#173963=CARTESIAN_POINT('Ctrl Pts',(7.30440169836636,15.2,-7.85949861731061));
#173964=CARTESIAN_POINT('Ctrl Pts',(7.30794205593796,15.2,-7.8616645545333));
#173965=CARTESIAN_POINT('Ctrl Pts',(7.3107743417637,15.2,-7.86339730416981));
#173966=CARTESIAN_POINT('Ctrl Pts',(7.31362365465114,15.2,-7.86513376828637));
#173967=CARTESIAN_POINT('Ctrl Pts',(7.31648993774905,15.2,-7.86687379586612));
#173968=CARTESIAN_POINT('Ctrl Pts',(7.31935622123749,15.2,-7.86861382368294));
#173969=CARTESIAN_POINT('Ctrl Pts',(7.32223947388583,15.2,-7.87035741397629));
#173970=CARTESIAN_POINT('Ctrl Pts',(7.32513963891247,15.2,-7.87210441927019));
#173971=CARTESIAN_POINT('Ctrl Pts',(7.32803980354397,15.2,-7.87385142432605));
#173972=CARTESIAN_POINT('Ctrl Pts',(7.33095688067336,15.2,-7.87560184292247));
#173973=CARTESIAN_POINT('Ctrl Pts',(7.33389081321019,15.2,-7.87735552789));
#173974=CARTESIAN_POINT('Ctrl Pts',(7.33682474614678,15.2,-7.87910921309649));
#173975=CARTESIAN_POINT('Ctrl Pts',(7.33977553461869,15.2,-7.88086616522557));
#173976=CARTESIAN_POINT('Ctrl Pts',(7.34274312222597,15.2,-7.88262623787725));
#173977=CARTESIAN_POINT('Ctrl Pts',(7.34571070942892,15.2,-7.88438631028913));
#173978=CARTESIAN_POINT('Ctrl Pts',(7.34869509506136,15.2,-7.88614950430848));
#173979=CARTESIAN_POINT('Ctrl Pts',(7.35169622363116,15.2,-7.88791567475207));
#173980=CARTESIAN_POINT('Ctrl Pts',(7.35469735260987,15.2,-7.88968184543631));
#173981=CARTESIAN_POINT('Ctrl Pts',(7.35771522422608,15.2,-7.89145099240646));
#173982=CARTESIAN_POINT('Ctrl Pts',(7.36074978128144,15.2,-7.89322297366989));
#173983=CARTESIAN_POINT('Ctrl Pts',(7.36378433792335,15.2,-7.89499495469188));
#173984=CARTESIAN_POINT('Ctrl Pts',(7.36683558060356,15.2,-7.89676977047163));
#173985=CARTESIAN_POINT('Ctrl Pts',(7.36990345373996,15.2,-7.89854727899272));
#173986=CARTESIAN_POINT('Ctrl Pts',(7.37450526407154,15.2,-7.90121354213762));
#173987=CARTESIAN_POINT('Ctrl Pts',(7.37914449107004,15.2,-7.90388586714569));
#173988=CARTESIAN_POINT('Ctrl Pts',(7.38382094847736,15.2,-7.90656378325908));
#173989=CARTESIAN_POINT('Ctrl Pts',(7.3877179961044,15.2,-7.9087953798986));
#173990=CARTESIAN_POINT('Ctrl Pts',(7.39164089426428,15.2,-7.91103086062592));
#173991=CARTESIAN_POINT('Ctrl Pts',(7.39558953926637,15.2,-7.91326995729288));
#173992=CARTESIAN_POINT('Ctrl Pts',(7.3987484550098,15.2,-7.91506123448001));
#173993=CARTESIAN_POINT('Ctrl Pts',(7.40192384672332,15.2,-7.91685482577517));
#173994=CARTESIAN_POINT('Ctrl Pts',(7.40511565923911,15.2,-7.91865059812822));
#173995=CARTESIAN_POINT('Ctrl Pts',(7.40830747218978,15.2,-7.92044637072596));
#173996=CARTESIAN_POINT('Ctrl Pts',(7.41151570710461,15.2,-7.92224432322578));
#173997=CARTESIAN_POINT('Ctrl Pts',(7.41474030694288,15.2,-7.92404432146954));
#173998=CARTESIAN_POINT('Ctrl Pts',(7.4179649063418,15.2,-7.92584431946806));
#173999=CARTESIAN_POINT('Ctrl Pts',(7.42120587123443,15.2,-7.92764636550015));
#174000=CARTESIAN_POINT('Ctrl Pts',(7.42446314696709,15.2,-7.92945032535255));
#174001=CARTESIAN_POINT('Ctrl Pts',(7.42772042314354,15.2,-7.93125428545074));
#174002=CARTESIAN_POINT('Ctrl Pts',(7.43099400907197,15.2,-7.93306016080194));
#174003=CARTESIAN_POINT('Ctrl Pts',(7.43428385125231,15.2,-7.9348678196228));
#174004=CARTESIAN_POINT('Ctrl Pts',(7.43839615375362,15.2,-7.93712739302571));
#174005=CARTESIAN_POINT('Ctrl Pts',(7.4425338536735,15.2,-7.93938975434406));
#174006=CARTESIAN_POINT('Ctrl Pts',(7.44669684721657,15.2,-7.94165465272127));
#174007=CARTESIAN_POINT('Ctrl Pts',(7.45002724177875,15.2,-7.94346657127492));
#174008=CARTESIAN_POINT('Ctrl Pts',(7.45337382243719,15.2,-7.94528011225012));
#174009=CARTESIAN_POINT('Ctrl Pts',(7.4567365362168,15.2,-7.94709515010164));
#174010=CARTESIAN_POINT('Ctrl Pts',(7.46009925045458,15.2,-7.94891018820047));
#174011=CARTESIAN_POINT('Ctrl Pts',(7.46347809617761,15.2,-7.95072672205225));
#174012=CARTESIAN_POINT('Ctrl Pts',(7.46687301975257,15.2,-7.95254462620697));
#174013=CARTESIAN_POINT('Ctrl Pts',(7.47026794286497,15.2,-7.954362530114));
#174014=CARTESIAN_POINT('Ctrl Pts',(7.47367894241303,15.2,-7.95618180382438));
#174015=CARTESIAN_POINT('Ctrl Pts',(7.47710596630269,15.2,-7.95800232371085));
#174016=CARTESIAN_POINT('Ctrl Pts',(7.48053299065928,15.2,-7.95982284384536));
#174017=CARTESIAN_POINT('Ctrl Pts',(7.48397603776546,15.2,-7.96164460979129));
#174018=CARTESIAN_POINT('Ctrl Pts',(7.48743505406614,15.2,-7.96346749739071));
#174019=CARTESIAN_POINT('Ctrl Pts',(7.49089406989552,15.2,-7.96529038474176));
#174020=CARTESIAN_POINT('Ctrl Pts',(7.49436905406058,15.2,-7.96711439526759));
#174021=CARTESIAN_POINT('Ctrl Pts',(7.49785995266246,15.2,-7.96893940645163));
#174022=CARTESIAN_POINT('Ctrl Pts',(7.50135085173997,15.2,-7.97076441788432));
#174023=CARTESIAN_POINT('Ctrl Pts',(7.50485766650815,15.2,-7.9725904296684));
#174024=CARTESIAN_POINT('Ctrl Pts',(7.50838034199395,15.2,-7.97441732127625));
#174025=CARTESIAN_POINT('Ctrl Pts',(7.51190301699978,15.2,-7.9762442126352));
#174026=CARTESIAN_POINT('Ctrl Pts',(7.51544155081094,15.2,-7.97807198345061));
#174027=CARTESIAN_POINT('Ctrl Pts',(7.51899589318542,15.2,-7.97990051596771));
#174028=CARTESIAN_POINT('Ctrl Pts',(7.52255023604418,15.2,-7.98172904873396));
#174029=CARTESIAN_POINT('Ctrl Pts',(7.52612038429057,15.2,-7.98355834170584));
#174030=CARTESIAN_POINT('Ctrl Pts',(7.52970628654155,15.2,-7.98538827725001));
#174031=CARTESIAN_POINT('Ctrl Pts',(7.53418866411098,15.2,-7.98767569655557));
#174032=CARTESIAN_POINT('Ctrl Pts',(7.53869565397767,15.2,-7.98996411995003));
#174033=CARTESIAN_POINT('Ctrl Pts',(7.54322715494988,15.2,-7.99225331849168));
#174034=CARTESIAN_POINT('Ctrl Pts',(7.54685235592522,15.2,-7.99408467742482));
#174035=CARTESIAN_POINT('Ctrl Pts',(7.5504932419663,15.2,-7.99591653310803));
#174036=CARTESIAN_POINT('Ctrl Pts',(7.5541497608894,15.2,-7.99774877004125));
#174037=CARTESIAN_POINT('Ctrl Pts',(7.5578062793143,15.2,-7.99958100672483));
#174038=CARTESIAN_POINT('Ctrl Pts',(7.56147842973493,15.2,-8.00141362508195));
#174039=CARTESIAN_POINT('Ctrl Pts',(7.56516615950571,15.2,-8.00324650977377));
#174040=CARTESIAN_POINT('Ctrl Pts',(7.56885388977894,15.2,-8.00507939471531));
#174041=CARTESIAN_POINT('Ctrl Pts',(7.57255719835921,15.2,-8.00691254635538));
#174042=CARTESIAN_POINT('Ctrl Pts',(7.57627603334126,15.2,-8.00874585256643));
#174043=CARTESIAN_POINT('Ctrl Pts',(7.58092457681545,15.2,-8.01103748520534));
#174044=CARTESIAN_POINT('Ctrl Pts',(7.58559737906784,15.2,-8.01332935810536));
#174045=CARTESIAN_POINT('Ctrl Pts',(7.59029433663925,15.2,-8.01562125254979));
#174046=CARTESIAN_POINT('Ctrl Pts',(7.5940519023892,15.2,-8.01745476795546));
#174047=CARTESIAN_POINT('Ctrl Pts',(7.59782492616485,15.2,-8.01928829830977));
#174048=CARTESIAN_POINT('Ctrl Pts',(7.60161335670564,15.2,-8.02112173122377));
#174049=CARTESIAN_POINT('Ctrl Pts',(7.6054017877626,15.2,-8.02295516438757));
#174050=CARTESIAN_POINT('Ctrl Pts',(7.60920562595072,15.2,-8.0247885025054));
#174051=CARTESIAN_POINT('Ctrl Pts',(7.61302481688267,15.2,-8.02662163404973));
#174052=CARTESIAN_POINT('Ctrl Pts',(7.61684400729424,15.2,-8.0284547653443));
#174053=CARTESIAN_POINT('Ctrl Pts',(7.62067855032046,15.2,-8.03028769017776));
#174054=CARTESIAN_POINT('Ctrl Pts',(7.62452839472697,15.2,-8.03212030158353));
#174055=CARTESIAN_POINT('Ctrl Pts',(7.62837823965803,15.2,-8.033952913239));
#174056=CARTESIAN_POINT('Ctrl Pts',(7.63224338392581,15.2,-8.0357852113995));
#174057=CARTESIAN_POINT('Ctrl Pts',(7.63612377705471,15.2,-8.0376170877575));
#174058=CARTESIAN_POINT('Ctrl Pts',(7.64000416965489,15.2,-8.03944896386589));
#174059=CARTESIAN_POINT('Ctrl Pts',(7.64389980889269,15.2,-8.04128041761109));
#174060=CARTESIAN_POINT('Ctrl Pts',(7.64781064340532,15.2,-8.04311134435034));
#174061=CARTESIAN_POINT('Ctrl Pts',(7.65172147845082,15.2,-8.04494227133905));
#174062=CARTESIAN_POINT('Ctrl Pts',(7.65564750900921,15.2,-8.04677267072491));
#174063=CARTESIAN_POINT('Ctrl Pts',(7.65958868261389,15.2,-8.04860243765793));
#174064=CARTESIAN_POINT('Ctrl Pts',(7.66352985568157,15.2,-8.05043220434163));
#174065=CARTESIAN_POINT('Ctrl Pts',(7.66748616990403,15.2,-8.05226133700944));
#174066=CARTESIAN_POINT('Ctrl Pts',(7.67145757516536,15.2,-8.0540897332847));
#174067=CARTESIAN_POINT('Ctrl Pts',(7.67542898096779,15.2,-8.05591812980909));
#174068=CARTESIAN_POINT('Ctrl Pts',(7.67941547718586,15.2,-8.05774578974429));
#174069=CARTESIAN_POINT('Ctrl Pts',(7.68341701029382,15.2,-8.05957260939935));
#174070=CARTESIAN_POINT('Ctrl Pts',(7.68741854285656,15.2,-8.06139942880551));
#174071=CARTESIAN_POINT('Ctrl Pts',(7.69143511387739,15.2,-8.06322540671183));
#174072=CARTESIAN_POINT('Ctrl Pts',(7.69546667032407,15.2,-8.06505044345163));
#174073=CARTESIAN_POINT('Ctrl Pts',(7.69949822732004,15.2,-8.06687548044008));
#174074=CARTESIAN_POINT('Ctrl Pts',(7.70354477009058,15.2,-8.06869957497418));
#174075=CARTESIAN_POINT('Ctrl Pts',(7.70760624521932,15.2,-8.07052262602626));
#174076=CARTESIAN_POINT('Ctrl Pts',(7.71166771979469,15.2,-8.07234567682996));
#174077=CARTESIAN_POINT('Ctrl Pts',(7.71574412950861,15.2,-8.07416768306215));
#174078=CARTESIAN_POINT('Ctrl Pts',(7.7198354193393,15.2,-8.07598854646898));
#174079=CARTESIAN_POINT('Ctrl Pts',(7.72290388740911,15.2,-8.07735419433421));
#174080=CARTESIAN_POINT('Ctrl Pts',(7.72598072637295,15.2,-8.07871919913259));
#174081=CARTESIAN_POINT('Ctrl Pts',(7.72906591394746,15.2,-8.08008351803911));
#174082=CARTESIAN_POINT('Ctrl Pts',(7.7321511009615,15.2,-8.08144783669778));
#174083=CARTESIAN_POINT('Ctrl Pts',(7.73524463656677,15.2,-8.08281146929815));
#174084=CARTESIAN_POINT('Ctrl Pts',(7.73834649953813,15.2,-8.08417437591523));
#174085=CARTESIAN_POINT('Ctrl Pts',(7.74144836250949,15.2,-8.08553728253232));
#174086=CARTESIAN_POINT('Ctrl Pts',(7.74455855253516,15.2,-8.08689946147788));
#174087=CARTESIAN_POINT('Ctrl Pts',(7.74767704701939,15.2,-8.08826087222626));
#174088=CARTESIAN_POINT('Ctrl Pts',(7.75183503947618,15.2,-8.09007608647499));
#174089=CARTESIAN_POINT('Ctrl Pts',(7.75600779751741,15.2,-8.09188993544337));
#174090=CARTESIAN_POINT('Ctrl Pts',(7.76019526734024,15.2,-8.09370232146203));
#174091=CARTESIAN_POINT('Ctrl Pts',(7.76333587042055,15.2,-8.09506161128469));
#174092=CARTESIAN_POINT('Ctrl Pts',(7.76648474912819,15.2,-8.09642007686546));
#174093=CARTESIAN_POINT('Ctrl Pts',(7.76964188221315,15.2,-8.09777767931265));
#174094=CARTESIAN_POINT('Ctrl Pts',(7.77279901472456,15.2,-8.0991352815132));
#174095=CARTESIAN_POINT('Ctrl Pts',(7.77596440179388,15.2,-8.10049202014713));
#174096=CARTESIAN_POINT('Ctrl Pts',(7.77913802034595,15.2,-8.10184785484779));
#174097=CARTESIAN_POINT('Ctrl Pts',(7.78231163889802,15.2,-8.10320368954846));
#174098=CARTESIAN_POINT('Ctrl Pts',(7.7854934897375,15.2,-8.10455862031097));
#174099=CARTESIAN_POINT('Ctrl Pts',(7.78868355171945,15.2,-8.10591260651792));
#174100=CARTESIAN_POINT('Ctrl Pts',(7.79187361370141,15.2,-8.10726659272487));
#174101=CARTESIAN_POINT('Ctrl Pts',(7.79507188673229,15.2,-8.1086196342751));
#174102=CARTESIAN_POINT('Ctrl Pts',(7.79827834775531,15.2,-8.10997169244046));
#174103=CARTESIAN_POINT('Ctrl Pts',(7.80148480877833,15.2,-8.11132375060581));
#174104=CARTESIAN_POINT('Ctrl Pts',(7.80469945859988,15.2,-8.11267482453515));
#174105=CARTESIAN_POINT('Ctrl Pts',(7.80792227510707,15.2,-8.11402487511118));
#174106=CARTESIAN_POINT('Ctrl Pts',(7.81114509161427,15.2,-8.11537492568722));
#174107=CARTESIAN_POINT('Ctrl Pts',(7.8143760758959,15.2,-8.11672395137166));
#174108=CARTESIAN_POINT('Ctrl Pts',(7.81761520536043,15.2,-8.11807191503117));
#174109=CARTESIAN_POINT('Ctrl Pts',(7.82085433541341,15.2,-8.11941987893555));
#174110=CARTESIAN_POINT('Ctrl Pts',(7.82410161060201,15.2,-8.12076677956464));
#174111=CARTESIAN_POINT('Ctrl Pts',(7.82735700970124,15.2,-8.12211257855174));
#174112=CARTESIAN_POINT('Ctrl Pts',(7.83061240820906,15.2,-8.12345837729435));
#174113=CARTESIAN_POINT('Ctrl Pts',(7.83387593048743,15.2,-8.12480307394178));
#174114=CARTESIAN_POINT('Ctrl Pts',(7.83714755511628,15.2,-8.12614663025162));
#174115=CARTESIAN_POINT('Ctrl Pts',(7.84041917974513,15.2,-8.12749018656146));
#174116=CARTESIAN_POINT('Ctrl Pts',(7.84369890559382,15.2,-8.12883260207837));
#174117=CARTESIAN_POINT('Ctrl Pts',(7.84698671255839,15.2,-8.13017383786286));
#174118=CARTESIAN_POINT('Ctrl Pts',(7.85027451952297,15.2,-8.13151507364736));
#174119=CARTESIAN_POINT('Ctrl Pts',(7.8535704072366,15.2,-8.132855130532));
#174120=CARTESIAN_POINT('Ctrl Pts',(7.85687435324155,15.2,-8.13419397023335));
#174121=CARTESIAN_POINT('Ctrl Pts',(7.86127961498163,15.2,-8.13597908999731));
#174122=CARTESIAN_POINT('Ctrl Pts',(7.86569920325117,15.2,-8.13776204476379));
#174123=CARTESIAN_POINT('Ctrl Pts',(7.8701330682165,15.2,-8.1395427452495));
#174124=CARTESIAN_POINT('Ctrl Pts',(7.87345846663844,15.2,-8.14087827049248));
#174125=CARTESIAN_POINT('Ctrl Pts',(7.87679189515162,15.2,-8.14221252771051));
#174126=CARTESIAN_POINT('Ctrl Pts',(7.88013333211424,15.2,-8.14354547941196));
#174127=CARTESIAN_POINT('Ctrl Pts',(7.88347476907685,15.2,-8.1448784311134));
#174128=CARTESIAN_POINT('Ctrl Pts',(7.88682421419297,15.2,-8.14621007677687));
#174129=CARTESIAN_POINT('Ctrl Pts',(7.89018164625294,15.2,-8.14754038002623));
#174130=CARTESIAN_POINT('Ctrl Pts',(7.89353907831292,15.2,-8.1488706832756));
#174131=CARTESIAN_POINT('Ctrl Pts',(7.89690449902077,15.2,-8.15019964365768));
#174132=CARTESIAN_POINT('Ctrl Pts',(7.90027788449683,15.2,-8.15152722299049));
#174133=CARTESIAN_POINT('Ctrl Pts',(7.90365126997288,15.2,-8.15285480232329));
#174134=CARTESIAN_POINT('Ctrl Pts',(7.90703261990442,15.2,-8.15418100155361));
#174135=CARTESIAN_POINT('Ctrl Pts',(7.91042191486392,15.2,-8.15550578383893));
#174136=CARTESIAN_POINT('Ctrl Pts',(7.91381120982342,15.2,-8.15683056612426));
#174137=CARTESIAN_POINT('Ctrl Pts',(7.9172084492157,15.2,-8.15815393170967));
#174138=CARTESIAN_POINT('Ctrl Pts',(7.92061361075757,15.2,-8.15947584345351));
#174139=CARTESIAN_POINT('Ctrl Pts',(7.92401877291804,15.2,-8.1607977554375));
#174140=CARTESIAN_POINT('Ctrl Pts',(7.92743185824741,15.2,-8.16211821359607));
#174141=CARTESIAN_POINT('Ctrl Pts',(7.93085284395401,15.2,-8.16343718157922));
#174142=CARTESIAN_POINT('Ctrl Pts',(7.93427382903912,15.2,-8.16475614932277));
#174143=CARTESIAN_POINT('Ctrl Pts',(7.93770271698383,15.2,-8.16607362622019));
#174144=CARTESIAN_POINT('Ctrl Pts',(7.94113948369823,15.2,-8.16738957798795));
#174145=CARTESIAN_POINT('Ctrl Pts',(7.94457625041264,15.2,-8.1687055297557));
#174146=CARTESIAN_POINT('Ctrl Pts',(7.94802089680109,15.2,-8.17001995414094));
#174147=CARTESIAN_POINT('Ctrl Pts',(7.95147340134301,15.2,-8.17133281688477));
#174148=CARTESIAN_POINT('Ctrl Pts',(7.95492590588493,15.2,-8.1726456796286));
#174149=CARTESIAN_POINT('Ctrl Pts',(7.95838626900923,15.2,-8.17395698016428));
#174150=CARTESIAN_POINT('Ctrl Pts',(7.96185446946655,15.2,-8.17526668253336));
#174151=CARTESIAN_POINT('Ctrl Pts',(7.96532266992388,15.2,-8.17657638490244));
#174152=CARTESIAN_POINT('Ctrl Pts',(7.96879870768088,15.2,-8.17788449018826));
#174153=CARTESIAN_POINT('Ctrl Pts',(7.97228256113695,15.2,-8.17919096205759));
#174154=CARTESIAN_POINT('Ctrl Pts',(7.97576641459302,15.2,-8.18049743392693));
#174155=CARTESIAN_POINT('Ctrl Pts',(7.97925808400946,15.2,-8.18180227364659));
#174156=CARTESIAN_POINT('Ctrl Pts',(7.98275754809791,15.2,-8.18310544349788));
#174157=CARTESIAN_POINT('Ctrl Pts',(7.98742350063965,15.2,-8.18484300345741));
#174158=CARTESIAN_POINT('Ctrl Pts',(7.99210330678536,15.2,-8.18657759313905));
#174159=CARTESIAN_POINT('Ctrl Pts',(7.99679691987539,15.2,-8.18830913439989));
#174160=CARTESIAN_POINT('Ctrl Pts',(8.00031712937317,15.2,-8.18960779022755));
#174161=CARTESIAN_POINT('Ctrl Pts',(8.00384510547836,15.2,-8.19090473193042));
#174162=CARTESIAN_POINT('Ctrl Pts',(8.00738082801655,15.2,-8.19219992675836));
#174163=CARTESIAN_POINT('Ctrl Pts',(8.01091655055476,15.2,-8.19349512158631));
#174164=CARTESIAN_POINT('Ctrl Pts',(8.0144600206093,15.2,-8.19478857045598));
#174165=CARTESIAN_POINT('Ctrl Pts',(8.01801121306294,15.2,-8.19608023411754));
#174166=CARTESIAN_POINT('Ctrl Pts',(8.02156240551658,15.2,-8.1973718977791));
#174167=CARTESIAN_POINT('Ctrl Pts',(8.02512132091221,15.2,-8.19866177459971));
#174168=CARTESIAN_POINT('Ctrl Pts',(8.02868793308492,15.2,-8.19994982449247));
#174169=CARTESIAN_POINT('Ctrl Pts',(8.03225454525763,15.2,-8.20123787438524));
#174170=CARTESIAN_POINT('Ctrl Pts',(8.03582885370021,15.2,-8.20252409623311));
#174171=CARTESIAN_POINT('Ctrl Pts',(8.03941084394403,15.2,-8.20380846647837));
#174172=CARTESIAN_POINT('Ctrl Pts',(8.04418683136959,15.2,-8.20552096029426));
#174173=CARTESIAN_POINT('Ctrl Pts',(8.04897647635771,15.2,-8.20723016286848));
#174174=CARTESIAN_POINT('Ctrl Pts',(8.05377977099995,15.2,-8.20893607000002));
#174175=CARTESIAN_POINT('Ctrl Pts',(7.01216898599994,12.2,-7.64657512400002));
#174176=CARTESIAN_POINT('Ctrl Pts',(7.01348522039998,12.2,-7.64778327244868));
#174177=CARTESIAN_POINT('Ctrl Pts',(7.0148472207803,12.2,-7.64902613336841));
#174178=CARTESIAN_POINT('Ctrl Pts',(7.01625467904572,12.2,-7.65030255165183));
#174179=CARTESIAN_POINT('Ctrl Pts',(7.01766892478633,12.2,-7.65158512546942));
#174180=CARTESIAN_POINT('Ctrl Pts',(7.01912907680239,12.2,-7.6529015883544));
#174181=CARTESIAN_POINT('Ctrl Pts',(7.02063486162897,12.2,-7.65425083033056));
#174182=CARTESIAN_POINT('Ctrl Pts',(7.0221406463188,12.2,-7.65560007218416));
#174183=CARTESIAN_POINT('Ctrl Pts',(7.0236920633662,12.2,-7.65698209165132));
#174184=CARTESIAN_POINT('Ctrl Pts',(7.02528884122486,12.2,-7.65839580976662));
#174185=CARTESIAN_POINT('Ctrl Pts',(7.02688561908352,12.2,-7.65980952788194));
#174186=CARTESIAN_POINT('Ctrl Pts',(7.02852775929138,12.2,-7.66125494592225));
#174187=CARTESIAN_POINT('Ctrl Pts',(7.03021499706176,12.2,-7.66273101410724));
#174188=CARTESIAN_POINT('Ctrl Pts',(7.03190223498538,12.2,-7.66420708242633));
#174189=CARTESIAN_POINT('Ctrl Pts',(7.03363456925201,12.2,-7.66571380189834));
#174190=CARTESIAN_POINT('Ctrl Pts',(7.03541173743525,12.2,-7.66725015515077));
#174191=CARTESIAN_POINT('Ctrl Pts',(7.03718890545706,12.2,-7.66878650826362));
#174192=CARTESIAN_POINT('Ctrl Pts',(7.03901091135163,12.2,-7.67035249414299));
#174193=CARTESIAN_POINT('Ctrl Pts',(7.04087749604239,12.2,-7.67194712350903));
#174194=CARTESIAN_POINT('Ctrl Pts',(7.04274408073314,12.2,-7.67354175287507));
#174195=CARTESIAN_POINT('Ctrl Pts',(7.04465524144143,12.2,-7.67516502671293));
#174196=CARTESIAN_POINT('Ctrl Pts',(7.04661073111848,12.2,-7.67681598040177));
#174197=CARTESIAN_POINT('Ctrl Pts',(7.04856622097314,12.2,-7.67846693424055));
#174198=CARTESIAN_POINT('Ctrl Pts',(7.0505660383916,12.2,-7.68014557138276));
#174199=CARTESIAN_POINT('Ctrl Pts',(7.052609930506,12.2,-7.68185095122753));
#174200=CARTESIAN_POINT('Ctrl Pts',(7.05465382243473,12.2,-7.68355633091739));
#174201=CARTESIAN_POINT('Ctrl Pts',(7.0567417943918,12.2,-7.68528845520865));
#174202=CARTESIAN_POINT('Ctrl Pts',(7.05887359714957,12.2,-7.68704641381255));
#174203=CARTESIAN_POINT('Ctrl Pts',(7.06100539990735,12.2,-7.68880437241647));
#174204=CARTESIAN_POINT('Ctrl Pts',(7.06318103490329,12.2,-7.69058816246829));
#174205=CARTESIAN_POINT('Ctrl Pts',(7.06540025990411,12.2,-7.6923968984015));
#174206=CARTESIAN_POINT('Ctrl Pts',(7.06761948490493,12.2,-7.69420563433471));
#174207=CARTESIAN_POINT('Ctrl Pts',(7.0698823003436,12.2,-7.69603931773329));
#174208=CARTESIAN_POINT('Ctrl Pts',(7.07218846800684,12.2,-7.69789707783082));
#174209=CARTESIAN_POINT('Ctrl Pts',(7.07449463587956,12.2,-7.69975483809708));
#174210=CARTESIAN_POINT('Ctrl Pts',(7.07684415358985,12.2,-7.7016366785324));
#174211=CARTESIAN_POINT('Ctrl Pts',(7.07923678863878,12.2,-7.70354175580389));
#174212=CARTESIAN_POINT('Ctrl Pts',(7.08162942347036,12.2,-7.70544683290233));
#174213=CARTESIAN_POINT('Ctrl Pts',(7.08406517439434,12.2,-7.70737514680284));
#174214=CARTESIAN_POINT('Ctrl Pts',(7.08654380831542,12.2,-7.70932587299076));
#174215=CARTESIAN_POINT('Ctrl Pts',(7.0890224422365,12.2,-7.71127659917867));
#174216=CARTESIAN_POINT('Ctrl Pts',(7.09154395894146,12.2,-7.71324973923985));
#174217=CARTESIAN_POINT('Ctrl Pts',(7.09410812976205,12.2,-7.71524449049922));
#174218=CARTESIAN_POINT('Ctrl Pts',(7.09667230081556,12.2,-7.7172392419398));
#174219=CARTESIAN_POINT('Ctrl Pts',(7.09927912588989,12.2,-7.71925560495751));
#174220=CARTESIAN_POINT('Ctrl Pts',(7.10192837511943,12.2,-7.72129279365276));
#174221=CARTESIAN_POINT('Ctrl Pts',(7.10457762410833,12.2,-7.72332998216297));
#174222=CARTESIAN_POINT('Ctrl Pts',(7.10726930113565,12.2,-7.72538800047348));
#174223=CARTESIAN_POINT('Ctrl Pts',(7.11000317804864,12.2,-7.72746607899071));
#174224=CARTESIAN_POINT('Ctrl Pts',(7.11273705496165,12.2,-7.72954415750795));
#174225=CARTESIAN_POINT('Ctrl Pts',(7.11551313393964,12.2,-7.73164229980578));
#174226=CARTESIAN_POINT('Ctrl Pts',(7.11833118991771,12.2,-7.73375975631085));
#174227=CARTESIAN_POINT('Ctrl Pts',(7.12114924615177,12.2,-7.73587721300827));
#174228=CARTESIAN_POINT('Ctrl Pts',(7.12400928121682,12.2,-7.73801398467397));
#174229=CARTESIAN_POINT('Ctrl Pts',(7.12691107627235,12.2,-7.74016934248353));
#174230=CARTESIAN_POINT('Ctrl Pts',(7.1298128710643,12.2,-7.7423247000973));
#174231=CARTESIAN_POINT('Ctrl Pts',(7.13275642209165,12.2,-7.74449864123795));
#174232=CARTESIAN_POINT('Ctrl Pts',(7.13574151498319,12.2,-7.74669045474164));
#174233=CARTESIAN_POINT('Ctrl Pts',(7.13872660787473,12.2,-7.74888226824533));
#174234=CARTESIAN_POINT('Ctrl Pts',(7.14175324050544,12.2,-7.75109195327193));
#174235=CARTESIAN_POINT('Ctrl Pts',(7.14482119846152,12.2,-7.75331881030127));
#174236=CARTESIAN_POINT('Ctrl Pts',(7.14788915669627,12.2,-7.7555456675329));
#174237=CARTESIAN_POINT('Ctrl Pts',(7.15099843786044,12.2,-7.75778969883038));
#174238=CARTESIAN_POINT('Ctrl Pts',(7.15414883011829,12.2,-7.76005022170473));
#174239=CARTESIAN_POINT('Ctrl Pts',(7.15729922208998,12.2,-7.76231074437373));
#174240=CARTESIAN_POINT('Ctrl Pts',(7.16049072419569,12.2,-7.76458775550723));
#174241=CARTESIAN_POINT('Ctrl Pts',(7.16372312500968,12.2,-7.7668805912677));
#174242=CARTESIAN_POINT('Ctrl Pts',(7.16695552582367,12.2,-7.76917342702817));
#174243=CARTESIAN_POINT('Ctrl Pts',(7.17022882447495,12.2,-7.77148208502517));
#174244=CARTESIAN_POINT('Ctrl Pts',(7.17354281051944,12.2,-7.77380591110674));
#174245=CARTESIAN_POINT('Ctrl Pts',(7.17630446565685,12.2,-7.77574243291175));
#174246=CARTESIAN_POINT('Ctrl Pts',(7.17909437698944,12.2,-7.77768948970035));
#174247=CARTESIAN_POINT('Ctrl Pts',(7.18191242205741,12.2,-7.77964670963038));
#174248=CARTESIAN_POINT('Ctrl Pts',(7.18473046712538,12.2,-7.7816039295604));
#174249=CARTESIAN_POINT('Ctrl Pts',(7.18757664829088,12.2,-7.78357131208995));
#174250=CARTESIAN_POINT('Ctrl Pts',(7.19045084253998,12.2,-7.78554849376558));
#174251=CARTESIAN_POINT('Ctrl Pts',(7.19332503678907,12.2,-7.78752567544121));
#174252=CARTESIAN_POINT('Ctrl Pts',(7.19622724572209,12.2,-7.78951265435554));
#174253=CARTESIAN_POINT('Ctrl Pts',(7.1991573499582,12.2,-7.79150907504999));
#174254=CARTESIAN_POINT('Ctrl Pts',(7.20208745419431,12.2,-7.79350549574444));
#174255=CARTESIAN_POINT('Ctrl Pts',(7.20504545320452,12.2,-7.79551135381969));
#174256=CARTESIAN_POINT('Ctrl Pts',(7.20803123050984,12.2,-7.79752630146776));
#174257=CARTESIAN_POINT('Ctrl Pts',(7.21101700781514,12.2,-7.79954124911583));
#174258=CARTESIAN_POINT('Ctrl Pts',(7.21403055872526,12.2,-7.80156528312142));
#174259=CARTESIAN_POINT('Ctrl Pts',(7.21707177115726,12.2,-7.80359805985798));
#174260=CARTESIAN_POINT('Ctrl Pts',(7.22011298358926,12.2,-7.80563083659454));
#174261=CARTESIAN_POINT('Ctrl Pts',(7.22318185372333,12.2,-7.80767235337257));
#174262=CARTESIAN_POINT('Ctrl Pts',(7.22627826691921,12.2,-7.80972227115077));
#174263=CARTESIAN_POINT('Ctrl Pts',(7.22937468011509,12.2,-7.81177218892898));
#174264=CARTESIAN_POINT('Ctrl Pts',(7.232498633412,12.2,-7.81383050583054));
#174265=CARTESIAN_POINT('Ctrl Pts',(7.2356500136408,12.2,-7.8158968902399));
#174266=CARTESIAN_POINT('Ctrl Pts',(7.2388013938696,12.2,-7.81796327464925));
#174267=CARTESIAN_POINT('Ctrl Pts',(7.24198019768924,12.2,-7.82003772281617));
#174268=CARTESIAN_POINT('Ctrl Pts',(7.24518631192758,12.2,-7.82211990649735));
#174269=CARTESIAN_POINT('Ctrl Pts',(7.24839242616592,12.2,-7.82420209017854));
#174270=CARTESIAN_POINT('Ctrl Pts',(7.25162585030193,12.2,-7.8262920095904));
#174271=CARTESIAN_POINT('Ctrl Pts',(7.25488646794304,12.2,-7.82838934000766));
#174272=CARTESIAN_POINT('Ctrl Pts',(7.25814708522875,12.2,-7.83048667019634));
#174273=CARTESIAN_POINT('Ctrl Pts',(7.26143489795204,12.2,-7.83259141059899));
#174274=CARTESIAN_POINT('Ctrl Pts',(7.26474978932463,12.2,-7.83470324321544));
#174275=CARTESIAN_POINT('Ctrl Pts',(7.26806468105854,12.2,-7.83681507606209));
#174276=CARTESIAN_POINT('Ctrl Pts',(7.27140665252256,12.2,-7.83893400037807));
#174277=CARTESIAN_POINT('Ctrl Pts',(7.27477558932589,12.2,-7.84105970169696));
#174278=CARTESIAN_POINT('Ctrl Pts',(7.27881831371023,12.2,-7.84361054341865));
#174279=CARTESIAN_POINT('Ctrl Pts',(7.28289986889003,12.2,-7.84617114590798));
#174280=CARTESIAN_POINT('Ctrl Pts',(7.28702005819959,12.2,-7.84874097163176));
#174281=CARTESIAN_POINT('Ctrl Pts',(7.29045354910377,12.2,-7.85088249295154));
#174282=CARTESIAN_POINT('Ctrl Pts',(7.29391387020648,12.2,-7.85303042183648));
#174283=CARTESIAN_POINT('Ctrl Pts',(7.2974009071881,12.2,-7.85518445250007));
#174284=CARTESIAN_POINT('Ctrl Pts',(7.30088794416971,12.2,-7.85733848316366));
#174285=CARTESIAN_POINT('Ctrl Pts',(7.30440169836636,12.2,-7.85949861731061));
#174286=CARTESIAN_POINT('Ctrl Pts',(7.30794205593796,12.2,-7.8616645545333));
#174287=CARTESIAN_POINT('Ctrl Pts',(7.3107743417637,12.2,-7.86339730416981));
#174288=CARTESIAN_POINT('Ctrl Pts',(7.31362365465114,12.2,-7.86513376828637));
#174289=CARTESIAN_POINT('Ctrl Pts',(7.31648993774905,12.2,-7.86687379586612));
#174290=CARTESIAN_POINT('Ctrl Pts',(7.31935622123749,12.2,-7.86861382368294));
#174291=CARTESIAN_POINT('Ctrl Pts',(7.32223947388583,12.2,-7.87035741397629));
#174292=CARTESIAN_POINT('Ctrl Pts',(7.32513963891247,12.2,-7.87210441927019));
#174293=CARTESIAN_POINT('Ctrl Pts',(7.32803980354397,12.2,-7.87385142432605));
#174294=CARTESIAN_POINT('Ctrl Pts',(7.33095688067336,12.2,-7.87560184292247));
#174295=CARTESIAN_POINT('Ctrl Pts',(7.33389081321019,12.2,-7.87735552789));
#174296=CARTESIAN_POINT('Ctrl Pts',(7.33755822918106,12.2,-7.87954763427864));
#174297=CARTESIAN_POINT('Ctrl Pts',(7.34125198209144,12.2,-7.88174484455071));
#174298=CARTESIAN_POINT('Ctrl Pts',(7.34497196125675,12.2,-7.88394687510602));
#174299=CARTESIAN_POINT('Ctrl Pts',(7.34794794475119,12.2,-7.88570849964627));
#174300=CARTESIAN_POINT('Ctrl Pts',(7.35094071298473,12.2,-7.88747320897994));
#174301=CARTESIAN_POINT('Ctrl Pts',(7.35395020891167,12.2,-7.88924085899819));
#174302=CARTESIAN_POINT('Ctrl Pts',(7.35695970442857,12.2,-7.89100850877559));
#174303=CARTESIAN_POINT('Ctrl Pts',(7.35998592972057,12.2,-7.8927790992141));
#174304=CARTESIAN_POINT('Ctrl Pts',(7.36302882619295,12.2,-7.89455248834672));
#174305=CARTESIAN_POINT('Ctrl Pts',(7.36607172307993,12.2,-7.89632587772097));
#174306=CARTESIAN_POINT('Ctrl Pts',(7.36913129149947,12.2,-7.89810206652612));
#174307=CARTESIAN_POINT('Ctrl Pts',(7.37220747700153,12.2,-7.89988091384546));
#174308=CARTESIAN_POINT('Ctrl Pts',(7.37528366208447,12.2,-7.90165976092243));
#174309=CARTESIAN_POINT('Ctrl Pts',(7.37837646182128,12.2,-7.90344126715918));
#174310=CARTESIAN_POINT('Ctrl Pts',(7.38148582249879,12.2,-7.90522529299115));
#174311=CARTESIAN_POINT('Ctrl Pts',(7.38459518359994,12.2,-7.90700931906619));
#174312=CARTESIAN_POINT('Ctrl Pts',(7.38772110534015,12.2,-7.90879586437362));
#174313=CARTESIAN_POINT('Ctrl Pts',(7.39086353029026,12.2,-7.91058479363794));
#174314=CARTESIAN_POINT('Ctrl Pts',(7.39400595481222,12.2,-7.91237372265852));
#174315=CARTESIAN_POINT('Ctrl Pts',(7.39716488463087,12.2,-7.91416503415361));
#174316=CARTESIAN_POINT('Ctrl Pts',(7.40034026248071,12.2,-7.91595859200676));
#174317=CARTESIAN_POINT('Ctrl Pts',(7.40351564076321,12.2,-7.91775215010429));
#174318=CARTESIAN_POINT('Ctrl Pts',(7.40670746712928,12.2,-7.91954795595341));
#174319=CARTESIAN_POINT('Ctrl Pts',(7.4099156879854,12.2,-7.92134587522623));
#174320=CARTESIAN_POINT('Ctrl Pts',(7.4131239084044,12.2,-7.92314379425408));
#174321=CARTESIAN_POINT('Ctrl Pts',(7.41634852180882,12.2,-7.92494382498344));
#174322=CARTESIAN_POINT('Ctrl Pts',(7.41958947298666,12.2,-7.92674583744705));
#174323=CARTESIAN_POINT('Ctrl Pts',(7.42283042460608,12.2,-7.92854785015617));
#174324=CARTESIAN_POINT('Ctrl Pts',(7.4260877143798,12.2,-7.93035184282937));
#174325=CARTESIAN_POINT('Ctrl Pts',(7.42936128672487,12.2,-7.93215768548334));
#174326=CARTESIAN_POINT('Ctrl Pts',(7.43263485906994,12.2,-7.93396352813731));
#174327=CARTESIAN_POINT('Ctrl Pts',(7.4359247148947,12.2,-7.93577121949983));
#174328=CARTESIAN_POINT('Ctrl Pts',(7.43923079846543,12.2,-7.93758063032085));
#174329=CARTESIAN_POINT('Ctrl Pts',(7.44253688158571,12.2,-7.93939004089532));
#174330=CARTESIAN_POINT('Ctrl Pts',(7.4458591925582,12.2,-7.94120117193874));
#174331=CARTESIAN_POINT('Ctrl Pts',(7.44919767702261,12.2,-7.94301389379877));
#174332=CARTESIAN_POINT('Ctrl Pts',(7.45253616194188,12.2,-7.94482661590579));
#174333=CARTESIAN_POINT('Ctrl Pts',(7.45589081965178,12.2,-7.94664092944779));
#174334=CARTESIAN_POINT('Ctrl Pts',(7.45926159655934,12.2,-7.94845670754689));
#174335=CARTESIAN_POINT('Ctrl Pts',(7.46263237300765,12.2,-7.95027248539859));
#174336=CARTESIAN_POINT('Ctrl Pts',(7.46601926710107,12.2,-7.95208972755287));
#174337=CARTESIAN_POINT('Ctrl Pts',(7.46942222548851,12.2,-7.95390830879302));
#174338=CARTESIAN_POINT('Ctrl Pts',(7.47282518433961,12.2,-7.95572689028095));
#174339=CARTESIAN_POINT('Ctrl Pts',(7.47624420656598,12.2,-7.95754681084617));
#174340=CARTESIAN_POINT('Ctrl Pts',(7.47967923848175,12.2,-7.95936794581428));
#174341=CARTESIAN_POINT('Ctrl Pts',(7.48311426992949,12.2,-7.96118908053426));
#174342=CARTESIAN_POINT('Ctrl Pts',(7.48656531214274,12.2,-7.96301143010287));
#174343=CARTESIAN_POINT('Ctrl Pts',(7.49003230869161,12.2,-7.96483487134262));
#174344=CARTESIAN_POINT('Ctrl Pts',(7.49349930571284,12.2,-7.96665831283081));
#174345=CARTESIAN_POINT('Ctrl Pts',(7.49698225712489,12.2,-7.96848284732471));
#174346=CARTESIAN_POINT('Ctrl Pts',(7.50048111126106,12.2,-7.97030835092426));
#174347=CARTESIAN_POINT('Ctrl Pts',(7.50397996492053,12.2,-7.97213385427508));
#174348=CARTESIAN_POINT('Ctrl Pts',(7.50749471944015,12.2,-7.97396032869579));
#174349=CARTESIAN_POINT('Ctrl Pts',(7.51102532077099,12.2,-7.9757876526932));
#174350=CARTESIAN_POINT('Ctrl Pts',(7.51455592258288,12.2,-7.97761497693956));
#174351=CARTESIAN_POINT('Ctrl Pts',(7.51810237148497,12.2,-7.97944315110537));
#174352=CARTESIAN_POINT('Ctrl Pts',(7.52166461379125,12.2,-7.98127205664953));
#174353=CARTESIAN_POINT('Ctrl Pts',(7.52522685561217,12.2,-7.98310096194451));
#174354=CARTESIAN_POINT('Ctrl Pts',(7.52880489064658,12.2,-7.98493059795321));
#174355=CARTESIAN_POINT('Ctrl Pts',(7.53239866512897,12.2,-7.98676084719243));
#174356=CARTESIAN_POINT('Ctrl Pts',(7.535992440101,12.2,-7.98859109668101));
#174357=CARTESIAN_POINT('Ctrl Pts',(7.53960195397454,12.2,-7.99042195955855));
#174358=CARTESIAN_POINT('Ctrl Pts',(7.54322715494989,12.2,-7.99225331849168));
#174359=CARTESIAN_POINT('Ctrl Pts',(7.54685235592523,12.2,-7.99408467742483));
#174360=CARTESIAN_POINT('Ctrl Pts',(7.55049324196629,12.2,-7.99591653310802));
#174361=CARTESIAN_POINT('Ctrl Pts',(7.55414976088939,12.2,-7.99774877004125));
#174362=CARTESIAN_POINT('Ctrl Pts',(7.55780627931429,12.2,-7.99958100672483));
#174363=CARTESIAN_POINT('Ctrl Pts',(7.56147842973493,12.2,-8.00141362508195));
#174364=CARTESIAN_POINT('Ctrl Pts',(7.56516615950571,12.2,-8.00324650977377));
#174365=CARTESIAN_POINT('Ctrl Pts',(7.56885388977894,12.2,-8.00507939471531));
#174366=CARTESIAN_POINT('Ctrl Pts',(7.57255719835921,12.2,-8.00691254635538));
#174367=CARTESIAN_POINT('Ctrl Pts',(7.57627603334126,12.2,-8.00874585256643));
#174368=CARTESIAN_POINT('Ctrl Pts',(7.5799948678166,12.2,-8.01057915852768));
#174369=CARTESIAN_POINT('Ctrl Pts',(7.58372922740104,12.2,-8.01241261765558));
#174370=CARTESIAN_POINT('Ctrl Pts',(7.58747906042681,12.2,-8.01424611961679));
#174371=CARTESIAN_POINT('Ctrl Pts',(7.59216635209222,12.2,-8.01653799725567));
#174372=CARTESIAN_POINT('Ctrl Pts',(7.59687781814253,12.2,-8.01882993989391));
#174373=CARTESIAN_POINT('Ctrl Pts',(7.60161335670564,12.2,-8.02112173122377));
#174374=CARTESIAN_POINT('Ctrl Pts',(7.6054017877626,12.2,-8.02295516438757));
#174375=CARTESIAN_POINT('Ctrl Pts',(7.60920562595072,12.2,-8.0247885025054));
#174376=CARTESIAN_POINT('Ctrl Pts',(7.61302481688267,12.2,-8.02662163404973));
#174377=CARTESIAN_POINT('Ctrl Pts',(7.61684400729424,12.2,-8.0284547653443));
#174378=CARTESIAN_POINT('Ctrl Pts',(7.62067855032046,12.2,-8.03028769017776));
#174379=CARTESIAN_POINT('Ctrl Pts',(7.62452839472697,12.2,-8.03212030158353));
#174380=CARTESIAN_POINT('Ctrl Pts',(7.62837823965803,12.2,-8.033952913239));
#174381=CARTESIAN_POINT('Ctrl Pts',(7.63224338392581,12.2,-8.0357852113995));
#174382=CARTESIAN_POINT('Ctrl Pts',(7.63612377705471,12.2,-8.0376170877575));
#174383=CARTESIAN_POINT('Ctrl Pts',(7.64000416965489,12.2,-8.03944896386589));
#174384=CARTESIAN_POINT('Ctrl Pts',(7.64389980889268,12.2,-8.04128041761109));
#174385=CARTESIAN_POINT('Ctrl Pts',(7.64781064340532,12.2,-8.04311134435034));
#174386=CARTESIAN_POINT('Ctrl Pts',(7.65172147845082,12.2,-8.04494227133905));
#174387=CARTESIAN_POINT('Ctrl Pts',(7.65564750900921,12.2,-8.04677267072491));
#174388=CARTESIAN_POINT('Ctrl Pts',(7.65958868261389,12.2,-8.04860243765793));
#174389=CARTESIAN_POINT('Ctrl Pts',(7.66352985568157,12.2,-8.05043220434163));
#174390=CARTESIAN_POINT('Ctrl Pts',(7.66748616990403,12.2,-8.05226133700944));
#174391=CARTESIAN_POINT('Ctrl Pts',(7.67145757516536,12.2,-8.0540897332847));
#174392=CARTESIAN_POINT('Ctrl Pts',(7.67542898096779,12.2,-8.05591812980909));
#174393=CARTESIAN_POINT('Ctrl Pts',(7.67941547718586,12.2,-8.05774578974429));
#174394=CARTESIAN_POINT('Ctrl Pts',(7.68341701029382,12.2,-8.05957260939935));
#174395=CARTESIAN_POINT('Ctrl Pts',(7.68741854285656,12.2,-8.06139942880551));
#174396=CARTESIAN_POINT('Ctrl Pts',(7.6914351138774,12.2,-8.06322540671183));
#174397=CARTESIAN_POINT('Ctrl Pts',(7.69546667032408,12.2,-8.06505044345163));
#174398=CARTESIAN_POINT('Ctrl Pts',(7.69949822732005,12.2,-8.06687548044008));
#174399=CARTESIAN_POINT('Ctrl Pts',(7.70354477009057,12.2,-8.06869957497417));
#174400=CARTESIAN_POINT('Ctrl Pts',(7.70760624521931,12.2,-8.07052262602626));
#174401=CARTESIAN_POINT('Ctrl Pts',(7.71065235128918,12.2,-8.07188991419113));
#174402=CARTESIAN_POINT('Ctrl Pts',(7.71370685831119,12.2,-8.07325661520887));
#174403=CARTESIAN_POINT('Ctrl Pts',(7.71676974325544,12.2,-8.07462268645711));
#174404=CARTESIAN_POINT('Ctrl Pts',(7.71983262819969,12.2,-8.07598875770535));
#174405=CARTESIAN_POINT('Ctrl Pts',(7.72290389047696,12.2,-8.07735420070077));
#174406=CARTESIAN_POINT('Ctrl Pts',(7.72598350940601,12.2,-8.07871897185958));
#174407=CARTESIAN_POINT('Ctrl Pts',(7.72906312833507,12.2,-8.08008374301838));
#174408=CARTESIAN_POINT('Ctrl Pts',(7.7321511031052,12.2,-8.08144784196891));
#174409=CARTESIAN_POINT('Ctrl Pts',(7.73524741211657,12.2,-8.08281122816947));
#174410=CARTESIAN_POINT('Ctrl Pts',(7.73834372169042,12.2,-8.08417461461772));
#174411=CARTESIAN_POINT('Ctrl Pts',(7.74144836607497,12.2,-8.08553728883243));
#174412=CARTESIAN_POINT('Ctrl Pts',(7.74456132215352,12.2,-8.08689920732192));
#174413=CARTESIAN_POINT('Ctrl Pts',(7.74871192931572,12.2,-8.08871509822889));
#174414=CARTESIAN_POINT('Ctrl Pts',(7.7528773134865,12.2,-8.09052964854155));
#174415=CARTESIAN_POINT('Ctrl Pts',(7.75705742449704,12.2,-8.09234275945712));
#174416=CARTESIAN_POINT('Ctrl Pts',(7.76019250789733,12.2,-8.09370259270556));
#174417=CARTESIAN_POINT('Ctrl Pts',(7.76333587322172,12.2,-8.09506161708457));
#174418=CARTESIAN_POINT('Ctrl Pts',(7.76648750064817,12.2,-8.09641979032697));
#174419=CARTESIAN_POINT('Ctrl Pts',(7.76963912807461,12.2,-8.09777796356937));
#174420=CARTESIAN_POINT('Ctrl Pts',(7.77279901690881,12.2,-8.09913528725348));
#174421=CARTESIAN_POINT('Ctrl Pts',(7.77596714533424,12.2,-8.10049171999599));
#174422=CARTESIAN_POINT('Ctrl Pts',(7.77913527433522,12.2,-8.1018481529849));
#174423=CARTESIAN_POINT('Ctrl Pts',(7.7823116421302,12.2,-8.10320369578193));
#174424=CARTESIAN_POINT('Ctrl Pts',(7.78549622821913,12.2,-8.10455830727033));
#174425=CARTESIAN_POINT('Ctrl Pts',(7.78868081372953,12.2,-8.10591291851264));
#174426=CARTESIAN_POINT('Ctrl Pts',(7.79187361794138,12.2,-8.10726659894341));
#174427=CARTESIAN_POINT('Ctrl Pts',(7.79507461761095,12.2,-8.10861930829506));
#174428=CARTESIAN_POINT('Ctrl Pts',(7.79934261697653,12.2,-8.11042292068202));
#174429=CARTESIAN_POINT('Ctrl Pts',(7.80362518662598,12.2,-8.11222480775822));
#174430=CARTESIAN_POINT('Ctrl Pts',(7.80792227510707,12.2,-8.11402487511118));
#174431=CARTESIAN_POINT('Ctrl Pts',(7.81114509161427,12.2,-8.11537492568722));
#174432=CARTESIAN_POINT('Ctrl Pts',(7.8143760758959,12.2,-8.11672395137166));
#174433=CARTESIAN_POINT('Ctrl Pts',(7.81761520536043,12.2,-8.11807191503117));
#174434=CARTESIAN_POINT('Ctrl Pts',(7.82085433541341,12.2,-8.11941987893555));
#174435=CARTESIAN_POINT('Ctrl Pts',(7.82410161060201,12.2,-8.12076677956464));
#174436=CARTESIAN_POINT('Ctrl Pts',(7.82735700970124,12.2,-8.12211257855174));
#174437=CARTESIAN_POINT('Ctrl Pts',(7.83061240820906,12.2,-8.12345837729435));
#174438=CARTESIAN_POINT('Ctrl Pts',(7.83387593048743,12.2,-8.12480307394178));
#174439=CARTESIAN_POINT('Ctrl Pts',(7.83714755511628,12.2,-8.12614663025162));
#174440=CARTESIAN_POINT('Ctrl Pts',(7.84041917974513,12.2,-8.12749018656146));
#174441=CARTESIAN_POINT('Ctrl Pts',(7.84369890559382,12.2,-8.12883260207837));
#174442=CARTESIAN_POINT('Ctrl Pts',(7.84698671255839,12.2,-8.13017383786286));
#174443=CARTESIAN_POINT('Ctrl Pts',(7.85027451952297,12.2,-8.13151507364736));
#174444=CARTESIAN_POINT('Ctrl Pts',(7.8535704072366,12.2,-8.132855130532));
#174445=CARTESIAN_POINT('Ctrl Pts',(7.85687435324155,12.2,-8.13419397023335));
#174446=CARTESIAN_POINT('Ctrl Pts',(7.8601782992465,12.2,-8.13553280993471));
#174447=CARTESIAN_POINT('Ctrl Pts',(7.86349030432613,12.2,-8.13687043210278));
#174448=CARTESIAN_POINT('Ctrl Pts',(7.86681034637147,12.2,-8.13820679838767));
#174449=CARTESIAN_POINT('Ctrl Pts',(7.87013038841681,12.2,-8.13954316467256));
#174450=CARTESIAN_POINT('Ctrl Pts',(7.8734584687616,12.2,-8.14087827564088));
#174451=CARTESIAN_POINT('Ctrl Pts',(7.8767945642643,12.2,-8.14221209342592));
#174452=CARTESIAN_POINT('Ctrl Pts',(7.88013066037304,12.2,-8.14354591145326));
#174453=CARTESIAN_POINT('Ctrl Pts',(7.88347477237572,12.2,-8.14487843628027));
#174454=CARTESIAN_POINT('Ctrl Pts',(7.88682687798899,12.2,-8.14620963076522));
#174455=CARTESIAN_POINT('Ctrl Pts',(7.89017898299329,12.2,-8.14754082500835));
#174456=CARTESIAN_POINT('Ctrl Pts',(7.89353908232146,12.2,-8.14887068922244));
#174457=CARTESIAN_POINT('Ctrl Pts',(7.89690715540994,12.2,-8.15019918503204));
#174458=CARTESIAN_POINT('Ctrl Pts',(7.90027522849842,12.2,-8.15152768084165));
#174459=CARTESIAN_POINT('Ctrl Pts',(7.90365127357448,12.2,-8.15285480812613));
#174460=CARTESIAN_POINT('Ctrl Pts',(7.90703526961888,12.2,-8.15418053091117));
#174461=CARTESIAN_POINT('Ctrl Pts',(7.91154726413984,12.2,-8.15594816121095));
#174462=CARTESIAN_POINT('Ctrl Pts',(7.91607339557461,12.2,-8.15771329454178));
#174463=CARTESIAN_POINT('Ctrl Pts',(7.92061361075757,12.2,-8.15947584345351));
#174464=CARTESIAN_POINT('Ctrl Pts',(7.92515382655913,12.2,-8.16123839260539));
#174465=CARTESIAN_POINT('Ctrl Pts',(7.92970812676935,12.2,-8.16299835740859));
#174466=CARTESIAN_POINT('Ctrl Pts',(7.93427646176133,12.2,-8.16475565073456));
#174467=CARTESIAN_POINT('Ctrl Pts',(7.9377027126941,12.2,-8.16607362060932));
#174468=CARTESIAN_POINT('Ctrl Pts',(7.94113685797289,12.2,-8.16739008949063));
#174469=CARTESIAN_POINT('Ctrl Pts',(7.94457887544676,12.2,-8.16870501928216));
#174470=CARTESIAN_POINT('Ctrl Pts',(7.94802089292064,12.2,-8.1700199490737));
#174471=CARTESIAN_POINT('Ctrl Pts',(7.95147078271611,12.2,-8.17133334008787));
#174472=CARTESIAN_POINT('Ctrl Pts',(7.95492852413146,12.2,-8.17264515737368));
#174473=CARTESIAN_POINT('Ctrl Pts',(7.95838626554681,12.2,-8.17395697465949));
#174474=CARTESIAN_POINT('Ctrl Pts',(7.96185185806996,12.2,-8.17526721716206));
#174475=CARTESIAN_POINT('Ctrl Pts',(7.96532528102603,12.2,-8.17657585090641));
#174476=CARTESIAN_POINT('Ctrl Pts',(7.96995651205477,12.2,-8.17832069605736));
#174477=CARTESIAN_POINT('Ctrl Pts',(7.97460166248075,12.2,-8.18006268020411));
#174478=CARTESIAN_POINT('Ctrl Pts',(7.97926068347808,12.2,-8.18180171875121));
#174479=CARTESIAN_POINT('Ctrl Pts',(7.98275494890868,12.2,-8.18310599754308));
#174480=CARTESIAN_POINT('Ctrl Pts',(7.98625701599166,12.2,-8.18440861915686));
#174481=CARTESIAN_POINT('Ctrl Pts',(7.98976686150504,12.2,-8.18570954653218));
#174482=CARTESIAN_POINT('Ctrl Pts',(7.99444665594795,12.2,-8.18744411652349));
#174483=CARTESIAN_POINT('Ctrl Pts',(7.99914028058659,12.2,-8.18917567643041));
#174484=CARTESIAN_POINT('Ctrl Pts',(8.00384768901123,12.2,-8.1909041510243));
#174485=CARTESIAN_POINT('Ctrl Pts',(8.007378245009,12.2,-8.19220050685196));
#174486=CARTESIAN_POINT('Ctrl Pts',(8.01091655503138,12.2,-8.19349512722138));
#174487=CARTESIAN_POINT('Ctrl Pts',(8.01446259644487,12.2,-8.19478797688259));
#174488=CARTESIAN_POINT('Ctrl Pts',(8.01800863785837,12.2,-8.19608082654379));
#174489=CARTESIAN_POINT('Ctrl Pts',(8.02156241031632,12.2,-8.19737190427552));
#174490=CARTESIAN_POINT('Ctrl Pts',(8.0251238882448,12.2,-8.1986611675262));
#174491=CARTESIAN_POINT('Ctrl Pts',(8.03105968500793,12.2,-8.20080993968872));
#174492=CARTESIAN_POINT('Ctrl Pts',(8.03701687660465,12.2,-8.20295365973189));
#174493=CARTESIAN_POINT('Ctrl Pts',(8.04299539641855,12.2,-8.20509222040386));
#174494=CARTESIAN_POINT('Ctrl Pts',(8.04658250817656,12.2,-8.20637535676042));
#174495=CARTESIAN_POINT('Ctrl Pts',(8.05017730034549,12.2,-8.20765663976758));
#174496=CARTESIAN_POINT('Ctrl Pts',(8.05377977099995,12.2,-8.20893607000002));
#174497=CARTESIAN_POINT('Origin',(-5.66257110645729E-14,15.2,-1.77635683940025E-14));
#174498=CARTESIAN_POINT('',(8.02901631833639,15.2,-6.57080831866923));
#174499=CARTESIAN_POINT('',(8.02901631833639,12.2,-6.57080831866923));
#174500=CARTESIAN_POINT('',(8.02901631799994,15.2,-6.57080831900001));
#174501=CARTESIAN_POINT('Origin',(-5.66257110645729E-14,12.2,-1.77635683940025E-14));
#174502=CARTESIAN_POINT('Origin',(-5.66257110645729E-14,15.2,-1.77635683940025E-14));
#174503=CARTESIAN_POINT('Origin',(-5.66257110645729E-14,15.2,-1.77635683940025E-14));
#174504=CARTESIAN_POINT('',(9.14005731399994,15.2,-6.97920857100002));
#174505=CARTESIAN_POINT('',(9.36775917399994,15.2,-6.67046385500001));
#174506=CARTESIAN_POINT('Origin',(-5.66257110645729E-14,15.2,-1.77635683940025E-14));
#174507=CARTESIAN_POINT('',(9.36775917399994,12.2,-6.67046385500001));
#174508=CARTESIAN_POINT('',(9.36775917399994,15.2,-6.67046385500001));
#174509=CARTESIAN_POINT('',(9.14005731399994,12.2,-6.97920857100002));
#174510=CARTESIAN_POINT('Origin',(-5.66257110645729E-14,12.2,-1.77635683940025E-14));
#174511=CARTESIAN_POINT('',(9.14005731399994,15.2,-6.97920857100002));
#174512=CARTESIAN_POINT('Ctrl Pts',(8.02901631899994,15.2,-6.57080831800001));
#174513=CARTESIAN_POINT('Ctrl Pts',(8.02901631899994,11.6,-6.57080831800001));
#174514=CARTESIAN_POINT('Ctrl Pts',(8.02916024099994,15.2,-6.57090674100001));
#174515=CARTESIAN_POINT('Ctrl Pts',(8.02916024099994,11.6,-6.57090674100001));
#174516=CARTESIAN_POINT('Ctrl Pts',(8.02945316199994,15.2,-6.57110695200001));
#174517=CARTESIAN_POINT('Ctrl Pts',(8.02945316199994,11.6,-6.57110695200001));
#174518=CARTESIAN_POINT('Ctrl Pts',(8.02989715799994,15.2,-6.57141009900001));
#174519=CARTESIAN_POINT('Ctrl Pts',(8.02989715799994,11.6,-6.57141009900001));
#174520=CARTESIAN_POINT('Ctrl Pts',(8.03049556399994,15.2,-6.57181801900002));
#174521=CARTESIAN_POINT('Ctrl Pts',(8.03049556399994,11.6,-6.57181801900002));
#174522=CARTESIAN_POINT('Ctrl Pts',(8.03125297399994,15.2,-6.57233322300002));
#174523=CARTESIAN_POINT('Ctrl Pts',(8.03125297399994,11.6,-6.57233322300002));
#174524=CARTESIAN_POINT('Ctrl Pts',(8.03202318499994,15.2,-6.57285600500002));
#174525=CARTESIAN_POINT('Ctrl Pts',(8.03202318499994,11.6,-6.57285600500002));
#174526=CARTESIAN_POINT('Ctrl Pts',(8.03280179799994,15.2,-6.57338335000002));
#174527=CARTESIAN_POINT('Ctrl Pts',(8.03280179799994,11.6,-6.57338335000002));
#174528=CARTESIAN_POINT('Ctrl Pts',(8.03358879899994,15.2,-6.57391522700002));
#174529=CARTESIAN_POINT('Ctrl Pts',(8.03358879899994,11.6,-6.57391522700002));
#174530=CARTESIAN_POINT('Ctrl Pts',(8.03438417899994,15.2,-6.57445160500002));
#174531=CARTESIAN_POINT('Ctrl Pts',(8.03438417899994,11.6,-6.57445160500002));
#174532=CARTESIAN_POINT('Ctrl Pts',(8.03518792399995,15.2,-6.57499245800001));
#174533=CARTESIAN_POINT('Ctrl Pts',(8.03518792399995,11.6,-6.57499245800001));
#174534=CARTESIAN_POINT('Ctrl Pts',(8.03600002099994,15.2,-6.57553775100002));
#174535=CARTESIAN_POINT('Ctrl Pts',(8.03600002099994,11.6,-6.57553775100002));
#174536=CARTESIAN_POINT('Ctrl Pts',(8.03682045999994,15.2,-6.57608745900002));
#174537=CARTESIAN_POINT('Ctrl Pts',(8.03682045999994,11.6,-6.57608745900002));
#174538=CARTESIAN_POINT('Ctrl Pts',(8.03764922899994,15.2,-6.57664155100001));
#174539=CARTESIAN_POINT('Ctrl Pts',(8.03764922899994,11.6,-6.57664155100001));
#174540=CARTESIAN_POINT('Ctrl Pts',(8.03848631399994,15.2,-6.57719999700002));
#174541=CARTESIAN_POINT('Ctrl Pts',(8.03848631399994,11.6,-6.57719999700002));
#174542=CARTESIAN_POINT('Ctrl Pts',(8.03933170499995,15.2,-6.57776276800002));
#174543=CARTESIAN_POINT('Ctrl Pts',(8.03933170499995,11.6,-6.57776276800002));
#174544=CARTESIAN_POINT('Ctrl Pts',(8.04018539099994,15.2,-6.57832983600001));
#174545=CARTESIAN_POINT('Ctrl Pts',(8.04018539099994,11.6,-6.57832983600001));
#174546=CARTESIAN_POINT('Ctrl Pts',(8.04104735699994,15.2,-6.57890117200001));
#174547=CARTESIAN_POINT('Ctrl Pts',(8.04104735699994,11.6,-6.57890117200001));
#174548=CARTESIAN_POINT('Ctrl Pts',(8.04191759399994,15.2,-6.57947674700001));
#174549=CARTESIAN_POINT('Ctrl Pts',(8.04191759399994,11.6,-6.57947674700001));
#174550=CARTESIAN_POINT('Ctrl Pts',(8.04279608999994,15.2,-6.58005653200001));
#174551=CARTESIAN_POINT('Ctrl Pts',(8.04279608999994,11.6,-6.58005653200001));
#174552=CARTESIAN_POINT('Ctrl Pts',(8.04368283299995,15.2,-6.58064049900001));
#174553=CARTESIAN_POINT('Ctrl Pts',(8.04368283299995,11.6,-6.58064049900001));
#174554=CARTESIAN_POINT('Ctrl Pts',(8.04457780999994,15.2,-6.58122862000001));
#174555=CARTESIAN_POINT('Ctrl Pts',(8.04457780999994,11.6,-6.58122862000001));
#174556=CARTESIAN_POINT('Ctrl Pts',(8.04548101299994,15.2,-6.58182086700001));
#174557=CARTESIAN_POINT('Ctrl Pts',(8.04548101299994,11.6,-6.58182086700001));
#174558=CARTESIAN_POINT('Ctrl Pts',(8.04639242599994,15.2,-6.58241721200002));
#174559=CARTESIAN_POINT('Ctrl Pts',(8.04639242599994,11.6,-6.58241721200002));
#174560=CARTESIAN_POINT('Ctrl Pts',(8.04731204199994,15.2,-6.58301762600002));
#174561=CARTESIAN_POINT('Ctrl Pts',(8.04731204199994,11.6,-6.58301762600002));
#174562=CARTESIAN_POINT('Ctrl Pts',(8.04823984699994,15.2,-6.58362208200002));
#174563=CARTESIAN_POINT('Ctrl Pts',(8.04823984699994,11.6,-6.58362208200002));
#174564=CARTESIAN_POINT('Ctrl Pts',(8.04917582899994,15.2,-6.58423055400001));
#174565=CARTESIAN_POINT('Ctrl Pts',(8.04917582899994,11.6,-6.58423055400001));
#174566=CARTESIAN_POINT('Ctrl Pts',(8.05011997799994,15.2,-6.58484301200001));
#174567=CARTESIAN_POINT('Ctrl Pts',(8.05011997799994,11.6,-6.58484301200001));
#174568=CARTESIAN_POINT('Ctrl Pts',(8.05107228299994,15.2,-6.58545943100001));
#174569=CARTESIAN_POINT('Ctrl Pts',(8.05107228299994,11.6,-6.58545943100001));
#174570=CARTESIAN_POINT('Ctrl Pts',(8.05203273199995,15.2,-6.58607978300001));
#174571=CARTESIAN_POINT('Ctrl Pts',(8.05203273199995,11.6,-6.58607978300001));
#174572=CARTESIAN_POINT('Ctrl Pts',(8.05300131399994,15.2,-6.58670403900001));
#174573=CARTESIAN_POINT('Ctrl Pts',(8.05300131399994,11.6,-6.58670403900001));
#174574=CARTESIAN_POINT('Ctrl Pts',(8.05397801699994,15.2,-6.58733217500002));
#174575=CARTESIAN_POINT('Ctrl Pts',(8.05397801699994,11.6,-6.58733217500002));
#174576=CARTESIAN_POINT('Ctrl Pts',(8.05496283099994,15.2,-6.58796416400002));
#174577=CARTESIAN_POINT('Ctrl Pts',(8.05496283099994,11.6,-6.58796416400002));
#174578=CARTESIAN_POINT('Ctrl Pts',(8.05595574499994,15.2,-6.58859997700001));
#174579=CARTESIAN_POINT('Ctrl Pts',(8.05595574499994,11.6,-6.58859997700001));
#174580=CARTESIAN_POINT('Ctrl Pts',(8.05695674699994,15.2,-6.58923959000001));
#174581=CARTESIAN_POINT('Ctrl Pts',(8.05695674699994,11.6,-6.58923959000001));
#174582=CARTESIAN_POINT('Ctrl Pts',(8.05796582599994,15.2,-6.58988297500001));
#174583=CARTESIAN_POINT('Ctrl Pts',(8.05796582599994,11.6,-6.58988297500001));
#174584=CARTESIAN_POINT('Ctrl Pts',(8.05898297299994,15.2,-6.59053010600001));
#174585=CARTESIAN_POINT('Ctrl Pts',(8.05898297299994,11.6,-6.59053010600001));
#174586=CARTESIAN_POINT('Ctrl Pts',(8.06000817399994,15.2,-6.59118095800002));
#174587=CARTESIAN_POINT('Ctrl Pts',(8.06000817399994,11.6,-6.59118095800002));
#174588=CARTESIAN_POINT('Ctrl Pts',(8.06104142099995,15.2,-6.59183550400002));
#174589=CARTESIAN_POINT('Ctrl Pts',(8.06104142099995,11.6,-6.59183550400002));
#174590=CARTESIAN_POINT('Ctrl Pts',(8.06208269999994,15.2,-6.59249371900002));
#174591=CARTESIAN_POINT('Ctrl Pts',(8.06208269999994,11.6,-6.59249371900002));
#174592=CARTESIAN_POINT('Ctrl Pts',(8.06313200299994,15.2,-6.59315557600002));
#174593=CARTESIAN_POINT('Ctrl Pts',(8.06313200299994,11.6,-6.59315557600002));
#174594=CARTESIAN_POINT('Ctrl Pts',(8.06418931899995,15.2,-6.59382104900001));
#174595=CARTESIAN_POINT('Ctrl Pts',(8.06418931899995,11.6,-6.59382104900001));
#174596=CARTESIAN_POINT('Ctrl Pts',(8.06525463399994,15.2,-6.59449011500002));
#174597=CARTESIAN_POINT('Ctrl Pts',(8.06525463399994,11.6,-6.59449011500002));
#174598=CARTESIAN_POINT('Ctrl Pts',(8.06632794099994,15.2,-6.59516274600002));
#174599=CARTESIAN_POINT('Ctrl Pts',(8.06632794099994,11.6,-6.59516274600002));
#174600=CARTESIAN_POINT('Ctrl Pts',(8.06740922699994,15.2,-6.59583891700001));
#174601=CARTESIAN_POINT('Ctrl Pts',(8.06740922699994,11.6,-6.59583891700001));
#174602=CARTESIAN_POINT('Ctrl Pts',(8.06849848299994,15.2,-6.59651860500002));
#174603=CARTESIAN_POINT('Ctrl Pts',(8.06849848299994,11.6,-6.59651860500002));
#174604=CARTESIAN_POINT('Ctrl Pts',(8.06959569799995,15.2,-6.59720178200002));
#174605=CARTESIAN_POINT('Ctrl Pts',(8.06959569799995,11.6,-6.59720178200002));
#174606=CARTESIAN_POINT('Ctrl Pts',(8.07070085999994,15.2,-6.59788842600002));
#174607=CARTESIAN_POINT('Ctrl Pts',(8.07070085999994,11.6,-6.59788842600002));
#174608=CARTESIAN_POINT('Ctrl Pts',(8.07181395999994,15.2,-6.59857851000002));
#174609=CARTESIAN_POINT('Ctrl Pts',(8.07181395999994,11.6,-6.59857851000002));
#174610=CARTESIAN_POINT('Ctrl Pts',(8.07293498599994,15.2,-6.59927200900002));
#174611=CARTESIAN_POINT('Ctrl Pts',(8.07293498599994,11.6,-6.59927200900002));
#174612=CARTESIAN_POINT('Ctrl Pts',(8.07406392899994,15.2,-6.59996890000001));
#174613=CARTESIAN_POINT('Ctrl Pts',(8.07406392899994,11.6,-6.59996890000001));
#174614=CARTESIAN_POINT('Ctrl Pts',(8.07520077799994,15.2,-6.60066915900002));
#174615=CARTESIAN_POINT('Ctrl Pts',(8.07520077799994,11.6,-6.60066915900002));
#174616=CARTESIAN_POINT('Ctrl Pts',(8.07634552199995,15.2,-6.60137276000002));
#174617=CARTESIAN_POINT('Ctrl Pts',(8.07634552199995,11.6,-6.60137276000002));
#174618=CARTESIAN_POINT('Ctrl Pts',(8.07749815199994,15.2,-6.60207968000002));
#174619=CARTESIAN_POINT('Ctrl Pts',(8.07749815199994,11.6,-6.60207968000002));
#174620=CARTESIAN_POINT('Ctrl Pts',(8.07865865699995,15.2,-6.60278989300001));
#174621=CARTESIAN_POINT('Ctrl Pts',(8.07865865699995,11.6,-6.60278989300001));
#174622=CARTESIAN_POINT('Ctrl Pts',(8.07982702499995,15.2,-6.60350337600002));
#174623=CARTESIAN_POINT('Ctrl Pts',(8.07982702499995,11.6,-6.60350337600002));
#174624=CARTESIAN_POINT('Ctrl Pts',(8.08100324799994,15.2,-6.60422010600002));
#174625=CARTESIAN_POINT('Ctrl Pts',(8.08100324799994,11.6,-6.60422010600002));
#174626=CARTESIAN_POINT('Ctrl Pts',(8.08218731399995,15.2,-6.60494005800001));
#174627=CARTESIAN_POINT('Ctrl Pts',(8.08218731399995,11.6,-6.60494005800001));
#174628=CARTESIAN_POINT('Ctrl Pts',(8.08337921499995,15.2,-6.60566320800001));
#174629=CARTESIAN_POINT('Ctrl Pts',(8.08337921499995,11.6,-6.60566320800001));
#174630=CARTESIAN_POINT('Ctrl Pts',(8.08457893799994,15.2,-6.60638953300002));
#174631=CARTESIAN_POINT('Ctrl Pts',(8.08457893799994,11.6,-6.60638953300002));
#174632=CARTESIAN_POINT('Ctrl Pts',(8.08578647499994,15.2,-6.60711901000001));
#174633=CARTESIAN_POINT('Ctrl Pts',(8.08578647499994,11.6,-6.60711901000001));
#174634=CARTESIAN_POINT('Ctrl Pts',(8.08700181499994,15.2,-6.60785161500002));
#174635=CARTESIAN_POINT('Ctrl Pts',(8.08700181499994,11.6,-6.60785161500002));
#174636=CARTESIAN_POINT('Ctrl Pts',(8.08822494799994,15.2,-6.60858732400002));
#174637=CARTESIAN_POINT('Ctrl Pts',(8.08822494799994,11.6,-6.60858732400002));
#174638=CARTESIAN_POINT('Ctrl Pts',(8.08945586299994,15.2,-6.60932611600002));
#174639=CARTESIAN_POINT('Ctrl Pts',(8.08945586299994,11.6,-6.60932611600002));
#174640=CARTESIAN_POINT('Ctrl Pts',(8.09069455099995,15.2,-6.61006796600002));
#174641=CARTESIAN_POINT('Ctrl Pts',(8.09069455099995,11.6,-6.61006796600002));
#174642=CARTESIAN_POINT('Ctrl Pts',(8.09194100299995,15.2,-6.61081285000002));
#174643=CARTESIAN_POINT('Ctrl Pts',(8.09194100299995,11.6,-6.61081285000002));
#174644=CARTESIAN_POINT('Ctrl Pts',(8.09319520699994,15.2,-6.61156074800001));
#174645=CARTESIAN_POINT('Ctrl Pts',(8.09319520699994,11.6,-6.61156074800001));
#174646=CARTESIAN_POINT('Ctrl Pts',(8.09445715399994,15.2,-6.61231163600001));
#174647=CARTESIAN_POINT('Ctrl Pts',(8.09445715399994,11.6,-6.61231163600001));
#174648=CARTESIAN_POINT('Ctrl Pts',(8.09572683299994,15.2,-6.61306549100001));
#174649=CARTESIAN_POINT('Ctrl Pts',(8.09572683299994,11.6,-6.61306549100001));
#174650=CARTESIAN_POINT('Ctrl Pts',(8.09700423599995,15.2,-6.61382228900001));
#174651=CARTESIAN_POINT('Ctrl Pts',(8.09700423599995,11.6,-6.61382228900001));
#174652=CARTESIAN_POINT('Ctrl Pts',(8.09828935199995,15.2,-6.61458201000002));
#174653=CARTESIAN_POINT('Ctrl Pts',(8.09828935199995,11.6,-6.61458201000002));
#174654=CARTESIAN_POINT('Ctrl Pts',(8.09958216999994,15.2,-6.61534463100002));
#174655=CARTESIAN_POINT('Ctrl Pts',(8.09958216999994,11.6,-6.61534463100002));
#174656=CARTESIAN_POINT('Ctrl Pts',(8.10088268299994,15.2,-6.61611012900002));
#174657=CARTESIAN_POINT('Ctrl Pts',(8.10088268299994,11.6,-6.61611012900002));
#174658=CARTESIAN_POINT('Ctrl Pts',(8.10219087899995,15.2,-6.61687848200001));
#174659=CARTESIAN_POINT('Ctrl Pts',(8.10219087899995,11.6,-6.61687848200001));
#174660=CARTESIAN_POINT('Ctrl Pts',(8.10350674899994,15.2,-6.61764966700002));
#174661=CARTESIAN_POINT('Ctrl Pts',(8.10350674899994,11.6,-6.61764966700002));
#174662=CARTESIAN_POINT('Ctrl Pts',(8.10483028199994,15.2,-6.61842366300001));
#174663=CARTESIAN_POINT('Ctrl Pts',(8.10483028199994,11.6,-6.61842366300001));
#174664=CARTESIAN_POINT('Ctrl Pts',(8.10616147099994,15.2,-6.61920044900001));
#174665=CARTESIAN_POINT('Ctrl Pts',(8.10616147099994,11.6,-6.61920044900001));
#174666=CARTESIAN_POINT('Ctrl Pts',(8.10750030299995,15.2,-6.61998000200001));
#174667=CARTESIAN_POINT('Ctrl Pts',(8.10750030299995,11.6,-6.61998000200001));
#174668=CARTESIAN_POINT('Ctrl Pts',(8.10884677199994,15.2,-6.62076229900002));
#174669=CARTESIAN_POINT('Ctrl Pts',(8.10884677199994,11.6,-6.62076229900002));
#174670=CARTESIAN_POINT('Ctrl Pts',(8.11020086499994,15.2,-6.62154732200002));
#174671=CARTESIAN_POINT('Ctrl Pts',(8.11020086499994,11.6,-6.62154732200002));
#174672=CARTESIAN_POINT('Ctrl Pts',(8.11156257299994,15.2,-6.62233504500002));
#174673=CARTESIAN_POINT('Ctrl Pts',(8.11156257299994,11.6,-6.62233504500002));
#174674=CARTESIAN_POINT('Ctrl Pts',(8.11293188799995,15.2,-6.62312544900002));
#174675=CARTESIAN_POINT('Ctrl Pts',(8.11293188799995,11.6,-6.62312544900002));
#174676=CARTESIAN_POINT('Ctrl Pts',(8.11430879999994,15.2,-6.62391851300002));
#174677=CARTESIAN_POINT('Ctrl Pts',(8.11430879999994,11.6,-6.62391851300002));
#174678=CARTESIAN_POINT('Ctrl Pts',(8.11569329999994,15.2,-6.62471421500002));
#174679=CARTESIAN_POINT('Ctrl Pts',(8.11569329999994,11.6,-6.62471421500002));
#174680=CARTESIAN_POINT('Ctrl Pts',(8.11708537499995,15.2,-6.62551253400002));
#174681=CARTESIAN_POINT('Ctrl Pts',(8.11708537499995,11.6,-6.62551253400002));
#174682=CARTESIAN_POINT('Ctrl Pts',(8.11848501999994,15.2,-6.62631344700002));
#174683=CARTESIAN_POINT('Ctrl Pts',(8.11848501999994,11.6,-6.62631344700002));
#174684=CARTESIAN_POINT('Ctrl Pts',(8.11989222299994,15.2,-6.62711693700002));
#174685=CARTESIAN_POINT('Ctrl Pts',(8.11989222299994,11.6,-6.62711693700002));
#174686=CARTESIAN_POINT('Ctrl Pts',(8.12130697599994,15.2,-6.62792297900002));
#174687=CARTESIAN_POINT('Ctrl Pts',(8.12130697599994,11.6,-6.62792297900002));
#174688=CARTESIAN_POINT('Ctrl Pts',(8.12272926799994,15.2,-6.62873155500002));
#174689=CARTESIAN_POINT('Ctrl Pts',(8.12272926799994,11.6,-6.62873155500002));
#174690=CARTESIAN_POINT('Ctrl Pts',(8.12415908999995,15.2,-6.62954264200001));
#174691=CARTESIAN_POINT('Ctrl Pts',(8.12415908999995,11.6,-6.62954264200001));
#174692=CARTESIAN_POINT('Ctrl Pts',(8.12559643299995,15.2,-6.63035622100002));
#174693=CARTESIAN_POINT('Ctrl Pts',(8.12559643299995,11.6,-6.63035622100002));
#174694=CARTESIAN_POINT('Ctrl Pts',(8.12704128799994,15.2,-6.63117227000001));
#174695=CARTESIAN_POINT('Ctrl Pts',(8.12704128799994,11.6,-6.63117227000001));
#174696=CARTESIAN_POINT('Ctrl Pts',(8.12849364599994,15.2,-6.63199077000002));
#174697=CARTESIAN_POINT('Ctrl Pts',(8.12849364599994,11.6,-6.63199077000002));
#174698=CARTESIAN_POINT('Ctrl Pts',(8.12995349699994,15.2,-6.63281170000002));
#174699=CARTESIAN_POINT('Ctrl Pts',(8.12995349699994,11.6,-6.63281170000002));
#174700=CARTESIAN_POINT('Ctrl Pts',(8.13142083099994,15.2,-6.63363503900002));
#174701=CARTESIAN_POINT('Ctrl Pts',(8.13142083099994,11.6,-6.63363503900002));
#174702=CARTESIAN_POINT('Ctrl Pts',(8.13289563999994,15.2,-6.63446076700002));
#174703=CARTESIAN_POINT('Ctrl Pts',(8.13289563999994,11.6,-6.63446076700002));
#174704=CARTESIAN_POINT('Ctrl Pts',(8.13437791499994,15.2,-6.63528886500002));
#174705=CARTESIAN_POINT('Ctrl Pts',(8.13437791499994,11.6,-6.63528886500002));
#174706=CARTESIAN_POINT('Ctrl Pts',(8.13586764499994,15.2,-6.63611931100001));
#174707=CARTESIAN_POINT('Ctrl Pts',(8.13586764499994,11.6,-6.63611931100001));
#174708=CARTESIAN_POINT('Ctrl Pts',(8.13736482299995,15.2,-6.63695208700001));
#174709=CARTESIAN_POINT('Ctrl Pts',(8.13736482299995,11.6,-6.63695208700001));
#174710=CARTESIAN_POINT('Ctrl Pts',(8.13886943899995,15.2,-6.63778717100002));
#174711=CARTESIAN_POINT('Ctrl Pts',(8.13886943899995,11.6,-6.63778717100002));
#174712=CARTESIAN_POINT('Ctrl Pts',(8.14038148299994,15.2,-6.63862454400002));
#174713=CARTESIAN_POINT('Ctrl Pts',(8.14038148299994,11.6,-6.63862454400002));
#174714=CARTESIAN_POINT('Ctrl Pts',(8.14190094599994,15.2,-6.63946418600001));
#174715=CARTESIAN_POINT('Ctrl Pts',(8.14190094599994,11.6,-6.63946418600001));
#174716=CARTESIAN_POINT('Ctrl Pts',(8.14342782099994,15.2,-6.64030607900001));
#174717=CARTESIAN_POINT('Ctrl Pts',(8.14342782099994,11.6,-6.64030607900001));
#174718=CARTESIAN_POINT('Ctrl Pts',(8.14496209699995,15.2,-6.64115020100001));
#174719=CARTESIAN_POINT('Ctrl Pts',(8.14496209699995,11.6,-6.64115020100001));
#174720=CARTESIAN_POINT('Ctrl Pts',(8.14650376499995,15.2,-6.64199653400001));
#174721=CARTESIAN_POINT('Ctrl Pts',(8.14650376499995,11.6,-6.64199653400001));
#174722=CARTESIAN_POINT('Ctrl Pts',(8.14805281799994,15.2,-6.64284505700002));
#174723=CARTESIAN_POINT('Ctrl Pts',(8.14805281799994,11.6,-6.64284505700002));
#174724=CARTESIAN_POINT('Ctrl Pts',(8.14960924299994,15.2,-6.64369575200002));
#174725=CARTESIAN_POINT('Ctrl Pts',(8.14960924299994,11.6,-6.64369575200002));
#174726=CARTESIAN_POINT('Ctrl Pts',(8.15117303599994,15.2,-6.64454860000002));
#174727=CARTESIAN_POINT('Ctrl Pts',(8.15117303599994,11.6,-6.64454860000002));
#174728=CARTESIAN_POINT('Ctrl Pts',(8.15274418299994,15.2,-6.64540358000002));
#174729=CARTESIAN_POINT('Ctrl Pts',(8.15274418299994,11.6,-6.64540358000002));
#174730=CARTESIAN_POINT('Ctrl Pts',(8.15432267899994,15.2,-6.64626067400001));
#174731=CARTESIAN_POINT('Ctrl Pts',(8.15432267899994,11.6,-6.64626067400001));
#174732=CARTESIAN_POINT('Ctrl Pts',(8.15590851399994,15.2,-6.64711986300001));
#174733=CARTESIAN_POINT('Ctrl Pts',(8.15590851399994,11.6,-6.64711986300001));
#174734=CARTESIAN_POINT('Ctrl Pts',(8.15750167799994,15.2,-6.64798112700002));
#174735=CARTESIAN_POINT('Ctrl Pts',(8.15750167799994,11.6,-6.64798112700002));
#174736=CARTESIAN_POINT('Ctrl Pts',(8.15910216299994,15.2,-6.64884444900002));
#174737=CARTESIAN_POINT('Ctrl Pts',(8.15910216299994,11.6,-6.64884444900002));
#174738=CARTESIAN_POINT('Ctrl Pts',(8.16070995999995,15.2,-6.64970980800001));
#174739=CARTESIAN_POINT('Ctrl Pts',(8.16070995999995,11.6,-6.64970980800001));
#174740=CARTESIAN_POINT('Ctrl Pts',(8.16232505999994,15.2,-6.65057718600002));
#174741=CARTESIAN_POINT('Ctrl Pts',(8.16232505999994,11.6,-6.65057718600002));
#174742=CARTESIAN_POINT('Ctrl Pts',(8.16394745599995,15.2,-6.65144656500001));
#174743=CARTESIAN_POINT('Ctrl Pts',(8.16394745599995,11.6,-6.65144656500001));
#174744=CARTESIAN_POINT('Ctrl Pts',(8.16557713499994,15.2,-6.65231792500002));
#174745=CARTESIAN_POINT('Ctrl Pts',(8.16557713499994,11.6,-6.65231792500002));
#174746=CARTESIAN_POINT('Ctrl Pts',(8.16721409299995,15.2,-6.65319124900002));
#174747=CARTESIAN_POINT('Ctrl Pts',(8.16721409299995,11.6,-6.65319124900002));
#174748=CARTESIAN_POINT('Ctrl Pts',(8.16885831799994,15.2,-6.65406651700001));
#174749=CARTESIAN_POINT('Ctrl Pts',(8.16885831799994,11.6,-6.65406651700001));
#174750=CARTESIAN_POINT('Ctrl Pts',(8.17050980299994,15.2,-6.65494371200002));
#174751=CARTESIAN_POINT('Ctrl Pts',(8.17050980299994,11.6,-6.65494371200002));
#174752=CARTESIAN_POINT('Ctrl Pts',(8.17216853799994,15.2,-6.65582281300001));
#174753=CARTESIAN_POINT('Ctrl Pts',(8.17216853799994,11.6,-6.65582281300001));
#174754=CARTESIAN_POINT('Ctrl Pts',(8.17383451599994,15.2,-6.65670380500002));
#174755=CARTESIAN_POINT('Ctrl Pts',(8.17383451599994,11.6,-6.65670380500002));
#174756=CARTESIAN_POINT('Ctrl Pts',(8.17550772699994,15.2,-6.65758666800001));
#174757=CARTESIAN_POINT('Ctrl Pts',(8.17550772699994,11.6,-6.65758666800001));
#174758=CARTESIAN_POINT('Ctrl Pts',(8.17718816199994,15.2,-6.65847138400002));
#174759=CARTESIAN_POINT('Ctrl Pts',(8.17718816199994,11.6,-6.65847138400002));
#174760=CARTESIAN_POINT('Ctrl Pts',(8.17887581399994,15.2,-6.65935793500001));
#174761=CARTESIAN_POINT('Ctrl Pts',(8.17887581399994,11.6,-6.65935793500001));
#174762=CARTESIAN_POINT('Ctrl Pts',(8.18057067299995,15.2,-6.66024630300001));
#174763=CARTESIAN_POINT('Ctrl Pts',(8.18057067299995,11.6,-6.66024630300001));
#174764=CARTESIAN_POINT('Ctrl Pts',(8.18227273099994,15.2,-6.66113646900002));
#174765=CARTESIAN_POINT('Ctrl Pts',(8.18227273099994,11.6,-6.66113646900002));
#174766=CARTESIAN_POINT('Ctrl Pts',(8.18398197899995,15.2,-6.66202841800001));
#174767=CARTESIAN_POINT('Ctrl Pts',(8.18398197899995,11.6,-6.66202841800001));
#174768=CARTESIAN_POINT('Ctrl Pts',(8.18569840899994,15.2,-6.66292212900002));
#174769=CARTESIAN_POINT('Ctrl Pts',(8.18569840899994,11.6,-6.66292212900002));
#174770=CARTESIAN_POINT('Ctrl Pts',(8.18742201199994,15.2,-6.66381758700001));
#174771=CARTESIAN_POINT('Ctrl Pts',(8.18742201199994,11.6,-6.66381758700001));
#174772=CARTESIAN_POINT('Ctrl Pts',(8.18915277999994,15.2,-6.66471477100002));
#174773=CARTESIAN_POINT('Ctrl Pts',(8.18915277999994,11.6,-6.66471477100002));
#174774=CARTESIAN_POINT('Ctrl Pts',(8.19089070299994,15.2,-6.66561366600002));
#174775=CARTESIAN_POINT('Ctrl Pts',(8.19089070299994,11.6,-6.66561366600002));
#174776=CARTESIAN_POINT('Ctrl Pts',(8.19263577499994,15.2,-6.66651425400002));
#174777=CARTESIAN_POINT('Ctrl Pts',(8.19263577499994,11.6,-6.66651425400002));
#174778=CARTESIAN_POINT('Ctrl Pts',(8.19438798599995,15.2,-6.66741651700002));
#174779=CARTESIAN_POINT('Ctrl Pts',(8.19438798599995,11.6,-6.66741651700002));
#174780=CARTESIAN_POINT('Ctrl Pts',(8.19614732799994,15.2,-6.66832043800002));
#174781=CARTESIAN_POINT('Ctrl Pts',(8.19614732799994,11.6,-6.66832043800002));
#174782=CARTESIAN_POINT('Ctrl Pts',(8.19791379199994,15.2,-6.66922599900002));
#174783=CARTESIAN_POINT('Ctrl Pts',(8.19791379199994,11.6,-6.66922599900002));
#174784=CARTESIAN_POINT('Ctrl Pts',(8.19968736899994,15.2,-6.67013318300001));
#174785=CARTESIAN_POINT('Ctrl Pts',(8.19968736899994,11.6,-6.67013318300001));
#174786=CARTESIAN_POINT('Ctrl Pts',(8.20146805299995,15.2,-6.67104197300001));
#174787=CARTESIAN_POINT('Ctrl Pts',(8.20146805299995,11.6,-6.67104197300001));
#174788=CARTESIAN_POINT('Ctrl Pts',(8.20325583299994,15.2,-6.67195235100002));
#174789=CARTESIAN_POINT('Ctrl Pts',(8.20325583299994,11.6,-6.67195235100002));
#174790=CARTESIAN_POINT('Ctrl Pts',(8.20505070199994,15.2,-6.67286430200001));
#174791=CARTESIAN_POINT('Ctrl Pts',(8.20505070199994,11.6,-6.67286430200001));
#174792=CARTESIAN_POINT('Ctrl Pts',(8.20685265099995,15.2,-6.67377780700001));
#174793=CARTESIAN_POINT('Ctrl Pts',(8.20685265099995,11.6,-6.67377780700001));
#174794=CARTESIAN_POINT('Ctrl Pts',(8.20866167299994,15.2,-6.67469284900001));
#174795=CARTESIAN_POINT('Ctrl Pts',(8.20866167299994,11.6,-6.67469284900001));
#174796=CARTESIAN_POINT('Ctrl Pts',(8.21047775899994,15.2,-6.67560941200002));
#174797=CARTESIAN_POINT('Ctrl Pts',(8.21047775899994,11.6,-6.67560941200002));
#174798=CARTESIAN_POINT('Ctrl Pts',(8.21230089999995,15.2,-6.67652747800001));
#174799=CARTESIAN_POINT('Ctrl Pts',(8.21230089999995,11.6,-6.67652747800001));
#174800=CARTESIAN_POINT('Ctrl Pts',(8.21413108799995,15.2,-6.67744703200002));
#174801=CARTESIAN_POINT('Ctrl Pts',(8.21413108799995,11.6,-6.67744703200002));
#174802=CARTESIAN_POINT('Ctrl Pts',(8.21596831499994,15.2,-6.67836805600002));
#174803=CARTESIAN_POINT('Ctrl Pts',(8.21596831499994,11.6,-6.67836805600002));
#174804=CARTESIAN_POINT('Ctrl Pts',(8.21781257299994,15.2,-6.67929053200002));
#174805=CARTESIAN_POINT('Ctrl Pts',(8.21781257299994,11.6,-6.67929053200002));
#174806=CARTESIAN_POINT('Ctrl Pts',(8.21966385399995,15.2,-6.68021444700001));
#174807=CARTESIAN_POINT('Ctrl Pts',(8.21966385399995,11.6,-6.68021444700001));
#174808=CARTESIAN_POINT('Ctrl Pts',(8.22152214799994,15.2,-6.68113978100001));
#174809=CARTESIAN_POINT('Ctrl Pts',(8.22152214799994,11.6,-6.68113978100001));
#174810=CARTESIAN_POINT('Ctrl Pts',(8.22338744899995,15.2,-6.68206651900002));
#174811=CARTESIAN_POINT('Ctrl Pts',(8.22338744899995,11.6,-6.68206651900002));
#174812=CARTESIAN_POINT('Ctrl Pts',(8.22525974799994,15.2,-6.68299464400001));
#174813=CARTESIAN_POINT('Ctrl Pts',(8.22525974799994,11.6,-6.68299464400001));
#174814=CARTESIAN_POINT('Ctrl Pts',(8.22713903599994,15.2,-6.68392414100002));
#174815=CARTESIAN_POINT('Ctrl Pts',(8.22713903599994,11.6,-6.68392414100002));
#174816=CARTESIAN_POINT('Ctrl Pts',(8.22902530599994,15.2,-6.68485499200001));
#174817=CARTESIAN_POINT('Ctrl Pts',(8.22902530599994,11.6,-6.68485499200001));
#174818=CARTESIAN_POINT('Ctrl Pts',(8.23091854999995,15.2,-6.68578718100001));
#174819=CARTESIAN_POINT('Ctrl Pts',(8.23091854999995,11.6,-6.68578718100001));
#174820=CARTESIAN_POINT('Ctrl Pts',(8.23281875799994,15.2,-6.68672069200002));
#174821=CARTESIAN_POINT('Ctrl Pts',(8.23281875799994,11.6,-6.68672069200002));
#174822=CARTESIAN_POINT('Ctrl Pts',(8.23472592499994,15.2,-6.68765551000002));
#174823=CARTESIAN_POINT('Ctrl Pts',(8.23472592499994,11.6,-6.68765551000002));
#174824=CARTESIAN_POINT('Ctrl Pts',(8.23664004099994,15.2,-6.68859161700002));
#174825=CARTESIAN_POINT('Ctrl Pts',(8.23664004099994,11.6,-6.68859161700002));
#174826=CARTESIAN_POINT('Ctrl Pts',(8.23856109699994,15.2,-6.68952899800002));
#174827=CARTESIAN_POINT('Ctrl Pts',(8.23856109699994,11.6,-6.68952899800002));
#174828=CARTESIAN_POINT('Ctrl Pts',(8.24048908699995,15.2,-6.69046763800001));
#174829=CARTESIAN_POINT('Ctrl Pts',(8.24048908699995,11.6,-6.69046763800001));
#174830=CARTESIAN_POINT('Ctrl Pts',(8.24242400099994,15.2,-6.69140751800001));
#174831=CARTESIAN_POINT('Ctrl Pts',(8.24242400099994,11.6,-6.69140751800001));
#174832=CARTESIAN_POINT('Ctrl Pts',(8.24436583299994,15.2,-6.69234862500002));
#174833=CARTESIAN_POINT('Ctrl Pts',(8.24436583299994,11.6,-6.69234862500002));
#174834=CARTESIAN_POINT('Ctrl Pts',(8.24631457299994,15.2,-6.69329094200001));
#174835=CARTESIAN_POINT('Ctrl Pts',(8.24631457299994,11.6,-6.69329094200001));
#174836=CARTESIAN_POINT('Ctrl Pts',(8.24827021499994,15.2,-6.69423445400002));
#174837=CARTESIAN_POINT('Ctrl Pts',(8.24827021499994,11.6,-6.69423445400002));
#174838=CARTESIAN_POINT('Ctrl Pts',(8.25023274999995,15.2,-6.69517914500001));
#174839=CARTESIAN_POINT('Ctrl Pts',(8.25023274999995,11.6,-6.69517914500001));
#174840=CARTESIAN_POINT('Ctrl Pts',(8.25220216899995,15.2,-6.69612499700002));
#174841=CARTESIAN_POINT('Ctrl Pts',(8.25220216899995,11.6,-6.69612499700002));
#174842=CARTESIAN_POINT('Ctrl Pts',(8.25417846599995,15.2,-6.69707199800002));
#174843=CARTESIAN_POINT('Ctrl Pts',(8.25417846599995,11.6,-6.69707199800002));
#174844=CARTESIAN_POINT('Ctrl Pts',(8.25616163199994,15.2,-6.69802013100002));
#174845=CARTESIAN_POINT('Ctrl Pts',(8.25616163199994,11.6,-6.69802013100002));
#174846=CARTESIAN_POINT('Ctrl Pts',(8.25815165799994,15.2,-6.69896938100001));
#174847=CARTESIAN_POINT('Ctrl Pts',(8.25815165799994,11.6,-6.69896938100001));
#174848=CARTESIAN_POINT('Ctrl Pts',(8.26014853899995,15.2,-6.69991973000001));
#174849=CARTESIAN_POINT('Ctrl Pts',(8.26014853899995,11.6,-6.69991973000001));
#174850=CARTESIAN_POINT('Ctrl Pts',(8.26215226399994,15.2,-6.70087116600002));
#174851=CARTESIAN_POINT('Ctrl Pts',(8.26215226399994,11.6,-6.70087116600002));
#174852=CARTESIAN_POINT('Ctrl Pts',(8.26416282699994,15.2,-6.70182367200002));
#174853=CARTESIAN_POINT('Ctrl Pts',(8.26416282699994,11.6,-6.70182367200002));
#174854=CARTESIAN_POINT('Ctrl Pts',(8.26618022099994,15.2,-6.70277723300002));
#174855=CARTESIAN_POINT('Ctrl Pts',(8.26618022099994,11.6,-6.70277723300002));
#174856=CARTESIAN_POINT('Ctrl Pts',(8.26820443599994,15.2,-6.70373183400002));
#174857=CARTESIAN_POINT('Ctrl Pts',(8.26820443599994,11.6,-6.70373183400002));
#174858=CARTESIAN_POINT('Ctrl Pts',(8.27023546499994,15.2,-6.70468746000001));
#174859=CARTESIAN_POINT('Ctrl Pts',(8.27023546499994,11.6,-6.70468746000001));
#174860=CARTESIAN_POINT('Ctrl Pts',(8.27227329999995,15.2,-6.70564409400002));
#174861=CARTESIAN_POINT('Ctrl Pts',(8.27227329999995,11.6,-6.70564409400002));
#174862=CARTESIAN_POINT('Ctrl Pts',(8.27431793299995,15.2,-6.70660172400002));
#174863=CARTESIAN_POINT('Ctrl Pts',(8.27431793299995,11.6,-6.70660172400002));
#174864=CARTESIAN_POINT('Ctrl Pts',(8.27636935699994,15.2,-6.70756033100002));
#174865=CARTESIAN_POINT('Ctrl Pts',(8.27636935699994,11.6,-6.70756033100002));
#174866=CARTESIAN_POINT('Ctrl Pts',(8.27842756399994,15.2,-6.70851990500001));
#174867=CARTESIAN_POINT('Ctrl Pts',(8.27842756399994,11.6,-6.70851990500001));
#174868=CARTESIAN_POINT('Ctrl Pts',(8.28049254599994,15.2,-6.70948042700001));
#174869=CARTESIAN_POINT('Ctrl Pts',(8.28049254599994,11.6,-6.70948042700001));
#174870=CARTESIAN_POINT('Ctrl Pts',(8.28256429399995,15.2,-6.71044188300002));
#174871=CARTESIAN_POINT('Ctrl Pts',(8.28256429399995,11.6,-6.71044188300002));
#174872=CARTESIAN_POINT('Ctrl Pts',(8.28464280299994,15.2,-6.71140425900001));
#174873=CARTESIAN_POINT('Ctrl Pts',(8.28464280299994,11.6,-6.71140425900001));
#174874=CARTESIAN_POINT('Ctrl Pts',(8.28672806299994,15.2,-6.71236754000001));
#174875=CARTESIAN_POINT('Ctrl Pts',(8.28672806299994,11.6,-6.71236754000001));
#174876=CARTESIAN_POINT('Ctrl Pts',(8.28882006799994,15.2,-6.71333171200001));
#174877=CARTESIAN_POINT('Ctrl Pts',(8.28882006799994,11.6,-6.71333171200001));
#174878=CARTESIAN_POINT('Ctrl Pts',(8.29091880799994,15.2,-6.71429675900002));
#174879=CARTESIAN_POINT('Ctrl Pts',(8.29091880799994,11.6,-6.71429675900002));
#174880=CARTESIAN_POINT('Ctrl Pts',(8.29302427799994,15.2,-6.71526266700001));
#174881=CARTESIAN_POINT('Ctrl Pts',(8.29302427799994,11.6,-6.71526266700001));
#174882=CARTESIAN_POINT('Ctrl Pts',(8.29513646899994,15.2,-6.71622942100001));
#174883=CARTESIAN_POINT('Ctrl Pts',(8.29513646899994,11.6,-6.71622942100001));
#174884=CARTESIAN_POINT('Ctrl Pts',(8.29725537199994,15.2,-6.71719700700002));
#174885=CARTESIAN_POINT('Ctrl Pts',(8.29725537199994,11.6,-6.71719700700002));
#174886=CARTESIAN_POINT('Ctrl Pts',(8.29938098199994,15.2,-6.71816541100001));
#174887=CARTESIAN_POINT('Ctrl Pts',(8.29938098199994,11.6,-6.71816541100001));
#174888=CARTESIAN_POINT('Ctrl Pts',(8.30151328999994,15.2,-6.71913461700001));
#174889=CARTESIAN_POINT('Ctrl Pts',(8.30151328999994,11.6,-6.71913461700001));
#174890=CARTESIAN_POINT('Ctrl Pts',(8.30365228799994,15.2,-6.72010461100002));
#174891=CARTESIAN_POINT('Ctrl Pts',(8.30365228799994,11.6,-6.72010461100002));
#174892=CARTESIAN_POINT('Ctrl Pts',(8.30579796699995,15.2,-6.72107538000001));
#174893=CARTESIAN_POINT('Ctrl Pts',(8.30579796699995,11.6,-6.72107538000001));
#174894=CARTESIAN_POINT('Ctrl Pts',(8.30795032399994,15.2,-6.72204690800001));
#174895=CARTESIAN_POINT('Ctrl Pts',(8.30795032399994,11.6,-6.72204690800001));
#174896=CARTESIAN_POINT('Ctrl Pts',(8.31010934699994,15.2,-6.72301918300001));
#174897=CARTESIAN_POINT('Ctrl Pts',(8.31010934699994,11.6,-6.72301918300001));
#174898=CARTESIAN_POINT('Ctrl Pts',(8.31227502999995,15.2,-6.72399218800001));
#174899=CARTESIAN_POINT('Ctrl Pts',(8.31227502999995,11.6,-6.72399218800001));
#174900=CARTESIAN_POINT('Ctrl Pts',(8.31444736699994,15.2,-6.72496591100002));
#174901=CARTESIAN_POINT('Ctrl Pts',(8.31444736699994,11.6,-6.72496591100002));
#174902=CARTESIAN_POINT('Ctrl Pts',(8.31662634799994,15.2,-6.72594033700002));
#174903=CARTESIAN_POINT('Ctrl Pts',(8.31662634799994,11.6,-6.72594033700002));
#174904=CARTESIAN_POINT('Ctrl Pts',(8.31881196599995,15.2,-6.72691545200002));
#174905=CARTESIAN_POINT('Ctrl Pts',(8.31881196599995,11.6,-6.72691545200002));
#174906=CARTESIAN_POINT('Ctrl Pts',(8.32100421399995,15.2,-6.72789124100002));
#174907=CARTESIAN_POINT('Ctrl Pts',(8.32100421399995,11.6,-6.72789124100002));
#174908=CARTESIAN_POINT('Ctrl Pts',(8.32320308399994,15.2,-6.72886769200002));
#174909=CARTESIAN_POINT('Ctrl Pts',(8.32320308399994,11.6,-6.72886769200002));
#174910=CARTESIAN_POINT('Ctrl Pts',(8.32540856899995,15.2,-6.72984479000001));
#174911=CARTESIAN_POINT('Ctrl Pts',(8.32540856899995,11.6,-6.72984479000001));
#174912=CARTESIAN_POINT('Ctrl Pts',(8.32762066299994,15.2,-6.73082252200001));
#174913=CARTESIAN_POINT('Ctrl Pts',(8.32762066299994,11.6,-6.73082252200001));
#174914=CARTESIAN_POINT('Ctrl Pts',(8.32983935499995,15.2,-6.73180087200001));
#174915=CARTESIAN_POINT('Ctrl Pts',(8.32983935499995,11.6,-6.73180087200001));
#174916=CARTESIAN_POINT('Ctrl Pts',(8.33206463999994,15.2,-6.73277982900002));
#174917=CARTESIAN_POINT('Ctrl Pts',(8.33206463999994,11.6,-6.73277982900002));
#174918=CARTESIAN_POINT('Ctrl Pts',(8.33429650899994,15.2,-6.73375937700002));
#174919=CARTESIAN_POINT('Ctrl Pts',(8.33429650899994,11.6,-6.73375937700002));
#174920=CARTESIAN_POINT('Ctrl Pts',(8.33653495599994,15.2,-6.73473950400002));
#174921=CARTESIAN_POINT('Ctrl Pts',(8.33653495599994,11.6,-6.73473950400002));
#174922=CARTESIAN_POINT('Ctrl Pts',(8.33877997299994,15.2,-6.73572019500002));
#174923=CARTESIAN_POINT('Ctrl Pts',(8.33877997299994,11.6,-6.73572019500002));
#174924=CARTESIAN_POINT('Ctrl Pts',(8.34103155399994,15.2,-6.73670143600001));
#174925=CARTESIAN_POINT('Ctrl Pts',(8.34103155399994,11.6,-6.73670143600001));
#174926=CARTESIAN_POINT('Ctrl Pts',(8.34328968799994,15.2,-6.73768321600001));
#174927=CARTESIAN_POINT('Ctrl Pts',(8.34328968799994,11.6,-6.73768321600001));
#174928=CARTESIAN_POINT('Ctrl Pts',(8.34555437099995,15.2,-6.73866551800002));
#174929=CARTESIAN_POINT('Ctrl Pts',(8.34555437099995,11.6,-6.73866551800002));
#174930=CARTESIAN_POINT('Ctrl Pts',(8.34782559499994,15.2,-6.73964833200002));
#174931=CARTESIAN_POINT('Ctrl Pts',(8.34782559499994,11.6,-6.73964833200002));
#174932=CARTESIAN_POINT('Ctrl Pts',(8.35010335099994,15.2,-6.74063164200001));
#174933=CARTESIAN_POINT('Ctrl Pts',(8.35010335099994,11.6,-6.74063164200001));
#174934=CARTESIAN_POINT('Ctrl Pts',(8.35238763299994,15.2,-6.74161543600002));
#174935=CARTESIAN_POINT('Ctrl Pts',(8.35238763299994,11.6,-6.74161543600002));
#174936=CARTESIAN_POINT('Ctrl Pts',(8.35467843299995,15.2,-6.74259969900002));
#174937=CARTESIAN_POINT('Ctrl Pts',(8.35467843299995,11.6,-6.74259969900002));
#174938=CARTESIAN_POINT('Ctrl Pts',(8.35697574399994,15.2,-6.74358442000001));
#174939=CARTESIAN_POINT('Ctrl Pts',(8.35697574399994,11.6,-6.74358442000001));
#174940=CARTESIAN_POINT('Ctrl Pts',(8.35927955899994,15.2,-6.74456958300001));
#174941=CARTESIAN_POINT('Ctrl Pts',(8.35927955899994,11.6,-6.74456958300001));
#174942=CARTESIAN_POINT('Ctrl Pts',(8.36158986899994,15.2,-6.74555517700002));
#174943=CARTESIAN_POINT('Ctrl Pts',(8.36158986899994,11.6,-6.74555517700002));
#174944=CARTESIAN_POINT('Ctrl Pts',(8.36390666999994,15.2,-6.74654118800002));
#174945=CARTESIAN_POINT('Ctrl Pts',(8.36390666999994,11.6,-6.74654118800002));
#174946=CARTESIAN_POINT('Ctrl Pts',(8.36622995199994,15.2,-6.74752760300001));
#174947=CARTESIAN_POINT('Ctrl Pts',(8.36622995199994,11.6,-6.74752760300001));
#174948=CARTESIAN_POINT('Ctrl Pts',(8.36855970799994,15.2,-6.74851440900002));
#174949=CARTESIAN_POINT('Ctrl Pts',(8.36855970799994,11.6,-6.74851440900002));
#174950=CARTESIAN_POINT('Ctrl Pts',(8.37089593099994,15.2,-6.74950159200002));
#174951=CARTESIAN_POINT('Ctrl Pts',(8.37089593099994,11.6,-6.74950159200002));
#174952=CARTESIAN_POINT('Ctrl Pts',(8.37323861399994,15.2,-6.75048914100002));
#174953=CARTESIAN_POINT('Ctrl Pts',(8.37323861399994,11.6,-6.75048914100002));
#174954=CARTESIAN_POINT('Ctrl Pts',(8.37558774999994,15.2,-6.75147704100001));
#174955=CARTESIAN_POINT('Ctrl Pts',(8.37558774999994,11.6,-6.75147704100001));
#174956=CARTESIAN_POINT('Ctrl Pts',(8.37794332999995,15.2,-6.75246527900002));
#174957=CARTESIAN_POINT('Ctrl Pts',(8.37794332999995,11.6,-6.75246527900002));
#174958=CARTESIAN_POINT('Ctrl Pts',(8.38030534899995,15.2,-6.75345384400002));
#174959=CARTESIAN_POINT('Ctrl Pts',(8.38030534899995,11.6,-6.75345384400002));
#174960=CARTESIAN_POINT('Ctrl Pts',(8.38267379899994,15.2,-6.75444272200002));
#174961=CARTESIAN_POINT('Ctrl Pts',(8.38267379899994,11.6,-6.75444272200002));
#174962=CARTESIAN_POINT('Ctrl Pts',(8.38504867299994,15.2,-6.75543189900001));
#174963=CARTESIAN_POINT('Ctrl Pts',(8.38504867299994,11.6,-6.75543189900001));
#174964=CARTESIAN_POINT('Ctrl Pts',(8.38742996299995,15.2,-6.75642136400001));
#174965=CARTESIAN_POINT('Ctrl Pts',(8.38742996299995,11.6,-6.75642136400001));
#174966=CARTESIAN_POINT('Ctrl Pts',(8.38981766199994,15.2,-6.75741110400002));
#174967=CARTESIAN_POINT('Ctrl Pts',(8.38981766199994,11.6,-6.75741110400002));
#174968=CARTESIAN_POINT('Ctrl Pts',(8.39221176299995,15.2,-6.75840110500002));
#174969=CARTESIAN_POINT('Ctrl Pts',(8.39221176299995,11.6,-6.75840110500002));
#174970=CARTESIAN_POINT('Ctrl Pts',(8.39461225899995,15.2,-6.75939135600002));
#174971=CARTESIAN_POINT('Ctrl Pts',(8.39461225899995,11.6,-6.75939135600002));
#174972=CARTESIAN_POINT('Ctrl Pts',(8.39701914299994,15.2,-6.76038184300002));
#174973=CARTESIAN_POINT('Ctrl Pts',(8.39701914299994,11.6,-6.76038184300002));
#174974=CARTESIAN_POINT('Ctrl Pts',(8.39943240599995,15.2,-6.76137255500001));
#174975=CARTESIAN_POINT('Ctrl Pts',(8.39943240599995,11.6,-6.76137255500001));
#174976=CARTESIAN_POINT('Ctrl Pts',(8.40185204399994,15.2,-6.76236347800002));
#174977=CARTESIAN_POINT('Ctrl Pts',(8.40185204399994,11.6,-6.76236347800002));
#174978=CARTESIAN_POINT('Ctrl Pts',(8.40427804899995,15.2,-6.76335459900002));
#174979=CARTESIAN_POINT('Ctrl Pts',(8.40427804899995,11.6,-6.76335459900002));
#174980=CARTESIAN_POINT('Ctrl Pts',(8.40671041099995,15.2,-6.76434590800002));
#174981=CARTESIAN_POINT('Ctrl Pts',(8.40671041099995,11.6,-6.76434590800002));
#174982=CARTESIAN_POINT('Ctrl Pts',(8.40914912599995,15.2,-6.76533739000002));
#174983=CARTESIAN_POINT('Ctrl Pts',(8.40914912599995,11.6,-6.76533739000002));
#174984=CARTESIAN_POINT('Ctrl Pts',(8.41159418599995,15.2,-6.76632903300002));
#174985=CARTESIAN_POINT('Ctrl Pts',(8.41159418599995,11.6,-6.76632903300002));
#174986=CARTESIAN_POINT('Ctrl Pts',(8.41404558399995,15.2,-6.76732082600001));
#174987=CARTESIAN_POINT('Ctrl Pts',(8.41404558399995,11.6,-6.76732082600001));
#174988=CARTESIAN_POINT('Ctrl Pts',(8.41650331199994,15.2,-6.76831275600002));
#174989=CARTESIAN_POINT('Ctrl Pts',(8.41650331199994,11.6,-6.76831275600002));
#174990=CARTESIAN_POINT('Ctrl Pts',(8.41896736399995,15.2,-6.76930481000002));
#174991=CARTESIAN_POINT('Ctrl Pts',(8.41896736399995,11.6,-6.76930481000002));
#174992=CARTESIAN_POINT('Ctrl Pts',(8.42143773199994,15.2,-6.77029697800001));
#174993=CARTESIAN_POINT('Ctrl Pts',(8.42143773199994,11.6,-6.77029697800001));
#174994=CARTESIAN_POINT('Ctrl Pts',(8.42391440899994,15.2,-6.77128924400002));
#174995=CARTESIAN_POINT('Ctrl Pts',(8.42391440899994,11.6,-6.77128924400002));
#174996=CARTESIAN_POINT('Ctrl Pts',(8.42639738999994,15.2,-6.77228159900002));
#174997=CARTESIAN_POINT('Ctrl Pts',(8.42639738999994,11.6,-6.77228159900002));
#174998=CARTESIAN_POINT('Ctrl Pts',(8.42888666599995,15.2,-6.77327402900002));
#174999=CARTESIAN_POINT('Ctrl Pts',(8.42888666599995,11.6,-6.77327402900002));
#175000=CARTESIAN_POINT('Ctrl Pts',(8.43138222999994,15.2,-6.77426652400002));
#175001=CARTESIAN_POINT('Ctrl Pts',(8.43138222999994,11.6,-6.77426652400002));
#175002=CARTESIAN_POINT('Ctrl Pts',(8.43388407399994,15.2,-6.77525907100001));
#175003=CARTESIAN_POINT('Ctrl Pts',(8.43388407399994,11.6,-6.77525907100001));
#175004=CARTESIAN_POINT('Ctrl Pts',(8.43639219399994,15.2,-6.77625165600002));
#175005=CARTESIAN_POINT('Ctrl Pts',(8.43639219399994,11.6,-6.77625165600002));
#175006=CARTESIAN_POINT('Ctrl Pts',(8.43890658199994,15.2,-6.77724426900002));
#175007=CARTESIAN_POINT('Ctrl Pts',(8.43890658199994,11.6,-6.77724426900002));
#175008=CARTESIAN_POINT('Ctrl Pts',(8.44142722799995,15.2,-6.77823689800002));
#175009=CARTESIAN_POINT('Ctrl Pts',(8.44142722799995,11.6,-6.77823689800002));
#175010=CARTESIAN_POINT('Ctrl Pts',(8.44395412799994,15.2,-6.77922953000002));
#175011=CARTESIAN_POINT('Ctrl Pts',(8.44395412799994,11.6,-6.77922953000002));
#175012=CARTESIAN_POINT('Ctrl Pts',(8.44648727499994,15.2,-6.78022215500001));
#175013=CARTESIAN_POINT('Ctrl Pts',(8.44648727499994,11.6,-6.78022215500001));
#175014=CARTESIAN_POINT('Ctrl Pts',(8.44902666199994,15.2,-6.78121475900002));
#175015=CARTESIAN_POINT('Ctrl Pts',(8.44902666199994,11.6,-6.78121475900002));
#175016=CARTESIAN_POINT('Ctrl Pts',(8.45157227999995,15.2,-6.78220733100002));
#175017=CARTESIAN_POINT('Ctrl Pts',(8.45157227999995,11.6,-6.78220733100002));
#175018=CARTESIAN_POINT('Ctrl Pts',(8.45412412299994,15.2,-6.78319985900002));
#175019=CARTESIAN_POINT('Ctrl Pts',(8.45412412299994,11.6,-6.78319985900002));
#175020=CARTESIAN_POINT('Ctrl Pts',(8.45668218599995,15.2,-6.78419233300002));
#175021=CARTESIAN_POINT('Ctrl Pts',(8.45668218599995,11.6,-6.78419233300002));
#175022=CARTESIAN_POINT('Ctrl Pts',(8.45924645999995,15.2,-6.78518473800001));
#175023=CARTESIAN_POINT('Ctrl Pts',(8.45924645999995,11.6,-6.78518473800001));
#175024=CARTESIAN_POINT('Ctrl Pts',(8.46181693799995,15.2,-6.78617706500001));
#175025=CARTESIAN_POINT('Ctrl Pts',(8.46181693799995,11.6,-6.78617706500001));
#175026=CARTESIAN_POINT('Ctrl Pts',(8.46439361399994,15.2,-6.78716930200002));
#175027=CARTESIAN_POINT('Ctrl Pts',(8.46439361399994,11.6,-6.78716930200002));
#175028=CARTESIAN_POINT('Ctrl Pts',(8.46697648099994,15.2,-6.78816143700002));
#175029=CARTESIAN_POINT('Ctrl Pts',(8.46697648099994,11.6,-6.78816143700002));
#175030=CARTESIAN_POINT('Ctrl Pts',(8.46956553199994,15.2,-6.78915345800001));
#175031=CARTESIAN_POINT('Ctrl Pts',(8.46956553199994,11.6,-6.78915345800001));
#175032=CARTESIAN_POINT('Ctrl Pts',(8.47216075899994,15.2,-6.79014535300002));
#175033=CARTESIAN_POINT('Ctrl Pts',(8.47216075899994,11.6,-6.79014535300002));
#175034=CARTESIAN_POINT('Ctrl Pts',(8.47476215699994,15.2,-6.79113711200002));
#175035=CARTESIAN_POINT('Ctrl Pts',(8.47476215699994,11.6,-6.79113711200002));
#175036=CARTESIAN_POINT('Ctrl Pts',(8.47736971999994,15.2,-6.79212872300001));
#175037=CARTESIAN_POINT('Ctrl Pts',(8.47736971999994,11.6,-6.79212872300001));
#175038=CARTESIAN_POINT('Ctrl Pts',(8.47998343699994,15.2,-6.79312017300001));
#175039=CARTESIAN_POINT('Ctrl Pts',(8.47998343699994,11.6,-6.79312017300001));
#175040=CARTESIAN_POINT('Ctrl Pts',(8.48260330399994,15.2,-6.79411145300002));
#175041=CARTESIAN_POINT('Ctrl Pts',(8.48260330399994,11.6,-6.79411145300002));
#175042=CARTESIAN_POINT('Ctrl Pts',(8.48522931299994,15.2,-6.79510255000002));
#175043=CARTESIAN_POINT('Ctrl Pts',(8.48522931299994,11.6,-6.79510255000002));
#175044=CARTESIAN_POINT('Ctrl Pts',(8.48786145799994,15.2,-6.79609345300002));
#175045=CARTESIAN_POINT('Ctrl Pts',(8.48786145799994,11.6,-6.79609345300002));
#175046=CARTESIAN_POINT('Ctrl Pts',(8.49049973399995,15.2,-6.79708415100002));
#175047=CARTESIAN_POINT('Ctrl Pts',(8.49049973399995,11.6,-6.79708415100002));
#175048=CARTESIAN_POINT('Ctrl Pts',(8.49314412999994,15.2,-6.79807463300002));
#175049=CARTESIAN_POINT('Ctrl Pts',(8.49314412999994,11.6,-6.79807463300002));
#175050=CARTESIAN_POINT('Ctrl Pts',(8.49579464199994,15.2,-6.79906488700002));
#175051=CARTESIAN_POINT('Ctrl Pts',(8.49579464199994,11.6,-6.79906488700002));
#175052=CARTESIAN_POINT('Ctrl Pts',(8.49845126199994,15.2,-6.80005490200001));
#175053=CARTESIAN_POINT('Ctrl Pts',(8.49845126199994,11.6,-6.80005490200001));
#175054=CARTESIAN_POINT('Ctrl Pts',(8.50111398399994,15.2,-6.80104466700002));
#175055=CARTESIAN_POINT('Ctrl Pts',(8.50111398399994,11.6,-6.80104466700002));
#175056=CARTESIAN_POINT('Ctrl Pts',(8.50378280199994,15.2,-6.80203417000002));
#175057=CARTESIAN_POINT('Ctrl Pts',(8.50378280199994,11.6,-6.80203417000002));
#175058=CARTESIAN_POINT('Ctrl Pts',(8.50645770599994,15.2,-6.80302340200001));
#175059=CARTESIAN_POINT('Ctrl Pts',(8.50645770599994,11.6,-6.80302340200001));
#175060=CARTESIAN_POINT('Ctrl Pts',(8.50913869399994,15.2,-6.80401235000001));
#175061=CARTESIAN_POINT('Ctrl Pts',(8.50913869399994,11.6,-6.80401235000001));
#175062=CARTESIAN_POINT('Ctrl Pts',(8.51182575499994,15.2,-6.80500100300002));
#175063=CARTESIAN_POINT('Ctrl Pts',(8.51182575499994,11.6,-6.80500100300002));
#175064=CARTESIAN_POINT('Ctrl Pts',(8.51451888399994,15.2,-6.80598935000001));
#175065=CARTESIAN_POINT('Ctrl Pts',(8.51451888399994,11.6,-6.80598935000001));
#175066=CARTESIAN_POINT('Ctrl Pts',(8.51721807399995,15.2,-6.80697738100001));
#175067=CARTESIAN_POINT('Ctrl Pts',(8.51721807399995,11.6,-6.80697738100001));
#175068=CARTESIAN_POINT('Ctrl Pts',(8.51992331799994,15.2,-6.80796508400002));
#175069=CARTESIAN_POINT('Ctrl Pts',(8.51992331799994,11.6,-6.80796508400002));
#175070=CARTESIAN_POINT('Ctrl Pts',(8.52263460999995,15.2,-6.80895244900002));
#175071=CARTESIAN_POINT('Ctrl Pts',(8.52263460999995,11.6,-6.80895244900002));
#175072=CARTESIAN_POINT('Ctrl Pts',(8.52535194299995,15.2,-6.80993946500001));
#175073=CARTESIAN_POINT('Ctrl Pts',(8.52535194299995,11.6,-6.80993946500001));
#175074=CARTESIAN_POINT('Ctrl Pts',(8.52807530999995,15.2,-6.81092612000001));
#175075=CARTESIAN_POINT('Ctrl Pts',(8.52807530999995,11.6,-6.81092612000001));
#175076=CARTESIAN_POINT('Ctrl Pts',(8.53080470399994,15.2,-6.81191240500001));
#175077=CARTESIAN_POINT('Ctrl Pts',(8.53080470399994,11.6,-6.81191240500001));
#175078=CARTESIAN_POINT('Ctrl Pts',(8.53354011899994,15.2,-6.81289830700001));
#175079=CARTESIAN_POINT('Ctrl Pts',(8.53354011899994,11.6,-6.81289830700001));
#175080=CARTESIAN_POINT('Ctrl Pts',(8.53628154899994,15.2,-6.81388381600001));
#175081=CARTESIAN_POINT('Ctrl Pts',(8.53628154899994,11.6,-6.81388381600001));
#175082=CARTESIAN_POINT('Ctrl Pts',(8.53902898399994,15.2,-6.81486892200001));
#175083=CARTESIAN_POINT('Ctrl Pts',(8.53902898399994,11.6,-6.81486892200001));
#175084=CARTESIAN_POINT('Ctrl Pts',(8.54178242199995,15.2,-6.81585361400002));
#175085=CARTESIAN_POINT('Ctrl Pts',(8.54178242199995,11.6,-6.81585361400002));
#175086=CARTESIAN_POINT('Ctrl Pts',(8.54454185299995,15.2,-6.81683788100001));
#175087=CARTESIAN_POINT('Ctrl Pts',(8.54454185299995,11.6,-6.81683788100001));
#175088=CARTESIAN_POINT('Ctrl Pts',(8.54730727099994,15.2,-6.81782171200001));
#175089=CARTESIAN_POINT('Ctrl Pts',(8.54730727099994,11.6,-6.81782171200001));
#175090=CARTESIAN_POINT('Ctrl Pts',(8.55007866999994,15.2,-6.81880509700001));
#175091=CARTESIAN_POINT('Ctrl Pts',(8.55007866999994,11.6,-6.81880509700001));
#175092=CARTESIAN_POINT('Ctrl Pts',(8.55285604299995,15.2,-6.81978802600002));
#175093=CARTESIAN_POINT('Ctrl Pts',(8.55285604299995,11.6,-6.81978802600002));
#175094=CARTESIAN_POINT('Ctrl Pts',(8.55563938299994,15.2,-6.82077048700001));
#175095=CARTESIAN_POINT('Ctrl Pts',(8.55563938299994,11.6,-6.82077048700001));
#175096=CARTESIAN_POINT('Ctrl Pts',(8.55842868299994,15.2,-6.82175247000002));
#175097=CARTESIAN_POINT('Ctrl Pts',(8.55842868299994,11.6,-6.82175247000002));
#175098=CARTESIAN_POINT('Ctrl Pts',(8.56122393899994,15.2,-6.82273396400002));
#175099=CARTESIAN_POINT('Ctrl Pts',(8.56122393899994,11.6,-6.82273396400002));
#175100=CARTESIAN_POINT('Ctrl Pts',(8.56402513999994,15.2,-6.82371496000002));
#175101=CARTESIAN_POINT('Ctrl Pts',(8.56402513999994,11.6,-6.82371496000002));
#175102=CARTESIAN_POINT('Ctrl Pts',(8.56683228399995,15.2,-6.82469544700002));
#175103=CARTESIAN_POINT('Ctrl Pts',(8.56683228399995,11.6,-6.82469544700002));
#175104=CARTESIAN_POINT('Ctrl Pts',(8.56964536099994,15.2,-6.82567541400001));
#175105=CARTESIAN_POINT('Ctrl Pts',(8.56964536099994,11.6,-6.82567541400001));
#175106=CARTESIAN_POINT('Ctrl Pts',(8.57246436599995,15.2,-6.82665485000002));
#175107=CARTESIAN_POINT('Ctrl Pts',(8.57246436599995,11.6,-6.82665485000002));
#175108=CARTESIAN_POINT('Ctrl Pts',(8.57528929199994,15.2,-6.82763374600002));
#175109=CARTESIAN_POINT('Ctrl Pts',(8.57528929199994,11.6,-6.82763374600002));
#175110=CARTESIAN_POINT('Ctrl Pts',(8.57812013199995,15.2,-6.82861209100002));
#175111=CARTESIAN_POINT('Ctrl Pts',(8.57812013199995,11.6,-6.82861209100002));
#175112=CARTESIAN_POINT('Ctrl Pts',(8.58095687899995,15.2,-6.82958987500002));
#175113=CARTESIAN_POINT('Ctrl Pts',(8.58095687899995,11.6,-6.82958987500002));
#175114=CARTESIAN_POINT('Ctrl Pts',(8.58379952799995,15.2,-6.83056708700001));
#175115=CARTESIAN_POINT('Ctrl Pts',(8.58379952799995,11.6,-6.83056708700001));
#175116=CARTESIAN_POINT('Ctrl Pts',(8.58664807299995,15.2,-6.83154371800001));
#175117=CARTESIAN_POINT('Ctrl Pts',(8.58664807299995,11.6,-6.83154371800001));
#175118=CARTESIAN_POINT('Ctrl Pts',(8.58950250399995,15.2,-6.83251975700002));
#175119=CARTESIAN_POINT('Ctrl Pts',(8.58950250399995,11.6,-6.83251975700002));
#175120=CARTESIAN_POINT('Ctrl Pts',(8.59236281799994,15.2,-6.83349519300001));
#175121=CARTESIAN_POINT('Ctrl Pts',(8.59236281799994,11.6,-6.83349519300001));
#175122=CARTESIAN_POINT('Ctrl Pts',(8.59522900599995,15.2,-6.83447001700002));
#175123=CARTESIAN_POINT('Ctrl Pts',(8.59522900599995,11.6,-6.83447001700002));
#175124=CARTESIAN_POINT('Ctrl Pts',(8.59810106299994,15.2,-6.83544421800002));
#175125=CARTESIAN_POINT('Ctrl Pts',(8.59810106299994,11.6,-6.83544421800002));
#175126=CARTESIAN_POINT('Ctrl Pts',(8.60097898199994,15.2,-6.83641778800002));
#175127=CARTESIAN_POINT('Ctrl Pts',(8.60097898199994,11.6,-6.83641778800002));
#175128=CARTESIAN_POINT('Ctrl Pts',(8.60386275599994,15.2,-6.83739071300002));
#175129=CARTESIAN_POINT('Ctrl Pts',(8.60386275599994,11.6,-6.83739071300002));
#175130=CARTESIAN_POINT('Ctrl Pts',(8.60675237799994,15.2,-6.83836298700002));
#175131=CARTESIAN_POINT('Ctrl Pts',(8.60675237799994,11.6,-6.83836298700002));
#175132=CARTESIAN_POINT('Ctrl Pts',(8.60964784399994,15.2,-6.83933459800001));
#175133=CARTESIAN_POINT('Ctrl Pts',(8.60964784399994,11.6,-6.83933459800001));
#175134=CARTESIAN_POINT('Ctrl Pts',(8.61254914499994,15.2,-6.84030553500002));
#175135=CARTESIAN_POINT('Ctrl Pts',(8.61254914499994,11.6,-6.84030553500002));
#175136=CARTESIAN_POINT('Ctrl Pts',(8.61545627499994,15.2,-6.84127579100001));
#175137=CARTESIAN_POINT('Ctrl Pts',(8.61545627499994,11.6,-6.84127579100001));
#175138=CARTESIAN_POINT('Ctrl Pts',(8.61836922799995,15.2,-6.84224535300002));
#175139=CARTESIAN_POINT('Ctrl Pts',(8.61836922799995,11.6,-6.84224535300002));
#175140=CARTESIAN_POINT('Ctrl Pts',(8.62128799699994,15.2,-6.84321421300002));
#175141=CARTESIAN_POINT('Ctrl Pts',(8.62128799699994,11.6,-6.84321421300002));
#175142=CARTESIAN_POINT('Ctrl Pts',(8.62421257699994,15.2,-6.84418236000001));
#175143=CARTESIAN_POINT('Ctrl Pts',(8.62421257699994,11.6,-6.84418236000001));
#175144=CARTESIAN_POINT('Ctrl Pts',(8.62714295899995,15.2,-6.84514978400002));
#175145=CARTESIAN_POINT('Ctrl Pts',(8.62714295899995,11.6,-6.84514978400002));
#175146=CARTESIAN_POINT('Ctrl Pts',(8.63007913999994,15.2,-6.84611647700001));
#175147=CARTESIAN_POINT('Ctrl Pts',(8.63007913999994,11.6,-6.84611647700001));
#175148=CARTESIAN_POINT('Ctrl Pts',(8.63302110999994,15.2,-6.84708242700002));
#175149=CARTESIAN_POINT('Ctrl Pts',(8.63302110999994,11.6,-6.84708242700002));
#175150=CARTESIAN_POINT('Ctrl Pts',(8.63596886299994,15.2,-6.84804762500002));
#175151=CARTESIAN_POINT('Ctrl Pts',(8.63596886299994,11.6,-6.84804762500002));
#175152=CARTESIAN_POINT('Ctrl Pts',(8.63892239499994,15.2,-6.84901206200001));
#175153=CARTESIAN_POINT('Ctrl Pts',(8.63892239499994,11.6,-6.84901206200001));
#175154=CARTESIAN_POINT('Ctrl Pts',(8.64188169699995,15.2,-6.84997572700001));
#175155=CARTESIAN_POINT('Ctrl Pts',(8.64188169699995,11.6,-6.84997572700001));
#175156=CARTESIAN_POINT('Ctrl Pts',(8.64484676499995,15.2,-6.85093861100002));
#175157=CARTESIAN_POINT('Ctrl Pts',(8.64484676499995,11.6,-6.85093861100002));
#175158=CARTESIAN_POINT('Ctrl Pts',(8.64781759099994,15.2,-6.85190070400001));
#175159=CARTESIAN_POINT('Ctrl Pts',(8.64781759099994,11.6,-6.85190070400001));
#175160=CARTESIAN_POINT('Ctrl Pts',(8.65079416799994,15.2,-6.85286199700001));
#175161=CARTESIAN_POINT('Ctrl Pts',(8.65079416799994,11.6,-6.85286199700001));
#175162=CARTESIAN_POINT('Ctrl Pts',(8.65377649099995,15.2,-6.85382247900002));
#175163=CARTESIAN_POINT('Ctrl Pts',(8.65377649099995,11.6,-6.85382247900002));
#175164=CARTESIAN_POINT('Ctrl Pts',(8.65676455199995,15.2,-6.85478214300002));
#175165=CARTESIAN_POINT('Ctrl Pts',(8.65676455199995,11.6,-6.85478214300002));
#175166=CARTESIAN_POINT('Ctrl Pts',(8.65975834599995,15.2,-6.85574097600002));
#175167=CARTESIAN_POINT('Ctrl Pts',(8.65975834599995,11.6,-6.85574097600002));
#175168=CARTESIAN_POINT('Ctrl Pts',(8.66275786699994,15.2,-6.85669897000002));
#175169=CARTESIAN_POINT('Ctrl Pts',(8.66275786699994,11.6,-6.85669897000002));
#175170=CARTESIAN_POINT('Ctrl Pts',(8.66576310799994,15.2,-6.85765611600001));
#175171=CARTESIAN_POINT('Ctrl Pts',(8.66576310799994,11.6,-6.85765611600001));
#175172=CARTESIAN_POINT('Ctrl Pts',(8.66877406099994,15.2,-6.85861240500002));
#175173=CARTESIAN_POINT('Ctrl Pts',(8.66877406099994,11.6,-6.85861240500002));
#175174=CARTESIAN_POINT('Ctrl Pts',(8.67179072199994,15.2,-6.85956782600002));
#175175=CARTESIAN_POINT('Ctrl Pts',(8.67179072199994,11.6,-6.85956782600002));
#175176=CARTESIAN_POINT('Ctrl Pts',(8.67481308299995,15.2,-6.86052237000002));
#175177=CARTESIAN_POINT('Ctrl Pts',(8.67481308299995,11.6,-6.86052237000002));
#175178=CARTESIAN_POINT('Ctrl Pts',(8.67784113899994,15.2,-6.86147602700002));
#175179=CARTESIAN_POINT('Ctrl Pts',(8.67784113899994,11.6,-6.86147602700002));
#175180=CARTESIAN_POINT('Ctrl Pts',(8.68087488199994,15.2,-6.86242879000002));
#175181=CARTESIAN_POINT('Ctrl Pts',(8.68087488199994,11.6,-6.86242879000002));
#175182=CARTESIAN_POINT('Ctrl Pts',(8.68391430599995,15.2,-6.86338064600001));
#175183=CARTESIAN_POINT('Ctrl Pts',(8.68391430599995,11.6,-6.86338064600001));
#175184=CARTESIAN_POINT('Ctrl Pts',(8.68695940699994,15.2,-6.86433158800002));
#175185=CARTESIAN_POINT('Ctrl Pts',(8.68695940699994,11.6,-6.86433158800002));
#175186=CARTESIAN_POINT('Ctrl Pts',(8.69001017599994,15.2,-6.86528160700002));
#175187=CARTESIAN_POINT('Ctrl Pts',(8.69001017599994,11.6,-6.86528160700002));
#175188=CARTESIAN_POINT('Ctrl Pts',(8.69306660699994,15.2,-6.86623069300002));
#175189=CARTESIAN_POINT('Ctrl Pts',(8.69306660699994,11.6,-6.86623069300002));
#175190=CARTESIAN_POINT('Ctrl Pts',(8.69612869499995,15.2,-6.86717883500001));
#175191=CARTESIAN_POINT('Ctrl Pts',(8.69612869499995,11.6,-6.86717883500001));
#175192=CARTESIAN_POINT('Ctrl Pts',(8.69919643199994,15.2,-6.86812602700002));
#175193=CARTESIAN_POINT('Ctrl Pts',(8.69919643199994,11.6,-6.86812602700002));
#175194=CARTESIAN_POINT('Ctrl Pts',(8.70226981399994,15.2,-6.86907225700002));
#175195=CARTESIAN_POINT('Ctrl Pts',(8.70226981399994,11.6,-6.86907225700002));
#175196=CARTESIAN_POINT('Ctrl Pts',(8.70534883099995,15.2,-6.87001751700001));
#175197=CARTESIAN_POINT('Ctrl Pts',(8.70534883099995,11.6,-6.87001751700001));
#175198=CARTESIAN_POINT('Ctrl Pts',(8.70843347999994,15.2,-6.87096179800001));
#175199=CARTESIAN_POINT('Ctrl Pts',(8.70843347999994,11.6,-6.87096179800001));
#175200=CARTESIAN_POINT('Ctrl Pts',(8.71152375499994,15.2,-6.87190509100001));
#175201=CARTESIAN_POINT('Ctrl Pts',(8.71152375499994,11.6,-6.87190509100001));
#175202=CARTESIAN_POINT('Ctrl Pts',(8.71461964599994,15.2,-6.87284738500002));
#175203=CARTESIAN_POINT('Ctrl Pts',(8.71461964599994,11.6,-6.87284738500002));
#175204=CARTESIAN_POINT('Ctrl Pts',(8.71772114999994,15.2,-6.87378867300002));
#175205=CARTESIAN_POINT('Ctrl Pts',(8.71772114999994,11.6,-6.87378867300002));
#175206=CARTESIAN_POINT('Ctrl Pts',(8.72082825999994,15.2,-6.87472894600001));
#175207=CARTESIAN_POINT('Ctrl Pts',(8.72082825999994,11.6,-6.87472894600001));
#175208=CARTESIAN_POINT('Ctrl Pts',(8.72394096899994,15.2,-6.87566819200002));
#175209=CARTESIAN_POINT('Ctrl Pts',(8.72394096899994,11.6,-6.87566819200002));
#175210=CARTESIAN_POINT('Ctrl Pts',(8.72705927099994,15.2,-6.87660640600001));
#175211=CARTESIAN_POINT('Ctrl Pts',(8.72705927099994,11.6,-6.87660640600001));
#175212=CARTESIAN_POINT('Ctrl Pts',(8.73018315999994,15.2,-6.87754357600002));
#175213=CARTESIAN_POINT('Ctrl Pts',(8.73018315999994,11.6,-6.87754357600002));
#175214=CARTESIAN_POINT('Ctrl Pts',(8.73331262999994,15.2,-6.87847969400002));
#175215=CARTESIAN_POINT('Ctrl Pts',(8.73331262999994,11.6,-6.87847969400002));
#175216=CARTESIAN_POINT('Ctrl Pts',(8.73644767399994,15.2,-6.87941475100001));
#175217=CARTESIAN_POINT('Ctrl Pts',(8.73644767399994,11.6,-6.87941475100001));
#175218=CARTESIAN_POINT('Ctrl Pts',(8.73958828699994,15.2,-6.88034873900002));
#175219=CARTESIAN_POINT('Ctrl Pts',(8.73958828699994,11.6,-6.88034873900002));
#175220=CARTESIAN_POINT('Ctrl Pts',(8.74273446099994,15.2,-6.88128164700001));
#175221=CARTESIAN_POINT('Ctrl Pts',(8.74273446099994,11.6,-6.88128164700001));
#175222=CARTESIAN_POINT('Ctrl Pts',(8.74588619099994,15.2,-6.88221346800002));
#175223=CARTESIAN_POINT('Ctrl Pts',(8.74588619099994,11.6,-6.88221346800002));
#175224=CARTESIAN_POINT('Ctrl Pts',(8.74904346899994,15.2,-6.88314419200001));
#175225=CARTESIAN_POINT('Ctrl Pts',(8.74904346899994,11.6,-6.88314419200001));
#175226=CARTESIAN_POINT('Ctrl Pts',(8.75220629199994,15.2,-6.88407381000002));
#175227=CARTESIAN_POINT('Ctrl Pts',(8.75220629199994,11.6,-6.88407381000002));
#175228=CARTESIAN_POINT('Ctrl Pts',(8.75537464999995,15.2,-6.88500231400001));
#175229=CARTESIAN_POINT('Ctrl Pts',(8.75537464999995,11.6,-6.88500231400001));
#175230=CARTESIAN_POINT('Ctrl Pts',(8.75854853999994,15.2,-6.88592969500001));
#175231=CARTESIAN_POINT('Ctrl Pts',(8.75854853999994,11.6,-6.88592969500001));
#175232=CARTESIAN_POINT('Ctrl Pts',(8.76172795499994,15.2,-6.88685594400001));
#175233=CARTESIAN_POINT('Ctrl Pts',(8.76172795499994,11.6,-6.88685594400001));
#175234=CARTESIAN_POINT('Ctrl Pts',(8.76491288799994,15.2,-6.88778105200001));
#175235=CARTESIAN_POINT('Ctrl Pts',(8.76491288799994,11.6,-6.88778105200001));
#175236=CARTESIAN_POINT('Ctrl Pts',(8.76810333299994,15.2,-6.88870501000002));
#175237=CARTESIAN_POINT('Ctrl Pts',(8.76810333299994,11.6,-6.88870501000002));
#175238=CARTESIAN_POINT('Ctrl Pts',(8.77129928299994,15.2,-6.88962781100001));
#175239=CARTESIAN_POINT('Ctrl Pts',(8.77129928299994,11.6,-6.88962781100001));
#175240=CARTESIAN_POINT('Ctrl Pts',(8.77450073399995,15.2,-6.89054944400001));
#175241=CARTESIAN_POINT('Ctrl Pts',(8.77450073399995,11.6,-6.89054944400001));
#175242=CARTESIAN_POINT('Ctrl Pts',(8.77770767799994,15.2,-6.89146990200002));
#175243=CARTESIAN_POINT('Ctrl Pts',(8.77770767799994,11.6,-6.89146990200002));
#175244=CARTESIAN_POINT('Ctrl Pts',(8.78092010799995,15.2,-6.89238917500001));
#175245=CARTESIAN_POINT('Ctrl Pts',(8.78092010799995,11.6,-6.89238917500001));
#175246=CARTESIAN_POINT('Ctrl Pts',(8.78413802099994,15.2,-6.89330725600002));
#175247=CARTESIAN_POINT('Ctrl Pts',(8.78413802099994,11.6,-6.89330725600002));
#175248=CARTESIAN_POINT('Ctrl Pts',(8.78736140799995,15.2,-6.89422413400001));
#175249=CARTESIAN_POINT('Ctrl Pts',(8.78736140799995,11.6,-6.89422413400001));
#175250=CARTESIAN_POINT('Ctrl Pts',(8.79059026399995,15.2,-6.89513980300001));
#175251=CARTESIAN_POINT('Ctrl Pts',(8.79059026399995,11.6,-6.89513980300001));
#175252=CARTESIAN_POINT('Ctrl Pts',(8.79382458299995,15.2,-6.89605425400002));
#175253=CARTESIAN_POINT('Ctrl Pts',(8.79382458299995,11.6,-6.89605425400002));
#175254=CARTESIAN_POINT('Ctrl Pts',(8.79706435899994,15.2,-6.89696747700002));
#175255=CARTESIAN_POINT('Ctrl Pts',(8.79706435899994,11.6,-6.89696747700002));
#175256=CARTESIAN_POINT('Ctrl Pts',(8.80030958499994,15.2,-6.89787946300001));
#175257=CARTESIAN_POINT('Ctrl Pts',(8.80030958499994,11.6,-6.89787946300001));
#175258=CARTESIAN_POINT('Ctrl Pts',(8.80356025499994,15.2,-6.89879020600002));
#175259=CARTESIAN_POINT('Ctrl Pts',(8.80356025499994,11.6,-6.89879020600002));
#175260=CARTESIAN_POINT('Ctrl Pts',(8.80681636199995,15.2,-6.89969969500002));
#175261=CARTESIAN_POINT('Ctrl Pts',(8.80681636199995,11.6,-6.89969969500002));
#175262=CARTESIAN_POINT('Ctrl Pts',(8.81007790199994,15.2,-6.90060792400002));
#175263=CARTESIAN_POINT('Ctrl Pts',(8.81007790199994,11.6,-6.90060792400002));
#175264=CARTESIAN_POINT('Ctrl Pts',(8.81334486699994,15.2,-6.90151488300002));
#175265=CARTESIAN_POINT('Ctrl Pts',(8.81334486699994,11.6,-6.90151488300002));
#175266=CARTESIAN_POINT('Ctrl Pts',(8.81661725299994,15.2,-6.90242056300002));
#175267=CARTESIAN_POINT('Ctrl Pts',(8.81661725299994,11.6,-6.90242056300002));
#175268=CARTESIAN_POINT('Ctrl Pts',(8.81989505199994,15.2,-6.90332495700002));
#175269=CARTESIAN_POINT('Ctrl Pts',(8.81989505199994,11.6,-6.90332495700002));
#175270=CARTESIAN_POINT('Ctrl Pts',(8.82317825799994,15.2,-6.90422805600001));
#175271=CARTESIAN_POINT('Ctrl Pts',(8.82317825799994,11.6,-6.90422805600001));
#175272=CARTESIAN_POINT('Ctrl Pts',(8.82646686599994,15.2,-6.90512985200002));
#175273=CARTESIAN_POINT('Ctrl Pts',(8.82646686599994,11.6,-6.90512985200002));
#175274=CARTESIAN_POINT('Ctrl Pts',(8.82976086799994,15.2,-6.90603033500001));
#175275=CARTESIAN_POINT('Ctrl Pts',(8.82976086799994,11.6,-6.90603033500001));
#175276=CARTESIAN_POINT('Ctrl Pts',(8.83306025999994,15.2,-6.90692950000001));
#175277=CARTESIAN_POINT('Ctrl Pts',(8.83306025999994,11.6,-6.90692950000001));
#175278=CARTESIAN_POINT('Ctrl Pts',(8.83636503499994,15.2,-6.90782733500001));
#175279=CARTESIAN_POINT('Ctrl Pts',(8.83636503499994,11.6,-6.90782733500001));
#175280=CARTESIAN_POINT('Ctrl Pts',(8.83967518699994,15.2,-6.90872383400002));
#175281=CARTESIAN_POINT('Ctrl Pts',(8.83967518699994,11.6,-6.90872383400002));
#175282=CARTESIAN_POINT('Ctrl Pts',(8.84299070999995,15.2,-6.90961898900002));
#175283=CARTESIAN_POINT('Ctrl Pts',(8.84299070999995,11.6,-6.90961898900002));
#175284=CARTESIAN_POINT('Ctrl Pts',(8.84631159699994,15.2,-6.91051279100002));
#175285=CARTESIAN_POINT('Ctrl Pts',(8.84631159699994,11.6,-6.91051279100002));
#175286=CARTESIAN_POINT('Ctrl Pts',(8.84963784299994,15.2,-6.91140523000002));
#175287=CARTESIAN_POINT('Ctrl Pts',(8.84963784299994,11.6,-6.91140523000002));
#175288=CARTESIAN_POINT('Ctrl Pts',(8.85296944199995,15.2,-6.91229630100001));
#175289=CARTESIAN_POINT('Ctrl Pts',(8.85296944199995,11.6,-6.91229630100001));
#175290=CARTESIAN_POINT('Ctrl Pts',(8.85630638699994,15.2,-6.91318599400002));
#175291=CARTESIAN_POINT('Ctrl Pts',(8.85630638699994,11.6,-6.91318599400002));
#175292=CARTESIAN_POINT('Ctrl Pts',(8.85964867399995,15.2,-6.91407430100002));
#175293=CARTESIAN_POINT('Ctrl Pts',(8.85964867399995,11.6,-6.91407430100002));
#175294=CARTESIAN_POINT('Ctrl Pts',(8.86299629299995,15.2,-6.91496121400001));
#175295=CARTESIAN_POINT('Ctrl Pts',(8.86299629299995,11.6,-6.91496121400001));
#175296=CARTESIAN_POINT('Ctrl Pts',(8.86634924199995,15.2,-6.91584672500002));
#175297=CARTESIAN_POINT('Ctrl Pts',(8.86634924199995,11.6,-6.91584672500002));
#175298=CARTESIAN_POINT('Ctrl Pts',(8.86970751299994,15.2,-6.91673082700002));
#175299=CARTESIAN_POINT('Ctrl Pts',(8.86970751299994,11.6,-6.91673082700002));
#175300=CARTESIAN_POINT('Ctrl Pts',(8.87307109999995,15.2,-6.91761350900002));
#175301=CARTESIAN_POINT('Ctrl Pts',(8.87307109999995,11.6,-6.91761350900002));
#175302=CARTESIAN_POINT('Ctrl Pts',(8.87643999799994,15.2,-6.91849476600002));
#175303=CARTESIAN_POINT('Ctrl Pts',(8.87643999799994,11.6,-6.91849476600002));
#175304=CARTESIAN_POINT('Ctrl Pts',(8.87981419899995,15.2,-6.91937458800002));
#175305=CARTESIAN_POINT('Ctrl Pts',(8.87981419899995,11.6,-6.91937458800002));
#175306=CARTESIAN_POINT('Ctrl Pts',(8.88319369999994,15.2,-6.92025296700002));
#175307=CARTESIAN_POINT('Ctrl Pts',(8.88319369999994,11.6,-6.92025296700002));
#175308=CARTESIAN_POINT('Ctrl Pts',(8.88657849099994,15.2,-6.92112989800002));
#175309=CARTESIAN_POINT('Ctrl Pts',(8.88657849099994,11.6,-6.92112989800002));
#175310=CARTESIAN_POINT('Ctrl Pts',(8.88996856999994,15.2,-6.92200536900001));
#175311=CARTESIAN_POINT('Ctrl Pts',(8.88996856999994,11.6,-6.92200536900001));
#175312=CARTESIAN_POINT('Ctrl Pts',(8.89336392799994,15.2,-6.92287937400001));
#175313=CARTESIAN_POINT('Ctrl Pts',(8.89336392799994,11.6,-6.92287937400001));
#175314=CARTESIAN_POINT('Ctrl Pts',(8.89676456199994,15.2,-6.92375190400002));
#175315=CARTESIAN_POINT('Ctrl Pts',(8.89676456199994,11.6,-6.92375190400002));
#175316=CARTESIAN_POINT('Ctrl Pts',(8.90017046199995,15.2,-6.92462295300002));
#175317=CARTESIAN_POINT('Ctrl Pts',(8.90017046199995,11.6,-6.92462295300002));
#175318=CARTESIAN_POINT('Ctrl Pts',(8.90358162499994,15.2,-6.92549251100001));
#175319=CARTESIAN_POINT('Ctrl Pts',(8.90358162499994,11.6,-6.92549251100001));
#175320=CARTESIAN_POINT('Ctrl Pts',(8.90699804399994,15.2,-6.92636057100002));
#175321=CARTESIAN_POINT('Ctrl Pts',(8.90699804399994,11.6,-6.92636057100002));
#175322=CARTESIAN_POINT('Ctrl Pts',(8.91041971299994,15.2,-6.92722712600002));
#175323=CARTESIAN_POINT('Ctrl Pts',(8.91041971299994,11.6,-6.92722712600002));
#175324=CARTESIAN_POINT('Ctrl Pts',(8.91384662699994,15.2,-6.92809216800002));
#175325=CARTESIAN_POINT('Ctrl Pts',(8.91384662699994,11.6,-6.92809216800002));
#175326=CARTESIAN_POINT('Ctrl Pts',(8.91727877799994,15.2,-6.92895568800001));
#175327=CARTESIAN_POINT('Ctrl Pts',(8.91727877799994,11.6,-6.92895568800001));
#175328=CARTESIAN_POINT('Ctrl Pts',(8.92071616199994,15.2,-6.92981767800001));
#175329=CARTESIAN_POINT('Ctrl Pts',(8.92071616199994,11.6,-6.92981767800001));
#175330=CARTESIAN_POINT('Ctrl Pts',(8.92415877199995,15.2,-6.93067813200001));
#175331=CARTESIAN_POINT('Ctrl Pts',(8.92415877199995,11.6,-6.93067813200001));
#175332=CARTESIAN_POINT('Ctrl Pts',(8.92760660199994,15.2,-6.93153704100002));
#175333=CARTESIAN_POINT('Ctrl Pts',(8.92760660199994,11.6,-6.93153704100002));
#175334=CARTESIAN_POINT('Ctrl Pts',(8.93105964599994,15.2,-6.93239439700001));
#175335=CARTESIAN_POINT('Ctrl Pts',(8.93105964599994,11.6,-6.93239439700001));
#175336=CARTESIAN_POINT('Ctrl Pts',(8.93451789999994,15.2,-6.93325019300002));
#175337=CARTESIAN_POINT('Ctrl Pts',(8.93451789999994,11.6,-6.93325019300002));
#175338=CARTESIAN_POINT('Ctrl Pts',(8.93798135499994,15.2,-6.93410442100002));
#175339=CARTESIAN_POINT('Ctrl Pts',(8.93798135499994,11.6,-6.93410442100002));
#175340=CARTESIAN_POINT('Ctrl Pts',(8.94145000699995,15.2,-6.93495707400002));
#175341=CARTESIAN_POINT('Ctrl Pts',(8.94145000699995,11.6,-6.93495707400002));
#175342=CARTESIAN_POINT('Ctrl Pts',(8.94492384899995,15.2,-6.93580814300002));
#175343=CARTESIAN_POINT('Ctrl Pts',(8.94492384899995,11.6,-6.93580814300002));
#175344=CARTESIAN_POINT('Ctrl Pts',(8.94840287499994,15.2,-6.93665762100002));
#175345=CARTESIAN_POINT('Ctrl Pts',(8.94840287499994,11.6,-6.93665762100002));
#175346=CARTESIAN_POINT('Ctrl Pts',(8.95188708099995,15.2,-6.93750550000001));
#175347=CARTESIAN_POINT('Ctrl Pts',(8.95188708099995,11.6,-6.93750550000001));
#175348=CARTESIAN_POINT('Ctrl Pts',(8.95537645899994,15.2,-6.93835177400001));
#175349=CARTESIAN_POINT('Ctrl Pts',(8.95537645899994,11.6,-6.93835177400001));
#175350=CARTESIAN_POINT('Ctrl Pts',(8.95887100399994,15.2,-6.93919643400001));
#175351=CARTESIAN_POINT('Ctrl Pts',(8.95887100399994,11.6,-6.93919643400001));
#175352=CARTESIAN_POINT('Ctrl Pts',(8.96237070999995,15.2,-6.94003947100001));
#175353=CARTESIAN_POINT('Ctrl Pts',(8.96237070999995,11.6,-6.94003947100001));
#175354=CARTESIAN_POINT('Ctrl Pts',(8.96587556999994,15.2,-6.94088088000001));
#175355=CARTESIAN_POINT('Ctrl Pts',(8.96587556999994,11.6,-6.94088088000001));
#175356=CARTESIAN_POINT('Ctrl Pts',(8.96938557999994,15.2,-6.94172065300001));
#175357=CARTESIAN_POINT('Ctrl Pts',(8.96938557999994,11.6,-6.94172065300001));
#175358=CARTESIAN_POINT('Ctrl Pts',(8.97290073199994,15.2,-6.94255878100002));
#175359=CARTESIAN_POINT('Ctrl Pts',(8.97290073199994,11.6,-6.94255878100002));
#175360=CARTESIAN_POINT('Ctrl Pts',(8.97642102299994,15.2,-6.94339525900002));
#175361=CARTESIAN_POINT('Ctrl Pts',(8.97642102299994,11.6,-6.94339525900002));
#175362=CARTESIAN_POINT('Ctrl Pts',(8.97994644299994,15.2,-6.94423007600002));
#175363=CARTESIAN_POINT('Ctrl Pts',(8.97994644299994,11.6,-6.94423007600002));
#175364=CARTESIAN_POINT('Ctrl Pts',(8.98347698999994,15.2,-6.94506322800001));
#175365=CARTESIAN_POINT('Ctrl Pts',(8.98347698999994,11.6,-6.94506322800001));
#175366=CARTESIAN_POINT('Ctrl Pts',(8.98701265699994,15.2,-6.94589470600001));
#175367=CARTESIAN_POINT('Ctrl Pts',(8.98701265699994,11.6,-6.94589470600001));
#175368=CARTESIAN_POINT('Ctrl Pts',(8.99055343599995,15.2,-6.94672450200001));
#175369=CARTESIAN_POINT('Ctrl Pts',(8.99055343599995,11.6,-6.94672450200001));
#175370=CARTESIAN_POINT('Ctrl Pts',(8.99409932299994,15.2,-6.94755260900001));
#175371=CARTESIAN_POINT('Ctrl Pts',(8.99409932299994,11.6,-6.94755260900001));
#175372=CARTESIAN_POINT('Ctrl Pts',(8.99765031299994,15.2,-6.94837902000002));
#175373=CARTESIAN_POINT('Ctrl Pts',(8.99765031299994,11.6,-6.94837902000002));
#175374=CARTESIAN_POINT('Ctrl Pts',(9.00120639799994,15.2,-6.94920372700001));
#175375=CARTESIAN_POINT('Ctrl Pts',(9.00120639799994,11.6,-6.94920372700001));
#175376=CARTESIAN_POINT('Ctrl Pts',(9.00476757299994,15.2,-6.95002672400002));
#175377=CARTESIAN_POINT('Ctrl Pts',(9.00476757299994,11.6,-6.95002672400002));
#175378=CARTESIAN_POINT('Ctrl Pts',(9.00833383199994,15.2,-6.95084800200001));
#175379=CARTESIAN_POINT('Ctrl Pts',(9.00833383199994,11.6,-6.95084800200001));
#175380=CARTESIAN_POINT('Ctrl Pts',(9.01190517099994,15.2,-6.95166755500002));
#175381=CARTESIAN_POINT('Ctrl Pts',(9.01190517099994,11.6,-6.95166755500002));
#175382=CARTESIAN_POINT('Ctrl Pts',(9.01548158099994,15.2,-6.95248537400002));
#175383=CARTESIAN_POINT('Ctrl Pts',(9.01548158099994,11.6,-6.95248537400002));
#175384=CARTESIAN_POINT('Ctrl Pts',(9.01906305899994,15.2,-6.95330145400002));
#175385=CARTESIAN_POINT('Ctrl Pts',(9.01906305899994,11.6,-6.95330145400002));
#175386=CARTESIAN_POINT('Ctrl Pts',(9.02264959699994,15.2,-6.95411578600002));
#175387=CARTESIAN_POINT('Ctrl Pts',(9.02264959699994,11.6,-6.95411578600002));
#175388=CARTESIAN_POINT('Ctrl Pts',(9.02624118899995,15.2,-6.95492836400001));
#175389=CARTESIAN_POINT('Ctrl Pts',(9.02624118899995,11.6,-6.95492836400001));
#175390=CARTESIAN_POINT('Ctrl Pts',(9.02983783099994,15.2,-6.95573917900001));
#175391=CARTESIAN_POINT('Ctrl Pts',(9.02983783099994,11.6,-6.95573917900001));
#175392=CARTESIAN_POINT('Ctrl Pts',(9.03343951599994,15.2,-6.95654822400002));
#175393=CARTESIAN_POINT('Ctrl Pts',(9.03343951599994,11.6,-6.95654822400002));
#175394=CARTESIAN_POINT('Ctrl Pts',(9.03704623799995,15.2,-6.95735549300001));
#175395=CARTESIAN_POINT('Ctrl Pts',(9.03704623799995,11.6,-6.95735549300001));
#175396=CARTESIAN_POINT('Ctrl Pts',(9.04065799199994,15.2,-6.95816097800002));
#175397=CARTESIAN_POINT('Ctrl Pts',(9.04065799199994,11.6,-6.95816097800002));
#175398=CARTESIAN_POINT('Ctrl Pts',(9.04427477099994,15.2,-6.95896467300001));
#175399=CARTESIAN_POINT('Ctrl Pts',(9.04427477099994,11.6,-6.95896467300001));
#175400=CARTESIAN_POINT('Ctrl Pts',(9.04789657099995,15.2,-6.95976657000001));
#175401=CARTESIAN_POINT('Ctrl Pts',(9.04789657099995,11.6,-6.95976657000001));
#175402=CARTESIAN_POINT('Ctrl Pts',(9.05152338599994,15.2,-6.96056666300001));
#175403=CARTESIAN_POINT('Ctrl Pts',(9.05152338599994,11.6,-6.96056666300001));
#175404=CARTESIAN_POINT('Ctrl Pts',(9.05515520799994,15.2,-6.96136494300001));
#175405=CARTESIAN_POINT('Ctrl Pts',(9.05515520799994,11.6,-6.96136494300001));
#175406=CARTESIAN_POINT('Ctrl Pts',(9.05879203399994,15.2,-6.96216140500002));
#175407=CARTESIAN_POINT('Ctrl Pts',(9.05879203399994,11.6,-6.96216140500002));
#175408=CARTESIAN_POINT('Ctrl Pts',(9.06243385699995,15.2,-6.96295603900002));
#175409=CARTESIAN_POINT('Ctrl Pts',(9.06243385699995,11.6,-6.96295603900002));
#175410=CARTESIAN_POINT('Ctrl Pts',(9.06608066899994,15.2,-6.96374884000001));
#175411=CARTESIAN_POINT('Ctrl Pts',(9.06608066899994,11.6,-6.96374884000001));
#175412=CARTESIAN_POINT('Ctrl Pts',(9.06973246699994,15.2,-6.96453980000002));
#175413=CARTESIAN_POINT('Ctrl Pts',(9.06973246699994,11.6,-6.96453980000002));
#175414=CARTESIAN_POINT('Ctrl Pts',(9.07338924199994,15.2,-6.96532891100002));
#175415=CARTESIAN_POINT('Ctrl Pts',(9.07338924199994,11.6,-6.96532891100002));
#175416=CARTESIAN_POINT('Ctrl Pts',(9.07705099099994,15.2,-6.96611616700002));
#175417=CARTESIAN_POINT('Ctrl Pts',(9.07705099099994,11.6,-6.96611616700002));
#175418=CARTESIAN_POINT('Ctrl Pts',(9.08071770699994,15.2,-6.96690156100002));
#175419=CARTESIAN_POINT('Ctrl Pts',(9.08071770699994,11.6,-6.96690156100002));
#175420=CARTESIAN_POINT('Ctrl Pts',(9.08438938599994,15.2,-6.96768508700002));
#175421=CARTESIAN_POINT('Ctrl Pts',(9.08438938599994,11.6,-6.96768508700002));
#175422=CARTESIAN_POINT('Ctrl Pts',(9.08806602099994,15.2,-6.96846673800002));
#175423=CARTESIAN_POINT('Ctrl Pts',(9.08806602099994,11.6,-6.96846673800002));
#175424=CARTESIAN_POINT('Ctrl Pts',(9.09174760799995,15.2,-6.96924650800002));
#175425=CARTESIAN_POINT('Ctrl Pts',(9.09174760799995,11.6,-6.96924650800002));
#175426=CARTESIAN_POINT('Ctrl Pts',(9.09543414099995,15.2,-6.97002439100002));
#175427=CARTESIAN_POINT('Ctrl Pts',(9.09543414099995,11.6,-6.97002439100002));
#175428=CARTESIAN_POINT('Ctrl Pts',(9.09912561399995,15.2,-6.97080037900002));
#175429=CARTESIAN_POINT('Ctrl Pts',(9.09912561399995,11.6,-6.97080037900002));
#175430=CARTESIAN_POINT('Ctrl Pts',(9.10282202199994,15.2,-6.97157446400002));
#175431=CARTESIAN_POINT('Ctrl Pts',(9.10282202199994,11.6,-6.97157446400002));
#175432=CARTESIAN_POINT('Ctrl Pts',(9.10652335599995,15.2,-6.97234663800002));
#175433=CARTESIAN_POINT('Ctrl Pts',(9.10652335599995,11.6,-6.97234663800002));
#175434=CARTESIAN_POINT('Ctrl Pts',(9.11022960799994,15.2,-6.97311689200002));
#175435=CARTESIAN_POINT('Ctrl Pts',(9.11022960799994,11.6,-6.97311689200002));
#175436=CARTESIAN_POINT('Ctrl Pts',(9.11394077299994,15.2,-6.97388521800002));
#175437=CARTESIAN_POINT('Ctrl Pts',(9.11394077299994,11.6,-6.97388521800002));
#175438=CARTESIAN_POINT('Ctrl Pts',(9.11765684399995,15.2,-6.97465160800002));
#175439=CARTESIAN_POINT('Ctrl Pts',(9.11765684399995,11.6,-6.97465160800002));
#175440=CARTESIAN_POINT('Ctrl Pts',(9.12137781599995,15.2,-6.97541605700001));
#175441=CARTESIAN_POINT('Ctrl Pts',(9.12137781599995,11.6,-6.97541605700001));
#175442=CARTESIAN_POINT('Ctrl Pts',(9.12510368599994,15.2,-6.97617855800001));
#175443=CARTESIAN_POINT('Ctrl Pts',(9.12510368599994,11.6,-6.97617855800001));
#175444=CARTESIAN_POINT('Ctrl Pts',(9.12883444799995,15.2,-6.97693911100002));
#175445=CARTESIAN_POINT('Ctrl Pts',(9.12883444799995,11.6,-6.97693911100002));
#175446=CARTESIAN_POINT('Ctrl Pts',(9.13257010499994,15.2,-6.97769771200001));
#175447=CARTESIAN_POINT('Ctrl Pts',(9.13257010499994,11.6,-6.97769771200001));
#175448=CARTESIAN_POINT('Ctrl Pts',(9.13556254299994,15.2,-6.97830303200002));
#175449=CARTESIAN_POINT('Ctrl Pts',(9.13556254299994,11.6,-6.97830303200002));
#175450=CARTESIAN_POINT('Ctrl Pts',(9.13780907299994,15.2,-6.97875614300001));
#175451=CARTESIAN_POINT('Ctrl Pts',(9.13780907299994,11.6,-6.97875614300001));
#175452=CARTESIAN_POINT('Ctrl Pts',(9.13930773799994,15.2,-6.97905782700002));
#175453=CARTESIAN_POINT('Ctrl Pts',(9.13930773799994,11.6,-6.97905782700002));
#175454=CARTESIAN_POINT('Ctrl Pts',(9.14005731399994,15.2,-6.97920857100002));
#175455=CARTESIAN_POINT('Ctrl Pts',(9.14005731399994,11.6,-6.97920857100002));
#175456=CARTESIAN_POINT('Ctrl Pts',(8.02901631899994,15.2,-6.57080831800001));
#175457=CARTESIAN_POINT('Ctrl Pts',(8.03049110016105,15.2,-6.57181686697944));
#175458=CARTESIAN_POINT('Ctrl Pts',(8.03201610877769,15.2,-6.57285322878717));
#175459=CARTESIAN_POINT('Ctrl Pts',(8.03359089353572,15.2,-6.5739163521752));
#175460=CARTESIAN_POINT('Ctrl Pts',(8.03517327270188,15.2,-6.57498460248157));
#175461=CARTESIAN_POINT('Ctrl Pts',(8.03680591622578,15.2,-6.5760798659982));
#175462=CARTESIAN_POINT('Ctrl Pts',(8.0384883906544,15.2,-6.57720107836683));
#175463=CARTESIAN_POINT('Ctrl Pts',(8.04017086493022,15.2,-6.5783222906336));
#175464=CARTESIAN_POINT('Ctrl Pts',(8.04190317335625,15.2,-6.57946945420923));
#175465=CARTESIAN_POINT('Ctrl Pts',(8.04368489154152,15.2,-6.58064153749996));
#175466=CARTESIAN_POINT('Ctrl Pts',(8.04546660972677,15.2,-6.5818136207907));
#175467=CARTESIAN_POINT('Ctrl Pts',(8.04729774128699,15.1999999999999,-6.58301062499168));
#175468=CARTESIAN_POINT('Ctrl Pts',(8.04917787055977,15.2,-6.58423155042359));
#175469=CARTESIAN_POINT('Ctrl Pts',(8.05105800000331,15.2,-6.5854524759664));
#175470=CARTESIAN_POINT('Ctrl Pts',(8.05298713001268,15.2,-6.58669732252585));
#175471=CARTESIAN_POINT('Ctrl Pts',(8.05496485620711,15.2,-6.58796512017984));
#175472=CARTESIAN_POINT('Ctrl Pts',(8.05694258222188,15.2,-6.58923291771867));
#175473=CARTESIAN_POINT('Ctrl Pts',(8.05896890494999,15.2,-6.59052366460892));
#175474=CARTESIAN_POINT('Ctrl Pts',(8.0610434290508,15.2,-6.59183642123391));
#175475=CARTESIAN_POINT('Ctrl Pts',(8.06311795315161,15.2,-6.59314917785888));
#175476=CARTESIAN_POINT('Ctrl Pts',(8.06524067911272,15.2,-6.59448394143469));
#175477=CARTESIAN_POINT('Ctrl Pts',(8.0674112193651,15.2,-6.59583979613451));
#175478=CARTESIAN_POINT('Ctrl Pts',(8.06958175981464,15.2,-6.59719565095748));
#175479=CARTESIAN_POINT('Ctrl Pts',(8.07180011545347,15.2,-6.59857259622476));
#175480=CARTESIAN_POINT('Ctrl Pts',(8.07406590574684,15.2,-6.5999697421356));
#175481=CARTESIAN_POINT('Ctrl Pts',(8.0763316958344,15.2,-6.60136688791955));
#175482=CARTESIAN_POINT('Ctrl Pts',(8.07864492166241,15.2,-6.60278423372139));
#175483=CARTESIAN_POINT('Ctrl Pts',(8.08100520891203,15.2,-6.6042209115867));
#175484=CARTESIAN_POINT('Ctrl Pts',(8.08336549616167,15.2,-6.605657589452));
#175485=CARTESIAN_POINT('Ctrl Pts',(8.08577284714085,15.2,-6.60711359752408));
#175486=CARTESIAN_POINT('Ctrl Pts',(8.08822689338298,15.2,-6.60858809463637));
#175487=CARTESIAN_POINT('Ctrl Pts',(8.09068093962512,15.2,-6.61006259174866));
#175488=CARTESIAN_POINT('Ctrl Pts',(8.09318168337629,15.2,-6.61155557734142));
#175489=CARTESIAN_POINT('Ctrl Pts',(8.09572876369724,15.2,-6.61306622661866));
#175490=CARTESIAN_POINT('Ctrl Pts',(8.09827584424958,15.2,-6.61457687603312));
#175491=CARTESIAN_POINT('Ctrl Pts',(8.10086926328141,15.2,-6.61610519224932));
#175492=CARTESIAN_POINT('Ctrl Pts',(8.10350866492724,15.2,-6.61765036983427));
#175493=CARTESIAN_POINT('Ctrl Pts',(8.10614806633333,15.2,-6.61919554727886));
#175494=CARTESIAN_POINT('Ctrl Pts',(8.10883345331891,15.2,-6.62075759161615));
#175495=CARTESIAN_POINT('Ctrl Pts',(8.11156447473196,15.2,-6.62233571523261));
#175496=CARTESIAN_POINT('Ctrl Pts',(8.11429549614501,15.2,-6.62391383884906));
#175497=CARTESIAN_POINT('Ctrl Pts',(8.11707215585626,15.2,-6.62550804652576));
#175498=CARTESIAN_POINT('Ctrl Pts',(8.11989411016728,15.2,-6.62711757488289));
#175499=CARTESIAN_POINT('Ctrl Pts',(8.12271606473465,15.2,-6.62872710338622));
#175500=CARTESIAN_POINT('Ctrl Pts',(8.12558331191476,15.2,-6.6303519509994));
#175501=CARTESIAN_POINT('Ctrl Pts',(8.12849551940877,15.2,-6.6319913775894));
#175502=CARTESIAN_POINT('Ctrl Pts',(8.13140772663827,15.2,-6.63363080403048));
#175503=CARTESIAN_POINT('Ctrl Pts',(8.13436489026072,15.2,-6.63528480749396));
#175504=CARTESIAN_POINT('Ctrl Pts',(8.13736668249851,15.2,-6.63695266402424));
#175505=CARTESIAN_POINT('Ctrl Pts',(8.14036847473628,15.2,-6.63862052055451));
#175506=CARTESIAN_POINT('Ctrl Pts',(8.143414891645,15.2,-6.64030222865274));
#175507=CARTESIAN_POINT('Ctrl Pts',(8.14650561086299,15.2,-6.64199708134026));
#175508=CARTESIAN_POINT('Ctrl Pts',(8.14959633036172,15.2,-6.64369193418172));
#175509=CARTESIAN_POINT('Ctrl Pts',(8.15273134873956,15.2,-6.64539993184436));
#175510=CARTESIAN_POINT('Ctrl Pts',(8.15591034657417,15.2,-6.64712038194146));
#175511=CARTESIAN_POINT('Ctrl Pts',(8.15908934412002,15.2,-6.64884083188229));
#175512=CARTESIAN_POINT('Ctrl Pts',(8.16231231913521,15.2,-6.65057373512171));
#175513=CARTESIAN_POINT('Ctrl Pts',(8.1655789546832,15.2,-6.65231841597499));
#175514=CARTESIAN_POINT('Ctrl Pts',(8.16884559023117,15.2,-6.65406309682827));
#175515=CARTESIAN_POINT('Ctrl Pts',(8.17215588798237,15.2,-6.6558195550556));
#175516=CARTESIAN_POINT('Ctrl Pts',(8.17550953269222,15.2,-6.65758713107903));
#175517=CARTESIAN_POINT('Ctrl Pts',(8.1788631777067,15.2,-6.65935470726302));
#175518=CARTESIAN_POINT('Ctrl Pts',(8.18226017085943,15.2,-6.66113339979679));
#175519=CARTESIAN_POINT('Ctrl Pts',(8.18570020263318,15.2,-6.66292256589502));
#175520=CARTESIAN_POINT('Ctrl Pts',(8.18914023409444,15.2,-6.66471173183071));
#175521=CARTESIAN_POINT('Ctrl Pts',(8.19262330411346,15.2,-6.66651136898332));
#175522=CARTESIAN_POINT('Ctrl Pts',(8.19614910850148,15.2,-6.66832084800916));
#175523=CARTESIAN_POINT('Ctrl Pts',(8.1996749128895,15.2,-6.67013032703499));
#175524=CARTESIAN_POINT('Ctrl Pts',(8.20324344950296,15.2,-6.67194964697554));
#175525=CARTESIAN_POINT('Ctrl Pts',(8.20685441903658,15.2,-6.67377819115871));
#175526=CARTESIAN_POINT('Ctrl Pts',(8.20986356042394,15.2,-6.67530197803339));
#175527=CARTESIAN_POINT('Ctrl Pts',(8.21290216949537,15.2,-6.67683217109432));
#175528=CARTESIAN_POINT('Ctrl Pts',(8.21597007254941,15.2,-6.67836841894123));
#175529=CARTESIAN_POINT('Ctrl Pts',(8.21903797560345,15.2,-6.67990466678815));
#175530=CARTESIAN_POINT('Ctrl Pts',(8.22213517386183,15.2,-6.68144697092547));
#175531=CARTESIAN_POINT('Ctrl Pts',(8.22526149526484,15.2,-6.68299498697416));
#175532=CARTESIAN_POINT('Ctrl Pts',(8.22838781666784,15.2,-6.68454300302283));
#175533=CARTESIAN_POINT('Ctrl Pts',(8.23154326107765,15.2,-6.68609673040001));
#175534=CARTESIAN_POINT('Ctrl Pts',(8.2347276622582,15.2,-6.687655832275));
#175535=CARTESIAN_POINT('Ctrl Pts',(8.23791206343875,15.2,-6.68921493415));
#175536=CARTESIAN_POINT('Ctrl Pts',(8.24112541779795,15.2,-6.6907794097326));
#175537=CARTESIAN_POINT('Ctrl Pts',(8.24436756003498,15.2,-6.69234892751752));
#175538=CARTESIAN_POINT('Ctrl Pts',(8.247609702272,15.2,-6.69391844530244));
#175539=CARTESIAN_POINT('Ctrl Pts',(8.25088063221433,15.2,-6.69549300500863));
#175540=CARTESIAN_POINT('Ctrl Pts',(8.25418018346584,15.2,-6.69707228111999));
#175541=CARTESIAN_POINT('Ctrl Pts',(8.25747973471735,15.2,-6.69865155723135));
#175542=CARTESIAN_POINT('Ctrl Pts',(8.2608079052903,15.2,-6.70023554877035));
#175543=CARTESIAN_POINT('Ctrl Pts',(8.26416453494457,15.2,-6.70182393585391));
#175544=CARTESIAN_POINT('Ctrl Pts',(8.26819249038333,15.2,-6.70373000028493));
#175545=CARTESIAN_POINT('Ctrl Pts',(8.27226142321209,15.2,-6.7056423941518));
#175546=CARTESIAN_POINT('Ctrl Pts',(8.27637105274801,15.2,-6.70756057267414));
#175547=CARTESIAN_POINT('Ctrl Pts',(8.27979574415238,15.2,-6.70915905483416));
#175548=CARTESIAN_POINT('Ctrl Pts',(8.28324869616098,15.2,-6.71076155398333));
#175549=CARTESIAN_POINT('Ctrl Pts',(8.28672974921653,15.2,-6.71236776273334));
#175550=CARTESIAN_POINT('Ctrl Pts',(8.29021080227209,15.2,-6.71397397148333));
#175551=CARTESIAN_POINT('Ctrl Pts',(8.29371995550789,15.2,-6.71558388856021));
#175552=CARTESIAN_POINT('Ctrl Pts',(8.29725704871847,15.2,-6.71719721148422));
#175553=CARTESIAN_POINT('Ctrl Pts',(8.30079414192906,15.2,-6.71881053440822));
#175554=CARTESIAN_POINT('Ctrl Pts',(8.3043591753669,15.2,-6.72042726099468));
#175555=CARTESIAN_POINT('Ctrl Pts',(8.30795199078501,15.2,-6.72204709481429));
#175556=CARTESIAN_POINT('Ctrl Pts',(8.31154480620312,15.2,-6.7236669286339));
#175557=CARTESIAN_POINT('Ctrl Pts',(8.31516540310386,15.2,-6.72528986917287));
#175558=CARTESIAN_POINT('Ctrl Pts',(8.3188136237303,15.2,-6.72691562063135));
#175559=CARTESIAN_POINT('Ctrl Pts',(8.32246184435675,15.2,-6.72854137208984));
#175560=CARTESIAN_POINT('Ctrl Pts',(8.32613769026303,15.2,-6.73016993652323));
#175561=CARTESIAN_POINT('Ctrl Pts',(8.32984100345891,15.2,-6.73180102381503));
#175562=CARTESIAN_POINT('Ctrl Pts',(8.33354431665477,15.2,-6.73343211110683));
#175563=CARTESIAN_POINT('Ctrl Pts',(8.33727509776325,15.2,-6.73506572191915));
#175564=CARTESIAN_POINT('Ctrl Pts',(8.34103319274456,15.2,-6.73670157088991));
#175565=CARTESIAN_POINT('Ctrl Pts',(8.34479128772588,15.2,-6.73833741986068));
#175566=CARTESIAN_POINT('Ctrl Pts',(8.34857669571301,15.2,-6.73997550780325));
#175567=CARTESIAN_POINT('Ctrl Pts',(8.3523892630069,15.2,-6.74161555349786));
#175568=CARTESIAN_POINT('Ctrl Pts',(8.35543931659267,15.2,-6.74292758994629));
#175569=CARTESIAN_POINT('Ctrl Pts',(8.35850675181227,15.2,-6.74424087942508));
#175570=CARTESIAN_POINT('Ctrl Pts',(8.36159149144786,15.2,-6.7455552811509));
#175571=CARTESIAN_POINT('Ctrl Pts',(8.36467623150374,15.2,-6.74686968305581));
#175572=CARTESIAN_POINT('Ctrl Pts',(8.36777827623639,15.2,-6.74818519696456));
#175573=CARTESIAN_POINT('Ctrl Pts',(8.37089754645259,15.2,-6.74950168365771));
#175574=CARTESIAN_POINT('Ctrl Pts',(8.3740168162438,15.2,-6.7508181701715));
#175575=CARTESIAN_POINT('Ctrl Pts',(8.37715331159283,15.2,-6.75213562847229));
#175576=CARTESIAN_POINT('Ctrl Pts',(8.38030695650056,15.2,-6.75345392214225));
#175577=CARTESIAN_POINT('Ctrl Pts',(8.38346060183799,15.2,-6.75477221599183));
#175578=CARTESIAN_POINT('Ctrl Pts',(8.3866313966969,15.2,-6.7560913433665));
#175579=CARTESIAN_POINT('Ctrl Pts',(8.38981926276065,15.2,-6.75741116938291));
#175580=CARTESIAN_POINT('Ctrl Pts',(8.39300712839004,15.2,-6.7587309952195));
#175581=CARTESIAN_POINT('Ctrl Pts',(8.3962120660197,15.2,-6.7600515191087));
#175582=CARTESIAN_POINT('Ctrl Pts',(8.39943399924912,15.2,-6.76137260756665));
#175583=CARTESIAN_POINT('Ctrl Pts',(8.40265593291753,15.2,-6.7626936962046));
#175584=CARTESIAN_POINT('Ctrl Pts',(8.40589486317934,15.2,-6.7640153482388));
#175585=CARTESIAN_POINT('Ctrl Pts',(8.40915071252453,15.2,-6.76533743036643));
#175586=CARTESIAN_POINT('Ctrl Pts',(8.41240656142612,15.2,-6.76665951231393));
#175587=CARTESIAN_POINT('Ctrl Pts',(8.415679330241,15.2,-6.76798202511968));
#175588=CARTESIAN_POINT('Ctrl Pts',(8.41896894247038,15.2,-6.76930483823374));
#175589=CARTESIAN_POINT('Ctrl Pts',(8.42225855514796,15.2,-6.77062765152803));
#175590=CARTESIAN_POINT('Ctrl Pts',(8.42556501196421,15.2,-6.77195076309222));
#175591=CARTESIAN_POINT('Ctrl Pts',(8.42888823799381,15.2,-6.77327404522592));
#175592=CARTESIAN_POINT('Ctrl Pts',(8.43221146357063,15.2,-6.77459732717931));
#175593=CARTESIAN_POINT('Ctrl Pts',(8.43555145772161,15.2,-6.77592077960571));
#175594=CARTESIAN_POINT('Ctrl Pts',(8.43890814600107,15.2,-6.77724427277529));
#175595=CARTESIAN_POINT('Ctrl Pts',(8.44226483473787,15.2,-6.7785677661252));
#175596=CARTESIAN_POINT('Ctrl Pts',(8.44563821709011,15.2,-6.77989130153066));
#175597=CARTESIAN_POINT('Ctrl Pts',(8.44902821977487,15.2,-6.78121475099168));
#175598=CARTESIAN_POINT('Ctrl Pts',(8.45241822245964,15.2,-6.7825382004527));
#175599=CARTESIAN_POINT('Ctrl Pts',(8.45582484410188,15.2,-6.78386156511927));
#175600=CARTESIAN_POINT('Ctrl Pts',(8.45924801156791,15.2,-6.78518471869135));
#175601=CARTESIAN_POINT('Ctrl Pts',(8.46267117856753,15.2,-6.78650787208315));
#175602=CARTESIAN_POINT('Ctrl Pts',(8.46611089167832,15.2,-6.78783081717345));
#175603=CARTESIAN_POINT('Ctrl Pts',(8.46956707602253,15.2,-6.78915342651578));
#175604=CARTESIAN_POINT('Ctrl Pts',(8.47302326083764,15.2,-6.79047603603832));
#175605=CARTESIAN_POINT('Ctrl Pts',(8.47649591951185,15.2,-6.79179831183302));
#175606=CARTESIAN_POINT('Ctrl Pts',(8.47998497503701,15.2,-6.7931201306828));
#175607=CARTESIAN_POINT('Ctrl Pts',(8.48434629420578,15.2,-6.79477240415497));
#175608=CARTESIAN_POINT('Ctrl Pts',(8.48873323704162,15.2,-6.79642396448822));
#175609=CARTESIAN_POINT('Ctrl Pts',(8.49314565954369,15.2,-6.79807457622425));
#175610=CARTESIAN_POINT('Ctrl Pts',(8.49667559725679,15.2,-6.79939506550513));
#175611=CARTESIAN_POINT('Ctrl Pts',(8.50022184317258,15.2,-6.8007149468732));
#175612=CARTESIAN_POINT('Ctrl Pts',(8.50378432356412,15.2,-6.80203410221579));
#175613=CARTESIAN_POINT('Ctrl Pts',(8.50734680444106,15.2,-6.80335325773811));
#175614=CARTESIAN_POINT('Ctrl Pts',(8.51092552108452,15.2,-6.80467168701595));
#175615=CARTESIAN_POINT('Ctrl Pts',(8.51452039983765,15.2,-6.80598927119878));
#175616=CARTESIAN_POINT('Ctrl Pts',(8.51901399803416,15.2,-6.80763625133755));
#175617=CARTESIAN_POINT('Ctrl Pts',(8.5235328507533,15.2,-6.80928191254298));
#175618=CARTESIAN_POINT('Ctrl Pts',(8.52807681735257,15.2,-6.81092602768173));
#175619=CARTESIAN_POINT('Ctrl Pts',(8.53171199033481,15.2,-6.81224131968522));
#175620=CARTESIAN_POINT('Ctrl Pts',(8.53536323696391,15.2,-6.81355562115606));
#175621=CARTESIAN_POINT('Ctrl Pts',(8.53903048468072,15.2,-6.81486881849912));
#175622=CARTESIAN_POINT('Ctrl Pts',(8.54361454470147,15.2,-6.81651031531213));
#175623=CARTESIAN_POINT('Ctrl Pts',(8.54822360822211,15.2,-6.81815008554447));
#175624=CARTESIAN_POINT('Ctrl Pts',(8.55285753474988,15.2,-6.81978790901669));
#175625=CARTESIAN_POINT('Ctrl Pts',(8.55656467617414,15.2,-6.82109816786587));
#175626=CARTESIAN_POINT('Ctrl Pts',(8.56028773008913,15.2,-6.82240717878159));
#175627=CARTESIAN_POINT('Ctrl Pts',(8.56402662629453,15.2,-6.82371483296382));
#175628=CARTESIAN_POINT('Ctrl Pts',(8.56776552199051,15.2,-6.8250224869679));
#175629=CARTESIAN_POINT('Ctrl Pts',(8.5715202608996,15.2,-6.82632878219154));
#175630=CARTESIAN_POINT('Ctrl Pts',(8.57529077049732,15.2,-6.82763360825747));
#175631=CARTESIAN_POINT('Ctrl Pts',(8.57906128060877,15.2,-6.82893843450118));
#175632=CARTESIAN_POINT('Ctrl Pts',(8.58284756169325,15.2,-6.8302417913643));
#175633=CARTESIAN_POINT('Ctrl Pts',(8.58664954517985,15.2,-6.83154357021286));
#175634=CARTESIAN_POINT('Ctrl Pts',(8.59045152814842,15.2,-6.83284534888406));
#175635=CARTESIAN_POINT('Ctrl Pts',(8.59426921194549,15.2,-6.83414554742212));
#175636=CARTESIAN_POINT('Ctrl Pts',(8.59810252818666,15.2,-6.83544406009385));
#175637=CARTESIAN_POINT('Ctrl Pts',(8.60193584495011,15.2,-6.83674257294251));
#175638=CARTESIAN_POINT('Ctrl Pts',(8.60578479237932,15.2,-6.83803939856874));
#175639=CARTESIAN_POINT('Ctrl Pts',(8.60964930309095,15.2,-6.8393344296392));
#175640=CARTESIAN_POINT('Ctrl Pts',(8.61351381327604,15.2,-6.84062946053322));
#175641=CARTESIAN_POINT('Ctrl Pts',(8.61739388405433,15.2,-6.84192269777852));
#175642=CARTESIAN_POINT('Ctrl Pts',(8.62128944915137,15.2,-6.84321403457097));
#175643=CARTESIAN_POINT('Ctrl Pts',(8.62518501477918,15.2,-6.84450537153935));
#175644=CARTESIAN_POINT('Ctrl Pts',(8.62909607442824,15.2,-6.84579480803522));
#175645=CARTESIAN_POINT('Ctrl Pts',(8.63302255608769,15.2,-6.84708223910525));
#175646=CARTESIAN_POINT('Ctrl Pts',(8.63694903721214,15.2,-6.84836966999987));
#175647=CARTESIAN_POINT('Ctrl Pts',(8.64089094235293,15.2,-6.84965509620877));
#175648=CARTESIAN_POINT('Ctrl Pts',(8.64484820386122,15.2,-6.85093841304854));
#175649=CARTESIAN_POINT('Ctrl Pts',(8.64880546590867,15.2,-6.85222173006314));
#175650=CARTESIAN_POINT('Ctrl Pts',(8.65277808228654,15.2,-6.85350293838371));
#175651=CARTESIAN_POINT('Ctrl Pts',(8.65676598524427,15.2,-6.85478193529256));
#175652=CARTESIAN_POINT('Ctrl Pts',(8.66075388765865,15.2,-6.85606093202714));
#175653=CARTESIAN_POINT('Ctrl Pts',(8.66475707897294,15.2,-6.85733771569004));
#175654=CARTESIAN_POINT('Ctrl Pts',(8.66877548730955,15.2,-6.85861218780832));
#175655=CARTESIAN_POINT('Ctrl Pts',(8.67279389619365,15.2,-6.85988666010024));
#175656=CARTESIAN_POINT('Ctrl Pts',(8.67682752460145,15.2,-6.86115881834193));
#175657=CARTESIAN_POINT('Ctrl Pts',(8.68087630226655,15.2,-6.86242856330003));
#175658=CARTESIAN_POINT('Ctrl Pts',(8.68492507993166,15.2,-6.86369830825812));
#175659=CARTESIAN_POINT('Ctrl Pts',(8.68898900972352,15.2,-6.8649656394576));
#175660=CARTESIAN_POINT('Ctrl Pts',(8.69306802189181,15.2,-6.86623045724849));
#175661=CARTESIAN_POINT('Ctrl Pts',(8.69714703350433,15.2,-6.86749527486705));
#175662=CARTESIAN_POINT('Ctrl Pts',(8.70124112912272,15.2,-6.86875757934641));
#175663=CARTESIAN_POINT('Ctrl Pts',(8.70535023897209,15.2,-6.87001727224917));
#175664=CARTESIAN_POINT('Ctrl Pts',(8.70945934938132,15.2,-6.87127696532355));
#175665=CARTESIAN_POINT('Ctrl Pts',(8.71358347672731,15.2,-6.8725340465287));
#175666=CARTESIAN_POINT('Ctrl Pts',(8.71772255217663,15.2,-6.87378841943011));
#175667=CARTESIAN_POINT('Ctrl Pts',(8.721861627062,15.2,-6.87504279216062));
#175668=CARTESIAN_POINT('Ctrl Pts',(8.72601564996489,15.2,-6.87629445526927));
#175669=CARTESIAN_POINT('Ctrl Pts',(8.73018455490089,15.2,-6.87754331288957));
#175670=CARTESIAN_POINT('Ctrl Pts',(8.73435346040489,15.2,-6.87879217068005));
#175671=CARTESIAN_POINT('Ctrl Pts',(8.7385372481999,15.2,-6.88003822355357));
#175672=CARTESIAN_POINT('Ctrl Pts',(8.74273585058421,15.2,-6.8812813754054));
#175673=CARTESIAN_POINT('Ctrl Pts',(8.74693445239646,15.2,-6.88252452708784));
#175674=CARTESIAN_POINT('Ctrl Pts',(8.75114786818987,15.2,-6.88376477758314));
#175675=CARTESIAN_POINT('Ctrl Pts',(8.75537603262104,15.2,-6.88500203314885));
#175676=CARTESIAN_POINT('Ctrl Pts',(8.7596041976283,15.2,-6.88623928888314));
#175677=CARTESIAN_POINT('Ctrl Pts',(8.76384711333453,15.2,-6.88747354908375));
#175678=CARTESIAN_POINT('Ctrl Pts',(8.76810470962308,15.2,-6.88870472081731));
#175679=CARTESIAN_POINT('Ctrl Pts',(8.77236230533153,15.2,-6.88993589238313));
#175680=CARTESIAN_POINT('Ctrl Pts',(8.77663458354881,15.2,-6.89116397516093));
#175681=CARTESIAN_POINT('Ctrl Pts',(8.78092147807791,15.2,-6.89238887678894));
#175682=CARTESIAN_POINT('Ctrl Pts',(8.78413664912077,15.2,-6.89330755305166));
#175683=CARTESIAN_POINT('Ctrl Pts',(8.78736004216393,15.2,-6.89422443911686));
#175684=CARTESIAN_POINT('Ctrl Pts',(8.79059162904541,15.2,-6.89513949829221));
#175685=CARTESIAN_POINT('Ctrl Pts',(8.79382321651396,15.2,-6.89605455763379));
#175686=CARTESIAN_POINT('Ctrl Pts',(8.79706299876813,15.2,-6.89696778848317));
#175687=CARTESIAN_POINT('Ctrl Pts',(8.80031094669962,15.2,-6.89787915240704));
#175688=CARTESIAN_POINT('Ctrl Pts',(8.80355889404106,15.2,-6.89879051616534));
#175689=CARTESIAN_POINT('Ctrl Pts',(8.80681500675705,15.2,-6.89970001343207));
#175690=CARTESIAN_POINT('Ctrl Pts',(8.81007925863916,15.2,-6.90060760660726));
#175691=CARTESIAN_POINT('Ctrl Pts',(8.81334351052127,15.2,-6.90151519978245));
#175692=CARTESIAN_POINT('Ctrl Pts',(8.81661590182379,15.2,-6.90242088749626));
#175693=CARTESIAN_POINT('Ctrl Pts',(8.8198964037612,15.2,-6.90332463325918));
#175694=CARTESIAN_POINT('Ctrl Pts',(8.82427040614576,15.2,-6.90452962755502));
#175695=CARTESIAN_POINT('Ctrl Pts',(8.82865882812198,15.2,-6.90573116845173));
#175696=CARTESIAN_POINT('Ctrl Pts',(8.83306160503838,15.2,-6.90692916735415));
#175697=CARTESIAN_POINT('Ctrl Pts',(8.83636368847552,15.2,-6.907827666735));
#175698=CARTESIAN_POINT('Ctrl Pts',(8.83967384675659,15.2,-6.90872417309864));
#175699=CARTESIAN_POINT('Ctrl Pts',(8.84299205173993,15.2,-6.90961865093669));
#175700=CARTESIAN_POINT('Ctrl Pts',(8.84631025612047,15.2,-6.91051312861225));
#175701=CARTESIAN_POINT('Ctrl Pts',(8.84963650746724,15.2,-6.91140557539624));
#175702=CARTESIAN_POINT('Ctrl Pts',(8.85297077888846,15.2,-6.91229595661371));
#175703=CARTESIAN_POINT('Ctrl Pts',(8.85630505030968,15.2,-6.91318633783118));
#175704=CARTESIAN_POINT('Ctrl Pts',(8.85964734197608,15.2,-6.91407465216235));
#175705=CARTESIAN_POINT('Ctrl Pts',(8.86299762545293,15.2,-6.91496086350917));
#175706=CARTESIAN_POINT('Ctrl Pts',(8.8663479089298,15.2,-6.91584707485598));
#175707=CARTESIAN_POINT('Ctrl Pts',(8.86970618587056,15.2,-6.91673118386059));
#175708=CARTESIAN_POINT('Ctrl Pts',(8.87307242772183,15.2,-6.91761315270756));
#175709=CARTESIAN_POINT('Ctrl Pts',(8.87643866957311,15.2,-6.91849512155453));
#175710=CARTESIAN_POINT('Ctrl Pts',(8.8798128768216,15.2,-6.91937495058603));
#175711=CARTESIAN_POINT('Ctrl Pts',(8.88319502219804,15.2,-6.920252604846));
#175712=CARTESIAN_POINT('Ctrl Pts',(8.88657716757447,15.2,-6.92113025910596));
#175713=CARTESIAN_POINT('Ctrl Pts',(8.889967250867,15.2,-6.92200573824108));
#175714=CARTESIAN_POINT('Ctrl Pts',(8.8933652462008,15.2,-6.92287900508466));
#175715=CARTESIAN_POINT('Ctrl Pts',(8.89676324215189,15.2,-6.92375227208687));
#175716=CARTESIAN_POINT('Ctrl Pts',(8.90016914879689,15.2,-6.9246233281468));
#175717=CARTESIAN_POINT('Ctrl Pts',(8.90358293975244,15.2,-6.92549213668943));
#175718=CARTESIAN_POINT('Ctrl Pts',(8.90699673008781,15.2,-6.92636094507422));
#175719=CARTESIAN_POINT('Ctrl Pts',(8.91041840489919,15.2,-6.92722750737238));
#175720=CARTESIAN_POINT('Ctrl Pts',(8.91384793694683,15.2,-6.92809178767556));
#175721=CARTESIAN_POINT('Ctrl Pts',(8.91727746899448,15.2,-6.92895606797873));
#175722=CARTESIAN_POINT('Ctrl Pts',(8.92071485800005,15.2,-6.9298180650918));
#175723=CARTESIAN_POINT('Ctrl Pts',(8.92416007737555,15.2,-6.93067774585203));
#175724=CARTESIAN_POINT('Ctrl Pts',(8.92760529675105,15.2,-6.93153742661226));
#175725=CARTESIAN_POINT('Ctrl Pts',(8.93105834645897,15.2,-6.93239478966444));
#175726=CARTESIAN_POINT('Ctrl Pts',(8.93451920029155,15.2,-6.93324980100837));
#175727=CARTESIAN_POINT('Ctrl Pts',(8.93798005412414,15.2,-6.9341048123523));
#175728=CARTESIAN_POINT('Ctrl Pts',(8.94144871118141,15.2,-6.93495747230466));
#175729=CARTESIAN_POINT('Ctrl Pts',(8.94492514463776,15.2,-6.93580774514898));
#175730=CARTESIAN_POINT('Ctrl Pts',(8.94840157809411,15.2,-6.9366580179933));
#175731=CARTESIAN_POINT('Ctrl Pts',(8.95188578906658,15.2,-6.9375059040961));
#175732=CARTESIAN_POINT('Ctrl Pts',(8.95537774998032,15.2,-6.93835137031572));
#175733=CARTESIAN_POINT('Ctrl Pts',(8.95886971152843,15.2,-6.93919683668892));
#175734=CARTESIAN_POINT('Ctrl Pts',(8.96236942322039,15.2,-6.94003988076145));
#175735=CARTESIAN_POINT('Ctrl Pts',(8.96587685823119,15.2,-6.94088047117494));
#175736=CARTESIAN_POINT('Ctrl Pts',(8.9693842926048,15.2,-6.94172106143573));
#175737=CARTESIAN_POINT('Ctrl Pts',(8.97289945094933,15.2,-6.94255919708392));
#175738=CARTESIAN_POINT('Ctrl Pts',(8.97642230599822,15.2,-6.94339484397002));
#175739=CARTESIAN_POINT('Ctrl Pts',(8.97994516104711,15.2,-6.94423049085612));
#175740=CARTESIAN_POINT('Ctrl Pts',(8.98347571304691,15.2,-6.94506364925427));
#175741=CARTESIAN_POINT('Ctrl Pts',(8.98701393541902,15.2,-6.94589428559886));
#175742=CARTESIAN_POINT('Ctrl Pts',(8.99055215779113,15.2,-6.94672492194347));
#175743=CARTESIAN_POINT('Ctrl Pts',(8.99409804994567,15.2,-6.94755303563003));
#175744=CARTESIAN_POINT('Ctrl Pts',(8.99765158677489,15.2,-6.9483785940167));
#175745=CARTESIAN_POINT('Ctrl Pts',(9.00238963631089,15.2,-6.94947933863225));
#175746=CARTESIAN_POINT('Ctrl Pts',(9.00714127398459,15.2,-6.95057554109726));
#175747=CARTESIAN_POINT('Ctrl Pts',(9.011906439579,15.2,-6.95166712171184));
#175748=CARTESIAN_POINT('Ctrl Pts',(9.01548031345019,15.2,-6.9524858070984));
#175749=CARTESIAN_POINT('Ctrl Pts',(9.01906179657791,15.2,-6.95330189324661));
#175750=CARTESIAN_POINT('Ctrl Pts',(9.02265086121103,15.2,-6.95411534763239));
#175751=CARTESIAN_POINT('Ctrl Pts',(9.02623992584414,15.2,-6.95492880201817));
#175752=CARTESIAN_POINT('Ctrl Pts',(9.02983657273984,15.2,-6.95573962368434));
#175753=CARTESIAN_POINT('Ctrl Pts',(9.03344077565121,15.2,-6.95654778007141));
#175754=CARTESIAN_POINT('Ctrl Pts',(9.03704497856259,15.2,-6.95735593645849));
#175755=CARTESIAN_POINT('Ctrl Pts',(9.04065673728139,15.2,-6.9581614281292));
#175756=CARTESIAN_POINT('Ctrl Pts',(9.04427602623322,15.2,-6.9589642235167));
#175757=CARTESIAN_POINT('Ctrl Pts',(9.04789531518505,15.2,-6.9597670189042));
#175758=CARTESIAN_POINT('Ctrl Pts',(9.05152213511992,15.2,-6.96056711802514));
#175759=CARTESIAN_POINT('Ctrl Pts',(9.05515645857055,15.2,-6.96136448837141));
#175760=CARTESIAN_POINT('Ctrl Pts',(9.05879078202118,15.2,-6.96216185871767));
#175761=CARTESIAN_POINT('Ctrl Pts',(9.06243261019506,15.2,-6.96295649975236));
#175762=CARTESIAN_POINT('Ctrl Pts',(9.06608191474392,15.2,-6.9637483795968));
#175763=CARTESIAN_POINT('Ctrl Pts',(9.07094765458435,15.2,-6.96480421948529));
#175764=CARTESIAN_POINT('Ctrl Pts',(9.07582668513524,15.2,-6.96585514807604));
#175765=CARTESIAN_POINT('Ctrl Pts',(9.08071894812496,15.2,-6.96690109407716));
#175766=CARTESIAN_POINT('Ctrl Pts',(9.08438814503396,15.2,-6.96768555350675));
#175767=CARTESIAN_POINT('Ctrl Pts',(9.08806478513374,15.2,-6.968467210345));
#175768=CARTESIAN_POINT('Ctrl Pts',(9.09174884449989,15.2,-6.96924603623337));
#175769=CARTESIAN_POINT('Ctrl Pts',(9.09666092410094,15.2,-6.97028447084552));
#175770=CARTESIAN_POINT('Ctrl Pts',(9.1015861961174,15.2,-6.97131787373208));
#175771=CARTESIAN_POINT('Ctrl Pts',(9.10652458633233,15.2,-6.97234615817649));
#175772=CARTESIAN_POINT('Ctrl Pts',(9.11022837865709,15.2,-6.97311737143975));
#175773=CARTESIAN_POINT('Ctrl Pts',(9.11393954876789,15.2,-6.97388570387134));
#175774=CARTESIAN_POINT('Ctrl Pts',(9.11765806998607,15.2,-6.97465112288143));
#175775=CARTESIAN_POINT('Ctrl Pts',(9.12137659120426,15.2,-6.97541654189152));
#175776=CARTESIAN_POINT('Ctrl Pts',(9.12510246279873,15.2,-6.97617904627868));
#175777=CARTESIAN_POINT('Ctrl Pts',(9.12883567209274,15.2,-6.9769386231241));
#175778=CARTESIAN_POINT('Ctrl Pts',(9.13256888138674,15.2,-6.97769819996954));
#175779=CARTESIAN_POINT('Ctrl Pts',(9.13630943331908,15.2,-6.9784548508631));
#175780=CARTESIAN_POINT('Ctrl Pts',(9.14005731399994,15.2,-6.97920857100002));
#175781=CARTESIAN_POINT('Ctrl Pts',(8.02901631899994,12.2,-6.57080831800001));
#175782=CARTESIAN_POINT('Ctrl Pts',(8.03049110016105,12.2,-6.57181686697944));
#175783=CARTESIAN_POINT('Ctrl Pts',(8.03201610877769,12.2,-6.57285322878717));
#175784=CARTESIAN_POINT('Ctrl Pts',(8.03359089353572,12.2,-6.5739163521752));
#175785=CARTESIAN_POINT('Ctrl Pts',(8.03517327270188,12.2,-6.57498460248157));
#175786=CARTESIAN_POINT('Ctrl Pts',(8.03680591622578,12.2,-6.5760798659982));
#175787=CARTESIAN_POINT('Ctrl Pts',(8.0384883906544,12.2,-6.57720107836683));
#175788=CARTESIAN_POINT('Ctrl Pts',(8.04017086493022,12.2,-6.5783222906336));
#175789=CARTESIAN_POINT('Ctrl Pts',(8.04190317335625,12.2,-6.57946945420923));
#175790=CARTESIAN_POINT('Ctrl Pts',(8.04368489154152,12.2,-6.58064153749996));
#175791=CARTESIAN_POINT('Ctrl Pts',(8.04546660972677,12.2,-6.5818136207907));
#175792=CARTESIAN_POINT('Ctrl Pts',(8.04729774128699,12.2,-6.58301062499168));
#175793=CARTESIAN_POINT('Ctrl Pts',(8.04917787055977,12.2,-6.58423155042359));
#175794=CARTESIAN_POINT('Ctrl Pts',(8.05105800000331,12.2,-6.5854524759664));
#175795=CARTESIAN_POINT('Ctrl Pts',(8.05298713001268,12.2,-6.58669732252585));
#175796=CARTESIAN_POINT('Ctrl Pts',(8.05496485620711,12.2,-6.58796512017984));
#175797=CARTESIAN_POINT('Ctrl Pts',(8.05694258222188,12.2,-6.58923291771867));
#175798=CARTESIAN_POINT('Ctrl Pts',(8.05896890494999,12.2,-6.59052366460892));
#175799=CARTESIAN_POINT('Ctrl Pts',(8.0610434290508,12.2,-6.59183642123391));
#175800=CARTESIAN_POINT('Ctrl Pts',(8.06311795315161,12.2,-6.59314917785888));
#175801=CARTESIAN_POINT('Ctrl Pts',(8.06524067911272,12.2,-6.59448394143469));
#175802=CARTESIAN_POINT('Ctrl Pts',(8.0674112193651,12.2,-6.59583979613451));
#175803=CARTESIAN_POINT('Ctrl Pts',(8.06958175981464,12.2,-6.59719565095748));
#175804=CARTESIAN_POINT('Ctrl Pts',(8.07180011545347,12.2,-6.59857259622476));
#175805=CARTESIAN_POINT('Ctrl Pts',(8.07406590574684,12.2,-6.5999697421356));
#175806=CARTESIAN_POINT('Ctrl Pts',(8.0763316958344,12.2,-6.60136688791955));
#175807=CARTESIAN_POINT('Ctrl Pts',(8.07864492166241,12.2,-6.60278423372139));
#175808=CARTESIAN_POINT('Ctrl Pts',(8.08100520891203,12.2,-6.6042209115867));
#175809=CARTESIAN_POINT('Ctrl Pts',(8.08336549616167,12.2,-6.605657589452));
#175810=CARTESIAN_POINT('Ctrl Pts',(8.08577284714085,12.2,-6.60711359752408));
#175811=CARTESIAN_POINT('Ctrl Pts',(8.08822689338298,12.2,-6.60858809463637));
#175812=CARTESIAN_POINT('Ctrl Pts',(8.09068093962512,12.2,-6.61006259174866));
#175813=CARTESIAN_POINT('Ctrl Pts',(8.09318168337629,12.2,-6.61155557734142));
#175814=CARTESIAN_POINT('Ctrl Pts',(8.09572876369724,12.2,-6.61306622661866));
#175815=CARTESIAN_POINT('Ctrl Pts',(8.09827584424958,12.2,-6.61457687603312));
#175816=CARTESIAN_POINT('Ctrl Pts',(8.10086926328141,12.2,-6.61610519224932));
#175817=CARTESIAN_POINT('Ctrl Pts',(8.10350866492724,12.2,-6.61765036983427));
#175818=CARTESIAN_POINT('Ctrl Pts',(8.10614806633333,12.2,-6.61919554727886));
#175819=CARTESIAN_POINT('Ctrl Pts',(8.1088334533189,12.2,-6.62075759161615));
#175820=CARTESIAN_POINT('Ctrl Pts',(8.11156447473195,12.2,-6.6223357152326));
#175821=CARTESIAN_POINT('Ctrl Pts',(8.114295496145,12.2,-6.62391383884905));
#175822=CARTESIAN_POINT('Ctrl Pts',(8.11707215585626,12.2,-6.62550804652576));
#175823=CARTESIAN_POINT('Ctrl Pts',(8.11989411016728,12.2,-6.62711757488289));
#175824=CARTESIAN_POINT('Ctrl Pts',(8.12271606473465,12.2,-6.62872710338622));
#175825=CARTESIAN_POINT('Ctrl Pts',(8.12558331191476,12.2,-6.6303519509994));
#175826=CARTESIAN_POINT('Ctrl Pts',(8.12849551940877,12.2,-6.6319913775894));
#175827=CARTESIAN_POINT('Ctrl Pts',(8.13140772663827,12.2,-6.63363080403048));
#175828=CARTESIAN_POINT('Ctrl Pts',(8.13436489026073,12.2,-6.63528480749396));
#175829=CARTESIAN_POINT('Ctrl Pts',(8.13736668249851,12.2,-6.63695266402424));
#175830=CARTESIAN_POINT('Ctrl Pts',(8.14036847473629,12.2,-6.63862052055451));
#175831=CARTESIAN_POINT('Ctrl Pts',(8.143414891645,12.2,-6.64030222865274));
#175832=CARTESIAN_POINT('Ctrl Pts',(8.14650561086298,12.2,-6.64199708134025));
#175833=CARTESIAN_POINT('Ctrl Pts',(8.14959633036172,12.2,-6.64369193418172));
#175834=CARTESIAN_POINT('Ctrl Pts',(8.15273134873956,12.2,-6.64539993184436));
#175835=CARTESIAN_POINT('Ctrl Pts',(8.15591034657417,12.2,-6.64712038194146));
#175836=CARTESIAN_POINT('Ctrl Pts',(8.15908934412002,12.2,-6.64884083188229));
#175837=CARTESIAN_POINT('Ctrl Pts',(8.16231231913522,12.2,-6.65057373512172));
#175838=CARTESIAN_POINT('Ctrl Pts',(8.16557895468321,12.2,-6.652318415975));
#175839=CARTESIAN_POINT('Ctrl Pts',(8.16884559023118,12.2,-6.65406309682828));
#175840=CARTESIAN_POINT('Ctrl Pts',(8.17215588798237,12.2,-6.6558195550556));
#175841=CARTESIAN_POINT('Ctrl Pts',(8.17550953269222,12.2,-6.65758713107903));
#175842=CARTESIAN_POINT('Ctrl Pts',(8.1788631777067,12.2,-6.65935470726302));
#175843=CARTESIAN_POINT('Ctrl Pts',(8.18226017085943,12.2,-6.66113339979679));
#175844=CARTESIAN_POINT('Ctrl Pts',(8.18570020263318,12.2,-6.66292256589502));
#175845=CARTESIAN_POINT('Ctrl Pts',(8.18914023409444,12.2,-6.66471173183071));
#175846=CARTESIAN_POINT('Ctrl Pts',(8.19262330411346,12.2,-6.66651136898332));
#175847=CARTESIAN_POINT('Ctrl Pts',(8.19614910850148,12.2,-6.66832084800916));
#175848=CARTESIAN_POINT('Ctrl Pts',(8.1996749128895,12.2,-6.67013032703499));
#175849=CARTESIAN_POINT('Ctrl Pts',(8.20324344950297,12.2,-6.67194964697555));
#175850=CARTESIAN_POINT('Ctrl Pts',(8.20685441903659,12.2,-6.67377819115872));
#175851=CARTESIAN_POINT('Ctrl Pts',(8.20986356042395,12.2,-6.67530197803339));
#175852=CARTESIAN_POINT('Ctrl Pts',(8.21290216949536,12.2,-6.67683217109432));
#175853=CARTESIAN_POINT('Ctrl Pts',(8.21597007254941,12.2,-6.67836841894123));
#175854=CARTESIAN_POINT('Ctrl Pts',(8.21903797560345,12.2,-6.67990466678815));
#175855=CARTESIAN_POINT('Ctrl Pts',(8.22213517386183,12.2,-6.68144697092547));
#175856=CARTESIAN_POINT('Ctrl Pts',(8.22526149526484,12.2,-6.68299498697416));
#175857=CARTESIAN_POINT('Ctrl Pts',(8.22838781666785,12.2,-6.68454300302284));
#175858=CARTESIAN_POINT('Ctrl Pts',(8.23154326107765,12.2,-6.68609673040001));
#175859=CARTESIAN_POINT('Ctrl Pts',(8.2347276622582,12.2,-6.687655832275));
#175860=CARTESIAN_POINT('Ctrl Pts',(8.23791206343875,12.2,-6.68921493415));
#175861=CARTESIAN_POINT('Ctrl Pts',(8.24112541779795,12.2,-6.6907794097326));
#175862=CARTESIAN_POINT('Ctrl Pts',(8.24436756003497,12.2,-6.69234892751752));
#175863=CARTESIAN_POINT('Ctrl Pts',(8.247609702272,12.2,-6.69391844530244));
#175864=CARTESIAN_POINT('Ctrl Pts',(8.25088063221432,12.2,-6.69549300500862));
#175865=CARTESIAN_POINT('Ctrl Pts',(8.25418018346583,12.2,-6.69707228111998));
#175866=CARTESIAN_POINT('Ctrl Pts',(8.25747973471734,12.2,-6.69865155723135));
#175867=CARTESIAN_POINT('Ctrl Pts',(8.2608079052903,12.2,-6.70023554877035));
#175868=CARTESIAN_POINT('Ctrl Pts',(8.26416453494457,12.2,-6.70182393585391));
#175869=CARTESIAN_POINT('Ctrl Pts',(8.26752116459883,12.2,-6.70341232293748));
#175870=CARTESIAN_POINT('Ctrl Pts',(8.27090625117372,12.2,-6.70500510627755));
#175871=CARTESIAN_POINT('Ctrl Pts',(8.27431963113788,12.2,-6.70660196851039));
#175872=CARTESIAN_POINT('Ctrl Pts',(8.27773301110205,12.2,-6.70819883074322));
#175873=CARTESIAN_POINT('Ctrl Pts',(8.28117468484588,12.2,-6.70979977331515));
#175874=CARTESIAN_POINT('Ctrl Pts',(8.28464449123708,12.2,-6.71140448546824));
#175875=CARTESIAN_POINT('Ctrl Pts',(8.28811429762827,12.2,-6.71300919762133));
#175876=CARTESIAN_POINT('Ctrl Pts',(8.29161223679768,12.2,-6.71461768115501));
#175877=CARTESIAN_POINT('Ctrl Pts',(8.2951381474944,12.2,-6.71622962921085));
#175878=CARTESIAN_POINT('Ctrl Pts',(8.29866405780679,12.2,-6.71784157709098));
#175879=CARTESIAN_POINT('Ctrl Pts',(8.30221794072407,12.2,-6.71945699085943));
#175880=CARTESIAN_POINT('Ctrl Pts',(8.3057996359564,12.2,-6.72107556957163));
#175881=CARTESIAN_POINT('Ctrl Pts',(8.30938133157914,12.2,-6.72269414846026));
#175882=CARTESIAN_POINT('Ctrl Pts',(8.3129908419153,12.2,-6.72431589354331));
#175883=CARTESIAN_POINT('Ctrl Pts',(8.31662800677414,12.2,-6.72594050902918));
#175884=CARTESIAN_POINT('Ctrl Pts',(8.32026517163299,12.2,-6.72756512451505));
#175885=CARTESIAN_POINT('Ctrl Pts',(8.32392999151359,12.2,-6.72919260987033));
#175886=CARTESIAN_POINT('Ctrl Pts',(8.32762231206693,12.2,-6.73082267632846));
#175887=CARTESIAN_POINT('Ctrl Pts',(8.33131463262026,12.2,-6.73245274278659));
#175888=CARTESIAN_POINT('Ctrl Pts',(8.33503444951857,12.2,-6.73408539065649));
#175889=CARTESIAN_POINT('Ctrl Pts',(8.33878161352332,12.2,-6.73572033233523));
#175890=CARTESIAN_POINT('Ctrl Pts',(8.34252877752806,12.2,-6.73735527401396));
#175891=CARTESIAN_POINT('Ctrl Pts',(8.34630328487505,12.2,-6.73899251140958));
#175892=CARTESIAN_POINT('Ctrl Pts',(8.35010498223474,12.2,-6.74063176286782));
#175893=CARTESIAN_POINT('Ctrl Pts',(8.35390667959444,12.2,-6.74227101432605));
#175894=CARTESIAN_POINT('Ctrl Pts',(8.35773556658815,12.2,-6.74391227885931));
#175895=CARTESIAN_POINT('Ctrl Pts',(8.36159149144786,12.2,-6.7455552811509));
#175896=CARTESIAN_POINT('Ctrl Pts',(8.36467623150374,12.2,-6.74686968305581));
#175897=CARTESIAN_POINT('Ctrl Pts',(8.36777827623639,12.2,-6.74818519696456));
#175898=CARTESIAN_POINT('Ctrl Pts',(8.37089754645259,12.2,-6.74950168365771));
#175899=CARTESIAN_POINT('Ctrl Pts',(8.3740168162438,12.2,-6.7508181701715));
#175900=CARTESIAN_POINT('Ctrl Pts',(8.37715331159283,12.2,-6.75213562847229));
#175901=CARTESIAN_POINT('Ctrl Pts',(8.38030695650056,12.2,-6.75345392214225));
#175902=CARTESIAN_POINT('Ctrl Pts',(8.38346060183799,12.2,-6.75477221599183));
#175903=CARTESIAN_POINT('Ctrl Pts',(8.3866313966969,12.2,-6.7560913433665));
#175904=CARTESIAN_POINT('Ctrl Pts',(8.38981926276065,12.2,-6.75741116938291));
#175905=CARTESIAN_POINT('Ctrl Pts',(8.39300712839004,12.2,-6.7587309952195));
#175906=CARTESIAN_POINT('Ctrl Pts',(8.3962120660197,12.2,-6.7600515191087));
#175907=CARTESIAN_POINT('Ctrl Pts',(8.39943399924911,12.2,-6.76137260756665));
#175908=CARTESIAN_POINT('Ctrl Pts',(8.40265593291753,12.2,-6.7626936962046));
#175909=CARTESIAN_POINT('Ctrl Pts',(8.40589486317934,12.2,-6.7640153482388));
#175910=CARTESIAN_POINT('Ctrl Pts',(8.40915071252453,12.2,-6.76533743036643));
#175911=CARTESIAN_POINT('Ctrl Pts',(8.41240656142612,12.2,-6.76665951231393));
#175912=CARTESIAN_POINT('Ctrl Pts',(8.415679330241,12.2,-6.76798202511968));
#175913=CARTESIAN_POINT('Ctrl Pts',(8.41896894247037,12.2,-6.76930483823374));
#175914=CARTESIAN_POINT('Ctrl Pts',(8.42225855514795,12.2,-6.77062765152802));
#175915=CARTESIAN_POINT('Ctrl Pts',(8.42556501196421,12.2,-6.77195076309222));
#175916=CARTESIAN_POINT('Ctrl Pts',(8.42888823799381,12.2,-6.77327404522592));
#175917=CARTESIAN_POINT('Ctrl Pts',(8.43221146357063,12.2,-6.77459732717931));
#175918=CARTESIAN_POINT('Ctrl Pts',(8.43555145772162,12.2,-6.77592077960571));
#175919=CARTESIAN_POINT('Ctrl Pts',(8.43890814600108,12.2,-6.7772442727753));
#175920=CARTESIAN_POINT('Ctrl Pts',(8.44226483473788,12.2,-6.77856776612521));
#175921=CARTESIAN_POINT('Ctrl Pts',(8.44563821709011,12.2,-6.77989130153066));
#175922=CARTESIAN_POINT('Ctrl Pts',(8.44902821977488,12.2,-6.78121475099168));
#175923=CARTESIAN_POINT('Ctrl Pts',(8.45241822245964,12.2,-6.7825382004527));
#175924=CARTESIAN_POINT('Ctrl Pts',(8.45582484410188,12.2,-6.78386156511927));
#175925=CARTESIAN_POINT('Ctrl Pts',(8.45924801156791,12.2,-6.78518471869135));
#175926=CARTESIAN_POINT('Ctrl Pts',(8.46267117856753,12.2,-6.78650787208315));
#175927=CARTESIAN_POINT('Ctrl Pts',(8.46611089167832,12.2,-6.78783081717345));
#175928=CARTESIAN_POINT('Ctrl Pts',(8.46956707602253,12.2,-6.78915342651578));
#175929=CARTESIAN_POINT('Ctrl Pts',(8.47302326083764,12.2,-6.79047603603832));
#175930=CARTESIAN_POINT('Ctrl Pts',(8.47649591951185,12.2,-6.79179831183302));
#175931=CARTESIAN_POINT('Ctrl Pts',(8.47998497503701,12.2,-6.7931201306828));
#175932=CARTESIAN_POINT('Ctrl Pts',(8.4834740300868,12.2,-6.79444194935248));
#175933=CARTESIAN_POINT('Ctrl Pts',(8.48697948355943,12.2,-6.79576331160275));
#175934=CARTESIAN_POINT('Ctrl Pts',(8.49050126377046,12.2,-6.79708409688371));
#175935=CARTESIAN_POINT('Ctrl Pts',(8.49402304446134,12.2,-6.79840488234462));
#175936=CARTESIAN_POINT('Ctrl Pts',(8.49756114899859,12.2,-6.79972509074538));
#175937=CARTESIAN_POINT('Ctrl Pts',(8.5011155084824,12.2,-6.80104460171649));
#175938=CARTESIAN_POINT('Ctrl Pts',(8.50466986748193,12.2,-6.80236411250781));
#175939=CARTESIAN_POINT('Ctrl Pts',(8.50824047931775,12.2,-6.80368292767495));
#175940=CARTESIAN_POINT('Ctrl Pts',(8.51182727169015,12.2,-6.8050009264006));
#175941=CARTESIAN_POINT('Ctrl Pts',(8.51541406455124,12.2,-6.80631892530581));
#175942=CARTESIAN_POINT('Ctrl Pts',(8.51901703779205,12.2,-6.80763610905538));
#175943=CARTESIAN_POINT('Ctrl Pts',(8.52263612054589,12.2,-6.80895236184928));
#175944=CARTESIAN_POINT('Ctrl Pts',(8.52625520280664,12.2,-6.81026861446384));
#175945=CARTESIAN_POINT('Ctrl Pts',(8.52989039319317,12.2,-6.8115839357121));
#175946=CARTESIAN_POINT('Ctrl Pts',(8.53354162218682,12.2,-6.8128982085593));
#175947=CARTESIAN_POINT('Ctrl Pts',(8.53719285167795,12.2,-6.81421248158557));
#175948=CARTESIAN_POINT('Ctrl Pts',(8.54086011784936,12.2,-6.8155257078775));
#175949=CARTESIAN_POINT('Ctrl Pts',(8.54454335005114,12.2,-6.8168377721156));
#175950=CARTESIAN_POINT('Ctrl Pts',(8.54822658175108,12.2,-6.81814983617493));
#175951=CARTESIAN_POINT('Ctrl Pts',(8.55192578000058,12.2,-6.81946073921782));
#175952=CARTESIAN_POINT('Ctrl Pts',(8.55564087241747,12.2,-6.82077036727756));
#175953=CARTESIAN_POINT('Ctrl Pts',(8.55935596534054,12.2,-6.82207999551573));
#175954=CARTESIAN_POINT('Ctrl Pts',(8.56308695390617,12.2,-6.82338834881264));
#175955=CARTESIAN_POINT('Ctrl Pts',(8.5668337672941,12.2,-6.82469531700091));
#175956=CARTESIAN_POINT('Ctrl Pts',(8.57058058017153,12.2,-6.82600228501111));
#175957=CARTESIAN_POINT('Ctrl Pts',(8.57434321779261,12.2,-6.82730786580159));
#175958=CARTESIAN_POINT('Ctrl Pts',(8.57812160814879,12.2,-6.82861195052847));
#175959=CARTESIAN_POINT('Ctrl Pts',(8.58189999901978,12.2,-6.82991603543304));
#175960=CARTESIAN_POINT('Ctrl Pts',(8.58569414515892,12.2,-6.83121862397356));
#175961=CARTESIAN_POINT('Ctrl Pts',(8.58950397469988,12.2,-6.83251960626669));
#175962=CARTESIAN_POINT('Ctrl Pts',(8.59426626136654,12.2,-6.83414583404446));
#175963=CARTESIAN_POINT('Ctrl Pts',(8.59905305545545,12.2,-6.83576955228337));
#175964=CARTESIAN_POINT('Ctrl Pts',(8.60386421802488,12.2,-6.83739055020003));
#175965=CARTESIAN_POINT('Ctrl Pts',(8.60771314829021,12.2,-6.83868734860403));
#175966=CARTESIAN_POINT('Ctrl Pts',(8.61157767655179,12.2,-6.83998240684951));
#175967=CARTESIAN_POINT('Ctrl Pts',(8.61545773137595,12.2,-6.84127561775313));
#175968=CARTESIAN_POINT('Ctrl Pts',(8.61933778567146,12.2,-6.84256882848056));
#175969=CARTESIAN_POINT('Ctrl Pts',(8.62323336771314,12.2,-6.84386019109314));
#175970=CARTESIAN_POINT('Ctrl Pts',(8.62714440868889,12.2,-6.84514960121581));
#175971=CARTESIAN_POINT('Ctrl Pts',(8.63105545019752,12.2,-6.84643901151416));
#175972=CARTESIAN_POINT('Ctrl Pts',(8.63498194935854,12.2,-6.84772646893479));
#175973=CARTESIAN_POINT('Ctrl Pts',(8.63892383818605,12.2,-6.84901186922685));
#175974=CARTESIAN_POINT('Ctrl Pts',(8.64286572647648,12.2,-6.85029726934378));
#175975=CARTESIAN_POINT('Ctrl Pts',(8.64682300519824,12.2,-6.85158061194986));
#175976=CARTESIAN_POINT('Ctrl Pts',(8.65079560415027,12.2,-6.8528617941786));
#175977=CARTESIAN_POINT('Ctrl Pts',(8.65476820364356,12.2,-6.85414297658189));
#175978=CARTESIAN_POINT('Ctrl Pts',(8.65875612331969,12.2,-6.85542199905211));
#175979=CARTESIAN_POINT('Ctrl Pts',(8.66275929757252,12.2,-6.85669875818528));
#175980=CARTESIAN_POINT('Ctrl Pts',(8.66676247127991,12.2,-6.8579755171445));
#175981=CARTESIAN_POINT('Ctrl Pts',(8.67078089611491,12.2,-6.8592500152193));
#175982=CARTESIAN_POINT('Ctrl Pts',(8.67481450639528,12.2,-6.860522148171));
#175983=CARTESIAN_POINT('Ctrl Pts',(8.67884811722522,12.2,-6.86179428129605));
#175984=CARTESIAN_POINT('Ctrl Pts',(8.68289691163479,12.2,-6.86306405099859));
#175985=CARTESIAN_POINT('Ctrl Pts',(8.68696082435725,12.2,-6.86433135734527));
#175986=CARTESIAN_POINT('Ctrl Pts',(8.69102473652601,12.2,-6.86559866351929));
#175987=CARTESIAN_POINT('Ctrl Pts',(8.69510376418181,12.2,-6.86686350616786));
#175988=CARTESIAN_POINT('Ctrl Pts',(8.6991978426059,12.2,-6.86812578635018));
#175989=CARTESIAN_POINT('Ctrl Pts',(8.70329192158781,12.2,-6.86938806670449));
#175990=CARTESIAN_POINT('Ctrl Pts',(8.70740104922534,12.2,-6.87064778431777));
#175991=CARTESIAN_POINT('Ctrl Pts',(8.71152515939551,12.2,-6.8719048413861));
#175992=CARTESIAN_POINT('Ctrl Pts',(8.71564926900379,12.2,-6.87316189828317));
#175993=CARTESIAN_POINT('Ctrl Pts',(8.71978836024517,12.2,-6.87441629478354));
#175994=CARTESIAN_POINT('Ctrl Pts',(8.72394236657071,12.2,-6.87566793373705));
#175995=CARTESIAN_POINT('Ctrl Pts',(8.72809637346226,12.2,-6.8769195728611));
#175996=CARTESIAN_POINT('Ctrl Pts',(8.73226529536955,12.2,-6.87816845470787));
#175997=CARTESIAN_POINT('Ctrl Pts',(8.73644906622774,12.2,-6.87941448372587));
#175998=CARTESIAN_POINT('Ctrl Pts',(8.74063283651589,12.2,-6.88066051257411));
#175999=CARTESIAN_POINT('Ctrl Pts',(8.74483145490418,12.2,-6.88190368835111));
#176000=CARTESIAN_POINT('Ctrl Pts',(8.74904485450267,12.2,-6.88314391530558));
#176001=CARTESIAN_POINT('Ctrl Pts',(8.75325825467524,12.2,-6.88438414242903));
#176002=CARTESIAN_POINT('Ctrl Pts',(8.75748643633254,12.2,-6.88562142168276));
#176003=CARTESIAN_POINT('Ctrl Pts',(8.76172933450822,12.2,-6.88685565875003));
#176004=CARTESIAN_POINT('Ctrl Pts',(8.76703295693875,12.2,-6.88839845500002));
#176005=CARTESIAN_POINT('Ctrl Pts',(8.77235957187289,12.2,-6.8899364977828));
#176006=CARTESIAN_POINT('Ctrl Pts',(8.77770904953614,12.2,-6.89146960577586));
#176007=CARTESIAN_POINT('Ctrl Pts',(8.78091873601747,12.2,-6.89238947053828));
#176008=CARTESIAN_POINT('Ctrl Pts',(8.78413665429956,12.2,-6.89330755887832));
#176009=CARTESIAN_POINT('Ctrl Pts',(8.78736277523863,12.2,-6.8942238317242));
#176010=CARTESIAN_POINT('Ctrl Pts',(8.79058889617769,12.2,-6.89514010457007));
#176011=CARTESIAN_POINT('Ctrl Pts',(8.79382322081512,12.2,-6.89605456383352));
#176012=CARTESIAN_POINT('Ctrl Pts',(8.79706572115493,12.2,-6.89696716767552));
#176013=CARTESIAN_POINT('Ctrl Pts',(8.80030822149474,12.2,-6.89787977151753));
#176014=CARTESIAN_POINT('Ctrl Pts',(8.80355889662566,12.2,-6.89879052146799));
#176015=CARTESIAN_POINT('Ctrl Pts',(8.80681771950614,12.2,-6.89969937976857));
#176016=CARTESIAN_POINT('Ctrl Pts',(8.81007654297864,12.2,-6.90060823823424));
#176017=CARTESIAN_POINT('Ctrl Pts',(8.81334351458678,12.2,-6.90151520521606));
#176018=CARTESIAN_POINT('Ctrl Pts',(8.81661860698053,12.2,-6.90242024168066));
#176019=CARTESIAN_POINT('Ctrl Pts',(8.81989369877931,12.2,-6.90332527798084));
#176020=CARTESIAN_POINT('Ctrl Pts',(8.8231769106243,12.2,-6.90422838507897));
#176021=CARTESIAN_POINT('Ctrl Pts',(8.82646821517008,12.2,-6.90512952396602));
#176022=CARTESIAN_POINT('Ctrl Pts',(8.82975951971587,12.2,-6.90603066285308));
#176023=CARTESIAN_POINT('Ctrl Pts',(8.83305891673001,12.2,-6.90692983469723));
#176024=CARTESIAN_POINT('Ctrl Pts',(8.83636637961053,12.2,-6.90782700108112));
#176025=CARTESIAN_POINT('Ctrl Pts',(8.83967384249106,12.2,-6.90872416746502));
#176026=CARTESIAN_POINT('Ctrl Pts',(8.84298937082064,12.2,-6.90961933044915));
#176027=CARTESIAN_POINT('Ctrl Pts',(8.84631293674155,12.2,-6.9105124502917));
#176028=CARTESIAN_POINT('Ctrl Pts',(8.84963650266246,12.2,-6.91140557013425));
#176029=CARTESIAN_POINT('Ctrl Pts',(8.85296810679138,12.2,-6.91229664810188));
#176030=CARTESIAN_POINT('Ctrl Pts',(8.856307722086,12.2,-6.91318564740309));
#176031=CARTESIAN_POINT('Ctrl Pts',(8.85964733738063,12.2,-6.91407464670431));
#176032=CARTESIAN_POINT('Ctrl Pts',(8.86299496240595,12.2,-6.91496156678319));
#176033=CARTESIAN_POINT('Ctrl Pts',(8.86635057186741,12.2,-6.91584637254549));
#176034=CARTESIAN_POINT('Ctrl Pts',(8.86970618132887,12.2,-6.91673117830779));
#176035=CARTESIAN_POINT('Ctrl Pts',(8.87306977413848,12.2,-6.91761386835644));
#176036=CARTESIAN_POINT('Ctrl Pts',(8.87644132305657,12.2,-6.91849440707474));
#176037=CARTESIAN_POINT('Ctrl Pts',(8.87981287258715,12.2,-6.91937494595301));
#176038=CARTESIAN_POINT('Ctrl Pts',(8.88319237864497,12.2,-6.920253332864));
#176039=CARTESIAN_POINT('Ctrl Pts',(8.88657981368003,12.2,-6.92112953324104));
#176040=CARTESIAN_POINT('Ctrl Pts',(8.8899672480997,12.2,-6.9220057334589));
#176041=CARTESIAN_POINT('Ctrl Pts',(8.89336261259395,12.2,-6.92287974501023));
#176042=CARTESIAN_POINT('Ctrl Pts',(8.89676587892931,12.2,-6.92375153381169));
#176043=CARTESIAN_POINT('Ctrl Pts',(8.90016914526467,12.2,-6.92462332261315));
#176044=CARTESIAN_POINT('Ctrl Pts',(8.90358031307833,12.2,-6.92549288789506));
#176045=CARTESIAN_POINT('Ctrl Pts',(8.90699935651133,12.2,-6.92636019474249));
#176046=CARTESIAN_POINT('Ctrl Pts',(8.91041839994434,12.2,-6.9272275015899));
#176047=CARTESIAN_POINT('Ctrl Pts',(8.91384531928933,12.2,-6.92809255112666));
#176048=CARTESIAN_POINT('Ctrl Pts',(8.91728008622177,12.2,-6.92895530551591));
#176049=CARTESIAN_POINT('Ctrl Pts',(8.92071485315421,12.2,-6.92981805990516));
#176050=CARTESIAN_POINT('Ctrl Pts',(8.9241574686833,12.2,-6.93067852082076));
#176051=CARTESIAN_POINT('Ctrl Pts',(8.92760790514059,12.2,-6.93153665266479));
#176052=CARTESIAN_POINT('Ctrl Pts',(8.93105834159788,12.2,-6.93239478450881));
#176053=CARTESIAN_POINT('Ctrl Pts',(8.93451660055463,12.2,-6.93325058724467));
#176054=CARTESIAN_POINT('Ctrl Pts',(8.9379826534693,12.2,-6.93410402704731));
#176055=CARTESIAN_POINT('Ctrl Pts',(8.94144870701363,12.2,-6.934957467005));
#176056=CARTESIAN_POINT('Ctrl Pts',(8.9449225547185,12.2,-6.93580854341203));
#176057=CARTESIAN_POINT('Ctrl Pts',(8.94840417072556,12.2,-6.93665722145171));
#176058=CARTESIAN_POINT('Ctrl Pts',(8.95188578610012,12.2,-6.93750589933722));
#176059=CARTESIAN_POINT('Ctrl Pts',(8.95537516979094,12.2,-6.93835218048951));
#176060=CARTESIAN_POINT('Ctrl Pts',(8.95887229462287,12.2,-6.9391960283753));
#176061=CARTESIAN_POINT('Ctrl Pts',(8.96236941945481,12.2,-6.9400398762611));
#176062=CARTESIAN_POINT('Ctrl Pts',(8.96587428511472,12.2,-6.94088129189414));
#176063=CARTESIAN_POINT('Ctrl Pts',(8.96938686554475,12.2,-6.94172024178413));
#176064=CARTESIAN_POINT('Ctrl Pts',(8.97289944597478,12.2,-6.94255919167411));
#176065=CARTESIAN_POINT('Ctrl Pts',(8.97641974169222,12.2,-6.94339567577577));
#176066=CARTESIAN_POINT('Ctrl Pts',(8.97994772470502,12.2,-6.94422965970761));
#176067=CARTESIAN_POINT('Ctrl Pts',(8.98347570771783,12.2,-6.94506364363944));
#176068=CARTESIAN_POINT('Ctrl Pts',(8.98701138010987,12.2,-6.94589512877286));
#176069=CARTESIAN_POINT('Ctrl Pts',(8.99055471260546,12.2,-6.94672407965963));
#176070=CARTESIAN_POINT('Ctrl Pts',(8.99409804510107,12.2,-6.9475530305464));
#176071=CARTESIAN_POINT('Ctrl Pts',(8.99764904030446,12.2,-6.94837944795001));
#176072=CARTESIAN_POINT('Ctrl Pts',(9.00120766971578,12.2,-6.94920329929543));
#176073=CARTESIAN_POINT('Ctrl Pts',(9.00476629977359,12.2,-6.95002715079051));
#176074=CARTESIAN_POINT('Ctrl Pts',(9.00833256505857,12.2,-6.95084843617654));
#176075=CARTESIAN_POINT('Ctrl Pts',(9.01190643957901,12.2,-6.95166712171184));
#176076=CARTESIAN_POINT('Ctrl Pts',(9.0154803134502,12.2,-6.9524858070984));
#176077=CARTESIAN_POINT('Ctrl Pts',(9.01906179657792,12.2,-6.95330189324661));
#176078=CARTESIAN_POINT('Ctrl Pts',(9.02265086121103,12.2,-6.95411534763239));
#176079=CARTESIAN_POINT('Ctrl Pts',(9.02623992584414,12.2,-6.95492880201817));
#176080=CARTESIAN_POINT('Ctrl Pts',(9.02983657273984,12.2,-6.95573962368434));
#176081=CARTESIAN_POINT('Ctrl Pts',(9.03344077565121,12.2,-6.95654778007141));
#176082=CARTESIAN_POINT('Ctrl Pts',(9.03704497856259,12.2,-6.95735593645849));
#176083=CARTESIAN_POINT('Ctrl Pts',(9.04065673728139,12.2,-6.9581614281292));
#176084=CARTESIAN_POINT('Ctrl Pts',(9.04427602623322,12.2,-6.9589642235167));
#176085=CARTESIAN_POINT('Ctrl Pts',(9.04789531518505,12.2,-6.9597670189042));
#176086=CARTESIAN_POINT('Ctrl Pts',(9.05152213511992,12.2,-6.96056711802514));
#176087=CARTESIAN_POINT('Ctrl Pts',(9.05515645857055,12.2,-6.96136448837141));
#176088=CARTESIAN_POINT('Ctrl Pts',(9.05879078202118,12.2,-6.96216185871767));
#176089=CARTESIAN_POINT('Ctrl Pts',(9.06243261019506,12.2,-6.96295649975236));
#176090=CARTESIAN_POINT('Ctrl Pts',(9.06608191474392,12.2,-6.9637483795968));
#176091=CARTESIAN_POINT('Ctrl Pts',(9.07094765458435,12.2,-6.96480421948529));
#176092=CARTESIAN_POINT('Ctrl Pts',(9.07582668513524,12.2,-6.96585514807604));
#176093=CARTESIAN_POINT('Ctrl Pts',(9.08071894812496,12.2,-6.96690109407716));
#176094=CARTESIAN_POINT('Ctrl Pts',(9.08438814503396,12.2,-6.96768555350675));
#176095=CARTESIAN_POINT('Ctrl Pts',(9.08806478513374,12.2,-6.968467210345));
#176096=CARTESIAN_POINT('Ctrl Pts',(9.09174884449989,12.2,-6.96924603623337));
#176097=CARTESIAN_POINT('Ctrl Pts',(9.09543290386604,12.2,-6.97002486212174));
#176098=CARTESIAN_POINT('Ctrl Pts',(9.09912438294854,12.2,-6.97080085739356));
#176099=CARTESIAN_POINT('Ctrl Pts',(9.10282325310517,12.2,-6.97157398615738));
#176100=CARTESIAN_POINT('Ctrl Pts',(9.10652212326181,12.2,-6.97234711492121));
#176101=CARTESIAN_POINT('Ctrl Pts',(9.11022838124838,12.2,-6.97311737640742));
#176102=CARTESIAN_POINT('Ctrl Pts',(9.11394199879815,12.2,-6.97388473387654));
#176103=CARTESIAN_POINT('Ctrl Pts',(9.1176556163479,12.2,-6.97465209134567));
#176104=CARTESIAN_POINT('Ctrl Pts',(9.12137659252359,12.2,-6.97541654399462));
#176105=CARTESIAN_POINT('Ctrl Pts',(9.12510490826213,12.2,-6.97617807080069));
#176106=CARTESIAN_POINT('Ctrl Pts',(9.13007599636506,12.2,-6.97719343996767));
#176107=CARTESIAN_POINT('Ctrl Pts',(9.13506013930488,12.2,-6.97820361072618));
#176108=CARTESIAN_POINT('Ctrl Pts',(9.14005731399994,12.2,-6.97920857100002));
#176109=CARTESIAN_POINT('Ctrl Pts',(9.36775917499994,15.2,-6.67046385500001));
#176110=CARTESIAN_POINT('Ctrl Pts',(9.36775917499994,11.6,-6.67046385500001));
#176111=CARTESIAN_POINT('Ctrl Pts',(9.36739372899994,15.2,-6.66979226100001));
#176112=CARTESIAN_POINT('Ctrl Pts',(9.36739372899994,11.6,-6.66979226100001));
#176113=CARTESIAN_POINT('Ctrl Pts',(9.36666279599994,15.2,-6.66844959700001));
#176114=CARTESIAN_POINT('Ctrl Pts',(9.36666279599994,11.6,-6.66844959700001));
#176115=CARTESIAN_POINT('Ctrl Pts',(9.36556626999994,15.2,-6.66643717600002));
#176116=CARTESIAN_POINT('Ctrl Pts',(9.36556626999994,11.6,-6.66643717600002));
#176117=CARTESIAN_POINT('Ctrl Pts',(9.36410398399994,15.2,-6.66375709800001));
#176118=CARTESIAN_POINT('Ctrl Pts',(9.36410398399994,11.6,-6.66375709800001));
#176119=CARTESIAN_POINT('Ctrl Pts',(9.36227570599995,15.2,-6.66041225100001));
#176120=CARTESIAN_POINT('Ctrl Pts',(9.36227570599995,11.6,-6.66041225100001));
#176121=CARTESIAN_POINT('Ctrl Pts',(9.36044700899994,15.2,-6.65707265500001));
#176122=CARTESIAN_POINT('Ctrl Pts',(9.36044700899994,11.6,-6.65707265500001));
#176123=CARTESIAN_POINT('Ctrl Pts',(9.35861789699995,15.2,-6.65373831100001));
#176124=CARTESIAN_POINT('Ctrl Pts',(9.35861789699995,11.6,-6.65373831100001));
#176125=CARTESIAN_POINT('Ctrl Pts',(9.35678837099994,15.2,-6.65040921900002));
#176126=CARTESIAN_POINT('Ctrl Pts',(9.35678837099994,11.6,-6.65040921900002));
#176127=CARTESIAN_POINT('Ctrl Pts',(9.35495843699995,15.2,-6.64708538300002));
#176128=CARTESIAN_POINT('Ctrl Pts',(9.35495843699995,11.6,-6.64708538300002));
#176129=CARTESIAN_POINT('Ctrl Pts',(9.35312810399994,15.2,-6.64376680700002));
#176130=CARTESIAN_POINT('Ctrl Pts',(9.35312810399994,11.6,-6.64376680700002));
#176131=CARTESIAN_POINT('Ctrl Pts',(9.35129737799994,15.2,-6.64045349300002));
#176132=CARTESIAN_POINT('Ctrl Pts',(9.35129737799994,11.6,-6.64045349300002));
#176133=CARTESIAN_POINT('Ctrl Pts',(9.34946627399994,15.2,-6.63714544600002));
#176134=CARTESIAN_POINT('Ctrl Pts',(9.34946627399994,11.6,-6.63714544600002));
#176135=CARTESIAN_POINT('Ctrl Pts',(9.34763479699994,15.2,-6.63384267000002));
#176136=CARTESIAN_POINT('Ctrl Pts',(9.34763479699994,11.6,-6.63384267000002));
#176137=CARTESIAN_POINT('Ctrl Pts',(9.34580295999995,15.2,-6.63054516900001));
#176138=CARTESIAN_POINT('Ctrl Pts',(9.34580295999995,11.6,-6.63054516900001));
#176139=CARTESIAN_POINT('Ctrl Pts',(9.34397077299994,15.2,-6.62725294900002));
#176140=CARTESIAN_POINT('Ctrl Pts',(9.34397077299994,11.6,-6.62725294900002));
#176141=CARTESIAN_POINT('Ctrl Pts',(9.34213824299994,15.2,-6.62396601100002));
#176142=CARTESIAN_POINT('Ctrl Pts',(9.34213824299994,11.6,-6.62396601100002));
#176143=CARTESIAN_POINT('Ctrl Pts',(9.34030537899995,15.2,-6.62068435900002));
#176144=CARTESIAN_POINT('Ctrl Pts',(9.34030537899995,11.6,-6.62068435900002));
#176145=CARTESIAN_POINT('Ctrl Pts',(9.33847218899994,15.2,-6.61740799700001));
#176146=CARTESIAN_POINT('Ctrl Pts',(9.33847218899994,11.6,-6.61740799700001));
#176147=CARTESIAN_POINT('Ctrl Pts',(9.33663867899994,15.2,-6.61413692800001));
#176148=CARTESIAN_POINT('Ctrl Pts',(9.33663867899994,11.6,-6.61413692800001));
#176149=CARTESIAN_POINT('Ctrl Pts',(9.33480485899995,15.2,-6.61087115400001));
#176150=CARTESIAN_POINT('Ctrl Pts',(9.33480485899995,11.6,-6.61087115400001));
#176151=CARTESIAN_POINT('Ctrl Pts',(9.33297073499994,15.2,-6.60761068000002));
#176152=CARTESIAN_POINT('Ctrl Pts',(9.33297073499994,11.6,-6.60761068000002));
#176153=CARTESIAN_POINT('Ctrl Pts',(9.33113631499995,15.2,-6.60435550800001));
#176154=CARTESIAN_POINT('Ctrl Pts',(9.33113631499995,11.6,-6.60435550800001));
#176155=CARTESIAN_POINT('Ctrl Pts',(9.32930160899994,15.2,-6.60110564200002));
#176156=CARTESIAN_POINT('Ctrl Pts',(9.32930160899994,11.6,-6.60110564200002));
#176157=CARTESIAN_POINT('Ctrl Pts',(9.32746662499994,15.2,-6.59786108500001));
#176158=CARTESIAN_POINT('Ctrl Pts',(9.32746662499994,11.6,-6.59786108500001));
#176159=CARTESIAN_POINT('Ctrl Pts',(9.32563137099994,15.2,-6.59462184300001));
#176160=CARTESIAN_POINT('Ctrl Pts',(9.32563137099994,11.6,-6.59462184300001));
#176161=CARTESIAN_POINT('Ctrl Pts',(9.32379585799995,15.2,-6.59138791600002));
#176162=CARTESIAN_POINT('Ctrl Pts',(9.32379585799995,11.6,-6.59138791600002));
#176163=CARTESIAN_POINT('Ctrl Pts',(9.32196009399994,15.2,-6.58815931000002));
#176164=CARTESIAN_POINT('Ctrl Pts',(9.32196009399994,11.6,-6.58815931000002));
#176165=CARTESIAN_POINT('Ctrl Pts',(9.32012408599994,15.2,-6.58493602700001));
#176166=CARTESIAN_POINT('Ctrl Pts',(9.32012408599994,11.6,-6.58493602700001));
#176167=CARTESIAN_POINT('Ctrl Pts',(9.31828784399995,15.2,-6.58171807200001));
#176168=CARTESIAN_POINT('Ctrl Pts',(9.31828784399995,11.6,-6.58171807200001));
#176169=CARTESIAN_POINT('Ctrl Pts',(9.31645137599994,15.2,-6.57850544700001));
#176170=CARTESIAN_POINT('Ctrl Pts',(9.31645137599994,11.6,-6.57850544700001));
#176171=CARTESIAN_POINT('Ctrl Pts',(9.31461468999995,15.2,-6.57529815700002));
#176172=CARTESIAN_POINT('Ctrl Pts',(9.31461468999995,11.6,-6.57529815700002));
#176173=CARTESIAN_POINT('Ctrl Pts',(9.31277779499995,15.2,-6.57209620300002));
#176174=CARTESIAN_POINT('Ctrl Pts',(9.31277779499995,11.6,-6.57209620300002));
#176175=CARTESIAN_POINT('Ctrl Pts',(9.31094069999994,15.2,-6.56889959000001));
#176176=CARTESIAN_POINT('Ctrl Pts',(9.31094069999994,11.6,-6.56889959000001));
#176177=CARTESIAN_POINT('Ctrl Pts',(9.30910341199995,15.2,-6.56570832200002));
#176178=CARTESIAN_POINT('Ctrl Pts',(9.30910341199995,11.6,-6.56570832200002));
#176179=CARTESIAN_POINT('Ctrl Pts',(9.30726594099994,15.2,-6.56252240200002));
#176180=CARTESIAN_POINT('Ctrl Pts',(9.30726594099994,11.6,-6.56252240200002));
#176181=CARTESIAN_POINT('Ctrl Pts',(9.30542829499995,15.2,-6.55934183200002));
#176182=CARTESIAN_POINT('Ctrl Pts',(9.30542829499995,11.6,-6.55934183200002));
#176183=CARTESIAN_POINT('Ctrl Pts',(9.30359048399995,15.2,-6.55616661700002));
#176184=CARTESIAN_POINT('Ctrl Pts',(9.30359048399995,11.6,-6.55616661700002));
#176185=CARTESIAN_POINT('Ctrl Pts',(9.30175251499995,15.2,-6.55299676000002));
#176186=CARTESIAN_POINT('Ctrl Pts',(9.30175251499995,11.6,-6.55299676000002));
#176187=CARTESIAN_POINT('Ctrl Pts',(9.29991439799995,15.2,-6.54983226400002));
#176188=CARTESIAN_POINT('Ctrl Pts',(9.29991439799995,11.6,-6.54983226400002));
#176189=CARTESIAN_POINT('Ctrl Pts',(9.29807614099994,15.2,-6.54667313400001));
#176190=CARTESIAN_POINT('Ctrl Pts',(9.29807614099994,11.6,-6.54667313400001));
#176191=CARTESIAN_POINT('Ctrl Pts',(9.29623775399994,15.2,-6.54351937200002));
#176192=CARTESIAN_POINT('Ctrl Pts',(9.29623775399994,11.6,-6.54351937200002));
#176193=CARTESIAN_POINT('Ctrl Pts',(9.29439924399994,15.2,-6.54037098200002));
#176194=CARTESIAN_POINT('Ctrl Pts',(9.29439924399994,11.6,-6.54037098200002));
#176195=CARTESIAN_POINT('Ctrl Pts',(9.29256062099994,15.2,-6.53722796600002));
#176196=CARTESIAN_POINT('Ctrl Pts',(9.29256062099994,11.6,-6.53722796600002));
#176197=CARTESIAN_POINT('Ctrl Pts',(9.29072189399994,15.2,-6.53409033000001));
#176198=CARTESIAN_POINT('Ctrl Pts',(9.29072189399994,11.6,-6.53409033000001));
#176199=CARTESIAN_POINT('Ctrl Pts',(9.28888307099994,15.2,-6.53095807600002));
#176200=CARTESIAN_POINT('Ctrl Pts',(9.28888307099994,11.6,-6.53095807600002));
#176201=CARTESIAN_POINT('Ctrl Pts',(9.28704415999994,15.2,-6.52783120700001));
#176202=CARTESIAN_POINT('Ctrl Pts',(9.28704415999994,11.6,-6.52783120700001));
#176203=CARTESIAN_POINT('Ctrl Pts',(9.28520517099994,15.2,-6.52470972700002));
#176204=CARTESIAN_POINT('Ctrl Pts',(9.28520517099994,11.6,-6.52470972700002));
#176205=CARTESIAN_POINT('Ctrl Pts',(9.28336611299994,15.2,-6.52159363900001));
#176206=CARTESIAN_POINT('Ctrl Pts',(9.28336611299994,11.6,-6.52159363900001));
#176207=CARTESIAN_POINT('Ctrl Pts',(9.28152699599995,15.2,-6.51848294700001));
#176208=CARTESIAN_POINT('Ctrl Pts',(9.28152699599995,11.6,-6.51848294700001));
#176209=CARTESIAN_POINT('Ctrl Pts',(9.27968782599994,15.2,-6.51537765500001));
#176210=CARTESIAN_POINT('Ctrl Pts',(9.27968782599994,11.6,-6.51537765500001));
#176211=CARTESIAN_POINT('Ctrl Pts',(9.27784861399994,15.2,-6.51227776500001));
#176212=CARTESIAN_POINT('Ctrl Pts',(9.27784861399994,11.6,-6.51227776500001));
#176213=CARTESIAN_POINT('Ctrl Pts',(9.27600936899994,15.2,-6.50918328100002));
#176214=CARTESIAN_POINT('Ctrl Pts',(9.27600936899994,11.6,-6.50918328100002));
#176215=CARTESIAN_POINT('Ctrl Pts',(9.27417009899994,15.2,-6.50609420700002));
#176216=CARTESIAN_POINT('Ctrl Pts',(9.27417009899994,11.6,-6.50609420700002));
#176217=CARTESIAN_POINT('Ctrl Pts',(9.27233081399994,15.2,-6.50301054500002));
#176218=CARTESIAN_POINT('Ctrl Pts',(9.27233081399994,11.6,-6.50301054500002));
#176219=CARTESIAN_POINT('Ctrl Pts',(9.27049152299994,15.2,-6.49993230000002));
#176220=CARTESIAN_POINT('Ctrl Pts',(9.27049152299994,11.6,-6.49993230000002));
#176221=CARTESIAN_POINT('Ctrl Pts',(9.26865223299994,15.2,-6.49685947500001));
#176222=CARTESIAN_POINT('Ctrl Pts',(9.26865223299994,11.6,-6.49685947500001));
#176223=CARTESIAN_POINT('Ctrl Pts',(9.26681295499994,15.2,-6.49379207200001));
#176224=CARTESIAN_POINT('Ctrl Pts',(9.26681295499994,11.6,-6.49379207200001));
#176225=CARTESIAN_POINT('Ctrl Pts',(9.26497369799995,15.2,-6.49073009700002));
#176226=CARTESIAN_POINT('Ctrl Pts',(9.26497369799995,11.6,-6.49073009700002));
#176227=CARTESIAN_POINT('Ctrl Pts',(9.26313447099995,15.2,-6.48767355100001));
#176228=CARTESIAN_POINT('Ctrl Pts',(9.26313447099995,11.6,-6.48767355100001));
#176229=CARTESIAN_POINT('Ctrl Pts',(9.26129528299995,15.2,-6.48462243900001));
#176230=CARTESIAN_POINT('Ctrl Pts',(9.26129528299995,11.6,-6.48462243900001));
#176231=CARTESIAN_POINT('Ctrl Pts',(9.25945614099994,15.2,-6.48157676400002));
#176232=CARTESIAN_POINT('Ctrl Pts',(9.25945614099994,11.6,-6.48157676400002));
#176233=CARTESIAN_POINT('Ctrl Pts',(9.25761705899994,15.2,-6.47853652900002));
#176234=CARTESIAN_POINT('Ctrl Pts',(9.25761705899994,11.6,-6.47853652900002));
#176235=CARTESIAN_POINT('Ctrl Pts',(9.25577804099994,15.2,-6.47550173700001));
#176236=CARTESIAN_POINT('Ctrl Pts',(9.25577804099994,11.6,-6.47550173700001));
#176237=CARTESIAN_POINT('Ctrl Pts',(9.25393909899995,15.2,-6.47247239300001));
#176238=CARTESIAN_POINT('Ctrl Pts',(9.25393909899995,11.6,-6.47247239300001));
#176239=CARTESIAN_POINT('Ctrl Pts',(9.25210024199994,15.2,-6.46944849900001));
#176240=CARTESIAN_POINT('Ctrl Pts',(9.25210024199994,11.6,-6.46944849900001));
#176241=CARTESIAN_POINT('Ctrl Pts',(9.25026147799995,15.2,-6.46643005900001));
#176242=CARTESIAN_POINT('Ctrl Pts',(9.25026147799995,11.6,-6.46643005900001));
#176243=CARTESIAN_POINT('Ctrl Pts',(9.24842281799994,15.2,-6.46341707500002));
#176244=CARTESIAN_POINT('Ctrl Pts',(9.24842281799994,11.6,-6.46341707500002));
#176245=CARTESIAN_POINT('Ctrl Pts',(9.24658427099994,15.2,-6.46040955400002));
#176246=CARTESIAN_POINT('Ctrl Pts',(9.24658427099994,11.6,-6.46040955400002));
#176247=CARTESIAN_POINT('Ctrl Pts',(9.24474584399994,15.2,-6.45740749500002));
#176248=CARTESIAN_POINT('Ctrl Pts',(9.24474584399994,11.6,-6.45740749500002));
#176249=CARTESIAN_POINT('Ctrl Pts',(9.24290754899994,15.2,-6.45441090500002));
#176250=CARTESIAN_POINT('Ctrl Pts',(9.24290754899994,11.6,-6.45441090500002));
#176251=CARTESIAN_POINT('Ctrl Pts',(9.24106939399995,15.2,-6.45141978400002));
#176252=CARTESIAN_POINT('Ctrl Pts',(9.24106939399995,11.6,-6.45141978400002));
#176253=CARTESIAN_POINT('Ctrl Pts',(9.23923138799994,15.2,-6.44843413900002));
#176254=CARTESIAN_POINT('Ctrl Pts',(9.23923138799994,11.6,-6.44843413900002));
#176255=CARTESIAN_POINT('Ctrl Pts',(9.23739354199994,15.2,-6.44545397100002));
#176256=CARTESIAN_POINT('Ctrl Pts',(9.23739354199994,11.6,-6.44545397100002));
#176257=CARTESIAN_POINT('Ctrl Pts',(9.23555586399995,15.2,-6.44247928500001));
#176258=CARTESIAN_POINT('Ctrl Pts',(9.23555586399995,11.6,-6.44247928500001));
#176259=CARTESIAN_POINT('Ctrl Pts',(9.23371836299994,15.2,-6.43951008200002));
#176260=CARTESIAN_POINT('Ctrl Pts',(9.23371836299994,11.6,-6.43951008200002));
#176261=CARTESIAN_POINT('Ctrl Pts',(9.23188104999995,15.2,-6.43654636700001));
#176262=CARTESIAN_POINT('Ctrl Pts',(9.23188104999995,11.6,-6.43654636700001));
#176263=CARTESIAN_POINT('Ctrl Pts',(9.23004393299994,15.2,-6.43358814300001));
#176264=CARTESIAN_POINT('Ctrl Pts',(9.23004393299994,11.6,-6.43358814300001));
#176265=CARTESIAN_POINT('Ctrl Pts',(9.22820702199994,15.2,-6.43063541500001));
#176266=CARTESIAN_POINT('Ctrl Pts',(9.22820702199994,11.6,-6.43063541500001));
#176267=CARTESIAN_POINT('Ctrl Pts',(9.22637032699994,15.2,-6.42768818500001));
#176268=CARTESIAN_POINT('Ctrl Pts',(9.22637032699994,11.6,-6.42768818500001));
#176269=CARTESIAN_POINT('Ctrl Pts',(9.22453385699994,15.2,-6.42474645400001));
#176270=CARTESIAN_POINT('Ctrl Pts',(9.22453385699994,11.6,-6.42474645400001));
#176271=CARTESIAN_POINT('Ctrl Pts',(9.22269762199995,15.2,-6.42181023000001));
#176272=CARTESIAN_POINT('Ctrl Pts',(9.22269762199995,11.6,-6.42181023000001));
#176273=CARTESIAN_POINT('Ctrl Pts',(9.22086162999994,15.2,-6.41887951300002));
#176274=CARTESIAN_POINT('Ctrl Pts',(9.22086162999994,11.6,-6.41887951300002));
#176275=CARTESIAN_POINT('Ctrl Pts',(9.21902589199994,15.2,-6.41595430800002));
#176276=CARTESIAN_POINT('Ctrl Pts',(9.21902589199994,11.6,-6.41595430800002));
#176277=CARTESIAN_POINT('Ctrl Pts',(9.21719041799994,15.2,-6.41303461800002));
#176278=CARTESIAN_POINT('Ctrl Pts',(9.21719041799994,11.6,-6.41303461800002));
#176279=CARTESIAN_POINT('Ctrl Pts',(9.21535521599994,15.2,-6.41012044600001));
#176280=CARTESIAN_POINT('Ctrl Pts',(9.21535521599994,11.6,-6.41012044600001));
#176281=CARTESIAN_POINT('Ctrl Pts',(9.21352029599994,15.2,-6.40721179700002));
#176282=CARTESIAN_POINT('Ctrl Pts',(9.21352029599994,11.6,-6.40721179700002));
#176283=CARTESIAN_POINT('Ctrl Pts',(9.21168566899994,15.2,-6.40430867100001));
#176284=CARTESIAN_POINT('Ctrl Pts',(9.21168566899994,11.6,-6.40430867100001));
#176285=CARTESIAN_POINT('Ctrl Pts',(9.20985134399994,15.2,-6.40141107500002));
#176286=CARTESIAN_POINT('Ctrl Pts',(9.20985134399994,11.6,-6.40141107500002));
#176287=CARTESIAN_POINT('Ctrl Pts',(9.20801732999994,15.2,-6.39851901000001));
#176288=CARTESIAN_POINT('Ctrl Pts',(9.20801732999994,11.6,-6.39851901000001));
#176289=CARTESIAN_POINT('Ctrl Pts',(9.20618363699995,15.2,-6.39563248100002));
#176290=CARTESIAN_POINT('Ctrl Pts',(9.20618363699995,11.6,-6.39563248100002));
#176291=CARTESIAN_POINT('Ctrl Pts',(9.20435027499994,15.2,-6.39275149000002));
#176292=CARTESIAN_POINT('Ctrl Pts',(9.20435027499994,11.6,-6.39275149000002));
#176293=CARTESIAN_POINT('Ctrl Pts',(9.20251725399994,15.2,-6.38987604000001));
#176294=CARTESIAN_POINT('Ctrl Pts',(9.20251725399994,11.6,-6.38987604000001));
#176295=CARTESIAN_POINT('Ctrl Pts',(9.20068458299994,15.2,-6.38700613600002));
#176296=CARTESIAN_POINT('Ctrl Pts',(9.20068458299994,11.6,-6.38700613600002));
#176297=CARTESIAN_POINT('Ctrl Pts',(9.19885227299994,15.2,-6.38414178100002));
#176298=CARTESIAN_POINT('Ctrl Pts',(9.19885227299994,11.6,-6.38414178100002));
#176299=CARTESIAN_POINT('Ctrl Pts',(9.19702033199994,15.2,-6.38128297800002));
#176300=CARTESIAN_POINT('Ctrl Pts',(9.19702033199994,11.6,-6.38128297800002));
#176301=CARTESIAN_POINT('Ctrl Pts',(9.19518877099994,15.2,-6.37842973000001));
#176302=CARTESIAN_POINT('Ctrl Pts',(9.19518877099994,11.6,-6.37842973000001));
#176303=CARTESIAN_POINT('Ctrl Pts',(9.19335759999995,15.2,-6.37558204000002));
#176304=CARTESIAN_POINT('Ctrl Pts',(9.19335759999995,11.6,-6.37558204000002));
#176305=CARTESIAN_POINT('Ctrl Pts',(9.19152682999994,15.2,-6.37273991300002));
#176306=CARTESIAN_POINT('Ctrl Pts',(9.19152682999994,11.6,-6.37273991300002));
#176307=CARTESIAN_POINT('Ctrl Pts',(9.18969646699994,15.2,-6.36990335200001));
#176308=CARTESIAN_POINT('Ctrl Pts',(9.18969646699994,11.6,-6.36990335200001));
#176309=CARTESIAN_POINT('Ctrl Pts',(9.18786652499995,15.2,-6.36707235900002));
#176310=CARTESIAN_POINT('Ctrl Pts',(9.18786652499995,11.6,-6.36707235900002));
#176311=CARTESIAN_POINT('Ctrl Pts',(9.18603701199994,15.2,-6.36424693700001));
#176312=CARTESIAN_POINT('Ctrl Pts',(9.18603701199994,11.6,-6.36424693700001));
#176313=CARTESIAN_POINT('Ctrl Pts',(9.18420793799994,15.2,-6.36142709300002));
#176314=CARTESIAN_POINT('Ctrl Pts',(9.18420793799994,11.6,-6.36142709300002));
#176315=CARTESIAN_POINT('Ctrl Pts',(9.18237931399995,15.2,-6.35861282700001));
#176316=CARTESIAN_POINT('Ctrl Pts',(9.18237931399995,11.6,-6.35861282700001));
#176317=CARTESIAN_POINT('Ctrl Pts',(9.18055114899994,15.2,-6.35580414200002));
#176318=CARTESIAN_POINT('Ctrl Pts',(9.18055114899994,11.6,-6.35580414200002));
#176319=CARTESIAN_POINT('Ctrl Pts',(9.17872345399994,15.2,-6.35300104400002));
#176320=CARTESIAN_POINT('Ctrl Pts',(9.17872345399994,11.6,-6.35300104400002));
#176321=CARTESIAN_POINT('Ctrl Pts',(9.17689623699994,15.2,-6.35020353500002));
#176322=CARTESIAN_POINT('Ctrl Pts',(9.17689623699994,11.6,-6.35020353500002));
#176323=CARTESIAN_POINT('Ctrl Pts',(9.17506951099995,15.2,-6.34741161800001));
#176324=CARTESIAN_POINT('Ctrl Pts',(9.17506951099995,11.6,-6.34741161800001));
#176325=CARTESIAN_POINT('Ctrl Pts',(9.17324328399994,15.2,-6.34462529700001));
#176326=CARTESIAN_POINT('Ctrl Pts',(9.17324328399994,11.6,-6.34462529700001));
#176327=CARTESIAN_POINT('Ctrl Pts',(9.17141756599994,15.2,-6.34184457400002));
#176328=CARTESIAN_POINT('Ctrl Pts',(9.17141756599994,11.6,-6.34184457400002));
#176329=CARTESIAN_POINT('Ctrl Pts',(9.16959236899995,15.2,-6.33906945400001));
#176330=CARTESIAN_POINT('Ctrl Pts',(9.16959236899995,11.6,-6.33906945400001));
#176331=CARTESIAN_POINT('Ctrl Pts',(9.16776770299995,15.2,-6.33629993900002));
#176332=CARTESIAN_POINT('Ctrl Pts',(9.16776770299995,11.6,-6.33629993900002));
#176333=CARTESIAN_POINT('Ctrl Pts',(9.16594357499994,15.2,-6.33353603400002));
#176334=CARTESIAN_POINT('Ctrl Pts',(9.16594357499994,11.6,-6.33353603400002));
#176335=CARTESIAN_POINT('Ctrl Pts',(9.16411999899994,15.2,-6.33077774000002));
#176336=CARTESIAN_POINT('Ctrl Pts',(9.16411999899994,11.6,-6.33077774000002));
#176337=CARTESIAN_POINT('Ctrl Pts',(9.16229698199994,15.2,-6.32802506300001));
#176338=CARTESIAN_POINT('Ctrl Pts',(9.16229698199994,11.6,-6.32802506300001));
#176339=CARTESIAN_POINT('Ctrl Pts',(9.16047453799994,15.2,-6.32527800400001));
#176340=CARTESIAN_POINT('Ctrl Pts',(9.16047453799994,11.6,-6.32527800400001));
#176341=CARTESIAN_POINT('Ctrl Pts',(9.15865267499994,15.2,-6.32253656800002));
#176342=CARTESIAN_POINT('Ctrl Pts',(9.15865267499994,11.6,-6.32253656800002));
#176343=CARTESIAN_POINT('Ctrl Pts',(9.15683140299994,15.2,-6.31980075800002));
#176344=CARTESIAN_POINT('Ctrl Pts',(9.15683140299994,11.6,-6.31980075800002));
#176345=CARTESIAN_POINT('Ctrl Pts',(9.15501073299994,15.2,-6.31707057600002));
#176346=CARTESIAN_POINT('Ctrl Pts',(9.15501073299994,11.6,-6.31707057600002));
#176347=CARTESIAN_POINT('Ctrl Pts',(9.15319067499994,15.2,-6.31434602700002));
#176348=CARTESIAN_POINT('Ctrl Pts',(9.15319067499994,11.6,-6.31434602700002));
#176349=CARTESIAN_POINT('Ctrl Pts',(9.15137123999994,15.2,-6.31162711400002));
#176350=CARTESIAN_POINT('Ctrl Pts',(9.15137123999994,11.6,-6.31162711400002));
#176351=CARTESIAN_POINT('Ctrl Pts',(9.14955243799995,15.2,-6.30891384000002));
#176352=CARTESIAN_POINT('Ctrl Pts',(9.14955243799995,11.6,-6.30891384000002));
#176353=CARTESIAN_POINT('Ctrl Pts',(9.14773427999994,15.2,-6.30620620700002));
#176354=CARTESIAN_POINT('Ctrl Pts',(9.14773427999994,11.6,-6.30620620700002));
#176355=CARTESIAN_POINT('Ctrl Pts',(9.14591677499994,15.2,-6.30350422100002));
#176356=CARTESIAN_POINT('Ctrl Pts',(9.14591677499994,11.6,-6.30350422100002));
#176357=CARTESIAN_POINT('Ctrl Pts',(9.14409993499994,15.2,-6.30080788400001));
#176358=CARTESIAN_POINT('Ctrl Pts',(9.14409993499994,11.6,-6.30080788400001));
#176359=CARTESIAN_POINT('Ctrl Pts',(9.14228376999995,15.2,-6.29811719800002));
#176360=CARTESIAN_POINT('Ctrl Pts',(9.14228376999995,11.6,-6.29811719800002));
#176361=CARTESIAN_POINT('Ctrl Pts',(9.14046828999994,15.2,-6.29543216900001));
#176362=CARTESIAN_POINT('Ctrl Pts',(9.14046828999994,11.6,-6.29543216900001));
#176363=CARTESIAN_POINT('Ctrl Pts',(9.13865350699994,15.2,-6.29275279900002));
#176364=CARTESIAN_POINT('Ctrl Pts',(9.13865350699994,11.6,-6.29275279900002));
#176365=CARTESIAN_POINT('Ctrl Pts',(9.13683942899995,15.2,-6.29007909000002));
#176366=CARTESIAN_POINT('Ctrl Pts',(9.13683942899995,11.6,-6.29007909000002));
#176367=CARTESIAN_POINT('Ctrl Pts',(9.13502606899995,15.2,-6.28741104800002));
#176368=CARTESIAN_POINT('Ctrl Pts',(9.13502606899995,11.6,-6.28741104800002));
#176369=CARTESIAN_POINT('Ctrl Pts',(9.13321343699995,15.2,-6.28474867500002));
#176370=CARTESIAN_POINT('Ctrl Pts',(9.13321343699995,11.6,-6.28474867500002));
#176371=CARTESIAN_POINT('Ctrl Pts',(9.13140154299995,15.2,-6.28209197300002));
#176372=CARTESIAN_POINT('Ctrl Pts',(9.13140154299995,11.6,-6.28209197300002));
#176373=CARTESIAN_POINT('Ctrl Pts',(9.12959039799994,15.2,-6.27944094700001));
#176374=CARTESIAN_POINT('Ctrl Pts',(9.12959039799994,11.6,-6.27944094700001));
#176375=CARTESIAN_POINT('Ctrl Pts',(9.12778001299994,15.2,-6.27679560000002));
#176376=CARTESIAN_POINT('Ctrl Pts',(9.12778001299994,11.6,-6.27679560000002));
#176377=CARTESIAN_POINT('Ctrl Pts',(9.12597039799994,15.2,-6.27415593400002));
#176378=CARTESIAN_POINT('Ctrl Pts',(9.12597039799994,11.6,-6.27415593400002));
#176379=CARTESIAN_POINT('Ctrl Pts',(9.12416156499994,15.2,-6.27152195500001));
#176380=CARTESIAN_POINT('Ctrl Pts',(9.12416156499994,11.6,-6.27152195500001));
#176381=CARTESIAN_POINT('Ctrl Pts',(9.12235352399994,15.2,-6.26889366400002));
#176382=CARTESIAN_POINT('Ctrl Pts',(9.12235352399994,11.6,-6.26889366400002));
#176383=CARTESIAN_POINT('Ctrl Pts',(9.12054628499994,15.2,-6.26627106500001));
#176384=CARTESIAN_POINT('Ctrl Pts',(9.12054628499994,11.6,-6.26627106500001));
#176385=CARTESIAN_POINT('Ctrl Pts',(9.11873985999994,15.2,-6.26365416200001));
#176386=CARTESIAN_POINT('Ctrl Pts',(9.11873985999994,11.6,-6.26365416200001));
#176387=CARTESIAN_POINT('Ctrl Pts',(9.11693425999994,15.2,-6.26104295700002));
#176388=CARTESIAN_POINT('Ctrl Pts',(9.11693425999994,11.6,-6.26104295700002));
#176389=CARTESIAN_POINT('Ctrl Pts',(9.11512949499994,15.2,-6.25843745400001));
#176390=CARTESIAN_POINT('Ctrl Pts',(9.11512949499994,11.6,-6.25843745400001));
#176391=CARTESIAN_POINT('Ctrl Pts',(9.11332557599994,15.2,-6.25583765700001));
#176392=CARTESIAN_POINT('Ctrl Pts',(9.11332557599994,11.6,-6.25583765700001));
#176393=CARTESIAN_POINT('Ctrl Pts',(9.11152251499994,15.2,-6.25324356700002));
#176394=CARTESIAN_POINT('Ctrl Pts',(9.11152251499994,11.6,-6.25324356700002));
#176395=CARTESIAN_POINT('Ctrl Pts',(9.10972032099994,15.2,-6.25065519100002));
#176396=CARTESIAN_POINT('Ctrl Pts',(9.10972032099994,11.6,-6.25065519100002));
#176397=CARTESIAN_POINT('Ctrl Pts',(9.10791900599994,15.2,-6.24807252900001));
#176398=CARTESIAN_POINT('Ctrl Pts',(9.10791900599994,11.6,-6.24807252900001));
#176399=CARTESIAN_POINT('Ctrl Pts',(9.10611858299994,15.2,-6.24549558500001));
#176400=CARTESIAN_POINT('Ctrl Pts',(9.10611858299994,11.6,-6.24549558500001));
#176401=CARTESIAN_POINT('Ctrl Pts',(9.10431905899994,15.2,-6.24292436300002));
#176402=CARTESIAN_POINT('Ctrl Pts',(9.10431905899994,11.6,-6.24292436300002));
#176403=CARTESIAN_POINT('Ctrl Pts',(9.10252044799994,15.2,-6.24035886600002));
#176404=CARTESIAN_POINT('Ctrl Pts',(9.10252044799994,11.6,-6.24035886600002));
#176405=CARTESIAN_POINT('Ctrl Pts',(9.10072275999994,15.2,-6.23779909700002));
#176406=CARTESIAN_POINT('Ctrl Pts',(9.10072275999994,11.6,-6.23779909700002));
#176407=CARTESIAN_POINT('Ctrl Pts',(9.09892600699994,15.2,-6.23524506100001));
#176408=CARTESIAN_POINT('Ctrl Pts',(9.09892600699994,11.6,-6.23524506100001));
#176409=CARTESIAN_POINT('Ctrl Pts',(9.09713019799994,15.2,-6.23269675900002));
#176410=CARTESIAN_POINT('Ctrl Pts',(9.09713019799994,11.6,-6.23269675900002));
#176411=CARTESIAN_POINT('Ctrl Pts',(9.09533534799994,15.2,-6.23015419500001));
#176412=CARTESIAN_POINT('Ctrl Pts',(9.09533534799994,11.6,-6.23015419500001));
#176413=CARTESIAN_POINT('Ctrl Pts',(9.09354146399994,15.2,-6.22761737200002));
#176414=CARTESIAN_POINT('Ctrl Pts',(9.09354146399994,11.6,-6.22761737200002));
#176415=CARTESIAN_POINT('Ctrl Pts',(9.09174855899994,15.2,-6.22508629400001));
#176416=CARTESIAN_POINT('Ctrl Pts',(9.09174855899994,11.6,-6.22508629400001));
#176417=CARTESIAN_POINT('Ctrl Pts',(9.08995664499994,15.2,-6.22256096500001));
#176418=CARTESIAN_POINT('Ctrl Pts',(9.08995664499994,11.6,-6.22256096500001));
#176419=CARTESIAN_POINT('Ctrl Pts',(9.08816573199994,15.2,-6.22004138600002));
#176420=CARTESIAN_POINT('Ctrl Pts',(9.08816573199994,11.6,-6.22004138600002));
#176421=CARTESIAN_POINT('Ctrl Pts',(9.08637583199994,15.2,-6.21752756200002));
#176422=CARTESIAN_POINT('Ctrl Pts',(9.08637583199994,11.6,-6.21752756200002));
#176423=CARTESIAN_POINT('Ctrl Pts',(9.08458695599995,15.2,-6.21501949500002));
#176424=CARTESIAN_POINT('Ctrl Pts',(9.08458695599995,11.6,-6.21501949500002));
#176425=CARTESIAN_POINT('Ctrl Pts',(9.08279911599994,15.2,-6.21251719000002));
#176426=CARTESIAN_POINT('Ctrl Pts',(9.08279911599994,11.6,-6.21251719000002));
#176427=CARTESIAN_POINT('Ctrl Pts',(9.08101232199994,15.2,-6.21002065000001));
#176428=CARTESIAN_POINT('Ctrl Pts',(9.08101232199994,11.6,-6.21002065000001));
#176429=CARTESIAN_POINT('Ctrl Pts',(9.07922658799994,15.2,-6.20752987600002));
#176430=CARTESIAN_POINT('Ctrl Pts',(9.07922658799994,11.6,-6.20752987600002));
#176431=CARTESIAN_POINT('Ctrl Pts',(9.07744192199995,15.2,-6.20504487400002));
#176432=CARTESIAN_POINT('Ctrl Pts',(9.07744192199995,11.6,-6.20504487400002));
#176433=CARTESIAN_POINT('Ctrl Pts',(9.07565833799995,15.2,-6.20256564500002));
#176434=CARTESIAN_POINT('Ctrl Pts',(9.07565833799995,11.6,-6.20256564500002));
#176435=CARTESIAN_POINT('Ctrl Pts',(9.07387584499994,15.2,-6.20009219400002));
#176436=CARTESIAN_POINT('Ctrl Pts',(9.07387584499994,11.6,-6.20009219400002));
#176437=CARTESIAN_POINT('Ctrl Pts',(9.07209445899994,15.2,-6.19762452400002));
#176438=CARTESIAN_POINT('Ctrl Pts',(9.07209445899994,11.6,-6.19762452400002));
#176439=CARTESIAN_POINT('Ctrl Pts',(9.07031418699994,15.2,-6.19516263800002));
#176440=CARTESIAN_POINT('Ctrl Pts',(9.07031418699994,11.6,-6.19516263800002));
#176441=CARTESIAN_POINT('Ctrl Pts',(9.06853504099994,15.2,-6.19270653800001));
#176442=CARTESIAN_POINT('Ctrl Pts',(9.06853504099994,11.6,-6.19270653800001));
#176443=CARTESIAN_POINT('Ctrl Pts',(9.06675703599995,15.2,-6.19025623000002));
#176444=CARTESIAN_POINT('Ctrl Pts',(9.06675703599995,11.6,-6.19025623000002));
#176445=CARTESIAN_POINT('Ctrl Pts',(9.06498018099994,15.2,-6.18781171400002));
#176446=CARTESIAN_POINT('Ctrl Pts',(9.06498018099994,11.6,-6.18781171400002));
#176447=CARTESIAN_POINT('Ctrl Pts',(9.06320448699995,15.2,-6.18537299700002));
#176448=CARTESIAN_POINT('Ctrl Pts',(9.06320448699995,11.6,-6.18537299700002));
#176449=CARTESIAN_POINT('Ctrl Pts',(9.06142996799994,15.2,-6.18294007900002));
#176450=CARTESIAN_POINT('Ctrl Pts',(9.06142996799994,11.6,-6.18294007900002));
#176451=CARTESIAN_POINT('Ctrl Pts',(9.05965663399994,15.2,-6.18051296400001));
#176452=CARTESIAN_POINT('Ctrl Pts',(9.05965663399994,11.6,-6.18051296400001));
#176453=CARTESIAN_POINT('Ctrl Pts',(9.05788449699994,15.2,-6.17809165700002));
#176454=CARTESIAN_POINT('Ctrl Pts',(9.05788449699994,11.6,-6.17809165700002));
#176455=CARTESIAN_POINT('Ctrl Pts',(9.05611356899995,15.2,-6.17567615900001));
#176456=CARTESIAN_POINT('Ctrl Pts',(9.05611356899995,11.6,-6.17567615900001));
#176457=CARTESIAN_POINT('Ctrl Pts',(9.05434386299994,15.2,-6.17326647400001));
#176458=CARTESIAN_POINT('Ctrl Pts',(9.05434386299994,11.6,-6.17326647400001));
#176459=CARTESIAN_POINT('Ctrl Pts',(9.05257538899994,15.2,-6.17086260600002));
#176460=CARTESIAN_POINT('Ctrl Pts',(9.05257538899994,11.6,-6.17086260600002));
#176461=CARTESIAN_POINT('Ctrl Pts',(9.05080815899994,15.2,-6.16846455700002));
#176462=CARTESIAN_POINT('Ctrl Pts',(9.05080815899994,11.6,-6.16846455700002));
#176463=CARTESIAN_POINT('Ctrl Pts',(9.04904218599994,15.2,-6.16607233100002));
#176464=CARTESIAN_POINT('Ctrl Pts',(9.04904218599994,11.6,-6.16607233100002));
#176465=CARTESIAN_POINT('Ctrl Pts',(9.04727748099994,15.2,-6.16368593200002));
#176466=CARTESIAN_POINT('Ctrl Pts',(9.04727748099994,11.6,-6.16368593200002));
#176467=CARTESIAN_POINT('Ctrl Pts',(9.04551405599994,15.2,-6.16130536200002));
#176468=CARTESIAN_POINT('Ctrl Pts',(9.04551405599994,11.6,-6.16130536200002));
#176469=CARTESIAN_POINT('Ctrl Pts',(9.04375192399994,15.2,-6.15893062400002));
#176470=CARTESIAN_POINT('Ctrl Pts',(9.04375192399994,11.6,-6.15893062400002));
#176471=CARTESIAN_POINT('Ctrl Pts',(9.04199109499995,15.2,-6.15656172200002));
#176472=CARTESIAN_POINT('Ctrl Pts',(9.04199109499995,11.6,-6.15656172200002));
#176473=CARTESIAN_POINT('Ctrl Pts',(9.04023158399994,15.2,-6.15419865900002));
#176474=CARTESIAN_POINT('Ctrl Pts',(9.04023158399994,11.6,-6.15419865900002));
#176475=CARTESIAN_POINT('Ctrl Pts',(9.03847339899994,15.2,-6.15184143900001));
#176476=CARTESIAN_POINT('Ctrl Pts',(9.03847339899994,11.6,-6.15184143900001));
#176477=CARTESIAN_POINT('Ctrl Pts',(9.03671655699995,15.2,-6.14949006400002));
#176478=CARTESIAN_POINT('Ctrl Pts',(9.03671655699995,11.6,-6.14949006400002));
#176479=CARTESIAN_POINT('Ctrl Pts',(9.03496106599994,15.2,-6.14714453800002));
#176480=CARTESIAN_POINT('Ctrl Pts',(9.03496106599994,11.6,-6.14714453800002));
#176481=CARTESIAN_POINT('Ctrl Pts',(9.03320693999994,15.2,-6.14480486300002));
#176482=CARTESIAN_POINT('Ctrl Pts',(9.03320693999994,11.6,-6.14480486300002));
#176483=CARTESIAN_POINT('Ctrl Pts',(9.03145419199994,15.2,-6.14247104400001));
#176484=CARTESIAN_POINT('Ctrl Pts',(9.03145419199994,11.6,-6.14247104400001));
#176485=CARTESIAN_POINT('Ctrl Pts',(9.02970283099994,15.2,-6.14014308300002));
#176486=CARTESIAN_POINT('Ctrl Pts',(9.02970283099994,11.6,-6.14014308300002));
#176487=CARTESIAN_POINT('Ctrl Pts',(9.02795287299995,15.2,-6.13782098500002));
#176488=CARTESIAN_POINT('Ctrl Pts',(9.02795287299995,11.6,-6.13782098500002));
#176489=CARTESIAN_POINT('Ctrl Pts',(9.02620432799995,15.2,-6.13550475000002));
#176490=CARTESIAN_POINT('Ctrl Pts',(9.02620432799995,11.6,-6.13550475000002));
#176491=CARTESIAN_POINT('Ctrl Pts',(9.02445720899994,15.2,-6.13319438400002));
#176492=CARTESIAN_POINT('Ctrl Pts',(9.02445720899994,11.6,-6.13319438400002));
#176493=CARTESIAN_POINT('Ctrl Pts',(9.02271152799995,15.2,-6.13088988900002));
#176494=CARTESIAN_POINT('Ctrl Pts',(9.02271152799995,11.6,-6.13088988900002));
#176495=CARTESIAN_POINT('Ctrl Pts',(9.02096729899995,15.2,-6.12859126900001));
#176496=CARTESIAN_POINT('Ctrl Pts',(9.02096729899995,11.6,-6.12859126900001));
#176497=CARTESIAN_POINT('Ctrl Pts',(9.01922453199994,15.2,-6.12629852600002));
#176498=CARTESIAN_POINT('Ctrl Pts',(9.01922453199994,11.6,-6.12629852600002));
#176499=CARTESIAN_POINT('Ctrl Pts',(9.01748323999995,15.2,-6.12401166400002));
#176500=CARTESIAN_POINT('Ctrl Pts',(9.01748323999995,11.6,-6.12401166400002));
#176501=CARTESIAN_POINT('Ctrl Pts',(9.01574343699994,15.2,-6.12173068600002));
#176502=CARTESIAN_POINT('Ctrl Pts',(9.01574343699994,11.6,-6.12173068600002));
#176503=CARTESIAN_POINT('Ctrl Pts',(9.01400513499994,15.2,-6.11945559600001));
#176504=CARTESIAN_POINT('Ctrl Pts',(9.01400513499994,11.6,-6.11945559600001));
#176505=CARTESIAN_POINT('Ctrl Pts',(9.01226834599994,15.2,-6.11718639600002));
#176506=CARTESIAN_POINT('Ctrl Pts',(9.01226834599994,11.6,-6.11718639600002));
#176507=CARTESIAN_POINT('Ctrl Pts',(9.01053308099995,15.2,-6.11492308900001));
#176508=CARTESIAN_POINT('Ctrl Pts',(9.01053308099995,11.6,-6.11492308900001));
#176509=CARTESIAN_POINT('Ctrl Pts',(9.00879935499994,15.2,-6.11266568000002));
#176510=CARTESIAN_POINT('Ctrl Pts',(9.00879935499994,11.6,-6.11266568000002));
#176511=CARTESIAN_POINT('Ctrl Pts',(9.00706718099994,15.2,-6.11041417100001));
#176512=CARTESIAN_POINT('Ctrl Pts',(9.00706718099994,11.6,-6.11041417100001));
#176513=CARTESIAN_POINT('Ctrl Pts',(9.00533656799994,15.2,-6.10816856500002));
#176514=CARTESIAN_POINT('Ctrl Pts',(9.00533656799994,11.6,-6.10816856500002));
#176515=CARTESIAN_POINT('Ctrl Pts',(9.00360753399994,15.2,-6.10592886600001));
#176516=CARTESIAN_POINT('Ctrl Pts',(9.00360753399994,11.6,-6.10592886600001));
#176517=CARTESIAN_POINT('Ctrl Pts',(9.00188008699994,15.2,-6.10369507500002));
#176518=CARTESIAN_POINT('Ctrl Pts',(9.00188008699994,11.6,-6.10369507500002));
#176519=CARTESIAN_POINT('Ctrl Pts',(9.00015424299994,15.2,-6.10146719900002));
#176520=CARTESIAN_POINT('Ctrl Pts',(9.00015424299994,11.6,-6.10146719900002));
#176521=CARTESIAN_POINT('Ctrl Pts',(8.99843001299995,15.2,-6.09924523800002));
#176522=CARTESIAN_POINT('Ctrl Pts',(8.99843001299995,11.6,-6.09924523800002));
#176523=CARTESIAN_POINT('Ctrl Pts',(8.99670740999994,15.2,-6.09702919700001));
#176524=CARTESIAN_POINT('Ctrl Pts',(8.99670740999994,11.6,-6.09702919700001));
#176525=CARTESIAN_POINT('Ctrl Pts',(8.99498644699994,15.2,-6.09481907700002));
#176526=CARTESIAN_POINT('Ctrl Pts',(8.99498644699994,11.6,-6.09481907700002));
#176527=CARTESIAN_POINT('Ctrl Pts',(8.99326713699995,15.2,-6.09261488300002));
#176528=CARTESIAN_POINT('Ctrl Pts',(8.99326713699995,11.6,-6.09261488300002));
#176529=CARTESIAN_POINT('Ctrl Pts',(8.99154949399994,15.2,-6.09041661900001));
#176530=CARTESIAN_POINT('Ctrl Pts',(8.99154949399994,11.6,-6.09041661900001));
#176531=CARTESIAN_POINT('Ctrl Pts',(8.98983352999995,15.2,-6.08822428600002));
#176532=CARTESIAN_POINT('Ctrl Pts',(8.98983352999995,11.6,-6.08822428600002));
#176533=CARTESIAN_POINT('Ctrl Pts',(8.98811925699994,15.2,-6.08603788900002));
#176534=CARTESIAN_POINT('Ctrl Pts',(8.98811925699994,11.6,-6.08603788900002));
#176535=CARTESIAN_POINT('Ctrl Pts',(8.98640668999995,15.2,-6.08385743000002));
#176536=CARTESIAN_POINT('Ctrl Pts',(8.98640668999995,11.6,-6.08385743000002));
#176537=CARTESIAN_POINT('Ctrl Pts',(8.98469584099994,15.2,-6.08168291200001));
#176538=CARTESIAN_POINT('Ctrl Pts',(8.98469584099994,11.6,-6.08168291200001));
#176539=CARTESIAN_POINT('Ctrl Pts',(8.98298672299994,15.2,-6.07951433900002));
#176540=CARTESIAN_POINT('Ctrl Pts',(8.98298672299994,11.6,-6.07951433900002));
#176541=CARTESIAN_POINT('Ctrl Pts',(8.98127934999994,15.2,-6.07735171400002));
#176542=CARTESIAN_POINT('Ctrl Pts',(8.98127934999994,11.6,-6.07735171400002));
#176543=CARTESIAN_POINT('Ctrl Pts',(8.97957373299995,15.2,-6.07519503900001));
#176544=CARTESIAN_POINT('Ctrl Pts',(8.97957373299995,11.6,-6.07519503900001));
#176545=CARTESIAN_POINT('Ctrl Pts',(8.97786988799995,15.2,-6.07304431900002));
#176546=CARTESIAN_POINT('Ctrl Pts',(8.97786988799995,11.6,-6.07304431900002));
#176547=CARTESIAN_POINT('Ctrl Pts',(8.97616782599994,15.2,-6.07089955700002));
#176548=CARTESIAN_POINT('Ctrl Pts',(8.97616782599994,11.6,-6.07089955700002));
#176549=CARTESIAN_POINT('Ctrl Pts',(8.97446756199994,15.2,-6.06876075400002));
#176550=CARTESIAN_POINT('Ctrl Pts',(8.97446756199994,11.6,-6.06876075400002));
#176551=CARTESIAN_POINT('Ctrl Pts',(8.97276910899994,15.2,-6.06662791500002));
#176552=CARTESIAN_POINT('Ctrl Pts',(8.97276910899994,11.6,-6.06662791500002));
#176553=CARTESIAN_POINT('Ctrl Pts',(8.97107247999994,15.2,-6.06450104300002));
#176554=CARTESIAN_POINT('Ctrl Pts',(8.97107247999994,11.6,-6.06450104300002));
#176555=CARTESIAN_POINT('Ctrl Pts',(8.96937768699994,15.2,-6.06238014200001));
#176556=CARTESIAN_POINT('Ctrl Pts',(8.96937768699994,11.6,-6.06238014200001));
#176557=CARTESIAN_POINT('Ctrl Pts',(8.96768474699994,15.2,-6.06026521400001));
#176558=CARTESIAN_POINT('Ctrl Pts',(8.96768474699994,11.6,-6.06026521400001));
#176559=CARTESIAN_POINT('Ctrl Pts',(8.96599366899994,15.2,-6.05815626100001));
#176560=CARTESIAN_POINT('Ctrl Pts',(8.96599366899994,11.6,-6.05815626100001));
#176561=CARTESIAN_POINT('Ctrl Pts',(8.96430446999995,15.2,-6.05605328800002));
#176562=CARTESIAN_POINT('Ctrl Pts',(8.96430446999995,11.6,-6.05605328800002));
#176563=CARTESIAN_POINT('Ctrl Pts',(8.96261716099995,15.2,-6.05395629800002));
#176564=CARTESIAN_POINT('Ctrl Pts',(8.96261716099995,11.6,-6.05395629800002));
#176565=CARTESIAN_POINT('Ctrl Pts',(8.96093175899994,15.2,-6.05186529300001));
#176566=CARTESIAN_POINT('Ctrl Pts',(8.96093175899994,11.6,-6.05186529300001));
#176567=CARTESIAN_POINT('Ctrl Pts',(8.95924827399995,15.2,-6.04978027700002));
#176568=CARTESIAN_POINT('Ctrl Pts',(8.95924827399995,11.6,-6.04978027700002));
#176569=CARTESIAN_POINT('Ctrl Pts',(8.95756672099994,15.2,-6.04770125400002));
#176570=CARTESIAN_POINT('Ctrl Pts',(8.95756672099994,11.6,-6.04770125400002));
#176571=CARTESIAN_POINT('Ctrl Pts',(8.95588711299995,15.2,-6.04562822500001));
#176572=CARTESIAN_POINT('Ctrl Pts',(8.95588711299995,11.6,-6.04562822500001));
#176573=CARTESIAN_POINT('Ctrl Pts',(8.95420946599994,15.2,-6.04356119500002));
#176574=CARTESIAN_POINT('Ctrl Pts',(8.95420946599994,11.6,-6.04356119500002));
#176575=CARTESIAN_POINT('Ctrl Pts',(8.95253379199995,15.2,-6.04150016600002));
#176576=CARTESIAN_POINT('Ctrl Pts',(8.95253379199995,11.6,-6.04150016600002));
#176577=CARTESIAN_POINT('Ctrl Pts',(8.95086010499995,15.2,-6.03944514200002));
#176578=CARTESIAN_POINT('Ctrl Pts',(8.95086010499995,11.6,-6.03944514200002));
#176579=CARTESIAN_POINT('Ctrl Pts',(8.94918841899995,15.2,-6.03739612600001));
#176580=CARTESIAN_POINT('Ctrl Pts',(8.94918841899995,11.6,-6.03739612600001));
#176581=CARTESIAN_POINT('Ctrl Pts',(8.94751874699995,15.2,-6.03535312000002));
#176582=CARTESIAN_POINT('Ctrl Pts',(8.94751874699995,11.6,-6.03535312000002));
#176583=CARTESIAN_POINT('Ctrl Pts',(8.94585110499994,15.2,-6.03331612800002));
#176584=CARTESIAN_POINT('Ctrl Pts',(8.94585110499994,11.6,-6.03331612800002));
#176585=CARTESIAN_POINT('Ctrl Pts',(8.94418550499994,15.2,-6.03128515400002));
#176586=CARTESIAN_POINT('Ctrl Pts',(8.94418550499994,11.6,-6.03128515400002));
#176587=CARTESIAN_POINT('Ctrl Pts',(8.94252196199995,15.2,-6.02926020000002));
#176588=CARTESIAN_POINT('Ctrl Pts',(8.94252196199995,11.6,-6.02926020000002));
#176589=CARTESIAN_POINT('Ctrl Pts',(8.94086048799995,15.2,-6.02724126900001));
#176590=CARTESIAN_POINT('Ctrl Pts',(8.94086048799995,11.6,-6.02724126900001));
#176591=CARTESIAN_POINT('Ctrl Pts',(8.93920109999994,15.2,-6.02522836400002));
#176592=CARTESIAN_POINT('Ctrl Pts',(8.93920109999994,11.6,-6.02522836400002));
#176593=CARTESIAN_POINT('Ctrl Pts',(8.93754381099994,15.2,-6.02322149000001));
#176594=CARTESIAN_POINT('Ctrl Pts',(8.93754381099994,11.6,-6.02322149000001));
#176595=CARTESIAN_POINT('Ctrl Pts',(8.93588863499994,15.2,-6.02122064700002));
#176596=CARTESIAN_POINT('Ctrl Pts',(8.93588863499994,11.6,-6.02122064700002));
#176597=CARTESIAN_POINT('Ctrl Pts',(8.93423558499994,15.2,-6.01922584200001));
#176598=CARTESIAN_POINT('Ctrl Pts',(8.93423558499994,11.6,-6.01922584200001));
#176599=CARTESIAN_POINT('Ctrl Pts',(8.93258467799994,15.2,-6.01723707400001));
#176600=CARTESIAN_POINT('Ctrl Pts',(8.93258467799994,11.6,-6.01723707400001));
#176601=CARTESIAN_POINT('Ctrl Pts',(8.93093592599995,15.2,-6.01525434800001));
#176602=CARTESIAN_POINT('Ctrl Pts',(8.93093592599995,11.6,-6.01525434800001));
#176603=CARTESIAN_POINT('Ctrl Pts',(8.92928934299994,15.2,-6.01327766800001));
#176604=CARTESIAN_POINT('Ctrl Pts',(8.92928934299994,11.6,-6.01327766800001));
#176605=CARTESIAN_POINT('Ctrl Pts',(8.92764494599994,15.2,-6.01130703600001));
#176606=CARTESIAN_POINT('Ctrl Pts',(8.92764494599994,11.6,-6.01130703600001));
#176607=CARTESIAN_POINT('Ctrl Pts',(8.92600274799995,15.2,-6.00934245600002));
#176608=CARTESIAN_POINT('Ctrl Pts',(8.92600274799995,11.6,-6.00934245600002));
#176609=CARTESIAN_POINT('Ctrl Pts',(8.92436276099994,15.2,-6.00738393100002));
#176610=CARTESIAN_POINT('Ctrl Pts',(8.92436276099994,11.6,-6.00738393100002));
#176611=CARTESIAN_POINT('Ctrl Pts',(8.92272500299994,15.2,-6.00543146300001));
#176612=CARTESIAN_POINT('Ctrl Pts',(8.92272500299994,11.6,-6.00543146300001));
#176613=CARTESIAN_POINT('Ctrl Pts',(8.92108948699994,15.2,-6.00348505400002));
#176614=CARTESIAN_POINT('Ctrl Pts',(8.92108948699994,11.6,-6.00348505400002));
#176615=CARTESIAN_POINT('Ctrl Pts',(8.91945622699994,15.2,-6.00154471100002));
#176616=CARTESIAN_POINT('Ctrl Pts',(8.91945622699994,11.6,-6.00154471100002));
#176617=CARTESIAN_POINT('Ctrl Pts',(8.91782523999994,15.2,-5.99961043300001));
#176618=CARTESIAN_POINT('Ctrl Pts',(8.91782523999994,11.6,-5.99961043300001));
#176619=CARTESIAN_POINT('Ctrl Pts',(8.91619653799994,15.2,-5.99768222700002));
#176620=CARTESIAN_POINT('Ctrl Pts',(8.91619653799994,11.6,-5.99768222700002));
#176621=CARTESIAN_POINT('Ctrl Pts',(8.91457013499994,15.2,-5.99576009400002));
#176622=CARTESIAN_POINT('Ctrl Pts',(8.91457013499994,11.6,-5.99576009400002));
#176623=CARTESIAN_POINT('Ctrl Pts',(8.91294604899995,15.2,-5.99384403500002));
#176624=CARTESIAN_POINT('Ctrl Pts',(8.91294604899995,11.6,-5.99384403500002));
#176625=CARTESIAN_POINT('Ctrl Pts',(8.91132429299994,15.2,-5.99193405800002));
#176626=CARTESIAN_POINT('Ctrl Pts',(8.91132429299994,11.6,-5.99193405800002));
#176627=CARTESIAN_POINT('Ctrl Pts',(8.90970488099994,15.2,-5.99003016200002));
#176628=CARTESIAN_POINT('Ctrl Pts',(8.90970488099994,11.6,-5.99003016200002));
#176629=CARTESIAN_POINT('Ctrl Pts',(8.90808782999994,15.2,-5.98813235200002));
#176630=CARTESIAN_POINT('Ctrl Pts',(8.90808782999994,11.6,-5.98813235200002));
#176631=CARTESIAN_POINT('Ctrl Pts',(8.90647315299995,15.2,-5.98624063000001));
#176632=CARTESIAN_POINT('Ctrl Pts',(8.90647315299995,11.6,-5.98624063000001));
#176633=CARTESIAN_POINT('Ctrl Pts',(8.90486086599994,15.2,-5.98435499900001));
#176634=CARTESIAN_POINT('Ctrl Pts',(8.90486086599994,11.6,-5.98435499900001));
#176635=CARTESIAN_POINT('Ctrl Pts',(8.90325098299994,15.2,-5.98247546400002));
#176636=CARTESIAN_POINT('Ctrl Pts',(8.90325098299994,11.6,-5.98247546400002));
#176637=CARTESIAN_POINT('Ctrl Pts',(8.90164351899994,15.2,-5.98060202600001));
#176638=CARTESIAN_POINT('Ctrl Pts',(8.90164351899994,11.6,-5.98060202600001));
#176639=CARTESIAN_POINT('Ctrl Pts',(8.90003849099994,15.2,-5.97873468800002));
#176640=CARTESIAN_POINT('Ctrl Pts',(8.90003849099994,11.6,-5.97873468800002));
#176641=CARTESIAN_POINT('Ctrl Pts',(8.89843591199994,15.2,-5.97687345600002));
#176642=CARTESIAN_POINT('Ctrl Pts',(8.89843591199994,11.6,-5.97687345600002));
#176643=CARTESIAN_POINT('Ctrl Pts',(8.89683579899994,15.2,-5.97501833000001));
#176644=CARTESIAN_POINT('Ctrl Pts',(8.89683579899994,11.6,-5.97501833000001));
#176645=CARTESIAN_POINT('Ctrl Pts',(8.89523816499995,15.2,-5.97316931300002));
#176646=CARTESIAN_POINT('Ctrl Pts',(8.89523816499995,11.6,-5.97316931300002));
#176647=CARTESIAN_POINT('Ctrl Pts',(8.89364302699994,15.2,-5.97132641100002));
#176648=CARTESIAN_POINT('Ctrl Pts',(8.89364302699994,11.6,-5.97132641100002));
#176649=CARTESIAN_POINT('Ctrl Pts',(8.89205039799995,15.2,-5.96948962400001));
#176650=CARTESIAN_POINT('Ctrl Pts',(8.89205039799995,11.6,-5.96948962400001));
#176651=CARTESIAN_POINT('Ctrl Pts',(8.89046029699994,15.2,-5.96765895700001));
#176652=CARTESIAN_POINT('Ctrl Pts',(8.89046029699994,11.6,-5.96765895700001));
#176653=CARTESIAN_POINT('Ctrl Pts',(8.88887273699994,15.2,-5.96583441200002));
#176654=CARTESIAN_POINT('Ctrl Pts',(8.88887273699994,11.6,-5.96583441200002));
#176655=CARTESIAN_POINT('Ctrl Pts',(8.88728773299994,15.2,-5.96401599200002));
#176656=CARTESIAN_POINT('Ctrl Pts',(8.88728773299994,11.6,-5.96401599200002));
#176657=CARTESIAN_POINT('Ctrl Pts',(8.88570530199994,15.2,-5.96220370100002));
#176658=CARTESIAN_POINT('Ctrl Pts',(8.88570530199994,11.6,-5.96220370100002));
#176659=CARTESIAN_POINT('Ctrl Pts',(8.88412545799994,15.2,-5.96039754200002));
#176660=CARTESIAN_POINT('Ctrl Pts',(8.88412545799994,11.6,-5.96039754200002));
#176661=CARTESIAN_POINT('Ctrl Pts',(8.88254821799995,15.2,-5.95859751700001));
#176662=CARTESIAN_POINT('Ctrl Pts',(8.88254821799995,11.6,-5.95859751700001));
#176663=CARTESIAN_POINT('Ctrl Pts',(8.88097359799995,15.2,-5.95680362900002));
#176664=CARTESIAN_POINT('Ctrl Pts',(8.88097359799995,11.6,-5.95680362900002));
#176665=CARTESIAN_POINT('Ctrl Pts',(8.87940161099994,15.2,-5.95501588200002));
#176666=CARTESIAN_POINT('Ctrl Pts',(8.87940161099994,11.6,-5.95501588200002));
#176667=CARTESIAN_POINT('Ctrl Pts',(8.87783227599994,15.2,-5.95323427800002));
#176668=CARTESIAN_POINT('Ctrl Pts',(8.87783227599994,11.6,-5.95323427800002));
#176669=CARTESIAN_POINT('Ctrl Pts',(8.87626560599994,15.2,-5.95145882200002));
#176670=CARTESIAN_POINT('Ctrl Pts',(8.87626560599994,11.6,-5.95145882200002));
#176671=CARTESIAN_POINT('Ctrl Pts',(8.87470161799994,15.2,-5.94968951600002));
#176672=CARTESIAN_POINT('Ctrl Pts',(8.87470161799994,11.6,-5.94968951600002));
#176673=CARTESIAN_POINT('Ctrl Pts',(8.87314032799994,15.2,-5.94792636200002));
#176674=CARTESIAN_POINT('Ctrl Pts',(8.87314032799994,11.6,-5.94792636200002));
#176675=CARTESIAN_POINT('Ctrl Pts',(8.87158175199994,15.2,-5.94616936400002));
#176676=CARTESIAN_POINT('Ctrl Pts',(8.87158175199994,11.6,-5.94616936400002));
#176677=CARTESIAN_POINT('Ctrl Pts',(8.87002590499994,15.2,-5.94441852500001));
#176678=CARTESIAN_POINT('Ctrl Pts',(8.87002590499994,11.6,-5.94441852500001));
#176679=CARTESIAN_POINT('Ctrl Pts',(8.86847280499994,15.2,-5.94267384800002));
#176680=CARTESIAN_POINT('Ctrl Pts',(8.86847280499994,11.6,-5.94267384800002));
#176681=CARTESIAN_POINT('Ctrl Pts',(8.86692246499994,15.2,-5.94093533700002));
#176682=CARTESIAN_POINT('Ctrl Pts',(8.86692246499994,11.6,-5.94093533700002));
#176683=CARTESIAN_POINT('Ctrl Pts',(8.86537490399994,15.2,-5.93920299200001));
#176684=CARTESIAN_POINT('Ctrl Pts',(8.86537490399994,11.6,-5.93920299200001));
#176685=CARTESIAN_POINT('Ctrl Pts',(8.86383013599995,15.2,-5.93747681900001));
#176686=CARTESIAN_POINT('Ctrl Pts',(8.86383013599995,11.6,-5.93747681900001));
#176687=CARTESIAN_POINT('Ctrl Pts',(8.86228817799994,15.2,-5.93575682000001));
#176688=CARTESIAN_POINT('Ctrl Pts',(8.86228817799994,11.6,-5.93575682000001));
#176689=CARTESIAN_POINT('Ctrl Pts',(8.86074904799995,15.2,-5.93404299900002));
#176690=CARTESIAN_POINT('Ctrl Pts',(8.86074904799995,11.6,-5.93404299900002));
#176691=CARTESIAN_POINT('Ctrl Pts',(8.85921275899994,15.2,-5.93233535700002));
#176692=CARTESIAN_POINT('Ctrl Pts',(8.85921275899994,11.6,-5.93233535700002));
#176693=CARTESIAN_POINT('Ctrl Pts',(8.85767932999994,15.2,-5.93063389900002));
#176694=CARTESIAN_POINT('Ctrl Pts',(8.85767932999994,11.6,-5.93063389900002));
#176695=CARTESIAN_POINT('Ctrl Pts',(8.85614877599994,15.2,-5.92893862600001));
#176696=CARTESIAN_POINT('Ctrl Pts',(8.85614877599994,11.6,-5.92893862600001));
#176697=CARTESIAN_POINT('Ctrl Pts',(8.85462111399994,15.2,-5.92724954300002));
#176698=CARTESIAN_POINT('Ctrl Pts',(8.85462111399994,11.6,-5.92724954300002));
#176699=CARTESIAN_POINT('Ctrl Pts',(8.85309636199995,15.2,-5.92556665200001));
#176700=CARTESIAN_POINT('Ctrl Pts',(8.85309636199995,11.6,-5.92556665200001));
#176701=CARTESIAN_POINT('Ctrl Pts',(8.85157453299995,15.2,-5.92388995600002));
#176702=CARTESIAN_POINT('Ctrl Pts',(8.85157453299995,11.6,-5.92388995600002));
#176703=CARTESIAN_POINT('Ctrl Pts',(8.85005564599994,15.2,-5.92221945900001));
#176704=CARTESIAN_POINT('Ctrl Pts',(8.85005564599994,11.6,-5.92221945900001));
#176705=CARTESIAN_POINT('Ctrl Pts',(8.84853971699994,15.2,-5.92055516300002));
#176706=CARTESIAN_POINT('Ctrl Pts',(8.84853971699994,11.6,-5.92055516300002));
#176707=CARTESIAN_POINT('Ctrl Pts',(8.84702676399994,15.2,-5.91889707100002));
#176708=CARTESIAN_POINT('Ctrl Pts',(8.84702676399994,11.6,-5.91889707100002));
#176709=CARTESIAN_POINT('Ctrl Pts',(8.84551680199994,15.2,-5.91724518500002));
#176710=CARTESIAN_POINT('Ctrl Pts',(8.84551680199994,11.6,-5.91724518500002));
#176711=CARTESIAN_POINT('Ctrl Pts',(8.84400984899994,15.2,-5.91559951100002));
#176712=CARTESIAN_POINT('Ctrl Pts',(8.84400984899994,11.6,-5.91559951100002));
#176713=CARTESIAN_POINT('Ctrl Pts',(8.84250591999994,15.2,-5.91396005000002));
#176714=CARTESIAN_POINT('Ctrl Pts',(8.84250591999994,11.6,-5.91396005000002));
#176715=CARTESIAN_POINT('Ctrl Pts',(8.84100503499995,15.2,-5.91232680500001));
#176716=CARTESIAN_POINT('Ctrl Pts',(8.84100503499995,11.6,-5.91232680500001));
#176717=CARTESIAN_POINT('Ctrl Pts',(8.83950720899995,15.2,-5.91069977900001));
#176718=CARTESIAN_POINT('Ctrl Pts',(8.83950720899995,11.6,-5.91069977900001));
#176719=CARTESIAN_POINT('Ctrl Pts',(8.83801245899994,15.2,-5.90907897500001));
#176720=CARTESIAN_POINT('Ctrl Pts',(8.83801245899994,11.6,-5.90907897500001));
#176721=CARTESIAN_POINT('Ctrl Pts',(8.83652080299994,15.2,-5.90746439700002));
#176722=CARTESIAN_POINT('Ctrl Pts',(8.83652080299994,11.6,-5.90746439700002));
#176723=CARTESIAN_POINT('Ctrl Pts',(8.83503225599994,15.2,-5.90585604700002));
#176724=CARTESIAN_POINT('Ctrl Pts',(8.83503225599994,11.6,-5.90585604700002));
#176725=CARTESIAN_POINT('Ctrl Pts',(8.83354683899995,15.2,-5.90425392800002));
#176726=CARTESIAN_POINT('Ctrl Pts',(8.83354683899995,11.6,-5.90425392800002));
#176727=CARTESIAN_POINT('Ctrl Pts',(8.83206456499994,15.2,-5.90265804300002));
#176728=CARTESIAN_POINT('Ctrl Pts',(8.83206456499994,11.6,-5.90265804300002));
#176729=CARTESIAN_POINT('Ctrl Pts',(8.83058545399994,15.2,-5.90106839600002));
#176730=CARTESIAN_POINT('Ctrl Pts',(8.83058545399994,11.6,-5.90106839600002));
#176731=CARTESIAN_POINT('Ctrl Pts',(8.82910952299994,15.2,-5.89948498800001));
#176732=CARTESIAN_POINT('Ctrl Pts',(8.82910952299994,11.6,-5.89948498800001));
#176733=CARTESIAN_POINT('Ctrl Pts',(8.82763678999994,15.2,-5.89790782400001));
#176734=CARTESIAN_POINT('Ctrl Pts',(8.82763678999994,11.6,-5.89790782400001));
#176735=CARTESIAN_POINT('Ctrl Pts',(8.82616726999995,15.2,-5.89633690700002));
#176736=CARTESIAN_POINT('Ctrl Pts',(8.82616726999995,11.6,-5.89633690700002));
#176737=CARTESIAN_POINT('Ctrl Pts',(8.82470098299994,15.2,-5.89477223700002));
#176738=CARTESIAN_POINT('Ctrl Pts',(8.82470098299994,11.6,-5.89477223700002));
#176739=CARTESIAN_POINT('Ctrl Pts',(8.82323794599994,15.2,-5.89321382000002));
#176740=CARTESIAN_POINT('Ctrl Pts',(8.82323794599994,11.6,-5.89321382000002));
#176741=CARTESIAN_POINT('Ctrl Pts',(8.82177817599995,15.2,-5.89166165800002));
#176742=CARTESIAN_POINT('Ctrl Pts',(8.82177817599995,11.6,-5.89166165800002));
#176743=CARTESIAN_POINT('Ctrl Pts',(8.82032169199995,15.2,-5.89011575500002));
#176744=CARTESIAN_POINT('Ctrl Pts',(8.82032169199995,11.6,-5.89011575500002));
#176745=CARTESIAN_POINT('Ctrl Pts',(8.81886850899994,15.2,-5.88857611200002));
#176746=CARTESIAN_POINT('Ctrl Pts',(8.81886850899994,11.6,-5.88857611200002));
#176747=CARTESIAN_POINT('Ctrl Pts',(8.81741864799995,15.2,-5.88704273300002));
#176748=CARTESIAN_POINT('Ctrl Pts',(8.81741864799995,11.6,-5.88704273300002));
#176749=CARTESIAN_POINT('Ctrl Pts',(8.81597212499994,15.2,-5.88551562100001));
#176750=CARTESIAN_POINT('Ctrl Pts',(8.81597212499994,11.6,-5.88551562100001));
#176751=CARTESIAN_POINT('Ctrl Pts',(8.81452895999994,15.2,-5.88399477900002));
#176752=CARTESIAN_POINT('Ctrl Pts',(8.81452895999994,11.6,-5.88399477900002));
#176753=CARTESIAN_POINT('Ctrl Pts',(8.81308916799994,15.2,-5.88248021000001));
#176754=CARTESIAN_POINT('Ctrl Pts',(8.81308916799994,11.6,-5.88248021000001));
#176755=CARTESIAN_POINT('Ctrl Pts',(8.81165276999995,15.2,-5.88097191600002));
#176756=CARTESIAN_POINT('Ctrl Pts',(8.81165276999995,11.6,-5.88097191600002));
#176757=CARTESIAN_POINT('Ctrl Pts',(8.81021978099995,15.2,-5.87946990100002));
#176758=CARTESIAN_POINT('Ctrl Pts',(8.81021978099995,11.6,-5.87946990100002));
#176759=CARTESIAN_POINT('Ctrl Pts',(8.80879022299995,15.2,-5.87797416800001));
#176760=CARTESIAN_POINT('Ctrl Pts',(8.80879022299995,11.6,-5.87797416800001));
#176761=CARTESIAN_POINT('Ctrl Pts',(8.80736410999994,15.2,-5.87648472000001));
#176762=CARTESIAN_POINT('Ctrl Pts',(8.80736410999994,11.6,-5.87648472000001));
#176763=CARTESIAN_POINT('Ctrl Pts',(8.80594146399994,15.2,-5.87500155900001));
#176764=CARTESIAN_POINT('Ctrl Pts',(8.80594146399994,11.6,-5.87500155900001));
#176765=CARTESIAN_POINT('Ctrl Pts',(8.80452230199994,15.2,-5.87352468900002));
#176766=CARTESIAN_POINT('Ctrl Pts',(8.80452230199994,11.6,-5.87352468900002));
#176767=CARTESIAN_POINT('Ctrl Pts',(8.80310664299994,15.2,-5.87205411200002));
#176768=CARTESIAN_POINT('Ctrl Pts',(8.80310664299994,11.6,-5.87205411200002));
#176769=CARTESIAN_POINT('Ctrl Pts',(8.80169450299995,15.2,-5.87058983100002));
#176770=CARTESIAN_POINT('Ctrl Pts',(8.80169450299995,11.6,-5.87058983100002));
#176771=CARTESIAN_POINT('Ctrl Pts',(8.80028590299995,15.2,-5.86913185100002));
#176772=CARTESIAN_POINT('Ctrl Pts',(8.80028590299995,11.6,-5.86913185100002));
#176773=CARTESIAN_POINT('Ctrl Pts',(8.79888086099994,15.2,-5.86768017200002));
#176774=CARTESIAN_POINT('Ctrl Pts',(8.79888086099994,11.6,-5.86768017200002));
#176775=CARTESIAN_POINT('Ctrl Pts',(8.79747939599994,15.2,-5.86623479800001));
#176776=CARTESIAN_POINT('Ctrl Pts',(8.79747939599994,11.6,-5.86623479800001));
#176777=CARTESIAN_POINT('Ctrl Pts',(8.79608152699995,15.2,-5.86479573300001));
#176778=CARTESIAN_POINT('Ctrl Pts',(8.79608152699995,11.6,-5.86479573300001));
#176779=CARTESIAN_POINT('Ctrl Pts',(8.79468727199994,15.2,-5.86336297900001));
#176780=CARTESIAN_POINT('Ctrl Pts',(8.79468727199994,11.6,-5.86336297900001));
#176781=CARTESIAN_POINT('Ctrl Pts',(8.79329664999995,15.2,-5.86193653900001));
#176782=CARTESIAN_POINT('Ctrl Pts',(8.79329664999995,11.6,-5.86193653900001));
#176783=CARTESIAN_POINT('Ctrl Pts',(8.79190967899994,15.2,-5.86051641600001));
#176784=CARTESIAN_POINT('Ctrl Pts',(8.79190967899994,11.6,-5.86051641600001));
#176785=CARTESIAN_POINT('Ctrl Pts',(8.79052638099994,15.2,-5.85910261200001));
#176786=CARTESIAN_POINT('Ctrl Pts',(8.79052638099994,11.6,-5.85910261200001));
#176787=CARTESIAN_POINT('Ctrl Pts',(8.78914677299995,15.2,-5.85769513200002));
#176788=CARTESIAN_POINT('Ctrl Pts',(8.78914677299995,11.6,-5.85769513200002));
#176789=CARTESIAN_POINT('Ctrl Pts',(8.78777087299994,15.2,-5.85629397800002));
#176790=CARTESIAN_POINT('Ctrl Pts',(8.78777087299994,11.6,-5.85629397800002));
#176791=CARTESIAN_POINT('Ctrl Pts',(8.78639870199994,15.2,-5.85489915100001));
#176792=CARTESIAN_POINT('Ctrl Pts',(8.78639870199994,11.6,-5.85489915100001));
#176793=CARTESIAN_POINT('Ctrl Pts',(8.78503027999994,15.2,-5.85351065700002));
#176794=CARTESIAN_POINT('Ctrl Pts',(8.78503027999994,11.6,-5.85351065700002));
#176795=CARTESIAN_POINT('Ctrl Pts',(8.78366562499994,15.2,-5.85212849700002));
#176796=CARTESIAN_POINT('Ctrl Pts',(8.78366562499994,11.6,-5.85212849700002));
#176797=CARTESIAN_POINT('Ctrl Pts',(8.78230475599995,15.2,-5.85075267500001));
#176798=CARTESIAN_POINT('Ctrl Pts',(8.78230475599995,11.6,-5.85075267500001));
#176799=CARTESIAN_POINT('Ctrl Pts',(8.78094769299994,15.2,-5.84938319200001));
#176800=CARTESIAN_POINT('Ctrl Pts',(8.78094769299994,11.6,-5.84938319200001));
#176801=CARTESIAN_POINT('Ctrl Pts',(8.77959445599994,15.2,-5.84802005300002));
#176802=CARTESIAN_POINT('Ctrl Pts',(8.77959445599994,11.6,-5.84802005300002));
#176803=CARTESIAN_POINT('Ctrl Pts',(8.77824506399994,15.2,-5.84666326000002));
#176804=CARTESIAN_POINT('Ctrl Pts',(8.77824506399994,11.6,-5.84666326000002));
#176805=CARTESIAN_POINT('Ctrl Pts',(8.77689953799995,15.2,-5.84531281600002));
#176806=CARTESIAN_POINT('Ctrl Pts',(8.77689953799995,11.6,-5.84531281600002));
#176807=CARTESIAN_POINT('Ctrl Pts',(8.77555789499995,15.2,-5.84396872400001));
#176808=CARTESIAN_POINT('Ctrl Pts',(8.77555789499995,11.6,-5.84396872400001));
#176809=CARTESIAN_POINT('Ctrl Pts',(8.77422015899995,15.2,-5.84263098700001));
#176810=CARTESIAN_POINT('Ctrl Pts',(8.77422015899995,11.6,-5.84263098700001));
#176811=CARTESIAN_POINT('Ctrl Pts',(8.77288634599994,15.2,-5.84129960800002));
#176812=CARTESIAN_POINT('Ctrl Pts',(8.77288634599994,11.6,-5.84129960800002));
#176813=CARTESIAN_POINT('Ctrl Pts',(8.77155647799994,15.2,-5.83997458900001));
#176814=CARTESIAN_POINT('Ctrl Pts',(8.77155647799994,11.6,-5.83997458900001));
#176815=CARTESIAN_POINT('Ctrl Pts',(8.77023057299994,15.2,-5.83865593400001));
#176816=CARTESIAN_POINT('Ctrl Pts',(8.77023057299994,11.6,-5.83865593400001));
#176817=CARTESIAN_POINT('Ctrl Pts',(8.76890865499995,15.2,-5.83734364500001));
#176818=CARTESIAN_POINT('Ctrl Pts',(8.76890865499995,11.6,-5.83734364500001));
#176819=CARTESIAN_POINT('Ctrl Pts',(8.76759074099994,15.2,-5.83603772600001));
#176820=CARTESIAN_POINT('Ctrl Pts',(8.76759074099994,11.6,-5.83603772600001));
#176821=CARTESIAN_POINT('Ctrl Pts',(8.76627685199994,15.2,-5.83473817900002));
#176822=CARTESIAN_POINT('Ctrl Pts',(8.76627685199994,11.6,-5.83473817900002));
#176823=CARTESIAN_POINT('Ctrl Pts',(8.76496700799994,15.2,-5.83344500600001));
#176824=CARTESIAN_POINT('Ctrl Pts',(8.76496700799994,11.6,-5.83344500600001));
#176825=CARTESIAN_POINT('Ctrl Pts',(8.76366123099995,15.2,-5.83215821200002));
#176826=CARTESIAN_POINT('Ctrl Pts',(8.76366123099995,11.6,-5.83215821200002));
#176827=CARTESIAN_POINT('Ctrl Pts',(8.76235953899995,15.2,-5.83087780000002));
#176828=CARTESIAN_POINT('Ctrl Pts',(8.76235953899995,11.6,-5.83087780000002));
#176829=CARTESIAN_POINT('Ctrl Pts',(8.76106195499995,15.2,-5.82960377000001));
#176830=CARTESIAN_POINT('Ctrl Pts',(8.76106195499995,11.6,-5.82960377000001));
#176831=CARTESIAN_POINT('Ctrl Pts',(8.75976849799994,15.2,-5.82833612700002));
#176832=CARTESIAN_POINT('Ctrl Pts',(8.75976849799994,11.6,-5.82833612700002));
#176833=CARTESIAN_POINT('Ctrl Pts',(8.75847918999994,15.2,-5.82707487400001));
#176834=CARTESIAN_POINT('Ctrl Pts',(8.75847918999994,11.6,-5.82707487400001));
#176835=CARTESIAN_POINT('Ctrl Pts',(8.75719405099994,15.2,-5.82582001200001));
#176836=CARTESIAN_POINT('Ctrl Pts',(8.75719405099994,11.6,-5.82582001200001));
#176837=CARTESIAN_POINT('Ctrl Pts',(8.75591310099994,15.2,-5.82457154700001));
#176838=CARTESIAN_POINT('Ctrl Pts',(8.75591310099994,11.6,-5.82457154700001));
#176839=CARTESIAN_POINT('Ctrl Pts',(8.75463636299994,15.2,-5.82332947900002));
#176840=CARTESIAN_POINT('Ctrl Pts',(8.75463636299994,11.6,-5.82332947900002));
#176841=CARTESIAN_POINT('Ctrl Pts',(8.75336385699995,15.2,-5.82209381200002));
#176842=CARTESIAN_POINT('Ctrl Pts',(8.75336385699995,11.6,-5.82209381200002));
#176843=CARTESIAN_POINT('Ctrl Pts',(8.75209560399994,15.2,-5.82086454900002));
#176844=CARTESIAN_POINT('Ctrl Pts',(8.75209560399994,11.6,-5.82086454900002));
#176845=CARTESIAN_POINT('Ctrl Pts',(8.75083162399994,15.2,-5.81964169300001));
#176846=CARTESIAN_POINT('Ctrl Pts',(8.75083162399994,11.6,-5.81964169300001));
#176847=CARTESIAN_POINT('Ctrl Pts',(8.74957194099995,15.2,-5.81842524600001));
#176848=CARTESIAN_POINT('Ctrl Pts',(8.74957194099995,11.6,-5.81842524600001));
#176849=CARTESIAN_POINT('Ctrl Pts',(8.74831657499995,15.2,-5.81721521200001));
#176850=CARTESIAN_POINT('Ctrl Pts',(8.74831657499995,11.6,-5.81721521200001));
#176851=CARTESIAN_POINT('Ctrl Pts',(8.74706554699994,15.2,-5.81601159300002));
#176852=CARTESIAN_POINT('Ctrl Pts',(8.74706554699994,11.6,-5.81601159300002));
#176853=CARTESIAN_POINT('Ctrl Pts',(8.74581887699994,15.2,-5.81481439200001));
#176854=CARTESIAN_POINT('Ctrl Pts',(8.74581887699994,11.6,-5.81481439200001));
#176855=CARTESIAN_POINT('Ctrl Pts',(8.74457659099994,15.2,-5.81362361200001));
#176856=CARTESIAN_POINT('Ctrl Pts',(8.74457659099994,11.6,-5.81362361200001));
#176857=CARTESIAN_POINT('Ctrl Pts',(8.74333870599994,15.2,-5.81243925600001));
#176858=CARTESIAN_POINT('Ctrl Pts',(8.74333870599994,11.6,-5.81243925600001));
#176859=CARTESIAN_POINT('Ctrl Pts',(8.74210524799994,15.2,-5.81126132700001));
#176860=CARTESIAN_POINT('Ctrl Pts',(8.74210524799994,11.6,-5.81126132700001));
#176861=CARTESIAN_POINT('Ctrl Pts',(8.74087623499994,15.2,-5.81008982700002));
#176862=CARTESIAN_POINT('Ctrl Pts',(8.74087623499994,11.6,-5.81008982700002));
#176863=CARTESIAN_POINT('Ctrl Pts',(8.73965169199994,15.2,-5.80892476100002));
#176864=CARTESIAN_POINT('Ctrl Pts',(8.73965169199994,11.6,-5.80892476100002));
#176865=CARTESIAN_POINT('Ctrl Pts',(8.73843163899994,15.2,-5.80776612800002));
#176866=CARTESIAN_POINT('Ctrl Pts',(8.73843163899994,11.6,-5.80776612800002));
#176867=CARTESIAN_POINT('Ctrl Pts',(8.73721609799994,15.2,-5.80661393400002));
#176868=CARTESIAN_POINT('Ctrl Pts',(8.73721609799994,11.6,-5.80661393400002));
#176869=CARTESIAN_POINT('Ctrl Pts',(8.73600509299994,15.2,-5.80546818100002));
#176870=CARTESIAN_POINT('Ctrl Pts',(8.73600509299994,11.6,-5.80546818100002));
#176871=CARTESIAN_POINT('Ctrl Pts',(8.73479864499994,15.2,-5.80432887100002));
#176872=CARTESIAN_POINT('Ctrl Pts',(8.73479864499994,11.6,-5.80432887100002));
#176873=CARTESIAN_POINT('Ctrl Pts',(8.73359677499994,15.2,-5.80319600900002));
#176874=CARTESIAN_POINT('Ctrl Pts',(8.73359677499994,11.6,-5.80319600900002));
#176875=CARTESIAN_POINT('Ctrl Pts',(8.73239950899995,15.2,-5.80206959500002));
#176876=CARTESIAN_POINT('Ctrl Pts',(8.73239950899995,11.6,-5.80206959500002));
#176877=CARTESIAN_POINT('Ctrl Pts',(8.73120686699994,15.2,-5.80094963400001));
#176878=CARTESIAN_POINT('Ctrl Pts',(8.73120686699994,11.6,-5.80094963400001));
#176879=CARTESIAN_POINT('Ctrl Pts',(8.73001887199995,15.2,-5.79983612900002));
#176880=CARTESIAN_POINT('Ctrl Pts',(8.73001887199995,11.6,-5.79983612900002));
#176881=CARTESIAN_POINT('Ctrl Pts',(8.72883554599994,15.2,-5.79872908100001));
#176882=CARTESIAN_POINT('Ctrl Pts',(8.72883554599994,11.6,-5.79872908100001));
#176883=CARTESIAN_POINT('Ctrl Pts',(8.72765691199995,15.2,-5.79762849300002));
#176884=CARTESIAN_POINT('Ctrl Pts',(8.72765691199995,11.6,-5.79762849300002));
#176885=CARTESIAN_POINT('Ctrl Pts',(8.72648299499994,15.2,-5.79653436900001));
#176886=CARTESIAN_POINT('Ctrl Pts',(8.72648299499994,11.6,-5.79653436900001));
#176887=CARTESIAN_POINT('Ctrl Pts',(8.72531381599994,15.2,-5.79544671200001));
#176888=CARTESIAN_POINT('Ctrl Pts',(8.72531381599994,11.6,-5.79544671200001));
#176889=CARTESIAN_POINT('Ctrl Pts',(8.72414939899994,15.2,-5.79436552400002));
#176890=CARTESIAN_POINT('Ctrl Pts',(8.72414939899994,11.6,-5.79436552400002));
#176891=CARTESIAN_POINT('Ctrl Pts',(8.72298976599994,15.2,-5.79329080700001));
#176892=CARTESIAN_POINT('Ctrl Pts',(8.72298976599994,11.6,-5.79329080700001));
#176893=CARTESIAN_POINT('Ctrl Pts',(8.72183494099994,15.2,-5.79222256600002));
#176894=CARTESIAN_POINT('Ctrl Pts',(8.72183494099994,11.6,-5.79222256600002));
#176895=CARTESIAN_POINT('Ctrl Pts',(8.72068494799995,15.2,-5.79116080200002));
#176896=CARTESIAN_POINT('Ctrl Pts',(8.72068494799995,11.6,-5.79116080200002));
#176897=CARTESIAN_POINT('Ctrl Pts',(8.71953980799994,15.2,-5.79010551900002));
#176898=CARTESIAN_POINT('Ctrl Pts',(8.71953980799994,11.6,-5.79010551900002));
#176899=CARTESIAN_POINT('Ctrl Pts',(8.71839954799994,15.2,-5.78905671900002));
#176900=CARTESIAN_POINT('Ctrl Pts',(8.71839954799994,11.6,-5.78905671900002));
#176901=CARTESIAN_POINT('Ctrl Pts',(8.71726418899994,15.2,-5.78801440500002));
#176902=CARTESIAN_POINT('Ctrl Pts',(8.71726418899994,11.6,-5.78801440500002));
#176903=CARTESIAN_POINT('Ctrl Pts',(8.71613375599994,15.2,-5.78697858000002));
#176904=CARTESIAN_POINT('Ctrl Pts',(8.71613375599994,11.6,-5.78697858000002));
#176905=CARTESIAN_POINT('Ctrl Pts',(8.71500827199995,15.2,-5.78594924700001));
#176906=CARTESIAN_POINT('Ctrl Pts',(8.71500827199995,11.6,-5.78594924700001));
#176907=CARTESIAN_POINT('Ctrl Pts',(8.71388776199994,15.2,-5.78492640800001));
#176908=CARTESIAN_POINT('Ctrl Pts',(8.71388776199994,11.6,-5.78492640800001));
#176909=CARTESIAN_POINT('Ctrl Pts',(8.71277224899995,15.2,-5.78391006700001));
#176910=CARTESIAN_POINT('Ctrl Pts',(8.71277224899995,11.6,-5.78391006700001));
#176911=CARTESIAN_POINT('Ctrl Pts',(8.71166175799994,15.2,-5.78290022500001));
#176912=CARTESIAN_POINT('Ctrl Pts',(8.71166175799994,11.6,-5.78290022500001));
#176913=CARTESIAN_POINT('Ctrl Pts',(8.71055631199994,15.2,-5.78189688600002));
#176914=CARTESIAN_POINT('Ctrl Pts',(8.71055631199994,11.6,-5.78189688600002));
#176915=CARTESIAN_POINT('Ctrl Pts',(8.70945593699994,15.2,-5.78090005400002));
#176916=CARTESIAN_POINT('Ctrl Pts',(8.70945593699994,11.6,-5.78090005400002));
#176917=CARTESIAN_POINT('Ctrl Pts',(8.70836065599994,15.2,-5.77990973000002));
#176918=CARTESIAN_POINT('Ctrl Pts',(8.70836065599994,11.6,-5.77990973000002));
#176919=CARTESIAN_POINT('Ctrl Pts',(8.70727049299994,15.2,-5.77892591600002));
#176920=CARTESIAN_POINT('Ctrl Pts',(8.70727049299994,11.6,-5.77892591600002));
#176921=CARTESIAN_POINT('Ctrl Pts',(8.70618547399994,15.2,-5.77794861800002));
#176922=CARTESIAN_POINT('Ctrl Pts',(8.70618547399994,11.6,-5.77794861800002));
#176923=CARTESIAN_POINT('Ctrl Pts',(8.70510562399994,15.2,-5.77697783500002));
#176924=CARTESIAN_POINT('Ctrl Pts',(8.70510562399994,11.6,-5.77697783500002));
#176925=CARTESIAN_POINT('Ctrl Pts',(8.70403096699994,15.2,-5.77601357300002));
#176926=CARTESIAN_POINT('Ctrl Pts',(8.70403096699994,11.6,-5.77601357300002));
#176927=CARTESIAN_POINT('Ctrl Pts',(8.70296152799994,15.2,-5.77505583400002));
#176928=CARTESIAN_POINT('Ctrl Pts',(8.70296152799994,11.6,-5.77505583400002));
#176929=CARTESIAN_POINT('Ctrl Pts',(8.70189733199994,15.2,-5.77410461900002));
#176930=CARTESIAN_POINT('Ctrl Pts',(8.70189733199994,11.6,-5.77410461900002));
#176931=CARTESIAN_POINT('Ctrl Pts',(8.70083840399994,15.2,-5.77315993200001));
#176932=CARTESIAN_POINT('Ctrl Pts',(8.70083840399994,11.6,-5.77315993200001));
#176933=CARTESIAN_POINT('Ctrl Pts',(8.69978476999994,15.2,-5.77222177600002));
#176934=CARTESIAN_POINT('Ctrl Pts',(8.69978476999994,11.6,-5.77222177600002));
#176935=CARTESIAN_POINT('Ctrl Pts',(8.69873645399995,15.2,-5.77129015300001));
#176936=CARTESIAN_POINT('Ctrl Pts',(8.69873645399995,11.6,-5.77129015300001));
#176937=CARTESIAN_POINT('Ctrl Pts',(8.69769348299995,15.2,-5.77036506700002));
#176938=CARTESIAN_POINT('Ctrl Pts',(8.69769348299995,11.6,-5.77036506700002));
#176939=CARTESIAN_POINT('Ctrl Pts',(8.69665588299994,15.2,-5.76944652000002));
#176940=CARTESIAN_POINT('Ctrl Pts',(8.69665588299994,11.6,-5.76944652000002));
#176941=CARTESIAN_POINT('Ctrl Pts',(8.69562367699995,15.2,-5.76853451600002));
#176942=CARTESIAN_POINT('Ctrl Pts',(8.69562367699995,11.6,-5.76853451600002));
#176943=CARTESIAN_POINT('Ctrl Pts',(8.69459689299994,15.2,-5.76762905500001));
#176944=CARTESIAN_POINT('Ctrl Pts',(8.69459689299994,11.6,-5.76762905500001));
#176945=CARTESIAN_POINT('Ctrl Pts',(8.69357555699995,15.2,-5.76673014200002));
#176946=CARTESIAN_POINT('Ctrl Pts',(8.69357555699995,11.6,-5.76673014200002));
#176947=CARTESIAN_POINT('Ctrl Pts',(8.69255969299994,15.2,-5.76583777900002));
#176948=CARTESIAN_POINT('Ctrl Pts',(8.69255969299994,11.6,-5.76583777900002));
#176949=CARTESIAN_POINT('Ctrl Pts',(8.69154932899994,15.2,-5.76495197000002));
#176950=CARTESIAN_POINT('Ctrl Pts',(8.69154932899994,11.6,-5.76495197000002));
#176951=CARTESIAN_POINT('Ctrl Pts',(8.69054449099995,15.2,-5.76407271500001));
#176952=CARTESIAN_POINT('Ctrl Pts',(8.69054449099995,11.6,-5.76407271500001));
#176953=CARTESIAN_POINT('Ctrl Pts',(8.68954520599994,15.2,-5.76320002000001));
#176954=CARTESIAN_POINT('Ctrl Pts',(8.68954520599994,11.6,-5.76320002000001));
#176955=CARTESIAN_POINT('Ctrl Pts',(8.68855149799994,15.2,-5.76233388600001));
#176956=CARTESIAN_POINT('Ctrl Pts',(8.68855149799994,11.6,-5.76233388600001));
#176957=CARTESIAN_POINT('Ctrl Pts',(8.68756339599994,15.2,-5.76147431500001));
#176958=CARTESIAN_POINT('Ctrl Pts',(8.68756339599994,11.6,-5.76147431500001));
#176959=CARTESIAN_POINT('Ctrl Pts',(8.68658092499994,15.2,-5.76062131100001));
#176960=CARTESIAN_POINT('Ctrl Pts',(8.68658092499994,11.6,-5.76062131100001));
#176961=CARTESIAN_POINT('Ctrl Pts',(8.68560411399995,15.2,-5.75977487700002));
#176962=CARTESIAN_POINT('Ctrl Pts',(8.68560411399995,11.6,-5.75977487700002));
#176963=CARTESIAN_POINT('Ctrl Pts',(8.68463298799995,15.2,-5.75893501600002));
#176964=CARTESIAN_POINT('Ctrl Pts',(8.68463298799995,11.6,-5.75893501600002));
#176965=CARTESIAN_POINT('Ctrl Pts',(8.68366757599994,15.2,-5.75810172900002));
#176966=CARTESIAN_POINT('Ctrl Pts',(8.68366757599994,11.6,-5.75810172900002));
#176967=CARTESIAN_POINT('Ctrl Pts',(8.68270790299994,15.2,-5.75727502000002));
#176968=CARTESIAN_POINT('Ctrl Pts',(8.68270790299994,11.6,-5.75727502000002));
#176969=CARTESIAN_POINT('Ctrl Pts',(8.68175399699994,15.2,-5.75645489200002));
#176970=CARTESIAN_POINT('Ctrl Pts',(8.68175399699994,11.6,-5.75645489200002));
#176971=CARTESIAN_POINT('Ctrl Pts',(8.68080588599994,15.2,-5.75564134800001));
#176972=CARTESIAN_POINT('Ctrl Pts',(8.68080588599994,11.6,-5.75564134800001));
#176973=CARTESIAN_POINT('Ctrl Pts',(8.67986359699995,15.2,-5.75483438900001));
#176974=CARTESIAN_POINT('Ctrl Pts',(8.67986359699995,11.6,-5.75483438900001));
#176975=CARTESIAN_POINT('Ctrl Pts',(8.67892715799995,15.2,-5.75403401900001));
#176976=CARTESIAN_POINT('Ctrl Pts',(8.67892715799995,11.6,-5.75403401900001));
#176977=CARTESIAN_POINT('Ctrl Pts',(8.67799659699994,15.2,-5.75324024000002));
#176978=CARTESIAN_POINT('Ctrl Pts',(8.67799659699994,11.6,-5.75324024000002));
#176979=CARTESIAN_POINT('Ctrl Pts',(8.67707194199994,15.2,-5.75245305500002));
#176980=CARTESIAN_POINT('Ctrl Pts',(8.67707194199994,11.6,-5.75245305500002));
#176981=CARTESIAN_POINT('Ctrl Pts',(8.67615321999994,15.2,-5.75167246800002));
#176982=CARTESIAN_POINT('Ctrl Pts',(8.67615321999994,11.6,-5.75167246800002));
#176983=CARTESIAN_POINT('Ctrl Pts',(8.67524046199994,15.2,-5.75089848100002));
#176984=CARTESIAN_POINT('Ctrl Pts',(8.67524046199994,11.6,-5.75089848100002));
#176985=CARTESIAN_POINT('Ctrl Pts',(8.67433369199994,15.2,-5.75013109600001));
#176986=CARTESIAN_POINT('Ctrl Pts',(8.67433369199994,11.6,-5.75013109600001));
#176987=CARTESIAN_POINT('Ctrl Pts',(8.67343294199994,15.2,-5.74937031600002));
#176988=CARTESIAN_POINT('Ctrl Pts',(8.67343294199994,11.6,-5.74937031600002));
#176989=CARTESIAN_POINT('Ctrl Pts',(8.67253823899994,15.2,-5.74861614500002));
#176990=CARTESIAN_POINT('Ctrl Pts',(8.67253823899994,11.6,-5.74861614500002));
#176991=CARTESIAN_POINT('Ctrl Pts',(8.67164961199994,15.2,-5.74786858400002));
#176992=CARTESIAN_POINT('Ctrl Pts',(8.67164961199994,11.6,-5.74786858400002));
#176993=CARTESIAN_POINT('Ctrl Pts',(8.67076709099995,15.2,-5.74712763600001));
#176994=CARTESIAN_POINT('Ctrl Pts',(8.67076709099995,11.6,-5.74712763600001));
#176995=CARTESIAN_POINT('Ctrl Pts',(8.66989070299995,15.2,-5.74639330500001));
#176996=CARTESIAN_POINT('Ctrl Pts',(8.66989070299995,11.6,-5.74639330500001));
#176997=CARTESIAN_POINT('Ctrl Pts',(8.66902047899995,15.2,-5.74566559300001));
#176998=CARTESIAN_POINT('Ctrl Pts',(8.66902047899995,11.6,-5.74566559300001));
#176999=CARTESIAN_POINT('Ctrl Pts',(8.66815644699994,15.2,-5.74494450200002));
#177000=CARTESIAN_POINT('Ctrl Pts',(8.66815644699994,11.6,-5.74494450200002));
#177001=CARTESIAN_POINT('Ctrl Pts',(8.66729863599994,15.2,-5.74423003600002));
#177002=CARTESIAN_POINT('Ctrl Pts',(8.66729863599994,11.6,-5.74423003600002));
#177003=CARTESIAN_POINT('Ctrl Pts',(8.66644707699994,15.2,-5.74352219600001));
#177004=CARTESIAN_POINT('Ctrl Pts',(8.66644707699994,11.6,-5.74352219600001));
#177005=CARTESIAN_POINT('Ctrl Pts',(8.66560179899994,15.2,-5.74282098700002));
#177006=CARTESIAN_POINT('Ctrl Pts',(8.66560179899994,11.6,-5.74282098700002));
#177007=CARTESIAN_POINT('Ctrl Pts',(8.66476283199994,15.2,-5.74212641100001));
#177008=CARTESIAN_POINT('Ctrl Pts',(8.66476283199994,11.6,-5.74212641100001));
#177009=CARTESIAN_POINT('Ctrl Pts',(8.66393020599994,15.2,-5.74143847000002));
#177010=CARTESIAN_POINT('Ctrl Pts',(8.66393020599994,11.6,-5.74143847000002));
#177011=CARTESIAN_POINT('Ctrl Pts',(8.66310394999994,15.2,-5.74075716600002));
#177012=CARTESIAN_POINT('Ctrl Pts',(8.66310394999994,11.6,-5.74075716600002));
#177013=CARTESIAN_POINT('Ctrl Pts',(8.66228409599995,15.2,-5.74008250400002));
#177014=CARTESIAN_POINT('Ctrl Pts',(8.66228409599995,11.6,-5.74008250400002));
#177015=CARTESIAN_POINT('Ctrl Pts',(8.66147067299995,15.2,-5.73941448500002));
#177016=CARTESIAN_POINT('Ctrl Pts',(8.66147067299995,11.6,-5.73941448500002));
#177017=CARTESIAN_POINT('Ctrl Pts',(8.66066371399994,15.2,-5.73875311200001));
#177018=CARTESIAN_POINT('Ctrl Pts',(8.66066371399994,11.6,-5.73875311200001));
#177019=CARTESIAN_POINT('Ctrl Pts',(8.65986324599995,15.2,-5.73809838800001));
#177020=CARTESIAN_POINT('Ctrl Pts',(8.65986324599995,11.6,-5.73809838800001));
#177021=CARTESIAN_POINT('Ctrl Pts',(8.65906930199994,15.2,-5.73745031600001));
#177022=CARTESIAN_POINT('Ctrl Pts',(8.65906930199994,11.6,-5.73745031600001));
#177023=CARTESIAN_POINT('Ctrl Pts',(8.65828191299994,15.2,-5.73680889800002));
#177024=CARTESIAN_POINT('Ctrl Pts',(8.65828191299994,11.6,-5.73680889800002));
#177025=CARTESIAN_POINT('Ctrl Pts',(8.65750110999995,15.2,-5.73617413800001));
#177026=CARTESIAN_POINT('Ctrl Pts',(8.65750110999995,11.6,-5.73617413800001));
#177027=CARTESIAN_POINT('Ctrl Pts',(8.65672692399994,15.2,-5.73554603700002));
#177028=CARTESIAN_POINT('Ctrl Pts',(8.65672692399994,11.6,-5.73554603700002));
#177029=CARTESIAN_POINT('Ctrl Pts',(8.65595938699995,15.2,-5.73492459900002));
#177030=CARTESIAN_POINT('Ctrl Pts',(8.65595938699995,11.6,-5.73492459900002));
#177031=CARTESIAN_POINT('Ctrl Pts',(8.65519852999994,15.2,-5.73430982600001));
#177032=CARTESIAN_POINT('Ctrl Pts',(8.65519852999994,11.6,-5.73430982600001));
#177033=CARTESIAN_POINT('Ctrl Pts',(8.65444438599994,15.2,-5.73370172000002));
#177034=CARTESIAN_POINT('Ctrl Pts',(8.65444438599994,11.6,-5.73370172000002));
#177035=CARTESIAN_POINT('Ctrl Pts',(8.65369698499994,15.2,-5.73310028600002));
#177036=CARTESIAN_POINT('Ctrl Pts',(8.65369698499994,11.6,-5.73310028600002));
#177037=CARTESIAN_POINT('Ctrl Pts',(8.65295636099994,15.2,-5.73250552500002));
#177038=CARTESIAN_POINT('Ctrl Pts',(8.65295636099994,11.6,-5.73250552500002));
#177039=CARTESIAN_POINT('Ctrl Pts',(8.65222254499994,15.2,-5.73191744000002));
#177040=CARTESIAN_POINT('Ctrl Pts',(8.65222254499994,11.6,-5.73191744000002));
#177041=CARTESIAN_POINT('Ctrl Pts',(8.65149556899994,15.2,-5.73133603500001));
#177042=CARTESIAN_POINT('Ctrl Pts',(8.65149556899994,11.6,-5.73133603500001));
#177043=CARTESIAN_POINT('Ctrl Pts',(8.65077961599994,15.2,-5.73076462100002));
#177044=CARTESIAN_POINT('Ctrl Pts',(8.65077961599994,11.6,-5.73076462100002));
#177045=CARTESIAN_POINT('Ctrl Pts',(8.65021312699995,15.2,-5.73031342200002));
#177046=CARTESIAN_POINT('Ctrl Pts',(8.65021312699995,11.6,-5.73031342200002));
#177047=CARTESIAN_POINT('Ctrl Pts',(8.64979234999995,15.2,-5.72997879200001));
#177048=CARTESIAN_POINT('Ctrl Pts',(8.64979234999995,11.6,-5.72997879200001));
#177049=CARTESIAN_POINT('Ctrl Pts',(8.64951454399994,15.2,-5.72975808600001));
#177050=CARTESIAN_POINT('Ctrl Pts',(8.64951454399994,11.6,-5.72975808600001));
#177051=CARTESIAN_POINT('Ctrl Pts',(8.64937799899994,15.2,-5.72964966100002));
#177052=CARTESIAN_POINT('Ctrl Pts',(8.64937799899994,11.6,-5.72964966100002));
#177053=CARTESIAN_POINT('',(8.64937799799994,12.2,-5.72964966100002));
#177054=CARTESIAN_POINT('',(8.64937799799994,15.2,-5.72964966100002));
#177055=CARTESIAN_POINT('',(8.64937799799994,12.2,-5.72964966100002));
#177056=CARTESIAN_POINT('Ctrl Pts',(9.36775917477149,12.2,-6.67046385458018));
#177057=CARTESIAN_POINT('Ctrl Pts',(9.36593194451564,12.2,-6.66710588411075));
#177058=CARTESIAN_POINT('Ctrl Pts',(9.36410408859324,12.2,-6.6637557852869));
#177059=CARTESIAN_POINT('Ctrl Pts',(9.36227560146925,12.2,-6.66041356411704));
#177060=CARTESIAN_POINT('Ctrl Pts',(9.36044711426905,12.2,-6.65707134280789));
#177061=CARTESIAN_POINT('Ctrl Pts',(9.3586179987788,12.2,-6.65373699735653));
#177062=CARTESIAN_POINT('Ctrl Pts',(9.35678826937895,12.2,-6.65041053364363));
#177063=CARTESIAN_POINT('Ctrl Pts',(9.35434862995754,12.2,-6.64597524829023));
#177064=CARTESIAN_POINT('Ctrl Pts',(9.35190790041681,12.2,-6.64155397851797));
#177065=CARTESIAN_POINT('Ctrl Pts',(9.34946618061699,12.2,-6.63714676338981));
#177066=CARTESIAN_POINT('Ctrl Pts',(9.34763489093348,12.2,-6.63384135234392));
#177067=CARTESIAN_POINT('Ctrl Pts',(9.34580304503337,12.2,-6.63054384819711));
#177068=CARTESIAN_POINT('Ctrl Pts',(9.34397068726661,12.2,-6.62725426952495));
#177069=CARTESIAN_POINT('Ctrl Pts',(9.34213832949985,12.2,-6.6239646908528));
#177070=CARTESIAN_POINT('Ctrl Pts',(9.34030545849978,12.2,-6.62068303577201));
#177071=CARTESIAN_POINT('Ctrl Pts',(9.33847210923311,12.2,-6.61740932059859));
#177072=CARTESIAN_POINT('Ctrl Pts',(9.33663875996642,12.2,-6.61413560542518));
#177073=CARTESIAN_POINT('Ctrl Pts',(9.33480493264643,12.2,-6.61086982894232));
#177074=CARTESIAN_POINT('Ctrl Pts',(9.3329706613715,12.2,-6.60761200614702));
#177075=CARTESIAN_POINT('Ctrl Pts',(9.33052496611611,12.2,-6.6032682420254));
#177076=CARTESIAN_POINT('Ctrl Pts',(9.32807848310274,12.2,-6.59893861734822));
#177077=CARTESIAN_POINT('Ctrl Pts',(9.32563130602488,12.2,-6.59462317144731));
#177078=CARTESIAN_POINT('Ctrl Pts',(9.32379592338321,12.2,-6.59138658731561));
#177079=CARTESIAN_POINT('Ctrl Pts',(9.32196015166656,12.2,-6.58815797756626));
#177080=CARTESIAN_POINT('Ctrl Pts',(9.32012402748328,12.2,-6.58493735897495));
#177081=CARTESIAN_POINT('Ctrl Pts',(9.3182879033,12.2,-6.58171674038365));
#177082=CARTESIAN_POINT('Ctrl Pts',(9.3164514276334,12.2,-6.57850411301701));
#177083=CARTESIAN_POINT('Ctrl Pts',(9.31461463795015,12.2,-6.57529949138273));
#177084=CARTESIAN_POINT('Ctrl Pts',(9.3127778482669,12.2,-6.57209486974845));
#177085=CARTESIAN_POINT('Ctrl Pts',(9.31094074536376,12.2,-6.56889825344464));
#177086=CARTESIAN_POINT('Ctrl Pts',(9.30910336658877,12.2,-6.56570965960862));
#177087=CARTESIAN_POINT('Ctrl Pts',(9.30726598781377,12.2,-6.5625210657726));
#177088=CARTESIAN_POINT('Ctrl Pts',(9.30542833415045,12.2,-6.55934049282739));
#177089=CARTESIAN_POINT('Ctrl Pts',(9.30359044492561,12.2,-6.55616795719158));
#177090=CARTESIAN_POINT('Ctrl Pts',(9.30175255536688,12.2,-6.55299542097943));
#177091=CARTESIAN_POINT('Ctrl Pts',(9.29991442963305,12.2,-6.54983092153616));
#177092=CARTESIAN_POINT('Ctrl Pts',(9.29807610807419,12.2,-6.54667447532853));
#177093=CARTESIAN_POINT('Ctrl Pts',(9.29623778684929,12.2,-6.54351802969431));
#177094=CARTESIAN_POINT('Ctrl Pts',(9.29439926901607,12.2,-6.54036963617634));
#177095=CARTESIAN_POINT('Ctrl Pts',(9.29256059479119,12.2,-6.53722931062446));
#177096=CARTESIAN_POINT('Ctrl Pts',(9.29072192056631,12.2,-6.53408898507259));
#177097=CARTESIAN_POINT('Ctrl Pts',(9.28888308963982,12.2,-6.53095672834776));
#177098=CARTESIAN_POINT('Ctrl Pts',(9.28704414048994,12.2,-6.52783255423879));
#177099=CARTESIAN_POINT('Ctrl Pts',(9.28520519134007,12.2,-6.52470838012981));
#177100=CARTESIAN_POINT('Ctrl Pts',(9.28336612552649,12.2,-6.52159228863737));
#177101=CARTESIAN_POINT('Ctrl Pts',(9.28152698279328,12.2,-6.51848429698611));
#177102=CARTESIAN_POINT('Ctrl Pts',(9.27968784006007,12.2,-6.51537630533485));
#177103=CARTESIAN_POINT('Ctrl Pts',(9.27784861965025,12.2,-6.51227641245879));
#177104=CARTESIAN_POINT('Ctrl Pts',(9.27600936296709,12.2,-6.50918463382044));
#177105=CARTESIAN_POINT('Ctrl Pts',(9.27417010628393,12.2,-6.50609285518209));
#177106=CARTESIAN_POINT('Ctrl Pts',(9.27233081336741,12.2,-6.50300919034312));
#177107=CARTESIAN_POINT('Ctrl Pts',(9.27049152368424,12.2,-6.4999336556621));
#177108=CARTESIAN_POINT('Ctrl Pts',(9.26865223366693,12.2,-6.49685812042235));
#177109=CARTESIAN_POINT('Ctrl Pts',(9.26681294661628,12.2,-6.49379071430988));
#177110=CARTESIAN_POINT('Ctrl Pts',(9.26497370509899,12.2,-6.49073145361638));
#177111=CARTESIAN_POINT('Ctrl Pts',(9.26313446391583,12.2,-6.48767219347865));
#177112=CARTESIAN_POINT('Ctrl Pts',(9.26129526689933,12.2,-6.48462107830714));
#177113=CARTESIAN_POINT('Ctrl Pts',(9.25945615571615,12.2,-6.48157812366841));
#177114=CARTESIAN_POINT('Ctrl Pts',(9.25761704453297,12.2,-6.47853516902967));
#177115=CARTESIAN_POINT('Ctrl Pts',(9.25577801897314,12.2,-6.47550037416762));
#177116=CARTESIAN_POINT('Ctrl Pts',(9.25393912023994,12.2,-6.47247375551388));
#177117=CARTESIAN_POINT('Ctrl Pts',(9.25210022150674,12.2,-6.46944713686013));
#177118=CARTESIAN_POINT('Ctrl Pts',(9.25026144900983,12.2,-6.46642869284037));
#177119=CARTESIAN_POINT('Ctrl Pts',(9.24842284623495,12.2,-6.46341844068603));
#177120=CARTESIAN_POINT('Ctrl Pts',(9.24658424346006,12.2,-6.46040818853168));
#177121=CARTESIAN_POINT('Ctrl Pts',(9.24474580843353,12.2,-6.45740612773502));
#177122=CARTESIAN_POINT('Ctrl Pts',(9.24290758420865,12.2,-6.45441227263476));
#177123=CARTESIAN_POINT('Ctrl Pts',(9.24045661835284,12.2,-6.45042046547183));
#177124=CARTESIAN_POINT('Ctrl Pts',(9.23800602642203,12.2,-6.44644324800782));
#177125=CARTESIAN_POINT('Ctrl Pts',(9.23555590806632,12.2,-6.44248065545949));
#177126=CARTESIAN_POINT('Ctrl Pts',(9.23371831946645,12.2,-6.43950871131819));
#177127=CARTESIAN_POINT('Ctrl Pts',(9.23188099760653,12.2,-6.4365449925866));
#177128=CARTESIAN_POINT('Ctrl Pts',(9.23004398449828,12.2,-6.43358951697227));
#177129=CARTESIAN_POINT('Ctrl Pts',(9.22820697139002,12.2,-6.43063404135795));
#177130=CARTESIAN_POINT('Ctrl Pts',(9.22637026742656,12.2,-6.42768680775923));
#177131=CARTESIAN_POINT('Ctrl Pts',(9.22453391573494,12.2,-6.42474783068596));
#177132=CARTESIAN_POINT('Ctrl Pts',(9.22269756404333,12.2,-6.4218088536127));
#177133=CARTESIAN_POINT('Ctrl Pts',(9.2208615633667,12.2,-6.41887813421319));
#177134=CARTESIAN_POINT('Ctrl Pts',(9.21902595818336,12.2,-6.41595568706864));
#177135=CARTESIAN_POINT('Ctrl Pts',(9.21657848438326,12.2,-6.41205909052198));
#177136=CARTESIAN_POINT('Ctrl Pts',(9.21413171143324,12.2,-6.4081772008993));
#177137=CARTESIAN_POINT('Ctrl Pts',(9.21168574429999,12.2,-6.40431005313396));
#177138=CARTESIAN_POINT('Ctrl Pts',(9.20985126911668,12.2,-6.4014096925734));
#177139=CARTESIAN_POINT('Ctrl Pts',(9.20801724635665,12.2,-6.39851762520561));
#177140=CARTESIAN_POINT('Ctrl Pts',(9.20618371974827,12.2,-6.39563386550567));
#177141=CARTESIAN_POINT('Ctrl Pts',(9.20435019313991,12.2,-6.39275010580573));
#177142=CARTESIAN_POINT('Ctrl Pts',(9.20251716287668,12.2,-6.38987465241145));
#177143=CARTESIAN_POINT('Ctrl Pts',(9.2006846732266,12.2,-6.38700752325256));
#177144=CARTESIAN_POINT('Ctrl Pts',(9.19885218357653,12.2,-6.38414039409368));
#177145=CARTESIAN_POINT('Ctrl Pts',(9.19702023376641,12.2,-6.38128158839129));
#177146=CARTESIAN_POINT('Ctrl Pts',(9.1951888687079,12.2,-6.37843111982747));
#177147=CARTESIAN_POINT('Ctrl Pts',(9.1933575036494,12.2,-6.37558065126365));
#177148=CARTESIAN_POINT('Ctrl Pts',(9.19152672411584,12.2,-6.37273852131591));
#177149=CARTESIAN_POINT('Ctrl Pts',(9.18969657259892,12.2,-6.36990474462607));
#177150=CARTESIAN_POINT('Ctrl Pts',(9.18786642074951,12.2,-6.36707096742142));
#177151=CARTESIAN_POINT('Ctrl Pts',(9.18603689851695,12.2,-6.36424554219412));
#177152=CARTESIAN_POINT('Ctrl Pts',(9.18420805008458,12.2,-6.36142848691084));
#177153=CARTESIAN_POINT('Ctrl Pts',(9.18237920198445,12.2,-6.35861143213933));
#177154=CARTESIAN_POINT('Ctrl Pts',(9.18055102833788,12.2,-6.35580274404545));
#177155=CARTESIAN_POINT('Ctrl Pts',(9.17872357318804,12.2,-6.35300244071658));
#177156=CARTESIAN_POINT('Ctrl Pts',(9.17689611803822,12.2,-6.35020213738771));
#177157=CARTESIAN_POINT('Ctrl Pts',(9.17506938258452,12.2,-6.34741021782817));
#177158=CARTESIAN_POINT('Ctrl Pts',(9.17324341106759,12.2,-6.34462669622169));
#177159=CARTESIAN_POINT('Ctrl Pts',(9.17080878248892,12.2,-6.34091533424828));
#177160=CARTESIAN_POINT('Ctrl Pts',(9.16837551464056,12.2,-6.33721890270524));
#177161=CARTESIAN_POINT('Ctrl Pts',(9.16594371333921,12.2,-6.33353743739355));
#177162=CARTESIAN_POINT('Ctrl Pts',(9.16351191170653,12.2,-6.32985597158027));
#177163=CARTESIAN_POINT('Ctrl Pts',(9.1610815784,12.2,-6.32618947176022));
#177164=CARTESIAN_POINT('Ctrl Pts',(9.15865282275661,12.2,-6.32253797448913));
#177165=CARTESIAN_POINT('Ctrl Pts',(9.15622406744414,12.2,-6.31888647771557));
#177166=CARTESIAN_POINT('Ctrl Pts',(9.15379688862335,12.2,-6.3152499817614));
#177167=CARTESIAN_POINT('Ctrl Pts',(9.15137139865484,12.2,-6.31162852433374));
#177168=CARTESIAN_POINT('Ctrl Pts',(9.14894590835584,12.2,-6.30800706641266));
#177169=CARTESIAN_POINT('Ctrl Pts',(9.14652210610415,12.2,-6.30440064520123));
#177170=CARTESIAN_POINT('Ctrl Pts',(9.14410010374994,12.2,-6.30080929678329));
#177171=CARTESIAN_POINT('Ctrl Pts',(9.14167810139572,12.2,-6.29721794836534));
#177172=CARTESIAN_POINT('Ctrl Pts',(9.13925789893337,12.2,-6.29364167321581));
#177173=CARTESIAN_POINT('Ctrl Pts',(9.13683960807955,12.2,-6.29008050613438));
#177174=CARTESIAN_POINT('Ctrl Pts',(9.13442131755522,12.2,-6.28651933953817));
#177175=CARTESIAN_POINT('Ctrl Pts',(9.13200493997352,12.2,-6.28297328152702));
#177176=CARTESIAN_POINT('Ctrl Pts',(9.12959058799325,12.2,-6.27944236674403));
#177177=CARTESIAN_POINT('Ctrl Pts',(9.12717623568403,12.2,-6.27591145147995));
#177178=CARTESIAN_POINT('Ctrl Pts',(9.12476390969812,12.2,-6.27239567950574));
#177179=CARTESIAN_POINT('Ctrl Pts',(9.12235372412254,12.2,-6.26889508642761));
#177180=CARTESIAN_POINT('Ctrl Pts',(9.11994353887535,12.2,-6.26539449382644));
#177181=CARTESIAN_POINT('Ctrl Pts',(9.11753549456399,12.2,-6.26190908019832));
#177182=CARTESIAN_POINT('Ctrl Pts',(9.11512970670496,12.2,-6.25843888075878));
#177183=CARTESIAN_POINT('Ctrl Pts',(9.11212247163533,12.2,-6.25410113110475));
#177184=CARTESIAN_POINT('Ctrl Pts',(9.10911876219854,12.2,-6.24978715336073));
#177185=CARTESIAN_POINT('Ctrl Pts',(9.1061188078099,12.2,-6.24549701549396));
#177186=CARTESIAN_POINT('Ctrl Pts',(9.10371884416819,12.2,-6.24206490501349));
#177187=CARTESIAN_POINT('Ctrl Pts',(9.10132128278861,12.2,-6.23864805254152));
#177188=CARTESIAN_POINT('Ctrl Pts',(9.09892624265835,12.2,-6.2352464939688));
#177189=CARTESIAN_POINT('Ctrl Pts',(9.0965312028544,12.2,-6.23184493585956));
#177190=CARTESIAN_POINT('Ctrl Pts',(9.09413868484457,12.2,-6.22845866894833));
#177191=CARTESIAN_POINT('Ctrl Pts',(9.09174880692867,12.2,-6.22508773150067));
#177192=CARTESIAN_POINT('Ctrl Pts',(9.08876145928956,12.2,-6.22087405934664));
#177193=CARTESIAN_POINT('Ctrl Pts',(9.08577823754842,12.2,-6.21668433514341));
#177194=CARTESIAN_POINT('Ctrl Pts',(9.08279937753489,12.2,-6.21251863123556));
#177195=CARTESIAN_POINT('Ctrl Pts',(9.08041628939419,12.2,-6.20918606792766));
#177196=CARTESIAN_POINT('Ctrl Pts',(9.07803599382661,12.2,-6.20586887534404));
#177197=CARTESIAN_POINT('Ctrl Pts',(9.07565861041957,12.2,-6.20256708894346));
#177198=CARTESIAN_POINT('Ctrl Pts',(9.07328122733644,12.2,-6.19926530299274));
#177199=CARTESIAN_POINT('Ctrl Pts',(9.07090675886684,12.2,-6.19597892428445));
#177200=CARTESIAN_POINT('Ctrl Pts',(9.06853532639383,12.2,-6.1927079862175));
#177201=CARTESIAN_POINT('Ctrl Pts',(9.06616389359771,12.2,-6.18943704770488));
#177202=CARTESIAN_POINT('Ctrl Pts',(9.06379549831308,12.2,-6.18618155116913));
#177203=CARTESIAN_POINT('Ctrl Pts',(9.06143026407328,12.2,-6.18294152949357));
#177204=CARTESIAN_POINT('Ctrl Pts',(9.05906503015573,12.2,-6.17970150825946));
#177205=CARTESIAN_POINT('Ctrl Pts',(9.05670295672863,12.2,-6.17647696359835));
#177206=CARTESIAN_POINT('Ctrl Pts',(9.05434417135889,12.2,-6.17326792869902));
#177207=CARTESIAN_POINT('Ctrl Pts',(9.05198538566777,12.2,-6.17005889336246));
#177208=CARTESIAN_POINT('Ctrl Pts',(9.04962988622175,12.2,-6.16686536822637));
#177209=CARTESIAN_POINT('Ctrl Pts',(9.04727780081601,12.2,-6.16368738899864));
#177210=CARTESIAN_POINT('Ctrl Pts',(9.04492571573076,12.2,-6.1605094102039));
#177211=CARTESIAN_POINT('Ctrl Pts',(9.04257704504476,12.2,-6.15734697499212));
#177212=CARTESIAN_POINT('Ctrl Pts',(9.04023191595836,12.2,-6.15420012024781));
#177213=CARTESIAN_POINT('Ctrl Pts',(9.03788678655243,12.2,-6.15105326507474));
#177214=CARTESIAN_POINT('Ctrl Pts',(9.0355451993808,12.2,-6.14792198943451));
#177215=CARTESIAN_POINT('Ctrl Pts',(9.033207284465,12.2,-6.14480632697283));
#177216=CARTESIAN_POINT('Ctrl Pts',(9.03086936986776,12.2,-6.14169066493567));
#177217=CARTESIAN_POINT('Ctrl Pts',(9.02853512596027,12.2,-6.13859061769259));
#177218=CARTESIAN_POINT('Ctrl Pts',(9.02620468487263,12.2,-6.13550621772093));
#177219=CARTESIAN_POINT('Ctrl Pts',(9.02387424346746,12.2,-6.13242181732903));
#177220=CARTESIAN_POINT('Ctrl Pts',(9.02154760538484,12.2,-6.12935306601911));
#177221=CARTESIAN_POINT('Ctrl Pts',(9.01922490075826,12.2,-6.12629999624162));
#177222=CARTESIAN_POINT('Ctrl Pts',(9.01690219613168,12.2,-6.12324692646413));
#177223=CARTESIAN_POINT('Ctrl Pts',(9.01458342800276,12.2,-6.12020953982454));
#177224=CARTESIAN_POINT('Ctrl Pts',(9.01226872665481,12.2,-6.11718786877259));
#177225=CARTESIAN_POINT('Ctrl Pts',(9.00995402562225,12.2,-6.11416619813234));
#177226=CARTESIAN_POINT('Ctrl Pts',(9.00764339237899,12.2,-6.11116024455174));
#177227=CARTESIAN_POINT('Ctrl Pts',(9.00533696266817,12.2,-6.108170041727));
#177228=CARTESIAN_POINT('Ctrl Pts',(9.00303053264308,12.2,-6.10517983849484));
#177229=CARTESIAN_POINT('Ctrl Pts',(9.00072830672124,12.2,-6.10220538530919));
#177230=CARTESIAN_POINT('Ctrl Pts',(8.99843041937422,12.2,-6.09924671748288));
#177231=CARTESIAN_POINT('Ctrl Pts',(8.9961325323403,12.2,-6.0962880500597));
#177232=CARTESIAN_POINT('Ctrl Pts',(8.99383898375026,12.2,-6.09334516611781));
#177233=CARTESIAN_POINT('Ctrl Pts',(8.9915499139371,12.2,-6.09041810202272));
#177234=CARTESIAN_POINT('Ctrl Pts',(8.98926084381204,12.2,-6.08749103752882));
#177235=CARTESIAN_POINT('Ctrl Pts',(8.9869762501652,12.2,-6.08457979173375));
#177236=CARTESIAN_POINT('Ctrl Pts',(8.98469627342745,12.2,-6.08168439782157));
#177237=CARTESIAN_POINT('Ctrl Pts',(8.98241629700034,12.2,-6.07878900430389));
#177238=CARTESIAN_POINT('Ctrl Pts',(8.98014093700583,12.2,-6.07590946292891));
#177239=CARTESIAN_POINT('Ctrl Pts',(8.97787033396893,12.2,-6.07304580871754));
#177240=CARTESIAN_POINT('Ctrl Pts',(8.97559973062265,12.2,-6.070182154116));
#177241=CARTESIAN_POINT('Ctrl Pts',(8.9733338853686,12.2,-6.06733438398857));
#177242=CARTESIAN_POINT('Ctrl Pts',(8.9710729388568,12.2,-6.06450253550193));
#177243=CARTESIAN_POINT('Ctrl Pts',(8.96881199265306,12.2,-6.06167068740113));
#177244=CARTESIAN_POINT('Ctrl Pts',(8.96655594658323,12.2,-6.05885475911592));
#177245=CARTESIAN_POINT('Ctrl Pts',(8.96430494287659,12.2,-6.05605478414801));
#177246=CARTESIAN_POINT('Ctrl Pts',(8.96205393886325,12.2,-6.0532548087986));
#177247=CARTESIAN_POINT('Ctrl Pts',(8.95980797960246,12.2,-6.05047078679032));
#177248=CARTESIAN_POINT('Ctrl Pts',(8.95756720709179,12.2,-6.04770275230715));
#177249=CARTESIAN_POINT('Ctrl Pts',(8.95532643488641,12.2,-6.04493471820114));
#177250=CARTESIAN_POINT('Ctrl Pts',(8.95309085259114,12.2,-6.04218267060583));
#177251=CARTESIAN_POINT('Ctrl Pts',(8.95086060560624,12.2,-6.03944664443897));
#177252=CARTESIAN_POINT('Ctrl Pts',(8.94863035831747,12.2,-6.03671061789931));
#177253=CARTESIAN_POINT('Ctrl Pts',(8.9464054465211,12.2,-6.03399061088827));
#177254=CARTESIAN_POINT('Ctrl Pts',(8.94418601922341,12.2,-6.03128665900645));
#177255=CARTESIAN_POINT('Ctrl Pts',(8.94196659222811,12.2,-6.02858270749303));
#177256=CARTESIAN_POINT('Ctrl Pts',(8.93975264792269,12.2,-6.02589480897279));
#177257=CARTESIAN_POINT('Ctrl Pts',(8.93754433960266,12.2,-6.02322299824515));
#177258=CARTESIAN_POINT('Ctrl Pts',(8.93533603098175,12.2,-6.02055118715346));
#177259=CARTESIAN_POINT('Ctrl Pts',(8.93313335667242,12.2,-6.01789546329379));
#177260=CARTESIAN_POINT('Ctrl Pts',(8.93093646827492,12.2,-6.01525585948327));
#177261=CARTESIAN_POINT('Ctrl Pts',(8.92873957987742,12.2,-6.01261625567276));
#177262=CARTESIAN_POINT('Ctrl Pts',(8.92654847958058,12.2,-6.00999277340856));
#177263=CARTESIAN_POINT('Ctrl Pts',(8.92436331785097,12.2,-6.00738544482365));
#177264=CARTESIAN_POINT('Ctrl Pts',(8.92217815641909,12.2,-6.00477811659399));
#177265=CARTESIAN_POINT('Ctrl Pts',(8.91999893565585,12.2,-6.00218693964183));
#177266=CARTESIAN_POINT('Ctrl Pts',(8.91782581126807,12.2,-5.99961195095171));
#177267=CARTESIAN_POINT('Ctrl Pts',(8.91565268658419,12.2,-5.99703696191074));
#177268=CARTESIAN_POINT('Ctrl Pts',(8.91348565573319,12.2,-5.99447815979893));
#177269=CARTESIAN_POINT('Ctrl Pts',(8.91132487867164,12.2,-5.99193557788425));
#177270=CARTESIAN_POINT('Ctrl Pts',(8.9086239074919,12.2,-5.98875735066412));
#177271=CARTESIAN_POINT('Ctrl Pts',(8.90593270769286,12.2,-5.9856044650777));
#177272=CARTESIAN_POINT('Ctrl Pts',(8.90325158741589,12.2,-5.98247698785755));
#177273=CARTESIAN_POINT('Ctrl Pts',(8.90057046743118,12.2,-5.97934951097829));
#177274=CARTESIAN_POINT('Ctrl Pts',(8.89789943027546,12.2,-5.97624744051913));
#177275=CARTESIAN_POINT('Ctrl Pts',(8.8952387893146,12.2,-5.97317084210238));
#177276=CARTESIAN_POINT('Ctrl Pts',(8.89257814806374,12.2,-5.97009424335028));
#177277=CARTESIAN_POINT('Ctrl Pts',(8.88992790358494,12.2,-5.96704311665336));
#177278=CARTESIAN_POINT('Ctrl Pts',(8.88728837657017,12.2,-5.96401752463737));
#177279=CARTESIAN_POINT('Ctrl Pts',(8.8846488495554,12.2,-5.96099193262139));
#177280=CARTESIAN_POINT('Ctrl Pts',(8.88202004040435,12.2,-5.95799187684668));
#177281=CARTESIAN_POINT('Ctrl Pts',(8.87940227429232,12.2,-5.95501741816402));
#177282=CARTESIAN_POINT('Ctrl Pts',(8.87678450818029,12.2,-5.95204295948134));
#177283=CARTESIAN_POINT('Ctrl Pts',(8.87417778491502,12.2,-5.94909410132054));
#177284=CARTESIAN_POINT('Ctrl Pts',(8.87158243457623,12.2,-5.94617090408938));
#177285=CARTESIAN_POINT('Ctrl Pts',(8.86898708423745,12.2,-5.94324770685821));
#177286=CARTESIAN_POINT('Ctrl Pts',(8.86640310791324,12.2,-5.94035017228924));
#177287=CARTESIAN_POINT('Ctrl Pts',(8.86383083867653,12.2,-5.93747836270457));
#177288=CARTESIAN_POINT('Ctrl Pts',(8.86125856943983,12.2,-5.93460655311991));
#177289=CARTESIAN_POINT('Ctrl Pts',(8.8586980100784,12.2,-5.93176046984146));
#177290=CARTESIAN_POINT('Ctrl Pts',(8.85614949917499,12.2,-5.92894017365955));
#177291=CARTESIAN_POINT('Ctrl Pts',(8.85360098827159,12.2,-5.92611987747765));
#177292=CARTESIAN_POINT('Ctrl Pts',(8.85106452702945,12.2,-5.9233253703252));
#177293=CARTESIAN_POINT('Ctrl Pts',(8.8485404609763,12.2,-5.92055671399313));
#177294=CARTESIAN_POINT('Ctrl Pts',(8.84601639492315,12.2,-5.91778805766107));
#177295=CARTESIAN_POINT('Ctrl Pts',(8.84350472337769,12.2,-5.91504525183329));
#177296=CARTESIAN_POINT('Ctrl Pts',(8.84100579976657,12.2,-5.91232835974994));
#177297=CARTESIAN_POINT('Ctrl Pts',(8.83850687615545,12.2,-5.9096114676666));
#177298=CARTESIAN_POINT('Ctrl Pts',(8.83602069835975,12.2,-5.90692048936608));
#177299=CARTESIAN_POINT('Ctrl Pts',(8.8335476248069,12.2,-5.90425548650684));
#177300=CARTESIAN_POINT('Ctrl Pts',(8.83107455125404,12.2,-5.90159048364759));
#177301=CARTESIAN_POINT('Ctrl Pts',(8.82861458132818,12.2,-5.89895145737786));
#177302=CARTESIAN_POINT('Ctrl Pts',(8.82616807806498,12.2,-5.89633846862921));
#177303=CARTESIAN_POINT('Ctrl Pts',(8.8237215748018,12.2,-5.89372547988056));
#177304=CARTESIAN_POINT('Ctrl Pts',(8.82128854006328,12.2,-5.89113852900349));
#177305=CARTESIAN_POINT('Ctrl Pts',(8.81886933930011,12.2,-5.8885776778243));
#177306=CARTESIAN_POINT('Ctrl Pts',(8.81645013853696,12.2,-5.88601682664509));
#177307=CARTESIAN_POINT('Ctrl Pts',(8.81404477541309,12.2,-5.88348207592123));
#177308=CARTESIAN_POINT('Ctrl Pts',(8.81165362203072,12.2,-5.8809734854505));
#177309=CARTESIAN_POINT('Ctrl Pts',(8.80926246864835,12.2,-5.87846489497977));
#177310=CARTESIAN_POINT('Ctrl Pts',(8.80688552581751,12.2,-5.87598246742099));
#177311=CARTESIAN_POINT('Ctrl Pts',(8.80452317741592,12.2,-5.87352626193703));
#177312=CARTESIAN_POINT('Ctrl Pts',(8.80216082901434,12.2,-5.87107005645307));
#177313=CARTESIAN_POINT('Ctrl Pts',(8.79981307044913,12.2,-5.86864007366674));
#177314=CARTESIAN_POINT('Ctrl Pts',(8.79748029468645,12.2,-5.86623637491888));
#177315=CARTESIAN_POINT('Ctrl Pts',(8.79468096387296,12.2,-5.86335193652626));
#177316=CARTESIAN_POINT('Ctrl Pts',(8.79190320452374,12.2,-5.86050534698501));
#177317=CARTESIAN_POINT('Ctrl Pts',(8.78914769987482,12.2,-5.8576967133387));
#177318=CARTESIAN_POINT('Ctrl Pts',(8.7863921952259,12.2,-5.85488807969241));
#177319=CARTESIAN_POINT('Ctrl Pts',(8.7836589462919,12.2,-5.85211739944306));
#177320=CARTESIAN_POINT('Ctrl Pts',(8.78094864963938,12.2,-5.84938477812404));
#177321=CARTESIAN_POINT('Ctrl Pts',(8.77823835298686,12.2,-5.846652156805));
#177322=CARTESIAN_POINT('Ctrl Pts',(8.77555101007843,12.2,-5.84395759571227));
#177323=CARTESIAN_POINT('Ctrl Pts',(8.77288733250692,12.2,-5.84130119830617));
#177324=CARTESIAN_POINT('Ctrl Pts',(8.77022365469345,12.2,-5.83864480065879));
#177325=CARTESIAN_POINT('Ctrl Pts',(8.76758364238227,12.2,-5.83602656706512));
#177326=CARTESIAN_POINT('Ctrl Pts',(8.76496802457412,12.2,-5.83344660059284));
#177327=CARTESIAN_POINT('Ctrl Pts',(8.76235240700355,12.2,-5.8308666343549));
#177328=CARTESIAN_POINT('Ctrl Pts',(8.75976118361121,12.2,-5.8283249376216));
#177329=CARTESIAN_POINT('Ctrl Pts',(8.75719509827607,12.2,-5.82582161120109));
#177330=CARTESIAN_POINT('Ctrl Pts',(8.75462901294091,12.2,-5.82331828478057));
#177331=CARTESIAN_POINT('Ctrl Pts',(8.75208806602611,12.2,-5.82085332991225));
#177332=CARTESIAN_POINT('Ctrl Pts',(8.74957302053237,12.2,-5.81842684949777));
#177333=CARTESIAN_POINT('Ctrl Pts',(8.74705797481019,12.2,-5.8160003688629));
#177334=CARTESIAN_POINT('Ctrl Pts',(8.74456882674242,12.2,-5.8136123627076));
#177335=CARTESIAN_POINT('Ctrl Pts',(8.74210635907009,12.2,-5.81126293404777));
#177336=CARTESIAN_POINT('Ctrl Pts',(8.73964389162143,12.2,-5.80891350560134));
#177337=CARTESIAN_POINT('Ctrl Pts',(8.73720810353741,12.2,-5.80660265445907));
#177338=CARTESIAN_POINT('Ctrl Pts',(8.73479978954156,12.2,-5.80433048295828));
#177339=CARTESIAN_POINT('Ctrl Pts',(8.7323914755457,12.2,-5.80205831145748));
#177340=CARTESIAN_POINT('Ctrl Pts',(8.73001063855613,12.2,-5.79982482057042));
#177341=CARTESIAN_POINT('Ctrl Pts',(8.72765809147299,12.2,-5.79763010923084));
#177342=CARTESIAN_POINT('Ctrl Pts',(8.72530554417617,12.2,-5.79543539769191));
#177343=CARTESIAN_POINT('Ctrl Pts',(8.722981290316,12.2,-5.79327946874748));
#177344=CARTESIAN_POINT('Ctrl Pts',(8.72068616107794,12.2,-5.79116242202858));
#177345=CARTESIAN_POINT('Ctrl Pts',(8.71839103204836,12.2,-5.78904537550198));
#177346=CARTESIAN_POINT('Ctrl Pts',(8.71612503018531,12.2,-5.78696721198419));
#177347=CARTESIAN_POINT('Ctrl Pts',(8.71388901126655,12.2,-5.78492803247494));
#177348=CARTESIAN_POINT('Ctrl Pts',(8.71165299234779,12.2,-5.7828888529657));
#177349=CARTESIAN_POINT('Ctrl Pts',(8.70944695698349,12.2,-5.78088865674373));
#177350=CARTESIAN_POINT('Ctrl Pts',(8.70727177920206,12.2,-5.77892754513143));
#177351=CARTESIAN_POINT('Ctrl Pts',(8.70509660122307,12.2,-5.77696643334098));
#177352=CARTESIAN_POINT('Ctrl Pts',(8.70295228519926,12.2,-5.77504440721966));
#177353=CARTESIAN_POINT('Ctrl Pts',(8.70083972725296,12.2,-5.77316156453639));
#177354=CARTESIAN_POINT('Ctrl Pts',(8.69872716949857,12.2,-5.77127872202416));
#177355=CARTESIAN_POINT('Ctrl Pts',(8.69664637075043,12.2,-5.76943506533334));
#177356=CARTESIAN_POINT('Ctrl Pts',(8.6945982549823,12.2,-5.76763069197414));
#177357=CARTESIAN_POINT('Ctrl Pts',(8.69255013921417,12.2,-5.76582631861494));
#177358=CARTESIAN_POINT('Ctrl Pts',(8.69053470500416,12.2,-5.76406123129984));
#177359=CARTESIAN_POINT('Ctrl Pts',(8.6885528995747,12.2,-5.76233552686083));
#177360=CARTESIAN_POINT('Ctrl Pts',(8.68657109396523,12.2,-5.76060982226505));
#177361=CARTESIAN_POINT('Ctrl Pts',(8.68462291897657,12.2,-5.75892350165751));
#177362=CARTESIAN_POINT('Ctrl Pts',(8.68270934454132,12.2,-5.75727666507045));
#177363=CARTESIAN_POINT('Ctrl Pts',(8.68079577027988,12.2,-5.75562982863299));
#177364=CARTESIAN_POINT('Ctrl Pts',(8.67891679728105,12.2,-5.75402247583932));
#177365=CARTESIAN_POINT('Ctrl Pts',(8.6770734251829,12.2,-5.752454704398));
#177366=CARTESIAN_POINT('Ctrl Pts',(8.67523005308474,12.2,-5.75088693295667));
#177367=CARTESIAN_POINT('Ctrl Pts',(8.67342228175881,12.2,-5.7493587457039));
#177368=CARTESIAN_POINT('Ctrl Pts',(8.67165113857156,12.2,-5.74787023733957));
#177369=CARTESIAN_POINT('Ctrl Pts',(8.6698799953843,12.2,-5.74638172897523));
#177370=CARTESIAN_POINT('Ctrl Pts',(8.66814547946741,12.2,-5.74493290224673));
#177371=CARTESIAN_POINT('Ctrl Pts',(8.66644864744318,12.2,-5.74352385387854));
#177372=CARTESIAN_POINT('Ctrl Pts',(8.66475181526481,12.2,-5.74211480538238));
#177373=CARTESIAN_POINT('Ctrl Pts',(8.66309266594835,12.2,-5.74074553799837));
#177374=CARTESIAN_POINT('Ctrl Pts',(8.66147228886173,12.2,-5.73941614642766));
#177375=CARTESIAN_POINT('Ctrl Pts',(8.65985191192229,12.2,-5.7380867549777));
#177376=CARTESIAN_POINT('Ctrl Pts',(8.65827030394331,12.2,-5.7367972411942));
#177377=CARTESIAN_POINT('Ctrl Pts',(8.65672858624224,12.2,-5.73554770273385));
#177378=CARTESIAN_POINT('Ctrl Pts',(8.65416645576684,12.2,-5.73347113543021));
#177379=CARTESIAN_POINT('Ctrl Pts',(8.65171447039556,12.2,-5.73150496079906));
#177380=CARTESIAN_POINT('Ctrl Pts',(8.64937799899994,12.2,-5.72964966100002));
#177381=CARTESIAN_POINT('Ctrl Pts',(8.64937799899994,15.2,-5.72964966100002));
#177382=CARTESIAN_POINT('Ctrl Pts',(8.65077718280868,15.2,-5.73076069768724));
#177383=CARTESIAN_POINT('Ctrl Pts',(8.65221780094386,15.2,-5.73191150037687));
#177384=CARTESIAN_POINT('Ctrl Pts',(8.65369867906269,15.2,-5.73310195413624));
#177385=CARTESIAN_POINT('Ctrl Pts',(8.65518669872435,15.2,-5.73429814886537));
#177386=CARTESIAN_POINT('Ctrl Pts',(8.65671537265224,15.2,-5.73553438487953));
#177387=CARTESIAN_POINT('Ctrl Pts',(8.65828355965168,15.2,-5.7368105625985));
#177388=CARTESIAN_POINT('Ctrl Pts',(8.65985174650868,15.2,-5.73808674020155));
#177389=CARTESIAN_POINT('Ctrl Pts',(8.661459445618,15.2,-5.73940286101586));
#177390=CARTESIAN_POINT('Ctrl Pts',(8.66310555047487,15.2,-5.7407588264666));
#177391=CARTESIAN_POINT('Ctrl Pts',(8.66475165533174,15.2,-5.74211479191736));
#177392=CARTESIAN_POINT('Ctrl Pts',(8.66643616407876,15.2,-5.74351060148557));
#177393=CARTESIAN_POINT('Ctrl Pts',(8.66815800210007,15.2,-5.74494615808617));
#177394=CARTESIAN_POINT('Ctrl Pts',(8.66987984027778,15.2,-5.74638171481717));
#177395=CARTESIAN_POINT('Ctrl Pts',(8.67163900552859,15.2,-5.74785701772148));
#177396=CARTESIAN_POINT('Ctrl Pts',(8.67343445396226,15.2,-5.74937196839009));
#177397=CARTESIAN_POINT('Ctrl Pts',(8.67522990223283,15.2,-5.75088691892109));
#177398=CARTESIAN_POINT('Ctrl Pts',(8.67706163222665,15.2,-5.75244151822626));
#177399=CARTESIAN_POINT('Ctrl Pts',(8.67892862750073,15.2,-5.75403566675901));
#177400=CARTESIAN_POINT('Ctrl Pts',(8.6807956227748,15.2,-5.75562981529175));
#177401=CARTESIAN_POINT('Ctrl Pts',(8.68269788293301,15.2,-5.75726351191311));
#177402=CARTESIAN_POINT('Ctrl Pts',(8.68463441636115,15.2,-5.75893665943392));
#177403=CARTESIAN_POINT('Ctrl Pts',(8.6865709499652,15.2,-5.76060980710673));
#177404=CARTESIAN_POINT('Ctrl Pts',(8.68854176058186,15.2,-5.76232240563443));
#177405=CARTESIAN_POINT('Ctrl Pts',(8.69054587944334,15.2,-5.76407435514925));
#177406=CARTESIAN_POINT('Ctrl Pts',(8.69254999812279,15.2,-5.76582630450495));
#177407=CARTESIAN_POINT('Ctrl Pts',(8.6945874299783,15.2,-5.76761760521468));
#177408=CARTESIAN_POINT('Ctrl Pts',(8.6966572316545,15.2,-5.76944815581655));
#177409=CARTESIAN_POINT('Ctrl Pts',(8.69872703333071,15.2,-5.77127870641841));
#177410=CARTESIAN_POINT('Ctrl Pts',(8.7008292078793,15.2,-5.77314851140881));
#177411=CARTESIAN_POINT('Ctrl Pts',(8.70296283863374,15.2,-5.77505746492108));
#177412=CARTESIAN_POINT('Ctrl Pts',(8.70509646938817,15.2,-5.77696641843334));
#177413=CARTESIAN_POINT('Ctrl Pts',(8.70726155826744,15.2,-5.77891452511656));
#177414=CARTESIAN_POINT('Ctrl Pts',(8.7094572102689,15.2,-5.78090168079169));
#177415=CARTESIAN_POINT('Ctrl Pts',(8.7116528624698,15.2,-5.78288883664731));
#177416=CARTESIAN_POINT('Ctrl Pts',(8.71387908026539,15.2,-5.78491504540674));
#177417=CARTESIAN_POINT('Ctrl Pts',(8.71613499338963,15.2,-5.78698020310433));
#177418=CARTESIAN_POINT('Ctrl Pts',(8.71839090630897,15.2,-5.78904536061433));
#177419=CARTESIAN_POINT('Ctrl Pts',(8.72067651407248,15.2,-5.79114946853386));
#177420=CARTESIAN_POINT('Ctrl Pts',(8.72299096799885,15.2,-5.79329242596564));
#177421=CARTESIAN_POINT('Ctrl Pts',(8.72530542192521,15.2,-5.79543538339742));
#177422=CARTESIAN_POINT('Ctrl Pts',(8.72764872183785,15.2,-5.79761719044126));
#177423=CARTESIAN_POINT('Ctrl Pts',(8.73002003899976,15.2,-5.79983774302458));
#177424=CARTESIAN_POINT('Ctrl Pts',(8.73239135637707,15.2,-5.80205829580961));
#177425=CARTESIAN_POINT('Ctrl Pts',(8.73479068972382,15.2,-5.80431759758176));
#177426=CARTESIAN_POINT('Ctrl Pts',(8.73721723210726,15.2,-5.80661554437535));
#177427=CARTESIAN_POINT('Ctrl Pts',(8.73964377427027,15.2,-5.80891349096022));
#177428=CARTESIAN_POINT('Ctrl Pts',(8.74209752398602,15.2,-5.81125008257448));
#177429=CARTESIAN_POINT('Ctrl Pts',(8.74457769132377,15.2,-5.81362521799887));
#177430=CARTESIAN_POINT('Ctrl Pts',(8.74705785866152,15.2,-5.81600035342327));
#177431=CARTESIAN_POINT('Ctrl Pts',(8.74956444276769,15.2,-5.81841403198276));
#177432=CARTESIAN_POINT('Ctrl Pts',(8.75209667200723,15.2,-5.82086615047434));
#177433=CARTESIAN_POINT('Ctrl Pts',(8.75462890147678,15.2,-5.82331826918867));
#177434=CARTESIAN_POINT('Ctrl Pts',(8.75718677371192,15.2,-5.82580882879497));
#177435=CARTESIAN_POINT('Ctrl Pts',(8.75976953548314,15.2,-5.82833772472801));
#177436=CARTESIAN_POINT('Ctrl Pts',(8.76235229701977,15.2,-5.83086662043136));
#177437=CARTESIAN_POINT('Ctrl Pts',(8.76495994775387,15.2,-5.83343385342796));
#177438=CARTESIAN_POINT('Ctrl Pts',(8.76759174724156,15.2,-5.83603931899994));
#177439=CARTESIAN_POINT('Ctrl Pts',(8.77022354672925,15.2,-5.83864478457192));
#177440=CARTESIAN_POINT('Ctrl Pts',(8.7728794957223,15.2,-5.84128848395629));
#177441=CARTESIAN_POINT('Ctrl Pts',(8.7755588714241,15.2,-5.84397031249061));
#177442=CARTESIAN_POINT('Ctrl Pts',(8.77823824736928,15.2,-5.84665214126852));
#177443=CARTESIAN_POINT('Ctrl Pts',(8.78094105090526,15.2,-5.84937210003936));
#177444=CARTESIAN_POINT('Ctrl Pts',(8.78366657180533,15.2,-5.85213008177558));
#177445=CARTESIAN_POINT('Ctrl Pts',(8.78639209245782,15.2,-5.85488806326128));
#177446=CARTESIAN_POINT('Ctrl Pts',(8.78914033154752,15.2,-5.85768406944958));
#177447=CARTESIAN_POINT('Ctrl Pts',(8.7919105972095,15.2,-5.86051799577624));
#177448=CARTESIAN_POINT('Ctrl Pts',(8.79468086287148,15.2,-5.8633519221029));
#177449=CARTESIAN_POINT('Ctrl Pts',(8.7974731535415,15.2,-5.86622376756559));
#177450=CARTESIAN_POINT('Ctrl Pts',(8.80028679235499,15.2,-5.86913342612486));
#177451=CARTESIAN_POINT('Ctrl Pts',(8.80263149145141,15.2,-5.87155814167902));
#177452=CARTESIAN_POINT('Ctrl Pts',(8.80499101342884,15.2,-5.87400911785615));
#177453=CARTESIAN_POINT('Ctrl Pts',(8.80736497655307,15.2,-5.87648629160477));
#177454=CARTESIAN_POINT('Ctrl Pts',(8.8097389396773,15.2,-5.87896346535338));
#177455=CARTESIAN_POINT('Ctrl Pts',(8.81212734162106,15.2,-5.88146683840938));
#177456=CARTESIAN_POINT('Ctrl Pts',(8.8145298032986,15.2,-5.88399634724024));
#177457=CARTESIAN_POINT('Ctrl Pts',(8.81693226497614,15.2,-5.8865258560711));
#177458=CARTESIAN_POINT('Ctrl Pts',(8.81934878816102,15.2,-5.88908150223884));
#177459=CARTESIAN_POINT('Ctrl Pts',(8.82177899746658,15.2,-5.89166322272495));
#177460=CARTESIAN_POINT('Ctrl Pts',(8.82420920677214,15.2,-5.89424494321107));
#177461=CARTESIAN_POINT('Ctrl Pts',(8.82665310475672,15.2,-5.89685273952825));
#177462=CARTESIAN_POINT('Ctrl Pts',(8.82911032247625,15.2,-5.89948654898472));
#177463=CARTESIAN_POINT('Ctrl Pts',(8.83156754019577,15.2,-5.9021203584412));
#177464=CARTESIAN_POINT('Ctrl Pts',(8.83403808046173,15.2,-5.90478018119662));
#177465=CARTESIAN_POINT('Ctrl Pts',(8.83652158046241,15.2,-5.90746595418409));
#177466=CARTESIAN_POINT('Ctrl Pts',(8.83900508046309,15.2,-5.91015172717154));
#177467=CARTESIAN_POINT('Ctrl Pts',(8.8415015393023,15.2,-5.91286345222221));
#177468=CARTESIAN_POINT('Ctrl Pts',(8.84401060520575,15.2,-5.91560106444582));
#177469=CARTESIAN_POINT('Ctrl Pts',(8.8470214841805,15.2,-5.91888619899478));
#177470=CARTESIAN_POINT('Ctrl Pts',(8.85005051456211,15.2,-5.92220861444699));
#177471=CARTESIAN_POINT('Ctrl Pts',(8.85309709279853,15.2,-5.92556820075676));
#177472=CARTESIAN_POINT('Ctrl Pts',(8.85563590808779,15.2,-5.92836785611662));
#177473=CARTESIAN_POINT('Ctrl Pts',(8.85818691135547,15.2,-5.9311933250333));
#177474=CARTESIAN_POINT('Ctrl Pts',(8.86074975829991,15.2,-5.93404454378328));
#177475=CARTESIAN_POINT('Ctrl Pts',(8.86331260524433,15.2,-5.93689576253325));
#177476=CARTESIAN_POINT('Ctrl Pts',(8.86588729726176,15.2,-5.93977273306605));
#177477=CARTESIAN_POINT('Ctrl Pts',(8.86847349505133,15.2,-5.9426753894682));
#177478=CARTESIAN_POINT('Ctrl Pts',(8.8710596928409,15.2,-5.94557804587036));
#177479=CARTESIAN_POINT('Ctrl Pts',(8.87365739728669,15.2,-5.94850639163639));
#177480=CARTESIAN_POINT('Ctrl Pts',(8.87626627666227,15.2,-5.95146035969329));
#177481=CARTESIAN_POINT('Ctrl Pts',(8.87887515603786,15.2,-5.9544143277502));
#177482=CARTESIAN_POINT('Ctrl Pts',(8.88149520812149,15.2,-5.95739392271755));
#177483=CARTESIAN_POINT('Ctrl Pts',(8.88412610916371,15.2,-5.96039907570498));
#177484=CARTESIAN_POINT('Ctrl Pts',(8.88675701020592,15.2,-5.9634042286924));
#177485=CARTESIAN_POINT('Ctrl Pts',(8.88939875734511,15.2,-5.96643494299308));
#177486=CARTESIAN_POINT('Ctrl Pts',(8.89205103012344,15.2,-5.96949115417498));
#177487=CARTESIAN_POINT('Ctrl Pts',(8.89470330290178,15.2,-5.97254736535688));
#177488=CARTESIAN_POINT('Ctrl Pts',(8.89736609970933,15.2,-5.97562907340372));
#177489=CARTESIAN_POINT('Ctrl Pts',(8.90003910359358,15.2,-5.97873621481074));
#177490=CARTESIAN_POINT('Ctrl Pts',(8.90271210747784,15.2,-5.98184335621774));
#177491=CARTESIAN_POINT('Ctrl Pts',(8.90539531922359,15.2,-5.98497593143315));
#177492=CARTESIAN_POINT('Ctrl Pts',(8.90808842387718,15.2,-5.98813387442135));
#177493=CARTESIAN_POINT('Ctrl Pts',(8.91024290742391,15.2,-5.99066022860537));
#177494=CARTESIAN_POINT('Ctrl Pts',(8.91240372326427,15.2,-5.99320281839282));
#177495=CARTESIAN_POINT('Ctrl Pts',(8.91457071403116,15.2,-5.99576161234926));
#177496=CARTESIAN_POINT('Ctrl Pts',(8.91727945271122,15.2,-5.99896010505626));
#177497=CARTESIAN_POINT('Ctrl Pts',(8.91999783703608,15.2,-6.00218391423351));
#177498=CARTESIAN_POINT('Ctrl Pts',(8.92272556350677,15.2,-6.00543297778985));
#177499=CARTESIAN_POINT('Ctrl Pts',(8.92490774480225,15.2,-6.00803222877659));
#177500=CARTESIAN_POINT('Ctrl Pts',(8.92709590470514,15.2,-6.01064763930181));
#177501=CARTESIAN_POINT('Ctrl Pts',(8.9292898898253,15.2,-6.01327918044687));
#177502=CARTESIAN_POINT('Ctrl Pts',(8.93148387464653,15.2,-6.01591072123339));
#177503=CARTESIAN_POINT('Ctrl Pts',(8.93368368420034,15.2,-6.01855839143449));
#177504=CARTESIAN_POINT('Ctrl Pts',(8.93588916635301,15.2,-6.02122215621567));
#177505=CARTESIAN_POINT('Ctrl Pts',(8.93809464880617,15.2,-6.0238859213598));
#177506=CARTESIAN_POINT('Ctrl Pts',(8.94030580299235,15.2,-6.02656578285822));
#177507=CARTESIAN_POINT('Ctrl Pts',(8.94252247961327,15.2,-6.02926170614124));
#177508=CARTESIAN_POINT('Ctrl Pts',(8.94473915593218,15.2,-6.03195762905694));
#177509=CARTESIAN_POINT('Ctrl Pts',(8.94696135213644,15.2,-6.03466961418449));
#177510=CARTESIAN_POINT('Ctrl Pts',(8.94918892234288,15.2,-6.03739762829376));
#177511=CARTESIAN_POINT('Ctrl Pts',(8.95197338532854,15.2,-6.04080764620911));
#177512=CARTESIAN_POINT('Ctrl Pts',(8.95476624160609,15.2,-6.04424270939178));
#177513=CARTESIAN_POINT('Ctrl Pts',(8.95756720709179,15.2,-6.04770275230715));
#177514=CARTESIAN_POINT('Ctrl Pts',(8.95980797960246,15.2,-6.05047078679032));
#177515=CARTESIAN_POINT('Ctrl Pts',(8.96205393886324,15.2,-6.05325480879859));
#177516=CARTESIAN_POINT('Ctrl Pts',(8.96430494287659,15.2,-6.056054784148));
#177517=CARTESIAN_POINT('Ctrl Pts',(8.96655594658323,15.2,-6.05885475911592));
#177518=CARTESIAN_POINT('Ctrl Pts',(8.96881199265308,15.2,-6.06167068740115));
#177519=CARTESIAN_POINT('Ctrl Pts',(8.97107293885681,15.2,-6.06450253550193));
#177520=CARTESIAN_POINT('Ctrl Pts',(8.9738991218425,15.2,-6.06804234591729));
#177521=CARTESIAN_POINT('Ctrl Pts',(8.97673295931455,15.2,-6.07160703222221));
#177522=CARTESIAN_POINT('Ctrl Pts',(8.97957417577249,15.2,-6.07519652749868));
#177523=CARTESIAN_POINT('Ctrl Pts',(8.98184714906271,15.2,-6.07806812387637));
#177524=CARTESIAN_POINT('Ctrl Pts',(8.98412484365622,15.2,-6.08095559776391));
#177525=CARTESIAN_POINT('Ctrl Pts',(8.98640711983946,15.2,-6.08385891567967));
#177526=CARTESIAN_POINT('Ctrl Pts',(8.98868939571174,15.2,-6.08676223319985));
#177527=CARTESIAN_POINT('Ctrl Pts',(8.99097625317804,15.2,-6.08968139375391));
#177528=CARTESIAN_POINT('Ctrl Pts',(8.99326755354599,15.2,-6.09261636523518));
#177529=CARTESIAN_POINT('Ctrl Pts',(8.99555885422614,15.2,-6.09555133711633));
#177530=CARTESIAN_POINT('Ctrl Pts',(8.99785459857904,15.2,-6.09850212014937));
#177531=CARTESIAN_POINT('Ctrl Pts',(9.00015464670467,15.2,-6.10146867803429));
#177532=CARTESIAN_POINT('Ctrl Pts',(9.00245469451691,15.2,-6.10443523551501));
#177533=CARTESIAN_POINT('Ctrl Pts',(9.00475904789705,15.2,-6.10741757014222));
#177534=CARTESIAN_POINT('Ctrl Pts',(9.00706757098997,15.2,-6.11041564632334));
#177535=CARTESIAN_POINT('Ctrl Pts',(9.00937609439743,15.2,-6.11341372291293));
#177536=CARTESIAN_POINT('Ctrl Pts',(9.01168878724896,15.2,-6.11642754220109));
#177537=CARTESIAN_POINT('Ctrl Pts',(9.01400551343103,15.2,-6.1194570687561));
#177538=CARTESIAN_POINT('Ctrl Pts',(9.01632223929744,15.2,-6.12248659489834));
#177539=CARTESIAN_POINT('Ctrl Pts',(9.01864300161307,15.2,-6.12553182968468));
#177540=CARTESIAN_POINT('Ctrl Pts',(9.02096766414485,15.2,-6.12859273776618));
#177541=CARTESIAN_POINT('Ctrl Pts',(9.02329232699336,15.2,-6.13165364626472));
#177542=CARTESIAN_POINT('Ctrl Pts',(9.02562089208325,15.2,-6.13473022895278));
#177543=CARTESIAN_POINT('Ctrl Pts',(9.02795322627652,15.2,-6.13782245080206));
#177544=CARTESIAN_POINT('Ctrl Pts',(9.03028556015201,15.2,-6.14091467223004));
#177545=CARTESIAN_POINT('Ctrl Pts',(9.03262166388402,15.2,-6.14402253357677));
#177546=CARTESIAN_POINT('Ctrl Pts',(9.03496140685905,15.2,-6.14714600026428));
#177547=CARTESIAN_POINT('Ctrl Pts',(9.03730115015287,15.2,-6.15026946737736));
#177548=CARTESIAN_POINT('Ctrl Pts',(9.03964453225813,15.2,-6.1534085386419));
#177549=CARTESIAN_POINT('Ctrl Pts',(9.0419914244416,15.2,-6.15656318175828));
#177550=CARTESIAN_POINT('Ctrl Pts',(9.04433831662507,15.2,-6.15971782487466));
#177551=CARTESIAN_POINT('Ctrl Pts',(9.04668871920892,15.2,-6.16288803841228));
#177552=CARTESIAN_POINT('Ctrl Pts',(9.04904250339311,15.2,-6.16607378825416));
#177553=CARTESIAN_POINT('Ctrl Pts',(9.05139628725659,15.2,-6.16925953766198));
#177554=CARTESIAN_POINT('Ctrl Pts',(9.05375345326669,15.2,-6.17246082427395));
#177555=CARTESIAN_POINT('Ctrl Pts',(9.05611387447333,15.2,-6.17567761224777));
#177556=CARTESIAN_POINT('Ctrl Pts',(9.05847429600157,15.2,-6.17889440065986));
#177557=CARTESIAN_POINT('Ctrl Pts',(9.06083797364093,15.2,-6.18212669069127));
#177558=CARTESIAN_POINT('Ctrl Pts',(9.06320478110357,15.2,-6.18537444731431));
#177559=CARTESIAN_POINT('Ctrl Pts',(9.06557158824375,15.2,-6.18862220349484));
#177560=CARTESIAN_POINT('Ctrl Pts',(9.06794152469183,15.2,-6.19188542764556));
#177561=CARTESIAN_POINT('Ctrl Pts',(9.07031446833097,15.2,-6.1951640842654));
#177562=CARTESIAN_POINT('Ctrl Pts',(9.07268741229343,15.2,-6.19844274133196));
#177563=CARTESIAN_POINT('Ctrl Pts',(9.07506336046737,15.2,-6.20173683037261));
#177564=CARTESIAN_POINT('Ctrl Pts',(9.07744219265276,15.2,-6.20504631755398));
#177565=CARTESIAN_POINT('Ctrl Pts',(9.07982102451402,15.2,-6.20835580428443));
#177566=CARTESIAN_POINT('Ctrl Pts',(9.0822027386022,15.2,-6.21168068755065));
#177567=CARTESIAN_POINT('Ctrl Pts',(9.08458721463728,15.2,-6.21502093499869));
#177568=CARTESIAN_POINT('Ctrl Pts',(9.08697169099724,15.2,-6.21836118290184));
#177569=CARTESIAN_POINT('Ctrl Pts',(9.08935892868715,15.2,-6.22171679359375));
#177570=CARTESIAN_POINT('Ctrl Pts',(9.09174880692867,15.2,-6.22508773150067));
#177571=CARTESIAN_POINT('Ctrl Pts',(9.09413868484456,15.2,-6.2284586689483));
#177572=CARTESIAN_POINT('Ctrl Pts',(9.09653120285438,15.2,-6.23184493585954));
#177573=CARTESIAN_POINT('Ctrl Pts',(9.09892624265835,15.2,-6.23524649396881));
#177574=CARTESIAN_POINT('Ctrl Pts',(9.10132128278864,15.2,-6.23864805254156));
#177575=CARTESIAN_POINT('Ctrl Pts',(9.10371884416819,15.2,-6.2420649050135));
#177576=CARTESIAN_POINT('Ctrl Pts',(9.1061188078099,15.2,-6.24549701549396));
#177577=CARTESIAN_POINT('Ctrl Pts',(9.10851877112462,15.2,-6.2489291255068));
#177578=CARTESIAN_POINT('Ctrl Pts',(9.11092113811192,15.2,-6.25237649262957));
#177579=CARTESIAN_POINT('Ctrl Pts',(9.11332579008178,15.2,-6.25583908323383));
#177580=CARTESIAN_POINT('Ctrl Pts',(9.11573044237927,15.2,-6.25930167430988));
#177581=CARTESIAN_POINT('Ctrl Pts',(9.11813738030475,15.2,-6.26277948779292));
#177582=CARTESIAN_POINT('Ctrl Pts',(9.1205464884916,15.2,-6.26627248898328));
#177583=CARTESIAN_POINT('Ctrl Pts',(9.12295559667845,15.2,-6.26976549017364));
#177584=CARTESIAN_POINT('Ctrl Pts',(9.12536687366834,15.2,-6.27327367911025));
#177585=CARTESIAN_POINT('Ctrl Pts',(9.12778020591118,15.2,-6.27679702085936));
#177586=CARTESIAN_POINT('Ctrl Pts',(9.1301935378252,15.2,-6.28032036212842));
#177587=CARTESIAN_POINT('Ctrl Pts',(9.13260892429605,15.2,-6.28385885574417));
#177588=CARTESIAN_POINT('Ctrl Pts',(9.13502625099829,15.2,-6.28741246524754));
#177589=CARTESIAN_POINT('Ctrl Pts',(9.13804790962313,15.2,-6.29185447748989));
#177590=CARTESIAN_POINT('Ctrl Pts',(9.14107260097217,15.2,-6.29632011150551));
#177591=CARTESIAN_POINT('Ctrl Pts',(9.14410010374993,15.2,-6.30080929678328));
#177592=CARTESIAN_POINT('Ctrl Pts',(9.14652210610415,15.2,-6.30440064520122));
#177593=CARTESIAN_POINT('Ctrl Pts',(9.14894590835582,15.2,-6.30800706641262));
#177594=CARTESIAN_POINT('Ctrl Pts',(9.15137139865484,15.2,-6.31162852433374));
#177595=CARTESIAN_POINT('Ctrl Pts',(9.15379688862337,15.2,-6.31524998176143));
#177596=CARTESIAN_POINT('Ctrl Pts',(9.15622406744413,15.2,-6.31888647771555));
#177597=CARTESIAN_POINT('Ctrl Pts',(9.15865282275662,15.2,-6.32253797448914));
#177598=CARTESIAN_POINT('Ctrl Pts',(9.16108157840002,15.2,-6.32618947176025));
#177599=CARTESIAN_POINT('Ctrl Pts',(9.16351191170652,15.2,-6.32985597158025));
#177600=CARTESIAN_POINT('Ctrl Pts',(9.1659437133392,15.2,-6.33353743739355));
#177601=CARTESIAN_POINT('Ctrl Pts',(9.16837551464057,15.2,-6.33721890270526));
#177602=CARTESIAN_POINT('Ctrl Pts',(9.17080878248892,15.2,-6.34091533424829));
#177603=CARTESIAN_POINT('Ctrl Pts',(9.17324341106759,15.2,-6.3446266962217));
#177604=CARTESIAN_POINT('Ctrl Pts',(9.17506938258452,15.2,-6.34741021782817));
#177605=CARTESIAN_POINT('Ctrl Pts',(9.17689611803823,15.2,-6.35020213738773));
#177606=CARTESIAN_POINT('Ctrl Pts',(9.17872357318805,15.2,-6.35300244071658));
#177607=CARTESIAN_POINT('Ctrl Pts',(9.1811601802758,15.2,-6.35673617882753));
#177608=CARTESIAN_POINT('Ctrl Pts',(9.18359806499132,15.2,-6.36048482126557));
#177609=CARTESIAN_POINT('Ctrl Pts',(9.18603712195768,15.2,-6.36424833174944));
#177610=CARTESIAN_POINT('Ctrl Pts',(9.18786641451628,15.2,-6.36707096435595));
#177611=CARTESIAN_POINT('Ctrl Pts',(9.18969636621646,15.2,-6.36990196080313));
#177612=CARTESIAN_POINT('Ctrl Pts',(9.1915269318166,15.2,-6.37274130449161));
#177613=CARTESIAN_POINT('Ctrl Pts',(9.19335749741674,15.2,-6.37558064818009));
#177614=CARTESIAN_POINT('Ctrl Pts',(9.19518867673356,15.2,-6.37842834129329));
#177615=CARTESIAN_POINT('Ctrl Pts',(9.19702042679196,15.2,-6.38128436643879));
#177616=CARTESIAN_POINT('Ctrl Pts',(9.19885217685036,15.2,-6.3841403915843));
#177617=CARTESIAN_POINT('Ctrl Pts',(9.20068449597042,15.2,-6.38700474922275));
#177618=CARTESIAN_POINT('Ctrl Pts',(9.20251734116201,15.2,-6.38987742592759));
#177619=CARTESIAN_POINT('Ctrl Pts',(9.20435018635358,15.2,-6.39275010263242));
#177620=CARTESIAN_POINT('Ctrl Pts',(9.20618355725019,15.2,-6.39563109674288));
#177621=CARTESIAN_POINT('Ctrl Pts',(9.20801740985017,15.2,-6.3985203933451));
#177622=CARTESIAN_POINT('Ctrl Pts',(9.20985126278329,15.2,-6.40140969047222));
#177623=CARTESIAN_POINT('Ctrl Pts',(9.21168559669987,15.2,-6.40430729080999));
#177624=CARTESIAN_POINT('Ctrl Pts',(9.21352036963325,15.2,-6.40721317844178));
#177625=CARTESIAN_POINT('Ctrl Pts',(9.21535514223331,15.2,-6.41011906554565));
#177626=CARTESIAN_POINT('Ctrl Pts',(9.21719035300002,15.2,-6.4130332399241));
#177627=CARTESIAN_POINT('Ctrl Pts',(9.21902595818336,15.2,-6.41595568706865));
#177628=CARTESIAN_POINT('Ctrl Pts',(9.22086156336671,15.2,-6.4188781342132));
#177629=CARTESIAN_POINT('Ctrl Pts',(9.22269756404333,15.2,-6.4218088536127));
#177630=CARTESIAN_POINT('Ctrl Pts',(9.22453391573494,15.2,-6.42474783068596));
#177631=CARTESIAN_POINT('Ctrl Pts',(9.22637026742656,15.2,-6.42768680775922));
#177632=CARTESIAN_POINT('Ctrl Pts',(9.22820697139,15.2,-6.43063404135792));
#177633=CARTESIAN_POINT('Ctrl Pts',(9.23004398449827,15.2,-6.43358951697227));
#177634=CARTESIAN_POINT('Ctrl Pts',(9.23188099760654,15.2,-6.43654499258663));
#177635=CARTESIAN_POINT('Ctrl Pts',(9.23371831946644,15.2,-6.43950871131818));
#177636=CARTESIAN_POINT('Ctrl Pts',(9.23555590806632,15.2,-6.44248065545949));
#177637=CARTESIAN_POINT('Ctrl Pts',(9.2373934966662,15.2,-6.4454525996008));
#177638=CARTESIAN_POINT('Ctrl Pts',(9.23923135126605,15.2,-6.44843276974153));
#177639=CARTESIAN_POINT('Ctrl Pts',(9.24106943086591,15.2,-6.45142115229851));
#177640=CARTESIAN_POINT('Ctrl Pts',(9.24290751079969,15.2,-6.45440953539837));
#177641=CARTESIAN_POINT('Ctrl Pts',(9.24474581496685,15.2,-6.45740613003387));
#177642=CARTESIAN_POINT('Ctrl Pts',(9.2465843014424,15.2,-6.46041092022168));
#177643=CARTESIAN_POINT('Ctrl Pts',(9.24842278758395,15.2,-6.46341570986361));
#177644=CARTESIAN_POINT('Ctrl Pts',(9.25026145589731,15.2,-6.46642869627579));
#177645=CARTESIAN_POINT('Ctrl Pts',(9.25210026563071,15.2,-6.46944986306789));
#177646=CARTESIAN_POINT('Ctrl Pts',(9.25393907536411,15.2,-6.47247102985999));
#177647=CARTESIAN_POINT('Ctrl Pts',(9.25577802600054,15.2,-6.47550037704083));
#177648=CARTESIAN_POINT('Ctrl Pts',(9.25761707526707,15.2,-6.47853789009785));
#177649=CARTESIAN_POINT('Ctrl Pts',(9.25945612453359,15.2,-6.48157540315487));
#177650=CARTESIAN_POINT('Ctrl Pts',(9.26129527396678,15.2,-6.48462108092759));
#177651=CARTESIAN_POINT('Ctrl Pts',(9.26313448073328,15.2,-6.48767490948329));
#177652=CARTESIAN_POINT('Ctrl Pts',(9.26497368749979,15.2,-6.49072873803899));
#177653=CARTESIAN_POINT('Ctrl Pts',(9.26681295268296,15.2,-6.49379071664437));
#177654=CARTESIAN_POINT('Ctrl Pts',(9.2686522357828,15.2,-6.49686083019878));
#177655=CARTESIAN_POINT('Ctrl Pts',(9.27049151888264,15.2,-6.4999309437532));
#177656=CARTESIAN_POINT('Ctrl Pts',(9.27233081819915,15.2,-6.50300919175707));
#177657=CARTESIAN_POINT('Ctrl Pts',(9.27417009484065,15.2,-6.50609555935214));
#177658=CARTESIAN_POINT('Ctrl Pts',(9.27600937181628,15.2,-6.50918192750791));
#177659=CARTESIAN_POINT('Ctrl Pts',(9.27784862545027,15.2,-6.51227641499099));
#177660=CARTESIAN_POINT('Ctrl Pts',(9.27968781588422,15.2,-6.51537900619299));
#177661=CARTESIAN_POINT('Ctrl Pts',(9.28152700598405,15.2,-6.51848159683136));
#177662=CARTESIAN_POINT('Ctrl Pts',(9.28336613138071,15.2,-6.52159229186002));
#177663=CARTESIAN_POINT('Ctrl Pts',(9.28520515411408,15.2,-6.52471107561178));
#177664=CARTESIAN_POINT('Ctrl Pts',(9.28704417684745,15.2,-6.52782985936353));
#177665=CARTESIAN_POINT('Ctrl Pts',(9.28888309593385,15.2,-6.53095673117165));
#177666=CARTESIAN_POINT('Ctrl Pts',(9.29072187020037,15.2,-6.53409167585014));
#177667=CARTESIAN_POINT('Ctrl Pts',(9.29317356911104,15.2,-6.53827160189827));
#177668=CARTESIAN_POINT('Ctrl Pts',(9.29562501321898,15.2,-6.54246588134071));
#177669=CARTESIAN_POINT('Ctrl Pts',(9.2980761080742,15.2,-6.54667447532854));
#177670=CARTESIAN_POINT('Ctrl Pts',(9.29991442963306,15.2,-6.54983092153617));
#177671=CARTESIAN_POINT('Ctrl Pts',(9.30175255536687,15.2,-6.55299542097941));
#177672=CARTESIAN_POINT('Ctrl Pts',(9.3035904449256,15.2,-6.55616795719157));
#177673=CARTESIAN_POINT('Ctrl Pts',(9.30542833415045,15.2,-6.55934049282739));
#177674=CARTESIAN_POINT('Ctrl Pts',(9.30726598781376,15.2,-6.56252106577258));
#177675=CARTESIAN_POINT('Ctrl Pts',(9.30910336658876,15.2,-6.56570965960861));
#177676=CARTESIAN_POINT('Ctrl Pts',(9.31094074536376,15.2,-6.56889825344465));
#177677=CARTESIAN_POINT('Ctrl Pts',(9.31277784826691,15.2,-6.57209486974847));
#177678=CARTESIAN_POINT('Ctrl Pts',(9.31461463795015,15.2,-6.57529949138273));
#177679=CARTESIAN_POINT('Ctrl Pts',(9.31645142763339,15.2,-6.578504113017));
#177680=CARTESIAN_POINT('Ctrl Pts',(9.31828790329999,15.2,-6.58171674038364));
#177681=CARTESIAN_POINT('Ctrl Pts',(9.32012402748328,15.2,-6.58493735897495));
#177682=CARTESIAN_POINT('Ctrl Pts',(9.32196015166657,15.2,-6.58815797756627));
#177683=CARTESIAN_POINT('Ctrl Pts',(9.32379592338319,15.2,-6.59138658731558));
#177684=CARTESIAN_POINT('Ctrl Pts',(9.32563130602488,15.2,-6.5946231714473));
#177685=CARTESIAN_POINT('Ctrl Pts',(9.32746668866658,15.2,-6.59785975557902));
#177686=CARTESIAN_POINT('Ctrl Pts',(9.32930168085329,15.2,-6.6011043151107));
#177687=CARTESIAN_POINT('Ctrl Pts',(9.33113624312833,15.2,-6.60435683386242));
#177688=CARTESIAN_POINT('Ctrl Pts',(9.33297080540338,15.2,-6.60760935261415));
#177689=CARTESIAN_POINT('Ctrl Pts',(9.33480493680011,15.2,-6.61086982997397));
#177690=CARTESIAN_POINT('Ctrl Pts',(9.33663860106688,15.2,-6.61413825106245));
#177691=CARTESIAN_POINT('Ctrl Pts',(9.33847226566676,15.2,-6.61740667274471));
#177692=CARTESIAN_POINT('Ctrl Pts',(9.34030546333319,15.2,-6.62068303807088));
#177693=CARTESIAN_POINT('Ctrl Pts',(9.34213815989114,15.2,-6.62396733321595));
#177694=CARTESIAN_POINT('Ctrl Pts',(9.34458175474684,15.2,-6.62834639241495));
#177695=CARTESIAN_POINT('Ctrl Pts',(9.34702446114987,15.2,-6.63273954886213));
#177696=CARTESIAN_POINT('Ctrl Pts',(9.349466180617,15.2,-6.63714676338981));
#177697=CARTESIAN_POINT('Ctrl Pts',(9.35129747030051,15.2,-6.64045217443569));
#177698=CARTESIAN_POINT('Ctrl Pts',(9.35312820397086,15.2,-6.64376549154647));
#177699=CARTESIAN_POINT('Ctrl Pts',(9.35495833687086,15.2,-6.64708669734081));
#177700=CARTESIAN_POINT('Ctrl Pts',(9.35678846977087,15.2,-6.65040790313515));
#177701=CARTESIAN_POINT('Ctrl Pts',(9.35861800060096,15.2,-6.65373699742817));
#177702=CARTESIAN_POINT('Ctrl Pts',(9.36044690482625,15.2,-6.65707396726418));
#177703=CARTESIAN_POINT('Ctrl Pts',(9.36288544393859,15.2,-6.66152326064393));
#177704=CARTESIAN_POINT('Ctrl Pts',(9.36532286751701,15.2,-6.66598656016761));
#177705=CARTESIAN_POINT('Ctrl Pts',(9.36775917477149,15.2,-6.67046385458018));
#177706=CARTESIAN_POINT('Origin',(-5.66257110645729E-14,15.2,-1.77635683940025E-14));
#177707=CARTESIAN_POINT('',(8.88241603246431,15.2,-5.36127880541243));
#177708=CARTESIAN_POINT('',(8.88241603246431,12.2,-5.36127880541243));
#177709=CARTESIAN_POINT('',(8.88241603199995,15.2,-5.36127880500001));
#177710=CARTESIAN_POINT('Origin',(-5.66257110645729E-14,12.2,-1.77635683940025E-14));
#177711=CARTESIAN_POINT('Origin',(-5.66257110645729E-14,15.2,-1.77635683940025E-14));
#177712=CARTESIAN_POINT('Origin',(-5.66257110645729E-14,15.2,-1.77635683940025E-14));
#177713=CARTESIAN_POINT('',(10.0402696489999,15.2,-5.60740451200001));
#177714=CARTESIAN_POINT('',(10.2217148779999,15.2,-5.26939701900002));
#177715=CARTESIAN_POINT('Origin',(-5.66257110645729E-14,15.2,-1.77635683940025E-14));
#177716=CARTESIAN_POINT('',(10.2217148779999,12.2,-5.26939701900002));
#177717=CARTESIAN_POINT('',(10.2217148779999,15.2,-5.26939701900002));
#177718=CARTESIAN_POINT('',(10.0402696489999,12.2,-5.60740451200001));
#177719=CARTESIAN_POINT('Origin',(-5.66257110645729E-14,12.2,-1.77635683940025E-14));
#177720=CARTESIAN_POINT('',(10.0402696489999,15.2,-5.60740451200001));
#177721=CARTESIAN_POINT('Ctrl Pts',(10.2217148779999,15.2,-5.26939701900002));
#177722=CARTESIAN_POINT('Ctrl Pts',(10.2217148779999,11.6,-5.26939701900002));
#177723=CARTESIAN_POINT('Ctrl Pts',(10.2212575739999,15.2,-5.26878426900002));
#177724=CARTESIAN_POINT('Ctrl Pts',(10.2212575739999,11.6,-5.26878426900002));
#177725=CARTESIAN_POINT('Ctrl Pts',(10.2203429999999,15.2,-5.26755929400001));
#177726=CARTESIAN_POINT('Ctrl Pts',(10.2203429999999,11.6,-5.26755929400001));
#177727=CARTESIAN_POINT('Ctrl Pts',(10.2189712369999,15.2,-5.26572340900001));
#177728=CARTESIAN_POINT('Ctrl Pts',(10.2189712369999,11.6,-5.26572340900001));
#177729=CARTESIAN_POINT('Ctrl Pts',(10.2171424209999,15.2,-5.26327871600001));
#177730=CARTESIAN_POINT('Ctrl Pts',(10.2171424209999,11.6,-5.26327871600001));
#177731=CARTESIAN_POINT('Ctrl Pts',(10.2148567309999,15.2,-5.26022810500002));
#177732=CARTESIAN_POINT('Ctrl Pts',(10.2148567309999,11.6,-5.26022810500002));
#177733=CARTESIAN_POINT('Ctrl Pts',(10.2125713739999,15.2,-5.25718275100001));
#177734=CARTESIAN_POINT('Ctrl Pts',(10.2125713739999,11.6,-5.25718275100001));
#177735=CARTESIAN_POINT('Ctrl Pts',(10.2102863519999,15.2,-5.25414265600002));
#177736=CARTESIAN_POINT('Ctrl Pts',(10.2102863519999,11.6,-5.25414265600002));
#177737=CARTESIAN_POINT('Ctrl Pts',(10.2080016679999,15.2,-5.25110781800001));
#177738=CARTESIAN_POINT('Ctrl Pts',(10.2080016679999,11.6,-5.25110781800001));
#177739=CARTESIAN_POINT('Ctrl Pts',(10.2057173299999,15.2,-5.24807824100002));
#177740=CARTESIAN_POINT('Ctrl Pts',(10.2057173299999,11.6,-5.24807824100002));
#177741=CARTESIAN_POINT('Ctrl Pts',(10.2034333439999,15.2,-5.24505392700001));
#177742=CARTESIAN_POINT('Ctrl Pts',(10.2034333439999,11.6,-5.24505392700001));
#177743=CARTESIAN_POINT('Ctrl Pts',(10.2011497209999,15.2,-5.24203487700001));
#177744=CARTESIAN_POINT('Ctrl Pts',(10.2011497209999,11.6,-5.24203487700001));
#177745=CARTESIAN_POINT('Ctrl Pts',(10.1988664679999,15.2,-5.23902109400002));
#177746=CARTESIAN_POINT('Ctrl Pts',(10.1988664679999,11.6,-5.23902109400002));
#177747=CARTESIAN_POINT('Ctrl Pts',(10.1965835999999,15.2,-5.23601258300001));
#177748=CARTESIAN_POINT('Ctrl Pts',(10.1965835999999,11.6,-5.23601258300001));
#177749=CARTESIAN_POINT('Ctrl Pts',(10.1943011249999,15.2,-5.23300934300002));
#177750=CARTESIAN_POINT('Ctrl Pts',(10.1943011249999,11.6,-5.23300934300002));
#177751=CARTESIAN_POINT('Ctrl Pts',(10.1920190549999,15.2,-5.23001138000001));
#177752=CARTESIAN_POINT('Ctrl Pts',(10.1920190549999,11.6,-5.23001138000001));
#177753=CARTESIAN_POINT('Ctrl Pts',(10.1897373969999,15.2,-5.22701869500001));
#177754=CARTESIAN_POINT('Ctrl Pts',(10.1897373969999,11.6,-5.22701869500001));
#177755=CARTESIAN_POINT('Ctrl Pts',(10.1874561619999,15.2,-5.22403129000002));
#177756=CARTESIAN_POINT('Ctrl Pts',(10.1874561619999,11.6,-5.22403129000002));
#177757=CARTESIAN_POINT('Ctrl Pts',(10.1851753559999,15.2,-5.22104916700001));
#177758=CARTESIAN_POINT('Ctrl Pts',(10.1851753559999,11.6,-5.22104916700001));
#177759=CARTESIAN_POINT('Ctrl Pts',(10.1828949879999,15.2,-5.21807232700001));
#177760=CARTESIAN_POINT('Ctrl Pts',(10.1828949879999,11.6,-5.21807232700001));
#177761=CARTESIAN_POINT('Ctrl Pts',(10.1806150639999,15.2,-5.21510077400002));
#177762=CARTESIAN_POINT('Ctrl Pts',(10.1806150639999,11.6,-5.21510077400002));
#177763=CARTESIAN_POINT('Ctrl Pts',(10.1783355949999,15.2,-5.21213451000001));
#177764=CARTESIAN_POINT('Ctrl Pts',(10.1783355949999,11.6,-5.21213451000001));
#177765=CARTESIAN_POINT('Ctrl Pts',(10.1760565879999,15.2,-5.20917353600002));
#177766=CARTESIAN_POINT('Ctrl Pts',(10.1760565879999,11.6,-5.20917353600002));
#177767=CARTESIAN_POINT('Ctrl Pts',(10.1737780519999,15.2,-5.20621785500001));
#177768=CARTESIAN_POINT('Ctrl Pts',(10.1737780519999,11.6,-5.20621785500001));
#177769=CARTESIAN_POINT('Ctrl Pts',(10.1714999969999,15.2,-5.20326746900002));
#177770=CARTESIAN_POINT('Ctrl Pts',(10.1714999969999,11.6,-5.20326746900002));
#177771=CARTESIAN_POINT('Ctrl Pts',(10.1692224309999,15.2,-5.20032238000002));
#177772=CARTESIAN_POINT('Ctrl Pts',(10.1692224309999,11.6,-5.20032238000002));
#177773=CARTESIAN_POINT('Ctrl Pts',(10.1669453649999,15.2,-5.19738259100002));
#177774=CARTESIAN_POINT('Ctrl Pts',(10.1669453649999,11.6,-5.19738259100002));
#177775=CARTESIAN_POINT('Ctrl Pts',(10.1646688079999,15.2,-5.19444810300001));
#177776=CARTESIAN_POINT('Ctrl Pts',(10.1646688079999,11.6,-5.19444810300001));
#177777=CARTESIAN_POINT('Ctrl Pts',(10.1623927679999,15.2,-5.19151892100002));
#177778=CARTESIAN_POINT('Ctrl Pts',(10.1623927679999,11.6,-5.19151892100002));
#177779=CARTESIAN_POINT('Ctrl Pts',(10.1601172529999,15.2,-5.18859504400002));
#177780=CARTESIAN_POINT('Ctrl Pts',(10.1601172529999,11.6,-5.18859504400002));
#177781=CARTESIAN_POINT('Ctrl Pts',(10.1578422729999,15.2,-5.18567647600001));
#177782=CARTESIAN_POINT('Ctrl Pts',(10.1578422729999,11.6,-5.18567647600001));
#177783=CARTESIAN_POINT('Ctrl Pts',(10.1555678379999,15.2,-5.18276321900002));
#177784=CARTESIAN_POINT('Ctrl Pts',(10.1555678379999,11.6,-5.18276321900002));
#177785=CARTESIAN_POINT('Ctrl Pts',(10.1532939539999,15.2,-5.17985527400001));
#177786=CARTESIAN_POINT('Ctrl Pts',(10.1532939539999,11.6,-5.17985527400001));
#177787=CARTESIAN_POINT('Ctrl Pts',(10.1510206309999,15.2,-5.17695264500002));
#177788=CARTESIAN_POINT('Ctrl Pts',(10.1510206309999,11.6,-5.17695264500002));
#177789=CARTESIAN_POINT('Ctrl Pts',(10.1487478799999,15.2,-5.17405533200002));
#177790=CARTESIAN_POINT('Ctrl Pts',(10.1487478799999,11.6,-5.17405533200002));
#177791=CARTESIAN_POINT('Ctrl Pts',(10.1464757069999,15.2,-5.17116333800002));
#177792=CARTESIAN_POINT('Ctrl Pts',(10.1464757069999,11.6,-5.17116333800002));
#177793=CARTESIAN_POINT('Ctrl Pts',(10.1442041239999,15.2,-5.16827666700001));
#177794=CARTESIAN_POINT('Ctrl Pts',(10.1442041239999,11.6,-5.16827666700001));
#177795=CARTESIAN_POINT('Ctrl Pts',(10.1419331389999,15.2,-5.16539531900001));
#177796=CARTESIAN_POINT('Ctrl Pts',(10.1419331389999,11.6,-5.16539531900001));
#177797=CARTESIAN_POINT('Ctrl Pts',(10.1396627609999,15.2,-5.16251929700001));
#177798=CARTESIAN_POINT('Ctrl Pts',(10.1396627609999,11.6,-5.16251929700001));
#177799=CARTESIAN_POINT('Ctrl Pts',(10.1373929979999,15.2,-5.15964860200001));
#177800=CARTESIAN_POINT('Ctrl Pts',(10.1373929979999,11.6,-5.15964860200001));
#177801=CARTESIAN_POINT('Ctrl Pts',(10.1351238609999,15.2,-5.15678323800001));
#177802=CARTESIAN_POINT('Ctrl Pts',(10.1351238609999,11.6,-5.15678323800001));
#177803=CARTESIAN_POINT('Ctrl Pts',(10.1328553589999,15.2,-5.15392320600002));
#177804=CARTESIAN_POINT('Ctrl Pts',(10.1328553589999,11.6,-5.15392320600002));
#177805=CARTESIAN_POINT('Ctrl Pts',(10.1305874999999,15.2,-5.15106851000001));
#177806=CARTESIAN_POINT('Ctrl Pts',(10.1305874999999,11.6,-5.15106851000001));
#177807=CARTESIAN_POINT('Ctrl Pts',(10.1283202939999,15.2,-5.14821914900002));
#177808=CARTESIAN_POINT('Ctrl Pts',(10.1283202939999,11.6,-5.14821914900002));
#177809=CARTESIAN_POINT('Ctrl Pts',(10.1260537499999,15.2,-5.14537512800001));
#177810=CARTESIAN_POINT('Ctrl Pts',(10.1260537499999,11.6,-5.14537512800001));
#177811=CARTESIAN_POINT('Ctrl Pts',(10.1237878759999,15.2,-5.14253644700001));
#177812=CARTESIAN_POINT('Ctrl Pts',(10.1237878759999,11.6,-5.14253644700001));
#177813=CARTESIAN_POINT('Ctrl Pts',(10.1215226839999,15.2,-5.13970310900001));
#177814=CARTESIAN_POINT('Ctrl Pts',(10.1215226839999,11.6,-5.13970310900001));
#177815=CARTESIAN_POINT('Ctrl Pts',(10.1192581799999,15.2,-5.13687511700001));
#177816=CARTESIAN_POINT('Ctrl Pts',(10.1192581799999,11.6,-5.13687511700001));
#177817=CARTESIAN_POINT('Ctrl Pts',(10.1169943759999,15.2,-5.13405247200001));
#177818=CARTESIAN_POINT('Ctrl Pts',(10.1169943759999,11.6,-5.13405247200001));
#177819=CARTESIAN_POINT('Ctrl Pts',(10.1147312799999,15.2,-5.13123517600001));
#177820=CARTESIAN_POINT('Ctrl Pts',(10.1147312799999,11.6,-5.13123517600001));
#177821=CARTESIAN_POINT('Ctrl Pts',(10.1124689019999,15.2,-5.12842323200001));
#177822=CARTESIAN_POINT('Ctrl Pts',(10.1124689019999,11.6,-5.12842323200001));
#177823=CARTESIAN_POINT('Ctrl Pts',(10.1102072499999,15.2,-5.12561664200001));
#177824=CARTESIAN_POINT('Ctrl Pts',(10.1102072499999,11.6,-5.12561664200001));
#177825=CARTESIAN_POINT('Ctrl Pts',(10.1079463349999,15.2,-5.12281540800001));
#177826=CARTESIAN_POINT('Ctrl Pts',(10.1079463349999,11.6,-5.12281540800001));
#177827=CARTESIAN_POINT('Ctrl Pts',(10.1056861639999,15.2,-5.12001953100001));
#177828=CARTESIAN_POINT('Ctrl Pts',(10.1056861639999,11.6,-5.12001953100001));
#177829=CARTESIAN_POINT('Ctrl Pts',(10.1034267499999,15.2,-5.11722901400002));
#177830=CARTESIAN_POINT('Ctrl Pts',(10.1034267499999,11.6,-5.11722901400002));
#177831=CARTESIAN_POINT('Ctrl Pts',(10.1011680999999,15.2,-5.11444386000001));
#177832=CARTESIAN_POINT('Ctrl Pts',(10.1011680999999,11.6,-5.11444386000001));
#177833=CARTESIAN_POINT('Ctrl Pts',(10.0989102229999,15.2,-5.11166406900001));
#177834=CARTESIAN_POINT('Ctrl Pts',(10.0989102229999,11.6,-5.11166406900001));
#177835=CARTESIAN_POINT('Ctrl Pts',(10.0966531299999,15.2,-5.10888964500001));
#177836=CARTESIAN_POINT('Ctrl Pts',(10.0966531299999,11.6,-5.10888964500001));
#177837=CARTESIAN_POINT('Ctrl Pts',(10.0943968289999,15.2,-5.10612059000001));
#177838=CARTESIAN_POINT('Ctrl Pts',(10.0943968289999,11.6,-5.10612059000001));
#177839=CARTESIAN_POINT('Ctrl Pts',(10.0921413299999,15.2,-5.10335690500002));
#177840=CARTESIAN_POINT('Ctrl Pts',(10.0921413299999,11.6,-5.10335690500002));
#177841=CARTESIAN_POINT('Ctrl Pts',(10.0898866439999,15.2,-5.10059859300001));
#177842=CARTESIAN_POINT('Ctrl Pts',(10.0898866439999,11.6,-5.10059859300001));
#177843=CARTESIAN_POINT('Ctrl Pts',(10.0876327779999,15.2,-5.09784565500001));
#177844=CARTESIAN_POINT('Ctrl Pts',(10.0876327779999,11.6,-5.09784565500001));
#177845=CARTESIAN_POINT('Ctrl Pts',(10.0853797429999,15.2,-5.09509809400001));
#177846=CARTESIAN_POINT('Ctrl Pts',(10.0853797429999,11.6,-5.09509809400001));
#177847=CARTESIAN_POINT('Ctrl Pts',(10.0831275479999,15.2,-5.09235591100001));
#177848=CARTESIAN_POINT('Ctrl Pts',(10.0831275479999,11.6,-5.09235591100001));
#177849=CARTESIAN_POINT('Ctrl Pts',(10.0808762039999,15.2,-5.08961911000001));
#177850=CARTESIAN_POINT('Ctrl Pts',(10.0808762039999,11.6,-5.08961911000001));
#177851=CARTESIAN_POINT('Ctrl Pts',(10.0786257189999,15.2,-5.08688769200001));
#177852=CARTESIAN_POINT('Ctrl Pts',(10.0786257189999,11.6,-5.08688769200001));
#177853=CARTESIAN_POINT('Ctrl Pts',(10.0763761029999,15.2,-5.08416165800002));
#177854=CARTESIAN_POINT('Ctrl Pts',(10.0763761029999,11.6,-5.08416165800002));
#177855=CARTESIAN_POINT('Ctrl Pts',(10.0741273649999,15.2,-5.08144101100001));
#177856=CARTESIAN_POINT('Ctrl Pts',(10.0741273649999,11.6,-5.08144101100001));
#177857=CARTESIAN_POINT('Ctrl Pts',(10.0718795159999,15.2,-5.07872575400001));
#177858=CARTESIAN_POINT('Ctrl Pts',(10.0718795159999,11.6,-5.07872575400001));
#177859=CARTESIAN_POINT('Ctrl Pts',(10.0696325649999,15.2,-5.07601588800001));
#177860=CARTESIAN_POINT('Ctrl Pts',(10.0696325649999,11.6,-5.07601588800001));
#177861=CARTESIAN_POINT('Ctrl Pts',(10.0673865209999,15.2,-5.07331141500002));
#177862=CARTESIAN_POINT('Ctrl Pts',(10.0673865209999,11.6,-5.07331141500002));
#177863=CARTESIAN_POINT('Ctrl Pts',(10.0651413949999,15.2,-5.07061233700002));
#177864=CARTESIAN_POINT('Ctrl Pts',(10.0651413949999,11.6,-5.07061233700002));
#177865=CARTESIAN_POINT('Ctrl Pts',(10.0628971959999,15.2,-5.06791865600002));
#177866=CARTESIAN_POINT('Ctrl Pts',(10.0628971959999,11.6,-5.06791865600002));
#177867=CARTESIAN_POINT('Ctrl Pts',(10.0606539349999,15.2,-5.06523037500001));
#177868=CARTESIAN_POINT('Ctrl Pts',(10.0606539349999,11.6,-5.06523037500001));
#177869=CARTESIAN_POINT('Ctrl Pts',(10.0584116189999,15.2,-5.06254749600001));
#177870=CARTESIAN_POINT('Ctrl Pts',(10.0584116189999,11.6,-5.06254749600001));
#177871=CARTESIAN_POINT('Ctrl Pts',(10.0561702599999,15.2,-5.05987001900001));
#177872=CARTESIAN_POINT('Ctrl Pts',(10.0561702599999,11.6,-5.05987001900001));
#177873=CARTESIAN_POINT('Ctrl Pts',(10.0539298679999,15.2,-5.05719794800001));
#177874=CARTESIAN_POINT('Ctrl Pts',(10.0539298679999,11.6,-5.05719794800001));
#177875=CARTESIAN_POINT('Ctrl Pts',(10.0516904509999,15.2,-5.05453128400001));
#177876=CARTESIAN_POINT('Ctrl Pts',(10.0516904509999,11.6,-5.05453128400001));
#177877=CARTESIAN_POINT('Ctrl Pts',(10.0494520199999,15.2,-5.05187002900001));
#177878=CARTESIAN_POINT('Ctrl Pts',(10.0494520199999,11.6,-5.05187002900001));
#177879=CARTESIAN_POINT('Ctrl Pts',(10.0472145849999,15.2,-5.04921418600001));
#177880=CARTESIAN_POINT('Ctrl Pts',(10.0472145849999,11.6,-5.04921418600001));
#177881=CARTESIAN_POINT('Ctrl Pts',(10.0449781559999,15.2,-5.04656375500002));
#177882=CARTESIAN_POINT('Ctrl Pts',(10.0449781559999,11.6,-5.04656375500002));
#177883=CARTESIAN_POINT('Ctrl Pts',(10.0427427419999,15.2,-5.04391874100001));
#177884=CARTESIAN_POINT('Ctrl Pts',(10.0427427419999,11.6,-5.04391874100001));
#177885=CARTESIAN_POINT('Ctrl Pts',(10.0405083539999,15.2,-5.04127914300001));
#177886=CARTESIAN_POINT('Ctrl Pts',(10.0405083539999,11.6,-5.04127914300001));
#177887=CARTESIAN_POINT('Ctrl Pts',(10.0382750009999,15.2,-5.03864496500002));
#177888=CARTESIAN_POINT('Ctrl Pts',(10.0382750009999,11.6,-5.03864496500002));
#177889=CARTESIAN_POINT('Ctrl Pts',(10.0360426939999,15.2,-5.03601620900001));
#177890=CARTESIAN_POINT('Ctrl Pts',(10.0360426939999,11.6,-5.03601620900001));
#177891=CARTESIAN_POINT('Ctrl Pts',(10.0338114419999,15.2,-5.03339287600001));
#177892=CARTESIAN_POINT('Ctrl Pts',(10.0338114419999,11.6,-5.03339287600001));
#177893=CARTESIAN_POINT('Ctrl Pts',(10.0315812549999,15.2,-5.03077496800001));
#177894=CARTESIAN_POINT('Ctrl Pts',(10.0315812549999,11.6,-5.03077496800001));
#177895=CARTESIAN_POINT('Ctrl Pts',(10.0293521449999,15.2,-5.02816248700002));
#177896=CARTESIAN_POINT('Ctrl Pts',(10.0293521449999,11.6,-5.02816248700002));
#177897=CARTESIAN_POINT('Ctrl Pts',(10.0271241189999,15.2,-5.02555543600002));
#177898=CARTESIAN_POINT('Ctrl Pts',(10.0271241189999,11.6,-5.02555543600002));
#177899=CARTESIAN_POINT('Ctrl Pts',(10.0248971889999,15.2,-5.02295381500002));
#177900=CARTESIAN_POINT('Ctrl Pts',(10.0248971889999,11.6,-5.02295381500002));
#177901=CARTESIAN_POINT('Ctrl Pts',(10.0226713639999,15.2,-5.02035762800002));
#177902=CARTESIAN_POINT('Ctrl Pts',(10.0226713639999,11.6,-5.02035762800002));
#177903=CARTESIAN_POINT('Ctrl Pts',(10.0204466549999,15.2,-5.01776687600001));
#177904=CARTESIAN_POINT('Ctrl Pts',(10.0204466549999,11.6,-5.01776687600001));
#177905=CARTESIAN_POINT('Ctrl Pts',(10.0182230729999,15.2,-5.01518156000001));
#177906=CARTESIAN_POINT('Ctrl Pts',(10.0182230729999,11.6,-5.01518156000001));
#177907=CARTESIAN_POINT('Ctrl Pts',(10.0160006259999,15.2,-5.01260168400002));
#177908=CARTESIAN_POINT('Ctrl Pts',(10.0160006259999,11.6,-5.01260168400002));
#177909=CARTESIAN_POINT('Ctrl Pts',(10.0137793259999,15.2,-5.01002724800002));
#177910=CARTESIAN_POINT('Ctrl Pts',(10.0137793259999,11.6,-5.01002724800002));
#177911=CARTESIAN_POINT('Ctrl Pts',(10.0115591819999,15.2,-5.00745825600001));
#177912=CARTESIAN_POINT('Ctrl Pts',(10.0115591819999,11.6,-5.00745825600001));
#177913=CARTESIAN_POINT('Ctrl Pts',(10.0093402039999,15.2,-5.00489470900002));
#177914=CARTESIAN_POINT('Ctrl Pts',(10.0093402039999,11.6,-5.00489470900002));
#177915=CARTESIAN_POINT('Ctrl Pts',(10.0071224029999,15.2,-5.00233660800002));
#177916=CARTESIAN_POINT('Ctrl Pts',(10.0071224029999,11.6,-5.00233660800002));
#177917=CARTESIAN_POINT('Ctrl Pts',(10.0049057889999,15.2,-4.99978395500001));
#177918=CARTESIAN_POINT('Ctrl Pts',(10.0049057889999,11.6,-4.99978395500001));
#177919=CARTESIAN_POINT('Ctrl Pts',(10.0026903729999,15.2,-4.99723675300002));
#177920=CARTESIAN_POINT('Ctrl Pts',(10.0026903729999,11.6,-4.99723675300002));
#177921=CARTESIAN_POINT('Ctrl Pts',(10.0004761639999,15.2,-4.99469500400001));
#177922=CARTESIAN_POINT('Ctrl Pts',(10.0004761639999,11.6,-4.99469500400001));
#177923=CARTESIAN_POINT('Ctrl Pts',(9.99826317399994,15.2,-4.99215870900001));
#177924=CARTESIAN_POINT('Ctrl Pts',(9.99826317399994,11.6,-4.99215870900002));
#177925=CARTESIAN_POINT('Ctrl Pts',(9.99605141199994,15.2,-4.98962787000002));
#177926=CARTESIAN_POINT('Ctrl Pts',(9.99605141199994,11.6,-4.98962787000002));
#177927=CARTESIAN_POINT('Ctrl Pts',(9.99384088799994,15.2,-4.98710249000001));
#177928=CARTESIAN_POINT('Ctrl Pts',(9.99384088799994,11.6,-4.98710249000002));
#177929=CARTESIAN_POINT('Ctrl Pts',(9.99163161399995,15.2,-4.98458256900001));
#177930=CARTESIAN_POINT('Ctrl Pts',(9.99163161399995,11.6,-4.98458256900001));
#177931=CARTESIAN_POINT('Ctrl Pts',(9.98942359899995,15.2,-4.98206811000002));
#177932=CARTESIAN_POINT('Ctrl Pts',(9.98942359899995,11.6,-4.98206811000002));
#177933=CARTESIAN_POINT('Ctrl Pts',(9.98721685399994,15.2,-4.97955911500001));
#177934=CARTESIAN_POINT('Ctrl Pts',(9.98721685399994,11.6,-4.97955911500001));
#177935=CARTESIAN_POINT('Ctrl Pts',(9.98501138999995,15.2,-4.97705558600002));
#177936=CARTESIAN_POINT('Ctrl Pts',(9.98501138999995,11.6,-4.97705558600002));
#177937=CARTESIAN_POINT('Ctrl Pts',(9.98280721699994,15.2,-4.97455752400001));
#177938=CARTESIAN_POINT('Ctrl Pts',(9.98280721699994,11.6,-4.97455752400001));
#177939=CARTESIAN_POINT('Ctrl Pts',(9.98060434499994,15.2,-4.97206493200002));
#177940=CARTESIAN_POINT('Ctrl Pts',(9.98060434499994,11.6,-4.97206493200002));
#177941=CARTESIAN_POINT('Ctrl Pts',(9.97840278499995,15.2,-4.96957781100001));
#177942=CARTESIAN_POINT('Ctrl Pts',(9.97840278499995,11.6,-4.96957781100001));
#177943=CARTESIAN_POINT('Ctrl Pts',(9.97620254699994,15.2,-4.96709616400001));
#177944=CARTESIAN_POINT('Ctrl Pts',(9.97620254699994,11.6,-4.96709616400001));
#177945=CARTESIAN_POINT('Ctrl Pts',(9.97400364199994,15.2,-4.96461999100001));
#177946=CARTESIAN_POINT('Ctrl Pts',(9.97400364199994,11.6,-4.96461999100002));
#177947=CARTESIAN_POINT('Ctrl Pts',(9.97180608099995,15.2,-4.96214929600002));
#177948=CARTESIAN_POINT('Ctrl Pts',(9.97180608099995,11.6,-4.96214929600002));
#177949=CARTESIAN_POINT('Ctrl Pts',(9.96960987299994,15.2,-4.95968407800001));
#177950=CARTESIAN_POINT('Ctrl Pts',(9.96960987299994,11.6,-4.95968407800001));
#177951=CARTESIAN_POINT('Ctrl Pts',(9.96741503199994,15.2,-4.95722434200002));
#177952=CARTESIAN_POINT('Ctrl Pts',(9.96741503199994,11.6,-4.95722434200002));
#177953=CARTESIAN_POINT('Ctrl Pts',(9.96522156599994,15.2,-4.95477008800002));
#177954=CARTESIAN_POINT('Ctrl Pts',(9.96522156599994,11.6,-4.95477008800002));
#177955=CARTESIAN_POINT('Ctrl Pts',(9.96302948499994,15.2,-4.95232131800002));
#177956=CARTESIAN_POINT('Ctrl Pts',(9.96302948499994,11.6,-4.95232131800002));
#177957=CARTESIAN_POINT('Ctrl Pts',(9.96083880199994,15.2,-4.94987803500001));
#177958=CARTESIAN_POINT('Ctrl Pts',(9.96083880199994,11.6,-4.94987803500001));
#177959=CARTESIAN_POINT('Ctrl Pts',(9.95864952599995,15.2,-4.94744023800001));
#177960=CARTESIAN_POINT('Ctrl Pts',(9.95864952599995,11.6,-4.94744023800001));
#177961=CARTESIAN_POINT('Ctrl Pts',(9.95646166799995,15.2,-4.94500793200002));
#177962=CARTESIAN_POINT('Ctrl Pts',(9.95646166799995,11.6,-4.94500793200002));
#177963=CARTESIAN_POINT('Ctrl Pts',(9.95427523999994,15.2,-4.94258111700002));
#177964=CARTESIAN_POINT('Ctrl Pts',(9.95427523999994,11.6,-4.94258111700002));
#177965=CARTESIAN_POINT('Ctrl Pts',(9.95209025099994,15.2,-4.94015979700002));
#177966=CARTESIAN_POINT('Ctrl Pts',(9.95209025099994,11.6,-4.94015979700002));
#177967=CARTESIAN_POINT('Ctrl Pts',(9.94990671399995,15.2,-4.93774397000001));
#177968=CARTESIAN_POINT('Ctrl Pts',(9.94990671399995,11.6,-4.93774397000002));
#177969=CARTESIAN_POINT('Ctrl Pts',(9.94772463699995,15.2,-4.93533364100001));
#177970=CARTESIAN_POINT('Ctrl Pts',(9.94772463699995,11.6,-4.93533364100002));
#177971=CARTESIAN_POINT('Ctrl Pts',(9.94554403299994,15.2,-4.93292881000002));
#177972=CARTESIAN_POINT('Ctrl Pts',(9.94554403299994,11.6,-4.93292881000002));
#177973=CARTESIAN_POINT('Ctrl Pts',(9.94336491299994,15.2,-4.93052948100001));
#177974=CARTESIAN_POINT('Ctrl Pts',(9.94336491299994,11.6,-4.93052948100001));
#177975=CARTESIAN_POINT('Ctrl Pts',(9.94118728699994,15.2,-4.92813565300001));
#177976=CARTESIAN_POINT('Ctrl Pts',(9.94118728699994,11.6,-4.92813565300002));
#177977=CARTESIAN_POINT('Ctrl Pts',(9.93901116599995,15.2,-4.92574732900001));
#177978=CARTESIAN_POINT('Ctrl Pts',(9.93901116599995,11.6,-4.92574732900002));
#177979=CARTESIAN_POINT('Ctrl Pts',(9.93683656099994,15.2,-4.92336451100002));
#177980=CARTESIAN_POINT('Ctrl Pts',(9.93683656099994,11.6,-4.92336451100002));
#177981=CARTESIAN_POINT('Ctrl Pts',(9.93466348399994,15.2,-4.92098720100001));
#177982=CARTESIAN_POINT('Ctrl Pts',(9.93466348399994,11.6,-4.92098720100001));
#177983=CARTESIAN_POINT('Ctrl Pts',(9.93249194399995,15.2,-4.91861540000002));
#177984=CARTESIAN_POINT('Ctrl Pts',(9.93249194399995,11.6,-4.91861540000002));
#177985=CARTESIAN_POINT('Ctrl Pts',(9.93032195399994,15.2,-4.91624911100002));
#177986=CARTESIAN_POINT('Ctrl Pts',(9.93032195399994,11.6,-4.91624911100002));
#177987=CARTESIAN_POINT('Ctrl Pts',(9.92815352399995,15.2,-4.91388833500002));
#177988=CARTESIAN_POINT('Ctrl Pts',(9.92815352399995,11.6,-4.91388833500002));
#177989=CARTESIAN_POINT('Ctrl Pts',(9.92598666499994,15.2,-4.91153307200001));
#177990=CARTESIAN_POINT('Ctrl Pts',(9.92598666499994,11.6,-4.91153307200001));
#177991=CARTESIAN_POINT('Ctrl Pts',(9.92382138899995,15.2,-4.90918332600002));
#177992=CARTESIAN_POINT('Ctrl Pts',(9.92382138899995,11.6,-4.90918332600002));
#177993=CARTESIAN_POINT('Ctrl Pts',(9.92165770599994,15.2,-4.90683909900001));
#177994=CARTESIAN_POINT('Ctrl Pts',(9.92165770599994,11.6,-4.90683909900001));
#177995=CARTESIAN_POINT('Ctrl Pts',(9.91949562799994,15.2,-4.90450039100002));
#177996=CARTESIAN_POINT('Ctrl Pts',(9.91949562799994,11.6,-4.90450039100002));
#177997=CARTESIAN_POINT('Ctrl Pts',(9.91733516599995,15.2,-4.90216720500001));
#177998=CARTESIAN_POINT('Ctrl Pts',(9.91733516599995,11.6,-4.90216720500001));
#177999=CARTESIAN_POINT('Ctrl Pts',(9.91517632999994,15.2,-4.89983954200001));
#178000=CARTESIAN_POINT('Ctrl Pts',(9.91517632999994,11.6,-4.89983954200001));
#178001=CARTESIAN_POINT('Ctrl Pts',(9.91301913399995,15.2,-4.89751740500001));
#178002=CARTESIAN_POINT('Ctrl Pts',(9.91301913399995,11.6,-4.89751740500001));
#178003=CARTESIAN_POINT('Ctrl Pts',(9.91086358699994,15.2,-4.89520079400001));
#178004=CARTESIAN_POINT('Ctrl Pts',(9.91086358699994,11.6,-4.89520079400002));
#178005=CARTESIAN_POINT('Ctrl Pts',(9.90870969999994,15.2,-4.89288971200001));
#178006=CARTESIAN_POINT('Ctrl Pts',(9.90870969999994,11.6,-4.89288971200002));
#178007=CARTESIAN_POINT('Ctrl Pts',(9.90655748599995,15.2,-4.89058415900002));
#178008=CARTESIAN_POINT('Ctrl Pts',(9.90655748599995,11.6,-4.89058415900002));
#178009=CARTESIAN_POINT('Ctrl Pts',(9.90440695499995,15.2,-4.88828413900002));
#178010=CARTESIAN_POINT('Ctrl Pts',(9.90440695499995,11.6,-4.88828413900002));
#178011=CARTESIAN_POINT('Ctrl Pts',(9.90225811999995,15.2,-4.88598965200001));
#178012=CARTESIAN_POINT('Ctrl Pts',(9.90225811999995,11.6,-4.88598965200001));
#178013=CARTESIAN_POINT('Ctrl Pts',(9.90011098899994,15.2,-4.88370070000002));
#178014=CARTESIAN_POINT('Ctrl Pts',(9.90011098899994,11.6,-4.88370070000002));
#178015=CARTESIAN_POINT('Ctrl Pts',(9.89796557699995,15.2,-4.88141728600001));
#178016=CARTESIAN_POINT('Ctrl Pts',(9.89796557699995,11.6,-4.88141728600001));
#178017=CARTESIAN_POINT('Ctrl Pts',(9.89582189499994,15.2,-4.87913940900001));
#178018=CARTESIAN_POINT('Ctrl Pts',(9.89582189499994,11.6,-4.87913940900001));
#178019=CARTESIAN_POINT('Ctrl Pts',(9.89367995199995,15.2,-4.87686707300002));
#178020=CARTESIAN_POINT('Ctrl Pts',(9.89367995199995,11.6,-4.87686707300002));
#178021=CARTESIAN_POINT('Ctrl Pts',(9.89153976099994,15.2,-4.87460027900001));
#178022=CARTESIAN_POINT('Ctrl Pts',(9.89153976099994,11.6,-4.87460027900002));
#178023=CARTESIAN_POINT('Ctrl Pts',(9.88940133499994,15.2,-4.87233902900002));
#178024=CARTESIAN_POINT('Ctrl Pts',(9.88940133499994,11.6,-4.87233902900002));
#178025=CARTESIAN_POINT('Ctrl Pts',(9.88726468299994,15.2,-4.87008332300002));
#178026=CARTESIAN_POINT('Ctrl Pts',(9.88726468299994,11.6,-4.87008332300002));
#178027=CARTESIAN_POINT('Ctrl Pts',(9.88512981699994,15.2,-4.86783316500001));
#178028=CARTESIAN_POINT('Ctrl Pts',(9.88512981699994,11.6,-4.86783316500001));
#178029=CARTESIAN_POINT('Ctrl Pts',(9.88299674999995,15.2,-4.86558855600002));
#178030=CARTESIAN_POINT('Ctrl Pts',(9.88299674999995,11.6,-4.86558855600002));
#178031=CARTESIAN_POINT('Ctrl Pts',(9.88086549299994,15.2,-4.86334949700002));
#178032=CARTESIAN_POINT('Ctrl Pts',(9.88086549299994,11.6,-4.86334949700002));
#178033=CARTESIAN_POINT('Ctrl Pts',(9.87873605699994,15.2,-4.86111598900001));
#178034=CARTESIAN_POINT('Ctrl Pts',(9.87873605699994,11.6,-4.86111598900001));
#178035=CARTESIAN_POINT('Ctrl Pts',(9.87660845399994,15.2,-4.85888803500002));
#178036=CARTESIAN_POINT('Ctrl Pts',(9.87660845399994,11.6,-4.85888803500002));
#178037=CARTESIAN_POINT('Ctrl Pts',(9.87448269599994,15.2,-4.85666563600001));
#178038=CARTESIAN_POINT('Ctrl Pts',(9.87448269599994,11.6,-4.85666563600002));
#178039=CARTESIAN_POINT('Ctrl Pts',(9.87235879499995,15.2,-4.85444879300001));
#178040=CARTESIAN_POINT('Ctrl Pts',(9.87235879499995,11.6,-4.85444879300002));
#178041=CARTESIAN_POINT('Ctrl Pts',(9.87023676299994,15.2,-4.85223750900001));
#178042=CARTESIAN_POINT('Ctrl Pts',(9.87023676299994,11.6,-4.85223750900001));
#178043=CARTESIAN_POINT('Ctrl Pts',(9.86811660899994,15.2,-4.85003178400001));
#178044=CARTESIAN_POINT('Ctrl Pts',(9.86811660899994,11.6,-4.85003178400001));
#178045=CARTESIAN_POINT('Ctrl Pts',(9.86599834899994,15.2,-4.84783162100001));
#178046=CARTESIAN_POINT('Ctrl Pts',(9.86599834899994,11.6,-4.84783162100001));
#178047=CARTESIAN_POINT('Ctrl Pts',(9.86388199199994,15.2,-4.84563702200001));
#178048=CARTESIAN_POINT('Ctrl Pts',(9.86388199199994,11.6,-4.84563702200001));
#178049=CARTESIAN_POINT('Ctrl Pts',(9.86176754899994,15.2,-4.84344798700001));
#178050=CARTESIAN_POINT('Ctrl Pts',(9.86176754899994,11.6,-4.84344798700001));
#178051=CARTESIAN_POINT('Ctrl Pts',(9.85965503599994,15.2,-4.84126451800002));
#178052=CARTESIAN_POINT('Ctrl Pts',(9.85965503599994,11.6,-4.84126451800002));
#178053=CARTESIAN_POINT('Ctrl Pts',(9.85754445999994,15.2,-4.83908661700001));
#178054=CARTESIAN_POINT('Ctrl Pts',(9.85754445999994,11.6,-4.83908661700002));
#178055=CARTESIAN_POINT('Ctrl Pts',(9.85543583699994,15.2,-4.83691428600002));
#178056=CARTESIAN_POINT('Ctrl Pts',(9.85543583699994,11.6,-4.83691428600002));
#178057=CARTESIAN_POINT('Ctrl Pts',(9.85332917699995,15.2,-4.83474752600001));
#178058=CARTESIAN_POINT('Ctrl Pts',(9.85332917699995,11.6,-4.83474752600001));
#178059=CARTESIAN_POINT('Ctrl Pts',(9.85122449199994,15.2,-4.83258633800002));
#178060=CARTESIAN_POINT('Ctrl Pts',(9.85122449199994,11.6,-4.83258633800002));
#178061=CARTESIAN_POINT('Ctrl Pts',(9.84912179299995,15.2,-4.83043072400001));
#178062=CARTESIAN_POINT('Ctrl Pts',(9.84912179299995,11.6,-4.83043072400002));
#178063=CARTESIAN_POINT('Ctrl Pts',(9.84702109499995,15.2,-4.82828068500002));
#178064=CARTESIAN_POINT('Ctrl Pts',(9.84702109499995,11.6,-4.82828068500002));
#178065=CARTESIAN_POINT('Ctrl Pts',(9.84492240799995,15.2,-4.82613622400001));
#178066=CARTESIAN_POINT('Ctrl Pts',(9.84492240799995,11.6,-4.82613622400002));
#178067=CARTESIAN_POINT('Ctrl Pts',(9.84282574499994,15.2,-4.82399734200001));
#178068=CARTESIAN_POINT('Ctrl Pts',(9.84282574499994,11.6,-4.82399734200001));
#178069=CARTESIAN_POINT('Ctrl Pts',(9.84073111699994,15.2,-4.82186404000001));
#178070=CARTESIAN_POINT('Ctrl Pts',(9.84073111699994,11.6,-4.82186404000002));
#178071=CARTESIAN_POINT('Ctrl Pts',(9.83863853799994,15.2,-4.81973632000001));
#178072=CARTESIAN_POINT('Ctrl Pts',(9.83863853799994,11.6,-4.81973632000001));
#178073=CARTESIAN_POINT('Ctrl Pts',(9.83654801799995,15.2,-4.81761418300001));
#178074=CARTESIAN_POINT('Ctrl Pts',(9.83654801799995,11.6,-4.81761418300001));
#178075=CARTESIAN_POINT('Ctrl Pts',(9.83445956999994,15.2,-4.81549763000002));
#178076=CARTESIAN_POINT('Ctrl Pts',(9.83445956999994,11.6,-4.81549763000002));
#178077=CARTESIAN_POINT('Ctrl Pts',(9.83237320799994,15.2,-4.81338666500001));
#178078=CARTESIAN_POINT('Ctrl Pts',(9.83237320799994,11.6,-4.81338666500002));
#178079=CARTESIAN_POINT('Ctrl Pts',(9.83028894099995,15.2,-4.81128128700002));
#178080=CARTESIAN_POINT('Ctrl Pts',(9.83028894099995,11.6,-4.81128128700002));
#178081=CARTESIAN_POINT('Ctrl Pts',(9.82820678499994,15.2,-4.80918149800001));
#178082=CARTESIAN_POINT('Ctrl Pts',(9.82820678499994,11.6,-4.80918149800001));
#178083=CARTESIAN_POINT('Ctrl Pts',(9.82612674899995,15.2,-4.80708730000002));
#178084=CARTESIAN_POINT('Ctrl Pts',(9.82612674899995,11.6,-4.80708730000002));
#178085=CARTESIAN_POINT('Ctrl Pts',(9.82404884799994,15.2,-4.80499869500001));
#178086=CARTESIAN_POINT('Ctrl Pts',(9.82404884799994,11.6,-4.80499869500001));
#178087=CARTESIAN_POINT('Ctrl Pts',(9.82197309199995,15.2,-4.80291568300002));
#178088=CARTESIAN_POINT('Ctrl Pts',(9.82197309199995,11.6,-4.80291568300002));
#178089=CARTESIAN_POINT('Ctrl Pts',(9.81989949599994,15.2,-4.80083826600001));
#178090=CARTESIAN_POINT('Ctrl Pts',(9.81989949599994,11.6,-4.80083826600001));
#178091=CARTESIAN_POINT('Ctrl Pts',(9.81782806999994,15.2,-4.79876644700001));
#178092=CARTESIAN_POINT('Ctrl Pts',(9.81782806999994,11.6,-4.79876644700001));
#178093=CARTESIAN_POINT('Ctrl Pts',(9.81575882799994,15.2,-4.79670022500001));
#178094=CARTESIAN_POINT('Ctrl Pts',(9.81575882799994,11.6,-4.79670022500002));
#178095=CARTESIAN_POINT('Ctrl Pts',(9.81369178299994,15.2,-4.79463960300002));
#178096=CARTESIAN_POINT('Ctrl Pts',(9.81369178299994,11.6,-4.79463960300002));
#178097=CARTESIAN_POINT('Ctrl Pts',(9.81162694599995,15.2,-4.79258458200002));
#178098=CARTESIAN_POINT('Ctrl Pts',(9.81162694599995,11.6,-4.79258458200002));
#178099=CARTESIAN_POINT('Ctrl Pts',(9.80956432999994,15.2,-4.79053516400001));
#178100=CARTESIAN_POINT('Ctrl Pts',(9.80956432999994,11.6,-4.79053516400001));
#178101=CARTESIAN_POINT('Ctrl Pts',(9.80750394899994,15.2,-4.78849134900001));
#178102=CARTESIAN_POINT('Ctrl Pts',(9.80750394899994,11.6,-4.78849134900001));
#178103=CARTESIAN_POINT('Ctrl Pts',(9.80544581399995,15.2,-4.78645314000001));
#178104=CARTESIAN_POINT('Ctrl Pts',(9.80544581399995,11.6,-4.78645314000001));
#178105=CARTESIAN_POINT('Ctrl Pts',(9.80338993799995,15.2,-4.78442053800002));
#178106=CARTESIAN_POINT('Ctrl Pts',(9.80338993799995,11.6,-4.78442053800002));
#178107=CARTESIAN_POINT('Ctrl Pts',(9.80133633399995,15.2,-4.78239354400001));
#178108=CARTESIAN_POINT('Ctrl Pts',(9.80133633399995,11.6,-4.78239354400001));
#178109=CARTESIAN_POINT('Ctrl Pts',(9.79928501499994,15.2,-4.78037216000001));
#178110=CARTESIAN_POINT('Ctrl Pts',(9.79928501499994,11.6,-4.78037216000002));
#178111=CARTESIAN_POINT('Ctrl Pts',(9.79723599299994,15.2,-4.77835638700002));
#178112=CARTESIAN_POINT('Ctrl Pts',(9.79723599299994,11.6,-4.77835638700002));
#178113=CARTESIAN_POINT('Ctrl Pts',(9.79518928099995,15.2,-4.77634622600001));
#178114=CARTESIAN_POINT('Ctrl Pts',(9.79518928099995,11.6,-4.77634622600002));
#178115=CARTESIAN_POINT('Ctrl Pts',(9.79314489299994,15.2,-4.77434167900002));
#178116=CARTESIAN_POINT('Ctrl Pts',(9.79314489299994,11.6,-4.77434167900002));
#178117=CARTESIAN_POINT('Ctrl Pts',(9.79110284099994,15.2,-4.77234274600002));
#178118=CARTESIAN_POINT('Ctrl Pts',(9.79110284099994,11.6,-4.77234274600002));
#178119=CARTESIAN_POINT('Ctrl Pts',(9.78906313699994,15.2,-4.77034943200001));
#178120=CARTESIAN_POINT('Ctrl Pts',(9.78906313699994,11.6,-4.77034943200001));
#178121=CARTESIAN_POINT('Ctrl Pts',(9.78702579499994,15.2,-4.76836173400002));
#178122=CARTESIAN_POINT('Ctrl Pts',(9.78702579499994,11.6,-4.76836173400002));
#178123=CARTESIAN_POINT('Ctrl Pts',(9.78499082799994,15.2,-4.76637965700001));
#178124=CARTESIAN_POINT('Ctrl Pts',(9.78499082799994,11.6,-4.76637965700002));
#178125=CARTESIAN_POINT('Ctrl Pts',(9.78295824899994,15.2,-4.76440319900002));
#178126=CARTESIAN_POINT('Ctrl Pts',(9.78295824899994,11.6,-4.76440319900002));
#178127=CARTESIAN_POINT('Ctrl Pts',(9.78092806999994,15.2,-4.76243236400002));
#178128=CARTESIAN_POINT('Ctrl Pts',(9.78092806999994,11.6,-4.76243236400002));
#178129=CARTESIAN_POINT('Ctrl Pts',(9.77890030599994,15.2,-4.76046715200001));
#178130=CARTESIAN_POINT('Ctrl Pts',(9.77890030599994,11.6,-4.76046715200001));
#178131=CARTESIAN_POINT('Ctrl Pts',(9.77687496799994,15.2,-4.75850756500002));
#178132=CARTESIAN_POINT('Ctrl Pts',(9.77687496799994,11.6,-4.75850756500002));
#178133=CARTESIAN_POINT('Ctrl Pts',(9.77485206899994,15.2,-4.75655360400001));
#178134=CARTESIAN_POINT('Ctrl Pts',(9.77485206899994,11.6,-4.75655360400001));
#178135=CARTESIAN_POINT('Ctrl Pts',(9.77283162499995,15.2,-4.75460527100001));
#178136=CARTESIAN_POINT('Ctrl Pts',(9.77283162499995,11.6,-4.75460527100002));
#178137=CARTESIAN_POINT('Ctrl Pts',(9.77081364699995,15.2,-4.75266256500001));
#178138=CARTESIAN_POINT('Ctrl Pts',(9.77081364699995,11.6,-4.75266256500001));
#178139=CARTESIAN_POINT('Ctrl Pts',(9.76879814799995,15.2,-4.75072549100001));
#178140=CARTESIAN_POINT('Ctrl Pts',(9.76879814799995,11.6,-4.75072549100001));
#178141=CARTESIAN_POINT('Ctrl Pts',(9.76678514199994,15.2,-4.74879404700001));
#178142=CARTESIAN_POINT('Ctrl Pts',(9.76678514199994,11.6,-4.74879404700001));
#178143=CARTESIAN_POINT('Ctrl Pts',(9.76477464199995,15.2,-4.74686823700001));
#178144=CARTESIAN_POINT('Ctrl Pts',(9.76477464199995,11.6,-4.74686823700001));
#178145=CARTESIAN_POINT('Ctrl Pts',(9.76276666199994,15.2,-4.74494806000001));
#178146=CARTESIAN_POINT('Ctrl Pts',(9.76276666199994,11.6,-4.74494806000001));
#178147=CARTESIAN_POINT('Ctrl Pts',(9.76076121399995,15.2,-4.74303351800001));
#178148=CARTESIAN_POINT('Ctrl Pts',(9.76076121399995,11.6,-4.74303351800002));
#178149=CARTESIAN_POINT('Ctrl Pts',(9.75875831199994,15.2,-4.74112461300002));
#178150=CARTESIAN_POINT('Ctrl Pts',(9.75875831199994,11.6,-4.74112461300002));
#178151=CARTESIAN_POINT('Ctrl Pts',(9.75675797099995,15.2,-4.73922134600001));
#178152=CARTESIAN_POINT('Ctrl Pts',(9.75675797099995,11.6,-4.73922134600001));
#178153=CARTESIAN_POINT('Ctrl Pts',(9.75476020099994,15.2,-4.73732371700001));
#178154=CARTESIAN_POINT('Ctrl Pts',(9.75476020099994,11.6,-4.73732371700002));
#178155=CARTESIAN_POINT('Ctrl Pts',(9.75276501899994,15.2,-4.73543173000001));
#178156=CARTESIAN_POINT('Ctrl Pts',(9.75276501899994,11.6,-4.73543173000001));
#178157=CARTESIAN_POINT('Ctrl Pts',(9.75077243699995,15.2,-4.73354538300002));
#178158=CARTESIAN_POINT('Ctrl Pts',(9.75077243699995,11.6,-4.73354538300002));
#178159=CARTESIAN_POINT('Ctrl Pts',(9.74878246899994,15.2,-4.73166467900001));
#178160=CARTESIAN_POINT('Ctrl Pts',(9.74878246899994,11.6,-4.73166467900001));
#178161=CARTESIAN_POINT('Ctrl Pts',(9.74679512899994,15.2,-4.72978962000001));
#178162=CARTESIAN_POINT('Ctrl Pts',(9.74679512899994,11.6,-4.72978962000001));
#178163=CARTESIAN_POINT('Ctrl Pts',(9.74481042799994,15.2,-4.72792020600002));
#178164=CARTESIAN_POINT('Ctrl Pts',(9.74481042799994,11.6,-4.72792020600002));
#178165=CARTESIAN_POINT('Ctrl Pts',(9.74282838199995,15.2,-4.72605643900001));
#178166=CARTESIAN_POINT('Ctrl Pts',(9.74282838199995,11.6,-4.72605643900002));
#178167=CARTESIAN_POINT('Ctrl Pts',(9.74084900499994,15.2,-4.72419831800002));
#178168=CARTESIAN_POINT('Ctrl Pts',(9.74084900499994,11.6,-4.72419831800002));
#178169=CARTESIAN_POINT('Ctrl Pts',(9.73887230999994,15.2,-4.72234584700002));
#178170=CARTESIAN_POINT('Ctrl Pts',(9.73887230999994,11.6,-4.72234584700002));
#178171=CARTESIAN_POINT('Ctrl Pts',(9.73689830999995,15.2,-4.72049902600002));
#178172=CARTESIAN_POINT('Ctrl Pts',(9.73689830999995,11.6,-4.72049902600002));
#178173=CARTESIAN_POINT('Ctrl Pts',(9.73492701999995,15.2,-4.71865785700002));
#178174=CARTESIAN_POINT('Ctrl Pts',(9.73492701999995,11.6,-4.71865785700002));
#178175=CARTESIAN_POINT('Ctrl Pts',(9.73295845299995,15.2,-4.71682234000002));
#178176=CARTESIAN_POINT('Ctrl Pts',(9.73295845299995,11.6,-4.71682234000002));
#178177=CARTESIAN_POINT('Ctrl Pts',(9.73099262399994,15.2,-4.71499247700002));
#178178=CARTESIAN_POINT('Ctrl Pts',(9.73099262399994,11.6,-4.71499247700002));
#178179=CARTESIAN_POINT('Ctrl Pts',(9.72902954599994,15.2,-4.71316826800001));
#178180=CARTESIAN_POINT('Ctrl Pts',(9.72902954599994,11.6,-4.71316826800001));
#178181=CARTESIAN_POINT('Ctrl Pts',(9.72706923299994,15.2,-4.71134971600002));
#178182=CARTESIAN_POINT('Ctrl Pts',(9.72706923299994,11.6,-4.71134971600002));
#178183=CARTESIAN_POINT('Ctrl Pts',(9.72511169899994,15.2,-4.70953682000002));
#178184=CARTESIAN_POINT('Ctrl Pts',(9.72511169899994,11.6,-4.70953682000002));
#178185=CARTESIAN_POINT('Ctrl Pts',(9.72315695899994,15.2,-4.70772958400001));
#178186=CARTESIAN_POINT('Ctrl Pts',(9.72315695899994,11.6,-4.70772958400001));
#178187=CARTESIAN_POINT('Ctrl Pts',(9.72120502599994,15.2,-4.70592800700001));
#178188=CARTESIAN_POINT('Ctrl Pts',(9.72120502599994,11.6,-4.70592800700001));
#178189=CARTESIAN_POINT('Ctrl Pts',(9.71925591399994,15.2,-4.70413209100002));
#178190=CARTESIAN_POINT('Ctrl Pts',(9.71925591399994,11.6,-4.70413209100002));
#178191=CARTESIAN_POINT('Ctrl Pts',(9.71730963799994,15.2,-4.70234183600001));
#178192=CARTESIAN_POINT('Ctrl Pts',(9.71730963799994,11.6,-4.70234183600002));
#178193=CARTESIAN_POINT('Ctrl Pts',(9.71536621099995,15.2,-4.70055724400002));
#178194=CARTESIAN_POINT('Ctrl Pts',(9.71536621099995,11.6,-4.70055724400002));
#178195=CARTESIAN_POINT('Ctrl Pts',(9.71342564799994,15.2,-4.69877831600002));
#178196=CARTESIAN_POINT('Ctrl Pts',(9.71342564799994,11.6,-4.69877831600002));
#178197=CARTESIAN_POINT('Ctrl Pts',(9.71148796399994,15.2,-4.69700505400001));
#178198=CARTESIAN_POINT('Ctrl Pts',(9.71148796399994,11.6,-4.69700505400002));
#178199=CARTESIAN_POINT('Ctrl Pts',(9.70955317199994,15.2,-4.69523745800001));
#178200=CARTESIAN_POINT('Ctrl Pts',(9.70955317199994,11.6,-4.69523745800002));
#178201=CARTESIAN_POINT('Ctrl Pts',(9.70762128699995,15.2,-4.69347552800001));
#178202=CARTESIAN_POINT('Ctrl Pts',(9.70762128699995,11.6,-4.69347552800001));
#178203=CARTESIAN_POINT('Ctrl Pts',(9.70569232299994,15.2,-4.69171926800001));
#178204=CARTESIAN_POINT('Ctrl Pts',(9.70569232299994,11.6,-4.69171926800002));
#178205=CARTESIAN_POINT('Ctrl Pts',(9.70376629399994,15.2,-4.68996867700001));
#178206=CARTESIAN_POINT('Ctrl Pts',(9.70376629399994,11.6,-4.68996867700001));
#178207=CARTESIAN_POINT('Ctrl Pts',(9.70184321499995,15.2,-4.68822375800002));
#178208=CARTESIAN_POINT('Ctrl Pts',(9.70184321499995,11.6,-4.68822375800002));
#178209=CARTESIAN_POINT('Ctrl Pts',(9.69992310199994,15.2,-4.68648450800002));
#178210=CARTESIAN_POINT('Ctrl Pts',(9.69992310199994,11.6,-4.68648450800002));
#178211=CARTESIAN_POINT('Ctrl Pts',(9.69800596699995,15.2,-4.68475093300002));
#178212=CARTESIAN_POINT('Ctrl Pts',(9.69800596699995,11.6,-4.68475093300002));
#178213=CARTESIAN_POINT('Ctrl Pts',(9.69609182599994,15.2,-4.68302303000002));
#178214=CARTESIAN_POINT('Ctrl Pts',(9.69609182599994,11.6,-4.68302303000002));
#178215=CARTESIAN_POINT('Ctrl Pts',(9.69418069299994,15.2,-4.68130080300002));
#178216=CARTESIAN_POINT('Ctrl Pts',(9.69418069299994,11.6,-4.68130080300002));
#178217=CARTESIAN_POINT('Ctrl Pts',(9.69227258299994,15.2,-4.67958425200001));
#178218=CARTESIAN_POINT('Ctrl Pts',(9.69227258299994,11.6,-4.67958425200001));
#178219=CARTESIAN_POINT('Ctrl Pts',(9.69036750899994,15.2,-4.67787337800001));
#178220=CARTESIAN_POINT('Ctrl Pts',(9.69036750899994,11.6,-4.67787337800001));
#178221=CARTESIAN_POINT('Ctrl Pts',(9.68846548899995,15.2,-4.67616818100002));
#178222=CARTESIAN_POINT('Ctrl Pts',(9.68846548899995,11.6,-4.67616818100002));
#178223=CARTESIAN_POINT('Ctrl Pts',(9.68656653499995,15.2,-4.67446866300001));
#178224=CARTESIAN_POINT('Ctrl Pts',(9.68656653499995,11.6,-4.67446866300001));
#178225=CARTESIAN_POINT('Ctrl Pts',(9.68467066399995,15.2,-4.67277482500001));
#178226=CARTESIAN_POINT('Ctrl Pts',(9.68467066399995,11.6,-4.67277482500002));
#178227=CARTESIAN_POINT('Ctrl Pts',(9.68277788899995,15.2,-4.67108666800002));
#178228=CARTESIAN_POINT('Ctrl Pts',(9.68277788899995,11.6,-4.67108666800002));
#178229=CARTESIAN_POINT('Ctrl Pts',(9.68088822599995,15.2,-4.66940419300002));
#178230=CARTESIAN_POINT('Ctrl Pts',(9.68088822599995,11.6,-4.66940419300002));
#178231=CARTESIAN_POINT('Ctrl Pts',(9.67900168899994,15.2,-4.66772740200001));
#178232=CARTESIAN_POINT('Ctrl Pts',(9.67900168899994,11.6,-4.66772740200002));
#178233=CARTESIAN_POINT('Ctrl Pts',(9.67711829399994,15.2,-4.66605629400001));
#178234=CARTESIAN_POINT('Ctrl Pts',(9.67711829399994,11.6,-4.66605629400001));
#178235=CARTESIAN_POINT('Ctrl Pts',(9.67523805399994,15.2,-4.66439087100001));
#178236=CARTESIAN_POINT('Ctrl Pts',(9.67523805399994,11.6,-4.66439087100001));
#178237=CARTESIAN_POINT('Ctrl Pts',(9.67336098799995,15.2,-4.66273113300002));
#178238=CARTESIAN_POINT('Ctrl Pts',(9.67336098799995,11.6,-4.66273113300002));
#178239=CARTESIAN_POINT('Ctrl Pts',(9.67148710599995,15.2,-4.66107708200001));
#178240=CARTESIAN_POINT('Ctrl Pts',(9.67148710599995,11.6,-4.66107708200001));
#178241=CARTESIAN_POINT('Ctrl Pts',(9.66961642799994,15.2,-4.65942871900001));
#178242=CARTESIAN_POINT('Ctrl Pts',(9.66961642799994,11.6,-4.65942871900001));
#178243=CARTESIAN_POINT('Ctrl Pts',(9.66774896599994,15.2,-4.65778604500001));
#178244=CARTESIAN_POINT('Ctrl Pts',(9.66774896599994,11.6,-4.65778604500002));
#178245=CARTESIAN_POINT('Ctrl Pts',(9.66588473599994,15.2,-4.65614906000001));
#178246=CARTESIAN_POINT('Ctrl Pts',(9.66588473599994,11.6,-4.65614906000001));
#178247=CARTESIAN_POINT('Ctrl Pts',(9.66402375299995,15.2,-4.65451776500001));
#178248=CARTESIAN_POINT('Ctrl Pts',(9.66402375299995,11.6,-4.65451776500002));
#178249=CARTESIAN_POINT('Ctrl Pts',(9.66216603399995,15.2,-4.65289216300001));
#178250=CARTESIAN_POINT('Ctrl Pts',(9.66216603399995,11.6,-4.65289216300001));
#178251=CARTESIAN_POINT('Ctrl Pts',(9.66031159299994,15.2,-4.65127225200002));
#178252=CARTESIAN_POINT('Ctrl Pts',(9.66031159299994,11.6,-4.65127225200002));
#178253=CARTESIAN_POINT('Ctrl Pts',(9.65846044499994,15.2,-4.64965803400001));
#178254=CARTESIAN_POINT('Ctrl Pts',(9.65846044499994,11.6,-4.64965803400002));
#178255=CARTESIAN_POINT('Ctrl Pts',(9.65661260499994,15.2,-4.64804951100001));
#178256=CARTESIAN_POINT('Ctrl Pts',(9.65661260499994,11.6,-4.64804951100002));
#178257=CARTESIAN_POINT('Ctrl Pts',(9.65476809099994,15.2,-4.64644668200001));
#178258=CARTESIAN_POINT('Ctrl Pts',(9.65476809099994,11.6,-4.64644668200001));
#178259=CARTESIAN_POINT('Ctrl Pts',(9.65292691699995,15.2,-4.64484954900001));
#178260=CARTESIAN_POINT('Ctrl Pts',(9.65292691699995,11.6,-4.64484954900002));
#178261=CARTESIAN_POINT('Ctrl Pts',(9.65108909699994,15.2,-4.64325811300002));
#178262=CARTESIAN_POINT('Ctrl Pts',(9.65108909699994,11.6,-4.64325811300002));
#178263=CARTESIAN_POINT('Ctrl Pts',(9.64925464999994,15.2,-4.64167237400002));
#178264=CARTESIAN_POINT('Ctrl Pts',(9.64925464999994,11.6,-4.64167237400002));
#178265=CARTESIAN_POINT('Ctrl Pts',(9.64742358899995,15.2,-4.64009233400001));
#178266=CARTESIAN_POINT('Ctrl Pts',(9.64742358899995,11.6,-4.64009233400002));
#178267=CARTESIAN_POINT('Ctrl Pts',(9.64559592999995,15.2,-4.63851799300001));
#178268=CARTESIAN_POINT('Ctrl Pts',(9.64559592999995,11.6,-4.63851799300001));
#178269=CARTESIAN_POINT('Ctrl Pts',(9.64377168999994,15.2,-4.63694935100001));
#178270=CARTESIAN_POINT('Ctrl Pts',(9.64377168999994,11.6,-4.63694935100001));
#178271=CARTESIAN_POINT('Ctrl Pts',(9.64195088399994,15.2,-4.63538641000001));
#178272=CARTESIAN_POINT('Ctrl Pts',(9.64195088399994,11.6,-4.63538641000001));
#178273=CARTESIAN_POINT('Ctrl Pts',(9.64013352699994,15.2,-4.63382917200001));
#178274=CARTESIAN_POINT('Ctrl Pts',(9.64013352699994,11.6,-4.63382917200002));
#178275=CARTESIAN_POINT('Ctrl Pts',(9.63831963699995,15.2,-4.63227763600001));
#178276=CARTESIAN_POINT('Ctrl Pts',(9.63831963699995,11.6,-4.63227763600001));
#178277=CARTESIAN_POINT('Ctrl Pts',(9.63650922799994,15.2,-4.63073180200002));
#178278=CARTESIAN_POINT('Ctrl Pts',(9.63650922799994,11.6,-4.63073180200002));
#178279=CARTESIAN_POINT('Ctrl Pts',(9.63470231799995,15.2,-4.62919167300001));
#178280=CARTESIAN_POINT('Ctrl Pts',(9.63470231799995,11.6,-4.62919167300001));
#178281=CARTESIAN_POINT('Ctrl Pts',(9.63289892099995,15.2,-4.62765724900001));
#178282=CARTESIAN_POINT('Ctrl Pts',(9.63289892099995,11.6,-4.62765724900002));
#178283=CARTESIAN_POINT('Ctrl Pts',(9.63109905299994,15.2,-4.62612853000001));
#178284=CARTESIAN_POINT('Ctrl Pts',(9.63109905299994,11.6,-4.62612853000001));
#178285=CARTESIAN_POINT('Ctrl Pts',(9.62930273199994,15.2,-4.62460551700001));
#178286=CARTESIAN_POINT('Ctrl Pts',(9.62930273199994,11.6,-4.62460551700001));
#178287=CARTESIAN_POINT('Ctrl Pts',(9.62750997299995,15.2,-4.62308821200001));
#178288=CARTESIAN_POINT('Ctrl Pts',(9.62750997299995,11.6,-4.62308821200002));
#178289=CARTESIAN_POINT('Ctrl Pts',(9.62572079199994,15.2,-4.62157661300001));
#178290=CARTESIAN_POINT('Ctrl Pts',(9.62572079199994,11.6,-4.62157661300001));
#178291=CARTESIAN_POINT('Ctrl Pts',(9.62393520599995,15.2,-4.62007072400001));
#178292=CARTESIAN_POINT('Ctrl Pts',(9.62393520599995,11.6,-4.62007072400001));
#178293=CARTESIAN_POINT('Ctrl Pts',(9.62215323099995,15.2,-4.61857054400001));
#178294=CARTESIAN_POINT('Ctrl Pts',(9.62215323099995,11.6,-4.61857054400001));
#178295=CARTESIAN_POINT('Ctrl Pts',(9.62037488299995,15.2,-4.61707607400001));
#178296=CARTESIAN_POINT('Ctrl Pts',(9.62037488299995,11.6,-4.61707607400002));
#178297=CARTESIAN_POINT('Ctrl Pts',(9.61860017899994,15.2,-4.61558731400002));
#178298=CARTESIAN_POINT('Ctrl Pts',(9.61860017899994,11.6,-4.61558731400002));
#178299=CARTESIAN_POINT('Ctrl Pts',(9.61682913599994,15.2,-4.61410426600001));
#178300=CARTESIAN_POINT('Ctrl Pts',(9.61682913599994,11.6,-4.61410426600002));
#178301=CARTESIAN_POINT('Ctrl Pts',(9.61506176799995,15.2,-4.61262692900001));
#178302=CARTESIAN_POINT('Ctrl Pts',(9.61506176799995,11.6,-4.61262692900002));
#178303=CARTESIAN_POINT('Ctrl Pts',(9.61329809399994,15.2,-4.61115530500001));
#178304=CARTESIAN_POINT('Ctrl Pts',(9.61329809399994,11.6,-4.61115530500001));
#178305=CARTESIAN_POINT('Ctrl Pts',(9.61153812999994,15.2,-4.60968939500002));
#178306=CARTESIAN_POINT('Ctrl Pts',(9.61153812999994,11.6,-4.60968939500002));
#178307=CARTESIAN_POINT('Ctrl Pts',(9.60978189399994,15.2,-4.60822919900002));
#178308=CARTESIAN_POINT('Ctrl Pts',(9.60978189399994,11.6,-4.60822919900002));
#178309=CARTESIAN_POINT('Ctrl Pts',(9.60802939899994,15.2,-4.60677471700001));
#178310=CARTESIAN_POINT('Ctrl Pts',(9.60802939899994,11.6,-4.60677471700001));
#178311=CARTESIAN_POINT('Ctrl Pts',(9.60628066499994,15.2,-4.60532595000001));
#178312=CARTESIAN_POINT('Ctrl Pts',(9.60628066499994,11.6,-4.60532595000002));
#178313=CARTESIAN_POINT('Ctrl Pts',(9.60453570799995,15.2,-4.60388290000001));
#178314=CARTESIAN_POINT('Ctrl Pts',(9.60453570799995,11.6,-4.60388290000001));
#178315=CARTESIAN_POINT('Ctrl Pts',(9.60279454499995,15.2,-4.60244556600002));
#178316=CARTESIAN_POINT('Ctrl Pts',(9.60279454499995,11.6,-4.60244556600002));
#178317=CARTESIAN_POINT('Ctrl Pts',(9.60105719199994,15.2,-4.60101394900001));
#178318=CARTESIAN_POINT('Ctrl Pts',(9.60105719199994,11.6,-4.60101394900002));
#178319=CARTESIAN_POINT('Ctrl Pts',(9.59932366799995,15.2,-4.59958805000001));
#178320=CARTESIAN_POINT('Ctrl Pts',(9.59932366799995,11.6,-4.59958805000001));
#178321=CARTESIAN_POINT('Ctrl Pts',(9.59759398799994,15.2,-4.59816786900001));
#178322=CARTESIAN_POINT('Ctrl Pts',(9.59759398799994,11.6,-4.59816786900001));
#178323=CARTESIAN_POINT('Ctrl Pts',(9.59586816799994,15.2,-4.59675340600001));
#178324=CARTESIAN_POINT('Ctrl Pts',(9.59586816799994,11.6,-4.59675340600001));
#178325=CARTESIAN_POINT('Ctrl Pts',(9.59414622799994,15.2,-4.59534466400001));
#178326=CARTESIAN_POINT('Ctrl Pts',(9.59414622799994,11.6,-4.59534466400001));
#178327=CARTESIAN_POINT('Ctrl Pts',(9.59242818399994,15.2,-4.59394164100001));
#178328=CARTESIAN_POINT('Ctrl Pts',(9.59242818399994,11.6,-4.59394164100001));
#178329=CARTESIAN_POINT('Ctrl Pts',(9.59071405399994,15.2,-4.59254433900002));
#178330=CARTESIAN_POINT('Ctrl Pts',(9.59071405399994,11.6,-4.59254433900002));
#178331=CARTESIAN_POINT('Ctrl Pts',(9.58900385399994,15.2,-4.59115275800002));
#178332=CARTESIAN_POINT('Ctrl Pts',(9.58900385399994,11.6,-4.59115275800002));
#178333=CARTESIAN_POINT('Ctrl Pts',(9.58729760199994,15.2,-4.58976689800001));
#178334=CARTESIAN_POINT('Ctrl Pts',(9.58729760199994,11.6,-4.58976689800001));
#178335=CARTESIAN_POINT('Ctrl Pts',(9.58559531499995,15.2,-4.58838676100001));
#178336=CARTESIAN_POINT('Ctrl Pts',(9.58559531499995,11.6,-4.58838676100001));
#178337=CARTESIAN_POINT('Ctrl Pts',(9.58389701199994,15.2,-4.58701234700001));
#178338=CARTESIAN_POINT('Ctrl Pts',(9.58389701199994,11.6,-4.58701234700001));
#178339=CARTESIAN_POINT('Ctrl Pts',(9.58220270699995,15.2,-4.58564365500001));
#178340=CARTESIAN_POINT('Ctrl Pts',(9.58220270699995,11.6,-4.58564365500001));
#178341=CARTESIAN_POINT('Ctrl Pts',(9.58051242199994,15.2,-4.58428068800002));
#178342=CARTESIAN_POINT('Ctrl Pts',(9.58051242199994,11.6,-4.58428068800002));
#178343=CARTESIAN_POINT('Ctrl Pts',(9.57882617099994,15.2,-4.58292344400002));
#178344=CARTESIAN_POINT('Ctrl Pts',(9.57882617099994,11.6,-4.58292344400002));
#178345=CARTESIAN_POINT('Ctrl Pts',(9.57714397399995,15.2,-4.58157192400002));
#178346=CARTESIAN_POINT('Ctrl Pts',(9.57714397399995,11.6,-4.58157192400002));
#178347=CARTESIAN_POINT('Ctrl Pts',(9.57546584599994,15.2,-4.58022613000002));
#178348=CARTESIAN_POINT('Ctrl Pts',(9.57546584599994,11.6,-4.58022613000002));
#178349=CARTESIAN_POINT('Ctrl Pts',(9.57379180899995,15.2,-4.57888606200001));
#178350=CARTESIAN_POINT('Ctrl Pts',(9.57379180899995,11.6,-4.57888606200001));
#178351=CARTESIAN_POINT('Ctrl Pts',(9.57212187699995,15.2,-4.57755172000001));
#178352=CARTESIAN_POINT('Ctrl Pts',(9.57212187699995,11.6,-4.57755172000002));
#178353=CARTESIAN_POINT('Ctrl Pts',(9.57045606999994,15.2,-4.57622310400001));
#178354=CARTESIAN_POINT('Ctrl Pts',(9.57045606999994,11.6,-4.57622310400002));
#178355=CARTESIAN_POINT('Ctrl Pts',(9.56879440599995,15.2,-4.57490021400002));
#178356=CARTESIAN_POINT('Ctrl Pts',(9.56879440599995,11.6,-4.57490021400002));
#178357=CARTESIAN_POINT('Ctrl Pts',(9.56713690099994,15.2,-4.57358305200001));
#178358=CARTESIAN_POINT('Ctrl Pts',(9.56713690099994,11.6,-4.57358305200002));
#178359=CARTESIAN_POINT('Ctrl Pts',(9.56548357399994,15.2,-4.57227161800001));
#178360=CARTESIAN_POINT('Ctrl Pts',(9.56548357399994,11.6,-4.57227161800002));
#178361=CARTESIAN_POINT('Ctrl Pts',(9.56383444399994,15.2,-4.57096591100001));
#178362=CARTESIAN_POINT('Ctrl Pts',(9.56383444399994,11.6,-4.57096591100001));
#178363=CARTESIAN_POINT('Ctrl Pts',(9.56218952899994,15.2,-4.56966593300002));
#178364=CARTESIAN_POINT('Ctrl Pts',(9.56218952899994,11.6,-4.56966593300002));
#178365=CARTESIAN_POINT('Ctrl Pts',(9.56054884799994,15.2,-4.56837168300002));
#178366=CARTESIAN_POINT('Ctrl Pts',(9.56054884799994,11.6,-4.56837168300002));
#178367=CARTESIAN_POINT('Ctrl Pts',(9.55891241699995,15.2,-4.56708316300002));
#178368=CARTESIAN_POINT('Ctrl Pts',(9.55891241699995,11.6,-4.56708316300002));
#178369=CARTESIAN_POINT('Ctrl Pts',(9.55728025499995,15.2,-4.56580037200002));
#178370=CARTESIAN_POINT('Ctrl Pts',(9.55728025499995,11.6,-4.56580037200002));
#178371=CARTESIAN_POINT('Ctrl Pts',(9.55565238299994,15.2,-4.56452331000001));
#178372=CARTESIAN_POINT('Ctrl Pts',(9.55565238299994,11.6,-4.56452331000001));
#178373=CARTESIAN_POINT('Ctrl Pts',(9.55402881599994,15.2,-4.56325197900001));
#178374=CARTESIAN_POINT('Ctrl Pts',(9.55402881599994,11.6,-4.56325197900001));
#178375=CARTESIAN_POINT('Ctrl Pts',(9.55240957399995,15.2,-4.56198637800002));
#178376=CARTESIAN_POINT('Ctrl Pts',(9.55240957399995,11.6,-4.56198637800002));
#178377=CARTESIAN_POINT('Ctrl Pts',(9.55079467599995,15.2,-4.56072650800001));
#178378=CARTESIAN_POINT('Ctrl Pts',(9.55079467599995,11.6,-4.56072650800001));
#178379=CARTESIAN_POINT('Ctrl Pts',(9.54918413999994,15.2,-4.55947236900001));
#178380=CARTESIAN_POINT('Ctrl Pts',(9.54918413999994,11.6,-4.55947236900002));
#178381=CARTESIAN_POINT('Ctrl Pts',(9.54757798599994,15.2,-4.55822396200002));
#178382=CARTESIAN_POINT('Ctrl Pts',(9.54757798599994,11.6,-4.55822396200002));
#178383=CARTESIAN_POINT('Ctrl Pts',(9.54597623199994,15.2,-4.55698128600002));
#178384=CARTESIAN_POINT('Ctrl Pts',(9.54597623199994,11.6,-4.55698128600002));
#178385=CARTESIAN_POINT('Ctrl Pts',(9.54437889599994,15.2,-4.55574434100001));
#178386=CARTESIAN_POINT('Ctrl Pts',(9.54437889599994,11.6,-4.55574434100001));
#178387=CARTESIAN_POINT('Ctrl Pts',(9.54278599799995,15.2,-4.55451312900002));
#178388=CARTESIAN_POINT('Ctrl Pts',(9.54278599799995,11.6,-4.55451312900002));
#178389=CARTESIAN_POINT('Ctrl Pts',(9.54119755599995,15.2,-4.55328764900001));
#178390=CARTESIAN_POINT('Ctrl Pts',(9.54119755599995,11.6,-4.55328764900001));
#178391=CARTESIAN_POINT('Ctrl Pts',(9.53961358999995,15.2,-4.55206790100001));
#178392=CARTESIAN_POINT('Ctrl Pts',(9.53961358999995,11.6,-4.55206790100002));
#178393=CARTESIAN_POINT('Ctrl Pts',(9.53803411899995,15.2,-4.55085388600001));
#178394=CARTESIAN_POINT('Ctrl Pts',(9.53803411899995,11.6,-4.55085388600002));
#178395=CARTESIAN_POINT('Ctrl Pts',(9.53645916199994,15.2,-4.54964560500001));
#178396=CARTESIAN_POINT('Ctrl Pts',(9.53645916199994,11.6,-4.54964560500002));
#178397=CARTESIAN_POINT('Ctrl Pts',(9.53488873799994,15.2,-4.54844305600002));
#178398=CARTESIAN_POINT('Ctrl Pts',(9.53488873799994,11.6,-4.54844305600002));
#178399=CARTESIAN_POINT('Ctrl Pts',(9.53332286699995,15.2,-4.54724624000002));
#178400=CARTESIAN_POINT('Ctrl Pts',(9.53332286699995,11.6,-4.54724624000002));
#178401=CARTESIAN_POINT('Ctrl Pts',(9.53176156699995,15.2,-4.54605515800001));
#178402=CARTESIAN_POINT('Ctrl Pts',(9.53176156699995,11.6,-4.54605515800001));
#178403=CARTESIAN_POINT('Ctrl Pts',(9.53020485899994,15.2,-4.54486981000001));
#178404=CARTESIAN_POINT('Ctrl Pts',(9.53020485899994,11.6,-4.54486981000001));
#178405=CARTESIAN_POINT('Ctrl Pts',(9.52865276099994,15.2,-4.54369019500001));
#178406=CARTESIAN_POINT('Ctrl Pts',(9.52865276099994,11.6,-4.54369019500002));
#178407=CARTESIAN_POINT('Ctrl Pts',(9.52710529499995,15.2,-4.54251631400002));
#178408=CARTESIAN_POINT('Ctrl Pts',(9.52710529499995,11.6,-4.54251631400002));
#178409=CARTESIAN_POINT('Ctrl Pts',(9.52556247699994,15.2,-4.54134816700002));
#178410=CARTESIAN_POINT('Ctrl Pts',(9.52556247699994,11.6,-4.54134816700002));
#178411=CARTESIAN_POINT('Ctrl Pts',(9.52402432899994,15.2,-4.54018575400001));
#178412=CARTESIAN_POINT('Ctrl Pts',(9.52402432899994,11.6,-4.54018575400002));
#178413=CARTESIAN_POINT('Ctrl Pts',(9.52249087199995,15.2,-4.53902907500002));
#178414=CARTESIAN_POINT('Ctrl Pts',(9.52249087199995,11.6,-4.53902907500002));
#178415=CARTESIAN_POINT('Ctrl Pts',(9.52096212299995,15.2,-4.53787813200002));
#178416=CARTESIAN_POINT('Ctrl Pts',(9.52096212299995,11.6,-4.53787813200002));
#178417=CARTESIAN_POINT('Ctrl Pts',(9.51943810399994,15.2,-4.53673292200001));
#178418=CARTESIAN_POINT('Ctrl Pts',(9.51943810399994,11.6,-4.53673292200001));
#178419=CARTESIAN_POINT('Ctrl Pts',(9.51791883399994,15.2,-4.53559344600002));
#178420=CARTESIAN_POINT('Ctrl Pts',(9.51791883399994,11.6,-4.53559344600002));
#178421=CARTESIAN_POINT('Ctrl Pts',(9.51640433299995,15.2,-4.53445970600002));
#178422=CARTESIAN_POINT('Ctrl Pts',(9.51640433299995,11.6,-4.53445970600002));
#178423=CARTESIAN_POINT('Ctrl Pts',(9.51489462199994,15.2,-4.53333169900001));
#178424=CARTESIAN_POINT('Ctrl Pts',(9.51489462199994,11.6,-4.53333169900001));
#178425=CARTESIAN_POINT('Ctrl Pts',(9.51338971899995,15.2,-4.53220942700002));
#178426=CARTESIAN_POINT('Ctrl Pts',(9.51338971899995,11.6,-4.53220942700002));
#178427=CARTESIAN_POINT('Ctrl Pts',(9.51188964699995,15.2,-4.53109288900002));
#178428=CARTESIAN_POINT('Ctrl Pts',(9.51188964699995,11.6,-4.53109288900002));
#178429=CARTESIAN_POINT('Ctrl Pts',(9.51039442599994,15.2,-4.52998208700001));
#178430=CARTESIAN_POINT('Ctrl Pts',(9.51039442599994,11.6,-4.52998208700001));
#178431=CARTESIAN_POINT('Ctrl Pts',(9.50890407399994,15.2,-4.52887701800002));
#178432=CARTESIAN_POINT('Ctrl Pts',(9.50890407399994,11.6,-4.52887701800002));
#178433=CARTESIAN_POINT('Ctrl Pts',(9.50741861299995,15.2,-4.52777768500002));
#178434=CARTESIAN_POINT('Ctrl Pts',(9.50741861299995,11.6,-4.52777768500002));
#178435=CARTESIAN_POINT('Ctrl Pts',(9.50593806399995,15.2,-4.52668408600001));
#178436=CARTESIAN_POINT('Ctrl Pts',(9.50593806399995,11.6,-4.52668408600002));
#178437=CARTESIAN_POINT('Ctrl Pts',(9.50446244799994,15.2,-4.52559622000001));
#178438=CARTESIAN_POINT('Ctrl Pts',(9.50446244799994,11.6,-4.52559622000001));
#178439=CARTESIAN_POINT('Ctrl Pts',(9.50299178499994,15.2,-4.52451409000002));
#178440=CARTESIAN_POINT('Ctrl Pts',(9.50299178499994,11.6,-4.52451409000002));
#178441=CARTESIAN_POINT('Ctrl Pts',(9.50152609399994,15.2,-4.52343769300001));
#178442=CARTESIAN_POINT('Ctrl Pts',(9.50152609399994,11.6,-4.52343769300002));
#178443=CARTESIAN_POINT('Ctrl Pts',(9.50006539899995,15.2,-4.52236703200001));
#178444=CARTESIAN_POINT('Ctrl Pts',(9.50006539899995,11.6,-4.52236703200002));
#178445=CARTESIAN_POINT('Ctrl Pts',(9.49860971899994,15.2,-4.52130210400002));
#178446=CARTESIAN_POINT('Ctrl Pts',(9.49860971899994,11.6,-4.52130210400002));
#178447=CARTESIAN_POINT('Ctrl Pts',(9.49715907499994,15.2,-4.52024291000001));
#178448=CARTESIAN_POINT('Ctrl Pts',(9.49715907499994,11.6,-4.52024291000001));
#178449=CARTESIAN_POINT('Ctrl Pts',(9.49571348799994,15.2,-4.51918944900001));
#178450=CARTESIAN_POINT('Ctrl Pts',(9.49571348799994,11.6,-4.51918944900001));
#178451=CARTESIAN_POINT('Ctrl Pts',(9.49427298099994,15.2,-4.51814172300002));
#178452=CARTESIAN_POINT('Ctrl Pts',(9.49427298099994,11.6,-4.51814172300002));
#178453=CARTESIAN_POINT('Ctrl Pts',(9.49283757399994,15.2,-4.51709973000002));
#178454=CARTESIAN_POINT('Ctrl Pts',(9.49283757399994,11.6,-4.51709973000002));
#178455=CARTESIAN_POINT('Ctrl Pts',(9.49140728699994,15.2,-4.51606347000002));
#178456=CARTESIAN_POINT('Ctrl Pts',(9.49140728699994,11.6,-4.51606347000002));
#178457=CARTESIAN_POINT('Ctrl Pts',(9.48998214199994,15.2,-4.51503294400001));
#178458=CARTESIAN_POINT('Ctrl Pts',(9.48998214199994,11.6,-4.51503294400002));
#178459=CARTESIAN_POINT('Ctrl Pts',(9.48856216199994,15.2,-4.51400815100001));
#178460=CARTESIAN_POINT('Ctrl Pts',(9.48856216199994,11.6,-4.51400815100001));
#178461=CARTESIAN_POINT('Ctrl Pts',(9.48714736699995,15.2,-4.51298909100001));
#178462=CARTESIAN_POINT('Ctrl Pts',(9.48714736699995,11.6,-4.51298909100002));
#178463=CARTESIAN_POINT('Ctrl Pts',(9.48573777999994,15.2,-4.51197576300002));
#178464=CARTESIAN_POINT('Ctrl Pts',(9.48573777999994,11.6,-4.51197576300002));
#178465=CARTESIAN_POINT('Ctrl Pts',(9.48433342199994,15.2,-4.51096816700002));
#178466=CARTESIAN_POINT('Ctrl Pts',(9.48433342199994,11.6,-4.51096816700002));
#178467=CARTESIAN_POINT('Ctrl Pts',(9.48293431399994,15.2,-4.50996630300001));
#178468=CARTESIAN_POINT('Ctrl Pts',(9.48293431399994,11.6,-4.50996630300002));
#178469=CARTESIAN_POINT('Ctrl Pts',(9.48154047899994,15.2,-4.50897017200001));
#178470=CARTESIAN_POINT('Ctrl Pts',(9.48154047899994,11.6,-4.50897017200001));
#178471=CARTESIAN_POINT('Ctrl Pts',(9.48015193699994,15.2,-4.50797977200001));
#178472=CARTESIAN_POINT('Ctrl Pts',(9.48015193699994,11.6,-4.50797977200002));
#178473=CARTESIAN_POINT('Ctrl Pts',(9.47876871299994,15.2,-4.50699510200002));
#178474=CARTESIAN_POINT('Ctrl Pts',(9.47876871299994,11.6,-4.50699510200002));
#178475=CARTESIAN_POINT('Ctrl Pts',(9.47739082699995,15.2,-4.50601616500002));
#178476=CARTESIAN_POINT('Ctrl Pts',(9.47739082699995,11.6,-4.50601616500002));
#178477=CARTESIAN_POINT('Ctrl Pts',(9.47601830199994,15.2,-4.50504295800001));
#178478=CARTESIAN_POINT('Ctrl Pts',(9.47601830199994,11.6,-4.50504295800001));
#178479=CARTESIAN_POINT('Ctrl Pts',(9.47465115999995,15.2,-4.50407548100001));
#178480=CARTESIAN_POINT('Ctrl Pts',(9.47465115999995,11.6,-4.50407548100001));
#178481=CARTESIAN_POINT('Ctrl Pts',(9.47328942199994,15.2,-4.50311373400002));
#178482=CARTESIAN_POINT('Ctrl Pts',(9.47328942199994,11.6,-4.50311373400002));
#178483=CARTESIAN_POINT('Ctrl Pts',(9.47193311299994,15.2,-4.50215771600002));
#178484=CARTESIAN_POINT('Ctrl Pts',(9.47193311299994,11.6,-4.50215771600002));
#178485=CARTESIAN_POINT('Ctrl Pts',(9.47058225499994,15.2,-4.50120742900001));
#178486=CARTESIAN_POINT('Ctrl Pts',(9.47058225499994,11.6,-4.50120742900001));
#178487=CARTESIAN_POINT('Ctrl Pts',(9.46923686899994,15.2,-4.50026286900002));
#178488=CARTESIAN_POINT('Ctrl Pts',(9.46923686899994,11.6,-4.50026286900002));
#178489=CARTESIAN_POINT('Ctrl Pts',(9.46789697899994,15.2,-4.49932403800001));
#178490=CARTESIAN_POINT('Ctrl Pts',(9.46789697899994,11.6,-4.49932403800002));
#178491=CARTESIAN_POINT('Ctrl Pts',(9.46656260799994,15.2,-4.49839093600001));
#178492=CARTESIAN_POINT('Ctrl Pts',(9.46656260799994,11.6,-4.49839093600001));
#178493=CARTESIAN_POINT('Ctrl Pts',(9.46523377699994,15.2,-4.49746356000002));
#178494=CARTESIAN_POINT('Ctrl Pts',(9.46523377699994,11.6,-4.49746356000002));
#178495=CARTESIAN_POINT('Ctrl Pts',(9.46391051099994,15.2,-4.49654191200001));
#178496=CARTESIAN_POINT('Ctrl Pts',(9.46391051099994,11.6,-4.49654191200001));
#178497=CARTESIAN_POINT('Ctrl Pts',(9.46259283199995,15.2,-4.49562599100001));
#178498=CARTESIAN_POINT('Ctrl Pts',(9.46259283199995,11.6,-4.49562599100001));
#178499=CARTESIAN_POINT('Ctrl Pts',(9.46128076299994,15.2,-4.49471579600001));
#178500=CARTESIAN_POINT('Ctrl Pts',(9.46128076299994,11.6,-4.49471579600001));
#178501=CARTESIAN_POINT('Ctrl Pts',(9.45997432899994,15.2,-4.49381132600001));
#178502=CARTESIAN_POINT('Ctrl Pts',(9.45997432899994,11.6,-4.49381132600002));
#178503=CARTESIAN_POINT('Ctrl Pts',(9.45867355199994,15.2,-4.49291258200001));
#178504=CARTESIAN_POINT('Ctrl Pts',(9.45867355199994,11.6,-4.49291258200002));
#178505=CARTESIAN_POINT('Ctrl Pts',(9.45737845499995,15.2,-4.49201956300001));
#178506=CARTESIAN_POINT('Ctrl Pts',(9.45737845499995,11.6,-4.49201956300001));
#178507=CARTESIAN_POINT('Ctrl Pts',(9.45608906199995,15.2,-4.49113226700002));
#178508=CARTESIAN_POINT('Ctrl Pts',(9.45608906199995,11.6,-4.49113226700002));
#178509=CARTESIAN_POINT('Ctrl Pts',(9.45480539699994,15.2,-4.49025069500002));
#178510=CARTESIAN_POINT('Ctrl Pts',(9.45480539699994,11.6,-4.49025069500002));
#178511=CARTESIAN_POINT('Ctrl Pts',(9.45352748199995,15.2,-4.48937484700001));
#178512=CARTESIAN_POINT('Ctrl Pts',(9.45352748199995,11.6,-4.48937484700001));
#178513=CARTESIAN_POINT('Ctrl Pts',(9.45225534299994,15.2,-4.48850472100002));
#178514=CARTESIAN_POINT('Ctrl Pts',(9.45225534299994,11.6,-4.48850472100002));
#178515=CARTESIAN_POINT('Ctrl Pts',(9.45098900299995,15.2,-4.48764031700001));
#178516=CARTESIAN_POINT('Ctrl Pts',(9.45098900299995,11.6,-4.48764031700002));
#178517=CARTESIAN_POINT('Ctrl Pts',(9.44972848499994,15.2,-4.48678163300002));
#178518=CARTESIAN_POINT('Ctrl Pts',(9.44972848499994,11.6,-4.48678163300002));
#178519=CARTESIAN_POINT('Ctrl Pts',(9.44847381499994,15.2,-4.48592867100002));
#178520=CARTESIAN_POINT('Ctrl Pts',(9.44847381499994,11.6,-4.48592867100002));
#178521=CARTESIAN_POINT('Ctrl Pts',(9.44722501599994,15.2,-4.48508142800002));
#178522=CARTESIAN_POINT('Ctrl Pts',(9.44722501599994,11.6,-4.48508142800002));
#178523=CARTESIAN_POINT('Ctrl Pts',(9.44598211199994,15.2,-4.48423990500002));
#178524=CARTESIAN_POINT('Ctrl Pts',(9.44598211199994,11.6,-4.48423990500002));
#178525=CARTESIAN_POINT('Ctrl Pts',(9.44474512899994,15.2,-4.48340410000001));
#178526=CARTESIAN_POINT('Ctrl Pts',(9.44474512899994,11.6,-4.48340410000002));
#178527=CARTESIAN_POINT('Ctrl Pts',(9.44351408899994,15.2,-4.48257401400001));
#178528=CARTESIAN_POINT('Ctrl Pts',(9.44351408899994,11.6,-4.48257401400001));
#178529=CARTESIAN_POINT('Ctrl Pts',(9.44228901899995,15.2,-4.48174964400001));
#178530=CARTESIAN_POINT('Ctrl Pts',(9.44228901899995,11.6,-4.48174964400002));
#178531=CARTESIAN_POINT('Ctrl Pts',(9.44106994199995,15.2,-4.48093099100001));
#178532=CARTESIAN_POINT('Ctrl Pts',(9.44106994199995,11.6,-4.48093099100001));
#178533=CARTESIAN_POINT('Ctrl Pts',(9.43985688299994,15.2,-4.48011805400002));
#178534=CARTESIAN_POINT('Ctrl Pts',(9.43985688299994,11.6,-4.48011805400002));
#178535=CARTESIAN_POINT('Ctrl Pts',(9.43864986699994,15.2,-4.47931083200002));
#178536=CARTESIAN_POINT('Ctrl Pts',(9.43864986699994,11.6,-4.47931083200002));
#178537=CARTESIAN_POINT('Ctrl Pts',(9.43744891899994,15.2,-4.47850932400002));
#178538=CARTESIAN_POINT('Ctrl Pts',(9.43744891899994,11.6,-4.47850932400002));
#178539=CARTESIAN_POINT('Ctrl Pts',(9.43625406499994,15.2,-4.47771352900002));
#178540=CARTESIAN_POINT('Ctrl Pts',(9.43625406499994,11.6,-4.47771352900002));
#178541=CARTESIAN_POINT('Ctrl Pts',(9.43506532899995,15.2,-4.47692344800001));
#178542=CARTESIAN_POINT('Ctrl Pts',(9.43506532899995,11.6,-4.47692344800002));
#178543=CARTESIAN_POINT('Ctrl Pts',(9.43388273599994,15.2,-4.47613907800001));
#178544=CARTESIAN_POINT('Ctrl Pts',(9.43388273599994,11.6,-4.47613907800002));
#178545=CARTESIAN_POINT('Ctrl Pts',(9.43270631299994,15.2,-4.47536041800001));
#178546=CARTESIAN_POINT('Ctrl Pts',(9.43270631299994,11.6,-4.47536041800001));
#178547=CARTESIAN_POINT('Ctrl Pts',(9.43153608499994,15.2,-4.47458746900002));
#178548=CARTESIAN_POINT('Ctrl Pts',(9.43153608499994,11.6,-4.47458746900002));
#178549=CARTESIAN_POINT('Ctrl Pts',(9.43037207599994,15.2,-4.47382023000001));
#178550=CARTESIAN_POINT('Ctrl Pts',(9.43037207599994,11.6,-4.47382023000001));
#178551=CARTESIAN_POINT('Ctrl Pts',(9.42921431399995,15.2,-4.47305869800001));
#178552=CARTESIAN_POINT('Ctrl Pts',(9.42921431399995,11.6,-4.47305869800002));
#178553=CARTESIAN_POINT('Ctrl Pts',(9.42806282299994,15.2,-4.47230287400001));
#178554=CARTESIAN_POINT('Ctrl Pts',(9.42806282299994,11.6,-4.47230287400001));
#178555=CARTESIAN_POINT('Ctrl Pts',(9.42691762999995,15.2,-4.47155275600001));
#178556=CARTESIAN_POINT('Ctrl Pts',(9.42691762999995,11.6,-4.47155275600002));
#178557=CARTESIAN_POINT('Ctrl Pts',(9.42577875999994,15.2,-4.47080834400001));
#178558=CARTESIAN_POINT('Ctrl Pts',(9.42577875999994,11.6,-4.47080834400001));
#178559=CARTESIAN_POINT('Ctrl Pts',(9.42464624099994,15.2,-4.47006963700002));
#178560=CARTESIAN_POINT('Ctrl Pts',(9.42464624099994,11.6,-4.47006963700002));
#178561=CARTESIAN_POINT('Ctrl Pts',(9.42352009699994,15.2,-4.46933663400001));
#178562=CARTESIAN_POINT('Ctrl Pts',(9.42352009699994,11.6,-4.46933663400001));
#178563=CARTESIAN_POINT('Ctrl Pts',(9.42240035499994,15.2,-4.46860933200002));
#178564=CARTESIAN_POINT('Ctrl Pts',(9.42240035499994,11.6,-4.46860933200002));
#178565=CARTESIAN_POINT('Ctrl Pts',(9.42128704299994,15.2,-4.46788773300002));
#178566=CARTESIAN_POINT('Ctrl Pts',(9.42128704299994,11.6,-4.46788773300002));
#178567=CARTESIAN_POINT('Ctrl Pts',(9.42018018699994,15.2,-4.46717183400001));
#178568=CARTESIAN_POINT('Ctrl Pts',(9.42018018699994,11.6,-4.46717183400002));
#178569=CARTESIAN_POINT('Ctrl Pts',(9.41907981199994,15.2,-4.46646163500001));
#178570=CARTESIAN_POINT('Ctrl Pts',(9.41907981199994,11.6,-4.46646163500002));
#178571=CARTESIAN_POINT('Ctrl Pts',(9.41798594799995,15.2,-4.46575713300001));
#178572=CARTESIAN_POINT('Ctrl Pts',(9.41798594799995,11.6,-4.46575713300002));
#178573=CARTESIAN_POINT('Ctrl Pts',(9.41689861899994,15.2,-4.46505832900002));
#178574=CARTESIAN_POINT('Ctrl Pts',(9.41689861899994,11.6,-4.46505832900002));
#178575=CARTESIAN_POINT('Ctrl Pts',(9.41581785299995,15.2,-4.46436522100001));
#178576=CARTESIAN_POINT('Ctrl Pts',(9.41581785299995,11.6,-4.46436522100001));
#178577=CARTESIAN_POINT('Ctrl Pts',(9.41474367699995,15.2,-4.46367780900002));
#178578=CARTESIAN_POINT('Ctrl Pts',(9.41474367699995,11.6,-4.46367780900002));
#178579=CARTESIAN_POINT('Ctrl Pts',(9.41367611899994,15.2,-4.46299609100001));
#178580=CARTESIAN_POINT('Ctrl Pts',(9.41367611899994,11.6,-4.46299609100001));
#178581=CARTESIAN_POINT('Ctrl Pts',(9.41261520599994,15.2,-4.46232006500002));
#178582=CARTESIAN_POINT('Ctrl Pts',(9.41261520599994,11.6,-4.46232006500002));
#178583=CARTESIAN_POINT('Ctrl Pts',(9.41156096599994,15.2,-4.46164973100001));
#178584=CARTESIAN_POINT('Ctrl Pts',(9.41156096599994,11.6,-4.46164973100002));
#178585=CARTESIAN_POINT('Ctrl Pts',(9.41051342599994,15.2,-4.46098508800001));
#178586=CARTESIAN_POINT('Ctrl Pts',(9.41051342599994,11.6,-4.46098508800001));
#178587=CARTESIAN_POINT('Ctrl Pts',(9.40947261499995,15.2,-4.46032613400002));
#178588=CARTESIAN_POINT('Ctrl Pts',(9.40947261499995,11.6,-4.46032613400002));
#178589=CARTESIAN_POINT('Ctrl Pts',(9.40843855899995,15.2,-4.45967286700002));
#178590=CARTESIAN_POINT('Ctrl Pts',(9.40843855899995,11.6,-4.45967286700002));
#178591=CARTESIAN_POINT('Ctrl Pts',(9.40741128799995,15.2,-4.45902528700001));
#178592=CARTESIAN_POINT('Ctrl Pts',(9.40741128799995,11.6,-4.45902528700001));
#178593=CARTESIAN_POINT('Ctrl Pts',(9.40639082799994,15.2,-4.45838339300002));
#178594=CARTESIAN_POINT('Ctrl Pts',(9.40639082799994,11.6,-4.45838339300002));
#178595=CARTESIAN_POINT('Ctrl Pts',(9.40537720899994,15.2,-4.45774718300001));
#178596=CARTESIAN_POINT('Ctrl Pts',(9.40537720899994,11.6,-4.45774718300001));
#178597=CARTESIAN_POINT('Ctrl Pts',(9.40437045999994,15.2,-4.45711665500002));
#178598=CARTESIAN_POINT('Ctrl Pts',(9.40437045999994,11.6,-4.45711665500002));
#178599=CARTESIAN_POINT('Ctrl Pts',(9.40337060799994,15.2,-4.45649181000002));
#178600=CARTESIAN_POINT('Ctrl Pts',(9.40337060799994,11.6,-4.45649181000002));
#178601=CARTESIAN_POINT('Ctrl Pts',(9.40237768099994,15.2,-4.45587264400002));
#178602=CARTESIAN_POINT('Ctrl Pts',(9.40237768099994,11.6,-4.45587264400002));
#178603=CARTESIAN_POINT('Ctrl Pts',(9.40139171099995,15.2,-4.45525915600001));
#178604=CARTESIAN_POINT('Ctrl Pts',(9.40139171099995,11.6,-4.45525915600001));
#178605=CARTESIAN_POINT('Ctrl Pts',(9.40041272399995,15.2,-4.45465134700001));
#178606=CARTESIAN_POINT('Ctrl Pts',(9.40041272399995,11.6,-4.45465134700001));
#178607=CARTESIAN_POINT('Ctrl Pts',(9.39944075099995,15.2,-4.45404921300002));
#178608=CARTESIAN_POINT('Ctrl Pts',(9.39944075099995,11.6,-4.45404921300002));
#178609=CARTESIAN_POINT('Ctrl Pts',(9.39847581899994,15.2,-4.45345275400001));
#178610=CARTESIAN_POINT('Ctrl Pts',(9.39847581899994,11.6,-4.45345275400001));
#178611=CARTESIAN_POINT('Ctrl Pts',(9.39751795899994,15.2,-4.45286196700001));
#178612=CARTESIAN_POINT('Ctrl Pts',(9.39751795899994,11.6,-4.45286196700002));
#178613=CARTESIAN_POINT('Ctrl Pts',(9.39656720199994,15.2,-4.45227685300001));
#178614=CARTESIAN_POINT('Ctrl Pts',(9.39656720199994,11.6,-4.45227685300001));
#178615=CARTESIAN_POINT('Ctrl Pts',(9.39562357399994,15.2,-4.45169740800001));
#178616=CARTESIAN_POINT('Ctrl Pts',(9.39562357399994,11.6,-4.45169740800001));
#178617=CARTESIAN_POINT('Ctrl Pts',(9.39468710699994,15.2,-4.45112363100002));
#178618=CARTESIAN_POINT('Ctrl Pts',(9.39468710699994,11.6,-4.45112363100002));
#178619=CARTESIAN_POINT('Ctrl Pts',(9.39375783099995,15.2,-4.45055552200001));
#178620=CARTESIAN_POINT('Ctrl Pts',(9.39375783099995,11.6,-4.45055552200001));
#178621=CARTESIAN_POINT('Ctrl Pts',(9.39283577499994,15.2,-4.44999307800002));
#178622=CARTESIAN_POINT('Ctrl Pts',(9.39283577499994,11.6,-4.44999307800002));
#178623=CARTESIAN_POINT('Ctrl Pts',(9.39192097099994,15.2,-4.44943629800001));
#178624=CARTESIAN_POINT('Ctrl Pts',(9.39192097099994,11.6,-4.44943629800001));
#178625=CARTESIAN_POINT('Ctrl Pts',(9.39101344699995,15.2,-4.44888518000001));
#178626=CARTESIAN_POINT('Ctrl Pts',(9.39101344699995,11.6,-4.44888518000001));
#178627=CARTESIAN_POINT('Ctrl Pts',(9.39011323499994,15.2,-4.44833972300001));
#178628=CARTESIAN_POINT('Ctrl Pts',(9.39011323499994,11.6,-4.44833972300002));
#178629=CARTESIAN_POINT('Ctrl Pts',(9.38922036599994,15.2,-4.44779992400001));
#178630=CARTESIAN_POINT('Ctrl Pts',(9.38922036599994,11.6,-4.44779992400001));
#178631=CARTESIAN_POINT('Ctrl Pts',(9.38833486899994,15.2,-4.44726578300001));
#178632=CARTESIAN_POINT('Ctrl Pts',(9.38833486899994,11.6,-4.44726578300001));
#178633=CARTESIAN_POINT('Ctrl Pts',(9.38745677599995,15.2,-4.44673729700002));
#178634=CARTESIAN_POINT('Ctrl Pts',(9.38745677599995,11.6,-4.44673729700002));
#178635=CARTESIAN_POINT('Ctrl Pts',(9.38658611799994,15.2,-4.44621446500001));
#178636=CARTESIAN_POINT('Ctrl Pts',(9.38658611799994,11.6,-4.44621446500001));
#178637=CARTESIAN_POINT('Ctrl Pts',(9.38572292599994,15.2,-4.44569728500001));
#178638=CARTESIAN_POINT('Ctrl Pts',(9.38572292599994,11.6,-4.44569728500001));
#178639=CARTESIAN_POINT('Ctrl Pts',(9.38486723299994,15.2,-4.44518575500001));
#178640=CARTESIAN_POINT('Ctrl Pts',(9.38486723299994,11.6,-4.44518575500001));
#178641=CARTESIAN_POINT('Ctrl Pts',(9.38401906799994,15.2,-4.44467987500001));
#178642=CARTESIAN_POINT('Ctrl Pts',(9.38401906799994,11.6,-4.44467987500001));
#178643=CARTESIAN_POINT('Ctrl Pts',(9.38317846499995,15.2,-4.44417964100001));
#178644=CARTESIAN_POINT('Ctrl Pts',(9.38317846499995,11.6,-4.44417964100001));
#178645=CARTESIAN_POINT('Ctrl Pts',(9.38234545299995,15.2,-4.44368505100002));
#178646=CARTESIAN_POINT('Ctrl Pts',(9.38234545299995,11.6,-4.44368505100002));
#178647=CARTESIAN_POINT('Ctrl Pts',(9.38152006799994,15.2,-4.44319610500001));
#178648=CARTESIAN_POINT('Ctrl Pts',(9.38152006799994,11.6,-4.44319610500001));
#178649=CARTESIAN_POINT('Ctrl Pts',(9.38070233899994,15.2,-4.44271280000001));
#178650=CARTESIAN_POINT('Ctrl Pts',(9.38070233899994,11.6,-4.44271280000002));
#178651=CARTESIAN_POINT('Ctrl Pts',(9.37989229799994,15.2,-4.44223513400001));
#178652=CARTESIAN_POINT('Ctrl Pts',(9.37989229799994,11.6,-4.44223513400001));
#178653=CARTESIAN_POINT('Ctrl Pts',(9.37908997999994,15.2,-4.44176310500001));
#178654=CARTESIAN_POINT('Ctrl Pts',(9.37908997999994,11.6,-4.44176310500001));
#178655=CARTESIAN_POINT('Ctrl Pts',(9.37829999299994,15.2,-4.44129939800002));
#178656=CARTESIAN_POINT('Ctrl Pts',(9.37829999299994,11.6,-4.44129939800002));
#178657=CARTESIAN_POINT('Ctrl Pts',(9.37767505799994,15.2,-4.44093341200002));
#178658=CARTESIAN_POINT('Ctrl Pts',(9.37767505799994,11.6,-4.44093341200002));
#178659=CARTESIAN_POINT('Ctrl Pts',(9.37721094099994,15.2,-4.44066207100001));
#178660=CARTESIAN_POINT('Ctrl Pts',(9.37721094099994,11.6,-4.44066207100002));
#178661=CARTESIAN_POINT('Ctrl Pts',(9.37690455299995,15.2,-4.44048314800002));
#178662=CARTESIAN_POINT('Ctrl Pts',(9.37690455299995,11.6,-4.44048314800002));
#178663=CARTESIAN_POINT('Ctrl Pts',(9.37675396699994,15.2,-4.44039525800001));
#178664=CARTESIAN_POINT('Ctrl Pts',(9.37675396699994,11.6,-4.44039525800001));
#178665=CARTESIAN_POINT('',(9.37675396699994,12.2,-4.44039525800001));
#178666=CARTESIAN_POINT('',(9.37675396699994,15.2,-4.44039525800001));
#178667=CARTESIAN_POINT('',(9.37675396699994,12.2,-4.44039525800001));
#178668=CARTESIAN_POINT('Ctrl Pts',(10.2217148779999,12.2,-5.26939701900002));
#178669=CARTESIAN_POINT('Ctrl Pts',(10.2212575739999,12.2,-5.26878426900002));
#178670=CARTESIAN_POINT('Ctrl Pts',(10.2203429999999,12.2,-5.26755929400001));
#178671=CARTESIAN_POINT('Ctrl Pts',(10.2189712369999,12.2,-5.26572340900001));
#178672=CARTESIAN_POINT('Ctrl Pts',(10.2171424209999,12.2,-5.26327871600001));
#178673=CARTESIAN_POINT('Ctrl Pts',(10.2148567309999,12.2,-5.26022810500002));
#178674=CARTESIAN_POINT('Ctrl Pts',(10.2125713739999,12.2,-5.25718275100001));
#178675=CARTESIAN_POINT('Ctrl Pts',(10.2102863519999,12.2,-5.25414265600002));
#178676=CARTESIAN_POINT('Ctrl Pts',(10.2080016679999,12.2,-5.25110781800001));
#178677=CARTESIAN_POINT('Ctrl Pts',(10.2057173299999,12.2,-5.24807824100002));
#178678=CARTESIAN_POINT('Ctrl Pts',(10.2034333439999,12.2,-5.24505392700001));
#178679=CARTESIAN_POINT('Ctrl Pts',(10.2011497209999,12.2,-5.24203487700001));
#178680=CARTESIAN_POINT('Ctrl Pts',(10.1988664679999,12.2,-5.23902109400002));
#178681=CARTESIAN_POINT('Ctrl Pts',(10.1965835999999,12.2,-5.23601258300001));
#178682=CARTESIAN_POINT('Ctrl Pts',(10.1943011249999,12.2,-5.23300934300002));
#178683=CARTESIAN_POINT('Ctrl Pts',(10.1920190549999,12.2,-5.23001138000001));
#178684=CARTESIAN_POINT('Ctrl Pts',(10.1897373969999,12.2,-5.22701869500001));
#178685=CARTESIAN_POINT('Ctrl Pts',(10.1874561619999,12.2,-5.22403129000002));
#178686=CARTESIAN_POINT('Ctrl Pts',(10.1851753559999,12.2,-5.22104916700001));
#178687=CARTESIAN_POINT('Ctrl Pts',(10.1828949879999,12.2,-5.21807232700001));
#178688=CARTESIAN_POINT('Ctrl Pts',(10.1806150639999,12.2,-5.21510077400002));
#178689=CARTESIAN_POINT('Ctrl Pts',(10.1783355949999,12.2,-5.21213451000001));
#178690=CARTESIAN_POINT('Ctrl Pts',(10.1760565879999,12.2,-5.20917353600002));
#178691=CARTESIAN_POINT('Ctrl Pts',(10.1737780519999,12.2,-5.20621785500001));
#178692=CARTESIAN_POINT('Ctrl Pts',(10.1714999969999,12.2,-5.20326746900002));
#178693=CARTESIAN_POINT('Ctrl Pts',(10.1692224309999,12.2,-5.20032238000002));
#178694=CARTESIAN_POINT('Ctrl Pts',(10.1669453649999,12.2,-5.19738259100002));
#178695=CARTESIAN_POINT('Ctrl Pts',(10.1646688079999,12.2,-5.19444810300001));
#178696=CARTESIAN_POINT('Ctrl Pts',(10.1623927679999,12.2,-5.19151892100002));
#178697=CARTESIAN_POINT('Ctrl Pts',(10.1601172529999,12.2,-5.18859504400002));
#178698=CARTESIAN_POINT('Ctrl Pts',(10.1578422729999,12.2,-5.18567647600001));
#178699=CARTESIAN_POINT('Ctrl Pts',(10.1555678379999,12.2,-5.18276321900002));
#178700=CARTESIAN_POINT('Ctrl Pts',(10.1532939539999,12.2,-5.17985527400001));
#178701=CARTESIAN_POINT('Ctrl Pts',(10.1510206309999,12.2,-5.17695264500002));
#178702=CARTESIAN_POINT('Ctrl Pts',(10.1487478799999,12.2,-5.17405533200002));
#178703=CARTESIAN_POINT('Ctrl Pts',(10.1464757069999,12.2,-5.17116333800002));
#178704=CARTESIAN_POINT('Ctrl Pts',(10.1442041239999,12.2,-5.16827666700001));
#178705=CARTESIAN_POINT('Ctrl Pts',(10.1419331389999,12.2,-5.16539531900001));
#178706=CARTESIAN_POINT('Ctrl Pts',(10.1396627609999,12.2,-5.16251929700001));
#178707=CARTESIAN_POINT('Ctrl Pts',(10.1373929979999,12.2,-5.15964860200001));
#178708=CARTESIAN_POINT('Ctrl Pts',(10.1351238609999,12.2,-5.15678323800001));
#178709=CARTESIAN_POINT('Ctrl Pts',(10.1328553589999,12.2,-5.15392320600002));
#178710=CARTESIAN_POINT('Ctrl Pts',(10.1305874999999,12.2,-5.15106851000001));
#178711=CARTESIAN_POINT('Ctrl Pts',(10.1283202939999,12.2,-5.14821914900002));
#178712=CARTESIAN_POINT('Ctrl Pts',(10.1260537499999,12.2,-5.14537512800001));
#178713=CARTESIAN_POINT('Ctrl Pts',(10.1237878759999,12.2,-5.14253644700001));
#178714=CARTESIAN_POINT('Ctrl Pts',(10.1215226839999,12.2,-5.13970310900001));
#178715=CARTESIAN_POINT('Ctrl Pts',(10.1192581799999,12.2,-5.13687511700001));
#178716=CARTESIAN_POINT('Ctrl Pts',(10.1169943759999,12.2,-5.13405247200001));
#178717=CARTESIAN_POINT('Ctrl Pts',(10.1147312799999,12.2,-5.13123517600001));
#178718=CARTESIAN_POINT('Ctrl Pts',(10.1124689019999,12.2,-5.12842323200001));
#178719=CARTESIAN_POINT('Ctrl Pts',(10.1102072499999,12.2,-5.12561664200001));
#178720=CARTESIAN_POINT('Ctrl Pts',(10.1079463349999,12.2,-5.12281540800001));
#178721=CARTESIAN_POINT('Ctrl Pts',(10.1056861639999,12.2,-5.12001953100001));
#178722=CARTESIAN_POINT('Ctrl Pts',(10.1034267499999,12.2,-5.11722901400002));
#178723=CARTESIAN_POINT('Ctrl Pts',(10.1011680999999,12.2,-5.11444386000001));
#178724=CARTESIAN_POINT('Ctrl Pts',(10.0989102229999,12.2,-5.11166406900001));
#178725=CARTESIAN_POINT('Ctrl Pts',(10.0966531299999,12.2,-5.10888964500001));
#178726=CARTESIAN_POINT('Ctrl Pts',(10.0943968289999,12.2,-5.10612059000001));
#178727=CARTESIAN_POINT('Ctrl Pts',(10.0921413299999,12.2,-5.10335690500002));
#178728=CARTESIAN_POINT('Ctrl Pts',(10.0898866439999,12.2,-5.10059859300001));
#178729=CARTESIAN_POINT('Ctrl Pts',(10.0876327779999,12.2,-5.09784565500001));
#178730=CARTESIAN_POINT('Ctrl Pts',(10.0853797429999,12.2,-5.09509809400001));
#178731=CARTESIAN_POINT('Ctrl Pts',(10.0831275479999,12.2,-5.09235591100001));
#178732=CARTESIAN_POINT('Ctrl Pts',(10.0808762039999,12.2,-5.08961911000001));
#178733=CARTESIAN_POINT('Ctrl Pts',(10.0786257189999,12.2,-5.08688769200001));
#178734=CARTESIAN_POINT('Ctrl Pts',(10.0763761029999,12.2,-5.08416165800002));
#178735=CARTESIAN_POINT('Ctrl Pts',(10.0741273649999,12.2,-5.08144101100001));
#178736=CARTESIAN_POINT('Ctrl Pts',(10.0718795159999,12.2,-5.07872575400001));
#178737=CARTESIAN_POINT('Ctrl Pts',(10.0696325649999,12.2,-5.07601588800001));
#178738=CARTESIAN_POINT('Ctrl Pts',(10.0673865209999,12.2,-5.07331141500002));
#178739=CARTESIAN_POINT('Ctrl Pts',(10.0651413949999,12.2,-5.07061233700002));
#178740=CARTESIAN_POINT('Ctrl Pts',(10.0628971959999,12.2,-5.06791865600002));
#178741=CARTESIAN_POINT('Ctrl Pts',(10.0606539349999,12.2,-5.06523037500001));
#178742=CARTESIAN_POINT('Ctrl Pts',(10.0584116189999,12.2,-5.06254749600001));
#178743=CARTESIAN_POINT('Ctrl Pts',(10.0561702599999,12.2,-5.05987001900001));
#178744=CARTESIAN_POINT('Ctrl Pts',(10.0539298679999,12.2,-5.05719794800001));
#178745=CARTESIAN_POINT('Ctrl Pts',(10.0516904509999,12.2,-5.05453128400001));
#178746=CARTESIAN_POINT('Ctrl Pts',(10.0494520199999,12.2,-5.05187002900001));
#178747=CARTESIAN_POINT('Ctrl Pts',(10.0472145849999,12.2,-5.04921418600001));
#178748=CARTESIAN_POINT('Ctrl Pts',(10.0449781559999,12.2,-5.04656375500002));
#178749=CARTESIAN_POINT('Ctrl Pts',(10.0427427419999,12.2,-5.04391874100001));
#178750=CARTESIAN_POINT('Ctrl Pts',(10.0405083539999,12.2,-5.04127914300001));
#178751=CARTESIAN_POINT('Ctrl Pts',(10.0382750009999,12.2,-5.03864496500002));
#178752=CARTESIAN_POINT('Ctrl Pts',(10.0360426939999,12.2,-5.03601620900001));
#178753=CARTESIAN_POINT('Ctrl Pts',(10.0338114419999,12.2,-5.03339287600001));
#178754=CARTESIAN_POINT('Ctrl Pts',(10.0315812549999,12.2,-5.03077496800001));
#178755=CARTESIAN_POINT('Ctrl Pts',(10.0293521449999,12.2,-5.02816248700002));
#178756=CARTESIAN_POINT('Ctrl Pts',(10.0271241189999,12.2,-5.02555543600002));
#178757=CARTESIAN_POINT('Ctrl Pts',(10.0248971889999,12.2,-5.02295381500002));
#178758=CARTESIAN_POINT('Ctrl Pts',(10.0226713639999,12.2,-5.02035762800002));
#178759=CARTESIAN_POINT('Ctrl Pts',(10.0204466549999,12.2,-5.01776687600001));
#178760=CARTESIAN_POINT('Ctrl Pts',(10.0182230729999,12.2,-5.01518156000001));
#178761=CARTESIAN_POINT('Ctrl Pts',(10.0160006259999,12.2,-5.01260168400002));
#178762=CARTESIAN_POINT('Ctrl Pts',(10.0137793259999,12.2,-5.01002724800002));
#178763=CARTESIAN_POINT('Ctrl Pts',(10.0115591819999,12.2,-5.00745825600001));
#178764=CARTESIAN_POINT('Ctrl Pts',(10.0093402039999,12.2,-5.00489470900002));
#178765=CARTESIAN_POINT('Ctrl Pts',(10.0071224029999,12.2,-5.00233660800002));
#178766=CARTESIAN_POINT('Ctrl Pts',(10.0049057889999,12.2,-4.99978395500001));
#178767=CARTESIAN_POINT('Ctrl Pts',(10.0026903729999,12.2,-4.99723675300002));
#178768=CARTESIAN_POINT('Ctrl Pts',(10.0004761639999,12.2,-4.99469500400001));
#178769=CARTESIAN_POINT('Ctrl Pts',(9.99826317399994,12.2,-4.99215870900001));
#178770=CARTESIAN_POINT('Ctrl Pts',(9.99605141199994,12.2,-4.98962787000002));
#178771=CARTESIAN_POINT('Ctrl Pts',(9.99384088799994,12.2,-4.98710249000001));
#178772=CARTESIAN_POINT('Ctrl Pts',(9.99163161399995,12.2,-4.98458256900001));
#178773=CARTESIAN_POINT('Ctrl Pts',(9.98942359899995,12.2,-4.98206811000002));
#178774=CARTESIAN_POINT('Ctrl Pts',(9.98721685399994,12.2,-4.97955911500001));
#178775=CARTESIAN_POINT('Ctrl Pts',(9.98501138999995,12.2,-4.97705558600002));
#178776=CARTESIAN_POINT('Ctrl Pts',(9.98280721699994,12.2,-4.97455752400001));
#178777=CARTESIAN_POINT('Ctrl Pts',(9.98060434499994,12.2,-4.97206493200002));
#178778=CARTESIAN_POINT('Ctrl Pts',(9.97840278499995,12.2,-4.96957781100001));
#178779=CARTESIAN_POINT('Ctrl Pts',(9.97620254699994,12.2,-4.96709616400001));
#178780=CARTESIAN_POINT('Ctrl Pts',(9.97400364199994,12.2,-4.96461999100001));
#178781=CARTESIAN_POINT('Ctrl Pts',(9.97180608099995,12.2,-4.96214929600002));
#178782=CARTESIAN_POINT('Ctrl Pts',(9.96960987299994,12.2,-4.95968407800001));
#178783=CARTESIAN_POINT('Ctrl Pts',(9.96741503199994,12.2,-4.95722434200002));
#178784=CARTESIAN_POINT('Ctrl Pts',(9.96522156599994,12.2,-4.95477008800002));
#178785=CARTESIAN_POINT('Ctrl Pts',(9.96302948499994,12.2,-4.95232131800002));
#178786=CARTESIAN_POINT('Ctrl Pts',(9.96083880199994,12.2,-4.94987803500001));
#178787=CARTESIAN_POINT('Ctrl Pts',(9.95864952599995,12.2,-4.94744023800001));
#178788=CARTESIAN_POINT('Ctrl Pts',(9.95646166799995,12.2,-4.94500793200002));
#178789=CARTESIAN_POINT('Ctrl Pts',(9.95427523999994,12.2,-4.94258111700002));
#178790=CARTESIAN_POINT('Ctrl Pts',(9.95209025099994,12.2,-4.94015979700002));
#178791=CARTESIAN_POINT('Ctrl Pts',(9.94990671399995,12.2,-4.93774397000001));
#178792=CARTESIAN_POINT('Ctrl Pts',(9.94772463699995,12.2,-4.93533364100001));
#178793=CARTESIAN_POINT('Ctrl Pts',(9.94554403299994,12.2,-4.93292881000002));
#178794=CARTESIAN_POINT('Ctrl Pts',(9.94336491299994,12.2,-4.93052948100001));
#178795=CARTESIAN_POINT('Ctrl Pts',(9.94118728699994,12.2,-4.92813565300001));
#178796=CARTESIAN_POINT('Ctrl Pts',(9.93901116599995,12.2,-4.92574732900001));
#178797=CARTESIAN_POINT('Ctrl Pts',(9.93683656099994,12.2,-4.92336451100002));
#178798=CARTESIAN_POINT('Ctrl Pts',(9.93466348399994,12.2,-4.92098720100001));
#178799=CARTESIAN_POINT('Ctrl Pts',(9.93249194399995,12.2,-4.91861540000002));
#178800=CARTESIAN_POINT('Ctrl Pts',(9.93032195399994,12.2,-4.91624911100002));
#178801=CARTESIAN_POINT('Ctrl Pts',(9.92815352399995,12.2,-4.91388833500002));
#178802=CARTESIAN_POINT('Ctrl Pts',(9.92598666499994,12.2,-4.91153307200001));
#178803=CARTESIAN_POINT('Ctrl Pts',(9.92382138899995,12.2,-4.90918332600002));
#178804=CARTESIAN_POINT('Ctrl Pts',(9.92165770599994,12.2,-4.90683909900001));
#178805=CARTESIAN_POINT('Ctrl Pts',(9.91949562799994,12.2,-4.90450039100002));
#178806=CARTESIAN_POINT('Ctrl Pts',(9.91733516599995,12.2,-4.90216720500001));
#178807=CARTESIAN_POINT('Ctrl Pts',(9.91517632999994,12.2,-4.89983954200001));
#178808=CARTESIAN_POINT('Ctrl Pts',(9.91301913399995,12.2,-4.89751740500001));
#178809=CARTESIAN_POINT('Ctrl Pts',(9.91086358699994,12.2,-4.89520079400001));
#178810=CARTESIAN_POINT('Ctrl Pts',(9.90870969999994,12.2,-4.89288971200001));
#178811=CARTESIAN_POINT('Ctrl Pts',(9.90655748599995,12.2,-4.89058415900002));
#178812=CARTESIAN_POINT('Ctrl Pts',(9.90440695499995,12.2,-4.88828413900002));
#178813=CARTESIAN_POINT('Ctrl Pts',(9.90225811999995,12.2,-4.88598965200001));
#178814=CARTESIAN_POINT('Ctrl Pts',(9.90011098899994,12.2,-4.88370070000002));
#178815=CARTESIAN_POINT('Ctrl Pts',(9.89796557699995,12.2,-4.88141728600001));
#178816=CARTESIAN_POINT('Ctrl Pts',(9.89582189499994,12.2,-4.87913940900001));
#178817=CARTESIAN_POINT('Ctrl Pts',(9.89367995199995,12.2,-4.87686707300002));
#178818=CARTESIAN_POINT('Ctrl Pts',(9.89153976099994,12.2,-4.87460027900001));
#178819=CARTESIAN_POINT('Ctrl Pts',(9.88940133499994,12.2,-4.87233902900002));
#178820=CARTESIAN_POINT('Ctrl Pts',(9.88726468299994,12.2,-4.87008332300002));
#178821=CARTESIAN_POINT('Ctrl Pts',(9.88512981699994,12.2,-4.86783316500001));
#178822=CARTESIAN_POINT('Ctrl Pts',(9.88299674999995,12.2,-4.86558855600002));
#178823=CARTESIAN_POINT('Ctrl Pts',(9.88086549299994,12.2,-4.86334949700002));
#178824=CARTESIAN_POINT('Ctrl Pts',(9.87873605699994,12.2,-4.86111598900001));
#178825=CARTESIAN_POINT('Ctrl Pts',(9.87660845399994,12.2,-4.85888803500002));
#178826=CARTESIAN_POINT('Ctrl Pts',(9.87448269599994,12.2,-4.85666563600001));
#178827=CARTESIAN_POINT('Ctrl Pts',(9.87235879499995,12.2,-4.85444879300001));
#178828=CARTESIAN_POINT('Ctrl Pts',(9.87023676299994,12.2,-4.85223750900001));
#178829=CARTESIAN_POINT('Ctrl Pts',(9.86811660899994,12.2,-4.85003178400001));
#178830=CARTESIAN_POINT('Ctrl Pts',(9.86599834899994,12.2,-4.84783162100001));
#178831=CARTESIAN_POINT('Ctrl Pts',(9.86388199199994,12.2,-4.84563702200001));
#178832=CARTESIAN_POINT('Ctrl Pts',(9.86176754899994,12.2,-4.84344798700001));
#178833=CARTESIAN_POINT('Ctrl Pts',(9.85965503599994,12.2,-4.84126451800002));
#178834=CARTESIAN_POINT('Ctrl Pts',(9.85754445999994,12.2,-4.83908661700001));
#178835=CARTESIAN_POINT('Ctrl Pts',(9.85543583699994,12.2,-4.83691428600002));
#178836=CARTESIAN_POINT('Ctrl Pts',(9.85332917699995,12.2,-4.83474752600001));
#178837=CARTESIAN_POINT('Ctrl Pts',(9.85122449199994,12.2,-4.83258633800002));
#178838=CARTESIAN_POINT('Ctrl Pts',(9.84912179299995,12.2,-4.83043072400001));
#178839=CARTESIAN_POINT('Ctrl Pts',(9.84702109499995,12.2,-4.82828068500002));
#178840=CARTESIAN_POINT('Ctrl Pts',(9.84492240799995,12.2,-4.82613622400001));
#178841=CARTESIAN_POINT('Ctrl Pts',(9.84282574499994,12.2,-4.82399734200001));
#178842=CARTESIAN_POINT('Ctrl Pts',(9.84073111699994,12.2,-4.82186404000001));
#178843=CARTESIAN_POINT('Ctrl Pts',(9.83863853799994,12.2,-4.81973632000001));
#178844=CARTESIAN_POINT('Ctrl Pts',(9.83654801799995,12.2,-4.81761418300001));
#178845=CARTESIAN_POINT('Ctrl Pts',(9.83445956999994,12.2,-4.81549763000002));
#178846=CARTESIAN_POINT('Ctrl Pts',(9.83237320799994,12.2,-4.81338666500001));
#178847=CARTESIAN_POINT('Ctrl Pts',(9.83028894099995,12.2,-4.81128128700002));
#178848=CARTESIAN_POINT('Ctrl Pts',(9.82820678499994,12.2,-4.80918149800001));
#178849=CARTESIAN_POINT('Ctrl Pts',(9.82612674899995,12.2,-4.80708730000002));
#178850=CARTESIAN_POINT('Ctrl Pts',(9.82404884799994,12.2,-4.80499869500001));
#178851=CARTESIAN_POINT('Ctrl Pts',(9.82197309199995,12.2,-4.80291568300002));
#178852=CARTESIAN_POINT('Ctrl Pts',(9.81989949599994,12.2,-4.80083826600001));
#178853=CARTESIAN_POINT('Ctrl Pts',(9.81782806999994,12.2,-4.79876644700001));
#178854=CARTESIAN_POINT('Ctrl Pts',(9.81575882799994,12.2,-4.79670022500001));
#178855=CARTESIAN_POINT('Ctrl Pts',(9.81369178299994,12.2,-4.79463960300002));
#178856=CARTESIAN_POINT('Ctrl Pts',(9.81162694599995,12.2,-4.79258458200002));
#178857=CARTESIAN_POINT('Ctrl Pts',(9.80956432999994,12.2,-4.79053516400001));
#178858=CARTESIAN_POINT('Ctrl Pts',(9.80750394899994,12.2,-4.78849134900001));
#178859=CARTESIAN_POINT('Ctrl Pts',(9.80544581399995,12.2,-4.78645314000001));
#178860=CARTESIAN_POINT('Ctrl Pts',(9.80338993799995,12.2,-4.78442053800002));
#178861=CARTESIAN_POINT('Ctrl Pts',(9.80133633399995,12.2,-4.78239354400001));
#178862=CARTESIAN_POINT('Ctrl Pts',(9.79928501499994,12.2,-4.78037216000001));
#178863=CARTESIAN_POINT('Ctrl Pts',(9.79723599299994,12.2,-4.77835638700002));
#178864=CARTESIAN_POINT('Ctrl Pts',(9.79518928099995,12.2,-4.77634622600001));
#178865=CARTESIAN_POINT('Ctrl Pts',(9.79314489299994,12.2,-4.77434167900002));
#178866=CARTESIAN_POINT('Ctrl Pts',(9.79110284099994,12.2,-4.77234274600002));
#178867=CARTESIAN_POINT('Ctrl Pts',(9.78906313699994,12.2,-4.77034943200001));
#178868=CARTESIAN_POINT('Ctrl Pts',(9.78702579499994,12.2,-4.76836173400002));
#178869=CARTESIAN_POINT('Ctrl Pts',(9.78499082799994,12.2,-4.76637965700001));
#178870=CARTESIAN_POINT('Ctrl Pts',(9.78295824899994,12.2,-4.76440319900002));
#178871=CARTESIAN_POINT('Ctrl Pts',(9.78092806999994,12.2,-4.76243236400002));
#178872=CARTESIAN_POINT('Ctrl Pts',(9.77890030599994,12.2,-4.76046715200001));
#178873=CARTESIAN_POINT('Ctrl Pts',(9.77687496799994,12.2,-4.75850756500002));
#178874=CARTESIAN_POINT('Ctrl Pts',(9.77485206899994,12.2,-4.75655360400001));
#178875=CARTESIAN_POINT('Ctrl Pts',(9.77283162499995,12.2,-4.75460527100001));
#178876=CARTESIAN_POINT('Ctrl Pts',(9.77081364699995,12.2,-4.75266256500001));
#178877=CARTESIAN_POINT('Ctrl Pts',(9.76879814799995,12.2,-4.75072549100001));
#178878=CARTESIAN_POINT('Ctrl Pts',(9.76678514199994,12.2,-4.74879404700001));
#178879=CARTESIAN_POINT('Ctrl Pts',(9.76477464199995,12.2,-4.74686823700001));
#178880=CARTESIAN_POINT('Ctrl Pts',(9.76276666199994,12.2,-4.74494806000001));
#178881=CARTESIAN_POINT('Ctrl Pts',(9.76076121399995,12.2,-4.74303351800001));
#178882=CARTESIAN_POINT('Ctrl Pts',(9.75875831199994,12.2,-4.74112461300002));
#178883=CARTESIAN_POINT('Ctrl Pts',(9.75675797099995,12.2,-4.73922134600001));
#178884=CARTESIAN_POINT('Ctrl Pts',(9.75476020099994,12.2,-4.73732371700001));
#178885=CARTESIAN_POINT('Ctrl Pts',(9.75276501899994,12.2,-4.73543173000001));
#178886=CARTESIAN_POINT('Ctrl Pts',(9.75077243699995,12.2,-4.73354538300002));
#178887=CARTESIAN_POINT('Ctrl Pts',(9.74878246899994,12.2,-4.73166467900001));
#178888=CARTESIAN_POINT('Ctrl Pts',(9.74679512899994,12.2,-4.72978962000001));
#178889=CARTESIAN_POINT('Ctrl Pts',(9.74481042799994,12.2,-4.72792020600002));
#178890=CARTESIAN_POINT('Ctrl Pts',(9.74282838199995,12.2,-4.72605643900001));
#178891=CARTESIAN_POINT('Ctrl Pts',(9.74084900499994,12.2,-4.72419831800002));
#178892=CARTESIAN_POINT('Ctrl Pts',(9.73887230999994,12.2,-4.72234584700002));
#178893=CARTESIAN_POINT('Ctrl Pts',(9.73689830999995,12.2,-4.72049902600002));
#178894=CARTESIAN_POINT('Ctrl Pts',(9.73492701999995,12.2,-4.71865785700002));
#178895=CARTESIAN_POINT('Ctrl Pts',(9.73295845299995,12.2,-4.71682234000002));
#178896=CARTESIAN_POINT('Ctrl Pts',(9.73099262399994,12.2,-4.71499247700002));
#178897=CARTESIAN_POINT('Ctrl Pts',(9.72902954599994,12.2,-4.71316826800001));
#178898=CARTESIAN_POINT('Ctrl Pts',(9.72706923299994,12.2,-4.71134971600002));
#178899=CARTESIAN_POINT('Ctrl Pts',(9.72511169899994,12.2,-4.70953682000002));
#178900=CARTESIAN_POINT('Ctrl Pts',(9.72315695899994,12.2,-4.70772958400001));
#178901=CARTESIAN_POINT('Ctrl Pts',(9.72120502599994,12.2,-4.70592800700001));
#178902=CARTESIAN_POINT('Ctrl Pts',(9.71925591399994,12.2,-4.70413209100002));
#178903=CARTESIAN_POINT('Ctrl Pts',(9.71730963799994,12.2,-4.70234183600001));
#178904=CARTESIAN_POINT('Ctrl Pts',(9.71536621099995,12.2,-4.70055724400002));
#178905=CARTESIAN_POINT('Ctrl Pts',(9.71342564799994,12.2,-4.69877831600002));
#178906=CARTESIAN_POINT('Ctrl Pts',(9.71148796399994,12.2,-4.69700505400001));
#178907=CARTESIAN_POINT('Ctrl Pts',(9.70955317199994,12.2,-4.69523745800001));
#178908=CARTESIAN_POINT('Ctrl Pts',(9.70762128699995,12.2,-4.69347552800001));
#178909=CARTESIAN_POINT('Ctrl Pts',(9.70569232299994,12.2,-4.69171926800001));
#178910=CARTESIAN_POINT('Ctrl Pts',(9.70376629399994,12.2,-4.68996867700001));
#178911=CARTESIAN_POINT('Ctrl Pts',(9.70184321499995,12.2,-4.68822375800002));
#178912=CARTESIAN_POINT('Ctrl Pts',(9.69992310199994,12.2,-4.68648450800002));
#178913=CARTESIAN_POINT('Ctrl Pts',(9.69800596699995,12.2,-4.68475093300002));
#178914=CARTESIAN_POINT('Ctrl Pts',(9.69609182599994,12.2,-4.68302303000002));
#178915=CARTESIAN_POINT('Ctrl Pts',(9.69418069299994,12.2,-4.68130080300002));
#178916=CARTESIAN_POINT('Ctrl Pts',(9.69227258299994,12.2,-4.67958425200001));
#178917=CARTESIAN_POINT('Ctrl Pts',(9.69036750899994,12.2,-4.67787337800001));
#178918=CARTESIAN_POINT('Ctrl Pts',(9.68846548899995,12.2,-4.67616818100002));
#178919=CARTESIAN_POINT('Ctrl Pts',(9.68656653499995,12.2,-4.67446866300001));
#178920=CARTESIAN_POINT('Ctrl Pts',(9.68467066399995,12.2,-4.67277482500001));
#178921=CARTESIAN_POINT('Ctrl Pts',(9.68277788899995,12.2,-4.67108666800002));
#178922=CARTESIAN_POINT('Ctrl Pts',(9.68088822599995,12.2,-4.66940419300002));
#178923=CARTESIAN_POINT('Ctrl Pts',(9.67900168899994,12.2,-4.66772740200001));
#178924=CARTESIAN_POINT('Ctrl Pts',(9.67711829399994,12.2,-4.66605629400001));
#178925=CARTESIAN_POINT('Ctrl Pts',(9.67523805399994,12.2,-4.66439087100001));
#178926=CARTESIAN_POINT('Ctrl Pts',(9.67336098799995,12.2,-4.66273113300002));
#178927=CARTESIAN_POINT('Ctrl Pts',(9.67148710599995,12.2,-4.66107708200001));
#178928=CARTESIAN_POINT('Ctrl Pts',(9.66961642799994,12.2,-4.65942871900001));
#178929=CARTESIAN_POINT('Ctrl Pts',(9.66774896599994,12.2,-4.65778604500001));
#178930=CARTESIAN_POINT('Ctrl Pts',(9.66588473599994,12.2,-4.65614906000001));
#178931=CARTESIAN_POINT('Ctrl Pts',(9.66402375299995,12.2,-4.65451776500001));
#178932=CARTESIAN_POINT('Ctrl Pts',(9.66216603399995,12.2,-4.65289216300001));
#178933=CARTESIAN_POINT('Ctrl Pts',(9.66031159299994,12.2,-4.65127225200002));
#178934=CARTESIAN_POINT('Ctrl Pts',(9.65846044499994,12.2,-4.64965803400001));
#178935=CARTESIAN_POINT('Ctrl Pts',(9.65661260499994,12.2,-4.64804951100001));
#178936=CARTESIAN_POINT('Ctrl Pts',(9.65476809099994,12.2,-4.64644668200001));
#178937=CARTESIAN_POINT('Ctrl Pts',(9.65292691699995,12.2,-4.64484954900001));
#178938=CARTESIAN_POINT('Ctrl Pts',(9.65108909699994,12.2,-4.64325811300002));
#178939=CARTESIAN_POINT('Ctrl Pts',(9.64925464999994,12.2,-4.64167237400002));
#178940=CARTESIAN_POINT('Ctrl Pts',(9.64742358899995,12.2,-4.64009233400001));
#178941=CARTESIAN_POINT('Ctrl Pts',(9.64559592999995,12.2,-4.63851799300001));
#178942=CARTESIAN_POINT('Ctrl Pts',(9.64377168999994,12.2,-4.63694935100001));
#178943=CARTESIAN_POINT('Ctrl Pts',(9.64195088399994,12.2,-4.63538641000001));
#178944=CARTESIAN_POINT('Ctrl Pts',(9.64013352699994,12.2,-4.63382917200001));
#178945=CARTESIAN_POINT('Ctrl Pts',(9.63831963699995,12.2,-4.63227763600001));
#178946=CARTESIAN_POINT('Ctrl Pts',(9.63650922799994,12.2,-4.63073180200002));
#178947=CARTESIAN_POINT('Ctrl Pts',(9.63470231799995,12.2,-4.62919167300001));
#178948=CARTESIAN_POINT('Ctrl Pts',(9.63289892099995,12.2,-4.62765724900001));
#178949=CARTESIAN_POINT('Ctrl Pts',(9.63109905299994,12.2,-4.62612853000001));
#178950=CARTESIAN_POINT('Ctrl Pts',(9.62930273199994,12.2,-4.62460551700001));
#178951=CARTESIAN_POINT('Ctrl Pts',(9.62750997299995,12.2,-4.62308821200001));
#178952=CARTESIAN_POINT('Ctrl Pts',(9.62572079199994,12.2,-4.62157661300001));
#178953=CARTESIAN_POINT('Ctrl Pts',(9.62393520599995,12.2,-4.62007072400001));
#178954=CARTESIAN_POINT('Ctrl Pts',(9.62215323099995,12.2,-4.61857054400001));
#178955=CARTESIAN_POINT('Ctrl Pts',(9.62037488299995,12.2,-4.61707607400001));
#178956=CARTESIAN_POINT('Ctrl Pts',(9.61860017899994,12.2,-4.61558731400002));
#178957=CARTESIAN_POINT('Ctrl Pts',(9.61682913599994,12.2,-4.61410426600001));
#178958=CARTESIAN_POINT('Ctrl Pts',(9.61506176799995,12.2,-4.61262692900001));
#178959=CARTESIAN_POINT('Ctrl Pts',(9.61329809399994,12.2,-4.61115530500001));
#178960=CARTESIAN_POINT('Ctrl Pts',(9.61153812999994,12.2,-4.60968939500002));
#178961=CARTESIAN_POINT('Ctrl Pts',(9.60978189399994,12.2,-4.60822919900002));
#178962=CARTESIAN_POINT('Ctrl Pts',(9.60802939899994,12.2,-4.60677471700001));
#178963=CARTESIAN_POINT('Ctrl Pts',(9.60628066499994,12.2,-4.60532595000001));
#178964=CARTESIAN_POINT('Ctrl Pts',(9.60453570799995,12.2,-4.60388290000001));
#178965=CARTESIAN_POINT('Ctrl Pts',(9.60279454499995,12.2,-4.60244556600002));
#178966=CARTESIAN_POINT('Ctrl Pts',(9.60105719199994,12.2,-4.60101394900001));
#178967=CARTESIAN_POINT('Ctrl Pts',(9.59932366799995,12.2,-4.59958805000001));
#178968=CARTESIAN_POINT('Ctrl Pts',(9.59759398799994,12.2,-4.59816786900001));
#178969=CARTESIAN_POINT('Ctrl Pts',(9.59586816799994,12.2,-4.59675340600001));
#178970=CARTESIAN_POINT('Ctrl Pts',(9.59414622799994,12.2,-4.59534466400001));
#178971=CARTESIAN_POINT('Ctrl Pts',(9.59242818399994,12.2,-4.59394164100001));
#178972=CARTESIAN_POINT('Ctrl Pts',(9.59071405399994,12.2,-4.59254433900002));
#178973=CARTESIAN_POINT('Ctrl Pts',(9.58900385399994,12.2,-4.59115275800002));
#178974=CARTESIAN_POINT('Ctrl Pts',(9.58729760199994,12.2,-4.58976689800001));
#178975=CARTESIAN_POINT('Ctrl Pts',(9.58559531499995,12.2,-4.58838676100001));
#178976=CARTESIAN_POINT('Ctrl Pts',(9.58389701199994,12.2,-4.58701234700001));
#178977=CARTESIAN_POINT('Ctrl Pts',(9.58220270699995,12.2,-4.58564365500001));
#178978=CARTESIAN_POINT('Ctrl Pts',(9.58051242199994,12.2,-4.58428068800002));
#178979=CARTESIAN_POINT('Ctrl Pts',(9.57882617099994,12.2,-4.58292344400002));
#178980=CARTESIAN_POINT('Ctrl Pts',(9.57714397399995,12.2,-4.58157192400002));
#178981=CARTESIAN_POINT('Ctrl Pts',(9.57546584599994,12.2,-4.58022613000002));
#178982=CARTESIAN_POINT('Ctrl Pts',(9.57379180899995,12.2,-4.57888606200001));
#178983=CARTESIAN_POINT('Ctrl Pts',(9.57212187699995,12.2,-4.57755172000001));
#178984=CARTESIAN_POINT('Ctrl Pts',(9.57045606999994,12.2,-4.57622310400001));
#178985=CARTESIAN_POINT('Ctrl Pts',(9.56879440599995,12.2,-4.57490021400002));
#178986=CARTESIAN_POINT('Ctrl Pts',(9.56713690099994,12.2,-4.57358305200001));
#178987=CARTESIAN_POINT('Ctrl Pts',(9.56548357399994,12.2,-4.57227161800001));
#178988=CARTESIAN_POINT('Ctrl Pts',(9.56383444399994,12.2,-4.57096591100001));
#178989=CARTESIAN_POINT('Ctrl Pts',(9.56218952899994,12.2,-4.56966593300002));
#178990=CARTESIAN_POINT('Ctrl Pts',(9.56054884799994,12.2,-4.56837168300002));
#178991=CARTESIAN_POINT('Ctrl Pts',(9.55891241699995,12.2,-4.56708316300002));
#178992=CARTESIAN_POINT('Ctrl Pts',(9.55728025499995,12.2,-4.56580037200002));
#178993=CARTESIAN_POINT('Ctrl Pts',(9.55565238299994,12.2,-4.56452331000001));
#178994=CARTESIAN_POINT('Ctrl Pts',(9.55402881599994,12.2,-4.56325197900001));
#178995=CARTESIAN_POINT('Ctrl Pts',(9.55240957399995,12.2,-4.56198637800002));
#178996=CARTESIAN_POINT('Ctrl Pts',(9.55079467599995,12.2,-4.56072650800001));
#178997=CARTESIAN_POINT('Ctrl Pts',(9.54918413999994,12.2,-4.55947236900001));
#178998=CARTESIAN_POINT('Ctrl Pts',(9.54757798599994,12.2,-4.55822396200002));
#178999=CARTESIAN_POINT('Ctrl Pts',(9.54597623199994,12.2,-4.55698128600002));
#179000=CARTESIAN_POINT('Ctrl Pts',(9.54437889599994,12.2,-4.55574434100001));
#179001=CARTESIAN_POINT('Ctrl Pts',(9.54278599799995,12.2,-4.55451312900002));
#179002=CARTESIAN_POINT('Ctrl Pts',(9.54119755599995,12.2,-4.55328764900001));
#179003=CARTESIAN_POINT('Ctrl Pts',(9.53961358999995,12.2,-4.55206790100001));
#179004=CARTESIAN_POINT('Ctrl Pts',(9.53803411899995,12.2,-4.55085388600001));
#179005=CARTESIAN_POINT('Ctrl Pts',(9.53645916199994,12.2,-4.54964560500001));
#179006=CARTESIAN_POINT('Ctrl Pts',(9.53488873799994,12.2,-4.54844305600002));
#179007=CARTESIAN_POINT('Ctrl Pts',(9.53332286699995,12.2,-4.54724624000002));
#179008=CARTESIAN_POINT('Ctrl Pts',(9.53176156699995,12.2,-4.54605515800001));
#179009=CARTESIAN_POINT('Ctrl Pts',(9.53020485899994,12.2,-4.54486981000001));
#179010=CARTESIAN_POINT('Ctrl Pts',(9.52865276099994,12.2,-4.54369019500001));
#179011=CARTESIAN_POINT('Ctrl Pts',(9.52710529499995,12.2,-4.54251631400002));
#179012=CARTESIAN_POINT('Ctrl Pts',(9.52556247699994,12.2,-4.54134816700002));
#179013=CARTESIAN_POINT('Ctrl Pts',(9.52402432899994,12.2,-4.54018575400001));
#179014=CARTESIAN_POINT('Ctrl Pts',(9.52249087199995,12.2,-4.53902907500002));
#179015=CARTESIAN_POINT('Ctrl Pts',(9.52096212299995,12.2,-4.53787813200002));
#179016=CARTESIAN_POINT('Ctrl Pts',(9.51943810399994,12.2,-4.53673292200001));
#179017=CARTESIAN_POINT('Ctrl Pts',(9.51791883399994,12.2,-4.53559344600002));
#179018=CARTESIAN_POINT('Ctrl Pts',(9.51640433299995,12.2,-4.53445970600002));
#179019=CARTESIAN_POINT('Ctrl Pts',(9.51489462199994,12.2,-4.53333169900001));
#179020=CARTESIAN_POINT('Ctrl Pts',(9.51338971899995,12.2,-4.53220942700002));
#179021=CARTESIAN_POINT('Ctrl Pts',(9.51188964699995,12.2,-4.53109288900002));
#179022=CARTESIAN_POINT('Ctrl Pts',(9.51039442599994,12.2,-4.52998208700001));
#179023=CARTESIAN_POINT('Ctrl Pts',(9.50890407399994,12.2,-4.52887701800002));
#179024=CARTESIAN_POINT('Ctrl Pts',(9.50741861299995,12.2,-4.52777768500002));
#179025=CARTESIAN_POINT('Ctrl Pts',(9.50593806399995,12.2,-4.52668408600001));
#179026=CARTESIAN_POINT('Ctrl Pts',(9.50446244799994,12.2,-4.52559622000001));
#179027=CARTESIAN_POINT('Ctrl Pts',(9.50299178499994,12.2,-4.52451409000002));
#179028=CARTESIAN_POINT('Ctrl Pts',(9.50152609399994,12.2,-4.52343769300001));
#179029=CARTESIAN_POINT('Ctrl Pts',(9.50006539899995,12.2,-4.52236703200001));
#179030=CARTESIAN_POINT('Ctrl Pts',(9.49860971899994,12.2,-4.52130210400002));
#179031=CARTESIAN_POINT('Ctrl Pts',(9.49715907499994,12.2,-4.52024291000001));
#179032=CARTESIAN_POINT('Ctrl Pts',(9.49571348799994,12.2,-4.51918944900001));
#179033=CARTESIAN_POINT('Ctrl Pts',(9.49427298099994,12.2,-4.51814172300002));
#179034=CARTESIAN_POINT('Ctrl Pts',(9.49283757399994,12.2,-4.51709973000002));
#179035=CARTESIAN_POINT('Ctrl Pts',(9.49140728699994,12.2,-4.51606347000002));
#179036=CARTESIAN_POINT('Ctrl Pts',(9.48998214199994,12.2,-4.51503294400001));
#179037=CARTESIAN_POINT('Ctrl Pts',(9.48856216199994,12.2,-4.51400815100001));
#179038=CARTESIAN_POINT('Ctrl Pts',(9.48714736699995,12.2,-4.51298909100001));
#179039=CARTESIAN_POINT('Ctrl Pts',(9.48573777999994,12.2,-4.51197576300002));
#179040=CARTESIAN_POINT('Ctrl Pts',(9.48433342199994,12.2,-4.51096816700002));
#179041=CARTESIAN_POINT('Ctrl Pts',(9.48293431399994,12.2,-4.50996630300001));
#179042=CARTESIAN_POINT('Ctrl Pts',(9.48154047899994,12.2,-4.50897017200001));
#179043=CARTESIAN_POINT('Ctrl Pts',(9.48015193699994,12.2,-4.50797977200001));
#179044=CARTESIAN_POINT('Ctrl Pts',(9.47876871299994,12.2,-4.50699510200002));
#179045=CARTESIAN_POINT('Ctrl Pts',(9.47739082699995,12.2,-4.50601616500002));
#179046=CARTESIAN_POINT('Ctrl Pts',(9.47601830199994,12.2,-4.50504295800001));
#179047=CARTESIAN_POINT('Ctrl Pts',(9.47465115999995,12.2,-4.50407548100001));
#179048=CARTESIAN_POINT('Ctrl Pts',(9.47328942199994,12.2,-4.50311373400002));
#179049=CARTESIAN_POINT('Ctrl Pts',(9.47193311299994,12.2,-4.50215771600002));
#179050=CARTESIAN_POINT('Ctrl Pts',(9.47058225499994,12.2,-4.50120742900001));
#179051=CARTESIAN_POINT('Ctrl Pts',(9.46923686899994,12.2,-4.50026286900002));
#179052=CARTESIAN_POINT('Ctrl Pts',(9.46789697899994,12.2,-4.49932403800001));
#179053=CARTESIAN_POINT('Ctrl Pts',(9.46656260799994,12.2,-4.49839093600001));
#179054=CARTESIAN_POINT('Ctrl Pts',(9.46523377699994,12.2,-4.49746356000002));
#179055=CARTESIAN_POINT('Ctrl Pts',(9.46391051099994,12.2,-4.49654191200001));
#179056=CARTESIAN_POINT('Ctrl Pts',(9.46259283199995,12.2,-4.49562599100001));
#179057=CARTESIAN_POINT('Ctrl Pts',(9.46128076299994,12.2,-4.49471579600001));
#179058=CARTESIAN_POINT('Ctrl Pts',(9.45997432899994,12.2,-4.49381132600001));
#179059=CARTESIAN_POINT('Ctrl Pts',(9.45867355199994,12.2,-4.49291258200001));
#179060=CARTESIAN_POINT('Ctrl Pts',(9.45737845499995,12.2,-4.49201956300001));
#179061=CARTESIAN_POINT('Ctrl Pts',(9.45608906199995,12.2,-4.49113226700002));
#179062=CARTESIAN_POINT('Ctrl Pts',(9.45480539699994,12.2,-4.49025069500002));
#179063=CARTESIAN_POINT('Ctrl Pts',(9.45352748199995,12.2,-4.48937484700001));
#179064=CARTESIAN_POINT('Ctrl Pts',(9.45225534299994,12.2,-4.48850472100002));
#179065=CARTESIAN_POINT('Ctrl Pts',(9.45098900299995,12.2,-4.48764031700001));
#179066=CARTESIAN_POINT('Ctrl Pts',(9.44972848499994,12.2,-4.48678163300002));
#179067=CARTESIAN_POINT('Ctrl Pts',(9.44847381499994,12.2,-4.48592867100002));
#179068=CARTESIAN_POINT('Ctrl Pts',(9.44722501599994,12.2,-4.48508142800002));
#179069=CARTESIAN_POINT('Ctrl Pts',(9.44598211199994,12.2,-4.48423990500002));
#179070=CARTESIAN_POINT('Ctrl Pts',(9.44474512899994,12.2,-4.48340410000001));
#179071=CARTESIAN_POINT('Ctrl Pts',(9.44351408899994,12.2,-4.48257401400001));
#179072=CARTESIAN_POINT('Ctrl Pts',(9.44228901899995,12.2,-4.48174964400001));
#179073=CARTESIAN_POINT('Ctrl Pts',(9.44106994199995,12.2,-4.48093099100001));
#179074=CARTESIAN_POINT('Ctrl Pts',(9.43985688299994,12.2,-4.48011805400002));
#179075=CARTESIAN_POINT('Ctrl Pts',(9.43864986699994,12.2,-4.47931083200002));
#179076=CARTESIAN_POINT('Ctrl Pts',(9.43744891899994,12.2,-4.47850932400002));
#179077=CARTESIAN_POINT('Ctrl Pts',(9.43625406499994,12.2,-4.47771352900002));
#179078=CARTESIAN_POINT('Ctrl Pts',(9.43506532899995,12.2,-4.47692344800001));
#179079=CARTESIAN_POINT('Ctrl Pts',(9.43388273599994,12.2,-4.47613907800001));
#179080=CARTESIAN_POINT('Ctrl Pts',(9.43270631299994,12.2,-4.47536041800001));
#179081=CARTESIAN_POINT('Ctrl Pts',(9.43153608499994,12.2,-4.47458746900002));
#179082=CARTESIAN_POINT('Ctrl Pts',(9.43037207599994,12.2,-4.47382023000001));
#179083=CARTESIAN_POINT('Ctrl Pts',(9.42921431399995,12.2,-4.47305869800001));
#179084=CARTESIAN_POINT('Ctrl Pts',(9.42806282299994,12.2,-4.47230287400001));
#179085=CARTESIAN_POINT('Ctrl Pts',(9.42691762999995,12.2,-4.47155275600001));
#179086=CARTESIAN_POINT('Ctrl Pts',(9.42577875999994,12.2,-4.47080834400001));
#179087=CARTESIAN_POINT('Ctrl Pts',(9.42464624099994,12.2,-4.47006963700002));
#179088=CARTESIAN_POINT('Ctrl Pts',(9.42352009699994,12.2,-4.46933663400001));
#179089=CARTESIAN_POINT('Ctrl Pts',(9.42240035499994,12.2,-4.46860933200002));
#179090=CARTESIAN_POINT('Ctrl Pts',(9.42128704299994,12.2,-4.46788773300002));
#179091=CARTESIAN_POINT('Ctrl Pts',(9.42018018699994,12.2,-4.46717183400001));
#179092=CARTESIAN_POINT('Ctrl Pts',(9.41907981199994,12.2,-4.46646163500001));
#179093=CARTESIAN_POINT('Ctrl Pts',(9.41798594799995,12.2,-4.46575713300001));
#179094=CARTESIAN_POINT('Ctrl Pts',(9.41689861899994,12.2,-4.46505832900002));
#179095=CARTESIAN_POINT('Ctrl Pts',(9.41581785299995,12.2,-4.46436522100001));
#179096=CARTESIAN_POINT('Ctrl Pts',(9.41474367699995,12.2,-4.46367780900002));
#179097=CARTESIAN_POINT('Ctrl Pts',(9.41367611899994,12.2,-4.46299609100001));
#179098=CARTESIAN_POINT('Ctrl Pts',(9.41261520599994,12.2,-4.46232006500002));
#179099=CARTESIAN_POINT('Ctrl Pts',(9.41156096599994,12.2,-4.46164973100001));
#179100=CARTESIAN_POINT('Ctrl Pts',(9.41051342599994,12.2,-4.46098508800001));
#179101=CARTESIAN_POINT('Ctrl Pts',(9.40947261499995,12.2,-4.46032613400002));
#179102=CARTESIAN_POINT('Ctrl Pts',(9.40843855899995,12.2,-4.45967286700002));
#179103=CARTESIAN_POINT('Ctrl Pts',(9.40741128799995,12.2,-4.45902528700001));
#179104=CARTESIAN_POINT('Ctrl Pts',(9.40639082799994,12.2,-4.45838339300002));
#179105=CARTESIAN_POINT('Ctrl Pts',(9.40537720899994,12.2,-4.45774718300001));
#179106=CARTESIAN_POINT('Ctrl Pts',(9.40437045999994,12.2,-4.45711665500002));
#179107=CARTESIAN_POINT('Ctrl Pts',(9.40337060799994,12.2,-4.45649181000002));
#179108=CARTESIAN_POINT('Ctrl Pts',(9.40237768099994,12.2,-4.45587264400002));
#179109=CARTESIAN_POINT('Ctrl Pts',(9.40139171099995,12.2,-4.45525915600001));
#179110=CARTESIAN_POINT('Ctrl Pts',(9.40041272399995,12.2,-4.45465134700001));
#179111=CARTESIAN_POINT('Ctrl Pts',(9.39944075099995,12.2,-4.45404921300002));
#179112=CARTESIAN_POINT('Ctrl Pts',(9.39847581899994,12.2,-4.45345275400001));
#179113=CARTESIAN_POINT('Ctrl Pts',(9.39751795899994,12.2,-4.45286196700001));
#179114=CARTESIAN_POINT('Ctrl Pts',(9.39656720199994,12.2,-4.45227685300001));
#179115=CARTESIAN_POINT('Ctrl Pts',(9.39562357399994,12.2,-4.45169740800001));
#179116=CARTESIAN_POINT('Ctrl Pts',(9.39468710699994,12.2,-4.45112363100002));
#179117=CARTESIAN_POINT('Ctrl Pts',(9.39375783099995,12.2,-4.45055552200001));
#179118=CARTESIAN_POINT('Ctrl Pts',(9.39283577499994,12.2,-4.44999307800002));
#179119=CARTESIAN_POINT('Ctrl Pts',(9.39192097099994,12.2,-4.44943629800001));
#179120=CARTESIAN_POINT('Ctrl Pts',(9.39101344699995,12.2,-4.44888518000001));
#179121=CARTESIAN_POINT('Ctrl Pts',(9.39011323499994,12.2,-4.44833972300001));
#179122=CARTESIAN_POINT('Ctrl Pts',(9.38922036599994,12.2,-4.44779992400001));
#179123=CARTESIAN_POINT('Ctrl Pts',(9.38833486899994,12.2,-4.44726578300001));
#179124=CARTESIAN_POINT('Ctrl Pts',(9.38745677599995,12.2,-4.44673729700002));
#179125=CARTESIAN_POINT('Ctrl Pts',(9.38658611799994,12.2,-4.44621446500001));
#179126=CARTESIAN_POINT('Ctrl Pts',(9.38572292599994,12.2,-4.44569728500001));
#179127=CARTESIAN_POINT('Ctrl Pts',(9.38486723299994,12.2,-4.44518575500001));
#179128=CARTESIAN_POINT('Ctrl Pts',(9.38401906799994,12.2,-4.44467987500001));
#179129=CARTESIAN_POINT('Ctrl Pts',(9.38317846499995,12.2,-4.44417964100001));
#179130=CARTESIAN_POINT('Ctrl Pts',(9.38234545299995,12.2,-4.44368505100002));
#179131=CARTESIAN_POINT('Ctrl Pts',(9.38152006799994,12.2,-4.44319610500001));
#179132=CARTESIAN_POINT('Ctrl Pts',(9.38070233899994,12.2,-4.44271280000001));
#179133=CARTESIAN_POINT('Ctrl Pts',(9.37989229799994,12.2,-4.44223513400001));
#179134=CARTESIAN_POINT('Ctrl Pts',(9.37908997999994,12.2,-4.44176310500001));
#179135=CARTESIAN_POINT('Ctrl Pts',(9.37829999299994,12.2,-4.44129939800002));
#179136=CARTESIAN_POINT('Ctrl Pts',(9.37767505699994,12.2,-4.44093341100002));
#179137=CARTESIAN_POINT('Ctrl Pts',(9.37721094099994,12.2,-4.44066207000001));
#179138=CARTESIAN_POINT('Ctrl Pts',(9.37690455199995,12.2,-4.44048314700002));
#179139=CARTESIAN_POINT('Ctrl Pts',(9.37675396699994,12.2,-4.44039525800001));
#179140=CARTESIAN_POINT('Ctrl Pts',(9.37675396699994,15.2,-4.44039525800001));
#179141=CARTESIAN_POINT('Ctrl Pts',(9.37690455199995,15.2,-4.44048314700002));
#179142=CARTESIAN_POINT('Ctrl Pts',(9.37721094099994,15.2,-4.44066207000001));
#179143=CARTESIAN_POINT('Ctrl Pts',(9.37767505699994,15.2,-4.44093341100002));
#179144=CARTESIAN_POINT('Ctrl Pts',(9.37829999299994,15.2,-4.44129939800002));
#179145=CARTESIAN_POINT('Ctrl Pts',(9.37908997999994,15.2,-4.44176310500001));
#179146=CARTESIAN_POINT('Ctrl Pts',(9.37989229799994,15.2,-4.44223513400001));
#179147=CARTESIAN_POINT('Ctrl Pts',(9.38070233899994,15.2,-4.44271280000001));
#179148=CARTESIAN_POINT('Ctrl Pts',(9.38152006799994,15.2,-4.44319610500001));
#179149=CARTESIAN_POINT('Ctrl Pts',(9.38234545299995,15.2,-4.44368505100002));
#179150=CARTESIAN_POINT('Ctrl Pts',(9.38317846499995,15.2,-4.44417964100001));
#179151=CARTESIAN_POINT('Ctrl Pts',(9.38401906799994,15.2,-4.44467987500001));
#179152=CARTESIAN_POINT('Ctrl Pts',(9.38486723299994,15.2,-4.44518575500001));
#179153=CARTESIAN_POINT('Ctrl Pts',(9.38572292599994,15.2,-4.44569728500001));
#179154=CARTESIAN_POINT('Ctrl Pts',(9.38658611799994,15.2,-4.44621446500001));
#179155=CARTESIAN_POINT('Ctrl Pts',(9.38745677599995,15.2,-4.44673729700002));
#179156=CARTESIAN_POINT('Ctrl Pts',(9.38833486899994,15.2,-4.44726578300001));
#179157=CARTESIAN_POINT('Ctrl Pts',(9.38922036599994,15.2,-4.44779992400001));
#179158=CARTESIAN_POINT('Ctrl Pts',(9.39011323499994,15.2,-4.44833972300001));
#179159=CARTESIAN_POINT('Ctrl Pts',(9.39101344699995,15.2,-4.44888518000001));
#179160=CARTESIAN_POINT('Ctrl Pts',(9.39192097099994,15.2,-4.44943629800001));
#179161=CARTESIAN_POINT('Ctrl Pts',(9.39283577499994,15.2,-4.44999307800002));
#179162=CARTESIAN_POINT('Ctrl Pts',(9.39375783099995,15.2,-4.45055552200001));
#179163=CARTESIAN_POINT('Ctrl Pts',(9.39468710699994,15.2,-4.45112363100002));
#179164=CARTESIAN_POINT('Ctrl Pts',(9.39562357399994,15.2,-4.45169740800001));
#179165=CARTESIAN_POINT('Ctrl Pts',(9.39656720199994,15.2,-4.45227685300001));
#179166=CARTESIAN_POINT('Ctrl Pts',(9.39751795899994,15.2,-4.45286196700001));
#179167=CARTESIAN_POINT('Ctrl Pts',(9.39847581899994,15.2,-4.45345275400001));
#179168=CARTESIAN_POINT('Ctrl Pts',(9.39944075099995,15.2,-4.45404921300002));
#179169=CARTESIAN_POINT('Ctrl Pts',(9.40041272399995,15.2,-4.45465134700001));
#179170=CARTESIAN_POINT('Ctrl Pts',(9.40139171099995,15.2,-4.45525915600001));
#179171=CARTESIAN_POINT('Ctrl Pts',(9.40237768099994,15.2,-4.45587264400002));
#179172=CARTESIAN_POINT('Ctrl Pts',(9.40337060799994,15.2,-4.45649181000002));
#179173=CARTESIAN_POINT('Ctrl Pts',(9.40437045999994,15.2,-4.45711665500002));
#179174=CARTESIAN_POINT('Ctrl Pts',(9.40537720899994,15.2,-4.45774718300001));
#179175=CARTESIAN_POINT('Ctrl Pts',(9.40639082799994,15.2,-4.45838339300002));
#179176=CARTESIAN_POINT('Ctrl Pts',(9.40741128799995,15.2,-4.45902528700001));
#179177=CARTESIAN_POINT('Ctrl Pts',(9.40843855899995,15.2,-4.45967286700002));
#179178=CARTESIAN_POINT('Ctrl Pts',(9.40947261499995,15.2,-4.46032613400002));
#179179=CARTESIAN_POINT('Ctrl Pts',(9.41051342599994,15.2,-4.46098508800001));
#179180=CARTESIAN_POINT('Ctrl Pts',(9.41156096599994,15.2,-4.46164973100001));
#179181=CARTESIAN_POINT('Ctrl Pts',(9.41261520599994,15.2,-4.46232006500002));
#179182=CARTESIAN_POINT('Ctrl Pts',(9.41367611899994,15.2,-4.46299609100001));
#179183=CARTESIAN_POINT('Ctrl Pts',(9.41474367699995,15.2,-4.46367780900002));
#179184=CARTESIAN_POINT('Ctrl Pts',(9.41581785299995,15.2,-4.46436522100001));
#179185=CARTESIAN_POINT('Ctrl Pts',(9.41689861899994,15.2,-4.46505832900002));
#179186=CARTESIAN_POINT('Ctrl Pts',(9.41798594799995,15.2,-4.46575713300001));
#179187=CARTESIAN_POINT('Ctrl Pts',(9.41907981199994,15.2,-4.46646163500001));
#179188=CARTESIAN_POINT('Ctrl Pts',(9.42018018699994,15.2,-4.46717183400001));
#179189=CARTESIAN_POINT('Ctrl Pts',(9.42128704299994,15.2,-4.46788773300002));
#179190=CARTESIAN_POINT('Ctrl Pts',(9.42240035499994,15.2,-4.46860933200002));
#179191=CARTESIAN_POINT('Ctrl Pts',(9.42352009699994,15.2,-4.46933663400001));
#179192=CARTESIAN_POINT('Ctrl Pts',(9.42464624099994,15.2,-4.47006963700002));
#179193=CARTESIAN_POINT('Ctrl Pts',(9.42577875999994,15.2,-4.47080834400001));
#179194=CARTESIAN_POINT('Ctrl Pts',(9.42691762999995,15.2,-4.47155275600001));
#179195=CARTESIAN_POINT('Ctrl Pts',(9.42806282299994,15.2,-4.47230287400001));
#179196=CARTESIAN_POINT('Ctrl Pts',(9.42921431399995,15.2,-4.47305869800001));
#179197=CARTESIAN_POINT('Ctrl Pts',(9.43037207599994,15.2,-4.47382023000001));
#179198=CARTESIAN_POINT('Ctrl Pts',(9.43153608499994,15.2,-4.47458746900002));
#179199=CARTESIAN_POINT('Ctrl Pts',(9.43270631299994,15.2,-4.47536041800001));
#179200=CARTESIAN_POINT('Ctrl Pts',(9.43388273599994,15.2,-4.47613907800001));
#179201=CARTESIAN_POINT('Ctrl Pts',(9.43506532899995,15.2,-4.47692344800001));
#179202=CARTESIAN_POINT('Ctrl Pts',(9.43625406499994,15.2,-4.47771352900002));
#179203=CARTESIAN_POINT('Ctrl Pts',(9.43744891899994,15.2,-4.47850932400002));
#179204=CARTESIAN_POINT('Ctrl Pts',(9.43864986699994,15.2,-4.47931083200002));
#179205=CARTESIAN_POINT('Ctrl Pts',(9.43985688299994,15.2,-4.48011805400002));
#179206=CARTESIAN_POINT('Ctrl Pts',(9.44106994199995,15.2,-4.48093099100001));
#179207=CARTESIAN_POINT('Ctrl Pts',(9.44228901899995,15.2,-4.48174964400001));
#179208=CARTESIAN_POINT('Ctrl Pts',(9.44351408899994,15.2,-4.48257401400001));
#179209=CARTESIAN_POINT('Ctrl Pts',(9.44474512899994,15.2,-4.48340410000001));
#179210=CARTESIAN_POINT('Ctrl Pts',(9.44598211199994,15.2,-4.48423990500002));
#179211=CARTESIAN_POINT('Ctrl Pts',(9.44722501599994,15.2,-4.48508142800002));
#179212=CARTESIAN_POINT('Ctrl Pts',(9.44847381499994,15.2,-4.48592867100002));
#179213=CARTESIAN_POINT('Ctrl Pts',(9.44972848499994,15.2,-4.48678163300002));
#179214=CARTESIAN_POINT('Ctrl Pts',(9.45098900299995,15.2,-4.48764031700001));
#179215=CARTESIAN_POINT('Ctrl Pts',(9.45225534299994,15.2,-4.48850472100002));
#179216=CARTESIAN_POINT('Ctrl Pts',(9.45352748199995,15.2,-4.48937484700001));
#179217=CARTESIAN_POINT('Ctrl Pts',(9.45480539699994,15.2,-4.49025069500002));
#179218=CARTESIAN_POINT('Ctrl Pts',(9.45608906199995,15.2,-4.49113226700002));
#179219=CARTESIAN_POINT('Ctrl Pts',(9.45737845499995,15.2,-4.49201956300001));
#179220=CARTESIAN_POINT('Ctrl Pts',(9.45867355199994,15.2,-4.49291258200001));
#179221=CARTESIAN_POINT('Ctrl Pts',(9.45997432899994,15.2,-4.49381132600001));
#179222=CARTESIAN_POINT('Ctrl Pts',(9.46128076299994,15.2,-4.49471579600001));
#179223=CARTESIAN_POINT('Ctrl Pts',(9.46259283199995,15.2,-4.49562599100001));
#179224=CARTESIAN_POINT('Ctrl Pts',(9.46391051099994,15.2,-4.49654191200001));
#179225=CARTESIAN_POINT('Ctrl Pts',(9.46523377699994,15.2,-4.49746356000002));
#179226=CARTESIAN_POINT('Ctrl Pts',(9.46656260799994,15.2,-4.49839093600001));
#179227=CARTESIAN_POINT('Ctrl Pts',(9.46789697899994,15.2,-4.49932403800001));
#179228=CARTESIAN_POINT('Ctrl Pts',(9.46923686899994,15.2,-4.50026286900002));
#179229=CARTESIAN_POINT('Ctrl Pts',(9.47058225499994,15.2,-4.50120742900001));
#179230=CARTESIAN_POINT('Ctrl Pts',(9.47193311299994,15.2,-4.50215771600002));
#179231=CARTESIAN_POINT('Ctrl Pts',(9.47328942199994,15.2,-4.50311373400002));
#179232=CARTESIAN_POINT('Ctrl Pts',(9.47465115999995,15.2,-4.50407548100001));
#179233=CARTESIAN_POINT('Ctrl Pts',(9.47601830199994,15.2,-4.50504295800001));
#179234=CARTESIAN_POINT('Ctrl Pts',(9.47739082699995,15.2,-4.50601616500002));
#179235=CARTESIAN_POINT('Ctrl Pts',(9.47876871299994,15.2,-4.50699510200002));
#179236=CARTESIAN_POINT('Ctrl Pts',(9.48015193699994,15.2,-4.50797977200001));
#179237=CARTESIAN_POINT('Ctrl Pts',(9.48154047899994,15.2,-4.50897017200001));
#179238=CARTESIAN_POINT('Ctrl Pts',(9.48293431399994,15.2,-4.50996630300001));
#179239=CARTESIAN_POINT('Ctrl Pts',(9.48433342199994,15.2,-4.51096816700002));
#179240=CARTESIAN_POINT('Ctrl Pts',(9.48573777999994,15.2,-4.51197576300002));
#179241=CARTESIAN_POINT('Ctrl Pts',(9.48714736699995,15.2,-4.51298909100001));
#179242=CARTESIAN_POINT('Ctrl Pts',(9.48856216199994,15.2,-4.51400815100001));
#179243=CARTESIAN_POINT('Ctrl Pts',(9.48998214199994,15.2,-4.51503294400001));
#179244=CARTESIAN_POINT('Ctrl Pts',(9.49140728699994,15.2,-4.51606347000002));
#179245=CARTESIAN_POINT('Ctrl Pts',(9.49283757399994,15.2,-4.51709973000002));
#179246=CARTESIAN_POINT('Ctrl Pts',(9.49427298099994,15.2,-4.51814172300002));
#179247=CARTESIAN_POINT('Ctrl Pts',(9.49571348799994,15.2,-4.51918944900001));
#179248=CARTESIAN_POINT('Ctrl Pts',(9.49715907499994,15.2,-4.52024291000001));
#179249=CARTESIAN_POINT('Ctrl Pts',(9.49860971899994,15.2,-4.52130210400002));
#179250=CARTESIAN_POINT('Ctrl Pts',(9.50006539899995,15.2,-4.52236703200001));
#179251=CARTESIAN_POINT('Ctrl Pts',(9.50152609399994,15.2,-4.52343769300001));
#179252=CARTESIAN_POINT('Ctrl Pts',(9.50299178499994,15.2,-4.52451409000002));
#179253=CARTESIAN_POINT('Ctrl Pts',(9.50446244799994,15.2,-4.52559622000001));
#179254=CARTESIAN_POINT('Ctrl Pts',(9.50593806399995,15.2,-4.52668408600001));
#179255=CARTESIAN_POINT('Ctrl Pts',(9.50741861299995,15.2,-4.52777768500002));
#179256=CARTESIAN_POINT('Ctrl Pts',(9.50890407399994,15.2,-4.52887701800002));
#179257=CARTESIAN_POINT('Ctrl Pts',(9.51039442599994,15.2,-4.52998208700001));
#179258=CARTESIAN_POINT('Ctrl Pts',(9.51188964699995,15.2,-4.53109288900002));
#179259=CARTESIAN_POINT('Ctrl Pts',(9.51338971899995,15.2,-4.53220942700002));
#179260=CARTESIAN_POINT('Ctrl Pts',(9.51489462199994,15.2,-4.53333169900001));
#179261=CARTESIAN_POINT('Ctrl Pts',(9.51640433299995,15.2,-4.53445970600002));
#179262=CARTESIAN_POINT('Ctrl Pts',(9.51791883399994,15.2,-4.53559344600002));
#179263=CARTESIAN_POINT('Ctrl Pts',(9.51943810399994,15.2,-4.53673292200001));
#179264=CARTESIAN_POINT('Ctrl Pts',(9.52096212299995,15.2,-4.53787813200002));
#179265=CARTESIAN_POINT('Ctrl Pts',(9.52249087199995,15.2,-4.53902907500002));
#179266=CARTESIAN_POINT('Ctrl Pts',(9.52402432899994,15.2,-4.54018575400001));
#179267=CARTESIAN_POINT('Ctrl Pts',(9.52556247699994,15.2,-4.54134816700002));
#179268=CARTESIAN_POINT('Ctrl Pts',(9.52710529499995,15.2,-4.54251631400002));
#179269=CARTESIAN_POINT('Ctrl Pts',(9.52865276099994,15.2,-4.54369019500001));
#179270=CARTESIAN_POINT('Ctrl Pts',(9.53020485899994,15.2,-4.54486981000001));
#179271=CARTESIAN_POINT('Ctrl Pts',(9.53176156699995,15.2,-4.54605515800001));
#179272=CARTESIAN_POINT('Ctrl Pts',(9.53332286699995,15.2,-4.54724624000002));
#179273=CARTESIAN_POINT('Ctrl Pts',(9.53488873799994,15.2,-4.54844305600002));
#179274=CARTESIAN_POINT('Ctrl Pts',(9.53645916199994,15.2,-4.54964560500001));
#179275=CARTESIAN_POINT('Ctrl Pts',(9.53803411899995,15.2,-4.55085388600001));
#179276=CARTESIAN_POINT('Ctrl Pts',(9.53961358999995,15.2,-4.55206790100001));
#179277=CARTESIAN_POINT('Ctrl Pts',(9.54119755599995,15.2,-4.55328764900001));
#179278=CARTESIAN_POINT('Ctrl Pts',(9.54278599799995,15.2,-4.55451312900002));
#179279=CARTESIAN_POINT('Ctrl Pts',(9.54437889599994,15.2,-4.55574434100001));
#179280=CARTESIAN_POINT('Ctrl Pts',(9.54597623199994,15.2,-4.55698128600002));
#179281=CARTESIAN_POINT('Ctrl Pts',(9.54757798599994,15.2,-4.55822396200002));
#179282=CARTESIAN_POINT('Ctrl Pts',(9.54918413999994,15.2,-4.55947236900001));
#179283=CARTESIAN_POINT('Ctrl Pts',(9.55079467599995,15.2,-4.56072650800001));
#179284=CARTESIAN_POINT('Ctrl Pts',(9.55240957399995,15.2,-4.56198637800002));
#179285=CARTESIAN_POINT('Ctrl Pts',(9.55402881599994,15.2,-4.56325197900001));
#179286=CARTESIAN_POINT('Ctrl Pts',(9.55565238299994,15.2,-4.56452331000001));
#179287=CARTESIAN_POINT('Ctrl Pts',(9.55728025499995,15.2,-4.56580037200002));
#179288=CARTESIAN_POINT('Ctrl Pts',(9.55891241699995,15.2,-4.56708316300002));
#179289=CARTESIAN_POINT('Ctrl Pts',(9.56054884799994,15.2,-4.56837168300002));
#179290=CARTESIAN_POINT('Ctrl Pts',(9.56218952899994,15.2,-4.56966593300002));
#179291=CARTESIAN_POINT('Ctrl Pts',(9.56383444399994,15.2,-4.57096591100001));
#179292=CARTESIAN_POINT('Ctrl Pts',(9.56548357399994,15.2,-4.57227161800001));
#179293=CARTESIAN_POINT('Ctrl Pts',(9.56713690099994,15.2,-4.57358305200001));
#179294=CARTESIAN_POINT('Ctrl Pts',(9.56879440599995,15.2,-4.57490021400002));
#179295=CARTESIAN_POINT('Ctrl Pts',(9.57045606999994,15.2,-4.57622310400001));
#179296=CARTESIAN_POINT('Ctrl Pts',(9.57212187699995,15.2,-4.57755172000001));
#179297=CARTESIAN_POINT('Ctrl Pts',(9.57379180899995,15.2,-4.57888606200001));
#179298=CARTESIAN_POINT('Ctrl Pts',(9.57546584599994,15.2,-4.58022613000002));
#179299=CARTESIAN_POINT('Ctrl Pts',(9.57714397399995,15.2,-4.58157192400002));
#179300=CARTESIAN_POINT('Ctrl Pts',(9.57882617099994,15.2,-4.58292344400002));
#179301=CARTESIAN_POINT('Ctrl Pts',(9.58051242199994,15.2,-4.58428068800002));
#179302=CARTESIAN_POINT('Ctrl Pts',(9.58220270699995,15.2,-4.58564365500001));
#179303=CARTESIAN_POINT('Ctrl Pts',(9.58389701199994,15.2,-4.58701234700001));
#179304=CARTESIAN_POINT('Ctrl Pts',(9.58559531499995,15.2,-4.58838676100001));
#179305=CARTESIAN_POINT('Ctrl Pts',(9.58729760199994,15.2,-4.58976689800001));
#179306=CARTESIAN_POINT('Ctrl Pts',(9.58900385399994,15.2,-4.59115275800002));
#179307=CARTESIAN_POINT('Ctrl Pts',(9.59071405399994,15.2,-4.59254433900002));
#179308=CARTESIAN_POINT('Ctrl Pts',(9.59242818399994,15.2,-4.59394164100001));
#179309=CARTESIAN_POINT('Ctrl Pts',(9.59414622799994,15.2,-4.59534466400001));
#179310=CARTESIAN_POINT('Ctrl Pts',(9.59586816799994,15.2,-4.59675340600001));
#179311=CARTESIAN_POINT('Ctrl Pts',(9.59759398799994,15.2,-4.59816786900001));
#179312=CARTESIAN_POINT('Ctrl Pts',(9.59932366799995,15.2,-4.59958805000001));
#179313=CARTESIAN_POINT('Ctrl Pts',(9.60105719199994,15.2,-4.60101394900001));
#179314=CARTESIAN_POINT('Ctrl Pts',(9.60279454499995,15.2,-4.60244556600002));
#179315=CARTESIAN_POINT('Ctrl Pts',(9.60453570799995,15.2,-4.60388290000001));
#179316=CARTESIAN_POINT('Ctrl Pts',(9.60628066499994,15.2,-4.60532595000001));
#179317=CARTESIAN_POINT('Ctrl Pts',(9.60802939899994,15.2,-4.60677471700001));
#179318=CARTESIAN_POINT('Ctrl Pts',(9.60978189399994,15.2,-4.60822919900002));
#179319=CARTESIAN_POINT('Ctrl Pts',(9.61153812999994,15.2,-4.60968939500002));
#179320=CARTESIAN_POINT('Ctrl Pts',(9.61329809399994,15.2,-4.61115530500001));
#179321=CARTESIAN_POINT('Ctrl Pts',(9.61506176799995,15.2,-4.61262692900001));
#179322=CARTESIAN_POINT('Ctrl Pts',(9.61682913599994,15.2,-4.61410426600001));
#179323=CARTESIAN_POINT('Ctrl Pts',(9.61860017899994,15.2,-4.61558731400002));
#179324=CARTESIAN_POINT('Ctrl Pts',(9.62037488299995,15.2,-4.61707607400001));
#179325=CARTESIAN_POINT('Ctrl Pts',(9.62215323099995,15.2,-4.61857054400001));
#179326=CARTESIAN_POINT('Ctrl Pts',(9.62393520599995,15.2,-4.62007072400001));
#179327=CARTESIAN_POINT('Ctrl Pts',(9.62572079199994,15.2,-4.62157661300001));
#179328=CARTESIAN_POINT('Ctrl Pts',(9.62750997299995,15.2,-4.62308821200001));
#179329=CARTESIAN_POINT('Ctrl Pts',(9.62930273199994,15.2,-4.62460551700001));
#179330=CARTESIAN_POINT('Ctrl Pts',(9.63109905299994,15.2,-4.62612853000001));
#179331=CARTESIAN_POINT('Ctrl Pts',(9.63289892099995,15.2,-4.62765724900001));
#179332=CARTESIAN_POINT('Ctrl Pts',(9.63470231799995,15.2,-4.62919167300001));
#179333=CARTESIAN_POINT('Ctrl Pts',(9.63650922799994,15.2,-4.63073180200002));
#179334=CARTESIAN_POINT('Ctrl Pts',(9.63831963699995,15.2,-4.63227763600001));
#179335=CARTESIAN_POINT('Ctrl Pts',(9.64013352699994,15.2,-4.63382917200001));
#179336=CARTESIAN_POINT('Ctrl Pts',(9.64195088399994,15.2,-4.63538641000001));
#179337=CARTESIAN_POINT('Ctrl Pts',(9.64377168999994,15.2,-4.63694935100001));
#179338=CARTESIAN_POINT('Ctrl Pts',(9.64559592999995,15.2,-4.63851799300001));
#179339=CARTESIAN_POINT('Ctrl Pts',(9.64742358899995,15.2,-4.64009233400001));
#179340=CARTESIAN_POINT('Ctrl Pts',(9.64925464999994,15.2,-4.64167237400002));
#179341=CARTESIAN_POINT('Ctrl Pts',(9.65108909699994,15.2,-4.64325811300002));
#179342=CARTESIAN_POINT('Ctrl Pts',(9.65292691699995,15.2,-4.64484954900001));
#179343=CARTESIAN_POINT('Ctrl Pts',(9.65476809099994,15.2,-4.64644668200001));
#179344=CARTESIAN_POINT('Ctrl Pts',(9.65661260499994,15.2,-4.64804951100001));
#179345=CARTESIAN_POINT('Ctrl Pts',(9.65846044499994,15.2,-4.64965803400001));
#179346=CARTESIAN_POINT('Ctrl Pts',(9.66031159299994,15.2,-4.65127225200002));
#179347=CARTESIAN_POINT('Ctrl Pts',(9.66216603399995,15.2,-4.65289216300001));
#179348=CARTESIAN_POINT('Ctrl Pts',(9.66402375299995,15.2,-4.65451776500001));
#179349=CARTESIAN_POINT('Ctrl Pts',(9.66588473599994,15.2,-4.65614906000001));
#179350=CARTESIAN_POINT('Ctrl Pts',(9.66774896599994,15.2,-4.65778604500001));
#179351=CARTESIAN_POINT('Ctrl Pts',(9.66961642799994,15.2,-4.65942871900001));
#179352=CARTESIAN_POINT('Ctrl Pts',(9.67148710599995,15.2,-4.66107708200001));
#179353=CARTESIAN_POINT('Ctrl Pts',(9.67336098799995,15.2,-4.66273113300002));
#179354=CARTESIAN_POINT('Ctrl Pts',(9.67523805399994,15.2,-4.66439087100001));
#179355=CARTESIAN_POINT('Ctrl Pts',(9.67711829399994,15.2,-4.66605629400001));
#179356=CARTESIAN_POINT('Ctrl Pts',(9.67900168899994,15.2,-4.66772740200001));
#179357=CARTESIAN_POINT('Ctrl Pts',(9.68088822599995,15.2,-4.66940419300002));
#179358=CARTESIAN_POINT('Ctrl Pts',(9.68277788899995,15.2,-4.67108666800002));
#179359=CARTESIAN_POINT('Ctrl Pts',(9.68467066399995,15.2,-4.67277482500001));
#179360=CARTESIAN_POINT('Ctrl Pts',(9.68656653499995,15.2,-4.67446866300001));
#179361=CARTESIAN_POINT('Ctrl Pts',(9.68846548899995,15.2,-4.67616818100002));
#179362=CARTESIAN_POINT('Ctrl Pts',(9.69036750899994,15.2,-4.67787337800001));
#179363=CARTESIAN_POINT('Ctrl Pts',(9.69227258299994,15.2,-4.67958425200001));
#179364=CARTESIAN_POINT('Ctrl Pts',(9.69418069299994,15.2,-4.68130080300002));
#179365=CARTESIAN_POINT('Ctrl Pts',(9.69609182599994,15.2,-4.68302303000002));
#179366=CARTESIAN_POINT('Ctrl Pts',(9.69800596699995,15.2,-4.68475093300002));
#179367=CARTESIAN_POINT('Ctrl Pts',(9.69992310199994,15.2,-4.68648450800002));
#179368=CARTESIAN_POINT('Ctrl Pts',(9.70184321499995,15.2,-4.68822375800002));
#179369=CARTESIAN_POINT('Ctrl Pts',(9.70376629399994,15.2,-4.68996867700001));
#179370=CARTESIAN_POINT('Ctrl Pts',(9.70569232299994,15.2,-4.69171926800001));
#179371=CARTESIAN_POINT('Ctrl Pts',(9.70762128699995,15.2,-4.69347552800001));
#179372=CARTESIAN_POINT('Ctrl Pts',(9.70955317199994,15.2,-4.69523745800001));
#179373=CARTESIAN_POINT('Ctrl Pts',(9.71148796399994,15.2,-4.69700505400001));
#179374=CARTESIAN_POINT('Ctrl Pts',(9.71342564799994,15.2,-4.69877831600002));
#179375=CARTESIAN_POINT('Ctrl Pts',(9.71536621099995,15.2,-4.70055724400002));
#179376=CARTESIAN_POINT('Ctrl Pts',(9.71730963799994,15.2,-4.70234183600001));
#179377=CARTESIAN_POINT('Ctrl Pts',(9.71925591399994,15.2,-4.70413209100002));
#179378=CARTESIAN_POINT('Ctrl Pts',(9.72120502599994,15.2,-4.70592800700001));
#179379=CARTESIAN_POINT('Ctrl Pts',(9.72315695899994,15.2,-4.70772958400001));
#179380=CARTESIAN_POINT('Ctrl Pts',(9.72511169899994,15.2,-4.70953682000002));
#179381=CARTESIAN_POINT('Ctrl Pts',(9.72706923299994,15.2,-4.71134971600002));
#179382=CARTESIAN_POINT('Ctrl Pts',(9.72902954599994,15.2,-4.71316826800001));
#179383=CARTESIAN_POINT('Ctrl Pts',(9.73099262399994,15.2,-4.71499247700002));
#179384=CARTESIAN_POINT('Ctrl Pts',(9.73295845299995,15.2,-4.71682234000002));
#179385=CARTESIAN_POINT('Ctrl Pts',(9.73492701999995,15.2,-4.71865785700002));
#179386=CARTESIAN_POINT('Ctrl Pts',(9.73689830999995,15.2,-4.72049902600002));
#179387=CARTESIAN_POINT('Ctrl Pts',(9.73887230999994,15.2,-4.72234584700002));
#179388=CARTESIAN_POINT('Ctrl Pts',(9.74084900499994,15.2,-4.72419831800002));
#179389=CARTESIAN_POINT('Ctrl Pts',(9.74282838199995,15.2,-4.72605643900001));
#179390=CARTESIAN_POINT('Ctrl Pts',(9.74481042799994,15.2,-4.72792020600002));
#179391=CARTESIAN_POINT('Ctrl Pts',(9.74679512899994,15.2,-4.72978962000001));
#179392=CARTESIAN_POINT('Ctrl Pts',(9.74878246899994,15.2,-4.73166467900001));
#179393=CARTESIAN_POINT('Ctrl Pts',(9.75077243699995,15.2,-4.73354538300002));
#179394=CARTESIAN_POINT('Ctrl Pts',(9.75276501899994,15.2,-4.73543173000001));
#179395=CARTESIAN_POINT('Ctrl Pts',(9.75476020099994,15.2,-4.73732371700001));
#179396=CARTESIAN_POINT('Ctrl Pts',(9.75675797099995,15.2,-4.73922134600001));
#179397=CARTESIAN_POINT('Ctrl Pts',(9.75875831199994,15.2,-4.74112461300002));
#179398=CARTESIAN_POINT('Ctrl Pts',(9.76076121399995,15.2,-4.74303351800001));
#179399=CARTESIAN_POINT('Ctrl Pts',(9.76276666199994,15.2,-4.74494806000001));
#179400=CARTESIAN_POINT('Ctrl Pts',(9.76477464199995,15.2,-4.74686823700001));
#179401=CARTESIAN_POINT('Ctrl Pts',(9.76678514199994,15.2,-4.74879404700001));
#179402=CARTESIAN_POINT('Ctrl Pts',(9.76879814799995,15.2,-4.75072549100001));
#179403=CARTESIAN_POINT('Ctrl Pts',(9.77081364699995,15.2,-4.75266256500001));
#179404=CARTESIAN_POINT('Ctrl Pts',(9.77283162499995,15.2,-4.75460527100001));
#179405=CARTESIAN_POINT('Ctrl Pts',(9.77485206899994,15.2,-4.75655360400001));
#179406=CARTESIAN_POINT('Ctrl Pts',(9.77687496799994,15.2,-4.75850756500002));
#179407=CARTESIAN_POINT('Ctrl Pts',(9.77890030599994,15.2,-4.76046715200001));
#179408=CARTESIAN_POINT('Ctrl Pts',(9.78092806999994,15.2,-4.76243236400002));
#179409=CARTESIAN_POINT('Ctrl Pts',(9.78295824899994,15.2,-4.76440319900002));
#179410=CARTESIAN_POINT('Ctrl Pts',(9.78499082799994,15.2,-4.76637965700001));
#179411=CARTESIAN_POINT('Ctrl Pts',(9.78702579499994,15.2,-4.76836173400002));
#179412=CARTESIAN_POINT('Ctrl Pts',(9.78906313699994,15.2,-4.77034943200001));
#179413=CARTESIAN_POINT('Ctrl Pts',(9.79110284099994,15.2,-4.77234274600002));
#179414=CARTESIAN_POINT('Ctrl Pts',(9.79314489299994,15.2,-4.77434167900002));
#179415=CARTESIAN_POINT('Ctrl Pts',(9.79518928099995,15.2,-4.77634622600001));
#179416=CARTESIAN_POINT('Ctrl Pts',(9.79723599299994,15.2,-4.77835638700002));
#179417=CARTESIAN_POINT('Ctrl Pts',(9.79928501499994,15.2,-4.78037216000001));
#179418=CARTESIAN_POINT('Ctrl Pts',(9.80133633399995,15.2,-4.78239354400001));
#179419=CARTESIAN_POINT('Ctrl Pts',(9.80338993799995,15.2,-4.78442053800002));
#179420=CARTESIAN_POINT('Ctrl Pts',(9.80544581399995,15.2,-4.78645314000001));
#179421=CARTESIAN_POINT('Ctrl Pts',(9.80750394899994,15.2,-4.78849134900001));
#179422=CARTESIAN_POINT('Ctrl Pts',(9.80956432999994,15.2,-4.79053516400001));
#179423=CARTESIAN_POINT('Ctrl Pts',(9.81162694599995,15.2,-4.79258458200002));
#179424=CARTESIAN_POINT('Ctrl Pts',(9.81369178299994,15.2,-4.79463960300002));
#179425=CARTESIAN_POINT('Ctrl Pts',(9.81575882799994,15.2,-4.79670022500001));
#179426=CARTESIAN_POINT('Ctrl Pts',(9.81782806999994,15.2,-4.79876644700001));
#179427=CARTESIAN_POINT('Ctrl Pts',(9.81989949599994,15.2,-4.80083826600001));
#179428=CARTESIAN_POINT('Ctrl Pts',(9.82197309199995,15.2,-4.80291568300002));
#179429=CARTESIAN_POINT('Ctrl Pts',(9.82404884799994,15.2,-4.80499869500001));
#179430=CARTESIAN_POINT('Ctrl Pts',(9.82612674899995,15.2,-4.80708730000002));
#179431=CARTESIAN_POINT('Ctrl Pts',(9.82820678499994,15.2,-4.80918149800001));
#179432=CARTESIAN_POINT('Ctrl Pts',(9.83028894099995,15.2,-4.81128128700002));
#179433=CARTESIAN_POINT('Ctrl Pts',(9.83237320799994,15.2,-4.81338666500001));
#179434=CARTESIAN_POINT('Ctrl Pts',(9.83445956999994,15.2,-4.81549763000002));
#179435=CARTESIAN_POINT('Ctrl Pts',(9.83654801799995,15.2,-4.81761418300001));
#179436=CARTESIAN_POINT('Ctrl Pts',(9.83863853799994,15.2,-4.81973632000001));
#179437=CARTESIAN_POINT('Ctrl Pts',(9.84073111699994,15.2,-4.82186404000001));
#179438=CARTESIAN_POINT('Ctrl Pts',(9.84282574499994,15.2,-4.82399734200001));
#179439=CARTESIAN_POINT('Ctrl Pts',(9.84492240799995,15.2,-4.82613622400001));
#179440=CARTESIAN_POINT('Ctrl Pts',(9.84702109499995,15.2,-4.82828068500002));
#179441=CARTESIAN_POINT('Ctrl Pts',(9.84912179299995,15.2,-4.83043072400001));
#179442=CARTESIAN_POINT('Ctrl Pts',(9.85122449199994,15.2,-4.83258633800002));
#179443=CARTESIAN_POINT('Ctrl Pts',(9.85332917699995,15.2,-4.83474752600001));
#179444=CARTESIAN_POINT('Ctrl Pts',(9.85543583699994,15.2,-4.83691428600002));
#179445=CARTESIAN_POINT('Ctrl Pts',(9.85754445999994,15.2,-4.83908661700001));
#179446=CARTESIAN_POINT('Ctrl Pts',(9.85965503599994,15.2,-4.84126451800002));
#179447=CARTESIAN_POINT('Ctrl Pts',(9.86176754899994,15.2,-4.84344798700001));
#179448=CARTESIAN_POINT('Ctrl Pts',(9.86388199199994,15.2,-4.84563702200001));
#179449=CARTESIAN_POINT('Ctrl Pts',(9.86599834899994,15.2,-4.84783162100001));
#179450=CARTESIAN_POINT('Ctrl Pts',(9.86811660899994,15.2,-4.85003178400001));
#179451=CARTESIAN_POINT('Ctrl Pts',(9.87023676299994,15.2,-4.85223750900001));
#179452=CARTESIAN_POINT('Ctrl Pts',(9.87235879499995,15.2,-4.85444879300001));
#179453=CARTESIAN_POINT('Ctrl Pts',(9.87448269599994,15.2,-4.85666563600001));
#179454=CARTESIAN_POINT('Ctrl Pts',(9.87660845399994,15.2,-4.85888803500002));
#179455=CARTESIAN_POINT('Ctrl Pts',(9.87873605699994,15.2,-4.86111598900001));
#179456=CARTESIAN_POINT('Ctrl Pts',(9.88086549299994,15.2,-4.86334949700002));
#179457=CARTESIAN_POINT('Ctrl Pts',(9.88299674999995,15.2,-4.86558855600002));
#179458=CARTESIAN_POINT('Ctrl Pts',(9.88512981699994,15.2,-4.86783316500001));
#179459=CARTESIAN_POINT('Ctrl Pts',(9.88726468299994,15.2,-4.87008332300002));
#179460=CARTESIAN_POINT('Ctrl Pts',(9.88940133499994,15.2,-4.87233902900002));
#179461=CARTESIAN_POINT('Ctrl Pts',(9.89153976099994,15.2,-4.87460027900001));
#179462=CARTESIAN_POINT('Ctrl Pts',(9.89367995199995,15.2,-4.87686707300002));
#179463=CARTESIAN_POINT('Ctrl Pts',(9.89582189499994,15.2,-4.87913940900001));
#179464=CARTESIAN_POINT('Ctrl Pts',(9.89796557699995,15.2,-4.88141728600001));
#179465=CARTESIAN_POINT('Ctrl Pts',(9.90011098899994,15.2,-4.88370070000002));
#179466=CARTESIAN_POINT('Ctrl Pts',(9.90225811999995,15.2,-4.88598965200001));
#179467=CARTESIAN_POINT('Ctrl Pts',(9.90440695499995,15.2,-4.88828413900002));
#179468=CARTESIAN_POINT('Ctrl Pts',(9.90655748599995,15.2,-4.89058415900002));
#179469=CARTESIAN_POINT('Ctrl Pts',(9.90870969999994,15.2,-4.89288971200001));
#179470=CARTESIAN_POINT('Ctrl Pts',(9.91086358699994,15.2,-4.89520079400001));
#179471=CARTESIAN_POINT('Ctrl Pts',(9.91301913399995,15.2,-4.89751740500001));
#179472=CARTESIAN_POINT('Ctrl Pts',(9.91517632999994,15.2,-4.89983954200001));
#179473=CARTESIAN_POINT('Ctrl Pts',(9.91733516599995,15.2,-4.90216720500001));
#179474=CARTESIAN_POINT('Ctrl Pts',(9.91949562799994,15.2,-4.90450039100002));
#179475=CARTESIAN_POINT('Ctrl Pts',(9.92165770599994,15.2,-4.90683909900001));
#179476=CARTESIAN_POINT('Ctrl Pts',(9.92382138899995,15.2,-4.90918332600002));
#179477=CARTESIAN_POINT('Ctrl Pts',(9.92598666499994,15.2,-4.91153307200001));
#179478=CARTESIAN_POINT('Ctrl Pts',(9.92815352399995,15.2,-4.91388833500002));
#179479=CARTESIAN_POINT('Ctrl Pts',(9.93032195399994,15.2,-4.91624911100002));
#179480=CARTESIAN_POINT('Ctrl Pts',(9.93249194399995,15.2,-4.91861540000002));
#179481=CARTESIAN_POINT('Ctrl Pts',(9.93466348399994,15.2,-4.92098720100001));
#179482=CARTESIAN_POINT('Ctrl Pts',(9.93683656099994,15.2,-4.92336451100002));
#179483=CARTESIAN_POINT('Ctrl Pts',(9.93901116599995,15.2,-4.92574732900001));
#179484=CARTESIAN_POINT('Ctrl Pts',(9.94118728699994,15.2,-4.92813565300001));
#179485=CARTESIAN_POINT('Ctrl Pts',(9.94336491299994,15.2,-4.93052948100001));
#179486=CARTESIAN_POINT('Ctrl Pts',(9.94554403299994,15.2,-4.93292881000002));
#179487=CARTESIAN_POINT('Ctrl Pts',(9.94772463699995,15.2,-4.93533364100001));
#179488=CARTESIAN_POINT('Ctrl Pts',(9.94990671399995,15.2,-4.93774397000001));
#179489=CARTESIAN_POINT('Ctrl Pts',(9.95209025099994,15.2,-4.94015979700002));
#179490=CARTESIAN_POINT('Ctrl Pts',(9.95427523999994,15.2,-4.94258111700002));
#179491=CARTESIAN_POINT('Ctrl Pts',(9.95646166799995,15.2,-4.94500793200002));
#179492=CARTESIAN_POINT('Ctrl Pts',(9.95864952599995,15.2,-4.94744023800001));
#179493=CARTESIAN_POINT('Ctrl Pts',(9.96083880199994,15.2,-4.94987803500001));
#179494=CARTESIAN_POINT('Ctrl Pts',(9.96302948499994,15.2,-4.95232131800002));
#179495=CARTESIAN_POINT('Ctrl Pts',(9.96522156599994,15.2,-4.95477008800002));
#179496=CARTESIAN_POINT('Ctrl Pts',(9.96741503199994,15.2,-4.95722434200002));
#179497=CARTESIAN_POINT('Ctrl Pts',(9.96960987299994,15.2,-4.95968407800001));
#179498=CARTESIAN_POINT('Ctrl Pts',(9.97180608099995,15.2,-4.96214929600002));
#179499=CARTESIAN_POINT('Ctrl Pts',(9.97400364199994,15.2,-4.96461999100001));
#179500=CARTESIAN_POINT('Ctrl Pts',(9.97620254699994,15.2,-4.96709616400001));
#179501=CARTESIAN_POINT('Ctrl Pts',(9.97840278499995,15.2,-4.96957781100001));
#179502=CARTESIAN_POINT('Ctrl Pts',(9.98060434499994,15.2,-4.97206493200002));
#179503=CARTESIAN_POINT('Ctrl Pts',(9.98280721699994,15.2,-4.97455752400001));
#179504=CARTESIAN_POINT('Ctrl Pts',(9.98501138999995,15.2,-4.97705558600002));
#179505=CARTESIAN_POINT('Ctrl Pts',(9.98721685399994,15.2,-4.97955911500001));
#179506=CARTESIAN_POINT('Ctrl Pts',(9.98942359899995,15.2,-4.98206811000002));
#179507=CARTESIAN_POINT('Ctrl Pts',(9.99163161399995,15.2,-4.98458256900001));
#179508=CARTESIAN_POINT('Ctrl Pts',(9.99384088799994,15.2,-4.98710249000001));
#179509=CARTESIAN_POINT('Ctrl Pts',(9.99605141199994,15.2,-4.98962787000002));
#179510=CARTESIAN_POINT('Ctrl Pts',(9.99826317399994,15.2,-4.99215870900001));
#179511=CARTESIAN_POINT('Ctrl Pts',(10.0004761639999,15.2,-4.99469500400001));
#179512=CARTESIAN_POINT('Ctrl Pts',(10.0026903729999,15.2,-4.99723675300002));
#179513=CARTESIAN_POINT('Ctrl Pts',(10.0049057889999,15.2,-4.99978395500001));
#179514=CARTESIAN_POINT('Ctrl Pts',(10.0071224029999,15.2,-5.00233660800002));
#179515=CARTESIAN_POINT('Ctrl Pts',(10.0093402039999,15.2,-5.00489470900002));
#179516=CARTESIAN_POINT('Ctrl Pts',(10.0115591819999,15.2,-5.00745825600001));
#179517=CARTESIAN_POINT('Ctrl Pts',(10.0137793259999,15.2,-5.01002724800002));
#179518=CARTESIAN_POINT('Ctrl Pts',(10.0160006259999,15.2,-5.01260168400002));
#179519=CARTESIAN_POINT('Ctrl Pts',(10.0182230729999,15.2,-5.01518156000001));
#179520=CARTESIAN_POINT('Ctrl Pts',(10.0204466549999,15.2,-5.01776687600001));
#179521=CARTESIAN_POINT('Ctrl Pts',(10.0226713639999,15.2,-5.02035762800002));
#179522=CARTESIAN_POINT('Ctrl Pts',(10.0248971889999,15.2,-5.02295381500002));
#179523=CARTESIAN_POINT('Ctrl Pts',(10.0271241189999,15.2,-5.02555543600002));
#179524=CARTESIAN_POINT('Ctrl Pts',(10.0293521449999,15.2,-5.02816248700002));
#179525=CARTESIAN_POINT('Ctrl Pts',(10.0315812549999,15.2,-5.03077496800001));
#179526=CARTESIAN_POINT('Ctrl Pts',(10.0338114419999,15.2,-5.03339287600001));
#179527=CARTESIAN_POINT('Ctrl Pts',(10.0360426939999,15.2,-5.03601620900001));
#179528=CARTESIAN_POINT('Ctrl Pts',(10.0382750009999,15.2,-5.03864496500002));
#179529=CARTESIAN_POINT('Ctrl Pts',(10.0405083539999,15.2,-5.04127914300001));
#179530=CARTESIAN_POINT('Ctrl Pts',(10.0427427419999,15.2,-5.04391874100001));
#179531=CARTESIAN_POINT('Ctrl Pts',(10.0449781559999,15.2,-5.04656375500002));
#179532=CARTESIAN_POINT('Ctrl Pts',(10.0472145849999,15.2,-5.04921418600001));
#179533=CARTESIAN_POINT('Ctrl Pts',(10.0494520199999,15.2,-5.05187002900001));
#179534=CARTESIAN_POINT('Ctrl Pts',(10.0516904509999,15.2,-5.05453128400001));
#179535=CARTESIAN_POINT('Ctrl Pts',(10.0539298679999,15.2,-5.05719794800001));
#179536=CARTESIAN_POINT('Ctrl Pts',(10.0561702599999,15.2,-5.05987001900001));
#179537=CARTESIAN_POINT('Ctrl Pts',(10.0584116189999,15.2,-5.06254749600001));
#179538=CARTESIAN_POINT('Ctrl Pts',(10.0606539349999,15.2,-5.06523037500001));
#179539=CARTESIAN_POINT('Ctrl Pts',(10.0628971959999,15.2,-5.06791865600002));
#179540=CARTESIAN_POINT('Ctrl Pts',(10.0651413949999,15.2,-5.07061233700002));
#179541=CARTESIAN_POINT('Ctrl Pts',(10.0673865209999,15.2,-5.07331141500002));
#179542=CARTESIAN_POINT('Ctrl Pts',(10.0696325649999,15.2,-5.07601588800001));
#179543=CARTESIAN_POINT('Ctrl Pts',(10.0718795159999,15.2,-5.07872575400001));
#179544=CARTESIAN_POINT('Ctrl Pts',(10.0741273649999,15.2,-5.08144101100001));
#179545=CARTESIAN_POINT('Ctrl Pts',(10.0763761029999,15.2,-5.08416165800002));
#179546=CARTESIAN_POINT('Ctrl Pts',(10.0786257189999,15.2,-5.08688769200001));
#179547=CARTESIAN_POINT('Ctrl Pts',(10.0808762039999,15.2,-5.08961911000001));
#179548=CARTESIAN_POINT('Ctrl Pts',(10.0831275479999,15.2,-5.09235591100001));
#179549=CARTESIAN_POINT('Ctrl Pts',(10.0853797429999,15.2,-5.09509809400001));
#179550=CARTESIAN_POINT('Ctrl Pts',(10.0876327779999,15.2,-5.09784565500001));
#179551=CARTESIAN_POINT('Ctrl Pts',(10.0898866439999,15.2,-5.10059859300001));
#179552=CARTESIAN_POINT('Ctrl Pts',(10.0921413299999,15.2,-5.10335690500002));
#179553=CARTESIAN_POINT('Ctrl Pts',(10.0943968289999,15.2,-5.10612059000001));
#179554=CARTESIAN_POINT('Ctrl Pts',(10.0966531299999,15.2,-5.10888964500001));
#179555=CARTESIAN_POINT('Ctrl Pts',(10.0989102229999,15.2,-5.11166406900001));
#179556=CARTESIAN_POINT('Ctrl Pts',(10.1011680999999,15.2,-5.11444386000001));
#179557=CARTESIAN_POINT('Ctrl Pts',(10.1034267499999,15.2,-5.11722901400002));
#179558=CARTESIAN_POINT('Ctrl Pts',(10.1056861639999,15.2,-5.12001953100001));
#179559=CARTESIAN_POINT('Ctrl Pts',(10.1079463349999,15.2,-5.12281540800001));
#179560=CARTESIAN_POINT('Ctrl Pts',(10.1102072499999,15.2,-5.12561664200001));
#179561=CARTESIAN_POINT('Ctrl Pts',(10.1124689019999,15.2,-5.12842323200001));
#179562=CARTESIAN_POINT('Ctrl Pts',(10.1147312799999,15.2,-5.13123517600001));
#179563=CARTESIAN_POINT('Ctrl Pts',(10.1169943759999,15.2,-5.13405247200001));
#179564=CARTESIAN_POINT('Ctrl Pts',(10.1192581799999,15.2,-5.13687511700001));
#179565=CARTESIAN_POINT('Ctrl Pts',(10.1215226839999,15.2,-5.13970310900001));
#179566=CARTESIAN_POINT('Ctrl Pts',(10.1237878759999,15.2,-5.14253644700001));
#179567=CARTESIAN_POINT('Ctrl Pts',(10.1260537499999,15.2,-5.14537512800001));
#179568=CARTESIAN_POINT('Ctrl Pts',(10.1283202939999,15.2,-5.14821914900002));
#179569=CARTESIAN_POINT('Ctrl Pts',(10.1305874999999,15.2,-5.15106851000001));
#179570=CARTESIAN_POINT('Ctrl Pts',(10.1328553589999,15.2,-5.15392320600002));
#179571=CARTESIAN_POINT('Ctrl Pts',(10.1351238609999,15.2,-5.15678323800001));
#179572=CARTESIAN_POINT('Ctrl Pts',(10.1373929979999,15.2,-5.15964860200001));
#179573=CARTESIAN_POINT('Ctrl Pts',(10.1396627609999,15.2,-5.16251929700001));
#179574=CARTESIAN_POINT('Ctrl Pts',(10.1419331389999,15.2,-5.16539531900001));
#179575=CARTESIAN_POINT('Ctrl Pts',(10.1442041239999,15.2,-5.16827666700001));
#179576=CARTESIAN_POINT('Ctrl Pts',(10.1464757069999,15.2,-5.17116333800002));
#179577=CARTESIAN_POINT('Ctrl Pts',(10.1487478799999,15.2,-5.17405533200002));
#179578=CARTESIAN_POINT('Ctrl Pts',(10.1510206309999,15.2,-5.17695264500002));
#179579=CARTESIAN_POINT('Ctrl Pts',(10.1532939539999,15.2,-5.17985527400001));
#179580=CARTESIAN_POINT('Ctrl Pts',(10.1555678379999,15.2,-5.18276321900002));
#179581=CARTESIAN_POINT('Ctrl Pts',(10.1578422729999,15.2,-5.18567647600001));
#179582=CARTESIAN_POINT('Ctrl Pts',(10.1601172529999,15.2,-5.18859504400002));
#179583=CARTESIAN_POINT('Ctrl Pts',(10.1623927679999,15.2,-5.19151892100002));
#179584=CARTESIAN_POINT('Ctrl Pts',(10.1646688079999,15.2,-5.19444810300001));
#179585=CARTESIAN_POINT('Ctrl Pts',(10.1669453649999,15.2,-5.19738259100002));
#179586=CARTESIAN_POINT('Ctrl Pts',(10.1692224309999,15.2,-5.20032238000002));
#179587=CARTESIAN_POINT('Ctrl Pts',(10.1714999969999,15.2,-5.20326746900002));
#179588=CARTESIAN_POINT('Ctrl Pts',(10.1737780519999,15.2,-5.20621785500001));
#179589=CARTESIAN_POINT('Ctrl Pts',(10.1760565879999,15.2,-5.20917353600002));
#179590=CARTESIAN_POINT('Ctrl Pts',(10.1783355949999,15.2,-5.21213451000001));
#179591=CARTESIAN_POINT('Ctrl Pts',(10.1806150639999,15.2,-5.21510077400002));
#179592=CARTESIAN_POINT('Ctrl Pts',(10.1828949879999,15.2,-5.21807232700001));
#179593=CARTESIAN_POINT('Ctrl Pts',(10.1851753559999,15.2,-5.22104916700001));
#179594=CARTESIAN_POINT('Ctrl Pts',(10.1874561619999,15.2,-5.22403129000002));
#179595=CARTESIAN_POINT('Ctrl Pts',(10.1897373969999,15.2,-5.22701869500001));
#179596=CARTESIAN_POINT('Ctrl Pts',(10.1920190549999,15.2,-5.23001138000001));
#179597=CARTESIAN_POINT('Ctrl Pts',(10.1943011249999,15.2,-5.23300934300002));
#179598=CARTESIAN_POINT('Ctrl Pts',(10.1965835999999,15.2,-5.23601258300001));
#179599=CARTESIAN_POINT('Ctrl Pts',(10.1988664679999,15.2,-5.23902109400002));
#179600=CARTESIAN_POINT('Ctrl Pts',(10.2011497209999,15.2,-5.24203487700001));
#179601=CARTESIAN_POINT('Ctrl Pts',(10.2034333439999,15.2,-5.24505392700001));
#179602=CARTESIAN_POINT('Ctrl Pts',(10.2057173299999,15.2,-5.24807824100002));
#179603=CARTESIAN_POINT('Ctrl Pts',(10.2080016679999,15.2,-5.25110781800001));
#179604=CARTESIAN_POINT('Ctrl Pts',(10.2102863519999,15.2,-5.25414265600002));
#179605=CARTESIAN_POINT('Ctrl Pts',(10.2125713739999,15.2,-5.25718275100001));
#179606=CARTESIAN_POINT('Ctrl Pts',(10.2148567309999,15.2,-5.26022810500002));
#179607=CARTESIAN_POINT('Ctrl Pts',(10.2171424209999,15.2,-5.26327871600001));
#179608=CARTESIAN_POINT('Ctrl Pts',(10.2189712369999,15.2,-5.26572340900001));
#179609=CARTESIAN_POINT('Ctrl Pts',(10.2203429999999,15.2,-5.26755929400001));
#179610=CARTESIAN_POINT('Ctrl Pts',(10.2212575739999,15.2,-5.26878426900002));
#179611=CARTESIAN_POINT('Ctrl Pts',(10.2217148779999,15.2,-5.26939701900002));
#179612=CARTESIAN_POINT('Ctrl Pts',(8.88241603299995,15.2,-5.36127880600001));
#179613=CARTESIAN_POINT('Ctrl Pts',(8.88241603299995,11.6,-5.36127880600001));
#179614=CARTESIAN_POINT('Ctrl Pts',(8.88257249699994,15.2,-5.36135574400001));
#179615=CARTESIAN_POINT('Ctrl Pts',(8.88257249699994,11.6,-5.36135574400001));
#179616=CARTESIAN_POINT('Ctrl Pts',(8.88289092999995,15.2,-5.36151222900001));
#179617=CARTESIAN_POINT('Ctrl Pts',(8.88289092999995,11.6,-5.36151222900001));
#179618=CARTESIAN_POINT('Ctrl Pts',(8.88337354799994,15.2,-5.36174910400002));
#179619=CARTESIAN_POINT('Ctrl Pts',(8.88337354799994,11.6,-5.36174910400002));
#179620=CARTESIAN_POINT('Ctrl Pts',(8.88402391699995,15.2,-5.36206771000002));
#179621=CARTESIAN_POINT('Ctrl Pts',(8.88402391699995,11.6,-5.36206771000002));
#179622=CARTESIAN_POINT('Ctrl Pts',(8.88484693799995,15.2,-5.36246988000002));
#179623=CARTESIAN_POINT('Ctrl Pts',(8.88484693799995,11.6,-5.36246988000002));
#179624=CARTESIAN_POINT('Ctrl Pts',(8.88568370899995,15.2,-5.36287772900002));
#179625=CARTESIAN_POINT('Ctrl Pts',(8.88568370899995,11.6,-5.36287772900002));
#179626=CARTESIAN_POINT('Ctrl Pts',(8.88652944499994,15.2,-5.36328889700001));
#179627=CARTESIAN_POINT('Ctrl Pts',(8.88652944499994,11.6,-5.36328889700001));
#179628=CARTESIAN_POINT('Ctrl Pts',(8.88738413099994,15.2,-5.36370335800001));
#179629=CARTESIAN_POINT('Ctrl Pts',(8.88738413099994,11.6,-5.36370335800001));
#179630=CARTESIAN_POINT('Ctrl Pts',(8.88824774899994,15.2,-5.36412108300001));
#179631=CARTESIAN_POINT('Ctrl Pts',(8.88824774899994,11.6,-5.36412108300001));
#179632=CARTESIAN_POINT('Ctrl Pts',(8.88912028499995,15.2,-5.36454204400002));
#179633=CARTESIAN_POINT('Ctrl Pts',(8.88912028499995,11.6,-5.36454204400002));
#179634=CARTESIAN_POINT('Ctrl Pts',(8.89000171999994,15.2,-5.36496621500001));
#179635=CARTESIAN_POINT('Ctrl Pts',(8.89000171999994,11.6,-5.36496621500001));
#179636=CARTESIAN_POINT('Ctrl Pts',(8.89089203999994,15.2,-5.36539356700001));
#179637=CARTESIAN_POINT('Ctrl Pts',(8.89089203999994,11.6,-5.36539356700001));
#179638=CARTESIAN_POINT('Ctrl Pts',(8.89179122799994,15.2,-5.36582407300001));
#179639=CARTESIAN_POINT('Ctrl Pts',(8.89179122799994,11.6,-5.36582407300001));
#179640=CARTESIAN_POINT('Ctrl Pts',(8.89269926799994,15.2,-5.36625770500001));
#179641=CARTESIAN_POINT('Ctrl Pts',(8.89269926799994,11.6,-5.36625770500001));
#179642=CARTESIAN_POINT('Ctrl Pts',(8.89361614499995,15.2,-5.36669443700001));
#179643=CARTESIAN_POINT('Ctrl Pts',(8.89361614499995,11.6,-5.36669443700001));
#179644=CARTESIAN_POINT('Ctrl Pts',(8.89454184299994,15.2,-5.36713424100002));
#179645=CARTESIAN_POINT('Ctrl Pts',(8.89454184299994,11.6,-5.36713424100002));
#179646=CARTESIAN_POINT('Ctrl Pts',(8.89547634599994,15.2,-5.36757709000002));
#179647=CARTESIAN_POINT('Ctrl Pts',(8.89547634599994,11.6,-5.36757709000002));
#179648=CARTESIAN_POINT('Ctrl Pts',(8.89641963799994,15.2,-5.36802295800001));
#179649=CARTESIAN_POINT('Ctrl Pts',(8.89641963799994,11.6,-5.36802295800001));
#179650=CARTESIAN_POINT('Ctrl Pts',(8.89737170299994,15.2,-5.36847181900002));
#179651=CARTESIAN_POINT('Ctrl Pts',(8.89737170299994,11.6,-5.36847181900002));
#179652=CARTESIAN_POINT('Ctrl Pts',(8.89833252799994,15.2,-5.36892364600002));
#179653=CARTESIAN_POINT('Ctrl Pts',(8.89833252799994,11.6,-5.36892364600002));
#179654=CARTESIAN_POINT('Ctrl Pts',(8.89930209399994,15.2,-5.36937841200002));
#179655=CARTESIAN_POINT('Ctrl Pts',(8.89930209399994,11.6,-5.36937841200002));
#179656=CARTESIAN_POINT('Ctrl Pts',(8.90028038899995,15.2,-5.36983609200002));
#179657=CARTESIAN_POINT('Ctrl Pts',(8.90028038899995,11.6,-5.36983609200002));
#179658=CARTESIAN_POINT('Ctrl Pts',(8.90126739499994,15.2,-5.37029665800001));
#179659=CARTESIAN_POINT('Ctrl Pts',(8.90126739499994,11.6,-5.37029665800001));
#179660=CARTESIAN_POINT('Ctrl Pts',(8.90226309699995,15.2,-5.37076008600001));
#179661=CARTESIAN_POINT('Ctrl Pts',(8.90226309699995,11.6,-5.37076008600001));
#179662=CARTESIAN_POINT('Ctrl Pts',(8.90326748199995,15.2,-5.37122635100001));
#179663=CARTESIAN_POINT('Ctrl Pts',(8.90326748199995,11.6,-5.37122635100001));
#179664=CARTESIAN_POINT('Ctrl Pts',(8.90428053099994,15.2,-5.37169542400001));
#179665=CARTESIAN_POINT('Ctrl Pts',(8.90428053099994,11.6,-5.37169542400001));
#179666=CARTESIAN_POINT('Ctrl Pts',(8.90530223199994,15.2,-5.37216728200002));
#179667=CARTESIAN_POINT('Ctrl Pts',(8.90530223199994,11.6,-5.37216728200002));
#179668=CARTESIAN_POINT('Ctrl Pts',(8.90633256899994,15.2,-5.37264190000001));
#179669=CARTESIAN_POINT('Ctrl Pts',(8.90633256899994,11.6,-5.37264190000001));
#179670=CARTESIAN_POINT('Ctrl Pts',(8.90737152799994,15.2,-5.37311925000001));
#179671=CARTESIAN_POINT('Ctrl Pts',(8.90737152799994,11.6,-5.37311925000001));
#179672=CARTESIAN_POINT('Ctrl Pts',(8.90841909199995,15.2,-5.37359931000001));
#179673=CARTESIAN_POINT('Ctrl Pts',(8.90841909199995,11.6,-5.37359931000001));
#179674=CARTESIAN_POINT('Ctrl Pts',(8.90947524599994,15.2,-5.37408205300002));
#179675=CARTESIAN_POINT('Ctrl Pts',(8.90947524599994,11.6,-5.37408205300002));
#179676=CARTESIAN_POINT('Ctrl Pts',(8.91053997899995,15.2,-5.37456745500001));
#179677=CARTESIAN_POINT('Ctrl Pts',(8.91053997899995,11.6,-5.37456745500001));
#179678=CARTESIAN_POINT('Ctrl Pts',(8.91161327099995,15.2,-5.37505549100001));
#179679=CARTESIAN_POINT('Ctrl Pts',(8.91161327099995,11.6,-5.37505549100001));
#179680=CARTESIAN_POINT('Ctrl Pts',(8.91269511199994,15.2,-5.37554613500001));
#179681=CARTESIAN_POINT('Ctrl Pts',(8.91269511199994,11.6,-5.37554613500001));
#179682=CARTESIAN_POINT('Ctrl Pts',(8.91378548299994,15.2,-5.37603936500001));
#179683=CARTESIAN_POINT('Ctrl Pts',(8.91378548299994,11.6,-5.37603936500001));
#179684=CARTESIAN_POINT('Ctrl Pts',(8.91488437199994,15.2,-5.37653515400002));
#179685=CARTESIAN_POINT('Ctrl Pts',(8.91488437199994,11.6,-5.37653515400002));
#179686=CARTESIAN_POINT('Ctrl Pts',(8.91599176499994,15.2,-5.37703348000001));
#179687=CARTESIAN_POINT('Ctrl Pts',(8.91599176499994,11.6,-5.37703348000001));
#179688=CARTESIAN_POINT('Ctrl Pts',(8.91710764499994,15.2,-5.37753431800001));
#179689=CARTESIAN_POINT('Ctrl Pts',(8.91710764499994,11.6,-5.37753431800001));
#179690=CARTESIAN_POINT('Ctrl Pts',(8.91823200099994,15.2,-5.37803764300001));
#179691=CARTESIAN_POINT('Ctrl Pts',(8.91823200099994,11.6,-5.37803764300001));
#179692=CARTESIAN_POINT('Ctrl Pts',(8.91936481499994,15.2,-5.37854343100001));
#179693=CARTESIAN_POINT('Ctrl Pts',(8.91936481499994,11.6,-5.37854343100001));
#179694=CARTESIAN_POINT('Ctrl Pts',(8.92050607399994,15.2,-5.37905166000002));
#179695=CARTESIAN_POINT('Ctrl Pts',(8.92050607399994,11.6,-5.37905166000002));
#179696=CARTESIAN_POINT('Ctrl Pts',(8.92165576499995,15.2,-5.37956230500001));
#179697=CARTESIAN_POINT('Ctrl Pts',(8.92165576499995,11.6,-5.37956230500001));
#179698=CARTESIAN_POINT('Ctrl Pts',(8.92281387199995,15.2,-5.38007534200001));
#179699=CARTESIAN_POINT('Ctrl Pts',(8.92281387199995,11.6,-5.38007534200001));
#179700=CARTESIAN_POINT('Ctrl Pts',(8.92398038299994,15.2,-5.38059074800001));
#179701=CARTESIAN_POINT('Ctrl Pts',(8.92398038299994,11.6,-5.38059074800001));
#179702=CARTESIAN_POINT('Ctrl Pts',(8.92515528099995,15.2,-5.38110850000002));
#179703=CARTESIAN_POINT('Ctrl Pts',(8.92515528099995,11.6,-5.38110850000002));
#179704=CARTESIAN_POINT('Ctrl Pts',(8.92633855299995,15.2,-5.38162857400001));
#179705=CARTESIAN_POINT('Ctrl Pts',(8.92633855299995,11.6,-5.38162857400001));
#179706=CARTESIAN_POINT('Ctrl Pts',(8.92753018699995,15.2,-5.38215094700002));
#179707=CARTESIAN_POINT('Ctrl Pts',(8.92753018699995,11.6,-5.38215094700002));
#179708=CARTESIAN_POINT('Ctrl Pts',(8.92873016599994,15.2,-5.38267559600001));
#179709=CARTESIAN_POINT('Ctrl Pts',(8.92873016599994,11.6,-5.38267559600001));
#179710=CARTESIAN_POINT('Ctrl Pts',(8.92993847699995,15.2,-5.38320249900002));
#179711=CARTESIAN_POINT('Ctrl Pts',(8.92993847699995,11.6,-5.38320249900002));
#179712=CARTESIAN_POINT('Ctrl Pts',(8.93115510699995,15.2,-5.38373163200002));
#179713=CARTESIAN_POINT('Ctrl Pts',(8.93115510699995,11.6,-5.38373163200002));
#179714=CARTESIAN_POINT('Ctrl Pts',(8.93238004199995,15.2,-5.38426297200001));
#179715=CARTESIAN_POINT('Ctrl Pts',(8.93238004199995,11.6,-5.38426297200001));
#179716=CARTESIAN_POINT('Ctrl Pts',(8.93361326699995,15.2,-5.38479649700002));
#179717=CARTESIAN_POINT('Ctrl Pts',(8.93361326699995,11.6,-5.38479649700002));
#179718=CARTESIAN_POINT('Ctrl Pts',(8.93485476899994,15.2,-5.38533218400001));
#179719=CARTESIAN_POINT('Ctrl Pts',(8.93485476899994,11.6,-5.38533218400001));
#179720=CARTESIAN_POINT('Ctrl Pts',(8.93610453499995,15.2,-5.38587001200002));
#179721=CARTESIAN_POINT('Ctrl Pts',(8.93610453499995,11.6,-5.38587001200002));
#179722=CARTESIAN_POINT('Ctrl Pts',(8.93736255099994,15.2,-5.38640995700002));
#179723=CARTESIAN_POINT('Ctrl Pts',(8.93736255099994,11.6,-5.38640995700002));
#179724=CARTESIAN_POINT('Ctrl Pts',(8.93862880299995,15.2,-5.38695199700001));
#179725=CARTESIAN_POINT('Ctrl Pts',(8.93862880299995,11.6,-5.38695199700001));
#179726=CARTESIAN_POINT('Ctrl Pts',(8.93990327699994,15.2,-5.38749611000001));
#179727=CARTESIAN_POINT('Ctrl Pts',(8.93990327699994,11.6,-5.38749611000001));
#179728=CARTESIAN_POINT('Ctrl Pts',(8.94118596099995,15.2,-5.38804227600002));
#179729=CARTESIAN_POINT('Ctrl Pts',(8.94118596099995,11.6,-5.38804227600002));
#179730=CARTESIAN_POINT('Ctrl Pts',(8.94247683899994,15.2,-5.38859046900001));
#179731=CARTESIAN_POINT('Ctrl Pts',(8.94247683899994,11.6,-5.38859046900001));
#179732=CARTESIAN_POINT('Ctrl Pts',(8.94377590099995,15.2,-5.38914067100002));
#179733=CARTESIAN_POINT('Ctrl Pts',(8.94377590099995,11.6,-5.38914067100002));
#179734=CARTESIAN_POINT('Ctrl Pts',(8.94508313099994,15.2,-5.38969285800002));
#179735=CARTESIAN_POINT('Ctrl Pts',(8.94508313099994,11.6,-5.38969285800002));
#179736=CARTESIAN_POINT('Ctrl Pts',(8.94639851599995,15.2,-5.39024700900002));
#179737=CARTESIAN_POINT('Ctrl Pts',(8.94639851599995,11.6,-5.39024700900002));
#179738=CARTESIAN_POINT('Ctrl Pts',(8.94772204399995,15.2,-5.39080310300001));
#179739=CARTESIAN_POINT('Ctrl Pts',(8.94772204399995,11.6,-5.39080310300001));
#179740=CARTESIAN_POINT('Ctrl Pts',(8.94905369999995,15.2,-5.39136111800001));
#179741=CARTESIAN_POINT('Ctrl Pts',(8.94905369999995,11.6,-5.39136111800001));
#179742=CARTESIAN_POINT('Ctrl Pts',(8.95039347299995,15.2,-5.39192103300001));
#179743=CARTESIAN_POINT('Ctrl Pts',(8.95039347299995,11.6,-5.39192103300001));
#179744=CARTESIAN_POINT('Ctrl Pts',(8.95174134799994,15.2,-5.39248282600001));
#179745=CARTESIAN_POINT('Ctrl Pts',(8.95174134799994,11.6,-5.39248282600001));
#179746=CARTESIAN_POINT('Ctrl Pts',(8.95309731299994,15.2,-5.39304647600002));
#179747=CARTESIAN_POINT('Ctrl Pts',(8.95309731299994,11.6,-5.39304647600002));
#179748=CARTESIAN_POINT('Ctrl Pts',(8.95446135299995,15.2,-5.39361196400002));
#179749=CARTESIAN_POINT('Ctrl Pts',(8.95446135299995,11.6,-5.39361196400002));
#179750=CARTESIAN_POINT('Ctrl Pts',(8.95583345699994,15.2,-5.39417926600001));
#179751=CARTESIAN_POINT('Ctrl Pts',(8.95583345699994,11.6,-5.39417926600001));
#179752=CARTESIAN_POINT('Ctrl Pts',(8.95721361099995,15.2,-5.39474836400001));
#179753=CARTESIAN_POINT('Ctrl Pts',(8.95721361099995,11.6,-5.39474836400001));
#179754=CARTESIAN_POINT('Ctrl Pts',(8.95860180399995,15.2,-5.39531923500002));
#179755=CARTESIAN_POINT('Ctrl Pts',(8.95860180399995,11.6,-5.39531923500002));
#179756=CARTESIAN_POINT('Ctrl Pts',(8.95999802099994,15.2,-5.39589185900001));
#179757=CARTESIAN_POINT('Ctrl Pts',(8.95999802099994,11.6,-5.39589185900001));
#179758=CARTESIAN_POINT('Ctrl Pts',(8.96140224899994,15.2,-5.39646621400002));
#179759=CARTESIAN_POINT('Ctrl Pts',(8.96140224899994,11.6,-5.39646621400002));
#179760=CARTESIAN_POINT('Ctrl Pts',(8.96281447699995,15.2,-5.39704228300002));
#179761=CARTESIAN_POINT('Ctrl Pts',(8.96281447699995,11.6,-5.39704228300002));
#179762=CARTESIAN_POINT('Ctrl Pts',(8.96423468899994,15.2,-5.39762004300002));
#179763=CARTESIAN_POINT('Ctrl Pts',(8.96423468899994,11.6,-5.39762004300002));
#179764=CARTESIAN_POINT('Ctrl Pts',(8.96566287699994,15.2,-5.39819947400002));
#179765=CARTESIAN_POINT('Ctrl Pts',(8.96566287699994,11.6,-5.39819947400002));
#179766=CARTESIAN_POINT('Ctrl Pts',(8.96709902399994,15.2,-5.39878055600001));
#179767=CARTESIAN_POINT('Ctrl Pts',(8.96709902399994,11.6,-5.39878055600001));
#179768=CARTESIAN_POINT('Ctrl Pts',(8.96854311899994,15.2,-5.39936326900001));
#179769=CARTESIAN_POINT('Ctrl Pts',(8.96854311899994,11.6,-5.39936326900001));
#179770=CARTESIAN_POINT('Ctrl Pts',(8.96999514999994,15.2,-5.39994759300002));
#179771=CARTESIAN_POINT('Ctrl Pts',(8.96999514999994,11.6,-5.39994759300002));
#179772=CARTESIAN_POINT('Ctrl Pts',(8.97145510299995,15.2,-5.40053350700001));
#179773=CARTESIAN_POINT('Ctrl Pts',(8.97145510299995,11.6,-5.40053350700001));
#179774=CARTESIAN_POINT('Ctrl Pts',(8.97292296699994,15.2,-5.40112099200002));
#179775=CARTESIAN_POINT('Ctrl Pts',(8.97292296699994,11.6,-5.40112099200002));
#179776=CARTESIAN_POINT('Ctrl Pts',(8.97439872899995,15.2,-5.40171002900002));
#179777=CARTESIAN_POINT('Ctrl Pts',(8.97439872899995,11.6,-5.40171002900002));
#179778=CARTESIAN_POINT('Ctrl Pts',(8.97588237599994,15.2,-5.40230059700002));
#179779=CARTESIAN_POINT('Ctrl Pts',(8.97588237599994,11.6,-5.40230059700002));
#179780=CARTESIAN_POINT('Ctrl Pts',(8.97737389499994,15.2,-5.40289267700001));
#179781=CARTESIAN_POINT('Ctrl Pts',(8.97737389499994,11.6,-5.40289267700001));
#179782=CARTESIAN_POINT('Ctrl Pts',(8.97887327499994,15.2,-5.40348624900002));
#179783=CARTESIAN_POINT('Ctrl Pts',(8.97887327499994,11.6,-5.40348624900002));
#179784=CARTESIAN_POINT('Ctrl Pts',(8.98038050299995,15.2,-5.40408129400001));
#179785=CARTESIAN_POINT('Ctrl Pts',(8.98038050299995,11.6,-5.40408129400001));
#179786=CARTESIAN_POINT('Ctrl Pts',(8.98189556799995,15.2,-5.40467779100001));
#179787=CARTESIAN_POINT('Ctrl Pts',(8.98189556799995,11.6,-5.40467779100001));
#179788=CARTESIAN_POINT('Ctrl Pts',(8.98341845499995,15.2,-5.40527572300002));
#179789=CARTESIAN_POINT('Ctrl Pts',(8.98341845499995,11.6,-5.40527572300002));
#179790=CARTESIAN_POINT('Ctrl Pts',(8.98494915299995,15.2,-5.40587507000001));
#179791=CARTESIAN_POINT('Ctrl Pts',(8.98494915299995,11.6,-5.40587507000001));
#179792=CARTESIAN_POINT('Ctrl Pts',(8.98648765099994,15.2,-5.40647581200002));
#179793=CARTESIAN_POINT('Ctrl Pts',(8.98648765099994,11.6,-5.40647581200002));
#179794=CARTESIAN_POINT('Ctrl Pts',(8.98803393599995,15.2,-5.40707793100001));
#179795=CARTESIAN_POINT('Ctrl Pts',(8.98803393599995,11.6,-5.40707793100001));
#179796=CARTESIAN_POINT('Ctrl Pts',(8.98958799499994,15.2,-5.40768140800001));
#179797=CARTESIAN_POINT('Ctrl Pts',(8.98958799499994,11.6,-5.40768140800001));
#179798=CARTESIAN_POINT('Ctrl Pts',(8.99114981699995,15.2,-5.40828622400001));
#179799=CARTESIAN_POINT('Ctrl Pts',(8.99114981699995,11.6,-5.40828622400001));
#179800=CARTESIAN_POINT('Ctrl Pts',(8.99271938899994,15.2,-5.40889235900002));
#179801=CARTESIAN_POINT('Ctrl Pts',(8.99271938899994,11.6,-5.40889235900002));
#179802=CARTESIAN_POINT('Ctrl Pts',(8.99429670099994,15.2,-5.40949979500001));
#179803=CARTESIAN_POINT('Ctrl Pts',(8.99429670099994,11.6,-5.40949979500001));
#179804=CARTESIAN_POINT('Ctrl Pts',(8.99588173899994,15.2,-5.41010851400001));
#179805=CARTESIAN_POINT('Ctrl Pts',(8.99588173899994,11.6,-5.41010851400001));
#179806=CARTESIAN_POINT('Ctrl Pts',(8.99747449099995,15.2,-5.41071849700002));
#179807=CARTESIAN_POINT('Ctrl Pts',(8.99747449099995,11.6,-5.41071849700002));
#179808=CARTESIAN_POINT('Ctrl Pts',(8.99907494499995,15.2,-5.41132972500002));
#179809=CARTESIAN_POINT('Ctrl Pts',(8.99907494499995,11.6,-5.41132972500002));
#179810=CARTESIAN_POINT('Ctrl Pts',(9.00068308999994,15.2,-5.41194218000001));
#179811=CARTESIAN_POINT('Ctrl Pts',(9.00068308999994,11.6,-5.41194218000001));
#179812=CARTESIAN_POINT('Ctrl Pts',(9.00229891499994,15.2,-5.41255584400002));
#179813=CARTESIAN_POINT('Ctrl Pts',(9.00229891499994,11.6,-5.41255584400002));
#179814=CARTESIAN_POINT('Ctrl Pts',(9.00392240699994,15.2,-5.41317069800002));
#179815=CARTESIAN_POINT('Ctrl Pts',(9.00392240699994,11.6,-5.41317069800002));
#179816=CARTESIAN_POINT('Ctrl Pts',(9.00555355399994,15.2,-5.41378672400001));
#179817=CARTESIAN_POINT('Ctrl Pts',(9.00555355399994,11.6,-5.41378672400001));
#179818=CARTESIAN_POINT('Ctrl Pts',(9.00719234299994,15.2,-5.41440390400002));
#179819=CARTESIAN_POINT('Ctrl Pts',(9.00719234299994,11.6,-5.41440390400002));
#179820=CARTESIAN_POINT('Ctrl Pts',(9.00883876599995,15.2,-5.41502222000001));
#179821=CARTESIAN_POINT('Ctrl Pts',(9.00883876599995,11.6,-5.41502222000001));
#179822=CARTESIAN_POINT('Ctrl Pts',(9.01049280799995,15.2,-5.41564165400001));
#179823=CARTESIAN_POINT('Ctrl Pts',(9.01049280799995,11.6,-5.41564165400001));
#179824=CARTESIAN_POINT('Ctrl Pts',(9.01215445899994,15.2,-5.41626218700001));
#179825=CARTESIAN_POINT('Ctrl Pts',(9.01215445899994,11.6,-5.41626218700001));
#179826=CARTESIAN_POINT('Ctrl Pts',(9.01382370599995,15.2,-5.41688380300001));
#179827=CARTESIAN_POINT('Ctrl Pts',(9.01382370599995,11.6,-5.41688380300001));
#179828=CARTESIAN_POINT('Ctrl Pts',(9.01550053899994,15.2,-5.41750648300001));
#179829=CARTESIAN_POINT('Ctrl Pts',(9.01550053899994,11.6,-5.41750648300001));
#179830=CARTESIAN_POINT('Ctrl Pts',(9.01718494499994,15.2,-5.41813021000001));
#179831=CARTESIAN_POINT('Ctrl Pts',(9.01718494499994,11.6,-5.41813021000001));
#179832=CARTESIAN_POINT('Ctrl Pts',(9.01887691299994,15.2,-5.41875496600001));
#179833=CARTESIAN_POINT('Ctrl Pts',(9.01887691299994,11.6,-5.41875496600001));
#179834=CARTESIAN_POINT('Ctrl Pts',(9.02057643199995,15.2,-5.41938073300001));
#179835=CARTESIAN_POINT('Ctrl Pts',(9.02057643199995,11.6,-5.41938073300001));
#179836=CARTESIAN_POINT('Ctrl Pts',(9.02228348999994,15.2,-5.42000749500001));
#179837=CARTESIAN_POINT('Ctrl Pts',(9.02228348999994,11.6,-5.42000749500001));
#179838=CARTESIAN_POINT('Ctrl Pts',(9.02399807499994,15.2,-5.42063523200001));
#179839=CARTESIAN_POINT('Ctrl Pts',(9.02399807499994,11.6,-5.42063523200001));
#179840=CARTESIAN_POINT('Ctrl Pts',(9.02572017699995,15.2,-5.42126392800002));
#179841=CARTESIAN_POINT('Ctrl Pts',(9.02572017699995,11.6,-5.42126392800002));
#179842=CARTESIAN_POINT('Ctrl Pts',(9.02744978399994,15.2,-5.42189356800002));
#179843=CARTESIAN_POINT('Ctrl Pts',(9.02744978399994,11.6,-5.42189356800002));
#179844=CARTESIAN_POINT('Ctrl Pts',(9.02918688399994,15.2,-5.42252413100002));
#179845=CARTESIAN_POINT('Ctrl Pts',(9.02918688399994,11.6,-5.42252413100002));
#179846=CARTESIAN_POINT('Ctrl Pts',(9.03093146599995,15.2,-5.42315560300001));
#179847=CARTESIAN_POINT('Ctrl Pts',(9.03093146599995,11.6,-5.42315560300001));
#179848=CARTESIAN_POINT('Ctrl Pts',(9.03268351899994,15.2,-5.42378796400001));
#179849=CARTESIAN_POINT('Ctrl Pts',(9.03268351899994,11.6,-5.42378796400001));
#179850=CARTESIAN_POINT('Ctrl Pts',(9.03444303299995,15.2,-5.42442119900001));
#179851=CARTESIAN_POINT('Ctrl Pts',(9.03444303299995,11.6,-5.42442119900001));
#179852=CARTESIAN_POINT('Ctrl Pts',(9.03620999399994,15.2,-5.42505529000001));
#179853=CARTESIAN_POINT('Ctrl Pts',(9.03620999399994,11.6,-5.42505529000001));
#179854=CARTESIAN_POINT('Ctrl Pts',(9.03798439199995,15.2,-5.42569022100002));
#179855=CARTESIAN_POINT('Ctrl Pts',(9.03798439199995,11.6,-5.42569022100002));
#179856=CARTESIAN_POINT('Ctrl Pts',(9.03976621699995,15.2,-5.42632597500001));
#179857=CARTESIAN_POINT('Ctrl Pts',(9.03976621699995,11.6,-5.42632597500001));
#179858=CARTESIAN_POINT('Ctrl Pts',(9.04155545599994,15.2,-5.42696253500001));
#179859=CARTESIAN_POINT('Ctrl Pts',(9.04155545599994,11.6,-5.42696253500001));
#179860=CARTESIAN_POINT('Ctrl Pts',(9.04335209899994,15.2,-5.42759988400002));
#179861=CARTESIAN_POINT('Ctrl Pts',(9.04335209899994,11.6,-5.42759988400002));
#179862=CARTESIAN_POINT('Ctrl Pts',(9.04515613499994,15.2,-5.42823800600001));
#179863=CARTESIAN_POINT('Ctrl Pts',(9.04515613499994,11.6,-5.42823800600001));
#179864=CARTESIAN_POINT('Ctrl Pts',(9.04696755199994,15.2,-5.42887688500001));
#179865=CARTESIAN_POINT('Ctrl Pts',(9.04696755199994,11.6,-5.42887688500001));
#179866=CARTESIAN_POINT('Ctrl Pts',(9.04878633899994,15.2,-5.42951650200001));
#179867=CARTESIAN_POINT('Ctrl Pts',(9.04878633899994,11.6,-5.42951650200001));
#179868=CARTESIAN_POINT('Ctrl Pts',(9.05061248799995,15.2,-5.43015684400002));
#179869=CARTESIAN_POINT('Ctrl Pts',(9.05061248799995,11.6,-5.43015684400002));
#179870=CARTESIAN_POINT('Ctrl Pts',(9.05244598299995,15.2,-5.43079789200001));
#179871=CARTESIAN_POINT('Ctrl Pts',(9.05244598299995,11.6,-5.43079789200001));
#179872=CARTESIAN_POINT('Ctrl Pts',(9.05428681799994,15.2,-5.43143963100002));
#179873=CARTESIAN_POINT('Ctrl Pts',(9.05428681799994,11.6,-5.43143963100002));
#179874=CARTESIAN_POINT('Ctrl Pts',(9.05613497799994,15.2,-5.43208204400001));
#179875=CARTESIAN_POINT('Ctrl Pts',(9.05613497799994,11.6,-5.43208204400001));
#179876=CARTESIAN_POINT('Ctrl Pts',(9.05799045399995,15.2,-5.43272511600001));
#179877=CARTESIAN_POINT('Ctrl Pts',(9.05799045399995,11.6,-5.43272511600001));
#179878=CARTESIAN_POINT('Ctrl Pts',(9.05985323499995,15.2,-5.43336883000002));
#179879=CARTESIAN_POINT('Ctrl Pts',(9.05985323499995,11.6,-5.43336883000002));
#179880=CARTESIAN_POINT('Ctrl Pts',(9.06172330999994,15.2,-5.43401316900002));
#179881=CARTESIAN_POINT('Ctrl Pts',(9.06172330999994,11.6,-5.43401316900002));
#179882=CARTESIAN_POINT('Ctrl Pts',(9.06360066799994,15.2,-5.43465811900001));
#179883=CARTESIAN_POINT('Ctrl Pts',(9.06360066799994,11.6,-5.43465811900001));
#179884=CARTESIAN_POINT('Ctrl Pts',(9.06548529999995,15.2,-5.43530366300002));
#179885=CARTESIAN_POINT('Ctrl Pts',(9.06548529999995,11.6,-5.43530366300002));
#179886=CARTESIAN_POINT('Ctrl Pts',(9.06737719299995,15.2,-5.43594978600002));
#179887=CARTESIAN_POINT('Ctrl Pts',(9.06737719299995,11.6,-5.43594978600002));
#179888=CARTESIAN_POINT('Ctrl Pts',(9.06927633599994,15.2,-5.43659647000001));
#179889=CARTESIAN_POINT('Ctrl Pts',(9.06927633599994,11.6,-5.43659647000001));
#179890=CARTESIAN_POINT('Ctrl Pts',(9.07118271999994,15.2,-5.43724370100001));
#179891=CARTESIAN_POINT('Ctrl Pts',(9.07118271999994,11.6,-5.43724370100001));
#179892=CARTESIAN_POINT('Ctrl Pts',(9.07309633399995,15.2,-5.43789146400002));
#179893=CARTESIAN_POINT('Ctrl Pts',(9.07309633399995,11.6,-5.43789146400002));
#179894=CARTESIAN_POINT('Ctrl Pts',(9.07501716599995,15.2,-5.43853974100001));
#179895=CARTESIAN_POINT('Ctrl Pts',(9.07501716599995,11.6,-5.43853974100001));
#179896=CARTESIAN_POINT('Ctrl Pts',(9.07694520799994,15.2,-5.43918851900001));
#179897=CARTESIAN_POINT('Ctrl Pts',(9.07694520799994,11.6,-5.43918851900001));
#179898=CARTESIAN_POINT('Ctrl Pts',(9.07888044599994,15.2,-5.43983778100001));
#179899=CARTESIAN_POINT('Ctrl Pts',(9.07888044599994,11.6,-5.43983778100001));
#179900=CARTESIAN_POINT('Ctrl Pts',(9.08082287199995,15.2,-5.44048751200001));
#179901=CARTESIAN_POINT('Ctrl Pts',(9.08082287199995,11.6,-5.44048751200001));
#179902=CARTESIAN_POINT('Ctrl Pts',(9.08277247299995,15.2,-5.44113769600001));
#179903=CARTESIAN_POINT('Ctrl Pts',(9.08277247299995,11.6,-5.44113769600001));
#179904=CARTESIAN_POINT('Ctrl Pts',(9.08472924199994,15.2,-5.44178831900001));
#179905=CARTESIAN_POINT('Ctrl Pts',(9.08472924199994,11.6,-5.44178831900001));
#179906=CARTESIAN_POINT('Ctrl Pts',(9.08669316599994,15.2,-5.44243936400001));
#179907=CARTESIAN_POINT('Ctrl Pts',(9.08669316599994,11.6,-5.44243936400001));
#179908=CARTESIAN_POINT('Ctrl Pts',(9.08866423499994,15.2,-5.44309081600002));
#179909=CARTESIAN_POINT('Ctrl Pts',(9.08866423499994,11.6,-5.44309081600002));
#179910=CARTESIAN_POINT('Ctrl Pts',(9.09064243799994,15.2,-5.44374266200002));
#179911=CARTESIAN_POINT('Ctrl Pts',(9.09064243799994,11.6,-5.44374266200002));
#179912=CARTESIAN_POINT('Ctrl Pts',(9.09262776499994,15.2,-5.44439488400001));
#179913=CARTESIAN_POINT('Ctrl Pts',(9.09262776499994,11.6,-5.44439488400001));
#179914=CARTESIAN_POINT('Ctrl Pts',(9.09462020699995,15.2,-5.44504747000001));
#179915=CARTESIAN_POINT('Ctrl Pts',(9.09462020699995,11.6,-5.44504747000001));
#179916=CARTESIAN_POINT('Ctrl Pts',(9.09661975099995,15.2,-5.44570040100002));
#179917=CARTESIAN_POINT('Ctrl Pts',(9.09661975099995,11.6,-5.44570040100002));
#179918=CARTESIAN_POINT('Ctrl Pts',(9.09862638799994,15.2,-5.44635366600001));
#179919=CARTESIAN_POINT('Ctrl Pts',(9.09862638799994,11.6,-5.44635366600001));
#179920=CARTESIAN_POINT('Ctrl Pts',(9.10064010799994,15.2,-5.44700724700002));
#179921=CARTESIAN_POINT('Ctrl Pts',(9.10064010799994,11.6,-5.44700724700002));
#179922=CARTESIAN_POINT('Ctrl Pts',(9.10266090099995,15.2,-5.44766113100001));
#179923=CARTESIAN_POINT('Ctrl Pts',(9.10266090099995,11.6,-5.44766113100001));
#179924=CARTESIAN_POINT('Ctrl Pts',(9.10468875499994,15.2,-5.44831530400002));
#179925=CARTESIAN_POINT('Ctrl Pts',(9.10468875499994,11.6,-5.44831530400002));
#179926=CARTESIAN_POINT('Ctrl Pts',(9.10672366199995,15.2,-5.44896974900002));
#179927=CARTESIAN_POINT('Ctrl Pts',(9.10672366199995,11.6,-5.44896974900002));
#179928=CARTESIAN_POINT('Ctrl Pts',(9.10876560899995,15.2,-5.44962445200001));
#179929=CARTESIAN_POINT('Ctrl Pts',(9.10876560899995,11.6,-5.44962445200001));
#179930=CARTESIAN_POINT('Ctrl Pts',(9.11081458899995,15.2,-5.45027940000002));
#179931=CARTESIAN_POINT('Ctrl Pts',(9.11081458899995,11.6,-5.45027940000002));
#179932=CARTESIAN_POINT('Ctrl Pts',(9.11287058799994,15.2,-5.45093457500001));
#179933=CARTESIAN_POINT('Ctrl Pts',(9.11287058799994,11.6,-5.45093457500001));
#179934=CARTESIAN_POINT('Ctrl Pts',(9.11493359899995,15.2,-5.45158996700001));
#179935=CARTESIAN_POINT('Ctrl Pts',(9.11493359899995,11.6,-5.45158996700001));
#179936=CARTESIAN_POINT('Ctrl Pts',(9.11700361099994,15.2,-5.45224555800001));
#179937=CARTESIAN_POINT('Ctrl Pts',(9.11700361099994,11.6,-5.45224555800001));
#179938=CARTESIAN_POINT('Ctrl Pts',(9.11908061299994,15.2,-5.45290133500002));
#179939=CARTESIAN_POINT('Ctrl Pts',(9.11908061299994,11.6,-5.45290133500002));
#179940=CARTESIAN_POINT('Ctrl Pts',(9.12116459599994,15.2,-5.45355728300001));
#179941=CARTESIAN_POINT('Ctrl Pts',(9.12116459599994,11.6,-5.45355728300001));
#179942=CARTESIAN_POINT('Ctrl Pts',(9.12325554899994,15.2,-5.45421338800002));
#179943=CARTESIAN_POINT('Ctrl Pts',(9.12325554899994,11.6,-5.45421338800002));
#179944=CARTESIAN_POINT('Ctrl Pts',(9.12535346199994,15.2,-5.45486963700001));
#179945=CARTESIAN_POINT('Ctrl Pts',(9.12535346199994,11.6,-5.45486963700001));
#179946=CARTESIAN_POINT('Ctrl Pts',(9.12745832599994,15.2,-5.45552601400002));
#179947=CARTESIAN_POINT('Ctrl Pts',(9.12745832599994,11.6,-5.45552601400002));
#179948=CARTESIAN_POINT('Ctrl Pts',(9.12957012999994,15.2,-5.45618250500001));
#179949=CARTESIAN_POINT('Ctrl Pts',(9.12957012999994,11.6,-5.45618250500001));
#179950=CARTESIAN_POINT('Ctrl Pts',(9.13168886399994,15.2,-5.45683909600001));
#179951=CARTESIAN_POINT('Ctrl Pts',(9.13168886399994,11.6,-5.45683909600001));
#179952=CARTESIAN_POINT('Ctrl Pts',(9.13381451899994,15.2,-5.45749577400001));
#179953=CARTESIAN_POINT('Ctrl Pts',(9.13381451899994,11.6,-5.45749577400001));
#179954=CARTESIAN_POINT('Ctrl Pts',(9.13594708299994,15.2,-5.45815252500002));
#179955=CARTESIAN_POINT('Ctrl Pts',(9.13594708299994,11.6,-5.45815252500002));
#179956=CARTESIAN_POINT('Ctrl Pts',(9.13808654799994,15.2,-5.45880933300001));
#179957=CARTESIAN_POINT('Ctrl Pts',(9.13808654799994,11.6,-5.45880933300001));
#179958=CARTESIAN_POINT('Ctrl Pts',(9.14023290399994,15.2,-5.45946618500002));
#179959=CARTESIAN_POINT('Ctrl Pts',(9.14023290399994,11.6,-5.45946618500002));
#179960=CARTESIAN_POINT('Ctrl Pts',(9.14238613999995,15.2,-5.46012306900002));
#179961=CARTESIAN_POINT('Ctrl Pts',(9.14238613999995,11.6,-5.46012306900002));
#179962=CARTESIAN_POINT('Ctrl Pts',(9.14454624699994,15.2,-5.46077996900001));
#179963=CARTESIAN_POINT('Ctrl Pts',(9.14454624699994,11.6,-5.46077996900001));
#179964=CARTESIAN_POINT('Ctrl Pts',(9.14671321399994,15.2,-5.46143687300002));
#179965=CARTESIAN_POINT('Ctrl Pts',(9.14671321399994,11.6,-5.46143687300002));
#179966=CARTESIAN_POINT('Ctrl Pts',(9.14888703299994,15.2,-5.46209376400002));
#179967=CARTESIAN_POINT('Ctrl Pts',(9.14888703299994,11.6,-5.46209376400002));
#179968=CARTESIAN_POINT('Ctrl Pts',(9.15106769299994,15.2,-5.46275063300001));
#179969=CARTESIAN_POINT('Ctrl Pts',(9.15106769299994,11.6,-5.46275063300001));
#179970=CARTESIAN_POINT('Ctrl Pts',(9.15325518399994,15.2,-5.46340746200002));
#179971=CARTESIAN_POINT('Ctrl Pts',(9.15325518399994,11.6,-5.46340746200002));
#179972=CARTESIAN_POINT('Ctrl Pts',(9.15544949599994,15.2,-5.46406424100002));
#179973=CARTESIAN_POINT('Ctrl Pts',(9.15544949599994,11.6,-5.46406424100002));
#179974=CARTESIAN_POINT('Ctrl Pts',(9.15765062099995,15.2,-5.46472095300001));
#179975=CARTESIAN_POINT('Ctrl Pts',(9.15765062099995,11.6,-5.46472095300001));
#179976=CARTESIAN_POINT('Ctrl Pts',(9.15985854799995,15.2,-5.46537758800001));
#179977=CARTESIAN_POINT('Ctrl Pts',(9.15985854799995,11.6,-5.46537758800001));
#179978=CARTESIAN_POINT('Ctrl Pts',(9.16207326699995,15.2,-5.46603413000001));
#179979=CARTESIAN_POINT('Ctrl Pts',(9.16207326699995,11.6,-5.46603413000001));
#179980=CARTESIAN_POINT('Ctrl Pts',(9.16429476899994,15.2,-5.46669056600001));
#179981=CARTESIAN_POINT('Ctrl Pts',(9.16429476899994,11.6,-5.46669056600001));
#179982=CARTESIAN_POINT('Ctrl Pts',(9.16652304299994,15.2,-5.46734688400001));
#179983=CARTESIAN_POINT('Ctrl Pts',(9.16652304299994,11.6,-5.46734688400001));
#179984=CARTESIAN_POINT('Ctrl Pts',(9.16875808299995,15.2,-5.46800307100002));
#179985=CARTESIAN_POINT('Ctrl Pts',(9.16875808299995,11.6,-5.46800307100002));
#179986=CARTESIAN_POINT('Ctrl Pts',(9.17099987399994,15.2,-5.46865911100001));
#179987=CARTESIAN_POINT('Ctrl Pts',(9.17099987399994,11.6,-5.46865911100001));
#179988=CARTESIAN_POINT('Ctrl Pts',(9.17324840999994,15.2,-5.46931499300001));
#179989=CARTESIAN_POINT('Ctrl Pts',(9.17324840999994,11.6,-5.46931499300001));
#179990=CARTESIAN_POINT('Ctrl Pts',(9.17550368099995,15.2,-5.46997070300002));
#179991=CARTESIAN_POINT('Ctrl Pts',(9.17550368099995,11.6,-5.46997070300002));
#179992=CARTESIAN_POINT('Ctrl Pts',(9.17776567599994,15.2,-5.47062622900001));
#179993=CARTESIAN_POINT('Ctrl Pts',(9.17776567599994,11.6,-5.47062622900001));
#179994=CARTESIAN_POINT('Ctrl Pts',(9.18003438699994,15.2,-5.47128155600001));
#179995=CARTESIAN_POINT('Ctrl Pts',(9.18003438699994,11.6,-5.47128155600001));
#179996=CARTESIAN_POINT('Ctrl Pts',(9.18230980399994,15.2,-5.47193667300002));
#179997=CARTESIAN_POINT('Ctrl Pts',(9.18230980399994,11.6,-5.47193667300002));
#179998=CARTESIAN_POINT('Ctrl Pts',(9.18459191699995,15.2,-5.47259156500001));
#179999=CARTESIAN_POINT('Ctrl Pts',(9.18459191699995,11.6,-5.47259156500001));
#180000=CARTESIAN_POINT('Ctrl Pts',(9.18688071799994,15.2,-5.47324622200001));
#180001=CARTESIAN_POINT('Ctrl Pts',(9.18688071799994,11.6,-5.47324622200001));
#180002=CARTESIAN_POINT('Ctrl Pts',(9.18917619399994,15.2,-5.47390062900002));
#180003=CARTESIAN_POINT('Ctrl Pts',(9.18917619399994,11.6,-5.47390062900002));
#180004=CARTESIAN_POINT('Ctrl Pts',(9.19147833999994,15.2,-5.47455477200002));
#180005=CARTESIAN_POINT('Ctrl Pts',(9.19147833999994,11.6,-5.47455477200002));
#180006=CARTESIAN_POINT('Ctrl Pts',(9.19378714199994,15.2,-5.47520864000001));
#180007=CARTESIAN_POINT('Ctrl Pts',(9.19378714199994,11.6,-5.47520864000001));
#180008=CARTESIAN_POINT('Ctrl Pts',(9.19610259599994,15.2,-5.47586222000001));
#180009=CARTESIAN_POINT('Ctrl Pts',(9.19610259599994,11.6,-5.47586222000001));
#180010=CARTESIAN_POINT('Ctrl Pts',(9.19842468799994,15.2,-5.47651550000001));
#180011=CARTESIAN_POINT('Ctrl Pts',(9.19842468799994,11.6,-5.47651550000001));
#180012=CARTESIAN_POINT('Ctrl Pts',(9.20075340999994,15.2,-5.47716846600002));
#180013=CARTESIAN_POINT('Ctrl Pts',(9.20075340999994,11.6,-5.47716846600002));
#180014=CARTESIAN_POINT('Ctrl Pts',(9.20308875299994,15.2,-5.47782110600001));
#180015=CARTESIAN_POINT('Ctrl Pts',(9.20308875299994,11.6,-5.47782110600001));
#180016=CARTESIAN_POINT('Ctrl Pts',(9.20543070799994,15.2,-5.47847340700002));
#180017=CARTESIAN_POINT('Ctrl Pts',(9.20543070799994,11.6,-5.47847340700002));
#180018=CARTESIAN_POINT('Ctrl Pts',(9.20777926399994,15.2,-5.47912535600001));
#180019=CARTESIAN_POINT('Ctrl Pts',(9.20777926399994,11.6,-5.47912535600001));
#180020=CARTESIAN_POINT('Ctrl Pts',(9.21013441399994,15.2,-5.47977694200001));
#180021=CARTESIAN_POINT('Ctrl Pts',(9.21013441399994,11.6,-5.47977694200001));
#180022=CARTESIAN_POINT('Ctrl Pts',(9.21249614799994,15.2,-5.48042815200001));
#180023=CARTESIAN_POINT('Ctrl Pts',(9.21249614799994,11.6,-5.48042815200001));
#180024=CARTESIAN_POINT('Ctrl Pts',(9.21486445499994,15.2,-5.48107897300001));
#180025=CARTESIAN_POINT('Ctrl Pts',(9.21486445499994,11.6,-5.48107897300001));
#180026=CARTESIAN_POINT('Ctrl Pts',(9.21723932699994,15.2,-5.48172939300001));
#180027=CARTESIAN_POINT('Ctrl Pts',(9.21723932699994,11.6,-5.48172939300001));
#180028=CARTESIAN_POINT('Ctrl Pts',(9.21962075499994,15.2,-5.48237939900002));
#180029=CARTESIAN_POINT('Ctrl Pts',(9.21962075499994,11.6,-5.48237939900002));
#180030=CARTESIAN_POINT('Ctrl Pts',(9.22200872899994,15.2,-5.48302898000002));
#180031=CARTESIAN_POINT('Ctrl Pts',(9.22200872899994,11.6,-5.48302898000002));
#180032=CARTESIAN_POINT('Ctrl Pts',(9.22440324099994,15.2,-5.48367812300001));
#180033=CARTESIAN_POINT('Ctrl Pts',(9.22440324099994,11.6,-5.48367812300001));
#180034=CARTESIAN_POINT('Ctrl Pts',(9.22680427999994,15.2,-5.48432681500001));
#180035=CARTESIAN_POINT('Ctrl Pts',(9.22680427999994,11.6,-5.48432681500001));
#180036=CARTESIAN_POINT('Ctrl Pts',(9.22921183799994,15.2,-5.48497504600002));
#180037=CARTESIAN_POINT('Ctrl Pts',(9.22921183799994,11.6,-5.48497504600002));
#180038=CARTESIAN_POINT('Ctrl Pts',(9.23162590699994,15.2,-5.48562280100001));
#180039=CARTESIAN_POINT('Ctrl Pts',(9.23162590699994,11.6,-5.48562280100001));
#180040=CARTESIAN_POINT('Ctrl Pts',(9.23404647499994,15.2,-5.48627007100002));
#180041=CARTESIAN_POINT('Ctrl Pts',(9.23404647499994,11.6,-5.48627007100002));
#180042=CARTESIAN_POINT('Ctrl Pts',(9.23647353599995,15.2,-5.48691684200001));
#180043=CARTESIAN_POINT('Ctrl Pts',(9.23647353599995,11.6,-5.48691684200001));
#180044=CARTESIAN_POINT('Ctrl Pts',(9.23890707799995,15.2,-5.48756310100002));
#180045=CARTESIAN_POINT('Ctrl Pts',(9.23890707799995,11.6,-5.48756310100002));
#180046=CARTESIAN_POINT('Ctrl Pts',(9.24134709299994,15.2,-5.48820883900001));
#180047=CARTESIAN_POINT('Ctrl Pts',(9.24134709299994,11.6,-5.48820883900001));
#180048=CARTESIAN_POINT('Ctrl Pts',(9.24379357299994,15.2,-5.48885404200002));
#180049=CARTESIAN_POINT('Ctrl Pts',(9.24379357299994,11.6,-5.48885404200002));
#180050=CARTESIAN_POINT('Ctrl Pts',(9.24624650799995,15.2,-5.48949869700001));
#180051=CARTESIAN_POINT('Ctrl Pts',(9.24624650799995,11.6,-5.48949869700001));
#180052=CARTESIAN_POINT('Ctrl Pts',(9.24870588899994,15.2,-5.49014279500001));
#180053=CARTESIAN_POINT('Ctrl Pts',(9.24870588899994,11.6,-5.49014279500001));
#180054=CARTESIAN_POINT('Ctrl Pts',(9.25117170699994,15.2,-5.49078632400001));
#180055=CARTESIAN_POINT('Ctrl Pts',(9.25117170699994,11.6,-5.49078632400001));
#180056=CARTESIAN_POINT('Ctrl Pts',(9.25364395199994,15.2,-5.49142926900001));
#180057=CARTESIAN_POINT('Ctrl Pts',(9.25364395199994,11.6,-5.49142926900001));
#180058=CARTESIAN_POINT('Ctrl Pts',(9.25612261599994,15.2,-5.49207162100001));
#180059=CARTESIAN_POINT('Ctrl Pts',(9.25612261599994,11.6,-5.49207162100001));
#180060=CARTESIAN_POINT('Ctrl Pts',(9.25860768999994,15.2,-5.49271336700001));
#180061=CARTESIAN_POINT('Ctrl Pts',(9.25860768999994,11.6,-5.49271336700001));
#180062=CARTESIAN_POINT('Ctrl Pts',(9.26109916599994,15.2,-5.49335449700001));
#180063=CARTESIAN_POINT('Ctrl Pts',(9.26109916599994,11.6,-5.49335449700001));
#180064=CARTESIAN_POINT('Ctrl Pts',(9.26359703299994,15.2,-5.49399499800002));
#180065=CARTESIAN_POINT('Ctrl Pts',(9.26359703299994,11.6,-5.49399499800002));
#180066=CARTESIAN_POINT('Ctrl Pts',(9.26610128399994,15.2,-5.49463485800001));
#180067=CARTESIAN_POINT('Ctrl Pts',(9.26610128399994,11.6,-5.49463485800001));
#180068=CARTESIAN_POINT('Ctrl Pts',(9.26861190799994,15.2,-5.49527406700001));
#180069=CARTESIAN_POINT('Ctrl Pts',(9.26861190799994,11.6,-5.49527406700001));
#180070=CARTESIAN_POINT('Ctrl Pts',(9.27112889699995,15.2,-5.49591261200002));
#180071=CARTESIAN_POINT('Ctrl Pts',(9.27112889699995,11.6,-5.49591261200002));
#180072=CARTESIAN_POINT('Ctrl Pts',(9.27365224399994,15.2,-5.49655048200002));
#180073=CARTESIAN_POINT('Ctrl Pts',(9.27365224399994,11.6,-5.49655048200002));
#180074=CARTESIAN_POINT('Ctrl Pts',(9.27618193699994,15.2,-5.49718766700002));
#180075=CARTESIAN_POINT('Ctrl Pts',(9.27618193699994,11.6,-5.49718766700002));
#180076=CARTESIAN_POINT('Ctrl Pts',(9.27871796999994,15.2,-5.49782415300001));
#180077=CARTESIAN_POINT('Ctrl Pts',(9.27871796999994,11.6,-5.49782415300001));
#180078=CARTESIAN_POINT('Ctrl Pts',(9.28126033199994,15.2,-5.49845993000002));
#180079=CARTESIAN_POINT('Ctrl Pts',(9.28126033199994,11.6,-5.49845993000002));
#180080=CARTESIAN_POINT('Ctrl Pts',(9.28380901399994,15.2,-5.49909498700002));
#180081=CARTESIAN_POINT('Ctrl Pts',(9.28380901399994,11.6,-5.49909498700002));
#180082=CARTESIAN_POINT('Ctrl Pts',(9.28636400899994,15.2,-5.49972931200001));
#180083=CARTESIAN_POINT('Ctrl Pts',(9.28636400899994,11.6,-5.49972931200001));
#180084=CARTESIAN_POINT('Ctrl Pts',(9.28892530699994,15.2,-5.50036289400001));
#180085=CARTESIAN_POINT('Ctrl Pts',(9.28892530699994,11.6,-5.50036289400001));
#180086=CARTESIAN_POINT('Ctrl Pts',(9.29149290099994,15.2,-5.50099572100001));
#180087=CARTESIAN_POINT('Ctrl Pts',(9.29149290099994,11.6,-5.50099572100001));
#180088=CARTESIAN_POINT('Ctrl Pts',(9.29406677899994,15.2,-5.50162778400002));
#180089=CARTESIAN_POINT('Ctrl Pts',(9.29406677899994,11.6,-5.50162778400002));
#180090=CARTESIAN_POINT('Ctrl Pts',(9.29664693399994,15.2,-5.50225906900002));
#180091=CARTESIAN_POINT('Ctrl Pts',(9.29664693399994,11.6,-5.50225906900002));
#180092=CARTESIAN_POINT('Ctrl Pts',(9.29923335799995,15.2,-5.50288956800001));
#180093=CARTESIAN_POINT('Ctrl Pts',(9.29923335799995,11.6,-5.50288956800001));
#180094=CARTESIAN_POINT('Ctrl Pts',(9.30182604099994,15.2,-5.50351926600001));
#180095=CARTESIAN_POINT('Ctrl Pts',(9.30182604099994,11.6,-5.50351926600001));
#180096=CARTESIAN_POINT('Ctrl Pts',(9.30442497499994,15.2,-5.50414815500002));
#180097=CARTESIAN_POINT('Ctrl Pts',(9.30442497499994,11.6,-5.50414815500002));
#180098=CARTESIAN_POINT('Ctrl Pts',(9.30703015099994,15.2,-5.50477622400001));
#180099=CARTESIAN_POINT('Ctrl Pts',(9.30703015099994,11.6,-5.50477622400001));
#180100=CARTESIAN_POINT('Ctrl Pts',(9.30964155999994,15.2,-5.50540346000002));
#180101=CARTESIAN_POINT('Ctrl Pts',(9.30964155999994,11.6,-5.50540346000002));
#180102=CARTESIAN_POINT('Ctrl Pts',(9.31225919399994,15.2,-5.50602985400001));
#180103=CARTESIAN_POINT('Ctrl Pts',(9.31225919399994,11.6,-5.50602985400001));
#180104=CARTESIAN_POINT('Ctrl Pts',(9.31488304399995,15.2,-5.50665539400002));
#180105=CARTESIAN_POINT('Ctrl Pts',(9.31488304399995,11.6,-5.50665539400002));
#180106=CARTESIAN_POINT('Ctrl Pts',(9.31751310199994,15.2,-5.50728006800002));
#180107=CARTESIAN_POINT('Ctrl Pts',(9.31751310199994,11.6,-5.50728006800002));
#180108=CARTESIAN_POINT('Ctrl Pts',(9.32014935799995,15.2,-5.50790386900001));
#180109=CARTESIAN_POINT('Ctrl Pts',(9.32014935799995,11.6,-5.50790386900001));
#180110=CARTESIAN_POINT('Ctrl Pts',(9.32279180499994,15.2,-5.50852678200001));
#180111=CARTESIAN_POINT('Ctrl Pts',(9.32279180499994,11.6,-5.50852678200001));
#180112=CARTESIAN_POINT('Ctrl Pts',(9.32544043299995,15.2,-5.50914879900001));
#180113=CARTESIAN_POINT('Ctrl Pts',(9.32544043299995,11.6,-5.50914879900001));
#180114=CARTESIAN_POINT('Ctrl Pts',(9.32809523399994,15.2,-5.50976990700002));
#180115=CARTESIAN_POINT('Ctrl Pts',(9.32809523399994,11.6,-5.50976990700002));
#180116=CARTESIAN_POINT('Ctrl Pts',(9.33075619899994,15.2,-5.51039009700002));
#180117=CARTESIAN_POINT('Ctrl Pts',(9.33075619899994,11.6,-5.51039009700002));
#180118=CARTESIAN_POINT('Ctrl Pts',(9.33342332099994,15.2,-5.51100935800001));
#180119=CARTESIAN_POINT('Ctrl Pts',(9.33342332099994,11.6,-5.51100935800001));
#180120=CARTESIAN_POINT('Ctrl Pts',(9.33609658899995,15.2,-5.51162767900002));
#180121=CARTESIAN_POINT('Ctrl Pts',(9.33609658899995,11.6,-5.51162767900002));
#180122=CARTESIAN_POINT('Ctrl Pts',(9.33877599599995,15.2,-5.51224504900001));
#180123=CARTESIAN_POINT('Ctrl Pts',(9.33877599599995,11.6,-5.51224504900001));
#180124=CARTESIAN_POINT('Ctrl Pts',(9.34146153499994,15.2,-5.51286145900002));
#180125=CARTESIAN_POINT('Ctrl Pts',(9.34146153499994,11.6,-5.51286145900002));
#180126=CARTESIAN_POINT('Ctrl Pts',(9.34415319399994,15.2,-5.51347689700001));
#180127=CARTESIAN_POINT('Ctrl Pts',(9.34415319399994,11.6,-5.51347689700001));
#180128=CARTESIAN_POINT('Ctrl Pts',(9.34685096599994,15.2,-5.51409135300001));
#180129=CARTESIAN_POINT('Ctrl Pts',(9.34685096599994,11.6,-5.51409135300001));
#180130=CARTESIAN_POINT('Ctrl Pts',(9.34955484399994,15.2,-5.51470481500001));
#180131=CARTESIAN_POINT('Ctrl Pts',(9.34955484399994,11.6,-5.51470481500001));
#180132=CARTESIAN_POINT('Ctrl Pts',(9.35226481699994,15.2,-5.51531727600001));
#180133=CARTESIAN_POINT('Ctrl Pts',(9.35226481699994,11.6,-5.51531727600001));
#180134=CARTESIAN_POINT('Ctrl Pts',(9.35498087799994,15.2,-5.51592872200001));
#180135=CARTESIAN_POINT('Ctrl Pts',(9.35498087799994,11.6,-5.51592872200001));
#180136=CARTESIAN_POINT('Ctrl Pts',(9.35770301899994,15.2,-5.51653914500001));
#180137=CARTESIAN_POINT('Ctrl Pts',(9.35770301899994,11.6,-5.51653914500001));
#180138=CARTESIAN_POINT('Ctrl Pts',(9.36043123099994,15.2,-5.51714853300002));
#180139=CARTESIAN_POINT('Ctrl Pts',(9.36043123099994,11.6,-5.51714853300002));
#180140=CARTESIAN_POINT('Ctrl Pts',(9.36316550599994,15.2,-5.51775687700002));
#180141=CARTESIAN_POINT('Ctrl Pts',(9.36316550599994,11.6,-5.51775687700002));
#180142=CARTESIAN_POINT('Ctrl Pts',(9.36590583399994,15.2,-5.51836416600001));
#180143=CARTESIAN_POINT('Ctrl Pts',(9.36590583399994,11.6,-5.51836416600001));
#180144=CARTESIAN_POINT('Ctrl Pts',(9.36865220799995,15.2,-5.51897039100002));
#180145=CARTESIAN_POINT('Ctrl Pts',(9.36865220799995,11.6,-5.51897039100002));
#180146=CARTESIAN_POINT('Ctrl Pts',(9.37140461999994,15.2,-5.51957553900001));
#180147=CARTESIAN_POINT('Ctrl Pts',(9.37140461999994,11.6,-5.51957553900001));
#180148=CARTESIAN_POINT('Ctrl Pts',(9.37416306099994,15.2,-5.52017960100001));
#180149=CARTESIAN_POINT('Ctrl Pts',(9.37416306099994,11.6,-5.52017960100001));
#180150=CARTESIAN_POINT('Ctrl Pts',(9.37692752299995,15.2,-5.52078256900002));
#180151=CARTESIAN_POINT('Ctrl Pts',(9.37692752299995,11.6,-5.52078256900002));
#180152=CARTESIAN_POINT('Ctrl Pts',(9.37969799599994,15.2,-5.52138443100001));
#180153=CARTESIAN_POINT('Ctrl Pts',(9.37969799599994,11.6,-5.52138443100001));
#180154=CARTESIAN_POINT('Ctrl Pts',(9.38247447299995,15.2,-5.52198517600001));
#180155=CARTESIAN_POINT('Ctrl Pts',(9.38247447299995,11.6,-5.52198517600001));
#180156=CARTESIAN_POINT('Ctrl Pts',(9.38525694699995,15.2,-5.52258479600002));
#180157=CARTESIAN_POINT('Ctrl Pts',(9.38525694699995,11.6,-5.52258479600002));
#180158=CARTESIAN_POINT('Ctrl Pts',(9.38804540799994,15.2,-5.52318328000001));
#180159=CARTESIAN_POINT('Ctrl Pts',(9.38804540799994,11.6,-5.52318328000001));
#180160=CARTESIAN_POINT('Ctrl Pts',(9.39083984799994,15.2,-5.52378061700002));
#180161=CARTESIAN_POINT('Ctrl Pts',(9.39083984799994,11.6,-5.52378061700002));
#180162=CARTESIAN_POINT('Ctrl Pts',(9.39364025899994,15.2,-5.52437679800001));
#180163=CARTESIAN_POINT('Ctrl Pts',(9.39364025899994,11.6,-5.52437679800001));
#180164=CARTESIAN_POINT('Ctrl Pts',(9.39644663199994,15.2,-5.52497181400001));
#180165=CARTESIAN_POINT('Ctrl Pts',(9.39644663199994,11.6,-5.52497181400001));
#180166=CARTESIAN_POINT('Ctrl Pts',(9.39925895999994,15.2,-5.52556565300002));
#180167=CARTESIAN_POINT('Ctrl Pts',(9.39925895999994,11.6,-5.52556565300002));
#180168=CARTESIAN_POINT('Ctrl Pts',(9.40207723299994,15.2,-5.52615830700002));
#180169=CARTESIAN_POINT('Ctrl Pts',(9.40207723299994,11.6,-5.52615830700002));
#180170=CARTESIAN_POINT('Ctrl Pts',(9.40490144599995,15.2,-5.52674976500001));
#180171=CARTESIAN_POINT('Ctrl Pts',(9.40490144599995,11.6,-5.52674976500001));
#180172=CARTESIAN_POINT('Ctrl Pts',(9.40773158599994,15.2,-5.52734001800002));
#180173=CARTESIAN_POINT('Ctrl Pts',(9.40773158599994,11.6,-5.52734001800002));
#180174=CARTESIAN_POINT('Ctrl Pts',(9.41056764899994,15.2,-5.52792905400001));
#180175=CARTESIAN_POINT('Ctrl Pts',(9.41056764899994,11.6,-5.52792905400001));
#180176=CARTESIAN_POINT('Ctrl Pts',(9.41340962499994,15.2,-5.52851686700001));
#180177=CARTESIAN_POINT('Ctrl Pts',(9.41340962499994,11.6,-5.52851686700001));
#180178=CARTESIAN_POINT('Ctrl Pts',(9.41625750599994,15.2,-5.52910344300001));
#180179=CARTESIAN_POINT('Ctrl Pts',(9.41625750599994,11.6,-5.52910344300001));
#180180=CARTESIAN_POINT('Ctrl Pts',(9.41911128299994,15.2,-5.52968877500001));
#180181=CARTESIAN_POINT('Ctrl Pts',(9.41911128299994,11.6,-5.52968877500001));
#180182=CARTESIAN_POINT('Ctrl Pts',(9.42197095099995,15.2,-5.53027285400002));
#180183=CARTESIAN_POINT('Ctrl Pts',(9.42197095099995,11.6,-5.53027285400002));
#180184=CARTESIAN_POINT('Ctrl Pts',(9.42483649799994,15.2,-5.53085566800001));
#180185=CARTESIAN_POINT('Ctrl Pts',(9.42483649799994,11.6,-5.53085566800001));
#180186=CARTESIAN_POINT('Ctrl Pts',(9.42770791699994,15.2,-5.53143720800001));
#180187=CARTESIAN_POINT('Ctrl Pts',(9.42770791699994,11.6,-5.53143720800001));
#180188=CARTESIAN_POINT('Ctrl Pts',(9.43058520099994,15.2,-5.53201746500001));
#180189=CARTESIAN_POINT('Ctrl Pts',(9.43058520099994,11.6,-5.53201746500001));
#180190=CARTESIAN_POINT('Ctrl Pts',(9.43346834199994,15.2,-5.53259643000001));
#180191=CARTESIAN_POINT('Ctrl Pts',(9.43346834199994,11.6,-5.53259643000001));
#180192=CARTESIAN_POINT('Ctrl Pts',(9.43635733099994,15.2,-5.53317409200002));
#180193=CARTESIAN_POINT('Ctrl Pts',(9.43635733099994,11.6,-5.53317409200002));
#180194=CARTESIAN_POINT('Ctrl Pts',(9.43925215899995,15.2,-5.53375044300001));
#180195=CARTESIAN_POINT('Ctrl Pts',(9.43925215899995,11.6,-5.53375044300001));
#180196=CARTESIAN_POINT('Ctrl Pts',(9.44215281999995,15.2,-5.53432547200002));
#180197=CARTESIAN_POINT('Ctrl Pts',(9.44215281999995,11.6,-5.53432547200002));
#180198=CARTESIAN_POINT('Ctrl Pts',(9.44505930299995,15.2,-5.53489917000002));
#180199=CARTESIAN_POINT('Ctrl Pts',(9.44505930299995,11.6,-5.53489917000002));
#180200=CARTESIAN_POINT('Ctrl Pts',(9.44797160499995,15.2,-5.53547152800002));
#180201=CARTESIAN_POINT('Ctrl Pts',(9.44797160499995,11.6,-5.53547152800002));
#180202=CARTESIAN_POINT('Ctrl Pts',(9.45088971199995,15.2,-5.53604253600001));
#180203=CARTESIAN_POINT('Ctrl Pts',(9.45088971199995,11.6,-5.53604253600001));
#180204=CARTESIAN_POINT('Ctrl Pts',(9.45381361999994,15.2,-5.53661218600002));
#180205=CARTESIAN_POINT('Ctrl Pts',(9.45381361999994,11.6,-5.53661218600002));
#180206=CARTESIAN_POINT('Ctrl Pts',(9.45674331999994,15.2,-5.53718046700002));
#180207=CARTESIAN_POINT('Ctrl Pts',(9.45674331999994,11.6,-5.53718046700002));
#180208=CARTESIAN_POINT('Ctrl Pts',(9.45967880299994,15.2,-5.53774737000001));
#180209=CARTESIAN_POINT('Ctrl Pts',(9.45967880299994,11.6,-5.53774737000001));
#180210=CARTESIAN_POINT('Ctrl Pts',(9.46262006299994,15.2,-5.53831288700001));
#180211=CARTESIAN_POINT('Ctrl Pts',(9.46262006299994,11.6,-5.53831288700001));
#180212=CARTESIAN_POINT('Ctrl Pts',(9.46556708999994,15.2,-5.53887700700002));
#180213=CARTESIAN_POINT('Ctrl Pts',(9.46556708999994,11.6,-5.53887700700002));
#180214=CARTESIAN_POINT('Ctrl Pts',(9.46851987599995,15.2,-5.53943972100001));
#180215=CARTESIAN_POINT('Ctrl Pts',(9.46851987599995,11.6,-5.53943972100001));
#180216=CARTESIAN_POINT('Ctrl Pts',(9.47147841599994,15.2,-5.54000102100002));
#180217=CARTESIAN_POINT('Ctrl Pts',(9.47147841599994,11.6,-5.54000102100002));
#180218=CARTESIAN_POINT('Ctrl Pts',(9.47444269799995,15.2,-5.54056089700001));
#180219=CARTESIAN_POINT('Ctrl Pts',(9.47444269799995,11.6,-5.54056089700001));
#180220=CARTESIAN_POINT('Ctrl Pts',(9.47741271699994,15.2,-5.54111934000002));
#180221=CARTESIAN_POINT('Ctrl Pts',(9.47741271699994,11.6,-5.54111934000002));
#180222=CARTESIAN_POINT('Ctrl Pts',(9.48038846399994,15.2,-5.54167634100001));
#180223=CARTESIAN_POINT('Ctrl Pts',(9.48038846399994,11.6,-5.54167634100001));
#180224=CARTESIAN_POINT('Ctrl Pts',(9.48336992999995,15.2,-5.54223189000002));
#180225=CARTESIAN_POINT('Ctrl Pts',(9.48336992999995,11.6,-5.54223189000002));
#180226=CARTESIAN_POINT('Ctrl Pts',(9.48635710799994,15.2,-5.54278597900002));
#180227=CARTESIAN_POINT('Ctrl Pts',(9.48635710799994,11.6,-5.54278597900002));
#180228=CARTESIAN_POINT('Ctrl Pts',(9.48934999199994,15.2,-5.54333859800002));
#180229=CARTESIAN_POINT('Ctrl Pts',(9.48934999199994,11.6,-5.54333859800002));
#180230=CARTESIAN_POINT('Ctrl Pts',(9.49234857199994,15.2,-5.54388973900001));
#180231=CARTESIAN_POINT('Ctrl Pts',(9.49234857199994,11.6,-5.54388973900001));
#180232=CARTESIAN_POINT('Ctrl Pts',(9.49535283999994,15.2,-5.54443939200001));
#180233=CARTESIAN_POINT('Ctrl Pts',(9.49535283999994,11.6,-5.54443939200001));
#180234=CARTESIAN_POINT('Ctrl Pts',(9.49836278899994,15.2,-5.54498754900001));
#180235=CARTESIAN_POINT('Ctrl Pts',(9.49836278899994,11.6,-5.54498754900001));
#180236=CARTESIAN_POINT('Ctrl Pts',(9.50137840999994,15.2,-5.54553420100001));
#180237=CARTESIAN_POINT('Ctrl Pts',(9.50137840999994,11.6,-5.54553420100001));
#180238=CARTESIAN_POINT('Ctrl Pts',(9.50439969699995,15.2,-5.54607933800002));
#180239=CARTESIAN_POINT('Ctrl Pts',(9.50439969699995,11.6,-5.54607933800002));
#180240=CARTESIAN_POINT('Ctrl Pts',(9.50742664099995,15.2,-5.54662295200002));
#180241=CARTESIAN_POINT('Ctrl Pts',(9.50742664099995,11.6,-5.54662295200002));
#180242=CARTESIAN_POINT('Ctrl Pts',(9.51045923299995,15.2,-5.54716503400002));
#180243=CARTESIAN_POINT('Ctrl Pts',(9.51045923299995,11.6,-5.54716503400002));
#180244=CARTESIAN_POINT('Ctrl Pts',(9.51349746799995,15.2,-5.54770557400001));
#180245=CARTESIAN_POINT('Ctrl Pts',(9.51349746799995,11.6,-5.54770557400001));
#180246=CARTESIAN_POINT('Ctrl Pts',(9.51654133599994,15.2,-5.54824456500001));
#180247=CARTESIAN_POINT('Ctrl Pts',(9.51654133599994,11.6,-5.54824456500001));
#180248=CARTESIAN_POINT('Ctrl Pts',(9.51959082999995,15.2,-5.54878199800001));
#180249=CARTESIAN_POINT('Ctrl Pts',(9.51959082999995,11.6,-5.54878199800001));
#180250=CARTESIAN_POINT('Ctrl Pts',(9.52264594199994,15.2,-5.54931786200001));
#180251=CARTESIAN_POINT('Ctrl Pts',(9.52264594199994,11.6,-5.54931786200001));
#180252=CARTESIAN_POINT('Ctrl Pts',(9.52570666499994,15.2,-5.54985215100002));
#180253=CARTESIAN_POINT('Ctrl Pts',(9.52570666499994,11.6,-5.54985215100002));
#180254=CARTESIAN_POINT('Ctrl Pts',(9.52877299099995,15.2,-5.55038485500001));
#180255=CARTESIAN_POINT('Ctrl Pts',(9.52877299099995,11.6,-5.55038485500001));
#180256=CARTESIAN_POINT('Ctrl Pts',(9.53184491099995,15.2,-5.55091596500001));
#180257=CARTESIAN_POINT('Ctrl Pts',(9.53184491099995,11.6,-5.55091596500001));
#180258=CARTESIAN_POINT('Ctrl Pts',(9.53492241699994,15.2,-5.55144547300001));
#180259=CARTESIAN_POINT('Ctrl Pts',(9.53492241699994,11.6,-5.55144547300001));
#180260=CARTESIAN_POINT('Ctrl Pts',(9.53800550299994,15.2,-5.55197337000001));
#180261=CARTESIAN_POINT('Ctrl Pts',(9.53800550299994,11.6,-5.55197337000001));
#180262=CARTESIAN_POINT('Ctrl Pts',(9.54109416199995,15.2,-5.55249964700002));
#180263=CARTESIAN_POINT('Ctrl Pts',(9.54109416199995,11.6,-5.55249964700002));
#180264=CARTESIAN_POINT('Ctrl Pts',(9.54418838399994,15.2,-5.55302429700001));
#180265=CARTESIAN_POINT('Ctrl Pts',(9.54418838399994,11.6,-5.55302429700001));
#180266=CARTESIAN_POINT('Ctrl Pts',(9.54728816099994,15.2,-5.55354730900001));
#180267=CARTESIAN_POINT('Ctrl Pts',(9.54728816099994,11.6,-5.55354730900001));
#180268=CARTESIAN_POINT('Ctrl Pts',(9.55039348899994,15.2,-5.55406867700002));
#180269=CARTESIAN_POINT('Ctrl Pts',(9.55039348899994,11.6,-5.55406867700002));
#180270=CARTESIAN_POINT('Ctrl Pts',(9.55350435499994,15.2,-5.55458839000002));
#180271=CARTESIAN_POINT('Ctrl Pts',(9.55350435499994,11.6,-5.55458839000002));
#180272=CARTESIAN_POINT('Ctrl Pts',(9.55662075599994,15.2,-5.55510644200002));
#180273=CARTESIAN_POINT('Ctrl Pts',(9.55662075599994,11.6,-5.55510644200002));
#180274=CARTESIAN_POINT('Ctrl Pts',(9.55974268199995,15.2,-5.55562282200002));
#180275=CARTESIAN_POINT('Ctrl Pts',(9.55974268199995,11.6,-5.55562282200002));
#180276=CARTESIAN_POINT('Ctrl Pts',(9.56287012499994,15.2,-5.55613752300002));
#180277=CARTESIAN_POINT('Ctrl Pts',(9.56287012499994,11.6,-5.55613752300002));
#180278=CARTESIAN_POINT('Ctrl Pts',(9.56600307899994,15.2,-5.55665053600002));
#180279=CARTESIAN_POINT('Ctrl Pts',(9.56600307899994,11.6,-5.55665053600002));
#180280=CARTESIAN_POINT('Ctrl Pts',(9.56914153599994,15.2,-5.55716185400001));
#180281=CARTESIAN_POINT('Ctrl Pts',(9.56914153599994,11.6,-5.55716185400001));
#180282=CARTESIAN_POINT('Ctrl Pts',(9.57228548599995,15.2,-5.55767146700001));
#180283=CARTESIAN_POINT('Ctrl Pts',(9.57228548599995,11.6,-5.55767146700001));
#180284=CARTESIAN_POINT('Ctrl Pts',(9.57543492599994,15.2,-5.55817936800001));
#180285=CARTESIAN_POINT('Ctrl Pts',(9.57543492599994,11.6,-5.55817936800001));
#180286=CARTESIAN_POINT('Ctrl Pts',(9.57858984399994,15.2,-5.55868554600002));
#180287=CARTESIAN_POINT('Ctrl Pts',(9.57858984399994,11.6,-5.55868554600002));
#180288=CARTESIAN_POINT('Ctrl Pts',(9.58175023399994,15.2,-5.55918999500001));
#180289=CARTESIAN_POINT('Ctrl Pts',(9.58175023399994,11.6,-5.55918999500001));
#180290=CARTESIAN_POINT('Ctrl Pts',(9.58491608899994,15.2,-5.55969270700002));
#180291=CARTESIAN_POINT('Ctrl Pts',(9.58491608899994,11.6,-5.55969270700002));
#180292=CARTESIAN_POINT('Ctrl Pts',(9.58808740099995,15.2,-5.56019367300001));
#180293=CARTESIAN_POINT('Ctrl Pts',(9.58808740099995,11.6,-5.56019367300001));
#180294=CARTESIAN_POINT('Ctrl Pts',(9.59126416099994,15.2,-5.56069288500002));
#180295=CARTESIAN_POINT('Ctrl Pts',(9.59126416099994,11.6,-5.56069288500002));
#180296=CARTESIAN_POINT('Ctrl Pts',(9.59444636399994,15.2,-5.56119033300002));
#180297=CARTESIAN_POINT('Ctrl Pts',(9.59444636399994,11.6,-5.56119033300002));
#180298=CARTESIAN_POINT('Ctrl Pts',(9.59763400099994,15.2,-5.56168601100001));
#180299=CARTESIAN_POINT('Ctrl Pts',(9.59763400099994,11.6,-5.56168601100001));
#180300=CARTESIAN_POINT('Ctrl Pts',(9.60082706499995,15.2,-5.56217991100001));
#180301=CARTESIAN_POINT('Ctrl Pts',(9.60082706499995,11.6,-5.56217991100001));
#180302=CARTESIAN_POINT('Ctrl Pts',(9.60402554699994,15.2,-5.56267202300001));
#180303=CARTESIAN_POINT('Ctrl Pts',(9.60402554699994,11.6,-5.56267202300001));
#180304=CARTESIAN_POINT('Ctrl Pts',(9.60722944199994,15.2,-5.56316234000001));
#180305=CARTESIAN_POINT('Ctrl Pts',(9.60722944199994,11.6,-5.56316234000001));
#180306=CARTESIAN_POINT('Ctrl Pts',(9.61043874099994,15.2,-5.56365085400001));
#180307=CARTESIAN_POINT('Ctrl Pts',(9.61043874099994,11.6,-5.56365085400001));
#180308=CARTESIAN_POINT('Ctrl Pts',(9.61365343599994,15.2,-5.56413755600001));
#180309=CARTESIAN_POINT('Ctrl Pts',(9.61365343599994,11.6,-5.56413755600001));
#180310=CARTESIAN_POINT('Ctrl Pts',(9.61687351899995,15.2,-5.56462243900001));
#180311=CARTESIAN_POINT('Ctrl Pts',(9.61687351899995,11.6,-5.56462243900001));
#180312=CARTESIAN_POINT('Ctrl Pts',(9.62009898499995,15.2,-5.56510549400001));
#180313=CARTESIAN_POINT('Ctrl Pts',(9.62009898499995,11.6,-5.56510549400001));
#180314=CARTESIAN_POINT('Ctrl Pts',(9.62332982499994,15.2,-5.56558671400001));
#180315=CARTESIAN_POINT('Ctrl Pts',(9.62332982499994,11.6,-5.56558671400001));
#180316=CARTESIAN_POINT('Ctrl Pts',(9.62656603099994,15.2,-5.56606609100001));
#180317=CARTESIAN_POINT('Ctrl Pts',(9.62656603099994,11.6,-5.56606609100001));
#180318=CARTESIAN_POINT('Ctrl Pts',(9.62980759699994,15.2,-5.56654361600001));
#180319=CARTESIAN_POINT('Ctrl Pts',(9.62980759699994,11.6,-5.56654361600001));
#180320=CARTESIAN_POINT('Ctrl Pts',(9.63305451399994,15.2,-5.56701928100001));
#180321=CARTESIAN_POINT('Ctrl Pts',(9.63305451399994,11.6,-5.56701928100001));
#180322=CARTESIAN_POINT('Ctrl Pts',(9.63630677599994,15.2,-5.56749307900001));
#180323=CARTESIAN_POINT('Ctrl Pts',(9.63630677599994,11.6,-5.56749307900001));
#180324=CARTESIAN_POINT('Ctrl Pts',(9.63956437399995,15.2,-5.56796500300001));
#180325=CARTESIAN_POINT('Ctrl Pts',(9.63956437399995,11.6,-5.56796500300001));
#180326=CARTESIAN_POINT('Ctrl Pts',(9.64282730199994,15.2,-5.56843504200002));
#180327=CARTESIAN_POINT('Ctrl Pts',(9.64282730199994,11.6,-5.56843504200002));
#180328=CARTESIAN_POINT('Ctrl Pts',(9.64609555199995,15.2,-5.56890319100001));
#180329=CARTESIAN_POINT('Ctrl Pts',(9.64609555199995,11.6,-5.56890319100001));
#180330=CARTESIAN_POINT('Ctrl Pts',(9.64936911699995,15.2,-5.56936944000002));
#180331=CARTESIAN_POINT('Ctrl Pts',(9.64936911699995,11.6,-5.56936944000002));
#180332=CARTESIAN_POINT('Ctrl Pts',(9.65264798699994,15.2,-5.56983378400002));
#180333=CARTESIAN_POINT('Ctrl Pts',(9.65264798699994,11.6,-5.56983378400002));
#180334=CARTESIAN_POINT('Ctrl Pts',(9.65593215899995,15.2,-5.57029621200002));
#180335=CARTESIAN_POINT('Ctrl Pts',(9.65593215899995,11.6,-5.57029621200002));
#180336=CARTESIAN_POINT('Ctrl Pts',(9.65922162299995,15.2,-5.57075671900002));
#180337=CARTESIAN_POINT('Ctrl Pts',(9.65922162299995,11.6,-5.57075671900002));
#180338=CARTESIAN_POINT('Ctrl Pts',(9.66251637199995,15.2,-5.57121529500002));
#180339=CARTESIAN_POINT('Ctrl Pts',(9.66251637199995,11.6,-5.57121529500002));
#180340=CARTESIAN_POINT('Ctrl Pts',(9.66581639799994,15.2,-5.57167193400002));
#180341=CARTESIAN_POINT('Ctrl Pts',(9.66581639799994,11.6,-5.57167193400002));
#180342=CARTESIAN_POINT('Ctrl Pts',(9.66912169399994,15.2,-5.57212662600001));
#180343=CARTESIAN_POINT('Ctrl Pts',(9.66912169399994,11.6,-5.57212662600001));
#180344=CARTESIAN_POINT('Ctrl Pts',(9.67243225399995,15.2,-5.57257936700001));
#180345=CARTESIAN_POINT('Ctrl Pts',(9.67243225399995,11.6,-5.57257936700001));
#180346=CARTESIAN_POINT('Ctrl Pts',(9.67574806899995,15.2,-5.57303014600001));
#180347=CARTESIAN_POINT('Ctrl Pts',(9.67574806899995,11.6,-5.57303014600001));
#180348=CARTESIAN_POINT('Ctrl Pts',(9.67906913299995,15.2,-5.57347895600001));
#180349=CARTESIAN_POINT('Ctrl Pts',(9.67906913299995,11.6,-5.57347895600001));
#180350=CARTESIAN_POINT('Ctrl Pts',(9.68239543699994,15.2,-5.57392579100001));
#180351=CARTESIAN_POINT('Ctrl Pts',(9.68239543699994,11.6,-5.57392579100001));
#180352=CARTESIAN_POINT('Ctrl Pts',(9.68572697499994,15.2,-5.57437064100001));
#180353=CARTESIAN_POINT('Ctrl Pts',(9.68572697499994,11.6,-5.57437064100001));
#180354=CARTESIAN_POINT('Ctrl Pts',(9.68906373899994,15.2,-5.57481350100002));
#180355=CARTESIAN_POINT('Ctrl Pts',(9.68906373899994,11.6,-5.57481350100002));
#180356=CARTESIAN_POINT('Ctrl Pts',(9.69240572199995,15.2,-5.57525436100001));
#180357=CARTESIAN_POINT('Ctrl Pts',(9.69240572199995,11.6,-5.57525436100001));
#180358=CARTESIAN_POINT('Ctrl Pts',(9.69575291699995,15.2,-5.57569321400001));
#180359=CARTESIAN_POINT('Ctrl Pts',(9.69575291699995,11.6,-5.57569321400001));
#180360=CARTESIAN_POINT('Ctrl Pts',(9.69910531599995,15.2,-5.57613005500002));
#180361=CARTESIAN_POINT('Ctrl Pts',(9.69910531599995,11.6,-5.57613005500002));
#180362=CARTESIAN_POINT('Ctrl Pts',(9.70246291199994,15.2,-5.57656487300001));
#180363=CARTESIAN_POINT('Ctrl Pts',(9.70246291199994,11.6,-5.57656487300001));
#180364=CARTESIAN_POINT('Ctrl Pts',(9.70582569899994,15.2,-5.57699766300002));
#180365=CARTESIAN_POINT('Ctrl Pts',(9.70582569899994,11.6,-5.57699766300002));
#180366=CARTESIAN_POINT('Ctrl Pts',(9.70919366699994,15.2,-5.57742841500001));
#180367=CARTESIAN_POINT('Ctrl Pts',(9.70919366699994,11.6,-5.57742841500001));
#180368=CARTESIAN_POINT('Ctrl Pts',(9.71256681199995,15.2,-5.57785712500001));
#180369=CARTESIAN_POINT('Ctrl Pts',(9.71256681199995,11.6,-5.57785712500001));
#180370=CARTESIAN_POINT('Ctrl Pts',(9.71594512499994,15.2,-5.57828378300002));
#180371=CARTESIAN_POINT('Ctrl Pts',(9.71594512499994,11.6,-5.57828378300002));
#180372=CARTESIAN_POINT('Ctrl Pts',(9.71932859799994,15.2,-5.57870838100001));
#180373=CARTESIAN_POINT('Ctrl Pts',(9.71932859799994,11.6,-5.57870838100001));
#180374=CARTESIAN_POINT('Ctrl Pts',(9.72271722499995,15.2,-5.57913091500001));
#180375=CARTESIAN_POINT('Ctrl Pts',(9.72271722499995,11.6,-5.57913091500001));
#180376=CARTESIAN_POINT('Ctrl Pts',(9.72611099799994,15.2,-5.57955137400001));
#180377=CARTESIAN_POINT('Ctrl Pts',(9.72611099799994,11.6,-5.57955137400001));
#180378=CARTESIAN_POINT('Ctrl Pts',(9.72950990999994,15.2,-5.57996975200002));
#180379=CARTESIAN_POINT('Ctrl Pts',(9.72950990999994,11.6,-5.57996975200002));
#180380=CARTESIAN_POINT('Ctrl Pts',(9.73291395499994,15.2,-5.58038604300001));
#180381=CARTESIAN_POINT('Ctrl Pts',(9.73291395499994,11.6,-5.58038604300001));
#180382=CARTESIAN_POINT('Ctrl Pts',(9.73632312399995,15.2,-5.58080023800001));
#180383=CARTESIAN_POINT('Ctrl Pts',(9.73632312399995,11.6,-5.58080023800001));
#180384=CARTESIAN_POINT('Ctrl Pts',(9.73973740999994,15.2,-5.58121233000001));
#180385=CARTESIAN_POINT('Ctrl Pts',(9.73973740999994,11.6,-5.58121233000001));
#180386=CARTESIAN_POINT('Ctrl Pts',(9.74315680699995,15.2,-5.58162231200001));
#180387=CARTESIAN_POINT('Ctrl Pts',(9.74315680699995,11.6,-5.58162231200001));
#180388=CARTESIAN_POINT('Ctrl Pts',(9.74658130799994,15.2,-5.58203017700002));
#180389=CARTESIAN_POINT('Ctrl Pts',(9.74658130799994,11.6,-5.58203017700002));
#180390=CARTESIAN_POINT('Ctrl Pts',(9.75001090399994,15.2,-5.58243591700001));
#180391=CARTESIAN_POINT('Ctrl Pts',(9.75001090399994,11.6,-5.58243591700001));
#180392=CARTESIAN_POINT('Ctrl Pts',(9.75344559099995,15.2,-5.58283952600001));
#180393=CARTESIAN_POINT('Ctrl Pts',(9.75344559099995,11.6,-5.58283952600001));
#180394=CARTESIAN_POINT('Ctrl Pts',(9.75688535799994,15.2,-5.58324099500001));
#180395=CARTESIAN_POINT('Ctrl Pts',(9.75688535799994,11.6,-5.58324099500001));
#180396=CARTESIAN_POINT('Ctrl Pts',(9.76033019899995,15.2,-5.58364031900001));
#180397=CARTESIAN_POINT('Ctrl Pts',(9.76033019899995,11.6,-5.58364031900001));
#180398=CARTESIAN_POINT('Ctrl Pts',(9.76378010899994,15.2,-5.58403749000002));
#180399=CARTESIAN_POINT('Ctrl Pts',(9.76378010899994,11.6,-5.58403749000002));
#180400=CARTESIAN_POINT('Ctrl Pts',(9.76723507899995,15.2,-5.58443250000002));
#180401=CARTESIAN_POINT('Ctrl Pts',(9.76723507899995,11.6,-5.58443250000002));
#180402=CARTESIAN_POINT('Ctrl Pts',(9.77069510099994,15.2,-5.58482534100001));
#180403=CARTESIAN_POINT('Ctrl Pts',(9.77069510099994,11.6,-5.58482534100001));
#180404=CARTESIAN_POINT('Ctrl Pts',(9.77416016999994,15.2,-5.58521600900002));
#180405=CARTESIAN_POINT('Ctrl Pts',(9.77416016999994,11.6,-5.58521600900002));
#180406=CARTESIAN_POINT('Ctrl Pts',(9.77763027799995,15.2,-5.58560449600002));
#180407=CARTESIAN_POINT('Ctrl Pts',(9.77763027799995,11.6,-5.58560449600002));
#180408=CARTESIAN_POINT('Ctrl Pts',(9.78110541799994,15.2,-5.58599079400001));
#180409=CARTESIAN_POINT('Ctrl Pts',(9.78110541799994,11.6,-5.58599079400001));
#180410=CARTESIAN_POINT('Ctrl Pts',(9.78458558299995,15.2,-5.58637489500001));
#180411=CARTESIAN_POINT('Ctrl Pts',(9.78458558299995,11.6,-5.58637489500001));
#180412=CARTESIAN_POINT('Ctrl Pts',(9.78807076599994,15.2,-5.58675679400002));
#180413=CARTESIAN_POINT('Ctrl Pts',(9.78807076599994,11.6,-5.58675679400002));
#180414=CARTESIAN_POINT('Ctrl Pts',(9.79156095799994,15.2,-5.58713648300001));
#180415=CARTESIAN_POINT('Ctrl Pts',(9.79156095799994,11.6,-5.58713648300001));
#180416=CARTESIAN_POINT('Ctrl Pts',(9.79505615499994,15.2,-5.58751395600002));
#180417=CARTESIAN_POINT('Ctrl Pts',(9.79505615499994,11.6,-5.58751395600002));
#180418=CARTESIAN_POINT('Ctrl Pts',(9.79855634899994,15.2,-5.58788920400001));
#180419=CARTESIAN_POINT('Ctrl Pts',(9.79855634899994,11.6,-5.58788920400001));
#180420=CARTESIAN_POINT('Ctrl Pts',(9.80206153099994,15.2,-5.58826222200001));
#180421=CARTESIAN_POINT('Ctrl Pts',(9.80206153099994,11.6,-5.58826222200001));
#180422=CARTESIAN_POINT('Ctrl Pts',(9.80557169599994,15.2,-5.58863300200001));
#180423=CARTESIAN_POINT('Ctrl Pts',(9.80557169599994,11.6,-5.58863300200001));
#180424=CARTESIAN_POINT('Ctrl Pts',(9.80908683699995,15.2,-5.58900153800002));
#180425=CARTESIAN_POINT('Ctrl Pts',(9.80908683699995,11.6,-5.58900153800002));
#180426=CARTESIAN_POINT('Ctrl Pts',(9.81260694599994,15.2,-5.58936782200002));
#180427=CARTESIAN_POINT('Ctrl Pts',(9.81260694599994,11.6,-5.58936782200002));
#180428=CARTESIAN_POINT('Ctrl Pts',(9.81613201599994,15.2,-5.58973184900001));
#180429=CARTESIAN_POINT('Ctrl Pts',(9.81613201599994,11.6,-5.58973184900001));
#180430=CARTESIAN_POINT('Ctrl Pts',(9.81966204099994,15.2,-5.59009360900002));
#180431=CARTESIAN_POINT('Ctrl Pts',(9.81966204099994,11.6,-5.59009360900002));
#180432=CARTESIAN_POINT('Ctrl Pts',(9.82319701199994,15.2,-5.59045309800001));
#180433=CARTESIAN_POINT('Ctrl Pts',(9.82319701199994,11.6,-5.59045309800001));
#180434=CARTESIAN_POINT('Ctrl Pts',(9.82673692399995,15.2,-5.59081030900002));
#180435=CARTESIAN_POINT('Ctrl Pts',(9.82673692399995,11.6,-5.59081030900002));
#180436=CARTESIAN_POINT('Ctrl Pts',(9.83028176999994,15.2,-5.59116523300002));
#180437=CARTESIAN_POINT('Ctrl Pts',(9.83028176999994,11.6,-5.59116523300002));
#180438=CARTESIAN_POINT('Ctrl Pts',(9.83383154199995,15.2,-5.59151786600002));
#180439=CARTESIAN_POINT('Ctrl Pts',(9.83383154199995,11.6,-5.59151786600002));
#180440=CARTESIAN_POINT('Ctrl Pts',(9.83738623299995,15.2,-5.59186819800002));
#180441=CARTESIAN_POINT('Ctrl Pts',(9.83738623299995,11.6,-5.59186819800002));
#180442=CARTESIAN_POINT('Ctrl Pts',(9.84094583499994,15.2,-5.59221622600001));
#180443=CARTESIAN_POINT('Ctrl Pts',(9.84094583499994,11.6,-5.59221622600001));
#180444=CARTESIAN_POINT('Ctrl Pts',(9.84451034499994,15.2,-5.59256194000001));
#180445=CARTESIAN_POINT('Ctrl Pts',(9.84451034499994,11.6,-5.59256194000001));
#180446=CARTESIAN_POINT('Ctrl Pts',(9.84807975099995,15.2,-5.59290533500001));
#180447=CARTESIAN_POINT('Ctrl Pts',(9.84807975099995,11.6,-5.59290533500001));
#180448=CARTESIAN_POINT('Ctrl Pts',(9.85165404999995,15.2,-5.59324640400002));
#180449=CARTESIAN_POINT('Ctrl Pts',(9.85165404999995,11.6,-5.59324640400002));
#180450=CARTESIAN_POINT('Ctrl Pts',(9.85523323299994,15.2,-5.59358514100001));
#180451=CARTESIAN_POINT('Ctrl Pts',(9.85523323299994,11.6,-5.59358514100001));
#180452=CARTESIAN_POINT('Ctrl Pts',(9.85881729299994,15.2,-5.59392153800002));
#180453=CARTESIAN_POINT('Ctrl Pts',(9.85881729299994,11.6,-5.59392153800002));
#180454=CARTESIAN_POINT('Ctrl Pts',(9.86240622499994,15.2,-5.59425558900001));
#180455=CARTESIAN_POINT('Ctrl Pts',(9.86240622499994,11.6,-5.59425558900001));
#180456=CARTESIAN_POINT('Ctrl Pts',(9.86600001899994,15.2,-5.59458728700001));
#180457=CARTESIAN_POINT('Ctrl Pts',(9.86600001899994,11.6,-5.59458728700001));
#180458=CARTESIAN_POINT('Ctrl Pts',(9.86959867099995,15.2,-5.59491662600001));
#180459=CARTESIAN_POINT('Ctrl Pts',(9.86959867099995,11.6,-5.59491662600001));
#180460=CARTESIAN_POINT('Ctrl Pts',(9.87320217199994,15.2,-5.59524360000001));
#180461=CARTESIAN_POINT('Ctrl Pts',(9.87320217199994,11.6,-5.59524360000001));
#180462=CARTESIAN_POINT('Ctrl Pts',(9.87681051699994,15.2,-5.59556820100001));
#180463=CARTESIAN_POINT('Ctrl Pts',(9.87681051699994,11.6,-5.59556820100001));
#180464=CARTESIAN_POINT('Ctrl Pts',(9.88042369799994,15.2,-5.59589042300002));
#180465=CARTESIAN_POINT('Ctrl Pts',(9.88042369799994,11.6,-5.59589042300002));
#180466=CARTESIAN_POINT('Ctrl Pts',(9.88404170699994,15.2,-5.59621025900002));
#180467=CARTESIAN_POINT('Ctrl Pts',(9.88404170699994,11.6,-5.59621025900002));
#180468=CARTESIAN_POINT('Ctrl Pts',(9.88766453899995,15.2,-5.59652770400001));
#180469=CARTESIAN_POINT('Ctrl Pts',(9.88766453899995,11.6,-5.59652770400001));
#180470=CARTESIAN_POINT('Ctrl Pts',(9.89129218699994,15.2,-5.59684275000001));
#180471=CARTESIAN_POINT('Ctrl Pts',(9.89129218699994,11.6,-5.59684275000001));
#180472=CARTESIAN_POINT('Ctrl Pts',(9.89492464299994,15.2,-5.59715539100001));
#180473=CARTESIAN_POINT('Ctrl Pts',(9.89492464299994,11.6,-5.59715539100001));
#180474=CARTESIAN_POINT('Ctrl Pts',(9.89856189999994,15.2,-5.59746562100001));
#180475=CARTESIAN_POINT('Ctrl Pts',(9.89856189999994,11.6,-5.59746562100001));
#180476=CARTESIAN_POINT('Ctrl Pts',(9.90220395199995,15.2,-5.59777343200001));
#180477=CARTESIAN_POINT('Ctrl Pts',(9.90220395199995,11.6,-5.59777343200001));
#180478=CARTESIAN_POINT('Ctrl Pts',(9.90585079199995,15.2,-5.59807881900001));
#180479=CARTESIAN_POINT('Ctrl Pts',(9.90585079199995,11.6,-5.59807881900001));
#180480=CARTESIAN_POINT('Ctrl Pts',(9.90950241399995,15.2,-5.59838177500001));
#180481=CARTESIAN_POINT('Ctrl Pts',(9.90950241399995,11.6,-5.59838177500001));
#180482=CARTESIAN_POINT('Ctrl Pts',(9.91315880899995,15.2,-5.59868229500001));
#180483=CARTESIAN_POINT('Ctrl Pts',(9.91315880899995,11.6,-5.59868229500001));
#180484=CARTESIAN_POINT('Ctrl Pts',(9.91681997199995,15.2,-5.59898037100002));
#180485=CARTESIAN_POINT('Ctrl Pts',(9.91681997199995,11.6,-5.59898037100002));
#180486=CARTESIAN_POINT('Ctrl Pts',(9.92048589699994,15.2,-5.59927599600002));
#180487=CARTESIAN_POINT('Ctrl Pts',(9.92048589699994,11.6,-5.59927599600002));
#180488=CARTESIAN_POINT('Ctrl Pts',(9.92415657399994,15.2,-5.59956916600001));
#180489=CARTESIAN_POINT('Ctrl Pts',(9.92415657399994,11.6,-5.59956916600001));
#180490=CARTESIAN_POINT('Ctrl Pts',(9.92783199799995,15.2,-5.59985987200001));
#180491=CARTESIAN_POINT('Ctrl Pts',(9.92783199799995,11.6,-5.59985987200001));
#180492=CARTESIAN_POINT('Ctrl Pts',(9.93151216199994,15.2,-5.60014811000002));
#180493=CARTESIAN_POINT('Ctrl Pts',(9.93151216199994,11.6,-5.60014811000002));
#180494=CARTESIAN_POINT('Ctrl Pts',(9.93519705899994,15.2,-5.60043387200002));
#180495=CARTESIAN_POINT('Ctrl Pts',(9.93519705899994,11.6,-5.60043387200002));
#180496=CARTESIAN_POINT('Ctrl Pts',(9.93888668299994,15.2,-5.60071715300001));
#180497=CARTESIAN_POINT('Ctrl Pts',(9.93888668299994,11.6,-5.60071715300001));
#180498=CARTESIAN_POINT('Ctrl Pts',(9.94258102699994,15.2,-5.60099794600001));
#180499=CARTESIAN_POINT('Ctrl Pts',(9.94258102699994,11.6,-5.60099794600001));
#180500=CARTESIAN_POINT('Ctrl Pts',(9.94628008499994,15.2,-5.60127624400002));
#180501=CARTESIAN_POINT('Ctrl Pts',(9.94628008499994,11.6,-5.60127624400002));
#180502=CARTESIAN_POINT('Ctrl Pts',(9.94998384799995,15.2,-5.60155204300001));
#180503=CARTESIAN_POINT('Ctrl Pts',(9.94998384799995,11.6,-5.60155204300001));
#180504=CARTESIAN_POINT('Ctrl Pts',(9.95369231099994,15.2,-5.60182533700001));
#180505=CARTESIAN_POINT('Ctrl Pts',(9.95369231099994,11.6,-5.60182533700001));
#180506=CARTESIAN_POINT('Ctrl Pts',(9.95740546699994,15.2,-5.60209611600001));
#180507=CARTESIAN_POINT('Ctrl Pts',(9.95740546699994,11.6,-5.60209611600001));
#180508=CARTESIAN_POINT('Ctrl Pts',(9.96112330899994,15.2,-5.60236437800001));
#180509=CARTESIAN_POINT('Ctrl Pts',(9.96112330899994,11.6,-5.60236437800001));
#180510=CARTESIAN_POINT('Ctrl Pts',(9.96484582999994,15.2,-5.60263011400002));
#180511=CARTESIAN_POINT('Ctrl Pts',(9.96484582999994,11.6,-5.60263011400002));
#180512=CARTESIAN_POINT('Ctrl Pts',(9.96857302299994,15.2,-5.60289331700002));
#180513=CARTESIAN_POINT('Ctrl Pts',(9.96857302299994,11.6,-5.60289331700002));
#180514=CARTESIAN_POINT('Ctrl Pts',(9.97230487899994,15.2,-5.60315398300002));
#180515=CARTESIAN_POINT('Ctrl Pts',(9.97230487899994,11.6,-5.60315398300002));
#180516=CARTESIAN_POINT('Ctrl Pts',(9.97604139599994,15.2,-5.60341210500001));
#180517=CARTESIAN_POINT('Ctrl Pts',(9.97604139599994,11.6,-5.60341210500001));
#180518=CARTESIAN_POINT('Ctrl Pts',(9.97978256299995,15.2,-5.60366767600001));
#180519=CARTESIAN_POINT('Ctrl Pts',(9.97978256299995,11.6,-5.60366767600001));
#180520=CARTESIAN_POINT('Ctrl Pts',(9.98352837599995,15.2,-5.60392069300002));
#180521=CARTESIAN_POINT('Ctrl Pts',(9.98352837599995,11.6,-5.60392069300002));
#180522=CARTESIAN_POINT('Ctrl Pts',(9.98727882999994,15.2,-5.60417114700002));
#180523=CARTESIAN_POINT('Ctrl Pts',(9.98727882999994,11.6,-5.60417114700002));
#180524=CARTESIAN_POINT('Ctrl Pts',(9.99103391599995,15.2,-5.60441903700001));
#180525=CARTESIAN_POINT('Ctrl Pts',(9.99103391599995,11.6,-5.60441903700001));
#180526=CARTESIAN_POINT('Ctrl Pts',(9.99479362999995,15.2,-5.60466435300001));
#180527=CARTESIAN_POINT('Ctrl Pts',(9.99479362999995,11.6,-5.60466435300001));
#180528=CARTESIAN_POINT('Ctrl Pts',(9.99855796499994,15.2,-5.60490709200002));
#180529=CARTESIAN_POINT('Ctrl Pts',(9.99855796499994,11.6,-5.60490709200002));
#180530=CARTESIAN_POINT('Ctrl Pts',(10.0023269109999,15.2,-5.60514724400001));
#180531=CARTESIAN_POINT('Ctrl Pts',(10.0023269109999,11.6,-5.60514724400001));
#180532=CARTESIAN_POINT('Ctrl Pts',(10.0061004619999,15.2,-5.60538480400002));
#180533=CARTESIAN_POINT('Ctrl Pts',(10.0061004619999,11.6,-5.60538480400002));
#180534=CARTESIAN_POINT('Ctrl Pts',(10.0098786099999,15.2,-5.60561976300002));
#180535=CARTESIAN_POINT('Ctrl Pts',(10.0098786099999,11.6,-5.60561976300002));
#180536=CARTESIAN_POINT('Ctrl Pts',(10.0136613449999,15.2,-5.60585211500001));
#180537=CARTESIAN_POINT('Ctrl Pts',(10.0136613449999,11.6,-5.60585211500001));
#180538=CARTESIAN_POINT('Ctrl Pts',(10.0174486609999,15.2,-5.60608185200001));
#180539=CARTESIAN_POINT('Ctrl Pts',(10.0174486609999,11.6,-5.60608185200001));
#180540=CARTESIAN_POINT('Ctrl Pts',(10.0212405509999,15.2,-5.60630897000001));
#180541=CARTESIAN_POINT('Ctrl Pts',(10.0212405509999,11.6,-5.60630897000001));
#180542=CARTESIAN_POINT('Ctrl Pts',(10.0250370109999,15.2,-5.60653346400001));
#180543=CARTESIAN_POINT('Ctrl Pts',(10.0250370109999,11.6,-5.60653346400001));
#180544=CARTESIAN_POINT('Ctrl Pts',(10.0288380379999,15.2,-5.60675533200001));
#180545=CARTESIAN_POINT('Ctrl Pts',(10.0288380379999,11.6,-5.60675533200001));
#180546=CARTESIAN_POINT('Ctrl Pts',(10.0326436309999,15.2,-5.60697457300002));
#180547=CARTESIAN_POINT('Ctrl Pts',(10.0326436309999,11.6,-5.60697457300002));
#180548=CARTESIAN_POINT('Ctrl Pts',(10.0356917559999,15.2,-5.60714786300001));
#180549=CARTESIAN_POINT('Ctrl Pts',(10.0356917559999,11.6,-5.60714786300001));
#180550=CARTESIAN_POINT('Ctrl Pts',(10.0379799039999,15.2,-5.60727664700002));
#180551=CARTESIAN_POINT('Ctrl Pts',(10.0379799039999,11.6,-5.60727664700002));
#180552=CARTESIAN_POINT('Ctrl Pts',(10.0395062489999,15.2,-5.60736197900002));
#180553=CARTESIAN_POINT('Ctrl Pts',(10.0395062489999,11.6,-5.60736197900002));
#180554=CARTESIAN_POINT('Ctrl Pts',(10.0402696489999,15.2,-5.60740451200001));
#180555=CARTESIAN_POINT('Ctrl Pts',(10.0402696489999,11.6,-5.60740451200001));
#180556=CARTESIAN_POINT('Ctrl Pts',(8.88241603299995,15.2,-5.36127880600001));
#180557=CARTESIAN_POINT('Ctrl Pts',(8.88401933304833,15.2,-5.36206719629503));
#180558=CARTESIAN_POINT('Ctrl Pts',(8.88567630917062,15.2,-5.36287598656166));
#180559=CARTESIAN_POINT('Ctrl Pts',(8.8873863638459,15.2,-5.36370417391761));
#180560=CARTESIAN_POINT('Ctrl Pts',(8.88910466526922,15.2,-5.36453635521162));
#180561=CARTESIAN_POINT('Ctrl Pts',(8.89087656280783,15.2,-5.36538812047558));
#180562=CARTESIAN_POINT('Ctrl Pts',(8.89270147741819,15.2,-5.36625848006756));
#180563=CARTESIAN_POINT('Ctrl Pts',(8.89452639186279,15.2,-5.3671288395805));
#180564=CARTESIAN_POINT('Ctrl Pts',(8.89640432496164,15.2,-5.36801779213292));
#180565=CARTESIAN_POINT('Ctrl Pts',(8.89833471330818,15.2,-5.36892438076665));
#180566=CARTESIAN_POINT('Ctrl Pts',(8.90026510165471,15.2,-5.36983096940038));
#180567=CARTESIAN_POINT('Ctrl Pts',(8.90224794607846,15.1999999999999,-5.37075519313048));
#180568=CARTESIAN_POINT('Ctrl Pts',(8.90428269376981,15.2,-5.37169612014234));
#180569=CARTESIAN_POINT('Ctrl Pts',(8.90631744164601,15.2,-5.37263704723965));
#180570=CARTESIAN_POINT('Ctrl Pts',(8.90840409644624,15.2,-5.37359467979364));
#180571=CARTESIAN_POINT('Ctrl Pts',(8.91054211906624,15.2,-5.37456811359776));
#180572=CARTESIAN_POINT('Ctrl Pts',(8.91268014149207,15.2,-5.37554154731347));
#180573=CARTESIAN_POINT('Ctrl Pts',(8.91486953043031,15.2,-5.37653078087401));
#180574=CARTESIAN_POINT('Ctrl Pts',(8.91710976394254,15.2,-5.37753493975878));
#180575=CARTESIAN_POINT('Ctrl Pts',(8.91934999745478,15.2,-5.37853909864355));
#180576=CARTESIAN_POINT('Ctrl Pts',(8.92164107324306,15.2,-5.37955818039023));
#180577=CARTESIAN_POINT('Ctrl Pts',(8.92398247965579,15.2,-5.38059133443541));
#180578=CARTESIAN_POINT('Ctrl Pts',(8.9263238862812,15.2,-5.38162448857445));
#180579=CARTESIAN_POINT('Ctrl Pts',(8.92871562078788,15.2,-5.38267171456523));
#180580=CARTESIAN_POINT('Ctrl Pts',(8.93115718350766,15.2,-5.38373218387392));
#180581=CARTESIAN_POINT('Ctrl Pts',(8.93359874600567,15.2,-5.38479265308629));
#180582=CARTESIAN_POINT('Ctrl Pts',(8.93609013491204,15.2,-5.38586636586483));
#180583=CARTESIAN_POINT('Ctrl Pts',(8.9386308586552,15.2,-5.3869525153259));
#180584=CARTESIAN_POINT('Ctrl Pts',(8.94117158239835,15.2,-5.38803866478697));
#180585=CARTESIAN_POINT('Ctrl Pts',(8.94376164092926,15.2,-5.38913725330539));
#180586=CARTESIAN_POINT('Ctrl Pts',(8.94640055158124,15.2,-5.3902474946812));
#180587=CARTESIAN_POINT('Ctrl Pts',(8.94903946223323,15.2,-5.39135773605702));
#180588=CARTESIAN_POINT('Ctrl Pts',(8.95172722686268,15.2,-5.39247963096843));
#180589=CARTESIAN_POINT('Ctrl Pts',(8.95446336867663,15.2,-5.39361241742653));
#180590=CARTESIAN_POINT('Ctrl Pts',(8.95719951073912,15.2,-5.39474520398751));
#180591=CARTESIAN_POINT('Ctrl Pts',(8.95998403506464,15.2,-5.39588888035792));
#180592=CARTESIAN_POINT('Ctrl Pts',(8.9628164732211,15.2,-5.39704270583792));
#180593=CARTESIAN_POINT('Ctrl Pts',(8.96564891112028,15.2,-5.39819653121312));
#180594=CARTESIAN_POINT('Ctrl Pts',(8.96852926582505,15.2,-5.39936050395345));
#180595=CARTESIAN_POINT('Ctrl Pts',(8.97145708073187,15.2,-5.40053389974947));
#180596=CARTESIAN_POINT('Ctrl Pts',(8.97438489563868,15.2,-5.40170729554548));
#180597=CARTESIAN_POINT('Ctrl Pts',(8.97736017116679,15.2,-5.402890118114));
#180598=CARTESIAN_POINT('Ctrl Pts',(8.98038246188711,15.2,-5.40408165690346));
#180599=CARTESIAN_POINT('Ctrl Pts',(8.98340475288196,15.2,-5.40527319580113));
#180600=CARTESIAN_POINT('Ctrl Pts',(8.98647405673137,15.2,-5.40647345299135));
#180601=CARTESIAN_POINT('Ctrl Pts',(8.98958993590321,15.2,-5.40768174280755));
#180602=CARTESIAN_POINT('Ctrl Pts',(8.99270581479201,15.2,-5.408890032514));
#180603=CARTESIAN_POINT('Ctrl Pts',(8.99586827068388,15.2,-5.41010635178838));
#180604=CARTESIAN_POINT('Ctrl Pts',(8.99907686774841,15.2,-5.41133003174945));
#180605=CARTESIAN_POINT('Ctrl Pts',(9.00228546481295,15.2,-5.41255371171051));
#180606=CARTESIAN_POINT('Ctrl Pts',(9.00554020763815,15.2,-5.41378475248552));
#180607=CARTESIAN_POINT('Ctrl Pts',(9.00884067043179,15.2,-5.41502249935676));
#180608=CARTESIAN_POINT('Ctrl Pts',(9.01214113352523,15.2,-5.41626024634042));
#180609=CARTESIAN_POINT('Ctrl Pts',(9.0154873156295,15.2,-5.41750469859));
#180610=CARTESIAN_POINT('Ctrl Pts',(9.01887880106973,15.2,-5.41875521888766));
#180611=CARTESIAN_POINT('Ctrl Pts',(9.0222702862019,15.2,-5.42000573907171));
#180612=CARTESIAN_POINT('Ctrl Pts',(9.02570707445971,15.2,-5.4212623260792));
#180613=CARTESIAN_POINT('Ctrl Pts',(9.02918875449986,15.2,-5.4225243582));
#180614=CARTESIAN_POINT('Ctrl Pts',(9.03325071475754,15.2,-5.42399672908404));
#180615=CARTESIAN_POINT('Ctrl Pts',(9.03737378010303,15.2,-5.42547650832552));
#180616=CARTESIAN_POINT('Ctrl Pts',(9.04155730733853,15.2,-5.42696273238159));
#180617=CARTESIAN_POINT('Ctrl Pts',(9.04514318763997,15.2,-5.42823663864923));
#180618=CARTESIAN_POINT('Ctrl Pts',(9.04877348980836,15.2,-5.42951528044662));
#180619=CARTESIAN_POINT('Ctrl Pts',(9.05244781792486,15.2,-5.43079806473334));
#180620=CARTESIAN_POINT('Ctrl Pts',(9.05612214604136,15.2,-5.43208084902007));
#180621=CARTESIAN_POINT('Ctrl Pts',(9.05984049788733,15.2,-5.43336777604114));
#180622=CARTESIAN_POINT('Ctrl Pts',(9.06360248610272,15.2,-5.43465826739185));
#180623=CARTESIAN_POINT('Ctrl Pts',(9.06736447465983,15.2,-5.43594875885977));
#180624=CARTESIAN_POINT('Ctrl Pts',(9.07117009649003,15.2,-5.43724281378716));
#180625=CARTESIAN_POINT('Ctrl Pts',(9.07501896886941,15.2,-5.43853986635806));
#180626=CARTESIAN_POINT('Ctrl Pts',(9.07822636234408,15.2,-5.43962074344155));
#180627=CARTESIAN_POINT('Ctrl Pts',(9.08146378863036,15.2,-5.4407037035473));
#180628=CARTESIAN_POINT('Ctrl Pts',(9.08473103120224,15.2,-5.44178842465856));
#180629=CARTESIAN_POINT('Ctrl Pts',(9.08799827341799,15.2,-5.44287314565157));
#180630=CARTESIAN_POINT('Ctrl Pts',(9.0912953289909,15.2,-5.44395962754308));
#180631=CARTESIAN_POINT('Ctrl Pts',(9.09462198209809,15.2,-5.44504755617438));
#180632=CARTESIAN_POINT('Ctrl Pts',(9.09794863556789,15.2,-5.44613548492426));
#180633=CARTESIAN_POINT('Ctrl Pts',(9.10130488505945,15.2,-5.44722485903524));
#180634=CARTESIAN_POINT('Ctrl Pts',(9.10469051776537,15.2,-5.44831537188237));
#180635=CARTESIAN_POINT('Ctrl Pts',(9.10807615047132,15.2,-5.44940588472951));
#180636=CARTESIAN_POINT('Ctrl Pts',(9.11149116437456,15.2,-5.45049753292978));
#180637=CARTESIAN_POINT('Ctrl Pts',(9.11493534885015,15.2,-5.45159001666486));
#180638=CARTESIAN_POINT('Ctrl Pts',(9.11837953332575,15.2,-5.45268250039993));
#180639=CARTESIAN_POINT('Ctrl Pts',(9.12185288672808,15.2,-5.45377581602851));
#180640=CARTESIAN_POINT('Ctrl Pts',(9.12535519950433,15.2,-5.45486966894515));
#180641=CARTESIAN_POINT('Ctrl Pts',(9.12955797506489,15.2,-5.45618229251665));
#180642=CARTESIAN_POINT('Ctrl Pts',(9.13380245172231,15.2,-5.45749568616325));
#180643=CARTESIAN_POINT('Ctrl Pts',(9.1380882712087,15.2,-5.45880934415154));
#180644=CARTESIAN_POINT('Ctrl Pts',(9.14165978686342,15.2,-5.45990405896278));
#180645=CARTESIAN_POINT('Ctrl Pts',(9.14526001213977,15.2,-5.46099896027614));
#180646=CARTESIAN_POINT('Ctrl Pts',(9.14888874278358,15.2,-5.46209375828182));
#180647=CARTESIAN_POINT('Ctrl Pts',(9.15251747382291,15.2,-5.46318855640682));
#180648=CARTESIAN_POINT('Ctrl Pts',(9.15617470851458,15.2,-5.46428325247907));
#180649=CARTESIAN_POINT('Ctrl Pts',(9.15986024552615,15.2,-5.46537756463188));
#180650=CARTESIAN_POINT('Ctrl Pts',(9.16428289018106,15.2,-5.46669073928682));
#180651=CARTESIAN_POINT('Ctrl Pts',(9.16874628845453,15.2,-5.46800336017328));
#180652=CARTESIAN_POINT('Ctrl Pts',(9.17325009417733,15.2,-5.46931495014356));
#180653=CARTESIAN_POINT('Ctrl Pts',(9.17700326540845,15.2,-5.47040794172589));
#180654=CARTESIAN_POINT('Ctrl Pts',(9.1807844959125,15.2,-5.47150021725395));
#180655=CARTESIAN_POINT('Ctrl Pts',(9.18459358945645,15.2,-5.47259150635109));
#180656=CARTESIAN_POINT('Ctrl Pts',(9.18840268300039,15.2,-5.47368279544823));
#180657=CARTESIAN_POINT('Ctrl Pts',(9.19223963591422,15.2,-5.47477309693146));
#180658=CARTESIAN_POINT('Ctrl Pts',(9.19610425605537,15.2,-5.4758621451258));
#180659=CARTESIAN_POINT('Ctrl Pts',(9.19996887619653,15.2,-5.47695119332015));
#180660=CARTESIAN_POINT('Ctrl Pts',(9.2038611591659,15.2,-5.47803898787556));
#180661=CARTESIAN_POINT('Ctrl Pts',(9.20778091298759,15.2,-5.47912526537544));
#180662=CARTESIAN_POINT('Ctrl Pts',(9.21170066638203,15.2,-5.48021154275691));
#180663=CARTESIAN_POINT('Ctrl Pts',(9.21564789101545,15.2,-5.48129630520959));
#180664=CARTESIAN_POINT('Ctrl Pts',(9.21962239099669,15.2,-5.4823792925917));
#180665=CARTESIAN_POINT('Ctrl Pts',(9.22359689141114,15.2,-5.48346228009185));
#180666=CARTESIAN_POINT('Ctrl Pts',(9.22759866835845,15.2,-5.48454349366425));
#180667=CARTESIAN_POINT('Ctrl Pts',(9.23162753127291,15.2,-5.4856226795672));
#180668=CARTESIAN_POINT('Ctrl Pts',(9.23485062178014,15.2,-5.48648602833661));
#180669=CARTESIAN_POINT('Ctrl Pts',(9.23809104670969,15.2,-5.4873480793748));
#180670=CARTESIAN_POINT('Ctrl Pts',(9.24134870923543,15.2,-5.48820870525894));
#180671=CARTESIAN_POINT('Ctrl Pts',(9.24460637131731,15.2,-5.48906933102582));
#180672=CARTESIAN_POINT('Ctrl Pts',(9.24788127249917,15.2,-5.48992852997974));
#180673=CARTESIAN_POINT('Ctrl Pts',(9.25117331322831,15.2,-5.4907861779098));
#180674=CARTESIAN_POINT('Ctrl Pts',(9.25446535440599,15.2,-5.4916438259567));
#180675=CARTESIAN_POINT('Ctrl Pts',(9.25777453593526,15.2,-5.49249992043401));
#180676=CARTESIAN_POINT('Ctrl Pts',(9.2611007637832,15.2,-5.49335433975835));
#180677=CARTESIAN_POINT('Ctrl Pts',(9.26442699163114,15.2,-5.4942087590827));
#180678=CARTESIAN_POINT('Ctrl Pts',(9.26777026387831,15.2,-5.49506150118462));
#180679=CARTESIAN_POINT('Ctrl Pts',(9.27113048700762,15.2,-5.49591244339748));
#180680=CARTESIAN_POINT('Ctrl Pts',(9.2744907096791,15.2,-5.49676338549441));
#180681=CARTESIAN_POINT('Ctrl Pts',(9.2778678838319,15.2,-5.49761252866762));
#180682=CARTESIAN_POINT('Ctrl Pts',(9.28126191201423,15.2,-5.49845974999111));
#180683=CARTESIAN_POINT('Ctrl Pts',(9.28465594065901,15.2,-5.49930697143003));
#180684=CARTESIAN_POINT('Ctrl Pts',(9.28806682546901,15.2,-5.50015227132826));
#180685=CARTESIAN_POINT('Ctrl Pts',(9.29149447260197,15.2,-5.50099553009623));
#180686=CARTESIAN_POINT('Ctrl Pts',(9.29577903128468,15.2,-5.50204960349875));
#180687=CARTESIAN_POINT('Ctrl Pts',(9.30008977898167,15.2,-5.50310048678731));
#180688=CARTESIAN_POINT('Ctrl Pts',(9.30442653606713,15.2,-5.50414795012036));
#180689=CARTESIAN_POINT('Ctrl Pts',(9.30789594145187,15.2,-5.5049859207183));
#180690=CARTESIAN_POINT('Ctrl Pts',(9.31138199191798,15.2,-5.50582170266102));
#180691=CARTESIAN_POINT('Ctrl Pts',(9.31488459598083,15.2,-5.50665517754112));
#180692=CARTESIAN_POINT('Ctrl Pts',(9.31838720052091,15.2,-5.50748865253479));
#180693=CARTESIAN_POINT('Ctrl Pts',(9.32190635823638,15.2,-5.50831982309616));
#180694=CARTESIAN_POINT('Ctrl Pts',(9.32544197681963,15.2,-5.50914857191886));
#180695=CARTESIAN_POINT('Ctrl Pts',(9.32986149980783,15.2,-5.51018450789076));
#180696=CARTESIAN_POINT('Ctrl Pts',(9.33430674252704,15.2,-5.51121666056817));
#180697=CARTESIAN_POINT('Ctrl Pts',(9.338777529543,15.2,-5.5122448091095));
#180698=CARTESIAN_POINT('Ctrl Pts',(9.34235415886339,15.2,-5.51306732787533));
#180699=CARTESIAN_POINT('Ctrl Pts',(9.34594713505947,15.2,-5.5138872839209));
#180700=CARTESIAN_POINT('Ctrl Pts',(9.34955636778076,15.2,-5.51470456469113));
#180701=CARTESIAN_POINT('Ctrl Pts',(9.35316560099381,15.2,-5.51552184557273));
#180702=CARTESIAN_POINT('Ctrl Pts',(9.35679109012851,15.2,-5.51633645184991));
#180703=CARTESIAN_POINT('Ctrl Pts',(9.36043274732863,15.2,-5.51714827211609));
#180704=CARTESIAN_POINT('Ctrl Pts',(9.36498481858069,15.2,-5.51816304739351));
#180705=CARTESIAN_POINT('Ctrl Pts',(9.3695621489165,15.2,-5.51917347065419));
#180706=CARTESIAN_POINT('Ctrl Pts',(9.37416456683522,15.2,-5.52017932759826));
#180707=CARTESIAN_POINT('Ctrl Pts',(9.37784650086919,15.2,-5.52098401308774));
#180708=CARTESIAN_POINT('Ctrl Pts',(9.38154448838416,15.2,-5.52178577728337));
#180709=CARTESIAN_POINT('Ctrl Pts',(9.38525844376402,15.2,-5.52258451199948));
#180710=CARTESIAN_POINT('Ctrl Pts',(9.38897239964991,15.2,-5.52338324682443));
#180711=CARTESIAN_POINT('Ctrl Pts',(9.39270232140934,15.2,-5.52417895098118));
#180712=CARTESIAN_POINT('Ctrl Pts',(9.39644812133733,15.2,-5.52497151991294));
#180713=CARTESIAN_POINT('Ctrl Pts',(9.40113037099213,15.2,-5.52596223102365));
#180714=CARTESIAN_POINT('Ctrl Pts',(9.40583742996678,15.2,-5.52694804220095));
#180715=CARTESIAN_POINT('Ctrl Pts',(9.41056912788546,15.2,-5.52792874831163));
#180716=CARTESIAN_POINT('Ctrl Pts',(9.41435448591096,15.2,-5.52871331313605));
#180717=CARTESIAN_POINT('Ctrl Pts',(9.41815561213925,15.2,-5.52949461033455));
#180718=CARTESIAN_POINT('Ctrl Pts',(9.42197242078895,15.2,-5.5302725377745));
#180719=CARTESIAN_POINT('Ctrl Pts',(9.4267434319911,15.2,-5.53124494715393));
#180720=CARTESIAN_POINT('Ctrl Pts',(9.43153894431655,15.2,-5.53221208804447));
#180721=CARTESIAN_POINT('Ctrl Pts',(9.43635879077488,15.2,-5.53317376422503));
#180722=CARTESIAN_POINT('Ctrl Pts',(9.44021466815169,15.2,-5.53394310521141));
#180723=CARTESIAN_POINT('Ctrl Pts',(9.44408611842199,15.2,-5.53470894760014));
#180724=CARTESIAN_POINT('Ctrl Pts',(9.44797305696874,15.2,-5.53547119064132));
#180725=CARTESIAN_POINT('Ctrl Pts',(9.4518599949859,15.2,-5.53623343357864));
#180726=CARTESIAN_POINT('Ctrl Pts',(9.45576241973865,15.2,-5.53699207792168));
#180727=CARTESIAN_POINT('Ctrl Pts',(9.45968024721388,15.2,-5.53774702347451));
#180728=CARTESIAN_POINT('Ctrl Pts',(9.46359807522292,15.2,-5.53850196913021));
#180729=CARTESIAN_POINT('Ctrl Pts',(9.46753130493149,15.2,-5.53925321547911));
#180730=CARTESIAN_POINT('Ctrl Pts',(9.47147985220381,15.2,-5.54000066513057));
#180731=CARTESIAN_POINT('Ctrl Pts',(9.4774026725743,15.2,-5.54112183950591));
#180732=CARTESIAN_POINT('Ctrl Pts',(9.48335995373423,15.2,-5.54223447002347));
#180733=CARTESIAN_POINT('Ctrl Pts',(9.48935141601654,15.2,-5.54333822848336));
#180734=CARTESIAN_POINT('Ctrl Pts',(9.49334572456758,15.2,-5.54407406752347));
#180735=CARTESIAN_POINT('Ctrl Pts',(9.49735522241203,15.2,-5.54480596401311));
#180736=CARTESIAN_POINT('Ctrl Pts',(9.50137982713292,15.2,-5.5455338223857));
#180737=CARTESIAN_POINT('Ctrl Pts',(9.50540443130545,15.2,-5.54626168065912));
#180738=CARTESIAN_POINT('Ctrl Pts',(9.50944414219635,15.2,-5.54698550034398));
#180739=CARTESIAN_POINT('Ctrl Pts',(9.51349887627213,15.2,-5.54770518673287));
#180740=CARTESIAN_POINT('Ctrl Pts',(9.51755361090036,15.2,-5.54842487321982));
#180741=CARTESIAN_POINT('Ctrl Pts',(9.52162336779638,15.2,-5.54914042722522));
#180742=CARTESIAN_POINT('Ctrl Pts',(9.52570806640941,15.2,-5.54985175487466));
#180743=CARTESIAN_POINT('Ctrl Pts',(9.5297927644659,15.2,-5.55056308242719));
#180744=CARTESIAN_POINT('Ctrl Pts',(9.53389240050378,15.2,-5.55127018323859));
#180745=CARTESIAN_POINT('Ctrl Pts',(9.53800689588867,15.2,-5.5519729649592));
#180746=CARTESIAN_POINT('Ctrl Pts',(9.54212139183417,15.2,-5.55267574677557));
#180747=CARTESIAN_POINT('Ctrl Pts',(9.54625074530604,15.2,-5.55337421026472));
#180748=CARTESIAN_POINT('Ctrl Pts',(9.55039487418464,15.2,-5.55406826339239));
#180749=CARTESIAN_POINT('Ctrl Pts',(9.55453900249861,15.2,-5.5547623164255));
#180750=CARTESIAN_POINT('Ctrl Pts',(9.5586979055121,15.2,-5.55545195923859));
#180751=CARTESIAN_POINT('Ctrl Pts',(9.56287150239217,15.2,-5.55613710096065));
#180752=CARTESIAN_POINT('Ctrl Pts',(9.56704509984088,15.2,-5.55682224277606));
#180753=CARTESIAN_POINT('Ctrl Pts',(9.57123339133027,15.2,-5.55750288558815));
#180754=CARTESIAN_POINT('Ctrl Pts',(9.57543629589361,15.2,-5.55817893734692));
#180755=CARTESIAN_POINT('Ctrl Pts',(9.57963919988431,15.2,-5.55885498901358));
#180756=CARTESIAN_POINT('Ctrl Pts',(9.58385671533278,15.2,-5.55952645007404));
#180757=CARTESIAN_POINT('Ctrl Pts',(9.58808876241921,15.2,-5.56019323438658));
#180758=CARTESIAN_POINT('Ctrl Pts',(9.59232081008225,15.2,-5.56086001878998));
#180759=CARTESIAN_POINT('Ctrl Pts',(9.59656738975964,15.2,-5.56152212365432));
#180760=CARTESIAN_POINT('Ctrl Pts',(9.6008284198817,15.2,-5.56217946407872));
#180761=CARTESIAN_POINT('Ctrl Pts',(9.6050894494232,15.2,-5.56283680441356));
#180762=CARTESIAN_POINT('Ctrl Pts',(9.6093649313979,15.2,-5.56348937873547));
#180763=CARTESIAN_POINT('Ctrl Pts',(9.6136547823235,15.2,-5.56413710112746));
#180764=CARTESIAN_POINT('Ctrl Pts',(9.61794463383362,15.2,-5.56478482360771));
#180765=CARTESIAN_POINT('Ctrl Pts',(9.62224885688947,15.2,-5.56542769424893));
#180766=CARTESIAN_POINT('Ctrl Pts',(9.62656737097783,15.2,-5.5660656280088));
#180767=CARTESIAN_POINT('Ctrl Pts',(9.6308858844778,15.2,-5.56670356168176));
#180768=CARTESIAN_POINT('Ctrl Pts',(9.63521868957375,15.2,-5.56733655730374));
#180769=CARTESIAN_POINT('Ctrl Pts',(9.63956570577249,15.2,-5.56796453169736));
#180770=CARTESIAN_POINT('Ctrl Pts',(9.6439127225635,15.2,-5.56859250617654));
#180771=CARTESIAN_POINT('Ctrl Pts',(9.64827395159198,15.2,-5.56921545790525));
#180772=CARTESIAN_POINT('Ctrl Pts',(9.65264931244155,15.2,-5.56983330505004));
#180773=CARTESIAN_POINT('Ctrl Pts',(9.65702467329112,15.2,-5.57045115219482));
#180774=CARTESIAN_POINT('Ctrl Pts',(9.661414168709,15.2,-5.57106389414457));
#180775=CARTESIAN_POINT('Ctrl Pts',(9.66581771622821,15.2,-5.57167144739937));
#180776=CARTESIAN_POINT('Ctrl Pts',(9.66912037656762,15.2,-5.57212711229908));
#180777=CARTESIAN_POINT('Ctrl Pts',(9.67243094294588,15.2,-5.57257985988124));
#180778=CARTESIAN_POINT('Ctrl Pts',(9.675749381867,15.2,-5.57302965384536));
#180779=CARTESIAN_POINT('Ctrl Pts',(9.67906782078813,15.2,-5.57347944780948));
#180780=CARTESIAN_POINT('Ctrl Pts',(9.68239413161724,15.2,-5.57392628914808));
#180781=CARTESIAN_POINT('Ctrl Pts',(9.68572828187178,15.2,-5.5743701435067));
#180782=CARTESIAN_POINT('Ctrl Pts',(9.68906243212632,15.2,-5.57481399786531));
#180783=CARTESIAN_POINT('Ctrl Pts',(9.69240442175493,15.2,-5.57525486463261));
#180784=CARTESIAN_POINT('Ctrl Pts',(9.69575421800822,15.2,-5.57569271095004));
#180785=CARTESIAN_POINT('Ctrl Pts',(9.7002206134183,15.2,-5.57627650609296));
#180786=CARTESIAN_POINT('Ctrl Pts',(9.70470088708556,15.2,-5.57685493062416));
#180787=CARTESIAN_POINT('Ctrl Pts',(9.70919496194301,15.2,-5.57742790454371));
#180788=CARTESIAN_POINT('Ctrl Pts',(9.71256551777994,15.2,-5.57785763494435));
#180789=CARTESIAN_POINT('Ctrl Pts',(9.71594383767472,15.2,-5.57828429964321));
#180790=CARTESIAN_POINT('Ctrl Pts',(9.71932988713841,15.2,-5.57870786502362));
#180791=CARTESIAN_POINT('Ctrl Pts',(9.72271593660211,15.2,-5.57913143040403));
#180792=CARTESIAN_POINT('Ctrl Pts',(9.7261097158437,15.2,-5.57955189641091));
#180793=CARTESIAN_POINT('Ctrl Pts',(9.72951119359578,15.2,-5.57996923027047));
#180794=CARTESIAN_POINT('Ctrl Pts',(9.73291267134787,15.2,-5.58038656413004));
#180795=CARTESIAN_POINT('Ctrl Pts',(9.73632184690737,15.2,-5.58080076609831));
#180796=CARTESIAN_POINT('Ctrl Pts',(9.73973868774155,15.2,-5.58121180250004));
#180797=CARTESIAN_POINT('Ctrl Pts',(9.74315552857575,15.2,-5.58162283890177));
#180798=CARTESIAN_POINT('Ctrl Pts',(9.74658003556795,15.2,-5.5820307103203));
#180799=CARTESIAN_POINT('Ctrl Pts',(9.75001217631758,15.2,-5.58243538418087));
#180800=CARTESIAN_POINT('Ctrl Pts',(9.75344431706722,15.2,-5.58284005804145));
#180801=CARTESIAN_POINT('Ctrl Pts',(9.75688409058689,15.2,-5.58324153383382));
#180802=CARTESIAN_POINT('Ctrl Pts',(9.76033146554965,15.2,-5.58363978067296));
#180803=CARTESIAN_POINT('Ctrl Pts',(9.76377884051241,15.2,-5.58403802751209));
#180804=CARTESIAN_POINT('Ctrl Pts',(9.76723381713857,15.2,-5.58443304364509));
#180805=CARTESIAN_POINT('Ctrl Pts',(9.77069636197007,15.2,-5.5848247976313));
#180806=CARTESIAN_POINT('Ctrl Pts',(9.77415890743059,15.2,-5.58521655168868));
#180807=CARTESIAN_POINT('Ctrl Pts',(9.77762902258492,15.2,-5.58560504584514));
#180808=CARTESIAN_POINT('Ctrl Pts',(9.78110667500803,15.2,-5.58599024485901));
#180809=CARTESIAN_POINT('Ctrl Pts',(9.78458432679936,15.2,-5.58637544380289));
#180810=CARTESIAN_POINT('Ctrl Pts',(9.78806951572364,15.2,-5.58675734865529));
#180811=CARTESIAN_POINT('Ctrl Pts',(9.79156220959739,15.2,-5.58713592901625));
#180812=CARTESIAN_POINT('Ctrl Pts',(9.79505490347114,15.2,-5.5875145093772));
#180813=CARTESIAN_POINT('Ctrl Pts',(9.79855510384789,15.2,-5.58788976411221));
#180814=CARTESIAN_POINT('Ctrl Pts',(9.80206277673642,15.2,-5.58826166251704));
#180815=CARTESIAN_POINT('Ctrl Pts',(9.80557044962494,15.2,-5.58863356092187));
#180816=CARTESIAN_POINT('Ctrl Pts',(9.80908559740872,15.2,-5.58900210284463));
#180817=CARTESIAN_POINT('Ctrl Pts',(9.81260818625503,15.2,-5.58936725770804));
#180818=CARTESIAN_POINT('Ctrl Pts',(9.81613077510134,15.2,-5.58973241257145));
#180819=CARTESIAN_POINT('Ctrl Pts',(9.81966080597694,15.2,-5.59009417912365));
#180820=CARTESIAN_POINT('Ctrl Pts',(9.82319824684777,15.2,-5.59045252844425));
#180821=CARTESIAN_POINT('Ctrl Pts',(9.8267356877186,15.2,-5.59081087776486));
#180822=CARTESIAN_POINT('Ctrl Pts',(9.83028054022225,15.2,-5.59116580878571));
#180823=CARTESIAN_POINT('Ctrl Pts',(9.83383277096718,15.2,-5.59151729073175));
#180824=CARTESIAN_POINT('Ctrl Pts',(9.83738500235744,15.2,-5.59186877274163));
#180825=CARTESIAN_POINT('Ctrl Pts',(9.8409446119581,15.2,-5.59221680625888));
#180826=CARTESIAN_POINT('Ctrl Pts',(9.8445115698525,15.2,-5.59256136030848));
#180827=CARTESIAN_POINT('Ctrl Pts',(9.8480785270989,15.2,-5.59290591429549));
#180828=CARTESIAN_POINT('Ctrl Pts',(9.85165283178658,15.2,-5.59324698964935));
#180829=CARTESIAN_POINT('Ctrl Pts',(9.85523445265708,15.2,-5.59358455605344));
#180830=CARTESIAN_POINT('Ctrl Pts',(9.85881607352759,15.2,-5.59392212245753));
#180831=CARTESIAN_POINT('Ctrl Pts',(9.86240501111746,15.2,-5.59425617926086));
#180832=CARTESIAN_POINT('Ctrl Pts',(9.8660012334615,15.2,-5.59458669725034));
#180833=CARTESIAN_POINT('Ctrl Pts',(9.86959745580553,15.2,-5.59491721523981));
#180834=CARTESIAN_POINT('Ctrl Pts',(9.87320096377811,15.2,-5.59524419529334));
#180835=CARTESIAN_POINT('Ctrl Pts',(9.87681172599662,15.2,-5.59556760624141));
#180836=CARTESIAN_POINT('Ctrl Pts',(9.88282966324612,15.2,-5.59610662450777));
#180837=CARTESIAN_POINT('Ctrl Pts',(9.88886774999433,15.2,-5.59663573003893));
#180838=CARTESIAN_POINT('Ctrl Pts',(9.89492584325822,15.2,-5.59715478823337));
#180839=CARTESIAN_POINT('Ctrl Pts',(9.89977231813347,15.2,-5.59757003481156));
#180840=CARTESIAN_POINT('Ctrl Pts',(9.90463159725743,15.2,-5.59797884940844));
#180841=CARTESIAN_POINT('Ctrl Pts',(9.90950360807981,15.2,-5.59838116604082));
#180842=CARTESIAN_POINT('Ctrl Pts',(9.91315761586468,15.2,-5.59868290348769));
#180843=CARTESIAN_POINT('Ctrl Pts',(9.91681878532555,15.2,-5.59898098530338));
#180844=CARTESIAN_POINT('Ctrl Pts',(9.92048708575136,15.2,-5.5992753822653));
#180845=CARTESIAN_POINT('Ctrl Pts',(9.92415538617716,15.2,-5.59956977922721));
#180846=CARTESIAN_POINT('Ctrl Pts',(9.92783081583459,15.2,-5.59986049160868));
#180847=CARTESIAN_POINT('Ctrl Pts',(9.93151334565974,15.2,-5.60014749105626));
#180848=CARTESIAN_POINT('Ctrl Pts',(9.93519587548489,15.2,-5.60043449050385));
#180849=CARTESIAN_POINT('Ctrl Pts',(9.93888550523421,15.2,-5.60071777724353));
#180850=CARTESIAN_POINT('Ctrl Pts',(9.94258220547489,15.2,-5.60099732227504));
#180851=CARTESIAN_POINT('Ctrl Pts',(9.94627890571557,15.2,-5.60127686730655));
#180852=CARTESIAN_POINT('Ctrl Pts',(9.94998267506431,15.2,-5.60155267229654));
#180853=CARTESIAN_POINT('Ctrl Pts',(9.95369348384554,15.2,-5.60182470828699));
#180854=CARTESIAN_POINT('Ctrl Pts',(9.95740429262676,15.2,-5.60209674427743));
#180855=CARTESIAN_POINT('Ctrl Pts',(9.96112214087936,15.2,-5.60236501167812));
#180856=CARTESIAN_POINT('Ctrl Pts',(9.96484699726263,15.2,-5.60262948072384));
#180857=CARTESIAN_POINT('Ctrl Pts',(9.96981347289146,15.2,-5.60298210615015));
#180858=CARTESIAN_POINT('Ctrl Pts',(9.97479240512689,15.2,-5.60332797945966));
#180859=CARTESIAN_POINT('Ctrl Pts',(9.97978372489972,15.2,-5.6036670374777));
#180860=CARTESIAN_POINT('Ctrl Pts',(9.98352721438932,15.2,-5.60392133096812));
#180861=CARTESIAN_POINT('Ctrl Pts',(9.98727767356974,15.2,-5.604171791109));
#180862=CARTESIAN_POINT('Ctrl Pts',(9.99103507297489,15.2,-5.60441839355838));
#180863=CARTESIAN_POINT('Ctrl Pts',(9.99604493930348,15.2,-5.60474719685407));
#180864=CARTESIAN_POINT('Ctrl Pts',(10.0010671467807,15.2,-5.60506914197675));
#180865=CARTESIAN_POINT('Ctrl Pts',(10.0061016120564,15.2,-5.60538415382655));
#180866=CARTESIAN_POINT('Ctrl Pts',(10.0098774606701,15.2,-5.60562041269244));
#180867=CARTESIAN_POINT('Ctrl Pts',(10.0136602026641,15.2,-5.60585277015821));
#180868=CARTESIAN_POINT('Ctrl Pts',(10.0174498052582,15.2,-5.60608119728586));
#180869=CARTESIAN_POINT('Ctrl Pts',(10.0212394078522,15.2,-5.60630962441352));
#180870=CARTESIAN_POINT('Ctrl Pts',(10.0250358702008,15.2,-5.60653412088277));
#180871=CARTESIAN_POINT('Ctrl Pts',(10.0288391798983,15.2,-5.60675467526975));
#180872=CARTESIAN_POINT('Ctrl Pts',(10.0326424895958,15.2,-5.60697522965674));
#180873=CARTESIAN_POINT('Ctrl Pts',(10.0364526483065,15.2,-5.60719184696139));
#180874=CARTESIAN_POINT('Ctrl Pts',(10.0402696489999,15.2,-5.60740451200001));
#180875=CARTESIAN_POINT('Ctrl Pts',(8.88241603299995,12.2,-5.36127880600001));
#180876=CARTESIAN_POINT('Ctrl Pts',(8.88401933304833,12.2,-5.36206719629503));
#180877=CARTESIAN_POINT('Ctrl Pts',(8.88567630917062,12.2,-5.36287598656166));
#180878=CARTESIAN_POINT('Ctrl Pts',(8.8873863638459,12.2,-5.36370417391761));
#180879=CARTESIAN_POINT('Ctrl Pts',(8.88910466526922,12.2,-5.36453635521162));
#180880=CARTESIAN_POINT('Ctrl Pts',(8.89087656280783,12.2,-5.36538812047557));
#180881=CARTESIAN_POINT('Ctrl Pts',(8.89270147741819,12.2,-5.36625848006756));
#180882=CARTESIAN_POINT('Ctrl Pts',(8.89452639186279,12.2,-5.3671288395805));
#180883=CARTESIAN_POINT('Ctrl Pts',(8.89640432496164,12.2,-5.36801779213292));
#180884=CARTESIAN_POINT('Ctrl Pts',(8.89833471330818,12.2,-5.36892438076665));
#180885=CARTESIAN_POINT('Ctrl Pts',(8.90026510165471,12.2,-5.36983096940038));
#180886=CARTESIAN_POINT('Ctrl Pts',(8.90224794607846,12.2,-5.37075519313048));
#180887=CARTESIAN_POINT('Ctrl Pts',(8.90428269376981,12.2,-5.37169612014234));
#180888=CARTESIAN_POINT('Ctrl Pts',(8.90631744164601,12.2,-5.37263704723965));
#180889=CARTESIAN_POINT('Ctrl Pts',(8.90840409644624,12.2,-5.37359467979364));
#180890=CARTESIAN_POINT('Ctrl Pts',(8.91054211906624,12.2,-5.37456811359776));
#180891=CARTESIAN_POINT('Ctrl Pts',(8.91268014149207,12.2,-5.37554154731347));
#180892=CARTESIAN_POINT('Ctrl Pts',(8.91486953043031,12.2,-5.37653078087401));
#180893=CARTESIAN_POINT('Ctrl Pts',(8.91710976394254,12.2,-5.37753493975878));
#180894=CARTESIAN_POINT('Ctrl Pts',(8.91934999745478,12.2,-5.37853909864355));
#180895=CARTESIAN_POINT('Ctrl Pts',(8.92164107324306,12.2,-5.37955818039023));
#180896=CARTESIAN_POINT('Ctrl Pts',(8.92398247965579,12.2,-5.38059133443541));
#180897=CARTESIAN_POINT('Ctrl Pts',(8.9263238862812,12.2,-5.38162448857445));
#180898=CARTESIAN_POINT('Ctrl Pts',(8.92871562078788,12.2,-5.38267171456523));
#180899=CARTESIAN_POINT('Ctrl Pts',(8.93115718350766,12.2,-5.38373218387392));
#180900=CARTESIAN_POINT('Ctrl Pts',(8.93359874600567,12.2,-5.38479265308629));
#180901=CARTESIAN_POINT('Ctrl Pts',(8.93609013491204,12.2,-5.38586636586483));
#180902=CARTESIAN_POINT('Ctrl Pts',(8.9386308586552,12.2,-5.3869525153259));
#180903=CARTESIAN_POINT('Ctrl Pts',(8.94117158239835,12.2,-5.38803866478697));
#180904=CARTESIAN_POINT('Ctrl Pts',(8.94376164092926,12.2,-5.38913725330539));
#180905=CARTESIAN_POINT('Ctrl Pts',(8.94640055158124,12.2,-5.3902474946812));
#180906=CARTESIAN_POINT('Ctrl Pts',(8.94903946223323,12.2,-5.39135773605702));
#180907=CARTESIAN_POINT('Ctrl Pts',(8.95172722686268,12.2,-5.39247963096843));
#180908=CARTESIAN_POINT('Ctrl Pts',(8.95446336867663,12.2,-5.39361241742653));
#180909=CARTESIAN_POINT('Ctrl Pts',(8.95719951073912,12.2,-5.39474520398751));
#180910=CARTESIAN_POINT('Ctrl Pts',(8.95998403506464,12.2,-5.39588888035792));
#180911=CARTESIAN_POINT('Ctrl Pts',(8.9628164732211,12.2,-5.39704270583792));
#180912=CARTESIAN_POINT('Ctrl Pts',(8.96564891112028,12.2,-5.39819653121312));
#180913=CARTESIAN_POINT('Ctrl Pts',(8.96852926582505,12.2,-5.39936050395345));
#180914=CARTESIAN_POINT('Ctrl Pts',(8.97145708073186,12.2,-5.40053389974946));
#180915=CARTESIAN_POINT('Ctrl Pts',(8.97438489563868,12.2,-5.40170729554548));
#180916=CARTESIAN_POINT('Ctrl Pts',(8.97736017116679,12.2,-5.402890118114));
#180917=CARTESIAN_POINT('Ctrl Pts',(8.98038246188711,12.2,-5.40408165690346));
#180918=CARTESIAN_POINT('Ctrl Pts',(8.98340475288196,12.2,-5.40527319580113));
#180919=CARTESIAN_POINT('Ctrl Pts',(8.98647405673137,12.2,-5.40647345299135));
#180920=CARTESIAN_POINT('Ctrl Pts',(8.98958993590321,12.2,-5.40768174280755));
#180921=CARTESIAN_POINT('Ctrl Pts',(8.99270581479201,12.2,-5.408890032514));
#180922=CARTESIAN_POINT('Ctrl Pts',(8.99586827068388,12.2,-5.41010635178838));
#180923=CARTESIAN_POINT('Ctrl Pts',(8.99907686774841,12.2,-5.41133003174945));
#180924=CARTESIAN_POINT('Ctrl Pts',(9.00228546481295,12.2,-5.41255371171051));
#180925=CARTESIAN_POINT('Ctrl Pts',(9.00554020763815,12.2,-5.41378475248552));
#180926=CARTESIAN_POINT('Ctrl Pts',(9.00884067043179,12.2,-5.41502249935676));
#180927=CARTESIAN_POINT('Ctrl Pts',(9.01214113352523,12.2,-5.41626024634042));
#180928=CARTESIAN_POINT('Ctrl Pts',(9.01548731562951,12.2,-5.41750469859001));
#180929=CARTESIAN_POINT('Ctrl Pts',(9.01887880106974,12.2,-5.41875521888766));
#180930=CARTESIAN_POINT('Ctrl Pts',(9.02227028620191,12.2,-5.42000573907171));
#180931=CARTESIAN_POINT('Ctrl Pts',(9.02570707445971,12.2,-5.4212623260792));
#180932=CARTESIAN_POINT('Ctrl Pts',(9.02918875449986,12.2,-5.4225243582));
#180933=CARTESIAN_POINT('Ctrl Pts',(9.03267043454002,12.2,-5.42378639032082));
#180934=CARTESIAN_POINT('Ctrl Pts',(9.03619700805011,12.2,-5.42505386519323));
#180935=CARTESIAN_POINT('Ctrl Pts',(9.03976807017952,12.2,-5.42632617637694));
#180936=CARTESIAN_POINT('Ctrl Pts',(9.04333913263329,12.2,-5.42759848767622));
#180937=CARTESIAN_POINT('Ctrl Pts',(9.046954682613,12.2,-5.42887563343622));
#180938=CARTESIAN_POINT('Ctrl Pts',(9.05061432498211,12.2,-5.43015702067301));
#180939=CARTESIAN_POINT('Ctrl Pts',(9.05427396701881,12.2,-5.43143840779341));
#180940=CARTESIAN_POINT('Ctrl Pts',(9.05797769955396,12.2,-5.43272403534991));
#180941=CARTESIAN_POINT('Ctrl Pts',(9.06172513076824,12.2,-5.43401332172559));
#180942=CARTESIAN_POINT('Ctrl Pts',(9.06547256198253,12.2,-5.43530260810128));
#180943=CARTESIAN_POINT('Ctrl Pts',(9.06926369413228,12.2,-5.43659555510162));
#180944=CARTESIAN_POINT('Ctrl Pts',(9.07309813832441,12.2,-5.43789159247105));
#180945=CARTESIAN_POINT('Ctrl Pts',(9.0762935086006,12.2,-5.4389716236515));
#180946=CARTESIAN_POINT('Ctrl Pts',(9.07951895779428,12.2,-5.44005380197366));
#180947=CARTESIAN_POINT('Ctrl Pts',(9.08277426473715,12.2,-5.44113780565413));
#180948=CARTESIAN_POINT('Ctrl Pts',(9.08602957168004,12.2,-5.44222180933458));
#180949=CARTESIAN_POINT('Ctrl Pts',(9.08931473772756,12.2,-5.44330763708894));
#180950=CARTESIAN_POINT('Ctrl Pts',(9.09262954371475,12.2,-5.44439497494109));
#180951=CARTESIAN_POINT('Ctrl Pts',(9.09594434970194,12.2,-5.44548231279324));
#180952=CARTESIAN_POINT('Ctrl Pts',(9.09928879517208,12.2,-5.44657115787779));
#180953=CARTESIAN_POINT('Ctrl Pts',(9.1026626662832,12.2,-5.44766120322501));
#180954=CARTESIAN_POINT('Ctrl Pts',(9.10603653739431,12.2,-5.44875124857224));
#180955=CARTESIAN_POINT('Ctrl Pts',(9.1094398338694,12.2,-5.44984249195675));
#180956=CARTESIAN_POINT('Ctrl Pts',(9.11287234096841,12.2,-5.45093462918394));
#180957=CARTESIAN_POINT('Ctrl Pts',(9.11630484806743,12.2,-5.45202676641113));
#180958=CARTESIAN_POINT('Ctrl Pts',(9.11976656888795,12.2,-5.45311979772707));
#180959=CARTESIAN_POINT('Ctrl Pts',(9.12325728923667,12.2,-5.45421342404654));
#180960=CARTESIAN_POINT('Ctrl Pts',(9.12674800958541,12.2,-5.45530705036601));
#180961=CARTESIAN_POINT('Ctrl Pts',(9.13026773206949,12.2,-5.45640127022158));
#180962=CARTESIAN_POINT('Ctrl Pts',(9.13381624651545,12.2,-5.45749579230493));
#180963=CARTESIAN_POINT('Ctrl Pts',(9.1373647609614,12.2,-5.45859031438828));
#180964=CARTESIAN_POINT('Ctrl Pts',(9.14094206858089,12.2,-5.45968513537797));
#180965=CARTESIAN_POINT('Ctrl Pts',(9.14454796244356,12.2,-5.46077997008544));
#180966=CARTESIAN_POINT('Ctrl Pts',(9.14815385630625,12.2,-5.46187480479292));
#180967=CARTESIAN_POINT('Ctrl Pts',(9.15178833685444,12.2,-5.4629696504932));
#180968=CARTESIAN_POINT('Ctrl Pts',(9.15545119970399,12.2,-5.46406422445152));
#180969=CARTESIAN_POINT('Ctrl Pts',(9.15911406255353,12.2,-5.46515879840983));
#180970=CARTESIAN_POINT('Ctrl Pts',(9.16280530803408,12.2,-5.46625309921534));
#180971=CARTESIAN_POINT('Ctrl Pts',(9.16652473491139,12.2,-5.46734685136808));
#180972=CARTESIAN_POINT('Ctrl Pts',(9.17024416138328,12.2,-5.46844060340159));
#180973=CARTESIAN_POINT('Ctrl Pts',(9.17399176781987,12.2,-5.46953380356503));
#180974=CARTESIAN_POINT('Ctrl Pts',(9.17776735448937,12.2,-5.47062617914047));
#180975=CARTESIAN_POINT('Ctrl Pts',(9.18154294157041,12.2,-5.47171855483498));
#180976=CARTESIAN_POINT('Ctrl Pts',(9.18534651057879,12.2,-5.47281010628507));
#180977=CARTESIAN_POINT('Ctrl Pts',(9.18917786092375,12.2,-5.47390056288239));
#180978=CARTESIAN_POINT('Ctrl Pts',(9.1930092112687,12.2,-5.47499101947969));
#180979=CARTESIAN_POINT('Ctrl Pts',(9.19686834516041,12.2,-5.47608038108537));
#180980=CARTESIAN_POINT('Ctrl Pts',(9.20075506474151,12.2,-5.47716838434937));
#180981=CARTESIAN_POINT('Ctrl Pts',(9.2046417843226,12.2,-5.47825638761337));
#180982=CARTESIAN_POINT('Ctrl Pts',(9.2085560911085,12.2,-5.47934303048085));
#180983=CARTESIAN_POINT('Ctrl Pts',(9.21249779081741,12.2,-5.48042805463239));
#180984=CARTESIAN_POINT('Ctrl Pts',(9.21643949052631,12.2,-5.48151307878393));
#180985=CARTESIAN_POINT('Ctrl Pts',(9.22040858133456,12.2,-5.48259648263473));
#180986=CARTESIAN_POINT('Ctrl Pts',(9.22440487251368,12.2,-5.48367801020428));
#180987=CARTESIAN_POINT('Ctrl Pts',(9.22840116369281,12.2,-5.48475953777381));
#180988=CARTESIAN_POINT('Ctrl Pts',(9.23242465490877,12.2,-5.48583919049053));
#180989=CARTESIAN_POINT('Ctrl Pts',(9.23647515601847,12.2,-5.48691671396287));
#180990=CARTESIAN_POINT('Ctrl Pts',(9.23971555708284,12.2,-5.48777873278772));
#180991=CARTESIAN_POINT('Ctrl Pts',(9.24297324329827,12.2,-5.48863939026006));
#180992=CARTESIAN_POINT('Ctrl Pts',(9.24624811997518,12.2,-5.48949855784968));
#180993=CARTESIAN_POINT('Ctrl Pts',(9.24952299620589,12.2,-5.49035772532223));
#180994=CARTESIAN_POINT('Ctrl Pts',(9.25281506078727,12.2,-5.49121540546935));
#180995=CARTESIAN_POINT('Ctrl Pts',(9.25612421823785,12.2,-5.49207146945502));
#180996=CARTESIAN_POINT('Ctrl Pts',(9.25943337613931,12.2,-5.49292753355734));
#180997=CARTESIAN_POINT('Ctrl Pts',(9.26275962842059,12.2,-5.49378198385947));
#180998=CARTESIAN_POINT('Ctrl Pts',(9.26610287754835,12.2,-5.49463469529471));
#180999=CARTESIAN_POINT('Ctrl Pts',(9.2694461262206,12.2,-5.49548740661378));
#181000=CARTESIAN_POINT('Ctrl Pts',(9.27280637185487,12.2,-5.4963383795203));
#181001=CARTESIAN_POINT('Ctrl Pts',(9.27618352146826,12.2,-5.49718749216014));
#181002=CARTESIAN_POINT('Ctrl Pts',(9.27956067154179,12.2,-5.49803660491565));
#181003=CARTESIAN_POINT('Ctrl Pts',(9.28295472381133,12.2,-5.49888385620928));
#181004=CARTESIAN_POINT('Ctrl Pts',(9.28636558505388,12.2,-5.49972912631077));
#181005=CARTESIAN_POINT('Ctrl Pts',(9.29062916137468,12.2,-5.50078571388004));
#181006=CARTESIAN_POINT('Ctrl Pts',(9.29491900179762,12.2,-5.50183920530774));
#181007=CARTESIAN_POINT('Ctrl Pts',(9.29923492304898,12.2,-5.50288936787702));
#181008=CARTESIAN_POINT('Ctrl Pts',(9.30355084430034,12.2,-5.50393953044628));
#181009=CARTESIAN_POINT('Ctrl Pts',(9.30789284614257,12.2,-5.50498636390258));
#181010=CARTESIAN_POINT('Ctrl Pts',(9.31226074851535,12.2,-5.50602964062112));
#181011=CARTESIAN_POINT('Ctrl Pts',(9.31575507012792,12.2,-5.50686426192772));
#181012=CARTESIAN_POINT('Ctrl Pts',(9.31926596793444,12.2,-5.50769660579151));
#181013=CARTESIAN_POINT('Ctrl Pts',(9.32279334997834,12.2,-5.50852655789049));
#181014=CARTESIAN_POINT('Ctrl Pts',(9.32632073250284,12.2,-5.50935651010254));
#181015=CARTESIAN_POINT('Ctrl Pts',(9.32986459862931,12.2,-5.51018406957821));
#181016=CARTESIAN_POINT('Ctrl Pts',(9.33342485782442,12.2,-5.51100912306745));
#181017=CARTESIAN_POINT('Ctrl Pts',(9.33698511653444,12.2,-5.51183417644428));
#181018=CARTESIAN_POINT('Ctrl Pts',(9.34056176862204,12.2,-5.5126567232791));
#181019=CARTESIAN_POINT('Ctrl Pts',(9.34415472172861,12.2,-5.51347665136437));
#181020=CARTESIAN_POINT('Ctrl Pts',(9.34774767532473,12.2,-5.51429657956135));
#181021=CARTESIAN_POINT('Ctrl Pts',(9.35135693103388,12.2,-5.51511388801682));
#181022=CARTESIAN_POINT('Ctrl Pts',(9.35498239828808,12.2,-5.51592846628326));
#181023=CARTESIAN_POINT('Ctrl Pts',(9.35860786504831,12.2,-5.51674304443871));
#181024=CARTESIAN_POINT('Ctrl Pts',(9.36224954469418,12.2,-5.51755489178915));
#181025=CARTESIAN_POINT('Ctrl Pts',(9.36590734489351,12.2,-5.51836389983442));
#181026=CARTESIAN_POINT('Ctrl Pts',(9.36956514559122,12.2,-5.51917290798992));
#181027=CARTESIAN_POINT('Ctrl Pts',(9.37323906983727,12.2,-5.51997907373927));
#181028=CARTESIAN_POINT('Ctrl Pts',(9.3769290257774,12.2,-5.52078229250891));
#181029=CARTESIAN_POINT('Ctrl Pts',(9.38061898121478,12.2,-5.52158551116911));
#181030=CARTESIAN_POINT('Ctrl Pts',(9.38432496933614,12.2,-5.52238578031232));
#181031=CARTESIAN_POINT('Ctrl Pts',(9.38804690214135,12.2,-5.52318299313635));
#181032=CARTESIAN_POINT('Ctrl Pts',(9.39176883545368,12.2,-5.52398020606899));
#181033=CARTESIAN_POINT('Ctrl Pts',(9.3955067129203,12.2,-5.52477436240414));
#181034=CARTESIAN_POINT('Ctrl Pts',(9.39926044629154,12.2,-5.52556535672503));
#181035=CARTESIAN_POINT('Ctrl Pts',(9.40301417966279,12.2,-5.52635635104592));
#181036=CARTESIAN_POINT('Ctrl Pts',(9.40678376934421,12.2,-5.52714418338032));
#181037=CARTESIAN_POINT('Ctrl Pts',(9.41056912788546,12.2,-5.52792874831163));
#181038=CARTESIAN_POINT('Ctrl Pts',(9.41530082528839,12.2,-5.52890945431543));
#181039=CARTESIAN_POINT('Ctrl Pts',(9.42005716186988,12.2,-5.52988505572844));
#181040=CARTESIAN_POINT('Ctrl Pts',(9.42483796537456,12.2,-5.53085534937311));
#181041=CARTESIAN_POINT('Ctrl Pts',(9.42866260880363,12.2,-5.53163158441576));
#181042=CARTESIAN_POINT('Ctrl Pts',(9.43250291339807,12.2,-5.53240442323866));
#181043=CARTESIAN_POINT('Ctrl Pts',(9.43635879077488,12.2,-5.53317376422503));
#181044=CARTESIAN_POINT('Ctrl Pts',(9.44021466815169,12.2,-5.53394310521141));
#181045=CARTESIAN_POINT('Ctrl Pts',(9.44408611842199,12.2,-5.53470894760014));
#181046=CARTESIAN_POINT('Ctrl Pts',(9.44797305696874,12.2,-5.53547119064132));
#181047=CARTESIAN_POINT('Ctrl Pts',(9.4518599949859,12.2,-5.53623343357864));
#181048=CARTESIAN_POINT('Ctrl Pts',(9.45576241973865,12.2,-5.53699207792168));
#181049=CARTESIAN_POINT('Ctrl Pts',(9.45968024721388,12.2,-5.53774702347451));
#181050=CARTESIAN_POINT('Ctrl Pts',(9.46359807522292,12.2,-5.53850196913021));
#181051=CARTESIAN_POINT('Ctrl Pts',(9.46753130493149,12.2,-5.53925321547911));
#181052=CARTESIAN_POINT('Ctrl Pts',(9.47147985220381,12.2,-5.54000066513057));
#181053=CARTESIAN_POINT('Ctrl Pts',(9.47542839893814,12.2,-5.54074811468018));
#181054=CARTESIAN_POINT('Ctrl Pts',(9.47939226273157,12.2,-5.54149176731641));
#181055=CARTESIAN_POINT('Ctrl Pts',(9.48337135768307,12.2,-5.54223152492285));
#181056=CARTESIAN_POINT('Ctrl Pts',(9.48735045317672,12.2,-5.5429712826301));
#181057=CARTESIAN_POINT('Ctrl Pts',(9.49134478323052,12.2,-5.54370714562297));
#181058=CARTESIAN_POINT('Ctrl Pts',(9.49535426056114,12.2,-5.54443901805149));
#181059=CARTESIAN_POINT('Ctrl Pts',(9.49936373734546,12.2,-5.54517089038029));
#181060=CARTESIAN_POINT('Ctrl Pts',(9.50338836268796,12.2,-5.54589877263153));
#181061=CARTESIAN_POINT('Ctrl Pts',(9.50742805244712,12.2,-5.54662256888665));
#181062=CARTESIAN_POINT('Ctrl Pts',(9.51146774275668,12.2,-5.54734636524039));
#181063=CARTESIAN_POINT('Ctrl Pts',(9.51552249811828,12.2,-5.54806607542254));
#181064=CARTESIAN_POINT('Ctrl Pts',(9.51959223484106,12.2,-5.54878160585015));
#181065=CARTESIAN_POINT('Ctrl Pts',(9.52366197100934,12.2,-5.54949713618028));
#181066=CARTESIAN_POINT('Ctrl Pts',(9.52774669062739,12.2,-5.55020848671123));
#181067=CARTESIAN_POINT('Ctrl Pts',(9.53184630684628,12.2,-5.55091556437609));
#181068=CARTESIAN_POINT('Ctrl Pts',(9.53594592362374,12.2,-5.55162264213728));
#181069=CARTESIAN_POINT('Ctrl Pts',(9.54006044054218,12.2,-5.55232544711206));
#181070=CARTESIAN_POINT('Ctrl Pts',(9.54418977278604,12.2,-5.55302388754217));
#181071=CARTESIAN_POINT('Ctrl Pts',(9.54831910446727,12.2,-5.55372232787712));
#181072=CARTESIAN_POINT('Ctrl Pts',(9.55246325326141,12.2,-5.55441640364321));
#181073=CARTESIAN_POINT('Ctrl Pts',(9.55662213658658,12.2,-5.55510602392061));
#181074=CARTESIAN_POINT('Ctrl Pts',(9.5607810204784,12.2,-5.55579564429198));
#181075=CARTESIAN_POINT('Ctrl Pts',(9.56495463846884,12.2,-5.55648080801572));
#181076=CARTESIAN_POINT('Ctrl Pts',(9.56914290930821,12.2,-5.55716142777503));
#181077=CARTESIAN_POINT('Ctrl Pts',(9.57333118014759,12.2,-5.55784204753435));
#181078=CARTESIAN_POINT('Ctrl Pts',(9.57753410486645,12.2,-5.55851812109313));
#181079=CARTESIAN_POINT('Ctrl Pts',(9.58175160093112,12.2,-5.55918956085148));
#181080=CARTESIAN_POINT('Ctrl Pts',(9.58596909642116,12.2,-5.55986100051834));
#181081=CARTESIAN_POINT('Ctrl Pts',(9.59020116373047,12.2,-5.5605278073118));
#181082=CARTESIAN_POINT('Ctrl Pts',(9.59444772251367,12.2,-5.56118989048292));
#181083=CARTESIAN_POINT('Ctrl Pts',(9.59975592142659,12.2,-5.56201749451447));
#181084=CARTESIAN_POINT('Ctrl Pts',(9.60508676277765,12.2,-5.56283772212781));
#181085=CARTESIAN_POINT('Ctrl Pts',(9.61044008999988,12.2,-5.5636504010167));
#181086=CARTESIAN_POINT('Ctrl Pts',(9.61472275201107,12.2,-5.56430054416324));
#181087=CARTESIAN_POINT('Ctrl Pts',(9.61901980376281,12.2,-5.56494585625644));
#181088=CARTESIAN_POINT('Ctrl Pts',(9.62333116722147,12.2,-5.5655862533464));
#181089=CARTESIAN_POINT('Ctrl Pts',(9.6276425300927,12.2,-5.5662266503491));
#181090=CARTESIAN_POINT('Ctrl Pts',(9.63196820452373,12.2,-5.5668621301816));
#181091=CARTESIAN_POINT('Ctrl Pts',(9.63630811002193,12.2,-5.56749261046627));
#181092=CARTESIAN_POINT('Ctrl Pts',(9.64064801611146,12.2,-5.56812309083684));
#181093=CARTESIAN_POINT('Ctrl Pts',(9.64500215450515,12.2,-5.56874856932373));
#181094=CARTESIAN_POINT('Ctrl Pts',(9.64937044402245,12.2,-5.56936896380147));
#181095=CARTESIAN_POINT('Ctrl Pts',(9.65373873294456,12.2,-5.56998935819468));
#181096=CARTESIAN_POINT('Ctrl Pts',(9.65812117542594,12.2,-5.57060466827187));
#181097=CARTESIAN_POINT('Ctrl Pts',(9.66251769089894,12.2,-5.57121481066678));
#181098=CARTESIAN_POINT('Ctrl Pts',(9.66581507765345,12.2,-5.57167241748373));
#181099=CARTESIAN_POINT('Ctrl Pts',(9.66912038021472,12.2,-5.57212711718944));
#181100=CARTESIAN_POINT('Ctrl Pts',(9.67243356713395,12.2,-5.57257887644593));
#181101=CARTESIAN_POINT('Ctrl Pts',(9.67574675405318,12.2,-5.57303063570243));
#181102=CARTESIAN_POINT('Ctrl Pts',(9.67906782446287,12.2,-5.57347945283529));
#181103=CARTESIAN_POINT('Ctrl Pts',(9.68239674475753,12.2,-5.57392529469451));
#181104=CARTESIAN_POINT('Ctrl Pts',(9.68572566565693,12.2,-5.57437113663471));
#181105=CARTESIAN_POINT('Ctrl Pts',(9.68906243685854,12.2,-5.57481400329908));
#181106=CARTESIAN_POINT('Ctrl Pts',(9.69240702572069,12.2,-5.57525385936259));
#181107=CARTESIAN_POINT('Ctrl Pts',(9.69575161397524,12.2,-5.5756937153462));
#181108=CARTESIAN_POINT('Ctrl Pts',(9.69910401937102,12.2,-5.57613056264663));
#181109=CARTESIAN_POINT('Ctrl Pts',(9.70246421008295,12.2,-5.5765643660056));
#181110=CARTESIAN_POINT('Ctrl Pts',(9.70582440079487,12.2,-5.57699816936458));
#181111=CARTESIAN_POINT('Ctrl Pts',(9.70919237582691,12.2,-5.5774289287807));
#181112=CARTESIAN_POINT('Ctrl Pts',(9.71256810401129,12.2,-5.57785661201709));
#181113=CARTESIAN_POINT('Ctrl Pts',(9.71706907471938,12.2,-5.57842685630638));
#181114=CARTESIAN_POINT('Ctrl Pts',(9.72158382644498,12.2,-5.57899162970374));
#181115=CARTESIAN_POINT('Ctrl Pts',(9.72611228201783,12.2,-5.5795508536586));
#181116=CARTESIAN_POINT('Ctrl Pts',(9.72950862446872,12.2,-5.57997027171998));
#181117=CARTESIAN_POINT('Ctrl Pts',(9.73291267654677,12.2,-5.58038656936382));
#181118=CARTESIAN_POINT('Ctrl Pts',(9.73632440400199,12.2,-5.5807997123401));
#181119=CARTESIAN_POINT('Ctrl Pts',(9.74087337290928,12.2,-5.58135056951672));
#181120=CARTESIAN_POINT('Ctrl Pts',(9.74543598885924,12.2,-5.58189581905794));
#181121=CARTESIAN_POINT('Ctrl Pts',(9.75001217631758,12.2,-5.58243538418087));
#181122=CARTESIAN_POINT('Ctrl Pts',(9.75344431706722,12.2,-5.58284005804145));
#181123=CARTESIAN_POINT('Ctrl Pts',(9.75688409058689,12.2,-5.58324153383382));
#181124=CARTESIAN_POINT('Ctrl Pts',(9.76033146554965,12.2,-5.58363978067296));
#181125=CARTESIAN_POINT('Ctrl Pts',(9.76377884051241,12.2,-5.58403802751209));
#181126=CARTESIAN_POINT('Ctrl Pts',(9.76723381713857,12.2,-5.58443304364509));
#181127=CARTESIAN_POINT('Ctrl Pts',(9.77069636197007,12.2,-5.5848247976313));
#181128=CARTESIAN_POINT('Ctrl Pts',(9.77415890743059,12.2,-5.58521655168868));
#181129=CARTESIAN_POINT('Ctrl Pts',(9.77762902258492,12.2,-5.58560504584514));
#181130=CARTESIAN_POINT('Ctrl Pts',(9.78110667500803,12.2,-5.58599024485901));
#181131=CARTESIAN_POINT('Ctrl Pts',(9.78458432679936,12.2,-5.58637544380289));
#181132=CARTESIAN_POINT('Ctrl Pts',(9.78806951572364,12.2,-5.58675734865529));
#181133=CARTESIAN_POINT('Ctrl Pts',(9.79156220959739,12.2,-5.58713592901625));
#181134=CARTESIAN_POINT('Ctrl Pts',(9.79505490347114,12.2,-5.5875145093772));
#181135=CARTESIAN_POINT('Ctrl Pts',(9.79855510384789,12.2,-5.58788976411221));
#181136=CARTESIAN_POINT('Ctrl Pts',(9.80206277673642,12.2,-5.58826166251704));
#181137=CARTESIAN_POINT('Ctrl Pts',(9.8067396737087,12.2,-5.5887575270343));
#181138=CARTESIAN_POINT('Ctrl Pts',(9.81142985850841,12.2,-5.58924742503764));
#181139=CARTESIAN_POINT('Ctrl Pts',(9.8161332539559,12.2,-5.58973128222093));
#181140=CARTESIAN_POINT('Ctrl Pts',(9.81966080134256,12.2,-5.59009417519079));
#181141=CARTESIAN_POINT('Ctrl Pts',(9.82319577937296,12.2,-5.59045367035971));
#181142=CARTESIAN_POINT('Ctrl Pts',(9.8267381582638,12.2,-5.59080973736932));
#181143=CARTESIAN_POINT('Ctrl Pts',(9.8302805365111,12.2,-5.59116580431426));
#181144=CARTESIAN_POINT('Ctrl Pts',(9.83383031526635,12.2,-5.59151844253437));
#181145=CARTESIAN_POINT('Ctrl Pts',(9.83738746117941,12.2,-5.59186762197971));
#181146=CARTESIAN_POINT('Ctrl Pts',(9.84094460709248,12.2,-5.59221680142505));
#181147=CARTESIAN_POINT('Ctrl Pts',(9.84450912232966,12.2,-5.59256252206248));
#181148=CARTESIAN_POINT('Ctrl Pts',(9.84808097419989,12.2,-5.59290475350837));
#181149=CARTESIAN_POINT('Ctrl Pts',(9.85165282607011,12.2,-5.59324698495427));
#181150=CARTESIAN_POINT('Ctrl Pts',(9.85523201532336,12.2,-5.59358572800864));
#181151=CARTESIAN_POINT('Ctrl Pts',(9.85881851056742,12.2,-5.59392095145511));
#181152=CARTESIAN_POINT('Ctrl Pts',(9.86240500581147,12.2,-5.59425617490156));
#181153=CARTESIAN_POINT('Ctrl Pts',(9.86599880662169,12.2,-5.5945878787483));
#181154=CARTESIAN_POINT('Ctrl Pts',(9.86959988258658,12.2,-5.59491603466985));
#181155=CARTESIAN_POINT('Ctrl Pts',(9.87320095855147,12.2,-5.5952441905914));
#181156=CARTESIAN_POINT('Ctrl Pts',(9.87680930991072,12.2,-5.5955687979579));
#181157=CARTESIAN_POINT('Ctrl Pts',(9.8804249042367,12.2,-5.59588982644672));
#181158=CARTESIAN_POINT('Ctrl Pts',(9.88524569710923,12.2,-5.5963178644707));
#181159=CARTESIAN_POINT('Ctrl Pts',(9.89007936838298,12.2,-5.59673954165519));
#181160=CARTESIAN_POINT('Ctrl Pts',(9.89492584325822,12.2,-5.59715478823337));
#181161=CARTESIAN_POINT('Ctrl Pts',(9.89856069908449,12.2,-5.59746622313872));
#181162=CARTESIAN_POINT('Ctrl Pts',(9.90220275683546,12.2,-5.59777404024422));
#181163=CARTESIAN_POINT('Ctrl Pts',(9.90585198707725,12.2,-5.59807821123349));
#181164=CARTESIAN_POINT('Ctrl Pts',(9.90950121731904,12.2,-5.59838238222276));
#181165=CARTESIAN_POINT('Ctrl Pts',(9.91315761837541,12.2,-5.59868290817144));
#181166=CARTESIAN_POINT('Ctrl Pts',(9.91682116175783,12.2,-5.59897975821757));
#181167=CARTESIAN_POINT('Ctrl Pts',(9.92170588671141,12.2,-5.59937555831504));
#181168=CARTESIAN_POINT('Ctrl Pts',(9.92660330544688,12.2,-5.59976482509139));
#181169=CARTESIAN_POINT('Ctrl Pts',(9.93151334565974,12.2,-5.60014749105626));
#181170=CARTESIAN_POINT('Ctrl Pts',(9.93519587548489,12.2,-5.60043449050385));
#181171=CARTESIAN_POINT('Ctrl Pts',(9.93888550523421,12.2,-5.60071777724353));
#181172=CARTESIAN_POINT('Ctrl Pts',(9.94258220547489,12.2,-5.60099732227504));
#181173=CARTESIAN_POINT('Ctrl Pts',(9.94627890571557,12.2,-5.60127686730655));
#181174=CARTESIAN_POINT('Ctrl Pts',(9.94998267506431,12.2,-5.60155267229654));
#181175=CARTESIAN_POINT('Ctrl Pts',(9.95369348384554,12.2,-5.60182470828699));
#181176=CARTESIAN_POINT('Ctrl Pts',(9.95740429262676,12.2,-5.60209674427743));
#181177=CARTESIAN_POINT('Ctrl Pts',(9.96112214087936,12.2,-5.60236501167812));
#181178=CARTESIAN_POINT('Ctrl Pts',(9.96484699726263,12.2,-5.60262948072384));
#181179=CARTESIAN_POINT('Ctrl Pts',(9.96857185364591,12.2,-5.60289394976955));
#181180=CARTESIAN_POINT('Ctrl Pts',(9.97230371650496,12.2,-5.60315462115286));
#181181=CARTESIAN_POINT('Ctrl Pts',(9.97604255774317,12.2,-5.60341146722738));
#181182=CARTESIAN_POINT('Ctrl Pts',(9.9797813996606,12.2,-5.60366831334856));
#181183=CARTESIAN_POINT('Ctrl Pts',(9.98352721885499,12.2,-5.60392133440201));
#181184=CARTESIAN_POINT('Ctrl Pts',(9.98727998885967,12.2,-5.60417050597936));
#181185=CARTESIAN_POINT('Ctrl Pts',(9.99103275818261,12.2,-5.60441967751145));
#181186=CARTESIAN_POINT('Ctrl Pts',(9.99479247849683,12.2,-5.60466500045207));
#181187=CARTESIAN_POINT('Ctrl Pts',(9.99855911819391,12.2,-5.60490644531796));
#181188=CARTESIAN_POINT('Ctrl Pts',(10.002325757891,12.2,-5.60514789018385));
#181189=CARTESIAN_POINT('Ctrl Pts',(10.0060993160735,12.2,-5.60538545632437));
#181190=CARTESIAN_POINT('Ctrl Pts',(10.0098797567867,12.2,-5.60561911123359));
#181191=CARTESIAN_POINT('Ctrl Pts',(10.0136601974998,12.2,-5.60585276614281));
#181192=CARTESIAN_POINT('Ctrl Pts',(10.0174475189171,12.2,-5.60608250832366));
#181193=CARTESIAN_POINT('Ctrl Pts',(10.0212416935048,12.2,-5.60630831402483));
#181194=CARTESIAN_POINT('Ctrl Pts',(10.0275653180473,12.2,-5.60668465687379));
#181195=CARTESIAN_POINT('Ctrl Pts',(10.0339079809464,12.2,-5.6070500702561));
#181196=CARTESIAN_POINT('Ctrl Pts',(10.0402696489999,12.2,-5.60740451200001));
#181197=CARTESIAN_POINT('Origin',(-5.66257110645729E-14,15.2,-1.77635683940025E-14));
#181198=CARTESIAN_POINT('',(9.55499537054798,15.2,-4.04260911609085));
#181199=CARTESIAN_POINT('',(9.55499537054798,12.2,-4.04260911609085));
#181200=CARTESIAN_POINT('',(9.55499536999995,15.2,-4.04260911600002));
#181201=CARTESIAN_POINT('Origin',(-5.66257110645729E-14,12.2,-1.77635683940025E-14));
#181202=CARTESIAN_POINT('Origin',(-5.66257110645729E-14,15.2,-1.77635683940025E-14));
#181203=CARTESIAN_POINT('Origin',(-5.66257110645729E-14,15.2,-1.77635683940025E-14));
#181204=CARTESIAN_POINT('',(10.736091047551,15.2,-4.12144986808358));
#181205=CARTESIAN_POINT('',(10.8675859439999,15.2,-3.76106045600002));
#181206=CARTESIAN_POINT('Origin',(-5.66257110645729E-14,15.2,-1.77635683940025E-14));
#181207=CARTESIAN_POINT('',(10.8675859439999,12.2,-3.76106045600002));
#181208=CARTESIAN_POINT('',(10.8675859439999,15.2,-3.76106045600002));
#181209=CARTESIAN_POINT('',(10.7360910469999,12.2,-4.12144986800001));
#181210=CARTESIAN_POINT('Origin',(-5.66257110645729E-14,12.2,-1.77635683940025E-14));
#181211=CARTESIAN_POINT('',(10.7360910469999,15.2,-4.12144986800001));
#181212=CARTESIAN_POINT('Ctrl Pts',(9.55499537099995,15.2,-4.04260911600002));
#181213=CARTESIAN_POINT('Ctrl Pts',(9.55499537099995,11.6,-4.04260911600002));
#181214=CARTESIAN_POINT('Ctrl Pts',(9.55516119299994,15.2,-4.04266300400002));
#181215=CARTESIAN_POINT('Ctrl Pts',(9.55516119299994,11.6,-4.04266300400002));
#181216=CARTESIAN_POINT('Ctrl Pts',(9.55549865399995,15.2,-4.04277257900001));
#181217=CARTESIAN_POINT('Ctrl Pts',(9.55549865399995,11.6,-4.04277257900001));
#181218=CARTESIAN_POINT('Ctrl Pts',(9.55601007099995,15.2,-4.04293835900001));
#181219=CARTESIAN_POINT('Ctrl Pts',(9.55601007099995,11.6,-4.04293835900001));
#181220=CARTESIAN_POINT('Ctrl Pts',(9.55669916199994,15.2,-4.04316116600001));
#181221=CARTESIAN_POINT('Ctrl Pts',(9.55669916199994,11.6,-4.04316116600001));
#181222=CARTESIAN_POINT('Ctrl Pts',(9.55757104099994,15.2,-4.04344211400002));
#181223=CARTESIAN_POINT('Ctrl Pts',(9.55757104099994,11.6,-4.04344211400002));
#181224=CARTESIAN_POINT('Ctrl Pts',(9.55845733799995,15.2,-4.04372672600001));
#181225=CARTESIAN_POINT('Ctrl Pts',(9.55845733799995,11.6,-4.04372672600002));
#181226=CARTESIAN_POINT('Ctrl Pts',(9.55935298099994,15.2,-4.04401334800002));
#181227=CARTESIAN_POINT('Ctrl Pts',(9.55935298099994,11.6,-4.04401334800002));
#181228=CARTESIAN_POINT('Ctrl Pts',(9.56025795099994,15.2,-4.04430195600002));
#181229=CARTESIAN_POINT('Ctrl Pts',(9.56025795099994,11.6,-4.04430195600002));
#181230=CARTESIAN_POINT('Ctrl Pts',(9.56117222799995,15.2,-4.04459252400001));
#181231=CARTESIAN_POINT('Ctrl Pts',(9.56117222799995,11.6,-4.04459252400002));
#181232=CARTESIAN_POINT('Ctrl Pts',(9.56209578999994,15.2,-4.04488502600001));
#181233=CARTESIAN_POINT('Ctrl Pts',(9.56209578999994,11.6,-4.04488502600001));
#181234=CARTESIAN_POINT('Ctrl Pts',(9.56302861899994,15.2,-4.04517943800002));
#181235=CARTESIAN_POINT('Ctrl Pts',(9.56302861899994,11.6,-4.04517943800002));
#181236=CARTESIAN_POINT('Ctrl Pts',(9.56397069599995,15.2,-4.04547573400002));
#181237=CARTESIAN_POINT('Ctrl Pts',(9.56397069599995,11.6,-4.04547573400002));
#181238=CARTESIAN_POINT('Ctrl Pts',(9.56492199899994,15.2,-4.04577389000002));
#181239=CARTESIAN_POINT('Ctrl Pts',(9.56492199899994,11.6,-4.04577389000002));
#181240=CARTESIAN_POINT('Ctrl Pts',(9.56588250899994,15.2,-4.04607388100001));
#181241=CARTESIAN_POINT('Ctrl Pts',(9.56588250899994,11.6,-4.04607388100001));
#181242=CARTESIAN_POINT('Ctrl Pts',(9.56685220699995,15.2,-4.04637568200001));
#181243=CARTESIAN_POINT('Ctrl Pts',(9.56685220699995,11.6,-4.04637568200001));
#181244=CARTESIAN_POINT('Ctrl Pts',(9.56783107299995,15.2,-4.04667926900002));
#181245=CARTESIAN_POINT('Ctrl Pts',(9.56783107299995,11.6,-4.04667926900002));
#181246=CARTESIAN_POINT('Ctrl Pts',(9.56881908799994,15.2,-4.04698461800002));
#181247=CARTESIAN_POINT('Ctrl Pts',(9.56881908799994,11.6,-4.04698461800002));
#181248=CARTESIAN_POINT('Ctrl Pts',(9.56981623299994,15.2,-4.04729170300001));
#181249=CARTESIAN_POINT('Ctrl Pts',(9.56981623299994,11.6,-4.04729170300001));
#181250=CARTESIAN_POINT('Ctrl Pts',(9.57082248799994,15.2,-4.04760050200001));
#181251=CARTESIAN_POINT('Ctrl Pts',(9.57082248799994,11.6,-4.04760050200002));
#181252=CARTESIAN_POINT('Ctrl Pts',(9.57183783399995,15.2,-4.04791099000001));
#181253=CARTESIAN_POINT('Ctrl Pts',(9.57183783399995,11.6,-4.04791099000002));
#181254=CARTESIAN_POINT('Ctrl Pts',(9.57286225199995,15.2,-4.04822314300001));
#181255=CARTESIAN_POINT('Ctrl Pts',(9.57286225199995,11.6,-4.04822314300001));
#181256=CARTESIAN_POINT('Ctrl Pts',(9.57389572299994,15.2,-4.04853693900002));
#181257=CARTESIAN_POINT('Ctrl Pts',(9.57389572299994,11.6,-4.04853693900002));
#181258=CARTESIAN_POINT('Ctrl Pts',(9.57493822699995,15.2,-4.04885235200001));
#181259=CARTESIAN_POINT('Ctrl Pts',(9.57493822699995,11.6,-4.04885235200002));
#181260=CARTESIAN_POINT('Ctrl Pts',(9.57598974799994,15.2,-4.04916936000001));
#181261=CARTESIAN_POINT('Ctrl Pts',(9.57598974799994,11.6,-4.04916936000001));
#181262=CARTESIAN_POINT('Ctrl Pts',(9.57705026499994,15.2,-4.04948793900001));
#181263=CARTESIAN_POINT('Ctrl Pts',(9.57705026499994,11.6,-4.04948793900001));
#181264=CARTESIAN_POINT('Ctrl Pts',(9.57811975999994,15.2,-4.04980806600001));
#181265=CARTESIAN_POINT('Ctrl Pts',(9.57811975999994,11.6,-4.04980806600001));
#181266=CARTESIAN_POINT('Ctrl Pts',(9.57919821399994,15.2,-4.05012971800002));
#181267=CARTESIAN_POINT('Ctrl Pts',(9.57919821399994,11.6,-4.05012971800002));
#181268=CARTESIAN_POINT('Ctrl Pts',(9.58028560899994,15.2,-4.05045287300001));
#181269=CARTESIAN_POINT('Ctrl Pts',(9.58028560899994,11.6,-4.05045287300002));
#181270=CARTESIAN_POINT('Ctrl Pts',(9.58138192599994,15.2,-4.05077750600002));
#181271=CARTESIAN_POINT('Ctrl Pts',(9.58138192599994,11.6,-4.05077750600002));
#181272=CARTESIAN_POINT('Ctrl Pts',(9.58248714699995,15.2,-4.05110359500001));
#181273=CARTESIAN_POINT('Ctrl Pts',(9.58248714699995,11.6,-4.05110359500001));
#181274=CARTESIAN_POINT('Ctrl Pts',(9.58360125399994,15.2,-4.05143111800002));
#181275=CARTESIAN_POINT('Ctrl Pts',(9.58360125399994,11.6,-4.05143111800002));
#181276=CARTESIAN_POINT('Ctrl Pts',(9.58472422699994,15.2,-4.05176005200001));
#181277=CARTESIAN_POINT('Ctrl Pts',(9.58472422699994,11.6,-4.05176005200001));
#181278=CARTESIAN_POINT('Ctrl Pts',(9.58585604999995,15.2,-4.05209037400001));
#181279=CARTESIAN_POINT('Ctrl Pts',(9.58585604999995,11.6,-4.05209037400002));
#181280=CARTESIAN_POINT('Ctrl Pts',(9.58699670499995,15.2,-4.05242206400001));
#181281=CARTESIAN_POINT('Ctrl Pts',(9.58699670499995,11.6,-4.05242206400002));
#181282=CARTESIAN_POINT('Ctrl Pts',(9.58814617199995,15.2,-4.05275509600001));
#181283=CARTESIAN_POINT('Ctrl Pts',(9.58814617199995,11.6,-4.05275509600001));
#181284=CARTESIAN_POINT('Ctrl Pts',(9.58930443499994,15.2,-4.05308945100002));
#181285=CARTESIAN_POINT('Ctrl Pts',(9.58930443499994,11.6,-4.05308945100002));
#181286=CARTESIAN_POINT('Ctrl Pts',(9.59047147499994,15.2,-4.05342510600001));
#181287=CARTESIAN_POINT('Ctrl Pts',(9.59047147499994,11.6,-4.05342510600002));
#181288=CARTESIAN_POINT('Ctrl Pts',(9.59164727399994,15.2,-4.05376204000001));
#181289=CARTESIAN_POINT('Ctrl Pts',(9.59164727399994,11.6,-4.05376204000001));
#181290=CARTESIAN_POINT('Ctrl Pts',(9.59283181499995,15.2,-4.05410022900002));
#181291=CARTESIAN_POINT('Ctrl Pts',(9.59283181499995,11.6,-4.05410022900002));
#181292=CARTESIAN_POINT('Ctrl Pts',(9.59402507999994,15.2,-4.05443965300002));
#181293=CARTESIAN_POINT('Ctrl Pts',(9.59402507999994,11.6,-4.05443965300002));
#181294=CARTESIAN_POINT('Ctrl Pts',(9.59522705299995,15.2,-4.05478029000002));
#181295=CARTESIAN_POINT('Ctrl Pts',(9.59522705299995,11.6,-4.05478029000002));
#181296=CARTESIAN_POINT('Ctrl Pts',(9.59643771299995,15.2,-4.05512212000001));
#181297=CARTESIAN_POINT('Ctrl Pts',(9.59643771299995,11.6,-4.05512212000002));
#181298=CARTESIAN_POINT('Ctrl Pts',(9.59765704499994,15.2,-4.05546511900001));
#181299=CARTESIAN_POINT('Ctrl Pts',(9.59765704499994,11.6,-4.05546511900001));
#181300=CARTESIAN_POINT('Ctrl Pts',(9.59888503199995,15.2,-4.05580926800001));
#181301=CARTESIAN_POINT('Ctrl Pts',(9.59888503199995,11.6,-4.05580926800001));
#181302=CARTESIAN_POINT('Ctrl Pts',(9.60012165499995,15.2,-4.05615454300001));
#181303=CARTESIAN_POINT('Ctrl Pts',(9.60012165499995,11.6,-4.05615454300001));
#181304=CARTESIAN_POINT('Ctrl Pts',(9.60136689799995,15.2,-4.05650092700002));
#181305=CARTESIAN_POINT('Ctrl Pts',(9.60136689799995,11.6,-4.05650092700002));
#181306=CARTESIAN_POINT('Ctrl Pts',(9.60262074299994,15.2,-4.05684839600001));
#181307=CARTESIAN_POINT('Ctrl Pts',(9.60262074299994,11.6,-4.05684839600002));
#181308=CARTESIAN_POINT('Ctrl Pts',(9.60388317399994,15.2,-4.05719693100002));
#181309=CARTESIAN_POINT('Ctrl Pts',(9.60388317399994,11.6,-4.05719693100002));
#181310=CARTESIAN_POINT('Ctrl Pts',(9.60515417299994,15.2,-4.05754650900001));
#181311=CARTESIAN_POINT('Ctrl Pts',(9.60515417299994,11.6,-4.05754650900001));
#181312=CARTESIAN_POINT('Ctrl Pts',(9.60643372199995,15.2,-4.05789711200002));
#181313=CARTESIAN_POINT('Ctrl Pts',(9.60643372199995,11.6,-4.05789711200002));
#181314=CARTESIAN_POINT('Ctrl Pts',(9.60772180599994,15.2,-4.05824871800001));
#181315=CARTESIAN_POINT('Ctrl Pts',(9.60772180599994,11.6,-4.05824871800002));
#181316=CARTESIAN_POINT('Ctrl Pts',(9.60901840799995,15.2,-4.05860130500002));
#181317=CARTESIAN_POINT('Ctrl Pts',(9.60901840799995,11.6,-4.05860130500002));
#181318=CARTESIAN_POINT('Ctrl Pts',(9.61032350999995,15.2,-4.05895485600002));
#181319=CARTESIAN_POINT('Ctrl Pts',(9.61032350999995,11.6,-4.05895485600002));
#181320=CARTESIAN_POINT('Ctrl Pts',(9.61163709499995,15.2,-4.05930934900002));
#181321=CARTESIAN_POINT('Ctrl Pts',(9.61163709499995,11.6,-4.05930934900002));
#181322=CARTESIAN_POINT('Ctrl Pts',(9.61295914899994,15.2,-4.05966476400001));
#181323=CARTESIAN_POINT('Ctrl Pts',(9.61295914899994,11.6,-4.05966476400002));
#181324=CARTESIAN_POINT('Ctrl Pts',(9.61428965299995,15.2,-4.06002108000001));
#181325=CARTESIAN_POINT('Ctrl Pts',(9.61428965299995,11.6,-4.06002108000001));
#181326=CARTESIAN_POINT('Ctrl Pts',(9.61562858999994,15.2,-4.06037827900001));
#181327=CARTESIAN_POINT('Ctrl Pts',(9.61562858999994,11.6,-4.06037827900002));
#181328=CARTESIAN_POINT('Ctrl Pts',(9.61697594499995,15.2,-4.06073634000002));
#181329=CARTESIAN_POINT('Ctrl Pts',(9.61697594499995,11.6,-4.06073634000002));
#181330=CARTESIAN_POINT('Ctrl Pts',(9.61833169999995,15.2,-4.06109524300001));
#181331=CARTESIAN_POINT('Ctrl Pts',(9.61833169999995,11.6,-4.06109524300002));
#181332=CARTESIAN_POINT('Ctrl Pts',(9.61969584099995,15.2,-4.06145496800002));
#181333=CARTESIAN_POINT('Ctrl Pts',(9.61969584099995,11.6,-4.06145496800002));
#181334=CARTESIAN_POINT('Ctrl Pts',(9.62106834999994,15.2,-4.06181549700001));
#181335=CARTESIAN_POINT('Ctrl Pts',(9.62106834999994,11.6,-4.06181549700001));
#181336=CARTESIAN_POINT('Ctrl Pts',(9.62244921099994,15.2,-4.06217680900001));
#181337=CARTESIAN_POINT('Ctrl Pts',(9.62244921099994,11.6,-4.06217680900001));
#181338=CARTESIAN_POINT('Ctrl Pts',(9.62383840699994,15.2,-4.06253888400002));
#181339=CARTESIAN_POINT('Ctrl Pts',(9.62383840699994,11.6,-4.06253888400002));
#181340=CARTESIAN_POINT('Ctrl Pts',(9.62523592199994,15.2,-4.06290170600001));
#181341=CARTESIAN_POINT('Ctrl Pts',(9.62523592199994,11.6,-4.06290170600002));
#181342=CARTESIAN_POINT('Ctrl Pts',(9.62664174299995,15.2,-4.06326525100001));
#181343=CARTESIAN_POINT('Ctrl Pts',(9.62664174299995,11.6,-4.06326525100001));
#181344=CARTESIAN_POINT('Ctrl Pts',(9.62805584999994,15.2,-4.06362950400001));
#181345=CARTESIAN_POINT('Ctrl Pts',(9.62805584999994,11.6,-4.06362950400002));
#181346=CARTESIAN_POINT('Ctrl Pts',(9.62947822799994,15.2,-4.06399444400002));
#181347=CARTESIAN_POINT('Ctrl Pts',(9.62947822799994,11.6,-4.06399444400002));
#181348=CARTESIAN_POINT('Ctrl Pts',(9.63090886199995,15.2,-4.06436005200002));
#181349=CARTESIAN_POINT('Ctrl Pts',(9.63090886199995,11.6,-4.06436005200002));
#181350=CARTESIAN_POINT('Ctrl Pts',(9.63234773499994,15.2,-4.06472630900002));
#181351=CARTESIAN_POINT('Ctrl Pts',(9.63234773499994,11.6,-4.06472630900002));
#181352=CARTESIAN_POINT('Ctrl Pts',(9.63379483299994,15.2,-4.06509319800001));
#181353=CARTESIAN_POINT('Ctrl Pts',(9.63379483299994,11.6,-4.06509319800001));
#181354=CARTESIAN_POINT('Ctrl Pts',(9.63525013899994,15.2,-4.06546069700001));
#181355=CARTESIAN_POINT('Ctrl Pts',(9.63525013899994,11.6,-4.06546069700001));
#181356=CARTESIAN_POINT('Ctrl Pts',(9.63671363699994,15.2,-4.06582879000001));
#181357=CARTESIAN_POINT('Ctrl Pts',(9.63671363699994,11.6,-4.06582879000002));
#181358=CARTESIAN_POINT('Ctrl Pts',(9.63818531199994,15.2,-4.06619745800001));
#181359=CARTESIAN_POINT('Ctrl Pts',(9.63818531199994,11.6,-4.06619745800001));
#181360=CARTESIAN_POINT('Ctrl Pts',(9.63966514799995,15.2,-4.06656668200001));
#181361=CARTESIAN_POINT('Ctrl Pts',(9.63966514799995,11.6,-4.06656668200002));
#181362=CARTESIAN_POINT('Ctrl Pts',(9.64115312899994,15.2,-4.06693644400002));
#181363=CARTESIAN_POINT('Ctrl Pts',(9.64115312899994,11.6,-4.06693644400002));
#181364=CARTESIAN_POINT('Ctrl Pts',(9.64264924099995,15.2,-4.06730672400001));
#181365=CARTESIAN_POINT('Ctrl Pts',(9.64264924099995,11.6,-4.06730672400002));
#181366=CARTESIAN_POINT('Ctrl Pts',(9.64415346699995,15.2,-4.06767750600002));
#181367=CARTESIAN_POINT('Ctrl Pts',(9.64415346699995,11.6,-4.06767750600002));
#181368=CARTESIAN_POINT('Ctrl Pts',(9.64566579199994,15.2,-4.06804877300001));
#181369=CARTESIAN_POINT('Ctrl Pts',(9.64566579199994,11.6,-4.06804877300001));
#181370=CARTESIAN_POINT('Ctrl Pts',(9.64718620099994,15.2,-4.06842050300002));
#181371=CARTESIAN_POINT('Ctrl Pts',(9.64718620099994,11.6,-4.06842050300002));
#181372=CARTESIAN_POINT('Ctrl Pts',(9.64871467899994,15.2,-4.06879268000001));
#181373=CARTESIAN_POINT('Ctrl Pts',(9.64871467899994,11.6,-4.06879268000001));
#181374=CARTESIAN_POINT('Ctrl Pts',(9.65025120999995,15.2,-4.06916528800001));
#181375=CARTESIAN_POINT('Ctrl Pts',(9.65025120999995,11.6,-4.06916528800001));
#181376=CARTESIAN_POINT('Ctrl Pts',(9.65179577899995,15.2,-4.06953830600001));
#181377=CARTESIAN_POINT('Ctrl Pts',(9.65179577899995,11.6,-4.06953830600001));
#181378=CARTESIAN_POINT('Ctrl Pts',(9.65334837099994,15.2,-4.06991171800001));
#181379=CARTESIAN_POINT('Ctrl Pts',(9.65334837099994,11.6,-4.06991171800002));
#181380=CARTESIAN_POINT('Ctrl Pts',(9.65490896999994,15.2,-4.07028550500002));
#181381=CARTESIAN_POINT('Ctrl Pts',(9.65490896999994,11.6,-4.07028550500002));
#181382=CARTESIAN_POINT('Ctrl Pts',(9.65647756399994,15.2,-4.07065965100001));
#181383=CARTESIAN_POINT('Ctrl Pts',(9.65647756399994,11.6,-4.07065965100002));
#181384=CARTESIAN_POINT('Ctrl Pts',(9.65805413299995,15.2,-4.07103413800002));
#181385=CARTESIAN_POINT('Ctrl Pts',(9.65805413299995,11.6,-4.07103413800002));
#181386=CARTESIAN_POINT('Ctrl Pts',(9.65963866699994,15.2,-4.07140894900001));
#181387=CARTESIAN_POINT('Ctrl Pts',(9.65963866699994,11.6,-4.07140894900001));
#181388=CARTESIAN_POINT('Ctrl Pts',(9.66123114799995,15.2,-4.07178406500002));
#181389=CARTESIAN_POINT('Ctrl Pts',(9.66123114799995,11.6,-4.07178406500002));
#181390=CARTESIAN_POINT('Ctrl Pts',(9.66283156199994,15.2,-4.07215947000001));
#181391=CARTESIAN_POINT('Ctrl Pts',(9.66283156199994,11.6,-4.07215947000001));
#181392=CARTESIAN_POINT('Ctrl Pts',(9.66443989499994,15.2,-4.07253514700002));
#181393=CARTESIAN_POINT('Ctrl Pts',(9.66443989499994,11.6,-4.07253514700002));
#181394=CARTESIAN_POINT('Ctrl Pts',(9.66605613099994,15.2,-4.07291107800001));
#181395=CARTESIAN_POINT('Ctrl Pts',(9.66605613099994,11.6,-4.07291107800001));
#181396=CARTESIAN_POINT('Ctrl Pts',(9.66768025599994,15.2,-4.07328724600001));
#181397=CARTESIAN_POINT('Ctrl Pts',(9.66768025599994,11.6,-4.07328724600002));
#181398=CARTESIAN_POINT('Ctrl Pts',(9.66931225499994,15.2,-4.07366363600001));
#181399=CARTESIAN_POINT('Ctrl Pts',(9.66931225499994,11.6,-4.07366363600001));
#181400=CARTESIAN_POINT('Ctrl Pts',(9.67095211399995,15.2,-4.07404022700002));
#181401=CARTESIAN_POINT('Ctrl Pts',(9.67095211399995,11.6,-4.07404022700002));
#181402=CARTESIAN_POINT('Ctrl Pts',(9.67259981799995,15.2,-4.07441700600002));
#181403=CARTESIAN_POINT('Ctrl Pts',(9.67259981799995,11.6,-4.07441700600002));
#181404=CARTESIAN_POINT('Ctrl Pts',(9.67425535199995,15.2,-4.07479395500001));
#181405=CARTESIAN_POINT('Ctrl Pts',(9.67425535199995,11.6,-4.07479395500001));
#181406=CARTESIAN_POINT('Ctrl Pts',(9.67591870099995,15.2,-4.07517105700002));
#181407=CARTESIAN_POINT('Ctrl Pts',(9.67591870099995,11.6,-4.07517105700002));
#181408=CARTESIAN_POINT('Ctrl Pts',(9.67758985199995,15.2,-4.07554829600001));
#181409=CARTESIAN_POINT('Ctrl Pts',(9.67758985199995,11.6,-4.07554829600001));
#181410=CARTESIAN_POINT('Ctrl Pts',(9.67926879099995,15.2,-4.07592565400002));
#181411=CARTESIAN_POINT('Ctrl Pts',(9.67926879099995,11.6,-4.07592565400002));
#181412=CARTESIAN_POINT('Ctrl Pts',(9.68095550199994,15.2,-4.07630311500002));
#181413=CARTESIAN_POINT('Ctrl Pts',(9.68095550199994,11.6,-4.07630311500002));
#181414=CARTESIAN_POINT('Ctrl Pts',(9.68264997199995,15.2,-4.07668066400001));
#181415=CARTESIAN_POINT('Ctrl Pts',(9.68264997199995,11.6,-4.07668066400001));
#181416=CARTESIAN_POINT('Ctrl Pts',(9.68435218499994,15.2,-4.07705828300001));
#181417=CARTESIAN_POINT('Ctrl Pts',(9.68435218499994,11.6,-4.07705828300002));
#181418=CARTESIAN_POINT('Ctrl Pts',(9.68606212899994,15.2,-4.07743595700001));
#181419=CARTESIAN_POINT('Ctrl Pts',(9.68606212899994,11.6,-4.07743595700001));
#181420=CARTESIAN_POINT('Ctrl Pts',(9.68777978799995,15.2,-4.07781366900001));
#181421=CARTESIAN_POINT('Ctrl Pts',(9.68777978799995,11.6,-4.07781366900002));
#181422=CARTESIAN_POINT('Ctrl Pts',(9.68950514999994,15.2,-4.07819140300001));
#181423=CARTESIAN_POINT('Ctrl Pts',(9.68950514999994,11.6,-4.07819140300001));
#181424=CARTESIAN_POINT('Ctrl Pts',(9.69123819799995,15.2,-4.07856914300002));
#181425=CARTESIAN_POINT('Ctrl Pts',(9.69123819799995,11.6,-4.07856914300002));
#181426=CARTESIAN_POINT('Ctrl Pts',(9.69297891999994,15.2,-4.07894687300002));
#181427=CARTESIAN_POINT('Ctrl Pts',(9.69297891999994,11.6,-4.07894687300002));
#181428=CARTESIAN_POINT('Ctrl Pts',(9.69472730099995,15.2,-4.07932457800001));
#181429=CARTESIAN_POINT('Ctrl Pts',(9.69472730099995,11.6,-4.07932457800001));
#181430=CARTESIAN_POINT('Ctrl Pts',(9.69648332799995,15.2,-4.07970224000001));
#181431=CARTESIAN_POINT('Ctrl Pts',(9.69648332799995,11.6,-4.07970224000001));
#181432=CARTESIAN_POINT('Ctrl Pts',(9.69824698699994,15.2,-4.08007984400002));
#181433=CARTESIAN_POINT('Ctrl Pts',(9.69824698699994,11.6,-4.08007984400002));
#181434=CARTESIAN_POINT('Ctrl Pts',(9.70001826299994,15.2,-4.08045737500002));
#181435=CARTESIAN_POINT('Ctrl Pts',(9.70001826299994,11.6,-4.08045737500002));
#181436=CARTESIAN_POINT('Ctrl Pts',(9.70179714199995,15.2,-4.08083481700002));
#181437=CARTESIAN_POINT('Ctrl Pts',(9.70179714199995,11.6,-4.08083481700002));
#181438=CARTESIAN_POINT('Ctrl Pts',(9.70358361299994,15.2,-4.08121215500001));
#181439=CARTESIAN_POINT('Ctrl Pts',(9.70358361299994,11.6,-4.08121215500001));
#181440=CARTESIAN_POINT('Ctrl Pts',(9.70537765899994,15.2,-4.08158937200001));
#181441=CARTESIAN_POINT('Ctrl Pts',(9.70537765899994,11.6,-4.08158937200001));
#181442=CARTESIAN_POINT('Ctrl Pts',(9.70717926699994,15.2,-4.08196645300002));
#181443=CARTESIAN_POINT('Ctrl Pts',(9.70717926699994,11.6,-4.08196645300002));
#181444=CARTESIAN_POINT('Ctrl Pts',(9.70898842499994,15.2,-4.08234338300002));
#181445=CARTESIAN_POINT('Ctrl Pts',(9.70898842499994,11.6,-4.08234338300002));
#181446=CARTESIAN_POINT('Ctrl Pts',(9.71080511699994,15.2,-4.08272014700001));
#181447=CARTESIAN_POINT('Ctrl Pts',(9.71080511699994,11.6,-4.08272014700001));
#181448=CARTESIAN_POINT('Ctrl Pts',(9.71262933199995,15.2,-4.08309672800002));
#181449=CARTESIAN_POINT('Ctrl Pts',(9.71262933199995,11.6,-4.08309672800002));
#181450=CARTESIAN_POINT('Ctrl Pts',(9.71446105399994,15.2,-4.08347311300002));
#181451=CARTESIAN_POINT('Ctrl Pts',(9.71446105399994,11.6,-4.08347311300002));
#181452=CARTESIAN_POINT('Ctrl Pts',(9.71630027099994,15.2,-4.08384928600002));
#181453=CARTESIAN_POINT('Ctrl Pts',(9.71630027099994,11.6,-4.08384928600002));
#181454=CARTESIAN_POINT('Ctrl Pts',(9.71814696899994,15.2,-4.08422523100001));
#181455=CARTESIAN_POINT('Ctrl Pts',(9.71814696899994,11.6,-4.08422523100001));
#181456=CARTESIAN_POINT('Ctrl Pts',(9.72000113399995,15.2,-4.08460093400001));
#181457=CARTESIAN_POINT('Ctrl Pts',(9.72000113399995,11.6,-4.08460093400001));
#181458=CARTESIAN_POINT('Ctrl Pts',(9.72186275299994,15.2,-4.08497637900001));
#181459=CARTESIAN_POINT('Ctrl Pts',(9.72186275299994,11.6,-4.08497637900001));
#181460=CARTESIAN_POINT('Ctrl Pts',(9.72373181399995,15.2,-4.08535155200001));
#181461=CARTESIAN_POINT('Ctrl Pts',(9.72373181399995,11.6,-4.08535155200001));
#181462=CARTESIAN_POINT('Ctrl Pts',(9.72560830199994,15.2,-4.08572643800001));
#181463=CARTESIAN_POINT('Ctrl Pts',(9.72560830199994,11.6,-4.08572643800001));
#181464=CARTESIAN_POINT('Ctrl Pts',(9.72749220299994,15.2,-4.08610102200001));
#181465=CARTESIAN_POINT('Ctrl Pts',(9.72749220299994,11.6,-4.08610102200001));
#181466=CARTESIAN_POINT('Ctrl Pts',(9.72938350499994,15.2,-4.08647528800001));
#181467=CARTESIAN_POINT('Ctrl Pts',(9.72938350499994,11.6,-4.08647528800001));
#181468=CARTESIAN_POINT('Ctrl Pts',(9.73128219499995,15.2,-4.08684922400001));
#181469=CARTESIAN_POINT('Ctrl Pts',(9.73128219499995,11.6,-4.08684922400001));
#181470=CARTESIAN_POINT('Ctrl Pts',(9.73318825999995,15.2,-4.08722281400001));
#181471=CARTESIAN_POINT('Ctrl Pts',(9.73318825999995,11.6,-4.08722281400001));
#181472=CARTESIAN_POINT('Ctrl Pts',(9.73510168599995,15.2,-4.08759604300001));
#181473=CARTESIAN_POINT('Ctrl Pts',(9.73510168599995,11.6,-4.08759604300002));
#181474=CARTESIAN_POINT('Ctrl Pts',(9.73702245899995,15.2,-4.08796889700001));
#181475=CARTESIAN_POINT('Ctrl Pts',(9.73702245899995,11.6,-4.08796889700001));
#181476=CARTESIAN_POINT('Ctrl Pts',(9.73895056799994,15.2,-4.08834136100001));
#181477=CARTESIAN_POINT('Ctrl Pts',(9.73895056799994,11.6,-4.08834136100001));
#181478=CARTESIAN_POINT('Ctrl Pts',(9.74088599799994,15.2,-4.08871342100001));
#181479=CARTESIAN_POINT('Ctrl Pts',(9.74088599799994,11.6,-4.08871342100001));
#181480=CARTESIAN_POINT('Ctrl Pts',(9.74282873799994,15.2,-4.08908506300001));
#181481=CARTESIAN_POINT('Ctrl Pts',(9.74282873799994,11.6,-4.08908506300001));
#181482=CARTESIAN_POINT('Ctrl Pts',(9.74477877399995,15.2,-4.08945627200001));
#181483=CARTESIAN_POINT('Ctrl Pts',(9.74477877399995,11.6,-4.08945627200001));
#181484=CARTESIAN_POINT('Ctrl Pts',(9.74673609199994,15.2,-4.08982703400001));
#181485=CARTESIAN_POINT('Ctrl Pts',(9.74673609199994,11.6,-4.08982703400001));
#181486=CARTESIAN_POINT('Ctrl Pts',(9.74870068199994,15.2,-4.09019733600001));
#181487=CARTESIAN_POINT('Ctrl Pts',(9.74870068199994,11.6,-4.09019733600002));
#181488=CARTESIAN_POINT('Ctrl Pts',(9.75067252699995,15.2,-4.09056716100002));
#181489=CARTESIAN_POINT('Ctrl Pts',(9.75067252699995,11.6,-4.09056716100002));
#181490=CARTESIAN_POINT('Ctrl Pts',(9.75265161799994,15.2,-4.09093649800001));
#181491=CARTESIAN_POINT('Ctrl Pts',(9.75265161799994,11.6,-4.09093649800001));
#181492=CARTESIAN_POINT('Ctrl Pts',(9.75463793899995,15.2,-4.09130533200001));
#181493=CARTESIAN_POINT('Ctrl Pts',(9.75463793899995,11.6,-4.09130533200001));
#181494=CARTESIAN_POINT('Ctrl Pts',(9.75663147999994,15.2,-4.09167364900001));
#181495=CARTESIAN_POINT('Ctrl Pts',(9.75663147999994,11.6,-4.09167364900001));
#181496=CARTESIAN_POINT('Ctrl Pts',(9.75863222799994,15.2,-4.09204143300002));
#181497=CARTESIAN_POINT('Ctrl Pts',(9.75863222799994,11.6,-4.09204143300002));
#181498=CARTESIAN_POINT('Ctrl Pts',(9.76064016799995,15.2,-4.09240867300001));
#181499=CARTESIAN_POINT('Ctrl Pts',(9.76064016799995,11.6,-4.09240867300001));
#181500=CARTESIAN_POINT('Ctrl Pts',(9.76265528799994,15.2,-4.09277535500001));
#181501=CARTESIAN_POINT('Ctrl Pts',(9.76265528799994,11.6,-4.09277535500001));
#181502=CARTESIAN_POINT('Ctrl Pts',(9.76467757799995,15.2,-4.09314146400002));
#181503=CARTESIAN_POINT('Ctrl Pts',(9.76467757799995,11.6,-4.09314146400002));
#181504=CARTESIAN_POINT('Ctrl Pts',(9.76670702199995,15.2,-4.09350698700001));
#181505=CARTESIAN_POINT('Ctrl Pts',(9.76670702199995,11.6,-4.09350698700001));
#181506=CARTESIAN_POINT('Ctrl Pts',(9.76874360999994,15.2,-4.09387191000001));
#181507=CARTESIAN_POINT('Ctrl Pts',(9.76874360999994,11.6,-4.09387191000001));
#181508=CARTESIAN_POINT('Ctrl Pts',(9.77078732699994,15.2,-4.09423622000002));
#181509=CARTESIAN_POINT('Ctrl Pts',(9.77078732699994,11.6,-4.09423622000002));
#181510=CARTESIAN_POINT('Ctrl Pts',(9.77283816299994,15.2,-4.09459990300002));
#181511=CARTESIAN_POINT('Ctrl Pts',(9.77283816299994,11.6,-4.09459990300002));
#181512=CARTESIAN_POINT('Ctrl Pts',(9.77489610299994,15.2,-4.09496294400002));
#181513=CARTESIAN_POINT('Ctrl Pts',(9.77489610299994,11.6,-4.09496294400002));
#181514=CARTESIAN_POINT('Ctrl Pts',(9.77696113599994,15.2,-4.09532533300002));
#181515=CARTESIAN_POINT('Ctrl Pts',(9.77696113599994,11.6,-4.09532533300002));
#181516=CARTESIAN_POINT('Ctrl Pts',(9.77903324999994,15.2,-4.09568705400002));
#181517=CARTESIAN_POINT('Ctrl Pts',(9.77903324999994,11.6,-4.09568705400002));
#181518=CARTESIAN_POINT('Ctrl Pts',(9.78111243199994,15.2,-4.09604809500001));
#181519=CARTESIAN_POINT('Ctrl Pts',(9.78111243199994,11.6,-4.09604809500001));
#181520=CARTESIAN_POINT('Ctrl Pts',(9.78319866899995,15.2,-4.09640844200001));
#181521=CARTESIAN_POINT('Ctrl Pts',(9.78319866899995,11.6,-4.09640844200002));
#181522=CARTESIAN_POINT('Ctrl Pts',(9.78529195099994,15.2,-4.09676808200001));
#181523=CARTESIAN_POINT('Ctrl Pts',(9.78529195099994,11.6,-4.09676808200001));
#181524=CARTESIAN_POINT('Ctrl Pts',(9.78739226299994,15.2,-4.09712700200001));
#181525=CARTESIAN_POINT('Ctrl Pts',(9.78739226299994,11.6,-4.09712700200001));
#181526=CARTESIAN_POINT('Ctrl Pts',(9.78949959499994,15.2,-4.09748518800002));
#181527=CARTESIAN_POINT('Ctrl Pts',(9.78949959499994,11.6,-4.09748518800002));
#181528=CARTESIAN_POINT('Ctrl Pts',(9.79161393199995,15.2,-4.09784262900001));
#181529=CARTESIAN_POINT('Ctrl Pts',(9.79161393199995,11.6,-4.09784262900002));
#181530=CARTESIAN_POINT('Ctrl Pts',(9.79373526299995,15.2,-4.09819930900001));
#181531=CARTESIAN_POINT('Ctrl Pts',(9.79373526299995,11.6,-4.09819930900001));
#181532=CARTESIAN_POINT('Ctrl Pts',(9.79586357799995,15.2,-4.09855521700001));
#181533=CARTESIAN_POINT('Ctrl Pts',(9.79586357799995,11.6,-4.09855521700001));
#181534=CARTESIAN_POINT('Ctrl Pts',(9.79799886199994,15.2,-4.09891034100001));
#181535=CARTESIAN_POINT('Ctrl Pts',(9.79799886199994,11.6,-4.09891034100002));
#181536=CARTESIAN_POINT('Ctrl Pts',(9.80014110399994,15.2,-4.09926466500002));
#181537=CARTESIAN_POINT('Ctrl Pts',(9.80014110399994,11.6,-4.09926466500002));
#181538=CARTESIAN_POINT('Ctrl Pts',(9.80229029299995,15.2,-4.09961817900002));
#181539=CARTESIAN_POINT('Ctrl Pts',(9.80229029299995,11.6,-4.09961817900002));
#181540=CARTESIAN_POINT('Ctrl Pts',(9.80444641399994,15.2,-4.09997086900002));
#181541=CARTESIAN_POINT('Ctrl Pts',(9.80444641399994,11.6,-4.09997086900002));
#181542=CARTESIAN_POINT('Ctrl Pts',(9.80660945899994,15.2,-4.10032272200001));
#181543=CARTESIAN_POINT('Ctrl Pts',(9.80660945899994,11.6,-4.10032272200001));
#181544=CARTESIAN_POINT('Ctrl Pts',(9.80877941099994,15.2,-4.10067372700002));
#181545=CARTESIAN_POINT('Ctrl Pts',(9.80877941099994,11.6,-4.10067372700002));
#181546=CARTESIAN_POINT('Ctrl Pts',(9.81095626399994,15.2,-4.10102387000002));
#181547=CARTESIAN_POINT('Ctrl Pts',(9.81095626399994,11.6,-4.10102387000002));
#181548=CARTESIAN_POINT('Ctrl Pts',(9.81313999999994,15.2,-4.10137313700002));
#181549=CARTESIAN_POINT('Ctrl Pts',(9.81313999999994,11.6,-4.10137313700002));
#181550=CARTESIAN_POINT('Ctrl Pts',(9.81533061199995,15.2,-4.10172151900001));
#181551=CARTESIAN_POINT('Ctrl Pts',(9.81533061199995,11.6,-4.10172151900001));
#181552=CARTESIAN_POINT('Ctrl Pts',(9.81752808499994,15.2,-4.10206900100002));
#181553=CARTESIAN_POINT('Ctrl Pts',(9.81752808499994,11.6,-4.10206900100002));
#181554=CARTESIAN_POINT('Ctrl Pts',(9.81973240799995,15.2,-4.10241557000001));
#181555=CARTESIAN_POINT('Ctrl Pts',(9.81973240799995,11.6,-4.10241557000001));
#181556=CARTESIAN_POINT('Ctrl Pts',(9.82194356999995,15.2,-4.10276121500001));
#181557=CARTESIAN_POINT('Ctrl Pts',(9.82194356999995,11.6,-4.10276121500001));
#181558=CARTESIAN_POINT('Ctrl Pts',(9.82416155899994,15.2,-4.10310592400001));
#181559=CARTESIAN_POINT('Ctrl Pts',(9.82416155899994,11.6,-4.10310592400002));
#181560=CARTESIAN_POINT('Ctrl Pts',(9.82638636299994,15.2,-4.10344968500001));
#181561=CARTESIAN_POINT('Ctrl Pts',(9.82638636299994,11.6,-4.10344968500001));
#181562=CARTESIAN_POINT('Ctrl Pts',(9.82861796899994,15.2,-4.10379248300002));
#181563=CARTESIAN_POINT('Ctrl Pts',(9.82861796899994,11.6,-4.10379248300002));
#181564=CARTESIAN_POINT('Ctrl Pts',(9.83085636699995,15.2,-4.10413430800002));
#181565=CARTESIAN_POINT('Ctrl Pts',(9.83085636699995,11.6,-4.10413430800002));
#181566=CARTESIAN_POINT('Ctrl Pts',(9.83310154499994,15.2,-4.10447514700001));
#181567=CARTESIAN_POINT('Ctrl Pts',(9.83310154499994,11.6,-4.10447514700001));
#181568=CARTESIAN_POINT('Ctrl Pts',(9.83535349099995,15.2,-4.10481498900001));
#181569=CARTESIAN_POINT('Ctrl Pts',(9.83535349099995,11.6,-4.10481498900001));
#181570=CARTESIAN_POINT('Ctrl Pts',(9.83761219299994,15.2,-4.10515382000002));
#181571=CARTESIAN_POINT('Ctrl Pts',(9.83761219299994,11.6,-4.10515382000002));
#181572=CARTESIAN_POINT('Ctrl Pts',(9.83987763999994,15.2,-4.10549163000002));
#181573=CARTESIAN_POINT('Ctrl Pts',(9.83987763999994,11.6,-4.10549163000002));
#181574=CARTESIAN_POINT('Ctrl Pts',(9.84214981999994,15.2,-4.10582840600001));
#181575=CARTESIAN_POINT('Ctrl Pts',(9.84214981999994,11.6,-4.10582840600001));
#181576=CARTESIAN_POINT('Ctrl Pts',(9.84442872299994,15.2,-4.10616413700001));
#181577=CARTESIAN_POINT('Ctrl Pts',(9.84442872299994,11.6,-4.10616413700002));
#181578=CARTESIAN_POINT('Ctrl Pts',(9.84671433499994,15.2,-4.10649880800001));
#181579=CARTESIAN_POINT('Ctrl Pts',(9.84671433499994,11.6,-4.10649880800001));
#181580=CARTESIAN_POINT('Ctrl Pts',(9.84900664499994,15.2,-4.10683241100001));
#181581=CARTESIAN_POINT('Ctrl Pts',(9.84900664499994,11.6,-4.10683241100002));
#181582=CARTESIAN_POINT('Ctrl Pts',(9.85130564399994,15.2,-4.10716493200002));
#181583=CARTESIAN_POINT('Ctrl Pts',(9.85130564399994,11.6,-4.10716493200002));
#181584=CARTESIAN_POINT('Ctrl Pts',(9.85361131799995,15.2,-4.10749636000002));
#181585=CARTESIAN_POINT('Ctrl Pts',(9.85361131799995,11.6,-4.10749636000002));
#181586=CARTESIAN_POINT('Ctrl Pts',(9.85592365599994,15.2,-4.10782668300001));
#181587=CARTESIAN_POINT('Ctrl Pts',(9.85592365599994,11.6,-4.10782668300001));
#181588=CARTESIAN_POINT('Ctrl Pts',(9.85824264599995,15.2,-4.10815588900002));
#181589=CARTESIAN_POINT('Ctrl Pts',(9.85824264599995,11.6,-4.10815588900002));
#181590=CARTESIAN_POINT('Ctrl Pts',(9.86056827899995,15.2,-4.10848396600001));
#181591=CARTESIAN_POINT('Ctrl Pts',(9.86056827899995,11.6,-4.10848396600001));
#181592=CARTESIAN_POINT('Ctrl Pts',(9.86290054199995,15.2,-4.10881090400002));
#181593=CARTESIAN_POINT('Ctrl Pts',(9.86290054199995,11.6,-4.10881090400002));
#181594=CARTESIAN_POINT('Ctrl Pts',(9.86523942299995,15.2,-4.10913669000001));
#181595=CARTESIAN_POINT('Ctrl Pts',(9.86523942299995,11.6,-4.10913669000002));
#181596=CARTESIAN_POINT('Ctrl Pts',(9.86758491299994,15.2,-4.10946131300001));
#181597=CARTESIAN_POINT('Ctrl Pts',(9.86758491299994,11.6,-4.10946131300001));
#181598=CARTESIAN_POINT('Ctrl Pts',(9.86993699799994,15.2,-4.10978476100002));
#181599=CARTESIAN_POINT('Ctrl Pts',(9.86993699799994,11.6,-4.10978476100002));
#181600=CARTESIAN_POINT('Ctrl Pts',(9.87229566899994,15.2,-4.11010702400001));
#181601=CARTESIAN_POINT('Ctrl Pts',(9.87229566899994,11.6,-4.11010702400001));
#181602=CARTESIAN_POINT('Ctrl Pts',(9.87466091299994,15.2,-4.11042808800001));
#181603=CARTESIAN_POINT('Ctrl Pts',(9.87466091299994,11.6,-4.11042808800001));
#181604=CARTESIAN_POINT('Ctrl Pts',(9.87703271999995,15.2,-4.11074794500002));
#181605=CARTESIAN_POINT('Ctrl Pts',(9.87703271999995,11.6,-4.11074794500002));
#181606=CARTESIAN_POINT('Ctrl Pts',(9.87941107799994,15.2,-4.11106658100001));
#181607=CARTESIAN_POINT('Ctrl Pts',(9.87941107799994,11.6,-4.11106658100001));
#181608=CARTESIAN_POINT('Ctrl Pts',(9.88179597699995,15.2,-4.11138398500002));
#181609=CARTESIAN_POINT('Ctrl Pts',(9.88179597699995,11.6,-4.11138398500002));
#181610=CARTESIAN_POINT('Ctrl Pts',(9.88418740499995,15.2,-4.11170014600001));
#181611=CARTESIAN_POINT('Ctrl Pts',(9.88418740499995,11.6,-4.11170014600002));
#181612=CARTESIAN_POINT('Ctrl Pts',(9.88658535099994,15.2,-4.11201505500001));
#181613=CARTESIAN_POINT('Ctrl Pts',(9.88658535099994,11.6,-4.11201505500001));
#181614=CARTESIAN_POINT('Ctrl Pts',(9.88898980499994,15.2,-4.11232869700001));
#181615=CARTESIAN_POINT('Ctrl Pts',(9.88898980499994,11.6,-4.11232869700001));
#181616=CARTESIAN_POINT('Ctrl Pts',(9.89140075299994,15.2,-4.11264106400001));
#181617=CARTESIAN_POINT('Ctrl Pts',(9.89140075299994,11.6,-4.11264106400001));
#181618=CARTESIAN_POINT('Ctrl Pts',(9.89381818699995,15.2,-4.11295214400001));
#181619=CARTESIAN_POINT('Ctrl Pts',(9.89381818699995,11.6,-4.11295214400001));
#181620=CARTESIAN_POINT('Ctrl Pts',(9.89624209499994,15.2,-4.11326192500002));
#181621=CARTESIAN_POINT('Ctrl Pts',(9.89624209499994,11.6,-4.11326192500002));
#181622=CARTESIAN_POINT('Ctrl Pts',(9.89867246499994,15.2,-4.11357039600002));
#181623=CARTESIAN_POINT('Ctrl Pts',(9.89867246499994,11.6,-4.11357039600002));
#181624=CARTESIAN_POINT('Ctrl Pts',(9.90110928899995,15.2,-4.11387754800002));
#181625=CARTESIAN_POINT('Ctrl Pts',(9.90110928899995,11.6,-4.11387754800002));
#181626=CARTESIAN_POINT('Ctrl Pts',(9.90355255199994,15.2,-4.11418336800002));
#181627=CARTESIAN_POINT('Ctrl Pts',(9.90355255199994,11.6,-4.11418336800002));
#181628=CARTESIAN_POINT('Ctrl Pts',(9.90600224599994,15.2,-4.11448784500001));
#181629=CARTESIAN_POINT('Ctrl Pts',(9.90600224599994,11.6,-4.11448784500002));
#181630=CARTESIAN_POINT('Ctrl Pts',(9.90845835999994,15.2,-4.11479097000001));
#181631=CARTESIAN_POINT('Ctrl Pts',(9.90845835999994,11.6,-4.11479097000001));
#181632=CARTESIAN_POINT('Ctrl Pts',(9.91092088199995,15.2,-4.11509273100001));
#181633=CARTESIAN_POINT('Ctrl Pts',(9.91092088199995,11.6,-4.11509273100001));
#181634=CARTESIAN_POINT('Ctrl Pts',(9.91338980099994,15.2,-4.11539311700002));
#181635=CARTESIAN_POINT('Ctrl Pts',(9.91338980099994,11.6,-4.11539311700002));
#181636=CARTESIAN_POINT('Ctrl Pts',(9.91586510599994,15.2,-4.11569211800002));
#181637=CARTESIAN_POINT('Ctrl Pts',(9.91586510599994,11.6,-4.11569211800002));
#181638=CARTESIAN_POINT('Ctrl Pts',(9.91834678799994,15.2,-4.11598972400002));
#181639=CARTESIAN_POINT('Ctrl Pts',(9.91834678799994,11.6,-4.11598972400002));
#181640=CARTESIAN_POINT('Ctrl Pts',(9.92083483399995,15.2,-4.11628592200001));
#181641=CARTESIAN_POINT('Ctrl Pts',(9.92083483399995,11.6,-4.11628592200001));
#181642=CARTESIAN_POINT('Ctrl Pts',(9.92332923599994,15.2,-4.11658070200001));
#181643=CARTESIAN_POINT('Ctrl Pts',(9.92332923599994,11.6,-4.11658070200002));
#181644=CARTESIAN_POINT('Ctrl Pts',(9.92582998099994,15.2,-4.11687405500002));
#181645=CARTESIAN_POINT('Ctrl Pts',(9.92582998099994,11.6,-4.11687405500002));
#181646=CARTESIAN_POINT('Ctrl Pts',(9.92833705899995,15.2,-4.11716596900002));
#181647=CARTESIAN_POINT('Ctrl Pts',(9.92833705899995,11.6,-4.11716596900002));
#181648=CARTESIAN_POINT('Ctrl Pts',(9.93085045799995,15.2,-4.11745643400002));
#181649=CARTESIAN_POINT('Ctrl Pts',(9.93085045799995,11.6,-4.11745643400002));
#181650=CARTESIAN_POINT('Ctrl Pts',(9.93337016999994,15.2,-4.11774544000002));
#181651=CARTESIAN_POINT('Ctrl Pts',(9.93337016999994,11.6,-4.11774544000002));
#181652=CARTESIAN_POINT('Ctrl Pts',(9.93589618199995,15.2,-4.11803297500001));
#181653=CARTESIAN_POINT('Ctrl Pts',(9.93589618199995,11.6,-4.11803297500002));
#181654=CARTESIAN_POINT('Ctrl Pts',(9.93842848399994,15.2,-4.11831903000001));
#181655=CARTESIAN_POINT('Ctrl Pts',(9.93842848399994,11.6,-4.11831903000001));
#181656=CARTESIAN_POINT('Ctrl Pts',(9.94096706699995,15.2,-4.11860359400002));
#181657=CARTESIAN_POINT('Ctrl Pts',(9.94096706699995,11.6,-4.11860359400002));
#181658=CARTESIAN_POINT('Ctrl Pts',(9.94351191899994,15.2,-4.11888665700001));
#181659=CARTESIAN_POINT('Ctrl Pts',(9.94351191899994,11.6,-4.11888665700001));
#181660=CARTESIAN_POINT('Ctrl Pts',(9.94606302899994,15.2,-4.11916820900001));
#181661=CARTESIAN_POINT('Ctrl Pts',(9.94606302899994,11.6,-4.11916820900002));
#181662=CARTESIAN_POINT('Ctrl Pts',(9.94862038599994,15.2,-4.11944823900001));
#181663=CARTESIAN_POINT('Ctrl Pts',(9.94862038599994,11.6,-4.11944823900001));
#181664=CARTESIAN_POINT('Ctrl Pts',(9.95118398199994,15.2,-4.11972673700001));
#181665=CARTESIAN_POINT('Ctrl Pts',(9.95118398199994,11.6,-4.11972673700001));
#181666=CARTESIAN_POINT('Ctrl Pts',(9.95375380499994,15.2,-4.12000369300001));
#181667=CARTESIAN_POINT('Ctrl Pts',(9.95375380499994,11.6,-4.12000369300001));
#181668=CARTESIAN_POINT('Ctrl Pts',(9.95632984299995,15.2,-4.12027909500001));
#181669=CARTESIAN_POINT('Ctrl Pts',(9.95632984299995,11.6,-4.12027909500001));
#181670=CARTESIAN_POINT('Ctrl Pts',(9.95891208799994,15.2,-4.12055293600002));
#181671=CARTESIAN_POINT('Ctrl Pts',(9.95891208799994,11.6,-4.12055293600002));
#181672=CARTESIAN_POINT('Ctrl Pts',(9.96150052899995,15.2,-4.12082520400002));
#181673=CARTESIAN_POINT('Ctrl Pts',(9.96150052899995,11.6,-4.12082520400002));
#181674=CARTESIAN_POINT('Ctrl Pts',(9.96409515399994,15.2,-4.12109589000002));
#181675=CARTESIAN_POINT('Ctrl Pts',(9.96409515399994,11.6,-4.12109589000002));
#181676=CARTESIAN_POINT('Ctrl Pts',(9.96669595399995,15.2,-4.12136498300002));
#181677=CARTESIAN_POINT('Ctrl Pts',(9.96669595399995,11.6,-4.12136498300002));
#181678=CARTESIAN_POINT('Ctrl Pts',(9.96930291999995,15.2,-4.12163247300001));
#181679=CARTESIAN_POINT('Ctrl Pts',(9.96930291999995,11.6,-4.12163247300002));
#181680=CARTESIAN_POINT('Ctrl Pts',(9.97191603899994,15.2,-4.12189835100001));
#181681=CARTESIAN_POINT('Ctrl Pts',(9.97191603899994,11.6,-4.12189835100001));
#181682=CARTESIAN_POINT('Ctrl Pts',(9.97453530099994,15.2,-4.12216260600001));
#181683=CARTESIAN_POINT('Ctrl Pts',(9.97453530099994,11.6,-4.12216260600002));
#181684=CARTESIAN_POINT('Ctrl Pts',(9.97716069799995,15.2,-4.12242522700002));
#181685=CARTESIAN_POINT('Ctrl Pts',(9.97716069799995,11.6,-4.12242522700002));
#181686=CARTESIAN_POINT('Ctrl Pts',(9.97979221599994,15.2,-4.12268620700001));
#181687=CARTESIAN_POINT('Ctrl Pts',(9.97979221599994,11.6,-4.12268620700001));
#181688=CARTESIAN_POINT('Ctrl Pts',(9.98242984799995,15.2,-4.12294553500002));
#181689=CARTESIAN_POINT('Ctrl Pts',(9.98242984799995,11.6,-4.12294553500002));
#181690=CARTESIAN_POINT('Ctrl Pts',(9.98507358299995,15.2,-4.12320320100001));
#181691=CARTESIAN_POINT('Ctrl Pts',(9.98507358299995,11.6,-4.12320320100002));
#181692=CARTESIAN_POINT('Ctrl Pts',(9.98772340999994,15.2,-4.12345919500002));
#181693=CARTESIAN_POINT('Ctrl Pts',(9.98772340999994,11.6,-4.12345919500002));
#181694=CARTESIAN_POINT('Ctrl Pts',(9.99037931799995,15.2,-4.12371350600001));
#181695=CARTESIAN_POINT('Ctrl Pts',(9.99037931799995,11.6,-4.12371350600001));
#181696=CARTESIAN_POINT('Ctrl Pts',(9.99304129899994,15.2,-4.12396612800002));
#181697=CARTESIAN_POINT('Ctrl Pts',(9.99304129899994,11.6,-4.12396612800002));
#181698=CARTESIAN_POINT('Ctrl Pts',(9.99570934199994,15.2,-4.12421704800002));
#181699=CARTESIAN_POINT('Ctrl Pts',(9.99570934199994,11.6,-4.12421704800002));
#181700=CARTESIAN_POINT('Ctrl Pts',(9.99838343599994,15.2,-4.12446625800001));
#181701=CARTESIAN_POINT('Ctrl Pts',(9.99838343599994,11.6,-4.12446625800001));
#181702=CARTESIAN_POINT('Ctrl Pts',(10.0010635709999,15.2,-4.12471374800001));
#181703=CARTESIAN_POINT('Ctrl Pts',(10.0010635709999,11.6,-4.12471374800001));
#181704=CARTESIAN_POINT('Ctrl Pts',(10.0037497379999,15.2,-4.12495950800002));
#181705=CARTESIAN_POINT('Ctrl Pts',(10.0037497379999,11.6,-4.12495950800002));
#181706=CARTESIAN_POINT('Ctrl Pts',(10.0064419259999,15.2,-4.12520352800001));
#181707=CARTESIAN_POINT('Ctrl Pts',(10.0064419259999,11.6,-4.12520352800002));
#181708=CARTESIAN_POINT('Ctrl Pts',(10.0091401249999,15.2,-4.12544580100001));
#181709=CARTESIAN_POINT('Ctrl Pts',(10.0091401249999,11.6,-4.12544580100001));
#181710=CARTESIAN_POINT('Ctrl Pts',(10.0118443249999,15.2,-4.12568631400001));
#181711=CARTESIAN_POINT('Ctrl Pts',(10.0118443249999,11.6,-4.12568631400002));
#181712=CARTESIAN_POINT('Ctrl Pts',(10.0145545159999,15.2,-4.12592506000002));
#181713=CARTESIAN_POINT('Ctrl Pts',(10.0145545159999,11.6,-4.12592506000002));
#181714=CARTESIAN_POINT('Ctrl Pts',(10.0172706879999,15.2,-4.12616202900002));
#181715=CARTESIAN_POINT('Ctrl Pts',(10.0172706879999,11.6,-4.12616202900002));
#181716=CARTESIAN_POINT('Ctrl Pts',(10.0199928309999,15.2,-4.12639721200001));
#181717=CARTESIAN_POINT('Ctrl Pts',(10.0199928309999,11.6,-4.12639721200002));
#181718=CARTESIAN_POINT('Ctrl Pts',(10.0227209349999,15.2,-4.12663059800002));
#181719=CARTESIAN_POINT('Ctrl Pts',(10.0227209349999,11.6,-4.12663059800002));
#181720=CARTESIAN_POINT('Ctrl Pts',(10.0254549889999,15.2,-4.12686218000001));
#181721=CARTESIAN_POINT('Ctrl Pts',(10.0254549889999,11.6,-4.12686218000002));
#181722=CARTESIAN_POINT('Ctrl Pts',(10.0281949849999,15.2,-4.12709194800001));
#181723=CARTESIAN_POINT('Ctrl Pts',(10.0281949849999,11.6,-4.12709194800002));
#181724=CARTESIAN_POINT('Ctrl Pts',(10.0309409119999,15.2,-4.12731989100001));
#181725=CARTESIAN_POINT('Ctrl Pts',(10.0309409119999,11.6,-4.12731989100002));
#181726=CARTESIAN_POINT('Ctrl Pts',(10.0336927599999,15.2,-4.12754600100001));
#181727=CARTESIAN_POINT('Ctrl Pts',(10.0336927599999,11.6,-4.12754600100001));
#181728=CARTESIAN_POINT('Ctrl Pts',(10.0364505199999,15.2,-4.12777026900002));
#181729=CARTESIAN_POINT('Ctrl Pts',(10.0364505199999,11.6,-4.12777026900002));
#181730=CARTESIAN_POINT('Ctrl Pts',(10.0392141799999,15.2,-4.12799268600001));
#181731=CARTESIAN_POINT('Ctrl Pts',(10.0392141799999,11.6,-4.12799268600002));
#181732=CARTESIAN_POINT('Ctrl Pts',(10.0419837319999,15.2,-4.12821324300001));
#181733=CARTESIAN_POINT('Ctrl Pts',(10.0419837319999,11.6,-4.12821324300001));
#181734=CARTESIAN_POINT('Ctrl Pts',(10.0447591649999,15.2,-4.12843193000001));
#181735=CARTESIAN_POINT('Ctrl Pts',(10.0447591649999,11.6,-4.12843193000001));
#181736=CARTESIAN_POINT('Ctrl Pts',(10.0475404719999,15.2,-4.12864873800002));
#181737=CARTESIAN_POINT('Ctrl Pts',(10.0475404719999,11.6,-4.12864873800002));
#181738=CARTESIAN_POINT('Ctrl Pts',(10.0503276389999,15.2,-4.12886366000001));
#181739=CARTESIAN_POINT('Ctrl Pts',(10.0503276389999,11.6,-4.12886366000001));
#181740=CARTESIAN_POINT('Ctrl Pts',(10.0531206589999,15.2,-4.12907668300001));
#181741=CARTESIAN_POINT('Ctrl Pts',(10.0531206589999,11.6,-4.12907668300001));
#181742=CARTESIAN_POINT('Ctrl Pts',(10.0559195209999,15.2,-4.12928780200001));
#181743=CARTESIAN_POINT('Ctrl Pts',(10.0559195209999,11.6,-4.12928780200002));
#181744=CARTESIAN_POINT('Ctrl Pts',(10.0587242159999,15.2,-4.12949700500001));
#181745=CARTESIAN_POINT('Ctrl Pts',(10.0587242159999,11.6,-4.12949700500001));
#181746=CARTESIAN_POINT('Ctrl Pts',(10.0615347329999,15.2,-4.12970428500001));
#181747=CARTESIAN_POINT('Ctrl Pts',(10.0615347329999,11.6,-4.12970428500001));
#181748=CARTESIAN_POINT('Ctrl Pts',(10.0643510649999,15.2,-4.12990963300001));
#181749=CARTESIAN_POINT('Ctrl Pts',(10.0643510649999,11.6,-4.12990963300001));
#181750=CARTESIAN_POINT('Ctrl Pts',(10.0671731989999,15.2,-4.13011303900001));
#181751=CARTESIAN_POINT('Ctrl Pts',(10.0671731989999,11.6,-4.13011303900001));
#181752=CARTESIAN_POINT('Ctrl Pts',(10.0700011269999,15.2,-4.13031449500001));
#181753=CARTESIAN_POINT('Ctrl Pts',(10.0700011269999,11.6,-4.13031449500001));
#181754=CARTESIAN_POINT('Ctrl Pts',(10.0728348389999,15.2,-4.13051399200001));
#181755=CARTESIAN_POINT('Ctrl Pts',(10.0728348389999,11.6,-4.13051399200001));
#181756=CARTESIAN_POINT('Ctrl Pts',(10.0756743259999,15.2,-4.13071152200001));
#181757=CARTESIAN_POINT('Ctrl Pts',(10.0756743259999,11.6,-4.13071152200002));
#181758=CARTESIAN_POINT('Ctrl Pts',(10.0785195769999,15.2,-4.13090707400002));
#181759=CARTESIAN_POINT('Ctrl Pts',(10.0785195769999,11.6,-4.13090707400002));
#181760=CARTESIAN_POINT('Ctrl Pts',(10.0813705839999,15.2,-4.13110064100001));
#181761=CARTESIAN_POINT('Ctrl Pts',(10.0813705839999,11.6,-4.13110064100001));
#181762=CARTESIAN_POINT('Ctrl Pts',(10.0842273359999,15.2,-4.13129221400002));
#181763=CARTESIAN_POINT('Ctrl Pts',(10.0842273359999,11.6,-4.13129221400002));
#181764=CARTESIAN_POINT('Ctrl Pts',(10.0870898239999,15.2,-4.13148178500002));
#181765=CARTESIAN_POINT('Ctrl Pts',(10.0870898239999,11.6,-4.13148178500002));
#181766=CARTESIAN_POINT('Ctrl Pts',(10.0899580389999,15.2,-4.13166934400001));
#181767=CARTESIAN_POINT('Ctrl Pts',(10.0899580389999,11.6,-4.13166934400001));
#181768=CARTESIAN_POINT('Ctrl Pts',(10.0928319699999,15.2,-4.13185488300002));
#181769=CARTESIAN_POINT('Ctrl Pts',(10.0928319699999,11.6,-4.13185488300002));
#181770=CARTESIAN_POINT('Ctrl Pts',(10.0957116079999,15.2,-4.13203839300001));
#181771=CARTESIAN_POINT('Ctrl Pts',(10.0957116079999,11.6,-4.13203839300001));
#181772=CARTESIAN_POINT('Ctrl Pts',(10.0985969439999,15.2,-4.13221986700002));
#181773=CARTESIAN_POINT('Ctrl Pts',(10.0985969439999,11.6,-4.13221986700002));
#181774=CARTESIAN_POINT('Ctrl Pts',(10.1014879679999,15.2,-4.13239929400001));
#181775=CARTESIAN_POINT('Ctrl Pts',(10.1014879679999,11.6,-4.13239929400001));
#181776=CARTESIAN_POINT('Ctrl Pts',(10.1043846719999,15.2,-4.13257666700002));
#181777=CARTESIAN_POINT('Ctrl Pts',(10.1043846719999,11.6,-4.13257666700002));
#181778=CARTESIAN_POINT('Ctrl Pts',(10.1072870439999,15.2,-4.13275197800001));
#181779=CARTESIAN_POINT('Ctrl Pts',(10.1072870439999,11.6,-4.13275197800001));
#181780=CARTESIAN_POINT('Ctrl Pts',(10.1101950759999,15.2,-4.13292521800001));
#181781=CARTESIAN_POINT('Ctrl Pts',(10.1101950759999,11.6,-4.13292521800001));
#181782=CARTESIAN_POINT('Ctrl Pts',(10.1131087579999,15.2,-4.13309637800001));
#181783=CARTESIAN_POINT('Ctrl Pts',(10.1131087579999,11.6,-4.13309637800001));
#181784=CARTESIAN_POINT('Ctrl Pts',(10.1160280819999,15.2,-4.13326545000002));
#181785=CARTESIAN_POINT('Ctrl Pts',(10.1160280819999,11.6,-4.13326545000002));
#181786=CARTESIAN_POINT('Ctrl Pts',(10.1189530369999,15.2,-4.13343242500002));
#181787=CARTESIAN_POINT('Ctrl Pts',(10.1189530369999,11.6,-4.13343242500002));
#181788=CARTESIAN_POINT('Ctrl Pts',(10.1218836129999,15.2,-4.13359729600002));
#181789=CARTESIAN_POINT('Ctrl Pts',(10.1218836129999,11.6,-4.13359729600002));
#181790=CARTESIAN_POINT('Ctrl Pts',(10.1248198019999,15.2,-4.13376005400002));
#181791=CARTESIAN_POINT('Ctrl Pts',(10.1248198019999,11.6,-4.13376005400002));
#181792=CARTESIAN_POINT('Ctrl Pts',(10.1277615949999,15.2,-4.13392069100002));
#181793=CARTESIAN_POINT('Ctrl Pts',(10.1277615949999,11.6,-4.13392069100002));
#181794=CARTESIAN_POINT('Ctrl Pts',(10.1307089819999,15.2,-4.13407919700001));
#181795=CARTESIAN_POINT('Ctrl Pts',(10.1307089819999,11.6,-4.13407919700001));
#181796=CARTESIAN_POINT('Ctrl Pts',(10.1336619529999,15.2,-4.13423556700002));
#181797=CARTESIAN_POINT('Ctrl Pts',(10.1336619529999,11.6,-4.13423556700002));
#181798=CARTESIAN_POINT('Ctrl Pts',(10.1366204989999,15.2,-4.13438979000002));
#181799=CARTESIAN_POINT('Ctrl Pts',(10.1366204989999,11.6,-4.13438979000002));
#181800=CARTESIAN_POINT('Ctrl Pts',(10.1395846109999,15.2,-4.13454185800001));
#181801=CARTESIAN_POINT('Ctrl Pts',(10.1395846109999,11.6,-4.13454185800001));
#181802=CARTESIAN_POINT('Ctrl Pts',(10.1425542799999,15.2,-4.13469176500001));
#181803=CARTESIAN_POINT('Ctrl Pts',(10.1425542799999,11.6,-4.13469176500001));
#181804=CARTESIAN_POINT('Ctrl Pts',(10.1455294969999,15.2,-4.13483950100002));
#181805=CARTESIAN_POINT('Ctrl Pts',(10.1455294969999,11.6,-4.13483950100002));
#181806=CARTESIAN_POINT('Ctrl Pts',(10.1485102509999,15.2,-4.13498505800002));
#181807=CARTESIAN_POINT('Ctrl Pts',(10.1485102509999,11.6,-4.13498505800002));
#181808=CARTESIAN_POINT('Ctrl Pts',(10.1514965349999,15.2,-4.13512842800001));
#181809=CARTESIAN_POINT('Ctrl Pts',(10.1514965349999,11.6,-4.13512842800001));
#181810=CARTESIAN_POINT('Ctrl Pts',(10.1544883369999,15.2,-4.13526960300001));
#181811=CARTESIAN_POINT('Ctrl Pts',(10.1544883369999,11.6,-4.13526960300001));
#181812=CARTESIAN_POINT('Ctrl Pts',(10.1574856509999,15.2,-4.13540857600001));
#181813=CARTESIAN_POINT('Ctrl Pts',(10.1574856509999,11.6,-4.13540857600002));
#181814=CARTESIAN_POINT('Ctrl Pts',(10.1604884649999,15.2,-4.13554533700002));
#181815=CARTESIAN_POINT('Ctrl Pts',(10.1604884649999,11.6,-4.13554533700002));
#181816=CARTESIAN_POINT('Ctrl Pts',(10.1634967709999,15.2,-4.13567988000001));
#181817=CARTESIAN_POINT('Ctrl Pts',(10.1634967709999,11.6,-4.13567988000001));
#181818=CARTESIAN_POINT('Ctrl Pts',(10.1665105609999,15.2,-4.13581219600001));
#181819=CARTESIAN_POINT('Ctrl Pts',(10.1665105609999,11.6,-4.13581219600002));
#181820=CARTESIAN_POINT('Ctrl Pts',(10.1695298229999,15.2,-4.13594227700001));
#181821=CARTESIAN_POINT('Ctrl Pts',(10.1695298229999,11.6,-4.13594227700001));
#181822=CARTESIAN_POINT('Ctrl Pts',(10.1725545499999,15.2,-4.13607011500002));
#181823=CARTESIAN_POINT('Ctrl Pts',(10.1725545499999,11.6,-4.13607011500002));
#181824=CARTESIAN_POINT('Ctrl Pts',(10.1755847329999,15.2,-4.13619570200002));
#181825=CARTESIAN_POINT('Ctrl Pts',(10.1755847329999,11.6,-4.13619570200002));
#181826=CARTESIAN_POINT('Ctrl Pts',(10.1786203619999,15.2,-4.13631903200002));
#181827=CARTESIAN_POINT('Ctrl Pts',(10.1786203619999,11.6,-4.13631903200002));
#181828=CARTESIAN_POINT('Ctrl Pts',(10.1816614279999,15.2,-4.13644009500001));
#181829=CARTESIAN_POINT('Ctrl Pts',(10.1816614279999,11.6,-4.13644009500001));
#181830=CARTESIAN_POINT('Ctrl Pts',(10.1847079219999,15.2,-4.13655888400001));
#181831=CARTESIAN_POINT('Ctrl Pts',(10.1847079219999,11.6,-4.13655888400002));
#181832=CARTESIAN_POINT('Ctrl Pts',(10.1877598339999,15.2,-4.13667539000001));
#181833=CARTESIAN_POINT('Ctrl Pts',(10.1877598339999,11.6,-4.13667539000001));
#181834=CARTESIAN_POINT('Ctrl Pts',(10.1908171569999,15.2,-4.13678960700001));
#181835=CARTESIAN_POINT('Ctrl Pts',(10.1908171569999,11.6,-4.13678960700001));
#181836=CARTESIAN_POINT('Ctrl Pts',(10.1938798809999,15.2,-4.13690152700001));
#181837=CARTESIAN_POINT('Ctrl Pts',(10.1938798809999,11.6,-4.13690152700002));
#181838=CARTESIAN_POINT('Ctrl Pts',(10.1969479959999,15.2,-4.13701114100002));
#181839=CARTESIAN_POINT('Ctrl Pts',(10.1969479959999,11.6,-4.13701114100002));
#181840=CARTESIAN_POINT('Ctrl Pts',(10.2000214939999,15.2,-4.13711844300002));
#181841=CARTESIAN_POINT('Ctrl Pts',(10.2000214939999,11.6,-4.13711844300002));
#181842=CARTESIAN_POINT('Ctrl Pts',(10.2031003659999,15.2,-4.13722342400002));
#181843=CARTESIAN_POINT('Ctrl Pts',(10.2031003659999,11.6,-4.13722342400002));
#181844=CARTESIAN_POINT('Ctrl Pts',(10.2061846029999,15.2,-4.13732607700001));
#181845=CARTESIAN_POINT('Ctrl Pts',(10.2061846029999,11.6,-4.13732607700002));
#181846=CARTESIAN_POINT('Ctrl Pts',(10.2092741959999,15.2,-4.13742639400001));
#181847=CARTESIAN_POINT('Ctrl Pts',(10.2092741959999,11.6,-4.13742639400002));
#181848=CARTESIAN_POINT('Ctrl Pts',(10.2123691339999,15.2,-4.13752436800001));
#181849=CARTESIAN_POINT('Ctrl Pts',(10.2123691339999,11.6,-4.13752436800001));
#181850=CARTESIAN_POINT('Ctrl Pts',(10.2154694119999,15.2,-4.13761999000001));
#181851=CARTESIAN_POINT('Ctrl Pts',(10.2154694119999,11.6,-4.13761999000002));
#181852=CARTESIAN_POINT('Ctrl Pts',(10.2185750179999,15.2,-4.13771325500001));
#181853=CARTESIAN_POINT('Ctrl Pts',(10.2185750179999,11.6,-4.13771325500001));
#181854=CARTESIAN_POINT('Ctrl Pts',(10.2216859439999,15.2,-4.13780415200002));
#181855=CARTESIAN_POINT('Ctrl Pts',(10.2216859439999,11.6,-4.13780415200002));
#181856=CARTESIAN_POINT('Ctrl Pts',(10.2248021809999,15.2,-4.13789267700002));
#181857=CARTESIAN_POINT('Ctrl Pts',(10.2248021809999,11.6,-4.13789267700002));
#181858=CARTESIAN_POINT('Ctrl Pts',(10.2279237199999,15.2,-4.13797882100001));
#181859=CARTESIAN_POINT('Ctrl Pts',(10.2279237199999,11.6,-4.13797882100001));
#181860=CARTESIAN_POINT('Ctrl Pts',(10.2310505519999,15.2,-4.13806257500001));
#181861=CARTESIAN_POINT('Ctrl Pts',(10.2310505519999,11.6,-4.13806257500002));
#181862=CARTESIAN_POINT('Ctrl Pts',(10.2341826699999,15.2,-4.13814393500001));
#181863=CARTESIAN_POINT('Ctrl Pts',(10.2341826699999,11.6,-4.13814393500001));
#181864=CARTESIAN_POINT('Ctrl Pts',(10.2373200619999,15.2,-4.13822289000001));
#181865=CARTESIAN_POINT('Ctrl Pts',(10.2373200619999,11.6,-4.13822289000001));
#181866=CARTESIAN_POINT('Ctrl Pts',(10.2404627209999,15.2,-4.13829943400001));
#181867=CARTESIAN_POINT('Ctrl Pts',(10.2404627209999,11.6,-4.13829943400002));
#181868=CARTESIAN_POINT('Ctrl Pts',(10.2436106389999,15.2,-4.13837356000001));
#181869=CARTESIAN_POINT('Ctrl Pts',(10.2436106389999,11.6,-4.13837356000002));
#181870=CARTESIAN_POINT('Ctrl Pts',(10.2467638039999,15.2,-4.13844526200001));
#181871=CARTESIAN_POINT('Ctrl Pts',(10.2467638039999,11.6,-4.13844526200002));
#181872=CARTESIAN_POINT('Ctrl Pts',(10.2499222099999,15.2,-4.13851453000001));
#181873=CARTESIAN_POINT('Ctrl Pts',(10.2499222099999,11.6,-4.13851453000001));
#181874=CARTESIAN_POINT('Ctrl Pts',(10.2530858489999,15.2,-4.13858135800002));
#181875=CARTESIAN_POINT('Ctrl Pts',(10.2530858489999,11.6,-4.13858135800002));
#181876=CARTESIAN_POINT('Ctrl Pts',(10.2562547089999,15.2,-4.13864573900002));
#181877=CARTESIAN_POINT('Ctrl Pts',(10.2562547089999,11.6,-4.13864573900002));
#181878=CARTESIAN_POINT('Ctrl Pts',(10.2594287839999,15.2,-4.13870766500001));
#181879=CARTESIAN_POINT('Ctrl Pts',(10.2594287839999,11.6,-4.13870766500002));
#181880=CARTESIAN_POINT('Ctrl Pts',(10.2626080629999,15.2,-4.13876712900001));
#181881=CARTESIAN_POINT('Ctrl Pts',(10.2626080629999,11.6,-4.13876712900001));
#181882=CARTESIAN_POINT('Ctrl Pts',(10.2657925389999,15.2,-4.13882412400001));
#181883=CARTESIAN_POINT('Ctrl Pts',(10.2657925389999,11.6,-4.13882412400001));
#181884=CARTESIAN_POINT('Ctrl Pts',(10.2689822019999,15.2,-4.13887864300001));
#181885=CARTESIAN_POINT('Ctrl Pts',(10.2689822019999,11.6,-4.13887864300001));
#181886=CARTESIAN_POINT('Ctrl Pts',(10.2721770449999,15.2,-4.13893067800001));
#181887=CARTESIAN_POINT('Ctrl Pts',(10.2721770449999,11.6,-4.13893067800002));
#181888=CARTESIAN_POINT('Ctrl Pts',(10.2753770579999,15.2,-4.13898022200001));
#181889=CARTESIAN_POINT('Ctrl Pts',(10.2753770579999,11.6,-4.13898022200002));
#181890=CARTESIAN_POINT('Ctrl Pts',(10.2785822319999,15.2,-4.13902726900002));
#181891=CARTESIAN_POINT('Ctrl Pts',(10.2785822319999,11.6,-4.13902726900002));
#181892=CARTESIAN_POINT('Ctrl Pts',(10.2817925589999,15.2,-4.13907181100001));
#181893=CARTESIAN_POINT('Ctrl Pts',(10.2817925589999,11.6,-4.13907181100001));
#181894=CARTESIAN_POINT('Ctrl Pts',(10.2850080309999,15.2,-4.13911384100001));
#181895=CARTESIAN_POINT('Ctrl Pts',(10.2850080309999,11.6,-4.13911384100001));
#181896=CARTESIAN_POINT('Ctrl Pts',(10.2882286369999,15.2,-4.13915335100001));
#181897=CARTESIAN_POINT('Ctrl Pts',(10.2882286369999,11.6,-4.13915335100001));
#181898=CARTESIAN_POINT('Ctrl Pts',(10.2914543719999,15.2,-4.13919033700001));
#181899=CARTESIAN_POINT('Ctrl Pts',(10.2914543719999,11.6,-4.13919033700001));
#181900=CARTESIAN_POINT('Ctrl Pts',(10.2946852229999,15.2,-4.13922478800002));
#181901=CARTESIAN_POINT('Ctrl Pts',(10.2946852229999,11.6,-4.13922478800002));
#181902=CARTESIAN_POINT('Ctrl Pts',(10.2979211849999,15.2,-4.13925669900001));
#181903=CARTESIAN_POINT('Ctrl Pts',(10.2979211849999,11.6,-4.13925669900001));
#181904=CARTESIAN_POINT('Ctrl Pts',(10.3011622479999,15.2,-4.13928606400002));
#181905=CARTESIAN_POINT('Ctrl Pts',(10.3011622479999,11.6,-4.13928606400002));
#181906=CARTESIAN_POINT('Ctrl Pts',(10.3044084029999,15.2,-4.13931287500001));
#181907=CARTESIAN_POINT('Ctrl Pts',(10.3044084029999,11.6,-4.13931287500001));
#181908=CARTESIAN_POINT('Ctrl Pts',(10.3076596409999,15.2,-4.13933712400001));
#181909=CARTESIAN_POINT('Ctrl Pts',(10.3076596409999,11.6,-4.13933712400001));
#181910=CARTESIAN_POINT('Ctrl Pts',(10.3109159559999,15.2,-4.13935880700001));
#181911=CARTESIAN_POINT('Ctrl Pts',(10.3109159559999,11.6,-4.13935880700001));
#181912=CARTESIAN_POINT('Ctrl Pts',(10.3141773369999,15.2,-4.13937791300001));
#181913=CARTESIAN_POINT('Ctrl Pts',(10.3141773369999,11.6,-4.13937791300001));
#181914=CARTESIAN_POINT('Ctrl Pts',(10.3174437759999,15.2,-4.13939443800002));
#181915=CARTESIAN_POINT('Ctrl Pts',(10.3174437759999,11.6,-4.13939443800002));
#181916=CARTESIAN_POINT('Ctrl Pts',(10.3207152649999,15.2,-4.13940837600002));
#181917=CARTESIAN_POINT('Ctrl Pts',(10.3207152649999,11.6,-4.13940837600002));
#181918=CARTESIAN_POINT('Ctrl Pts',(10.3239917949999,15.2,-4.13941971700002));
#181919=CARTESIAN_POINT('Ctrl Pts',(10.3239917949999,11.6,-4.13941971700002));
#181920=CARTESIAN_POINT('Ctrl Pts',(10.3272733569999,15.2,-4.13942845600001));
#181921=CARTESIAN_POINT('Ctrl Pts',(10.3272733569999,11.6,-4.13942845600001));
#181922=CARTESIAN_POINT('Ctrl Pts',(10.3305599449999,15.2,-4.13943458700002));
#181923=CARTESIAN_POINT('Ctrl Pts',(10.3305599449999,11.6,-4.13943458700002));
#181924=CARTESIAN_POINT('Ctrl Pts',(10.3338515469999,15.2,-4.13943810200001));
#181925=CARTESIAN_POINT('Ctrl Pts',(10.3338515469999,11.6,-4.13943810200002));
#181926=CARTESIAN_POINT('Ctrl Pts',(10.3371481569999,15.2,-4.13943899400001));
#181927=CARTESIAN_POINT('Ctrl Pts',(10.3371481569999,11.6,-4.13943899400001));
#181928=CARTESIAN_POINT('Ctrl Pts',(10.3404497649999,15.2,-4.13943725700001));
#181929=CARTESIAN_POINT('Ctrl Pts',(10.3404497649999,11.6,-4.13943725700001));
#181930=CARTESIAN_POINT('Ctrl Pts',(10.3437563629999,15.2,-4.13943288400001));
#181931=CARTESIAN_POINT('Ctrl Pts',(10.3437563629999,11.6,-4.13943288400001));
#181932=CARTESIAN_POINT('Ctrl Pts',(10.3470679429999,15.2,-4.13942586900002));
#181933=CARTESIAN_POINT('Ctrl Pts',(10.3470679429999,11.6,-4.13942586900002));
#181934=CARTESIAN_POINT('Ctrl Pts',(10.3503844979999,15.2,-4.13941620500001));
#181935=CARTESIAN_POINT('Ctrl Pts',(10.3503844979999,11.6,-4.13941620500002));
#181936=CARTESIAN_POINT('Ctrl Pts',(10.3537060159999,15.2,-4.13940388400002));
#181937=CARTESIAN_POINT('Ctrl Pts',(10.3537060159999,11.6,-4.13940388400002));
#181938=CARTESIAN_POINT('Ctrl Pts',(10.3570324909999,15.2,-4.13938890200001));
#181939=CARTESIAN_POINT('Ctrl Pts',(10.3570324909999,11.6,-4.13938890200001));
#181940=CARTESIAN_POINT('Ctrl Pts',(10.3603639139999,15.2,-4.13937124900002));
#181941=CARTESIAN_POINT('Ctrl Pts',(10.3603639139999,11.6,-4.13937124900002));
#181942=CARTESIAN_POINT('Ctrl Pts',(10.3637002769999,15.2,-4.13935092100001));
#181943=CARTESIAN_POINT('Ctrl Pts',(10.3637002769999,11.6,-4.13935092100001));
#181944=CARTESIAN_POINT('Ctrl Pts',(10.3670415719999,15.2,-4.13932791100001));
#181945=CARTESIAN_POINT('Ctrl Pts',(10.3670415719999,11.6,-4.13932791100002));
#181946=CARTESIAN_POINT('Ctrl Pts',(10.3703877889999,15.2,-4.13930221300001));
#181947=CARTESIAN_POINT('Ctrl Pts',(10.3703877889999,11.6,-4.13930221300001));
#181948=CARTESIAN_POINT('Ctrl Pts',(10.3737389219999,15.2,-4.13927381900002));
#181949=CARTESIAN_POINT('Ctrl Pts',(10.3737389219999,11.6,-4.13927381900002));
#181950=CARTESIAN_POINT('Ctrl Pts',(10.3770949599999,15.2,-4.13924272200001));
#181951=CARTESIAN_POINT('Ctrl Pts',(10.3770949599999,11.6,-4.13924272200001));
#181952=CARTESIAN_POINT('Ctrl Pts',(10.3804558959999,15.2,-4.13920891800001));
#181953=CARTESIAN_POINT('Ctrl Pts',(10.3804558959999,11.6,-4.13920891800002));
#181954=CARTESIAN_POINT('Ctrl Pts',(10.3838217219999,15.2,-4.13917239800002));
#181955=CARTESIAN_POINT('Ctrl Pts',(10.3838217219999,11.6,-4.13917239800002));
#181956=CARTESIAN_POINT('Ctrl Pts',(10.3871924299999,15.2,-4.13913315800002));
#181957=CARTESIAN_POINT('Ctrl Pts',(10.3871924299999,11.6,-4.13913315800002));
#181958=CARTESIAN_POINT('Ctrl Pts',(10.3905680109999,15.2,-4.13909118900001));
#181959=CARTESIAN_POINT('Ctrl Pts',(10.3905680109999,11.6,-4.13909118900001));
#181960=CARTESIAN_POINT('Ctrl Pts',(10.3939484559999,15.2,-4.13904648600001));
#181961=CARTESIAN_POINT('Ctrl Pts',(10.3939484559999,11.6,-4.13904648600001));
#181962=CARTESIAN_POINT('Ctrl Pts',(10.3973337579999,15.2,-4.13899904300001));
#181963=CARTESIAN_POINT('Ctrl Pts',(10.3973337579999,11.6,-4.13899904300001));
#181964=CARTESIAN_POINT('Ctrl Pts',(10.4007239089999,15.2,-4.13894885300001));
#181965=CARTESIAN_POINT('Ctrl Pts',(10.4007239089999,11.6,-4.13894885300001));
#181966=CARTESIAN_POINT('Ctrl Pts',(10.4041188989999,15.2,-4.13889591000002));
#181967=CARTESIAN_POINT('Ctrl Pts',(10.4041188989999,11.6,-4.13889591000002));
#181968=CARTESIAN_POINT('Ctrl Pts',(10.4075187209999,15.2,-4.13884020700001));
#181969=CARTESIAN_POINT('Ctrl Pts',(10.4075187209999,11.6,-4.13884020700001));
#181970=CARTESIAN_POINT('Ctrl Pts',(10.4109233669999,15.2,-4.13878173800001));
#181971=CARTESIAN_POINT('Ctrl Pts',(10.4109233669999,11.6,-4.13878173800002));
#181972=CARTESIAN_POINT('Ctrl Pts',(10.4143328269999,15.2,-4.13872049700001));
#181973=CARTESIAN_POINT('Ctrl Pts',(10.4143328269999,11.6,-4.13872049700002));
#181974=CARTESIAN_POINT('Ctrl Pts',(10.4177470959999,15.2,-4.13865647700002));
#181975=CARTESIAN_POINT('Ctrl Pts',(10.4177470959999,11.6,-4.13865647700002));
#181976=CARTESIAN_POINT('Ctrl Pts',(10.4211661629999,15.2,-4.13858967300001));
#181977=CARTESIAN_POINT('Ctrl Pts',(10.4211661629999,11.6,-4.13858967300001));
#181978=CARTESIAN_POINT('Ctrl Pts',(10.4245900209999,15.2,-4.13852007700001));
#181979=CARTESIAN_POINT('Ctrl Pts',(10.4245900209999,11.6,-4.13852007700002));
#181980=CARTESIAN_POINT('Ctrl Pts',(10.4280186619999,15.2,-4.13844768400002));
#181981=CARTESIAN_POINT('Ctrl Pts',(10.4280186619999,11.6,-4.13844768400002));
#181982=CARTESIAN_POINT('Ctrl Pts',(10.4314520759999,15.2,-4.13837248700001));
#181983=CARTESIAN_POINT('Ctrl Pts',(10.4314520759999,11.6,-4.13837248700002));
#181984=CARTESIAN_POINT('Ctrl Pts',(10.4348902579999,15.2,-4.13829448200001));
#181985=CARTESIAN_POINT('Ctrl Pts',(10.4348902579999,11.6,-4.13829448200001));
#181986=CARTESIAN_POINT('Ctrl Pts',(10.4383331969999,15.2,-4.13821366000001));
#181987=CARTESIAN_POINT('Ctrl Pts',(10.4383331969999,11.6,-4.13821366000002));
#181988=CARTESIAN_POINT('Ctrl Pts',(10.4417808859999,15.2,-4.13813001600001));
#181989=CARTESIAN_POINT('Ctrl Pts',(10.4417808859999,11.6,-4.13813001600001));
#181990=CARTESIAN_POINT('Ctrl Pts',(10.4452333159999,15.2,-4.13804354400002));
#181991=CARTESIAN_POINT('Ctrl Pts',(10.4452333159999,11.6,-4.13804354400002));
#181992=CARTESIAN_POINT('Ctrl Pts',(10.4486904819999,15.2,-4.13795423800002));
#181993=CARTESIAN_POINT('Ctrl Pts',(10.4486904819999,11.6,-4.13795423800002));
#181994=CARTESIAN_POINT('Ctrl Pts',(10.4521523719999,15.2,-4.13786209000001));
#181995=CARTESIAN_POINT('Ctrl Pts',(10.4521523719999,11.6,-4.13786209000001));
#181996=CARTESIAN_POINT('Ctrl Pts',(10.4556189809999,15.2,-4.13776709800001));
#181997=CARTESIAN_POINT('Ctrl Pts',(10.4556189809999,11.6,-4.13776709800001));
#181998=CARTESIAN_POINT('Ctrl Pts',(10.4590902979999,15.2,-4.13766925300001));
#181999=CARTESIAN_POINT('Ctrl Pts',(10.4590902979999,11.6,-4.13766925300001));
#182000=CARTESIAN_POINT('Ctrl Pts',(10.4625663159999,15.2,-4.13756854800001));
#182001=CARTESIAN_POINT('Ctrl Pts',(10.4625663159999,11.6,-4.13756854800001));
#182002=CARTESIAN_POINT('Ctrl Pts',(10.4660470279999,15.2,-4.13746497900001));
#182003=CARTESIAN_POINT('Ctrl Pts',(10.4660470279999,11.6,-4.13746497900001));
#182004=CARTESIAN_POINT('Ctrl Pts',(10.4695324259999,15.2,-4.13735854000001));
#182005=CARTESIAN_POINT('Ctrl Pts',(10.4695324259999,11.6,-4.13735854000001));
#182006=CARTESIAN_POINT('Ctrl Pts',(10.4730225009999,15.2,-4.13724922400001));
#182007=CARTESIAN_POINT('Ctrl Pts',(10.4730225009999,11.6,-4.13724922400002));
#182008=CARTESIAN_POINT('Ctrl Pts',(10.4765172449999,15.2,-4.13713702500001));
#182009=CARTESIAN_POINT('Ctrl Pts',(10.4765172449999,11.6,-4.13713702500001));
#182010=CARTESIAN_POINT('Ctrl Pts',(10.4800166499999,15.2,-4.13702193900002));
#182011=CARTESIAN_POINT('Ctrl Pts',(10.4800166499999,11.6,-4.13702193900002));
#182012=CARTESIAN_POINT('Ctrl Pts',(10.4835207079999,15.2,-4.13690395700002));
#182013=CARTESIAN_POINT('Ctrl Pts',(10.4835207079999,11.6,-4.13690395700002));
#182014=CARTESIAN_POINT('Ctrl Pts',(10.4870294109999,15.2,-4.13678307500001));
#182015=CARTESIAN_POINT('Ctrl Pts',(10.4870294109999,11.6,-4.13678307500002));
#182016=CARTESIAN_POINT('Ctrl Pts',(10.4905427519999,15.2,-4.13665928700001));
#182017=CARTESIAN_POINT('Ctrl Pts',(10.4905427519999,11.6,-4.13665928700001));
#182018=CARTESIAN_POINT('Ctrl Pts',(10.4940607219999,15.2,-4.13653258700001));
#182019=CARTESIAN_POINT('Ctrl Pts',(10.4940607219999,11.6,-4.13653258700002));
#182020=CARTESIAN_POINT('Ctrl Pts',(10.4975833129999,15.2,-4.13640296900001));
#182021=CARTESIAN_POINT('Ctrl Pts',(10.4975833129999,11.6,-4.13640296900002));
#182022=CARTESIAN_POINT('Ctrl Pts',(10.5011105169999,15.2,-4.13627042700002));
#182023=CARTESIAN_POINT('Ctrl Pts',(10.5011105169999,11.6,-4.13627042700002));
#182024=CARTESIAN_POINT('Ctrl Pts',(10.5046423259999,15.2,-4.13613495500002));
#182025=CARTESIAN_POINT('Ctrl Pts',(10.5046423259999,11.6,-4.13613495500002));
#182026=CARTESIAN_POINT('Ctrl Pts',(10.5081787329999,15.2,-4.13599654600001));
#182027=CARTESIAN_POINT('Ctrl Pts',(10.5081787329999,11.6,-4.13599654600001));
#182028=CARTESIAN_POINT('Ctrl Pts',(10.5117197289999,15.2,-4.13585519800002));
#182029=CARTESIAN_POINT('Ctrl Pts',(10.5117197289999,11.6,-4.13585519800002));
#182030=CARTESIAN_POINT('Ctrl Pts',(10.5152653079999,15.2,-4.13571090200001));
#182031=CARTESIAN_POINT('Ctrl Pts',(10.5152653079999,11.6,-4.13571090200001));
#182032=CARTESIAN_POINT('Ctrl Pts',(10.5188154589999,15.2,-4.13556365200002));
#182033=CARTESIAN_POINT('Ctrl Pts',(10.5188154589999,11.6,-4.13556365200002));
#182034=CARTESIAN_POINT('Ctrl Pts',(10.5223701759999,15.2,-4.13541344400001));
#182035=CARTESIAN_POINT('Ctrl Pts',(10.5223701759999,11.6,-4.13541344400001));
#182036=CARTESIAN_POINT('Ctrl Pts',(10.5259294509999,15.2,-4.13526027200001));
#182037=CARTESIAN_POINT('Ctrl Pts',(10.5259294509999,11.6,-4.13526027200002));
#182038=CARTESIAN_POINT('Ctrl Pts',(10.5294932759999,15.2,-4.13510413000001));
#182039=CARTESIAN_POINT('Ctrl Pts',(10.5294932759999,11.6,-4.13510413000001));
#182040=CARTESIAN_POINT('Ctrl Pts',(10.5330616439999,15.2,-4.13494501200002));
#182041=CARTESIAN_POINT('Ctrl Pts',(10.5330616439999,11.6,-4.13494501200002));
#182042=CARTESIAN_POINT('Ctrl Pts',(10.5366345439999,15.2,-4.13478291300001));
#182043=CARTESIAN_POINT('Ctrl Pts',(10.5366345439999,11.6,-4.13478291300002));
#182044=CARTESIAN_POINT('Ctrl Pts',(10.5402119719999,15.2,-4.13461782500002));
#182045=CARTESIAN_POINT('Ctrl Pts',(10.5402119719999,11.6,-4.13461782500002));
#182046=CARTESIAN_POINT('Ctrl Pts',(10.5437939179999,15.2,-4.13444974600001));
#182047=CARTESIAN_POINT('Ctrl Pts',(10.5437939179999,11.6,-4.13444974600001));
#182048=CARTESIAN_POINT('Ctrl Pts',(10.5473803739999,15.2,-4.13427866800001));
#182049=CARTESIAN_POINT('Ctrl Pts',(10.5473803739999,11.6,-4.13427866800001));
#182050=CARTESIAN_POINT('Ctrl Pts',(10.5509713329999,15.2,-4.13410458600001));
#182051=CARTESIAN_POINT('Ctrl Pts',(10.5509713329999,11.6,-4.13410458600001));
#182052=CARTESIAN_POINT('Ctrl Pts',(10.5545667879999,15.2,-4.13392749400002));
#182053=CARTESIAN_POINT('Ctrl Pts',(10.5545667879999,11.6,-4.13392749400002));
#182054=CARTESIAN_POINT('Ctrl Pts',(10.5581667289999,15.2,-4.13374738700002));
#182055=CARTESIAN_POINT('Ctrl Pts',(10.5581667289999,11.6,-4.13374738700002));
#182056=CARTESIAN_POINT('Ctrl Pts',(10.5617711499999,15.2,-4.13356425800002));
#182057=CARTESIAN_POINT('Ctrl Pts',(10.5617711499999,11.6,-4.13356425800002));
#182058=CARTESIAN_POINT('Ctrl Pts',(10.5653800419999,15.2,-4.13337810400002));
#182059=CARTESIAN_POINT('Ctrl Pts',(10.5653800419999,11.6,-4.13337810400002));
#182060=CARTESIAN_POINT('Ctrl Pts',(10.5689933989999,15.2,-4.13318891700001));
#182061=CARTESIAN_POINT('Ctrl Pts',(10.5689933989999,11.6,-4.13318891700001));
#182062=CARTESIAN_POINT('Ctrl Pts',(10.5726112109999,15.2,-4.13299669400002));
#182063=CARTESIAN_POINT('Ctrl Pts',(10.5726112109999,11.6,-4.13299669400002));
#182064=CARTESIAN_POINT('Ctrl Pts',(10.5762334719999,15.2,-4.13280142700001));
#182065=CARTESIAN_POINT('Ctrl Pts',(10.5762334719999,11.6,-4.13280142700002));
#182066=CARTESIAN_POINT('Ctrl Pts',(10.5798601729999,15.2,-4.13260311100001));
#182067=CARTESIAN_POINT('Ctrl Pts',(10.5798601729999,11.6,-4.13260311100002));
#182068=CARTESIAN_POINT('Ctrl Pts',(10.5834913069999,15.2,-4.13240174200002));
#182069=CARTESIAN_POINT('Ctrl Pts',(10.5834913069999,11.6,-4.13240174200002));
#182070=CARTESIAN_POINT('Ctrl Pts',(10.5871268649999,15.2,-4.13219731300002));
#182071=CARTESIAN_POINT('Ctrl Pts',(10.5871268649999,11.6,-4.13219731300002));
#182072=CARTESIAN_POINT('Ctrl Pts',(10.5907668409999,15.2,-4.13198982000001));
#182073=CARTESIAN_POINT('Ctrl Pts',(10.5907668409999,11.6,-4.13198982000001));
#182074=CARTESIAN_POINT('Ctrl Pts',(10.5944112269999,15.2,-4.13177925500001));
#182075=CARTESIAN_POINT('Ctrl Pts',(10.5944112269999,11.6,-4.13177925500001));
#182076=CARTESIAN_POINT('Ctrl Pts',(10.5980600139999,15.2,-4.13156561600001));
#182077=CARTESIAN_POINT('Ctrl Pts',(10.5980600139999,11.6,-4.13156561600002));
#182078=CARTESIAN_POINT('Ctrl Pts',(10.6017131959999,15.2,-4.13134889500002));
#182079=CARTESIAN_POINT('Ctrl Pts',(10.6017131959999,11.6,-4.13134889500002));
#182080=CARTESIAN_POINT('Ctrl Pts',(10.6053707649999,15.2,-4.13112908800001));
#182081=CARTESIAN_POINT('Ctrl Pts',(10.6053707649999,11.6,-4.13112908800001));
#182082=CARTESIAN_POINT('Ctrl Pts',(10.6090327119999,15.2,-4.13090618900001));
#182083=CARTESIAN_POINT('Ctrl Pts',(10.6090327119999,11.6,-4.13090618900002));
#182084=CARTESIAN_POINT('Ctrl Pts',(10.6126990299999,15.2,-4.13068019300002));
#182085=CARTESIAN_POINT('Ctrl Pts',(10.6126990299999,11.6,-4.13068019300002));
#182086=CARTESIAN_POINT('Ctrl Pts',(10.6163697119999,15.2,-4.13045109400001));
#182087=CARTESIAN_POINT('Ctrl Pts',(10.6163697119999,11.6,-4.13045109400001));
#182088=CARTESIAN_POINT('Ctrl Pts',(10.6200447499999,15.2,-4.13021888800001));
#182089=CARTESIAN_POINT('Ctrl Pts',(10.6200447499999,11.6,-4.13021888800001));
#182090=CARTESIAN_POINT('Ctrl Pts',(10.6237241349999,15.2,-4.12998356800002));
#182091=CARTESIAN_POINT('Ctrl Pts',(10.6237241349999,11.6,-4.12998356800002));
#182092=CARTESIAN_POINT('Ctrl Pts',(10.6274078609999,15.2,-4.12974512900002));
#182093=CARTESIAN_POINT('Ctrl Pts',(10.6274078609999,11.6,-4.12974512900002));
#182094=CARTESIAN_POINT('Ctrl Pts',(10.6310959199999,15.2,-4.12950356700001));
#182095=CARTESIAN_POINT('Ctrl Pts',(10.6310959199999,11.6,-4.12950356700002));
#182096=CARTESIAN_POINT('Ctrl Pts',(10.6347883039999,15.2,-4.12925887700001));
#182097=CARTESIAN_POINT('Ctrl Pts',(10.6347883039999,11.6,-4.12925887700002));
#182098=CARTESIAN_POINT('Ctrl Pts',(10.6384850049999,15.2,-4.12901105200001));
#182099=CARTESIAN_POINT('Ctrl Pts',(10.6384850049999,11.6,-4.12901105200001));
#182100=CARTESIAN_POINT('Ctrl Pts',(10.6421860169999,15.2,-4.12876008700001));
#182101=CARTESIAN_POINT('Ctrl Pts',(10.6421860169999,11.6,-4.12876008700001));
#182102=CARTESIAN_POINT('Ctrl Pts',(10.6458913319999,15.2,-4.12850597800002));
#182103=CARTESIAN_POINT('Ctrl Pts',(10.6458913319999,11.6,-4.12850597800002));
#182104=CARTESIAN_POINT('Ctrl Pts',(10.6496009419999,15.2,-4.12824872000002));
#182105=CARTESIAN_POINT('Ctrl Pts',(10.6496009419999,11.6,-4.12824872000002));
#182106=CARTESIAN_POINT('Ctrl Pts',(10.6533148399999,15.2,-4.12798830700002));
#182107=CARTESIAN_POINT('Ctrl Pts',(10.6533148399999,11.6,-4.12798830700002));
#182108=CARTESIAN_POINT('Ctrl Pts',(10.6570330169999,15.2,-4.12772473300001));
#182109=CARTESIAN_POINT('Ctrl Pts',(10.6570330169999,11.6,-4.12772473300001));
#182110=CARTESIAN_POINT('Ctrl Pts',(10.6607554659999,15.2,-4.12745799400001));
#182111=CARTESIAN_POINT('Ctrl Pts',(10.6607554659999,11.6,-4.12745799400002));
#182112=CARTESIAN_POINT('Ctrl Pts',(10.6644821789999,15.2,-4.12718808500002));
#182113=CARTESIAN_POINT('Ctrl Pts',(10.6644821789999,11.6,-4.12718808500002));
#182114=CARTESIAN_POINT('Ctrl Pts',(10.6682131479999,15.2,-4.12691499800002));
#182115=CARTESIAN_POINT('Ctrl Pts',(10.6682131479999,11.6,-4.12691499800002));
#182116=CARTESIAN_POINT('Ctrl Pts',(10.6719483659999,15.2,-4.12663873100001));
#182117=CARTESIAN_POINT('Ctrl Pts',(10.6719483659999,11.6,-4.12663873100001));
#182118=CARTESIAN_POINT('Ctrl Pts',(10.6756878259999,15.2,-4.12635927800002));
#182119=CARTESIAN_POINT('Ctrl Pts',(10.6756878259999,11.6,-4.12635927800002));
#182120=CARTESIAN_POINT('Ctrl Pts',(10.6794315189999,15.2,-4.12607663400001));
#182121=CARTESIAN_POINT('Ctrl Pts',(10.6794315189999,11.6,-4.12607663400001));
#182122=CARTESIAN_POINT('Ctrl Pts',(10.6831794419999,15.2,-4.12579079500001));
#182123=CARTESIAN_POINT('Ctrl Pts',(10.6831794419999,11.6,-4.12579079500001));
#182124=CARTESIAN_POINT('Ctrl Pts',(10.6869315859999,15.2,-4.12550175600002));
#182125=CARTESIAN_POINT('Ctrl Pts',(10.6869315859999,11.6,-4.12550175600002));
#182126=CARTESIAN_POINT('Ctrl Pts',(10.6906879429999,15.2,-4.12520951200001));
#182127=CARTESIAN_POINT('Ctrl Pts',(10.6906879429999,11.6,-4.12520951200001));
#182128=CARTESIAN_POINT('Ctrl Pts',(10.6944485069999,15.2,-4.12491405900001));
#182129=CARTESIAN_POINT('Ctrl Pts',(10.6944485069999,11.6,-4.12491405900001));
#182130=CARTESIAN_POINT('Ctrl Pts',(10.6982132689999,15.2,-4.12461539000001));
#182131=CARTESIAN_POINT('Ctrl Pts',(10.6982132689999,11.6,-4.12461539000002));
#182132=CARTESIAN_POINT('Ctrl Pts',(10.7019822189999,15.2,-4.12431349900002));
#182133=CARTESIAN_POINT('Ctrl Pts',(10.7019822189999,11.6,-4.12431349900002));
#182134=CARTESIAN_POINT('Ctrl Pts',(10.7057553479999,15.2,-4.12400838100002));
#182135=CARTESIAN_POINT('Ctrl Pts',(10.7057553479999,11.6,-4.12400838100002));
#182136=CARTESIAN_POINT('Ctrl Pts',(10.7095326469999,15.2,-4.12370002800001));
#182137=CARTESIAN_POINT('Ctrl Pts',(10.7095326469999,11.6,-4.12370002800001));
#182138=CARTESIAN_POINT('Ctrl Pts',(10.7133141079999,15.2,-4.12338843600002));
#182139=CARTESIAN_POINT('Ctrl Pts',(10.7133141079999,11.6,-4.12338843600002));
#182140=CARTESIAN_POINT('Ctrl Pts',(10.7170997259999,15.2,-4.12307359900002));
#182141=CARTESIAN_POINT('Ctrl Pts',(10.7170997259999,11.6,-4.12307359900002));
#182142=CARTESIAN_POINT('Ctrl Pts',(10.7208894919999,15.2,-4.12275551600001));
#182143=CARTESIAN_POINT('Ctrl Pts',(10.7208894919999,11.6,-4.12275551600001));
#182144=CARTESIAN_POINT('Ctrl Pts',(10.7246834049999,15.2,-4.12243418400001));
#182145=CARTESIAN_POINT('Ctrl Pts',(10.7246834049999,11.6,-4.12243418400002));
#182146=CARTESIAN_POINT('Ctrl Pts',(10.7284814639999,15.2,-4.12210960000001));
#182147=CARTESIAN_POINT('Ctrl Pts',(10.7284814639999,11.6,-4.12210960000001));
#182148=CARTESIAN_POINT('Ctrl Pts',(10.7315232249999,15.2,-4.12184733300001));
#182149=CARTESIAN_POINT('Ctrl Pts',(10.7315232249999,11.6,-4.12184733300002));
#182150=CARTESIAN_POINT('Ctrl Pts',(10.7338064109999,15.2,-4.12164917000001));
#182151=CARTESIAN_POINT('Ctrl Pts',(10.7338064109999,11.6,-4.12164917000002));
#182152=CARTESIAN_POINT('Ctrl Pts',(10.7353293639999,15.2,-4.12151641100001));
#182153=CARTESIAN_POINT('Ctrl Pts',(10.7353293639999,11.6,-4.12151641100001));
#182154=CARTESIAN_POINT('Ctrl Pts',(10.7360910479999,15.2,-4.12144986800001));
#182155=CARTESIAN_POINT('Ctrl Pts',(10.7360910479999,11.6,-4.12144986800001));
#182156=CARTESIAN_POINT('Ctrl Pts',(9.55499537099995,15.2,-4.04260911600002));
#182157=CARTESIAN_POINT('Ctrl Pts',(9.55669454752162,15.2,-4.04316130584455));
#182158=CARTESIAN_POINT('Ctrl Pts',(9.55844976514545,15.2,-4.04372605389322));
#182159=CARTESIAN_POINT('Ctrl Pts',(9.5602602775349,15.2,-4.04430244593687));
#182160=CARTESIAN_POINT('Ctrl Pts',(9.56207952113026,15.2,-4.04488161763431));
#182161=CARTESIAN_POINT('Ctrl Pts',(9.56395460122355,15.2,-4.04547254558642));
#182162=CARTESIAN_POINT('Ctrl Pts',(9.56588480617837,15.2,-4.04607433356657));
#182163=CARTESIAN_POINT('Ctrl Pts',(9.56781501095787,15.2,-4.04667612149206));
#182164=CARTESIAN_POINT('Ctrl Pts',(9.56980034124062,15.2,-4.04728876912261));
#182165=CARTESIAN_POINT('Ctrl Pts',(9.57184010199984,15.2,-4.04791140626666));
#182166=CARTESIAN_POINT('Ctrl Pts',(9.57387986275907,15.2,-4.04853404341071));
#182167=CARTESIAN_POINT('Ctrl Pts',(9.57597405360772,15.1999999999999,-4.04916667193805));
#182168=CARTESIAN_POINT('Ctrl Pts',(9.57812199955053,15.2,-4.04980844719627));
#182169=CARTESIAN_POINT('Ctrl Pts',(9.58026994568846,15.2,-4.05045022251278));
#182170=CARTESIAN_POINT('Ctrl Pts',(9.5824716464358,15.2,-4.0511011466437));
#182171=CARTESIAN_POINT('Ctrl Pts',(9.58472643972897,15.2,-4.05176039909686));
#182172=CARTESIAN_POINT('Ctrl Pts',(9.58698123281733,15.2,-4.05241965149014));
#182173=CARTESIAN_POINT('Ctrl Pts',(9.58928912248419,15.2,-4.05308723447175));
#182174=CARTESIAN_POINT('Ctrl Pts',(9.5916494594926,15.2,-4.05376235378364));
#182175=CARTESIAN_POINT('Ctrl Pts',(9.59400979650101,15.2,-4.05443747309553));
#182176=CARTESIAN_POINT('Ctrl Pts',(9.59642258389921,15.2,-4.05512012896279));
#182177=CARTESIAN_POINT('Ctrl Pts',(9.59888719089075,15.2,-4.05580954952079));
#182178=CARTESIAN_POINT('Ctrl Pts',(9.60135179810616,15.2,-4.0564989701414));
#182179=CARTESIAN_POINT('Ctrl Pts',(9.60386822553632,15.2,-4.05719515745453));
#182180=CARTESIAN_POINT('Ctrl Pts',(9.60643585601307,15.2,-4.05789736282655));
#182181=CARTESIAN_POINT('Ctrl Pts',(9.6090034862566,15.2,-4.05859956813477));
#182182=CARTESIAN_POINT('Ctrl Pts',(9.61162232317368,15.2,-4.05930778903961));
#182183=CARTESIAN_POINT('Ctrl Pts',(9.61429176141222,15.2,-4.06002130076391));
#182184=CARTESIAN_POINT('Ctrl Pts',(9.61696119965077,15.2,-4.06073481248822));
#182185=CARTESIAN_POINT('Ctrl Pts',(9.61968124046026,15.2,-4.06145361577042));
#182186=CARTESIAN_POINT('Ctrl Pts',(9.62245129460743,15.2,-4.06217699974393));
#182187=CARTESIAN_POINT('Ctrl Pts',(9.6252213487546,15.2,-4.06290038371745));
#182188=CARTESIAN_POINT('Ctrl Pts',(9.62804141715304,15.2,-4.06362835221376));
#182189=CARTESIAN_POINT('Ctrl Pts',(9.63091092146209,15.2,-4.0643602141869));
#182190=CARTESIAN_POINT('Ctrl Pts',(9.63378042603179,15.2,-4.06509207622652));
#182191=CARTESIAN_POINT('Ctrl Pts',(9.63669936976461,15.2,-4.06582783364988));
#182192=CARTESIAN_POINT('Ctrl Pts',(9.63966718442848,15.2,-4.06656681652363));
#182193=CARTESIAN_POINT('Ctrl Pts',(9.64263499882278,15.2,-4.06730579933026));
#182194=CARTESIAN_POINT('Ctrl Pts',(9.64565168593768,15.2,-4.06804800581502));
#182195=CARTESIAN_POINT('Ctrl Pts',(9.64871669225681,15.2,-4.06879278770801));
#182196=CARTESIAN_POINT('Ctrl Pts',(9.65178169857594,15.2,-4.06953756960099));
#182197=CARTESIAN_POINT('Ctrl Pts',(9.65489502329009,15.2,-4.07028492392903));
#182198=CARTESIAN_POINT('Ctrl Pts',(9.65805612383864,15.2,-4.07103421890167));
#182199=CARTESIAN_POINT('Ctrl Pts',(9.66121722467433,15.2,-4.07178351394237));
#182200=CARTESIAN_POINT('Ctrl Pts',(9.66442610292301,15.2,-4.07253474644996));
#182201=CARTESIAN_POINT('Ctrl Pts',(9.66768222468585,15.2,-4.07328730149103));
#182202=CARTESIAN_POINT('Ctrl Pts',(9.67093834615294,15.2,-4.07403985646375));
#182203=CARTESIAN_POINT('Ctrl Pts',(9.67424171158829,15.2,-4.07479373162366));
#182204=CARTESIAN_POINT('Ctrl Pts',(9.67759179898168,15.2,-4.07554832576634));
#182205=CARTESIAN_POINT('Ctrl Pts',(9.68094188637507,15.2,-4.07630291990901));
#182206=CARTESIAN_POINT('Ctrl Pts',(9.68433869487785,15.2,-4.07705823111179));
#182207=CARTESIAN_POINT('Ctrl Pts',(9.68778171333292,15.2,-4.07781367441767));
#182208=CARTESIAN_POINT('Ctrl Pts',(9.69122473210076,15.2,-4.07856911779216));
#182209=CARTESIAN_POINT('Ctrl Pts',(9.69471395864503,15.2,-4.07932469331921));
#182210=CARTESIAN_POINT('Ctrl Pts',(9.69824889160027,15.2,-4.08007982581473));
#182211=CARTESIAN_POINT('Ctrl Pts',(9.70178382423443,15.2,-4.08083495824166));
#182212=CARTESIAN_POINT('Ctrl Pts',(9.70536446092327,15.2,-4.0815896501774));
#182213=CARTESIAN_POINT('Ctrl Pts',(9.70899030854152,15.2,-4.08234334148335));
#182214=CARTESIAN_POINT('Ctrl Pts',(9.7126161561598,15.2,-4.0830970327893));
#182215=CARTESIAN_POINT('Ctrl Pts',(9.71628721518416,15.2,-4.08384972393369));
#182216=CARTESIAN_POINT('Ctrl Pts',(9.72000299714885,15.2,-4.08460086944402));
#182217=CARTESIAN_POINT('Ctrl Pts',(9.72371877945107,15.2,-4.08535201502257));
#182218=CARTESIAN_POINT('Ctrl Pts',(9.72747928619589,15.2,-4.08610161413256));
#182219=CARTESIAN_POINT('Ctrl Pts',(9.73128403915626,15.2,-4.08684913758983));
#182220=CARTESIAN_POINT('Ctrl Pts',(9.73508879177105,15.2,-4.0875966609792));
#182221=CARTESIAN_POINT('Ctrl Pts',(9.73893778845863,15.2,-4.08834210619898));
#182222=CARTESIAN_POINT('Ctrl Pts',(9.74283056200164,15.2,-4.08908495475869));
#182223=CARTESIAN_POINT('Ctrl Pts',(9.74737213137088,15.2,-4.08995161145667));
#182224=CARTESIAN_POINT('Ctrl Pts',(9.75197328098147,15.2,-4.09081473398381));
#182225=CARTESIAN_POINT('Ctrl Pts',(9.75663328216859,15.2,-4.09167351587192));
#182226=CARTESIAN_POINT('Ctrl Pts',(9.75996185439326,15.2,-4.09228693149674));
#182227=CARTESIAN_POINT('Ctrl Pts',(9.76332045013508,15.2,-4.09289813396317));
#182228=CARTESIAN_POINT('Ctrl Pts',(9.76670880840141,15.2,-4.09350683708797));
#182229=CARTESIAN_POINT('Ctrl Pts',(9.77009716629839,15.2,-4.09411554014641));
#182230=CARTESIAN_POINT('Ctrl Pts',(9.7735152854049,15.2,-4.09472174296442));
#182231=CARTESIAN_POINT('Ctrl Pts',(9.7769629057906,15.2,-4.09532516595443));
#182232=CARTESIAN_POINT('Ctrl Pts',(9.78041052655207,15.2,-4.09592858901021));
#182233=CARTESIAN_POINT('Ctrl Pts',(9.78388764923809,15.2,-4.09652923184938));
#182234=CARTESIAN_POINT('Ctrl Pts',(9.78739401749958,15.2,-4.09712681844686));
#182235=CARTESIAN_POINT('Ctrl Pts',(9.79090038576108,15.2,-4.09772440504433));
#182236=CARTESIAN_POINT('Ctrl Pts',(9.79443599743787,15.2,-4.0983189360905));
#182237=CARTESIAN_POINT('Ctrl Pts',(9.79800060108618,15.2,-4.09891014098138));
#182238=CARTESIAN_POINT('Ctrl Pts',(9.80156520473446,15.2,-4.09950134587226));
#182239=CARTESIAN_POINT('Ctrl Pts',(9.80515880008132,15.2,-4.10008922340605));
#182240=CARTESIAN_POINT('Ctrl Pts',(9.80878113591315,15.2,-4.10067351146179));
#182241=CARTESIAN_POINT('Ctrl Pts',(9.81240347174498,15.2,-4.10125779951754));
#182242=CARTESIAN_POINT('Ctrl Pts',(9.81605454826645,15.2,-4.10183849555097));
#182243=CARTESIAN_POINT('Ctrl Pts',(9.81973411750107,15.2,-4.10241533895394));
#182244=CARTESIAN_POINT('Ctrl Pts',(9.82341368673569,15.2,-4.10299218235692));
#182245=CARTESIAN_POINT('Ctrl Pts',(9.82712175031428,15.2,-4.10356517651379));
#182246=CARTESIAN_POINT('Ctrl Pts',(9.83085806199784,15.2,-4.10413406151638));
#182247=CARTESIAN_POINT('Ctrl Pts',(9.83459437368139,15.2,-4.10470294651897));
#182248=CARTESIAN_POINT('Ctrl Pts',(9.83835893321653,15.2,-4.10526772402225));
#182249=CARTESIAN_POINT('Ctrl Pts',(9.84215150071653,15.2,-4.10582814471669));
#182250=CARTESIAN_POINT('Ctrl Pts',(9.84594406821654,15.2,-4.10638856541114));
#182251=CARTESIAN_POINT('Ctrl Pts',(9.84976464223998,15.2,-4.10694462624784));
#182252=CARTESIAN_POINT('Ctrl Pts',(9.85361298399364,15.2,-4.10749608375033));
#182253=CARTESIAN_POINT('Ctrl Pts',(9.8574613257473,15.2,-4.10804754125282));
#182254=CARTESIAN_POINT('Ctrl Pts',(9.86133743455946,15.2,-4.10859439337459));
#182255=CARTESIAN_POINT('Ctrl Pts',(9.86524107546368,15.2,-4.10913639927711));
#182256=CARTESIAN_POINT('Ctrl Pts',(9.86914471636789,15.2,-4.10967840517963));
#182257=CARTESIAN_POINT('Ctrl Pts',(9.87307588871861,15.2,-4.11021556404617));
#182258=CARTESIAN_POINT('Ctrl Pts',(9.87703435802559,15.2,-4.11074763980979));
#182259=CARTESIAN_POINT('Ctrl Pts',(9.88099282733258,15.2,-4.11127971557342));
#182260=CARTESIAN_POINT('Ctrl Pts',(9.88497859533885,15.2,-4.11180670547328));
#182261=CARTESIAN_POINT('Ctrl Pts',(9.88899142881248,15.2,-4.11232837825078));
#182262=CARTESIAN_POINT('Ctrl Pts',(9.89300426228612,15.2,-4.11285005102828));
#182263=CARTESIAN_POINT('Ctrl Pts',(9.89704416150592,15.2,-4.11336640671751));
#182264=CARTESIAN_POINT('Ctrl Pts',(9.90111089928039,15.2,-4.11387721507597));
#182265=CARTESIAN_POINT('Ctrl Pts',(9.90517763705487,15.2,-4.11438802343444));
#182266=CARTESIAN_POINT('Ctrl Pts',(9.90927121277551,15.2,-4.11489328303806));
#182267=CARTESIAN_POINT('Ctrl Pts',(9.91339139805547,15.2,-4.11539277081536));
#182268=CARTESIAN_POINT('Ctrl Pts',(9.91668754600997,15.2,-4.11579236100454));
#182269=CARTESIAN_POINT('Ctrl Pts',(9.92000072505391,15.2,-4.11618825772474));
#182270=CARTESIAN_POINT('Ctrl Pts',(9.9233308215028,15.2,-4.11658034519294));
#182271=CARTESIAN_POINT('Ctrl Pts',(9.92666091840542,15.2,-4.11697243271456));
#182272=CARTESIAN_POINT('Ctrl Pts',(9.93000793043803,15.2,-4.11736071279098));
#182273=CARTESIAN_POINT('Ctrl Pts',(9.93337174551308,15.2,-4.11774507233078));
#182274=CARTESIAN_POINT('Ctrl Pts',(9.93757651412774,15.2,-4.11822552172936));
#182275=CARTESIAN_POINT('Ctrl Pts',(9.9418075368157,15.2,-4.11869984502843));
#182276=CARTESIAN_POINT('Ctrl Pts',(9.94606459133171,15.2,-4.11916782856957));
#182277=CARTESIAN_POINT('Ctrl Pts',(9.95032164584772,15.2,-4.11963581211072));
#182278=CARTESIAN_POINT('Ctrl Pts',(9.95460473415027,15.2,-4.12009745346009));
#182279=CARTESIAN_POINT('Ctrl Pts',(9.95891363755516,15.2,-4.12055254283456));
#182280=CARTESIAN_POINT('Ctrl Pts',(9.96236075999727,15.2,-4.12091661430437));
#182281=CARTESIAN_POINT('Ctrl Pts',(9.96582440315237,15.2,-4.12127649245501));
#182282=CARTESIAN_POINT('Ctrl Pts',(9.96930445827251,15.2,-4.12163206998312));
#182283=CARTESIAN_POINT('Ctrl Pts',(9.97278451386681,15.2,-4.12198764755968));
#182284=CARTESIAN_POINT('Ctrl Pts',(9.97628097918112,15.2,-4.12233892321329));
#182285=CARTESIAN_POINT('Ctrl Pts',(9.97979374504089,15.2,-4.12268579406508));
#182286=CARTESIAN_POINT('Ctrl Pts',(9.9841847021263,15.2,-4.12311938260618));
#182287=CARTESIAN_POINT('Ctrl Pts',(9.98860112993991,15.2,-4.12354608572216));
#182288=CARTESIAN_POINT('Ctrl Pts',(9.99304281508086,15.2,-4.12396570259658));
#182289=CARTESIAN_POINT('Ctrl Pts',(9.99659616290314,15.2,-4.12430139606867));
#182290=CARTESIAN_POINT('Ctrl Pts',(10.0001656746993,15.2,-4.12463255399445));
#182291=CARTESIAN_POINT('Ctrl Pts',(10.0037512432558,15.2,-4.12495907302481));
#182292=CARTESIAN_POINT('Ctrl Pts',(10.0073368123007,15.2,-4.12528559209966));
#182293=CARTESIAN_POINT('Ctrl Pts',(10.0109384374204,15.2,-4.12560747351564));
#182294=CARTESIAN_POINT('Ctrl Pts',(10.0145560118414,15.2,-4.12592461581022));
#182295=CARTESIAN_POINT('Ctrl Pts',(10.0181735857695,15.2,-4.12624175806159));
#182296=CARTESIAN_POINT('Ctrl Pts',(10.021807108865,15.2,-4.12655416099134));
#182297=CARTESIAN_POINT('Ctrl Pts',(10.0254564741767,15.2,-4.12686172646651));
#182298=CARTESIAN_POINT('Ctrl Pts',(10.0291058399857,15.2,-4.12716929198359));
#182299=CARTESIAN_POINT('Ctrl Pts',(10.032771049626,15.2,-4.12747201726254));
#182300=CARTESIAN_POINT('Ctrl Pts',(10.0364519955674,15.2,-4.12776980629322));
#182301=CARTESIAN_POINT('Ctrl Pts',(10.0401329410073,15.2,-4.12806759528332));
#182302=CARTESIAN_POINT('Ctrl Pts',(10.0438296222261,15.2,-4.12836044756077));
#182303=CARTESIAN_POINT('Ctrl Pts',(10.0475419367549,15.2,-4.12864826642646));
#182304=CARTESIAN_POINT('Ctrl Pts',(10.0512542517895,15.2,-4.12893608533136));
#182305=CARTESIAN_POINT('Ctrl Pts',(10.0549821979677,15.2,-4.12921886979678));
#182306=CARTESIAN_POINT('Ctrl Pts',(10.0587256718394,15.2,-4.12949652425602));
#182307=CARTESIAN_POINT('Ctrl Pts',(10.0624691452011,15.2,-4.12977417867743));
#182308=CARTESIAN_POINT('Ctrl Pts',(10.0662281469708,15.2,-4.13004670417204));
#182309=CARTESIAN_POINT('Ctrl Pts',(10.0700025724606,15.2,-4.13031400521955));
#182310=CARTESIAN_POINT('Ctrl Pts',(10.0756642114667,15.2,-4.13071495684545));
#182311=CARTESIAN_POINT('Ctrl Pts',(10.0813605547099,15.2,-4.13110415353808));
#182312=CARTESIAN_POINT('Ctrl Pts',(10.0870912563579,15.2,-4.13148128205781));
#182313=CARTESIAN_POINT('Ctrl Pts',(10.0909117236027,15.2,-4.1317327010367));
#182314=CARTESIAN_POINT('Ctrl Pts',(10.094747460351,15.2,-4.1319787556163));
#182315=CARTESIAN_POINT('Ctrl Pts',(10.0985983657019,15.2,-4.13221935526365));
#182316=CARTESIAN_POINT('Ctrl Pts',(10.1024492715774,15.2,-4.13245995494378));
#182317=CARTESIAN_POINT('Ctrl Pts',(10.1063153470064,15.2,-4.13269509896259));
#182318=CARTESIAN_POINT('Ctrl Pts',(10.1101964890798,15.2,-4.13292469804165));
#182319=CARTESIAN_POINT('Ctrl Pts',(10.1160182016611,15.2,-4.13326909662895));
#182320=CARTESIAN_POINT('Ctrl Pts',(10.1218738153805,15.2,-4.13360101655331));
#182321=CARTESIAN_POINT('Ctrl Pts',(10.1277629934999,15.2,-4.13392015829171));
#182322=CARTESIAN_POINT('Ctrl Pts',(10.1316891126027,15.2,-4.13413291946997));
#182323=CARTESIAN_POINT('Ctrl Pts',(10.1356301476796,15.2,-4.13434000196146));
#182324=CARTESIAN_POINT('Ctrl Pts',(10.1395860008967,15.2,-4.13454131774962));
#182325=CARTESIAN_POINT('Ctrl Pts',(10.1435418535748,15.2,-4.13474263351034));
#182326=CARTESIAN_POINT('Ctrl Pts',(10.1475125251883,15.2,-4.13493818343953));
#182327=CARTESIAN_POINT('Ctrl Pts',(10.1514979145472,15.2,-4.13512787925824));
#182328=CARTESIAN_POINT('Ctrl Pts',(10.1554833044491,15.2,-4.13531757510279));
#182329=CARTESIAN_POINT('Ctrl Pts',(10.1594834128471,15.2,-4.13550141822281));
#182330=CARTESIAN_POINT('Ctrl Pts',(10.163498142623,15.2,-4.13567932328746));
#182331=CARTESIAN_POINT('Ctrl Pts',(10.1695202367397,15.2,-4.13594618086018));
#182332=CARTESIAN_POINT('Ctrl Pts',(10.1755752267961,15.2,-4.13619967582542));
#182333=CARTESIAN_POINT('Ctrl Pts',(10.1816627849915,15.2,-4.13643952648337));
#182334=CARTESIAN_POINT('Ctrl Pts',(10.1857211574905,15.2,-4.13659942693653));
#182335=CARTESIAN_POINT('Ctrl Pts',(10.1897940042106,15.2,-4.13675326204176));
#182336=CARTESIAN_POINT('Ctrl Pts',(10.1938812294348,15.2,-4.13690095054918));
#182337=CARTESIAN_POINT('Ctrl Pts',(10.1979684541022,15.2,-4.13704863903648));
#182338=CARTESIAN_POINT('Ctrl Pts',(10.2020700567427,15.2,-4.13719018051871));
#182339=CARTESIAN_POINT('Ctrl Pts',(10.2061859419804,15.2,-4.13732549300828));
#182340=CARTESIAN_POINT('Ctrl Pts',(10.2103018277789,15.2,-4.13746080551629));
#182341=CARTESIAN_POINT('Ctrl Pts',(10.2144319947196,15.2,-4.13758988923906));
#182342=CARTESIAN_POINT('Ctrl Pts',(10.2185763486692,15.2,-4.13771266307844));
#182343=CARTESIAN_POINT('Ctrl Pts',(10.2237567908237,15.2,-4.13786613036931));
#182344=CARTESIAN_POINT('Ctrl Pts',(10.2289593988759,15.2,-4.13800973915722));
#182345=CARTESIAN_POINT('Ctrl Pts',(10.2341839892249,15.2,-4.13814333380918));
#182346=CARTESIAN_POINT('Ctrl Pts',(10.2383636611625,15.2,-4.138250209522));
#182347=CARTESIAN_POINT('Ctrl Pts',(10.2425574013331,15.2,-4.13835067442943));
#182348=CARTESIAN_POINT('Ctrl Pts',(10.2467651142304,15.2,-4.13844465353331));
#182349=CARTESIAN_POINT('Ctrl Pts',(10.250972827701,15.2,-4.13853863264999));
#182350=CARTESIAN_POINT('Ctrl Pts',(10.2551945171602,15.2,-4.13862612362064));
#182351=CARTESIAN_POINT('Ctrl Pts',(10.2594300857257,15.2,-4.13870704951327));
#182352=CARTESIAN_POINT('Ctrl Pts',(10.2647245461442,15.2,-4.13880820687354));
#182353=CARTESIAN_POINT('Ctrl Pts',(10.2700406943019,15.2,-4.13889910621697));
#182354=CARTESIAN_POINT('Ctrl Pts',(10.2753783489564,15.2,-4.1389795977439));
#182355=CARTESIAN_POINT('Ctrl Pts',(10.2796484723309,15.2,-4.13904399096018));
#182356=CARTESIAN_POINT('Ctrl Pts',(10.2839323598455,15.2,-4.13910172344558));
#182357=CARTESIAN_POINT('Ctrl Pts',(10.2882299191803,15.2,-4.13915271994167));
#182358=CARTESIAN_POINT('Ctrl Pts',(10.2925274791007,15.2,-4.13920371644471));
#182359=CARTESIAN_POINT('Ctrl Pts',(10.2968387104699,15.2,-4.13924797572704));
#182360=CARTESIAN_POINT('Ctrl Pts',(10.301163521707,15.2,-4.13928542550616));
#182361=CARTESIAN_POINT('Ctrl Pts',(10.3065695354587,15.2,-4.13933223772751));
#182362=CARTESIAN_POINT('Ctrl Pts',(10.3119967670497,15.2,-4.13936840649868));
#182363=CARTESIAN_POINT('Ctrl Pts',(10.3174450392042,15.2,-4.13939379122003));
#182364=CARTESIAN_POINT('Ctrl Pts',(10.3218036565715,15.2,-4.13941409899544));
#182365=CARTESIAN_POINT('Ctrl Pts',(10.3261757398855,15.2,-4.13942750317551));
#182366=CARTESIAN_POINT('Ctrl Pts',(10.3305611985469,15.2,-4.13943393300837));
#182367=CARTESIAN_POINT('Ctrl Pts',(10.3349466578058,15.2,-4.13944036284211));
#182368=CARTESIAN_POINT('Ctrl Pts',(10.3393454911545,15.2,-4.13943981621382));
#182369=CARTESIAN_POINT('Ctrl Pts',(10.3437576092296,15.2,-4.13943222349046));
#182370=CARTESIAN_POINT('Ctrl Pts',(10.349272756523,15.2,-4.13942273258679));
#182371=CARTESIAN_POINT('Ctrl Pts',(10.3548086625028,15.2,-4.13940223181903));
#182372=CARTESIAN_POINT('Ctrl Pts',(10.3603651497267,15.2,-4.1393705802209));
#182373=CARTESIAN_POINT('Ctrl Pts',(10.3636990419399,15.2,-4.13935158926271));
#182374=CARTESIAN_POINT('Ctrl Pts',(10.367040344268,15.2,-4.13932858562894));
#182375=CARTESIAN_POINT('Ctrl Pts',(10.3703890186062,15.2,-4.1393015390031));
#182376=CARTESIAN_POINT('Ctrl Pts',(10.3737376929443,15.2,-4.13927449237727));
#182377=CARTESIAN_POINT('Ctrl Pts',(10.3770937386549,15.2,-4.13924340157855));
#182378=CARTESIAN_POINT('Ctrl Pts',(10.3804571188666,15.2,-4.13920823903781));
#182379=CARTESIAN_POINT('Ctrl Pts',(10.3838204990784,15.2,-4.13917307649707));
#182380=CARTESIAN_POINT('Ctrl Pts',(10.387191214806,15.2,-4.13913384194847));
#182381=CARTESIAN_POINT('Ctrl Pts',(10.3905692270166,15.2,-4.13909050549171));
#182382=CARTESIAN_POINT('Ctrl Pts',(10.3939472392272,15.2,-4.13904716903495));
#182383=CARTESIAN_POINT('Ctrl Pts',(10.3973325487375,15.2,-4.13899973178669));
#182384=CARTESIAN_POINT('Ctrl Pts',(10.4007251184052,15.2,-4.13894816474726));
#182385=CARTESIAN_POINT('Ctrl Pts',(10.404117688073,15.2,-4.13889659770783));
#182386=CARTESIAN_POINT('Ctrl Pts',(10.4075175174619,15.2,-4.13884090054525));
#182387=CARTESIAN_POINT('Ctrl Pts',(10.4109245698825,15.2,-4.13878104500325));
#182388=CARTESIAN_POINT('Ctrl Pts',(10.414331622303,15.2,-4.13872118946125));
#182389=CARTESIAN_POINT('Ctrl Pts',(10.417745898246,15.2,-4.13865717557852));
#182390=CARTESIAN_POINT('Ctrl Pts',(10.4211673599957,15.2,-4.13858897503991));
#182391=CARTESIAN_POINT('Ctrl Pts',(10.424588822367,15.2,-4.1385207744889));
#182392=CARTESIAN_POINT('Ctrl Pts',(10.4280174708653,15.2,-4.13844838649505));
#182393=CARTESIAN_POINT('Ctrl Pts',(10.4314532686989,15.2,-4.13837178494167));
#182394=CARTESIAN_POINT('Ctrl Pts',(10.4348890659084,15.2,-4.13829518340222));
#182395=CARTESIAN_POINT('Ctrl Pts',(10.4383320128675,15.2,-4.13821436748798));
#182396=CARTESIAN_POINT('Ctrl Pts',(10.4417820716594,15.2,-4.1381293089907));
#182397=CARTESIAN_POINT('Ctrl Pts',(10.4452321304513,15.2,-4.13804425049342));
#182398=CARTESIAN_POINT('Ctrl Pts',(10.4486893029798,15.2,-4.137954949397));
#182399=CARTESIAN_POINT('Ctrl Pts',(10.452153551703,15.2,-4.13786137894162));
#182400=CARTESIAN_POINT('Ctrl Pts',(10.4556178004263,15.2,-4.13776780848625));
#182401=CARTESIAN_POINT('Ctrl Pts',(10.459089125224,15.2,-4.13766996939687));
#182402=CARTESIAN_POINT('Ctrl Pts',(10.4625674894884,15.2,-4.13756783198347));
#182403=CARTESIAN_POINT('Ctrl Pts',(10.4660458537528,15.2,-4.13746569457007));
#182404=CARTESIAN_POINT('Ctrl Pts',(10.4695312591635,15.2,-4.13735926119098));
#182405=CARTESIAN_POINT('Ctrl Pts',(10.4730236678693,15.2,-4.13724850327871));
#182406=CARTESIAN_POINT('Ctrl Pts',(10.4765160765752,15.2,-4.13713774536645));
#182407=CARTESIAN_POINT('Ctrl Pts',(10.4800154887472,15.2,-4.13702266442115));
#182408=CARTESIAN_POINT('Ctrl Pts',(10.4835218684938,15.2,-4.13690323200941));
#182409=CARTESIAN_POINT('Ctrl Pts',(10.4870282488775,15.2,-4.13678379957598));
#182410=CARTESIAN_POINT('Ctrl Pts',(10.4905415976714,15.2,-4.13666001699133));
#182411=CARTESIAN_POINT('Ctrl Pts',(10.4940618780173,15.2,-4.1365318574721));
#182412=CARTESIAN_POINT('Ctrl Pts',(10.4975821577237,15.2,-4.13640369797616));
#182413=CARTESIAN_POINT('Ctrl Pts',(10.5011093687848,15.2,-4.13627116164255));
#182414=CARTESIAN_POINT('Ctrl Pts',(10.5046434761671,15.2,-4.13613422076518));
#182415=CARTESIAN_POINT('Ctrl Pts',(10.5081775835493,15.2,-4.1359972798878));
#182416=CARTESIAN_POINT('Ctrl Pts',(10.511718587265,15.2,-4.13585593691251));
#182417=CARTESIAN_POINT('Ctrl Pts',(10.5152664514284,15.2,-4.13571016350075));
#182418=CARTESIAN_POINT('Ctrl Pts',(10.5188143155918,15.2,-4.13556439008899));
#182419=CARTESIAN_POINT('Ctrl Pts',(10.5223690392626,15.2,-4.13541418699443));
#182420=CARTESIAN_POINT('Ctrl Pts',(10.5259305885082,15.2,-4.13525952950005));
#182421=CARTESIAN_POINT('Ctrl Pts',(10.5294921377538,15.2,-4.13510487200567));
#182422=CARTESIAN_POINT('Ctrl Pts',(10.5330605122741,15.2,-4.13494575972813));
#182423=CARTESIAN_POINT('Ctrl Pts',(10.5366356755603,15.2,-4.1347821658178));
#182424=CARTESIAN_POINT('Ctrl Pts',(10.5402108388465,15.2,-4.13461857190747));
#182425=CARTESIAN_POINT('Ctrl Pts',(10.5437927921822,15.2,-4.13445049748077));
#182426=CARTESIAN_POINT('Ctrl Pts',(10.5473814989676,15.2,-4.13427791702933));
#182427=CARTESIAN_POINT('Ctrl Pts',(10.5509702064049,15.2,-4.13410533654653));
#182428=CARTESIAN_POINT('Ctrl Pts',(10.5545656688607,15.2,-4.13392824993746));
#182429=CARTESIAN_POINT('Ctrl Pts',(10.5581678497602,15.2,-4.13374663149378));
#182430=CARTESIAN_POINT('Ctrl Pts',(10.5617700300052,15.2,-4.1335650130831));
#182431=CARTESIAN_POINT('Ctrl Pts',(10.5653789295994,15.2,-4.1333788633829));
#182432=CARTESIAN_POINT('Ctrl Pts',(10.5689945134828,15.2,-4.13318815792144));
#182433=CARTESIAN_POINT('Ctrl Pts',(10.5726100973662,15.2,-4.13299745245998));
#182434=CARTESIAN_POINT('Ctrl Pts',(10.5762323649268,15.2,-4.13280219065466));
#182435=CARTESIAN_POINT('Ctrl Pts',(10.5798612816289,15.2,-4.13260234770319));
#182436=CARTESIAN_POINT('Ctrl Pts',(10.5834901983309,15.2,-4.13240250475172));
#182437=CARTESIAN_POINT('Ctrl Pts',(10.5871257633322,15.2,-4.13219808145912));
#182438=CARTESIAN_POINT('Ctrl Pts',(10.5907679434916,15.2,-4.13198905205005));
#182439=CARTESIAN_POINT('Ctrl Pts',(10.5956241841451,15.2,-4.13171034614597));
#182440=CARTESIAN_POINT('Ctrl Pts',(10.6004921836028,15.2,-4.13142345292149));
#182441=CARTESIAN_POINT('Ctrl Pts',(10.6053718603144,15.2,-4.13112831496012));
#182442=CARTESIAN_POINT('Ctrl Pts',(10.6090316175157,15.2,-4.1309069615092));
#182443=CARTESIAN_POINT('Ctrl Pts',(10.6126979423598,15.2,-4.13068097014239));
#182444=CARTESIAN_POINT('Ctrl Pts',(10.6163708017022,15.2,-4.13045031718038));
#182445=CARTESIAN_POINT('Ctrl Pts',(10.6200436610447,15.2,-4.13021966421836));
#182446=CARTESIAN_POINT('Ctrl Pts',(10.6237230529518,15.2,-4.12998434908217));
#182447=CARTESIAN_POINT('Ctrl Pts',(10.6274089446518,15.2,-4.12974434821548));
#182448=CARTESIAN_POINT('Ctrl Pts',(10.6310948363517,15.2,-4.12950434734879));
#182449=CARTESIAN_POINT('Ctrl Pts',(10.634787226951,15.2,-4.12925966237432));
#182450=CARTESIAN_POINT('Ctrl Pts',(10.6384860827332,15.2,-4.12901026700838));
#182451=CARTESIAN_POINT('Ctrl Pts',(10.6446508425944,15.2,-4.12859460805005));
#182452=CARTESIAN_POINT('Ctrl Pts',(10.6508335643418,15.2,-4.12816586986851));
#182453=CARTESIAN_POINT('Ctrl Pts',(10.6570340849949,15.2,-4.12772394174147));
#182454=CARTESIAN_POINT('Ctrl Pts',(10.6607543972517,15.2,-4.12745878487488));
#182455=CARTESIAN_POINT('Ctrl Pts',(10.6644811174486,15.2,-4.12718888029154));
#182456=CARTESIAN_POINT('Ctrl Pts',(10.6682142102465,15.2,-4.12691420296696));
#182457=CARTESIAN_POINT('Ctrl Pts',(10.6731916677626,15.2,-4.12654796650093));
#182458=CARTESIAN_POINT('Ctrl Pts',(10.6781804540799,15.2,-4.12617324751469));
#182459=CARTESIAN_POINT('Ctrl Pts',(10.6831804980757,15.2,-4.12578999493738));
#182460=CARTESIAN_POINT('Ctrl Pts',(10.686930530732,15.2,-4.12550255553051));
#182461=CARTESIAN_POINT('Ctrl Pts',(10.6906868948296,15.2,-4.12521031650721));
#182462=CARTESIAN_POINT('Ctrl Pts',(10.6944495569018,15.2,-4.12491325497592));
#182463=CARTESIAN_POINT('Ctrl Pts',(10.698212218974,15.2,-4.12461619344463));
#182464=CARTESIAN_POINT('Ctrl Pts',(10.70198117734,15.2,-4.12431430827337));
#182465=CARTESIAN_POINT('Ctrl Pts',(10.7057563905117,15.2,-4.1240075722831));
#182466=CARTESIAN_POINT('Ctrl Pts',(10.7095316036833,15.2,-4.12370083629283));
#182467=CARTESIAN_POINT('Ctrl Pts',(10.7133130716002,15.2,-4.12338924764025));
#182468=CARTESIAN_POINT('Ctrl Pts',(10.7171007630631,15.2,-4.12307278748367));
#182469=CARTESIAN_POINT('Ctrl Pts',(10.7234135823973,15.2,-4.1225453538702));
#182470=CARTESIAN_POINT('Ctrl Pts',(10.7297436872271,15.2,-4.12200439248384));
#182471=CARTESIAN_POINT('Ctrl Pts',(10.7360910470075,15.2,-4.12144986808671));
#182472=CARTESIAN_POINT('Ctrl Pts',(9.55499537099995,12.2,-4.04260911600002));
#182473=CARTESIAN_POINT('Ctrl Pts',(9.55669454752162,12.2,-4.04316130584455));
#182474=CARTESIAN_POINT('Ctrl Pts',(9.55844976514545,12.2,-4.04372605389323));
#182475=CARTESIAN_POINT('Ctrl Pts',(9.5602602775349,12.2,-4.04430244593687));
#182476=CARTESIAN_POINT('Ctrl Pts',(9.56207952113026,12.2,-4.0448816176343));
#182477=CARTESIAN_POINT('Ctrl Pts',(9.56395460122355,12.2,-4.04547254558642));
#182478=CARTESIAN_POINT('Ctrl Pts',(9.56588480617837,12.2,-4.04607433356657));
#182479=CARTESIAN_POINT('Ctrl Pts',(9.56781501095787,12.2,-4.04667612149206));
#182480=CARTESIAN_POINT('Ctrl Pts',(9.56980034124062,12.2,-4.04728876912262));
#182481=CARTESIAN_POINT('Ctrl Pts',(9.57184010199984,12.2,-4.04791140626666));
#182482=CARTESIAN_POINT('Ctrl Pts',(9.57387986275907,12.2,-4.04853404341071));
#182483=CARTESIAN_POINT('Ctrl Pts',(9.57597405360772,12.2,-4.04916667193806));
#182484=CARTESIAN_POINT('Ctrl Pts',(9.57812199955053,12.2,-4.04980844719627));
#182485=CARTESIAN_POINT('Ctrl Pts',(9.58026994568846,12.2,-4.05045022251278));
#182486=CARTESIAN_POINT('Ctrl Pts',(9.5824716464358,12.2,-4.0511011466437));
#182487=CARTESIAN_POINT('Ctrl Pts',(9.58472643972897,12.2,-4.05176039909686));
#182488=CARTESIAN_POINT('Ctrl Pts',(9.58698123281733,12.2,-4.05241965149014));
#182489=CARTESIAN_POINT('Ctrl Pts',(9.58928912248419,12.2,-4.05308723447175));
#182490=CARTESIAN_POINT('Ctrl Pts',(9.5916494594926,12.2,-4.05376235378364));
#182491=CARTESIAN_POINT('Ctrl Pts',(9.59400979650101,12.2,-4.05443747309554));
#182492=CARTESIAN_POINT('Ctrl Pts',(9.59642258389921,12.2,-4.0551201289628));
#182493=CARTESIAN_POINT('Ctrl Pts',(9.59888719089075,12.2,-4.05580954952079));
#182494=CARTESIAN_POINT('Ctrl Pts',(9.60135179810616,12.2,-4.0564989701414));
#182495=CARTESIAN_POINT('Ctrl Pts',(9.60386822553632,12.2,-4.05719515745453));
#182496=CARTESIAN_POINT('Ctrl Pts',(9.60643585601307,12.2,-4.05789736282655));
#182497=CARTESIAN_POINT('Ctrl Pts',(9.6090034862566,12.2,-4.05859956813477));
#182498=CARTESIAN_POINT('Ctrl Pts',(9.61162232317368,12.2,-4.05930778903961));
#182499=CARTESIAN_POINT('Ctrl Pts',(9.61429176141222,12.2,-4.06002130076391));
#182500=CARTESIAN_POINT('Ctrl Pts',(9.61696119965077,12.2,-4.06073481248822));
#182501=CARTESIAN_POINT('Ctrl Pts',(9.61968124046026,12.2,-4.06145361577042));
#182502=CARTESIAN_POINT('Ctrl Pts',(9.62245129460743,12.2,-4.06217699974393));
#182503=CARTESIAN_POINT('Ctrl Pts',(9.6252213487546,12.2,-4.06290038371745));
#182504=CARTESIAN_POINT('Ctrl Pts',(9.62804141715304,12.2,-4.06362835221376));
#182505=CARTESIAN_POINT('Ctrl Pts',(9.63091092146209,12.2,-4.0643602141869));
#182506=CARTESIAN_POINT('Ctrl Pts',(9.63378042603179,12.2,-4.06509207622652));
#182507=CARTESIAN_POINT('Ctrl Pts',(9.63669936976461,12.2,-4.06582783364988));
#182508=CARTESIAN_POINT('Ctrl Pts',(9.63966718442848,12.2,-4.06656681652363));
#182509=CARTESIAN_POINT('Ctrl Pts',(9.64263499882278,12.2,-4.06730579933026));
#182510=CARTESIAN_POINT('Ctrl Pts',(9.64565168593768,12.2,-4.06804800581502));
#182511=CARTESIAN_POINT('Ctrl Pts',(9.6487166922568,12.2,-4.068792787708));
#182512=CARTESIAN_POINT('Ctrl Pts',(9.65178169857594,12.2,-4.06953756960099));
#182513=CARTESIAN_POINT('Ctrl Pts',(9.65489502329009,12.2,-4.07028492392903));
#182514=CARTESIAN_POINT('Ctrl Pts',(9.65805612383864,12.2,-4.07103421890167));
#182515=CARTESIAN_POINT('Ctrl Pts',(9.66121722467433,12.2,-4.07178351394237));
#182516=CARTESIAN_POINT('Ctrl Pts',(9.66442610292301,12.2,-4.07253474644996));
#182517=CARTESIAN_POINT('Ctrl Pts',(9.66768222468585,12.2,-4.07328730149103));
#182518=CARTESIAN_POINT('Ctrl Pts',(9.67093834615294,12.2,-4.07403985646375));
#182519=CARTESIAN_POINT('Ctrl Pts',(9.67424171158829,12.2,-4.07479373162366));
#182520=CARTESIAN_POINT('Ctrl Pts',(9.67759179898168,12.2,-4.07554832576634));
#182521=CARTESIAN_POINT('Ctrl Pts',(9.68094188637507,12.2,-4.07630291990902));
#182522=CARTESIAN_POINT('Ctrl Pts',(9.68433869487785,12.2,-4.07705823111179));
#182523=CARTESIAN_POINT('Ctrl Pts',(9.68778171333292,12.2,-4.07781367441767));
#182524=CARTESIAN_POINT('Ctrl Pts',(9.69122473210076,12.2,-4.07856911779217));
#182525=CARTESIAN_POINT('Ctrl Pts',(9.69471395864503,12.2,-4.07932469331921));
#182526=CARTESIAN_POINT('Ctrl Pts',(9.69824889160027,12.2,-4.08007982581473));
#182527=CARTESIAN_POINT('Ctrl Pts',(9.70178382423443,12.2,-4.08083495824166));
#182528=CARTESIAN_POINT('Ctrl Pts',(9.70536446092327,12.2,-4.08158965017741));
#182529=CARTESIAN_POINT('Ctrl Pts',(9.70899030854153,12.2,-4.08234334148335));
#182530=CARTESIAN_POINT('Ctrl Pts',(9.7126161561598,12.2,-4.0830970327893));
#182531=CARTESIAN_POINT('Ctrl Pts',(9.71628721518416,12.2,-4.08384972393369));
#182532=CARTESIAN_POINT('Ctrl Pts',(9.72000299714885,12.2,-4.08460086944402));
#182533=CARTESIAN_POINT('Ctrl Pts',(9.72371877945107,12.2,-4.08535201502257));
#182534=CARTESIAN_POINT('Ctrl Pts',(9.72747928619589,12.2,-4.08610161413256));
#182535=CARTESIAN_POINT('Ctrl Pts',(9.73128403915626,12.2,-4.08684913758983));
#182536=CARTESIAN_POINT('Ctrl Pts',(9.73508879177105,12.2,-4.0875966609792));
#182537=CARTESIAN_POINT('Ctrl Pts',(9.73893778845863,12.2,-4.08834210619898));
#182538=CARTESIAN_POINT('Ctrl Pts',(9.74283056200164,12.2,-4.08908495475869));
#182539=CARTESIAN_POINT('Ctrl Pts',(9.74672333554465,12.2,-4.0898278033184));
#182540=CARTESIAN_POINT('Ctrl Pts',(9.75065988382131,12.2,-4.09056805421981));
#182541=CARTESIAN_POINT('Ctrl Pts',(9.75463974375815,12.2,-4.09130520269317));
#182542=CARTESIAN_POINT('Ctrl Pts',(9.75795629382602,12.2,-4.09191949310994));
#182543=CARTESIAN_POINT('Ctrl Pts',(9.76130292313634,12.2,-4.09253162599334));
#182544=CARTESIAN_POINT('Ctrl Pts',(9.76467936632923,12.2,-4.0931413174518));
#182545=CARTESIAN_POINT('Ctrl Pts',(9.76805580952212,12.2,-4.09375100891026));
#182546=CARTESIAN_POINT('Ctrl Pts',(9.77146206698804,12.2,-4.0943582577525));
#182547=CARTESIAN_POINT('Ctrl Pts',(9.77489787623967,12.2,-4.09496278094969));
#182548=CARTESIAN_POINT('Ctrl Pts',(9.77833368549131,12.2,-4.09556730414689));
#182549=CARTESIAN_POINT('Ctrl Pts',(9.78179904861098,12.2,-4.09616910386669));
#182550=CARTESIAN_POINT('Ctrl Pts',(9.78529370854153,12.2,-4.09676790199169));
#182551=CARTESIAN_POINT('Ctrl Pts',(9.78878836847207,12.2,-4.09736670011669));
#182552=CARTESIAN_POINT('Ctrl Pts',(9.79231232290782,12.2,-4.0979624962421));
#182553=CARTESIAN_POINT('Ctrl Pts',(9.79586532028515,12.2,-4.09855502096701));
#182554=CARTESIAN_POINT('Ctrl Pts',(9.79941831766247,12.2,-4.09914754569192));
#182555=CARTESIAN_POINT('Ctrl Pts',(9.80300035684025,12.2,-4.0997367967496));
#182556=CARTESIAN_POINT('Ctrl Pts',(9.80661118607787,12.2,-4.10032251001331));
#182557=CARTESIAN_POINT('Ctrl Pts',(9.8102220153155,12.2,-4.10090822327702));
#182558=CARTESIAN_POINT('Ctrl Pts',(9.8138616359329,12.2,-4.10149039863802));
#182559=CARTESIAN_POINT('Ctrl Pts',(9.81752979773994,12.2,-4.10206877280449));
#182560=CARTESIAN_POINT('Ctrl Pts',(9.82119795954699,12.2,-4.10264714697096));
#182561=CARTESIAN_POINT('Ctrl Pts',(9.82489466542211,12.2,-4.10322172219358));
#182562=CARTESIAN_POINT('Ctrl Pts',(9.82861966741573,12.2,-4.10379223979124));
#182563=CARTESIAN_POINT('Ctrl Pts',(9.83234466940933,12.2,-4.1043627573889));
#182564=CARTESIAN_POINT('Ctrl Pts',(9.83609796945329,12.2,-4.10492921825724));
#182565=CARTESIAN_POINT('Ctrl Pts',(9.83987932376116,12.2,-4.10549137159022));
#182566=CARTESIAN_POINT('Ctrl Pts',(9.84366067806901,12.2,-4.1060535249232));
#182567=CARTESIAN_POINT('Ctrl Pts',(9.84747008751064,12.2,-4.10661136957832));
#182568=CARTESIAN_POINT('Ctrl Pts',(9.85130731327679,12.2,-4.10716465881406));
#182569=CARTESIAN_POINT('Ctrl Pts',(9.8551445386247,12.2,-4.1077179479895));
#182570=CARTESIAN_POINT('Ctrl Pts',(9.85900957790061,12.2,-4.10826668100445));
#182571=CARTESIAN_POINT('Ctrl Pts',(9.86290219601573,12.2,-4.10881061594555));
#182572=CARTESIAN_POINT('Ctrl Pts',(9.86679481455514,12.2,-4.10935455094594));
#182573=CARTESIAN_POINT('Ctrl Pts',(9.87071501224689,12.2,-4.1098936868242));
#182574=CARTESIAN_POINT('Ctrl Pts',(9.87466255321688,12.2,-4.11042778613017));
#182575=CARTESIAN_POINT('Ctrl Pts',(9.87861009418686,12.2,-4.11096188543613));
#182576=CARTESIAN_POINT('Ctrl Pts',(9.88258497911197,12.2,-4.11149094733663));
#182577=CARTESIAN_POINT('Ctrl Pts',(9.88658697744309,12.2,-4.11201473823985));
#182578=CARTESIAN_POINT('Ctrl Pts',(9.8905889757742,12.2,-4.11253852914305));
#182579=CARTESIAN_POINT('Ctrl Pts',(9.89461808436726,12.2,-4.11305704849222));
#182580=CARTESIAN_POINT('Ctrl Pts',(9.8986740779708,12.2,-4.11357006615712));
#182581=CARTESIAN_POINT('Ctrl Pts',(9.90273007157434,12.2,-4.11408308382203));
#182582=CARTESIAN_POINT('Ctrl Pts',(9.90681294834378,12.2,-4.11459059951687));
#182583=CARTESIAN_POINT('Ctrl Pts',(9.91092248098127,12.2,-4.11509238722551));
#182584=CARTESIAN_POINT('Ctrl Pts',(9.91503201361877,12.2,-4.11559417493415));
#182585=CARTESIAN_POINT('Ctrl Pts',(9.9191682006014,12.2,-4.11609023581762));
#182586=CARTESIAN_POINT('Ctrl Pts',(9.9233308215028,12.2,-4.11658034519294));
#182587=CARTESIAN_POINT('Ctrl Pts',(9.92749344240421,12.2,-4.11707045456826));
#182588=CARTESIAN_POINT('Ctrl Pts',(9.93168249413961,12.2,-4.11755461470314));
#182589=CARTESIAN_POINT('Ctrl Pts',(9.93589775450592,12.2,-4.1180326049831));
#182590=CARTESIAN_POINT('Ctrl Pts',(9.93926996298274,12.2,-4.11841499722791));
#182591=CARTESIAN_POINT('Ctrl Pts',(9.9426589475333,12.2,-4.11879344171625));
#182592=CARTESIAN_POINT('Ctrl Pts',(9.94606459133171,12.2,-4.11916782856957));
#182593=CARTESIAN_POINT('Ctrl Pts',(9.94947023466611,12.2,-4.11954221537189));
#182594=CARTESIAN_POINT('Ctrl Pts',(9.95289254044834,12.2,-4.1199125437636));
#182595=CARTESIAN_POINT('Ctrl Pts',(9.95633139444391,12.2,-4.12027870467839));
#182596=CARTESIAN_POINT('Ctrl Pts',(9.95977024890802,12.2,-4.12064486564307));
#182597=CARTESIAN_POINT('Ctrl Pts',(9.96322565282856,12.2,-4.12100686132881));
#182598=CARTESIAN_POINT('Ctrl Pts',(9.96669749597043,12.2,-4.12136458231025));
#182599=CARTESIAN_POINT('Ctrl Pts',(9.97016933863925,12.2,-4.12172230324295));
#182600=CARTESIAN_POINT('Ctrl Pts',(9.9736576194761,12.2,-4.12207575038304));
#182601=CARTESIAN_POINT('Ctrl Pts',(9.97716222802187,12.2,-4.12242481668812));
#182602=CARTESIAN_POINT('Ctrl Pts',(9.98066683704513,12.2,-4.12277388304076));
#182603=CARTESIAN_POINT('Ctrl Pts',(9.98418777475925,12.2,-4.12311857191233));
#182604=CARTESIAN_POINT('Ctrl Pts',(9.98772493056419,12.2,-4.12345877431947));
#182605=CARTESIAN_POINT('Ctrl Pts',(9.9912620858872,12.2,-4.12379897668025));
#182606=CARTESIAN_POINT('Ctrl Pts',(9.99481546091078,12.2,-4.12413469573986));
#182607=CARTESIAN_POINT('Ctrl Pts',(9.99838494574035,12.2,-4.12446582795196));
#182608=CARTESIAN_POINT('Ctrl Pts',(10.0019544310563,12.2,-4.12479696020917));
#182609=CARTESIAN_POINT('Ctrl Pts',(10.0055400271249,12.2,-4.12512350483684));
#182610=CARTESIAN_POINT('Ctrl Pts',(10.0091416255445,12.2,-4.1254453610763));
#182611=CARTESIAN_POINT('Ctrl Pts',(10.0127432234733,12.2,-4.12576721727191));
#182612=CARTESIAN_POINT('Ctrl Pts',(10.0163608241128,12.2,-4.12608438442401));
#182613=CARTESIAN_POINT('Ctrl Pts',(10.0199943206475,12.2,-4.12639676273229));
#182614=CARTESIAN_POINT('Ctrl Pts',(10.0236278176772,12.2,-4.12670914108314));
#182615=CARTESIAN_POINT('Ctrl Pts',(10.0272772097665,12.2,-4.12701673166849));
#182616=CARTESIAN_POINT('Ctrl Pts',(10.0309423922607,12.2,-4.12731943274191));
#182617=CARTESIAN_POINT('Ctrl Pts',(10.0346075742556,12.2,-4.12762213377407));
#182618=CARTESIAN_POINT('Ctrl Pts',(10.038288546316,12.2,-4.12791994720614));
#182619=CARTESIAN_POINT('Ctrl Pts',(10.0419852016788,12.2,-4.12821277546049));
#182620=CARTESIAN_POINT('Ctrl Pts',(10.0456818575453,12.2,-4.12850560375473));
#182621=CARTESIAN_POINT('Ctrl Pts',(10.0493941990912,12.2,-4.1287934465374));
#182622=CARTESIAN_POINT('Ctrl Pts',(10.0531221195165,12.2,-4.1290762069417));
#182623=CARTESIAN_POINT('Ctrl Pts',(10.0568500399419,12.2,-4.129358967346));
#182624=CARTESIAN_POINT('Ctrl Pts',(10.060593539783,12.2,-4.12963664588026));
#182625=CARTESIAN_POINT('Ctrl Pts',(10.0643525161561,12.2,-4.12990914756125));
#182626=CARTESIAN_POINT('Ctrl Pts',(10.0681114920171,12.2,-4.13018164920511));
#182627=CARTESIAN_POINT('Ctrl Pts',(10.0718859430372,12.2,-4.13044897388674));
#182628=CARTESIAN_POINT('Ctrl Pts',(10.0756757670223,12.2,-4.13071102753319));
#182629=CARTESIAN_POINT('Ctrl Pts',(10.0794655915238,12.2,-4.13097308121535));
#182630=CARTESIAN_POINT('Ctrl Pts',(10.0832707885925,12.2,-4.13122986304465));
#182631=CARTESIAN_POINT('Ctrl Pts',(10.0870912563579,12.2,-4.13148128205781));
#182632=CARTESIAN_POINT('Ctrl Pts',(10.0909117236027,12.2,-4.13173270103671));
#182633=CARTESIAN_POINT('Ctrl Pts',(10.094747460351,12.2,-4.13197875561629));
#182634=CARTESIAN_POINT('Ctrl Pts',(10.0985983657019,12.2,-4.13221935526365));
#182635=CARTESIAN_POINT('Ctrl Pts',(10.103411997784,12.2,-4.13252010484743));
#182636=CARTESIAN_POINT('Ctrl Pts',(10.1082493314363,12.2,-4.13281233050412));
#182637=CARTESIAN_POINT('Ctrl Pts',(10.1131101684722,12.2,-4.13309585599155));
#182638=CARTESIAN_POINT('Ctrl Pts',(10.1169988383129,12.2,-4.13332267639385));
#182639=CARTESIAN_POINT('Ctrl Pts',(10.1209025498061,12.2,-4.13354392809078));
#182640=CARTESIAN_POINT('Ctrl Pts',(10.1248212036323,12.2,-4.13375952376862));
#182641=CARTESIAN_POINT('Ctrl Pts',(10.1287398569245,12.2,-4.13397511941709));
#182642=CARTESIAN_POINT('Ctrl Pts',(10.1326734528343,12.2,-4.13418505804406));
#182643=CARTESIAN_POINT('Ctrl Pts',(10.1366218901772,12.2,-4.13438925124996));
#182644=CARTESIAN_POINT('Ctrl Pts',(10.1405703280581,12.2,-4.13459344448368));
#182645=CARTESIAN_POINT('Ctrl Pts',(10.1445336093409,12.2,-4.13479189414723));
#182646=CARTESIAN_POINT('Ctrl Pts',(10.1485116340355,12.2,-4.13498451127796));
#182647=CARTESIAN_POINT('Ctrl Pts',(10.1524896581881,12.2,-4.13517712838243));
#182648=CARTESIAN_POINT('Ctrl Pts',(10.1564824255565,12.2,-4.13536391397459));
#182649=CARTESIAN_POINT('Ctrl Pts',(10.1604898376724,12.2,-4.1355447824602));
#182650=CARTESIAN_POINT('Ctrl Pts',(10.1654991032268,12.2,-4.13577086808568));
#182651=CARTESIAN_POINT('Ctrl Pts',(10.1705312521651,12.2,-4.13598770798037));
#182652=CARTESIAN_POINT('Ctrl Pts',(10.1755860941778,12.2,-4.13619513770308));
#182653=CARTESIAN_POINT('Ctrl Pts',(10.1806409361905,12.2,-4.1364025674258));
#182654=CARTESIAN_POINT('Ctrl Pts',(10.1857184691399,12.2,-4.13660058640938));
#182655=CARTESIAN_POINT('Ctrl Pts',(10.1908185069165,12.2,-4.13678903272932));
#182656=CARTESIAN_POINT('Ctrl Pts',(10.1948985373601,12.2,-4.1369397897935));
#182657=CARTESIAN_POINT('Ctrl Pts',(10.1989929690824,12.2,-4.13708442016451));
#182658=CARTESIAN_POINT('Ctrl Pts',(10.2031017078462,12.2,-4.13722284201176));
#182659=CARTESIAN_POINT('Ctrl Pts',(10.2072104460501,12.2,-4.13736126384015));
#182660=CARTESIAN_POINT('Ctrl Pts',(10.2113334891454,12.2,-4.13749347692179));
#182661=CARTESIAN_POINT('Ctrl Pts',(10.2154707436951,12.2,-4.13761940068969));
#182662=CARTESIAN_POINT('Ctrl Pts',(10.2196079988086,12.2,-4.13774532447474));
#182663=CARTESIAN_POINT('Ctrl Pts',(10.2237594636015,12.2,-4.13786495893404));
#182664=CARTESIAN_POINT('Ctrl Pts',(10.2279250436072,12.2,-4.13797822355091));
#182665=CARTESIAN_POINT('Ctrl Pts',(10.2341734130482,12.2,-4.13814812046077));
#182666=CARTESIAN_POINT('Ctrl Pts',(10.2404535445977,12.2,-4.13830368487109));
#182667=CARTESIAN_POINT('Ctrl Pts',(10.2467651142304,12.2,-4.13844465353331));
#182668=CARTESIAN_POINT('Ctrl Pts',(10.250972827701,12.2,-4.13853863264999));
#182669=CARTESIAN_POINT('Ctrl Pts',(10.2551945171602,12.2,-4.13862612362064));
#182670=CARTESIAN_POINT('Ctrl Pts',(10.2594300857257,12.2,-4.13870704951327));
#182671=CARTESIAN_POINT('Ctrl Pts',(10.2636656537142,12.2,-4.13878797539487));
#182672=CARTESIAN_POINT('Ctrl Pts',(10.2679151012315,12.2,-4.13886233664676));
#182673=CARTESIAN_POINT('Ctrl Pts',(10.2721783371598,12.2,-4.13893005525278));
#182674=CARTESIAN_POINT('Ctrl Pts',(10.2775073825059,12.2,-4.13901470351721));
#182675=CARTESIAN_POINT('Ctrl Pts',(10.2828579695726,12.2,-4.13908897431635));
#182676=CARTESIAN_POINT('Ctrl Pts',(10.2882299191803,12.2,-4.13915271994167));
#182677=CARTESIAN_POINT('Ctrl Pts',(10.2925274791007,12.2,-4.13920371644471));
#182678=CARTESIAN_POINT('Ctrl Pts',(10.2968387104699,12.2,-4.13924797572704));
#182679=CARTESIAN_POINT('Ctrl Pts',(10.301163521707,12.2,-4.13928542550616));
#182680=CARTESIAN_POINT('Ctrl Pts',(10.3054883323548,12.2,-4.13932287528018));
#182681=CARTESIAN_POINT('Ctrl Pts',(10.3098267223898,12.2,-4.13935351428841));
#182682=CARTESIAN_POINT('Ctrl Pts',(10.3141786011443,12.2,-4.13937726773137));
#182683=CARTESIAN_POINT('Ctrl Pts',(10.3185304804917,12.2,-4.13940102117756));
#182684=CARTESIAN_POINT('Ctrl Pts',(10.3228958479601,12.2,-4.13941789142879));
#182685=CARTESIAN_POINT('Ctrl Pts',(10.3272746140854,12.2,-4.13942780398478));
#182686=CARTESIAN_POINT('Ctrl Pts',(10.331653379614,12.2,-4.13943771653941));
#182687=CARTESIAN_POINT('Ctrl Pts',(10.3360455427231,12.2,-4.1394406720634));
#182688=CARTESIAN_POINT('Ctrl Pts',(10.3404510121399,12.2,-4.13943659800864));
#182689=CARTESIAN_POINT('Ctrl Pts',(10.345957849361,12.2,-4.13943150543977));
#182690=CARTESIAN_POINT('Ctrl Pts',(10.3514854804938,12.2,-4.13941543110673));
#182691=CARTESIAN_POINT('Ctrl Pts',(10.3570337276455,12.2,-4.13938823430175));
#182692=CARTESIAN_POINT('Ctrl Pts',(10.3603626758156,12.2,-4.13937191621936));
#182693=CARTESIAN_POINT('Ctrl Pts',(10.3636990465083,12.2,-4.13935159357125));
#182694=CARTESIAN_POINT('Ctrl Pts',(10.3670428018864,12.2,-4.13932723898805));
#182695=CARTESIAN_POINT('Ctrl Pts',(10.3715011427954,12.2,-4.1392947662075));
#182696=CARTESIAN_POINT('Ctrl Pts',(10.3759726115103,12.2,-4.13925512242972));
#182697=CARTESIAN_POINT('Ctrl Pts',(10.3804571188666,12.2,-4.13920823903781));
#182698=CARTESIAN_POINT('Ctrl Pts',(10.3838204990784,12.2,-4.13917307649707));
#182699=CARTESIAN_POINT('Ctrl Pts',(10.387191214806,12.2,-4.13913384194847));
#182700=CARTESIAN_POINT('Ctrl Pts',(10.3905692270166,12.2,-4.13909050549171));
#182701=CARTESIAN_POINT('Ctrl Pts',(10.3939472392272,12.2,-4.13904716903495));
#182702=CARTESIAN_POINT('Ctrl Pts',(10.3973325487375,12.2,-4.13899973178669));
#182703=CARTESIAN_POINT('Ctrl Pts',(10.4007251184052,12.2,-4.13894816474726));
#182704=CARTESIAN_POINT('Ctrl Pts',(10.404117688073,12.2,-4.13889659770783));
#182705=CARTESIAN_POINT('Ctrl Pts',(10.4075175174619,12.2,-4.13884090054525));
#182706=CARTESIAN_POINT('Ctrl Pts',(10.4109245698825,12.2,-4.13878104500325));
#182707=CARTESIAN_POINT('Ctrl Pts',(10.4154673068559,12.2,-4.13870123760667));
#182708=CARTESIAN_POINT('Ctrl Pts',(10.4200228851903,12.2,-4.13861403773121));
#182709=CARTESIAN_POINT('Ctrl Pts',(10.4245912171068,12.2,-4.13851937772557));
#182710=CARTESIAN_POINT('Ctrl Pts',(10.4280174657329,12.2,-4.13844838272778));
#182711=CARTESIAN_POINT('Ctrl Pts',(10.4314508876582,12.2,-4.13837319186383));
#182712=CARTESIAN_POINT('Ctrl Pts',(10.4348914472832,12.2,-4.13829377778338));
#182713=CARTESIAN_POINT('Ctrl Pts',(10.4383320069082,12.2,-4.13821436370293));
#182714=CARTESIAN_POINT('Ctrl Pts',(10.4417797023996,12.2,-4.13813072507266));
#182715=CARTESIAN_POINT('Ctrl Pts',(10.4452344995651,12.2,-4.13804283549289));
#182716=CARTESIAN_POINT('Ctrl Pts',(10.4486892967306,12.2,-4.13795494591312));
#182717=CARTESIAN_POINT('Ctrl Pts',(10.4521511950657,12.2,-4.13786280395281));
#182718=CARTESIAN_POINT('Ctrl Pts',(10.4556201573621,12.2,-4.13776638478532));
#182719=CARTESIAN_POINT('Ctrl Pts',(10.4590891196586,12.2,-4.13766996561784));
#182720=CARTESIAN_POINT('Ctrl Pts',(10.4625651445681,12.2,-4.13756926605186));
#182721=CARTESIAN_POINT('Ctrl Pts',(10.4660481987323,12.2,-4.1374642615146));
#182722=CARTESIAN_POINT('Ctrl Pts',(10.4695312535292,12.2,-4.13735925695826));
#182723=CARTESIAN_POINT('Ctrl Pts',(10.4730213366697,12.2,-4.13724994624237));
#182724=CARTESIAN_POINT('Ctrl Pts',(10.4765184110123,12.2,-4.1371363031836));
#182725=CARTESIAN_POINT('Ctrl Pts',(10.4800154847195,12.2,-4.13702266014548));
#182726=CARTESIAN_POINT('Ctrl Pts',(10.4835195496597,12.2,-4.13690468398257));
#182727=CARTESIAN_POINT('Ctrl Pts',(10.487030570866,12.2,-4.13678234848664));
#182728=CARTESIAN_POINT('Ctrl Pts',(10.4905415920724,12.2,-4.1366600129907));
#182729=CARTESIAN_POINT('Ctrl Pts',(10.4940595695318,12.2,-4.13653331849578));
#182730=CARTESIAN_POINT('Ctrl Pts',(10.4975844662531,12.2,-4.13640223799993));
#182731=CARTESIAN_POINT('Ctrl Pts',(10.5022843283347,12.2,-4.1362274640134));
#182732=CARTESIAN_POINT('Ctrl Pts',(10.5069964919344,12.2,-4.13604489120647));
#182733=CARTESIAN_POINT('Ctrl Pts',(10.5117208739358,12.2,-4.13585446105618));
#182734=CARTESIAN_POINT('Ctrl Pts',(10.5152641612415,12.2,-4.13571163841102));
#182735=CARTESIAN_POINT('Ctrl Pts',(10.5188143204241,12.2,-4.13556439348963));
#182736=CARTESIAN_POINT('Ctrl Pts',(10.5223713162753,12.2,-4.13541270296697));
#182737=CARTESIAN_POINT('Ctrl Pts',(10.5259283114804,12.2,-4.13526101247188));
#182738=CARTESIAN_POINT('Ctrl Pts',(10.5294921442017,12.2,-4.13510487574368));
#182739=CARTESIAN_POINT('Ctrl Pts',(10.5330627774475,12.2,-4.13494426670747));
#182740=CARTESIAN_POINT('Ctrl Pts',(10.5366334106934,12.2,-4.13478365767124));
#182741=CARTESIAN_POINT('Ctrl Pts',(10.5402108452635,12.2,-4.13461857531055));
#182742=CARTESIAN_POINT('Ctrl Pts',(10.5437950455082,12.2,-4.13444899627505));
#182743=CARTESIAN_POINT('Ctrl Pts',(10.547379245753,12.2,-4.13427941723954));
#182744=CARTESIAN_POINT('Ctrl Pts',(10.5509702119392,12.2,-4.13410534024589));
#182745=CARTESIAN_POINT('Ctrl Pts',(10.5545679091412,12.2,-4.13392674025277));
#182746=CARTESIAN_POINT('Ctrl Pts',(10.5581656063432,12.2,-4.13374814025966));
#182747=CARTESIAN_POINT('Ctrl Pts',(10.5617700336362,12.2,-4.13356501678834));
#182748=CARTESIAN_POINT('Ctrl Pts',(10.565381157518,12.2,-4.13337734582798));
#182749=CARTESIAN_POINT('Ctrl Pts',(10.5689922813997,12.2,-4.13318967486761));
#182750=CARTESIAN_POINT('Ctrl Pts',(10.5726101010257,12.2,-4.1329974566685));
#182751=CARTESIAN_POINT('Ctrl Pts',(10.5762345812264,12.2,-4.13280066480128));
#182752=CARTESIAN_POINT('Ctrl Pts',(10.5822753817805,12.2,-4.13247267834398));
#182753=CARTESIAN_POINT('Ctrl Pts',(10.5883346833564,12.2,-4.13213199052301));
#182754=CARTESIAN_POINT('Ctrl Pts',(10.59441232648,12.2,-4.13177848649628));
#182755=CARTESIAN_POINT('Ctrl Pts',(10.598058912884,12.2,-4.13156638404942));
#182756=CARTESIAN_POINT('Ctrl Pts',(10.6017121024483,12.2,-4.13134966845126));
#182757=CARTESIAN_POINT('Ctrl Pts',(10.6053718603144,12.2,-4.13112831496012));
#182758=CARTESIAN_POINT('Ctrl Pts',(10.6090316175157,12.2,-4.13090696150919));
#182759=CARTESIAN_POINT('Ctrl Pts',(10.6126979423598,12.2,-4.13068097014239));
#182760=CARTESIAN_POINT('Ctrl Pts',(10.6163708017022,12.2,-4.13045031718038));
#182761=CARTESIAN_POINT('Ctrl Pts',(10.6200436610447,12.2,-4.13021966421836));
#182762=CARTESIAN_POINT('Ctrl Pts',(10.6237230529518,12.2,-4.12998434908217));
#182763=CARTESIAN_POINT('Ctrl Pts',(10.6274089446518,12.2,-4.12974434821548));
#182764=CARTESIAN_POINT('Ctrl Pts',(10.6310948363517,12.2,-4.12950434734879));
#182765=CARTESIAN_POINT('Ctrl Pts',(10.634787226951,12.2,-4.12925966237432));
#182766=CARTESIAN_POINT('Ctrl Pts',(10.6384860827332,12.2,-4.12901026700838));
#182767=CARTESIAN_POINT('Ctrl Pts',(10.6434178908909,12.2,-4.12867773982359));
#182768=CARTESIAN_POINT('Ctrl Pts',(10.6483611945277,12.2,-4.12833684195172));
#182769=CARTESIAN_POINT('Ctrl Pts',(10.6533159105767,12.2,-4.1279875167096));
#182770=CARTESIAN_POINT('Ctrl Pts',(10.6595093046253,12.2,-4.12755086022833));
#182771=CARTESIAN_POINT('Ctrl Pts',(10.6657205291267,12.2,-4.12710103528128));
#182772=CARTESIAN_POINT('Ctrl Pts',(10.6719494256685,12.2,-4.12663793456895));
#182773=CARTESIAN_POINT('Ctrl Pts',(10.6756867645441,12.2,-4.12636007407089));
#182774=CARTESIAN_POINT('Ctrl Pts',(10.6794304647382,12.2,-4.12607743439647));
#182775=CARTESIAN_POINT('Ctrl Pts',(10.6831804980757,12.2,-4.12578999493738));
#182776=CARTESIAN_POINT('Ctrl Pts',(10.686930530732,12.2,-4.1255025555305));
#182777=CARTESIAN_POINT('Ctrl Pts',(10.6906868948296,12.2,-4.12521031650721));
#182778=CARTESIAN_POINT('Ctrl Pts',(10.6944495569018,12.2,-4.12491325497592));
#182779=CARTESIAN_POINT('Ctrl Pts',(10.698212218974,12.2,-4.12461619344463));
#182780=CARTESIAN_POINT('Ctrl Pts',(10.70198117734,12.2,-4.12431430827338));
#182781=CARTESIAN_POINT('Ctrl Pts',(10.7057563905117,12.2,-4.1240075722831));
#182782=CARTESIAN_POINT('Ctrl Pts',(10.7095316036833,12.2,-4.12370083629283));
#182783=CARTESIAN_POINT('Ctrl Pts',(10.7133130716002,12.2,-4.12338924764025));
#182784=CARTESIAN_POINT('Ctrl Pts',(10.7171007630631,12.2,-4.12307278748367));
#182785=CARTESIAN_POINT('Ctrl Pts',(10.7234135823973,12.2,-4.1225453538702));
#182786=CARTESIAN_POINT('Ctrl Pts',(10.7297436872271,12.2,-4.12200439248384));
#182787=CARTESIAN_POINT('Ctrl Pts',(10.7360910470075,12.2,-4.12144986808672));
#182788=CARTESIAN_POINT('Ctrl Pts',(10.8675859439999,15.2,-3.76106045600002));
#182789=CARTESIAN_POINT('Ctrl Pts',(10.8675859439999,11.6,-3.76106045600002));
#182790=CARTESIAN_POINT('Ctrl Pts',(10.8670460909999,15.2,-3.76051902400001));
#182791=CARTESIAN_POINT('Ctrl Pts',(10.8670460909999,11.6,-3.76051902400001));
#182792=CARTESIAN_POINT('Ctrl Pts',(10.8659664939999,15.2,-3.75943667400001));
#182793=CARTESIAN_POINT('Ctrl Pts',(10.8659664939999,11.6,-3.75943667400001));
#182794=CARTESIAN_POINT('Ctrl Pts',(10.8643474199999,15.2,-3.75781469800001));
#182795=CARTESIAN_POINT('Ctrl Pts',(10.8643474199999,11.6,-3.75781469800002));
#182796=CARTESIAN_POINT('Ctrl Pts',(10.8621893019999,15.2,-3.75565515600002));
#182797=CARTESIAN_POINT('Ctrl Pts',(10.8621893019999,11.6,-3.75565515600002));
#182798=CARTESIAN_POINT('Ctrl Pts',(10.8594927299999,15.2,-3.75296088400002));
#182799=CARTESIAN_POINT('Ctrl Pts',(10.8594927299999,11.6,-3.75296088400002));
#182800=CARTESIAN_POINT('Ctrl Pts',(10.8567972349999,15.2,-3.75027176800002));
#182801=CARTESIAN_POINT('Ctrl Pts',(10.8567972349999,11.6,-3.75027176800002));
#182802=CARTESIAN_POINT('Ctrl Pts',(10.8541028209999,15.2,-3.74758780800001));
#182803=CARTESIAN_POINT('Ctrl Pts',(10.8541028209999,11.6,-3.74758780800002));
#182804=CARTESIAN_POINT('Ctrl Pts',(10.8514094899999,15.2,-3.74490900600001));
#182805=CARTESIAN_POINT('Ctrl Pts',(10.8514094899999,11.6,-3.74490900600001));
#182806=CARTESIAN_POINT('Ctrl Pts',(10.8487172499999,15.2,-3.74223536100001));
#182807=CARTESIAN_POINT('Ctrl Pts',(10.8487172499999,11.6,-3.74223536100002));
#182808=CARTESIAN_POINT('Ctrl Pts',(10.8460261069999,15.2,-3.73956687500002));
#182809=CARTESIAN_POINT('Ctrl Pts',(10.8460261069999,11.6,-3.73956687500002));
#182810=CARTESIAN_POINT('Ctrl Pts',(10.8433360699999,15.2,-3.73690354800001));
#182811=CARTESIAN_POINT('Ctrl Pts',(10.8433360699999,11.6,-3.73690354800001));
#182812=CARTESIAN_POINT('Ctrl Pts',(10.8406471529999,15.2,-3.73424538200001));
#182813=CARTESIAN_POINT('Ctrl Pts',(10.8406471529999,11.6,-3.73424538200001));
#182814=CARTESIAN_POINT('Ctrl Pts',(10.8379593649999,15.2,-3.73159237800001));
#182815=CARTESIAN_POINT('Ctrl Pts',(10.8379593649999,11.6,-3.73159237800001));
#182816=CARTESIAN_POINT('Ctrl Pts',(10.8352727169999,15.2,-3.72894453800001));
#182817=CARTESIAN_POINT('Ctrl Pts',(10.8352727169999,11.6,-3.72894453800001));
#182818=CARTESIAN_POINT('Ctrl Pts',(10.8325872199999,15.2,-3.72630186200002));
#182819=CARTESIAN_POINT('Ctrl Pts',(10.8325872199999,11.6,-3.72630186200002));
#182820=CARTESIAN_POINT('Ctrl Pts',(10.8299028829999,15.2,-3.72366435100002));
#182821=CARTESIAN_POINT('Ctrl Pts',(10.8299028829999,11.6,-3.72366435100002));
#182822=CARTESIAN_POINT('Ctrl Pts',(10.8272197149999,15.2,-3.72103200700002));
#182823=CARTESIAN_POINT('Ctrl Pts',(10.8272197149999,11.6,-3.72103200700002));
#182824=CARTESIAN_POINT('Ctrl Pts',(10.8245377239999,15.2,-3.71840483100002));
#182825=CARTESIAN_POINT('Ctrl Pts',(10.8245377239999,11.6,-3.71840483100002));
#182826=CARTESIAN_POINT('Ctrl Pts',(10.8218569179999,15.2,-3.71578282200002));
#182827=CARTESIAN_POINT('Ctrl Pts',(10.8218569179999,11.6,-3.71578282200002));
#182828=CARTESIAN_POINT('Ctrl Pts',(10.8191773059999,15.2,-3.71316598200002));
#182829=CARTESIAN_POINT('Ctrl Pts',(10.8191773059999,11.6,-3.71316598200002));
#182830=CARTESIAN_POINT('Ctrl Pts',(10.8164988939999,15.2,-3.71055431200002));
#182831=CARTESIAN_POINT('Ctrl Pts',(10.8164988939999,11.6,-3.71055431200002));
#182832=CARTESIAN_POINT('Ctrl Pts',(10.8138216939999,15.2,-3.70794781300001));
#182833=CARTESIAN_POINT('Ctrl Pts',(10.8138216939999,11.6,-3.70794781300001));
#182834=CARTESIAN_POINT('Ctrl Pts',(10.8111457129999,15.2,-3.70534648600001));
#182835=CARTESIAN_POINT('Ctrl Pts',(10.8111457129999,11.6,-3.70534648600001));
#182836=CARTESIAN_POINT('Ctrl Pts',(10.8084709609999,15.2,-3.70275033200001));
#182837=CARTESIAN_POINT('Ctrl Pts',(10.8084709609999,11.6,-3.70275033200001));
#182838=CARTESIAN_POINT('Ctrl Pts',(10.8057974489999,15.2,-3.70015935000001));
#182839=CARTESIAN_POINT('Ctrl Pts',(10.8057974489999,11.6,-3.70015935000001));
#182840=CARTESIAN_POINT('Ctrl Pts',(10.8031251839999,15.2,-3.69757354500001));
#182841=CARTESIAN_POINT('Ctrl Pts',(10.8031251839999,11.6,-3.69757354500001));
#182842=CARTESIAN_POINT('Ctrl Pts',(10.8004541779999,15.2,-3.69499291500002));
#182843=CARTESIAN_POINT('Ctrl Pts',(10.8004541779999,11.6,-3.69499291500002));
#182844=CARTESIAN_POINT('Ctrl Pts',(10.7977844379999,15.2,-3.69241746100001));
#182845=CARTESIAN_POINT('Ctrl Pts',(10.7977844379999,11.6,-3.69241746100002));
#182846=CARTESIAN_POINT('Ctrl Pts',(10.7951159729999,15.2,-3.68984718400001));
#182847=CARTESIAN_POINT('Ctrl Pts',(10.7951159729999,11.6,-3.68984718400002));
#182848=CARTESIAN_POINT('Ctrl Pts',(10.7924487949999,15.2,-3.68728208700002));
#182849=CARTESIAN_POINT('Ctrl Pts',(10.7924487949999,11.6,-3.68728208700002));
#182850=CARTESIAN_POINT('Ctrl Pts',(10.7897829079999,15.2,-3.68472216800001));
#182851=CARTESIAN_POINT('Ctrl Pts',(10.7897829079999,11.6,-3.68472216800001));
#182852=CARTESIAN_POINT('Ctrl Pts',(10.7871183259999,15.2,-3.68216742900001));
#182853=CARTESIAN_POINT('Ctrl Pts',(10.7871183259999,11.6,-3.68216742900001));
#182854=CARTESIAN_POINT('Ctrl Pts',(10.7844550569999,15.2,-3.67961787200001));
#182855=CARTESIAN_POINT('Ctrl Pts',(10.7844550569999,11.6,-3.67961787200001));
#182856=CARTESIAN_POINT('Ctrl Pts',(10.7817931069999,15.2,-3.67707349500002));
#182857=CARTESIAN_POINT('Ctrl Pts',(10.7817931069999,11.6,-3.67707349500002));
#182858=CARTESIAN_POINT('Ctrl Pts',(10.7791324889999,15.2,-3.67453430200001));
#182859=CARTESIAN_POINT('Ctrl Pts',(10.7791324889999,11.6,-3.67453430200001));
#182860=CARTESIAN_POINT('Ctrl Pts',(10.7764732109999,15.2,-3.67200029300002));
#182861=CARTESIAN_POINT('Ctrl Pts',(10.7764732109999,11.6,-3.67200029300002));
#182862=CARTESIAN_POINT('Ctrl Pts',(10.7738152829999,15.2,-3.66947146800001));
#182863=CARTESIAN_POINT('Ctrl Pts',(10.7738152829999,11.6,-3.66947146800001));
#182864=CARTESIAN_POINT('Ctrl Pts',(10.7711587129999,15.2,-3.66694782800002));
#182865=CARTESIAN_POINT('Ctrl Pts',(10.7711587129999,11.6,-3.66694782800002));
#182866=CARTESIAN_POINT('Ctrl Pts',(10.7685035109999,15.2,-3.66442937400001));
#182867=CARTESIAN_POINT('Ctrl Pts',(10.7685035109999,11.6,-3.66442937400001));
#182868=CARTESIAN_POINT('Ctrl Pts',(10.7658496859999,15.2,-3.66191610700001));
#182869=CARTESIAN_POINT('Ctrl Pts',(10.7658496859999,11.6,-3.66191610700001));
#182870=CARTESIAN_POINT('Ctrl Pts',(10.7631972489999,15.2,-3.65940802800001));
#182871=CARTESIAN_POINT('Ctrl Pts',(10.7631972489999,11.6,-3.65940802800001));
#182872=CARTESIAN_POINT('Ctrl Pts',(10.7605462079999,15.2,-3.65690513800002));
#182873=CARTESIAN_POINT('Ctrl Pts',(10.7605462079999,11.6,-3.65690513800002));
#182874=CARTESIAN_POINT('Ctrl Pts',(10.7578965719999,15.2,-3.65440743700002));
#182875=CARTESIAN_POINT('Ctrl Pts',(10.7578965719999,11.6,-3.65440743700002));
#182876=CARTESIAN_POINT('Ctrl Pts',(10.7552483519999,15.2,-3.65191492600001));
#182877=CARTESIAN_POINT('Ctrl Pts',(10.7552483519999,11.6,-3.65191492600002));
#182878=CARTESIAN_POINT('Ctrl Pts',(10.7526015559999,15.2,-3.64942760700002));
#182879=CARTESIAN_POINT('Ctrl Pts',(10.7526015559999,11.6,-3.64942760700002));
#182880=CARTESIAN_POINT('Ctrl Pts',(10.7499561929999,15.2,-3.64694547900001));
#182881=CARTESIAN_POINT('Ctrl Pts',(10.7499561929999,11.6,-3.64694547900001));
#182882=CARTESIAN_POINT('Ctrl Pts',(10.7473122739999,15.2,-3.64446854400001));
#182883=CARTESIAN_POINT('Ctrl Pts',(10.7473122739999,11.6,-3.64446854400002));
#182884=CARTESIAN_POINT('Ctrl Pts',(10.7446698079999,15.2,-3.64199680200001));
#182885=CARTESIAN_POINT('Ctrl Pts',(10.7446698079999,11.6,-3.64199680200001));
#182886=CARTESIAN_POINT('Ctrl Pts',(10.7420288039999,15.2,-3.63953025500001));
#182887=CARTESIAN_POINT('Ctrl Pts',(10.7420288039999,11.6,-3.63953025500001));
#182888=CARTESIAN_POINT('Ctrl Pts',(10.7393892719999,15.2,-3.63706890200001));
#182889=CARTESIAN_POINT('Ctrl Pts',(10.7393892719999,11.6,-3.63706890200001));
#182890=CARTESIAN_POINT('Ctrl Pts',(10.7367512209999,15.2,-3.63461274500001));
#182891=CARTESIAN_POINT('Ctrl Pts',(10.7367512209999,11.6,-3.63461274500001));
#182892=CARTESIAN_POINT('Ctrl Pts',(10.7341146619999,15.2,-3.63216178500001));
#182893=CARTESIAN_POINT('Ctrl Pts',(10.7341146619999,11.6,-3.63216178500001));
#182894=CARTESIAN_POINT('Ctrl Pts',(10.7314796019999,15.2,-3.62971602300002));
#182895=CARTESIAN_POINT('Ctrl Pts',(10.7314796019999,11.6,-3.62971602300002));
#182896=CARTESIAN_POINT('Ctrl Pts',(10.7288460529999,15.2,-3.62727545700002));
#182897=CARTESIAN_POINT('Ctrl Pts',(10.7288460529999,11.6,-3.62727545700002));
#182898=CARTESIAN_POINT('Ctrl Pts',(10.7262140239999,15.2,-3.62484009100001));
#182899=CARTESIAN_POINT('Ctrl Pts',(10.7262140239999,11.6,-3.62484009100001));
#182900=CARTESIAN_POINT('Ctrl Pts',(10.7235835239999,15.2,-3.62240992500002));
#182901=CARTESIAN_POINT('Ctrl Pts',(10.7235835239999,11.6,-3.62240992500002));
#182902=CARTESIAN_POINT('Ctrl Pts',(10.7209545619999,15.2,-3.61998495800002));
#182903=CARTESIAN_POINT('Ctrl Pts',(10.7209545619999,11.6,-3.61998495800002));
#182904=CARTESIAN_POINT('Ctrl Pts',(10.7183271499999,15.2,-3.61756519200001));
#182905=CARTESIAN_POINT('Ctrl Pts',(10.7183271499999,11.6,-3.61756519200001));
#182906=CARTESIAN_POINT('Ctrl Pts',(10.7157012959999,15.2,-3.61515062900001));
#182907=CARTESIAN_POINT('Ctrl Pts',(10.7157012959999,11.6,-3.61515062900002));
#182908=CARTESIAN_POINT('Ctrl Pts',(10.7130770099999,15.2,-3.61274126800001));
#182909=CARTESIAN_POINT('Ctrl Pts',(10.7130770099999,11.6,-3.61274126800002));
#182910=CARTESIAN_POINT('Ctrl Pts',(10.7104543019999,15.2,-3.61033710900001));
#182911=CARTESIAN_POINT('Ctrl Pts',(10.7104543019999,11.6,-3.61033710900002));
#182912=CARTESIAN_POINT('Ctrl Pts',(10.7078331809999,15.2,-3.60793815500001));
#182913=CARTESIAN_POINT('Ctrl Pts',(10.7078331809999,11.6,-3.60793815500001));
#182914=CARTESIAN_POINT('Ctrl Pts',(10.7052136559999,15.2,-3.60554440400001));
#182915=CARTESIAN_POINT('Ctrl Pts',(10.7052136559999,11.6,-3.60554440400001));
#182916=CARTESIAN_POINT('Ctrl Pts',(10.7025957399999,15.2,-3.60315585900001));
#182917=CARTESIAN_POINT('Ctrl Pts',(10.7025957399999,11.6,-3.60315585900001));
#182918=CARTESIAN_POINT('Ctrl Pts',(10.6999794399999,15.2,-3.60077252100002));
#182919=CARTESIAN_POINT('Ctrl Pts',(10.6999794399999,11.6,-3.60077252100002));
#182920=CARTESIAN_POINT('Ctrl Pts',(10.6973647669999,15.2,-3.59839438800002));
#182921=CARTESIAN_POINT('Ctrl Pts',(10.6973647669999,11.6,-3.59839438800002));
#182922=CARTESIAN_POINT('Ctrl Pts',(10.6947517299999,15.2,-3.59602146200002));
#182923=CARTESIAN_POINT('Ctrl Pts',(10.6947517299999,11.6,-3.59602146200002));
#182924=CARTESIAN_POINT('Ctrl Pts',(10.6921403399999,15.2,-3.59365374400001));
#182925=CARTESIAN_POINT('Ctrl Pts',(10.6921403399999,11.6,-3.59365374400001));
#182926=CARTESIAN_POINT('Ctrl Pts',(10.6895306049999,15.2,-3.59129123500002));
#182927=CARTESIAN_POINT('Ctrl Pts',(10.6895306049999,11.6,-3.59129123500002));
#182928=CARTESIAN_POINT('Ctrl Pts',(10.6869225359999,15.2,-3.58893393500002));
#182929=CARTESIAN_POINT('Ctrl Pts',(10.6869225359999,11.6,-3.58893393500002));
#182930=CARTESIAN_POINT('Ctrl Pts',(10.6843161429999,15.2,-3.58658184500001));
#182931=CARTESIAN_POINT('Ctrl Pts',(10.6843161429999,11.6,-3.58658184500001));
#182932=CARTESIAN_POINT('Ctrl Pts',(10.6817114369999,15.2,-3.58423496500002));
#182933=CARTESIAN_POINT('Ctrl Pts',(10.6817114369999,11.6,-3.58423496500002));
#182934=CARTESIAN_POINT('Ctrl Pts',(10.6791084249999,15.2,-3.58189329600001));
#182935=CARTESIAN_POINT('Ctrl Pts',(10.6791084249999,11.6,-3.58189329600001));
#182936=CARTESIAN_POINT('Ctrl Pts',(10.6765071199999,15.2,-3.57955683900002));
#182937=CARTESIAN_POINT('Ctrl Pts',(10.6765071199999,11.6,-3.57955683900002));
#182938=CARTESIAN_POINT('Ctrl Pts',(10.6739075299999,15.2,-3.57722559400001));
#182939=CARTESIAN_POINT('Ctrl Pts',(10.6739075299999,11.6,-3.57722559400001));
#182940=CARTESIAN_POINT('Ctrl Pts',(10.6713096659999,15.2,-3.57489956100002));
#182941=CARTESIAN_POINT('Ctrl Pts',(10.6713096659999,11.6,-3.57489956100002));
#182942=CARTESIAN_POINT('Ctrl Pts',(10.6687135369999,15.2,-3.57257874200001));
#182943=CARTESIAN_POINT('Ctrl Pts',(10.6687135369999,11.6,-3.57257874200001));
#182944=CARTESIAN_POINT('Ctrl Pts',(10.6661191539999,15.2,-3.57026313700001));
#182945=CARTESIAN_POINT('Ctrl Pts',(10.6661191539999,11.6,-3.57026313700001));
#182946=CARTESIAN_POINT('Ctrl Pts',(10.6635265279999,15.2,-3.56795274600001));
#182947=CARTESIAN_POINT('Ctrl Pts',(10.6635265279999,11.6,-3.56795274600001));
#182948=CARTESIAN_POINT('Ctrl Pts',(10.6609356659999,15.2,-3.56564757100001));
#182949=CARTESIAN_POINT('Ctrl Pts',(10.6609356659999,11.6,-3.56564757100002));
#182950=CARTESIAN_POINT('Ctrl Pts',(10.6583465819999,15.2,-3.56334761200001));
#182951=CARTESIAN_POINT('Ctrl Pts',(10.6583465819999,11.6,-3.56334761200001));
#182952=CARTESIAN_POINT('Ctrl Pts',(10.6557592819999,15.2,-3.56105286800001));
#182953=CARTESIAN_POINT('Ctrl Pts',(10.6557592819999,11.6,-3.56105286800001));
#182954=CARTESIAN_POINT('Ctrl Pts',(10.6531737789999,15.2,-3.55876334200001));
#182955=CARTESIAN_POINT('Ctrl Pts',(10.6531737789999,11.6,-3.55876334200001));
#182956=CARTESIAN_POINT('Ctrl Pts',(10.6505900819999,15.2,-3.55647903300001));
#182957=CARTESIAN_POINT('Ctrl Pts',(10.6505900819999,11.6,-3.55647903300001));
#182958=CARTESIAN_POINT('Ctrl Pts',(10.6480082019999,15.2,-3.55419994100002));
#182959=CARTESIAN_POINT('Ctrl Pts',(10.6480082019999,11.6,-3.55419994100002));
#182960=CARTESIAN_POINT('Ctrl Pts',(10.6454281479999,15.2,-3.55192606900002));
#182961=CARTESIAN_POINT('Ctrl Pts',(10.6454281479999,11.6,-3.55192606900002));
#182962=CARTESIAN_POINT('Ctrl Pts',(10.6428499309999,15.2,-3.54965741400001));
#182963=CARTESIAN_POINT('Ctrl Pts',(10.6428499309999,11.6,-3.54965741400001));
#182964=CARTESIAN_POINT('Ctrl Pts',(10.6402735619999,15.2,-3.54739398000001));
#182965=CARTESIAN_POINT('Ctrl Pts',(10.6402735619999,11.6,-3.54739398000001));
#182966=CARTESIAN_POINT('Ctrl Pts',(10.6376990499999,15.2,-3.54513576600001));
#182967=CARTESIAN_POINT('Ctrl Pts',(10.6376990499999,11.6,-3.54513576600001));
#182968=CARTESIAN_POINT('Ctrl Pts',(10.6351264049999,15.2,-3.54288277200002));
#182969=CARTESIAN_POINT('Ctrl Pts',(10.6351264049999,11.6,-3.54288277200002));
#182970=CARTESIAN_POINT('Ctrl Pts',(10.6325556389999,15.2,-3.54063499900001));
#182971=CARTESIAN_POINT('Ctrl Pts',(10.6325556389999,11.6,-3.54063499900001));
#182972=CARTESIAN_POINT('Ctrl Pts',(10.6299867589999,15.2,-3.53839244700001));
#182973=CARTESIAN_POINT('Ctrl Pts',(10.6299867589999,11.6,-3.53839244700001));
#182974=CARTESIAN_POINT('Ctrl Pts',(10.6274197799999,15.2,-3.53615511700001));
#182975=CARTESIAN_POINT('Ctrl Pts',(10.6274197799999,11.6,-3.53615511700002));
#182976=CARTESIAN_POINT('Ctrl Pts',(10.6248547079999,15.2,-3.53392301000001));
#182977=CARTESIAN_POINT('Ctrl Pts',(10.6248547079999,11.6,-3.53392301000001));
#182978=CARTESIAN_POINT('Ctrl Pts',(10.6222915559999,15.2,-3.53169612600002));
#182979=CARTESIAN_POINT('Ctrl Pts',(10.6222915559999,11.6,-3.53169612600002));
#182980=CARTESIAN_POINT('Ctrl Pts',(10.6197303339999,15.2,-3.52947446500002));
#182981=CARTESIAN_POINT('Ctrl Pts',(10.6197303339999,11.6,-3.52947446500002));
#182982=CARTESIAN_POINT('Ctrl Pts',(10.6171710509999,15.2,-3.52725802700002));
#182983=CARTESIAN_POINT('Ctrl Pts',(10.6171710509999,11.6,-3.52725802700002));
#182984=CARTESIAN_POINT('Ctrl Pts',(10.6146137189999,15.2,-3.52504681400001));
#182985=CARTESIAN_POINT('Ctrl Pts',(10.6146137189999,11.6,-3.52504681400002));
#182986=CARTESIAN_POINT('Ctrl Pts',(10.6120583479999,15.2,-3.52284082600002));
#182987=CARTESIAN_POINT('Ctrl Pts',(10.6120583479999,11.6,-3.52284082600002));
#182988=CARTESIAN_POINT('Ctrl Pts',(10.6095049489999,15.2,-3.52064006300001));
#182989=CARTESIAN_POINT('Ctrl Pts',(10.6095049489999,11.6,-3.52064006300001));
#182990=CARTESIAN_POINT('Ctrl Pts',(10.6069535309999,15.2,-3.51844452500002));
#182991=CARTESIAN_POINT('Ctrl Pts',(10.6069535309999,11.6,-3.51844452500002));
#182992=CARTESIAN_POINT('Ctrl Pts',(10.6044041049999,15.2,-3.51625421300001));
#182993=CARTESIAN_POINT('Ctrl Pts',(10.6044041049999,11.6,-3.51625421300001));
#182994=CARTESIAN_POINT('Ctrl Pts',(10.6018566829999,15.2,-3.51406912700002));
#182995=CARTESIAN_POINT('Ctrl Pts',(10.6018566829999,11.6,-3.51406912700002));
#182996=CARTESIAN_POINT('Ctrl Pts',(10.5993112729999,15.2,-3.51188926900001));
#182997=CARTESIAN_POINT('Ctrl Pts',(10.5993112729999,11.6,-3.51188926900001));
#182998=CARTESIAN_POINT('Ctrl Pts',(10.5967678879999,15.2,-3.50971463600001));
#182999=CARTESIAN_POINT('Ctrl Pts',(10.5967678879999,11.6,-3.50971463600001));
#183000=CARTESIAN_POINT('Ctrl Pts',(10.5942265379999,15.2,-3.50754523200001));
#183001=CARTESIAN_POINT('Ctrl Pts',(10.5942265379999,11.6,-3.50754523200001));
#183002=CARTESIAN_POINT('Ctrl Pts',(10.5916872319999,15.2,-3.50538105500001));
#183003=CARTESIAN_POINT('Ctrl Pts',(10.5916872319999,11.6,-3.50538105500001));
#183004=CARTESIAN_POINT('Ctrl Pts',(10.5891499829999,15.2,-3.50322210700002));
#183005=CARTESIAN_POINT('Ctrl Pts',(10.5891499829999,11.6,-3.50322210700002));
#183006=CARTESIAN_POINT('Ctrl Pts',(10.5866147999999,15.2,-3.50106838700002));
#183007=CARTESIAN_POINT('Ctrl Pts',(10.5866147999999,11.6,-3.50106838700002));
#183008=CARTESIAN_POINT('Ctrl Pts',(10.5840816949999,15.2,-3.49891989600001));
#183009=CARTESIAN_POINT('Ctrl Pts',(10.5840816949999,11.6,-3.49891989600001));
#183010=CARTESIAN_POINT('Ctrl Pts',(10.5815506769999,15.2,-3.49677663500001));
#183011=CARTESIAN_POINT('Ctrl Pts',(10.5815506769999,11.6,-3.49677663500001));
#183012=CARTESIAN_POINT('Ctrl Pts',(10.5790217569999,15.2,-3.49463860200002));
#183013=CARTESIAN_POINT('Ctrl Pts',(10.5790217569999,11.6,-3.49463860200002));
#183014=CARTESIAN_POINT('Ctrl Pts',(10.5764949479999,15.2,-3.49250580000001));
#183015=CARTESIAN_POINT('Ctrl Pts',(10.5764949479999,11.6,-3.49250580000001));
#183016=CARTESIAN_POINT('Ctrl Pts',(10.5739702579999,15.2,-3.49037822900002));
#183017=CARTESIAN_POINT('Ctrl Pts',(10.5739702579999,11.6,-3.49037822900002));
#183018=CARTESIAN_POINT('Ctrl Pts',(10.5714476989999,15.2,-3.48825588800001));
#183019=CARTESIAN_POINT('Ctrl Pts',(10.5714476989999,11.6,-3.48825588800001));
#183020=CARTESIAN_POINT('Ctrl Pts',(10.5689272829999,15.2,-3.48613877700001));
#183021=CARTESIAN_POINT('Ctrl Pts',(10.5689272829999,11.6,-3.48613877700001));
#183022=CARTESIAN_POINT('Ctrl Pts',(10.5664090179999,15.2,-3.48402689800002));
#183023=CARTESIAN_POINT('Ctrl Pts',(10.5664090179999,11.6,-3.48402689800002));
#183024=CARTESIAN_POINT('Ctrl Pts',(10.5638929169999,15.2,-3.48192025000001));
#183025=CARTESIAN_POINT('Ctrl Pts',(10.5638929169999,11.6,-3.48192025000001));
#183026=CARTESIAN_POINT('Ctrl Pts',(10.5613789899999,15.2,-3.47981883400001));
#183027=CARTESIAN_POINT('Ctrl Pts',(10.5613789899999,11.6,-3.47981883400002));
#183028=CARTESIAN_POINT('Ctrl Pts',(10.5588672479999,15.2,-3.47772265000001));
#183029=CARTESIAN_POINT('Ctrl Pts',(10.5588672479999,11.6,-3.47772265000002));
#183030=CARTESIAN_POINT('Ctrl Pts',(10.5563577029999,15.2,-3.47563169800001));
#183031=CARTESIAN_POINT('Ctrl Pts',(10.5563577029999,11.6,-3.47563169800001));
#183032=CARTESIAN_POINT('Ctrl Pts',(10.5538503639999,15.2,-3.47354597800001));
#183033=CARTESIAN_POINT('Ctrl Pts',(10.5538503639999,11.6,-3.47354597800001));
#183034=CARTESIAN_POINT('Ctrl Pts',(10.5513452449999,15.2,-3.47146549100001));
#183035=CARTESIAN_POINT('Ctrl Pts',(10.5513452449999,11.6,-3.47146549100001));
#183036=CARTESIAN_POINT('Ctrl Pts',(10.5488423529999,15.2,-3.46939023800001));
#183037=CARTESIAN_POINT('Ctrl Pts',(10.5488423529999,11.6,-3.46939023800001));
#183038=CARTESIAN_POINT('Ctrl Pts',(10.5463417019999,15.2,-3.46732021700001));
#183039=CARTESIAN_POINT('Ctrl Pts',(10.5463417019999,11.6,-3.46732021700001));
#183040=CARTESIAN_POINT('Ctrl Pts',(10.5438433009999,15.2,-3.46525543000002));
#183041=CARTESIAN_POINT('Ctrl Pts',(10.5438433009999,11.6,-3.46525543000002));
#183042=CARTESIAN_POINT('Ctrl Pts',(10.5413471629999,15.2,-3.46319587600001));
#183043=CARTESIAN_POINT('Ctrl Pts',(10.5413471629999,11.6,-3.46319587600001));
#183044=CARTESIAN_POINT('Ctrl Pts',(10.5388532969999,15.2,-3.46114155700001));
#183045=CARTESIAN_POINT('Ctrl Pts',(10.5388532969999,11.6,-3.46114155700001));
#183046=CARTESIAN_POINT('Ctrl Pts',(10.5363617169999,15.2,-3.45909247100002));
#183047=CARTESIAN_POINT('Ctrl Pts',(10.5363617169999,11.6,-3.45909247100002));
#183048=CARTESIAN_POINT('Ctrl Pts',(10.5338724319999,15.2,-3.45704862000002));
#183049=CARTESIAN_POINT('Ctrl Pts',(10.5338724319999,11.6,-3.45704862000002));
#183050=CARTESIAN_POINT('Ctrl Pts',(10.5313854529999,15.2,-3.45501000300001));
#183051=CARTESIAN_POINT('Ctrl Pts',(10.5313854529999,11.6,-3.45501000300001));
#183052=CARTESIAN_POINT('Ctrl Pts',(10.5289007929999,15.2,-3.45297662100001));
#183053=CARTESIAN_POINT('Ctrl Pts',(10.5289007929999,11.6,-3.45297662100002));
#183054=CARTESIAN_POINT('Ctrl Pts',(10.5264184599999,15.2,-3.45094847300001));
#183055=CARTESIAN_POINT('Ctrl Pts',(10.5264184599999,11.6,-3.45094847300001));
#183056=CARTESIAN_POINT('Ctrl Pts',(10.5239384669999,15.2,-3.44892556000001));
#183057=CARTESIAN_POINT('Ctrl Pts',(10.5239384669999,11.6,-3.44892556000001));
#183058=CARTESIAN_POINT('Ctrl Pts',(10.5214608269999,15.2,-3.44690788300001));
#183059=CARTESIAN_POINT('Ctrl Pts',(10.5214608269999,11.6,-3.44690788300001));
#183060=CARTESIAN_POINT('Ctrl Pts',(10.5189855499999,15.2,-3.44489544000002));
#183061=CARTESIAN_POINT('Ctrl Pts',(10.5189855499999,11.6,-3.44489544000002));
#183062=CARTESIAN_POINT('Ctrl Pts',(10.5165126449999,15.2,-3.44288823300001));
#183063=CARTESIAN_POINT('Ctrl Pts',(10.5165126449999,11.6,-3.44288823300001));
#183064=CARTESIAN_POINT('Ctrl Pts',(10.5140421269999,15.2,-3.44088626100001));
#183065=CARTESIAN_POINT('Ctrl Pts',(10.5140421269999,11.6,-3.44088626100001));
#183066=CARTESIAN_POINT('Ctrl Pts',(10.5115740039999,15.2,-3.43888952500001));
#183067=CARTESIAN_POINT('Ctrl Pts',(10.5115740039999,11.6,-3.43888952500001));
#183068=CARTESIAN_POINT('Ctrl Pts',(10.5091082899999,15.2,-3.43689802500001));
#183069=CARTESIAN_POINT('Ctrl Pts',(10.5091082899999,11.6,-3.43689802500002));
#183070=CARTESIAN_POINT('Ctrl Pts',(10.5066449939999,15.2,-3.43491176000001));
#183071=CARTESIAN_POINT('Ctrl Pts',(10.5066449939999,11.6,-3.43491176000001));
#183072=CARTESIAN_POINT('Ctrl Pts',(10.5041841299999,15.2,-3.43293073100002));
#183073=CARTESIAN_POINT('Ctrl Pts',(10.5041841299999,11.6,-3.43293073100002));
#183074=CARTESIAN_POINT('Ctrl Pts',(10.5017257079999,15.2,-3.43095493800002));
#183075=CARTESIAN_POINT('Ctrl Pts',(10.5017257079999,11.6,-3.43095493800002));
#183076=CARTESIAN_POINT('Ctrl Pts',(10.4992697399999,15.2,-3.42898438100002));
#183077=CARTESIAN_POINT('Ctrl Pts',(10.4992697399999,11.6,-3.42898438100002));
#183078=CARTESIAN_POINT('Ctrl Pts',(10.4968162359999,15.2,-3.42701906000002));
#183079=CARTESIAN_POINT('Ctrl Pts',(10.4968162359999,11.6,-3.42701906000002));
#183080=CARTESIAN_POINT('Ctrl Pts',(10.4943652099999,15.2,-3.42505897500001));
#183081=CARTESIAN_POINT('Ctrl Pts',(10.4943652099999,11.6,-3.42505897500002));
#183082=CARTESIAN_POINT('Ctrl Pts',(10.4919166709999,15.2,-3.42310412600002));
#183083=CARTESIAN_POINT('Ctrl Pts',(10.4919166709999,11.6,-3.42310412600002));
#183084=CARTESIAN_POINT('Ctrl Pts',(10.4894706319999,15.2,-3.42115451300002));
#183085=CARTESIAN_POINT('Ctrl Pts',(10.4894706319999,11.6,-3.42115451300002));
#183086=CARTESIAN_POINT('Ctrl Pts',(10.4870271039999,15.2,-3.41921013700001));
#183087=CARTESIAN_POINT('Ctrl Pts',(10.4870271039999,11.6,-3.41921013700001));
#183088=CARTESIAN_POINT('Ctrl Pts',(10.4845860999999,15.2,-3.41727099600002));
#183089=CARTESIAN_POINT('Ctrl Pts',(10.4845860999999,11.6,-3.41727099600002));
#183090=CARTESIAN_POINT('Ctrl Pts',(10.4821476289999,15.2,-3.41533709100001));
#183091=CARTESIAN_POINT('Ctrl Pts',(10.4821476289999,11.6,-3.41533709100002));
#183092=CARTESIAN_POINT('Ctrl Pts',(10.4797117049999,15.2,-3.41340842300002));
#183093=CARTESIAN_POINT('Ctrl Pts',(10.4797117049999,11.6,-3.41340842300002));
#183094=CARTESIAN_POINT('Ctrl Pts',(10.4772783389999,15.2,-3.41148499200001));
#183095=CARTESIAN_POINT('Ctrl Pts',(10.4772783389999,11.6,-3.41148499200001));
#183096=CARTESIAN_POINT('Ctrl Pts',(10.4748475419999,15.2,-3.40956679600001));
#183097=CARTESIAN_POINT('Ctrl Pts',(10.4748475419999,11.6,-3.40956679600001));
#183098=CARTESIAN_POINT('Ctrl Pts',(10.4724193259999,15.2,-3.40765383700001));
#183099=CARTESIAN_POINT('Ctrl Pts',(10.4724193259999,11.6,-3.40765383700001));
#183100=CARTESIAN_POINT('Ctrl Pts',(10.4699937039999,15.2,-3.40574611300001));
#183101=CARTESIAN_POINT('Ctrl Pts',(10.4699937039999,11.6,-3.40574611300001));
#183102=CARTESIAN_POINT('Ctrl Pts',(10.4675706859999,15.2,-3.40384362500001));
#183103=CARTESIAN_POINT('Ctrl Pts',(10.4675706859999,11.6,-3.40384362500001));
#183104=CARTESIAN_POINT('Ctrl Pts',(10.4651502849999,15.2,-3.40194637400002));
#183105=CARTESIAN_POINT('Ctrl Pts',(10.4651502849999,11.6,-3.40194637400002));
#183106=CARTESIAN_POINT('Ctrl Pts',(10.4627325119999,15.2,-3.40005435900002));
#183107=CARTESIAN_POINT('Ctrl Pts',(10.4627325119999,11.6,-3.40005435900002));
#183108=CARTESIAN_POINT('Ctrl Pts',(10.4603173799999,15.2,-3.39816757900001));
#183109=CARTESIAN_POINT('Ctrl Pts',(10.4603173799999,11.6,-3.39816757900001));
#183110=CARTESIAN_POINT('Ctrl Pts',(10.4579048999999,15.2,-3.39628603500001));
#183111=CARTESIAN_POINT('Ctrl Pts',(10.4579048999999,11.6,-3.39628603500001));
#183112=CARTESIAN_POINT('Ctrl Pts',(10.4554950839999,15.2,-3.39440972700002));
#183113=CARTESIAN_POINT('Ctrl Pts',(10.4554950839999,11.6,-3.39440972700002));
#183114=CARTESIAN_POINT('Ctrl Pts',(10.4530879439999,15.2,-3.39253865400002));
#183115=CARTESIAN_POINT('Ctrl Pts',(10.4530879439999,11.6,-3.39253865400002));
#183116=CARTESIAN_POINT('Ctrl Pts',(10.4506834919999,15.2,-3.39067281600002));
#183117=CARTESIAN_POINT('Ctrl Pts',(10.4506834919999,11.6,-3.39067281600002));
#183118=CARTESIAN_POINT('Ctrl Pts',(10.4482817399999,15.2,-3.38881221500001));
#183119=CARTESIAN_POINT('Ctrl Pts',(10.4482817399999,11.6,-3.38881221500001));
#183120=CARTESIAN_POINT('Ctrl Pts',(10.4458826999999,15.2,-3.38695684700001));
#183121=CARTESIAN_POINT('Ctrl Pts',(10.4458826999999,11.6,-3.38695684700001));
#183122=CARTESIAN_POINT('Ctrl Pts',(10.4434863849999,15.2,-3.38510671600002));
#183123=CARTESIAN_POINT('Ctrl Pts',(10.4434863849999,11.6,-3.38510671600002));
#183124=CARTESIAN_POINT('Ctrl Pts',(10.4410928049999,15.2,-3.38326181800001));
#183125=CARTESIAN_POINT('Ctrl Pts',(10.4410928049999,11.6,-3.38326181800001));
#183126=CARTESIAN_POINT('Ctrl Pts',(10.4387019739999,15.2,-3.38142215600001));
#183127=CARTESIAN_POINT('Ctrl Pts',(10.4387019739999,11.6,-3.38142215600001));
#183128=CARTESIAN_POINT('Ctrl Pts',(10.4363139019999,15.2,-3.37958772900001));
#183129=CARTESIAN_POINT('Ctrl Pts',(10.4363139019999,11.6,-3.37958772900001));
#183130=CARTESIAN_POINT('Ctrl Pts',(10.4339286029999,15.2,-3.37775853500001));
#183131=CARTESIAN_POINT('Ctrl Pts',(10.4339286029999,11.6,-3.37775853500002));
#183132=CARTESIAN_POINT('Ctrl Pts',(10.4315460899999,15.2,-3.37593457500001));
#183133=CARTESIAN_POINT('Ctrl Pts',(10.4315460899999,11.6,-3.37593457500002));
#183134=CARTESIAN_POINT('Ctrl Pts',(10.4291663729999,15.2,-3.37411585000002));
#183135=CARTESIAN_POINT('Ctrl Pts',(10.4291663729999,11.6,-3.37411585000002));
#183136=CARTESIAN_POINT('Ctrl Pts',(10.4267894639999,15.2,-3.37230235900002));
#183137=CARTESIAN_POINT('Ctrl Pts',(10.4267894639999,11.6,-3.37230235900002));
#183138=CARTESIAN_POINT('Ctrl Pts',(10.4244153789999,15.2,-3.37049410100001));
#183139=CARTESIAN_POINT('Ctrl Pts',(10.4244153789999,11.6,-3.37049410100001));
#183140=CARTESIAN_POINT('Ctrl Pts',(10.4220441259999,15.2,-3.36869107600001));
#183141=CARTESIAN_POINT('Ctrl Pts',(10.4220441259999,11.6,-3.36869107600001));
#183142=CARTESIAN_POINT('Ctrl Pts',(10.4196757189999,15.2,-3.36689328500002));
#183143=CARTESIAN_POINT('Ctrl Pts',(10.4196757189999,11.6,-3.36689328500002));
#183144=CARTESIAN_POINT('Ctrl Pts',(10.4173101699999,15.2,-3.36510072600001));
#183145=CARTESIAN_POINT('Ctrl Pts',(10.4173101699999,11.6,-3.36510072600001));
#183146=CARTESIAN_POINT('Ctrl Pts',(10.4149474929999,15.2,-3.36331340000001));
#183147=CARTESIAN_POINT('Ctrl Pts',(10.4149474929999,11.6,-3.36331340000001));
#183148=CARTESIAN_POINT('Ctrl Pts',(10.4125876979999,15.2,-3.36153130600001));
#183149=CARTESIAN_POINT('Ctrl Pts',(10.4125876979999,11.6,-3.36153130600001));
#183150=CARTESIAN_POINT('Ctrl Pts',(10.4102307989999,15.2,-3.35975444400002));
#183151=CARTESIAN_POINT('Ctrl Pts',(10.4102307989999,11.6,-3.35975444400002));
#183152=CARTESIAN_POINT('Ctrl Pts',(10.4078768069999,15.2,-3.35798281300002));
#183153=CARTESIAN_POINT('Ctrl Pts',(10.4078768069999,11.6,-3.35798281300002));
#183154=CARTESIAN_POINT('Ctrl Pts',(10.4055257379999,15.2,-3.35621641400001));
#183155=CARTESIAN_POINT('Ctrl Pts',(10.4055257379999,11.6,-3.35621641400001));
#183156=CARTESIAN_POINT('Ctrl Pts',(10.4031775999999,15.2,-3.35445524600001));
#183157=CARTESIAN_POINT('Ctrl Pts',(10.4031775999999,11.6,-3.35445524600001));
#183158=CARTESIAN_POINT('Ctrl Pts',(10.4008324069999,15.2,-3.35269930900001));
#183159=CARTESIAN_POINT('Ctrl Pts',(10.4008324069999,11.6,-3.35269930900001));
#183160=CARTESIAN_POINT('Ctrl Pts',(10.3984901739999,15.2,-3.35094860300002));
#183161=CARTESIAN_POINT('Ctrl Pts',(10.3984901739999,11.6,-3.35094860300002));
#183162=CARTESIAN_POINT('Ctrl Pts',(10.3961509099999,15.2,-3.34920312600001));
#183163=CARTESIAN_POINT('Ctrl Pts',(10.3961509099999,11.6,-3.34920312600001));
#183164=CARTESIAN_POINT('Ctrl Pts',(10.3938146309999,15.2,-3.34746287900002));
#183165=CARTESIAN_POINT('Ctrl Pts',(10.3938146309999,11.6,-3.34746287900002));
#183166=CARTESIAN_POINT('Ctrl Pts',(10.3914813469999,15.2,-3.34572786200001));
#183167=CARTESIAN_POINT('Ctrl Pts',(10.3914813469999,11.6,-3.34572786200001));
#183168=CARTESIAN_POINT('Ctrl Pts',(10.3891510709999,15.2,-3.34399807300001));
#183169=CARTESIAN_POINT('Ctrl Pts',(10.3891510709999,11.6,-3.34399807300001));
#183170=CARTESIAN_POINT('Ctrl Pts',(10.3868238179999,15.2,-3.34227351400001));
#183171=CARTESIAN_POINT('Ctrl Pts',(10.3868238179999,11.6,-3.34227351400001));
#183172=CARTESIAN_POINT('Ctrl Pts',(10.3844995979999,15.2,-3.34055418200002));
#183173=CARTESIAN_POINT('Ctrl Pts',(10.3844995979999,11.6,-3.34055418200002));
#183174=CARTESIAN_POINT('Ctrl Pts',(10.3821784259999,15.2,-3.33884007800001));
#183175=CARTESIAN_POINT('Ctrl Pts',(10.3821784259999,11.6,-3.33884007800001));
#183176=CARTESIAN_POINT('Ctrl Pts',(10.3798603139999,15.2,-3.33713120100001));
#183177=CARTESIAN_POINT('Ctrl Pts',(10.3798603139999,11.6,-3.33713120100001));
#183178=CARTESIAN_POINT('Ctrl Pts',(10.3775452729999,15.2,-3.33542755200002));
#183179=CARTESIAN_POINT('Ctrl Pts',(10.3775452729999,11.6,-3.33542755200002));
#183180=CARTESIAN_POINT('Ctrl Pts',(10.3752333189999,15.2,-3.33372913000002));
#183181=CARTESIAN_POINT('Ctrl Pts',(10.3752333189999,11.6,-3.33372913000002));
#183182=CARTESIAN_POINT('Ctrl Pts',(10.3729244619999,15.2,-3.33203593300002));
#183183=CARTESIAN_POINT('Ctrl Pts',(10.3729244619999,11.6,-3.33203593300002));
#183184=CARTESIAN_POINT('Ctrl Pts',(10.3706187169999,15.2,-3.33034796100002));
#183185=CARTESIAN_POINT('Ctrl Pts',(10.3706187169999,11.6,-3.33034796100002));
#183186=CARTESIAN_POINT('Ctrl Pts',(10.3683160969999,15.2,-3.32866521600002));
#183187=CARTESIAN_POINT('Ctrl Pts',(10.3683160969999,11.6,-3.32866521600002));
#183188=CARTESIAN_POINT('Ctrl Pts',(10.3660166129999,15.2,-3.32698769300002));
#183189=CARTESIAN_POINT('Ctrl Pts',(10.3660166129999,11.6,-3.32698769300002));
#183190=CARTESIAN_POINT('Ctrl Pts',(10.3637202799999,15.2,-3.32531539600001));
#183191=CARTESIAN_POINT('Ctrl Pts',(10.3637202799999,11.6,-3.32531539600002));
#183192=CARTESIAN_POINT('Ctrl Pts',(10.3614271109999,15.2,-3.32364832300001));
#183193=CARTESIAN_POINT('Ctrl Pts',(10.3614271109999,11.6,-3.32364832300002));
#183194=CARTESIAN_POINT('Ctrl Pts',(10.3591371169999,15.2,-3.32198647300002));
#183195=CARTESIAN_POINT('Ctrl Pts',(10.3591371169999,11.6,-3.32198647300002));
#183196=CARTESIAN_POINT('Ctrl Pts',(10.3568503129999,15.2,-3.32032984500001));
#183197=CARTESIAN_POINT('Ctrl Pts',(10.3568503129999,11.6,-3.32032984500001));
#183198=CARTESIAN_POINT('Ctrl Pts',(10.3545667119999,15.2,-3.31867843900001));
#183199=CARTESIAN_POINT('Ctrl Pts',(10.3545667119999,11.6,-3.31867843900001));
#183200=CARTESIAN_POINT('Ctrl Pts',(10.3522863269999,15.2,-3.31703225500001));
#183201=CARTESIAN_POINT('Ctrl Pts',(10.3522863269999,11.6,-3.31703225500001));
#183202=CARTESIAN_POINT('Ctrl Pts',(10.3500091699999,15.2,-3.31539129200001));
#183203=CARTESIAN_POINT('Ctrl Pts',(10.3500091699999,11.6,-3.31539129200001));
#183204=CARTESIAN_POINT('Ctrl Pts',(10.3477352559999,15.2,-3.31375555000001));
#183205=CARTESIAN_POINT('Ctrl Pts',(10.3477352559999,11.6,-3.31375555000002));
#183206=CARTESIAN_POINT('Ctrl Pts',(10.3454645979999,15.2,-3.31212502700001));
#183207=CARTESIAN_POINT('Ctrl Pts',(10.3454645979999,11.6,-3.31212502700002));
#183208=CARTESIAN_POINT('Ctrl Pts',(10.3431972079999,15.2,-3.31049972300002));
#183209=CARTESIAN_POINT('Ctrl Pts',(10.3431972079999,11.6,-3.31049972300002));
#183210=CARTESIAN_POINT('Ctrl Pts',(10.3409331009999,15.2,-3.30887963800001));
#183211=CARTESIAN_POINT('Ctrl Pts',(10.3409331009999,11.6,-3.30887963800001));
#183212=CARTESIAN_POINT('Ctrl Pts',(10.3386722889999,15.2,-3.30726477100002));
#183213=CARTESIAN_POINT('Ctrl Pts',(10.3386722889999,11.6,-3.30726477100002));
#183214=CARTESIAN_POINT('Ctrl Pts',(10.3364147869999,15.2,-3.30565512200002));
#183215=CARTESIAN_POINT('Ctrl Pts',(10.3364147869999,11.6,-3.30565512200002));
#183216=CARTESIAN_POINT('Ctrl Pts',(10.3341606059999,15.2,-3.30405069000001));
#183217=CARTESIAN_POINT('Ctrl Pts',(10.3341606059999,11.6,-3.30405069000001));
#183218=CARTESIAN_POINT('Ctrl Pts',(10.3319097619999,15.2,-3.30245147300001));
#183219=CARTESIAN_POINT('Ctrl Pts',(10.3319097619999,11.6,-3.30245147300001));
#183220=CARTESIAN_POINT('Ctrl Pts',(10.3296622669999,15.2,-3.30085747200001));
#183221=CARTESIAN_POINT('Ctrl Pts',(10.3296622669999,11.6,-3.30085747200001));
#183222=CARTESIAN_POINT('Ctrl Pts',(10.3274181339999,15.2,-3.29926868600001));
#183223=CARTESIAN_POINT('Ctrl Pts',(10.3274181339999,11.6,-3.29926868600001));
#183224=CARTESIAN_POINT('Ctrl Pts',(10.3251773799999,15.2,-3.29768511400002));
#183225=CARTESIAN_POINT('Ctrl Pts',(10.3251773799999,11.6,-3.29768511400002));
#183226=CARTESIAN_POINT('Ctrl Pts',(10.3229400139999,15.2,-3.29610675500001));
#183227=CARTESIAN_POINT('Ctrl Pts',(10.3229400139999,11.6,-3.29610675500001));
#183228=CARTESIAN_POINT('Ctrl Pts',(10.3207060529999,15.2,-3.29453360900001));
#183229=CARTESIAN_POINT('Ctrl Pts',(10.3207060529999,11.6,-3.29453360900001));
#183230=CARTESIAN_POINT('Ctrl Pts',(10.3184755079999,15.2,-3.29296567500001));
#183231=CARTESIAN_POINT('Ctrl Pts',(10.3184755079999,11.6,-3.29296567500002));
#183232=CARTESIAN_POINT('Ctrl Pts',(10.3162483959999,15.2,-3.29140295300002));
#183233=CARTESIAN_POINT('Ctrl Pts',(10.3162483959999,11.6,-3.29140295300002));
#183234=CARTESIAN_POINT('Ctrl Pts',(10.3140247269999,15.2,-3.28984544000001));
#183235=CARTESIAN_POINT('Ctrl Pts',(10.3140247269999,11.6,-3.28984544000001));
#183236=CARTESIAN_POINT('Ctrl Pts',(10.3118045179999,15.2,-3.28829313800002));
#183237=CARTESIAN_POINT('Ctrl Pts',(10.3118045179999,11.6,-3.28829313800002));
#183238=CARTESIAN_POINT('Ctrl Pts',(10.3095877799999,15.2,-3.28674604500002));
#183239=CARTESIAN_POINT('Ctrl Pts',(10.3095877799999,11.6,-3.28674604500002));
#183240=CARTESIAN_POINT('Ctrl Pts',(10.3073745299999,15.2,-3.28520415900002));
#183241=CARTESIAN_POINT('Ctrl Pts',(10.3073745299999,11.6,-3.28520415900002));
#183242=CARTESIAN_POINT('Ctrl Pts',(10.3051647789999,15.2,-3.28366748100001));
#183243=CARTESIAN_POINT('Ctrl Pts',(10.3051647789999,11.6,-3.28366748100001));
#183244=CARTESIAN_POINT('Ctrl Pts',(10.3029585419999,15.2,-3.28213601000002));
#183245=CARTESIAN_POINT('Ctrl Pts',(10.3029585419999,11.6,-3.28213601000002));
#183246=CARTESIAN_POINT('Ctrl Pts',(10.3007558329999,15.2,-3.28060974400001));
#183247=CARTESIAN_POINT('Ctrl Pts',(10.3007558329999,11.6,-3.28060974400001));
#183248=CARTESIAN_POINT('Ctrl Pts',(10.2985566669999,15.2,-3.27908868400002));
#183249=CARTESIAN_POINT('Ctrl Pts',(10.2985566669999,11.6,-3.27908868400002));
#183250=CARTESIAN_POINT('Ctrl Pts',(10.2963610559999,15.2,-3.27757282800002));
#183251=CARTESIAN_POINT('Ctrl Pts',(10.2963610559999,11.6,-3.27757282800002));
#183252=CARTESIAN_POINT('Ctrl Pts',(10.2941690149999,15.2,-3.27606217500001));
#183253=CARTESIAN_POINT('Ctrl Pts',(10.2941690149999,11.6,-3.27606217500001));
#183254=CARTESIAN_POINT('Ctrl Pts',(10.2919805579999,15.2,-3.27455672400002));
#183255=CARTESIAN_POINT('Ctrl Pts',(10.2919805579999,11.6,-3.27455672400002));
#183256=CARTESIAN_POINT('Ctrl Pts',(10.2897957009999,15.2,-3.27305647500001));
#183257=CARTESIAN_POINT('Ctrl Pts',(10.2897957009999,11.6,-3.27305647500001));
#183258=CARTESIAN_POINT('Ctrl Pts',(10.2876144549999,15.2,-3.27156142700002));
#183259=CARTESIAN_POINT('Ctrl Pts',(10.2876144549999,11.6,-3.27156142700002));
#183260=CARTESIAN_POINT('Ctrl Pts',(10.2854368349999,15.2,-3.27007157800002));
#183261=CARTESIAN_POINT('Ctrl Pts',(10.2854368349999,11.6,-3.27007157800002));
#183262=CARTESIAN_POINT('Ctrl Pts',(10.2832628569999,15.2,-3.26858692800001));
#183263=CARTESIAN_POINT('Ctrl Pts',(10.2832628569999,11.6,-3.26858692800002));
#183264=CARTESIAN_POINT('Ctrl Pts',(10.2810925339999,15.2,-3.26710747600002));
#183265=CARTESIAN_POINT('Ctrl Pts',(10.2810925339999,11.6,-3.26710747600002));
#183266=CARTESIAN_POINT('Ctrl Pts',(10.2789258799999,15.2,-3.26563322100001));
#183267=CARTESIAN_POINT('Ctrl Pts',(10.2789258799999,11.6,-3.26563322100002));
#183268=CARTESIAN_POINT('Ctrl Pts',(10.2767629099999,15.2,-3.26416416200002));
#183269=CARTESIAN_POINT('Ctrl Pts',(10.2767629099999,11.6,-3.26416416200002));
#183270=CARTESIAN_POINT('Ctrl Pts',(10.2746036379999,15.2,-3.26270029800002));
#183271=CARTESIAN_POINT('Ctrl Pts',(10.2746036379999,11.6,-3.26270029800002));
#183272=CARTESIAN_POINT('Ctrl Pts',(10.2724480789999,15.2,-3.26124162800001));
#183273=CARTESIAN_POINT('Ctrl Pts',(10.2724480789999,11.6,-3.26124162800001));
#183274=CARTESIAN_POINT('Ctrl Pts',(10.2702962469999,15.2,-3.25978815000001));
#183275=CARTESIAN_POINT('Ctrl Pts',(10.2702962469999,11.6,-3.25978815000001));
#183276=CARTESIAN_POINT('Ctrl Pts',(10.2681481549999,15.2,-3.25833986600002));
#183277=CARTESIAN_POINT('Ctrl Pts',(10.2681481549999,11.6,-3.25833986600002));
#183278=CARTESIAN_POINT('Ctrl Pts',(10.2660038209999,15.2,-3.25689677200002));
#183279=CARTESIAN_POINT('Ctrl Pts',(10.2660038209999,11.6,-3.25689677200002));
#183280=CARTESIAN_POINT('Ctrl Pts',(10.2638632559999,15.2,-3.25545886800001));
#183281=CARTESIAN_POINT('Ctrl Pts',(10.2638632559999,11.6,-3.25545886800001));
#183282=CARTESIAN_POINT('Ctrl Pts',(10.2617264769999,15.2,-3.25402615300002));
#183283=CARTESIAN_POINT('Ctrl Pts',(10.2617264769999,11.6,-3.25402615300002));
#183284=CARTESIAN_POINT('Ctrl Pts',(10.2595934979999,15.2,-3.25259862700001));
#183285=CARTESIAN_POINT('Ctrl Pts',(10.2595934979999,11.6,-3.25259862700001));
#183286=CARTESIAN_POINT('Ctrl Pts',(10.2574643339999,15.2,-3.25117628600001));
#183287=CARTESIAN_POINT('Ctrl Pts',(10.2574643339999,11.6,-3.25117628600002));
#183288=CARTESIAN_POINT('Ctrl Pts',(10.2553389979999,15.2,-3.24975913200001));
#183289=CARTESIAN_POINT('Ctrl Pts',(10.2553389979999,11.6,-3.24975913200001));
#183290=CARTESIAN_POINT('Ctrl Pts',(10.2532175069999,15.2,-3.24834716200002));
#183291=CARTESIAN_POINT('Ctrl Pts',(10.2532175069999,11.6,-3.24834716200002));
#183292=CARTESIAN_POINT('Ctrl Pts',(10.2510998739999,15.2,-3.24694037600001));
#183293=CARTESIAN_POINT('Ctrl Pts',(10.2510998739999,11.6,-3.24694037600001));
#183294=CARTESIAN_POINT('Ctrl Pts',(10.2489861149999,15.2,-3.24553877200001));
#183295=CARTESIAN_POINT('Ctrl Pts',(10.2489861149999,11.6,-3.24553877200001));
#183296=CARTESIAN_POINT('Ctrl Pts',(10.2468762449999,15.2,-3.24414235000001));
#183297=CARTESIAN_POINT('Ctrl Pts',(10.2468762449999,11.6,-3.24414235000001));
#183298=CARTESIAN_POINT('Ctrl Pts',(10.2447702779999,15.2,-3.24275110800002));
#183299=CARTESIAN_POINT('Ctrl Pts',(10.2447702779999,11.6,-3.24275110800002));
#183300=CARTESIAN_POINT('Ctrl Pts',(10.2426682289999,15.2,-3.24136504400002));
#183301=CARTESIAN_POINT('Ctrl Pts',(10.2426682289999,11.6,-3.24136504400002));
#183302=CARTESIAN_POINT('Ctrl Pts',(10.2405701139999,15.2,-3.23998415800002));
#183303=CARTESIAN_POINT('Ctrl Pts',(10.2405701139999,11.6,-3.23998415800002));
#183304=CARTESIAN_POINT('Ctrl Pts',(10.2384759469999,15.2,-3.23860844800001));
#183305=CARTESIAN_POINT('Ctrl Pts',(10.2384759469999,11.6,-3.23860844800001));
#183306=CARTESIAN_POINT('Ctrl Pts',(10.2363857439999,15.2,-3.23723791500001));
#183307=CARTESIAN_POINT('Ctrl Pts',(10.2363857439999,11.6,-3.23723791500001));
#183308=CARTESIAN_POINT('Ctrl Pts',(10.2342995189999,15.2,-3.23587255500001));
#183309=CARTESIAN_POINT('Ctrl Pts',(10.2342995189999,11.6,-3.23587255500001));
#183310=CARTESIAN_POINT('Ctrl Pts',(10.2322172889999,15.2,-3.23451236800001));
#183311=CARTESIAN_POINT('Ctrl Pts',(10.2322172889999,11.6,-3.23451236800001));
#183312=CARTESIAN_POINT('Ctrl Pts',(10.2301390659999,15.2,-3.23315735300001));
#183313=CARTESIAN_POINT('Ctrl Pts',(10.2301390659999,11.6,-3.23315735300001));
#183314=CARTESIAN_POINT('Ctrl Pts',(10.2280648689999,15.2,-3.23180750800002));
#183315=CARTESIAN_POINT('Ctrl Pts',(10.2280648689999,11.6,-3.23180750800002));
#183316=CARTESIAN_POINT('Ctrl Pts',(10.2259947109999,15.2,-3.23046283300001));
#183317=CARTESIAN_POINT('Ctrl Pts',(10.2259947109999,11.6,-3.23046283300001));
#183318=CARTESIAN_POINT('Ctrl Pts',(10.2239286079999,15.2,-3.22912332500001));
#183319=CARTESIAN_POINT('Ctrl Pts',(10.2239286079999,11.6,-3.22912332500001));
#183320=CARTESIAN_POINT('Ctrl Pts',(10.2218665749999,15.2,-3.22778898400002));
#183321=CARTESIAN_POINT('Ctrl Pts',(10.2218665749999,11.6,-3.22778898400002));
#183322=CARTESIAN_POINT('Ctrl Pts',(10.2198086269999,15.2,-3.22645980700001));
#183323=CARTESIAN_POINT('Ctrl Pts',(10.2198086269999,11.6,-3.22645980700001));
#183324=CARTESIAN_POINT('Ctrl Pts',(10.2177547809999,15.2,-3.22513579400002));
#183325=CARTESIAN_POINT('Ctrl Pts',(10.2177547809999,11.6,-3.22513579400002));
#183326=CARTESIAN_POINT('Ctrl Pts',(10.2157050509999,15.2,-3.22381694500002));
#183327=CARTESIAN_POINT('Ctrl Pts',(10.2157050509999,11.6,-3.22381694500002));
#183328=CARTESIAN_POINT('Ctrl Pts',(10.2136594529999,15.2,-3.22250325600002));
#183329=CARTESIAN_POINT('Ctrl Pts',(10.2136594529999,11.6,-3.22250325600002));
#183330=CARTESIAN_POINT('Ctrl Pts',(10.2116180039999,15.2,-3.22119472700001));
#183331=CARTESIAN_POINT('Ctrl Pts',(10.2116180039999,11.6,-3.22119472700001));
#183332=CARTESIAN_POINT('Ctrl Pts',(10.2095807169999,15.2,-3.21989135600001));
#183333=CARTESIAN_POINT('Ctrl Pts',(10.2095807169999,11.6,-3.21989135600001));
#183334=CARTESIAN_POINT('Ctrl Pts',(10.2075476089999,15.2,-3.21859314200001));
#183335=CARTESIAN_POINT('Ctrl Pts',(10.2075476089999,11.6,-3.21859314200002));
#183336=CARTESIAN_POINT('Ctrl Pts',(10.2055186959999,15.2,-3.21730008500001));
#183337=CARTESIAN_POINT('Ctrl Pts',(10.2055186959999,11.6,-3.21730008500001));
#183338=CARTESIAN_POINT('Ctrl Pts',(10.2034939929999,15.2,-3.21601218000001));
#183339=CARTESIAN_POINT('Ctrl Pts',(10.2034939929999,11.6,-3.21601218000001));
#183340=CARTESIAN_POINT('Ctrl Pts',(10.2014735169999,15.2,-3.21472942900002));
#183341=CARTESIAN_POINT('Ctrl Pts',(10.2014735169999,11.6,-3.21472942900002));
#183342=CARTESIAN_POINT('Ctrl Pts',(10.1994572829999,15.2,-3.21345182800002));
#183343=CARTESIAN_POINT('Ctrl Pts',(10.1994572829999,11.6,-3.21345182800002));
#183344=CARTESIAN_POINT('Ctrl Pts',(10.1974453069999,15.2,-3.21217937700002));
#183345=CARTESIAN_POINT('Ctrl Pts',(10.1974453069999,11.6,-3.21217937700002));
#183346=CARTESIAN_POINT('Ctrl Pts',(10.1954376039999,15.2,-3.21091207400002));
#183347=CARTESIAN_POINT('Ctrl Pts',(10.1954376039999,11.6,-3.21091207400002));
#183348=CARTESIAN_POINT('Ctrl Pts',(10.1934341909999,15.2,-3.20964991800002));
#183349=CARTESIAN_POINT('Ctrl Pts',(10.1934341909999,11.6,-3.20964991800002));
#183350=CARTESIAN_POINT('Ctrl Pts',(10.1914350849999,15.2,-3.20839290800001));
#183351=CARTESIAN_POINT('Ctrl Pts',(10.1914350849999,11.6,-3.20839290800001));
#183352=CARTESIAN_POINT('Ctrl Pts',(10.1894402999999,15.2,-3.20714104000002));
#183353=CARTESIAN_POINT('Ctrl Pts',(10.1894402999999,11.6,-3.20714104000002));
#183354=CARTESIAN_POINT('Ctrl Pts',(10.1874498539999,15.2,-3.20589431400002));
#183355=CARTESIAN_POINT('Ctrl Pts',(10.1874498539999,11.6,-3.20589431400002));
#183356=CARTESIAN_POINT('Ctrl Pts',(10.1854637609999,15.2,-3.20465272900002));
#183357=CARTESIAN_POINT('Ctrl Pts',(10.1854637609999,11.6,-3.20465272900002));
#183358=CARTESIAN_POINT('Ctrl Pts',(10.1834820399999,15.2,-3.20341628300001));
#183359=CARTESIAN_POINT('Ctrl Pts',(10.1834820399999,11.6,-3.20341628300001));
#183360=CARTESIAN_POINT('Ctrl Pts',(10.1815047049999,15.2,-3.20218497500001));
#183361=CARTESIAN_POINT('Ctrl Pts',(10.1815047049999,11.6,-3.20218497500001));
#183362=CARTESIAN_POINT('Ctrl Pts',(10.1795317729999,15.2,-3.20095880100002));
#183363=CARTESIAN_POINT('Ctrl Pts',(10.1795317729999,11.6,-3.20095880100002));
#183364=CARTESIAN_POINT('Ctrl Pts',(10.1775632609999,15.2,-3.19973776100001));
#183365=CARTESIAN_POINT('Ctrl Pts',(10.1775632609999,11.6,-3.19973776100001));
#183366=CARTESIAN_POINT('Ctrl Pts',(10.1755991829999,15.2,-3.19852185400002));
#183367=CARTESIAN_POINT('Ctrl Pts',(10.1755991829999,11.6,-3.19852185400002));
#183368=CARTESIAN_POINT('Ctrl Pts',(10.1736395589999,15.2,-3.19731107700001));
#183369=CARTESIAN_POINT('Ctrl Pts',(10.1736395589999,11.6,-3.19731107700001));
#183370=CARTESIAN_POINT('Ctrl Pts',(10.1716844029999,15.2,-3.19610542900001));
#183371=CARTESIAN_POINT('Ctrl Pts',(10.1716844029999,11.6,-3.19610542900001));
#183372=CARTESIAN_POINT('Ctrl Pts',(10.1697337309999,15.2,-3.19490490900002));
#183373=CARTESIAN_POINT('Ctrl Pts',(10.1697337309999,11.6,-3.19490490900002));
#183374=CARTESIAN_POINT('Ctrl Pts',(10.1677875629999,15.2,-3.19370951400002));
#183375=CARTESIAN_POINT('Ctrl Pts',(10.1677875629999,11.6,-3.19370951400002));
#183376=CARTESIAN_POINT('Ctrl Pts',(10.1658459129999,15.2,-3.19251924300001));
#183377=CARTESIAN_POINT('Ctrl Pts',(10.1658459129999,11.6,-3.19251924300001));
#183378=CARTESIAN_POINT('Ctrl Pts',(10.1639087969999,15.2,-3.19133409300001));
#183379=CARTESIAN_POINT('Ctrl Pts',(10.1639087969999,11.6,-3.19133409300001));
#183380=CARTESIAN_POINT('Ctrl Pts',(10.1619762339999,15.2,-3.19015406500001));
#183381=CARTESIAN_POINT('Ctrl Pts',(10.1619762339999,11.6,-3.19015406500002));
#183382=CARTESIAN_POINT('Ctrl Pts',(10.1600482389999,15.2,-3.18897915400001));
#183383=CARTESIAN_POINT('Ctrl Pts',(10.1600482389999,11.6,-3.18897915400001));
#183384=CARTESIAN_POINT('Ctrl Pts',(10.1581248299999,15.2,-3.18780935900001));
#183385=CARTESIAN_POINT('Ctrl Pts',(10.1581248299999,11.6,-3.18780935900001));
#183386=CARTESIAN_POINT('Ctrl Pts',(10.1562060229999,15.2,-3.18664468000001));
#183387=CARTESIAN_POINT('Ctrl Pts',(10.1562060229999,11.6,-3.18664468000002));
#183388=CARTESIAN_POINT('Ctrl Pts',(10.1542918349999,15.2,-3.18548511300001));
#183389=CARTESIAN_POINT('Ctrl Pts',(10.1542918349999,11.6,-3.18548511300001));
#183390=CARTESIAN_POINT('Ctrl Pts',(10.1523822839999,15.2,-3.18433065800001));
#183391=CARTESIAN_POINT('Ctrl Pts',(10.1523822839999,11.6,-3.18433065800001));
#183392=CARTESIAN_POINT('Ctrl Pts',(10.1504773859999,15.2,-3.18318131200002));
#183393=CARTESIAN_POINT('Ctrl Pts',(10.1504773859999,11.6,-3.18318131200002));
#183394=CARTESIAN_POINT('Ctrl Pts',(10.1485771589999,15.2,-3.18203707400002));
#183395=CARTESIAN_POINT('Ctrl Pts',(10.1485771589999,11.6,-3.18203707400002));
#183396=CARTESIAN_POINT('Ctrl Pts',(10.1466816179999,15.2,-3.18089793900001));
#183397=CARTESIAN_POINT('Ctrl Pts',(10.1466816179999,11.6,-3.18089793900001));
#183398=CARTESIAN_POINT('Ctrl Pts',(10.1447907829999,15.2,-3.17976391000002));
#183399=CARTESIAN_POINT('Ctrl Pts',(10.1447907829999,11.6,-3.17976391000002));
#183400=CARTESIAN_POINT('Ctrl Pts',(10.1429046699999,15.2,-3.17863498200001));
#183401=CARTESIAN_POINT('Ctrl Pts',(10.1429046699999,11.6,-3.17863498200001));
#183402=CARTESIAN_POINT('Ctrl Pts',(10.1410232959999,15.2,-3.17751115200001));
#183403=CARTESIAN_POINT('Ctrl Pts',(10.1410232959999,11.6,-3.17751115200001));
#183404=CARTESIAN_POINT('Ctrl Pts',(10.1391466789999,15.2,-3.17639242200002));
#183405=CARTESIAN_POINT('Ctrl Pts',(10.1391466789999,11.6,-3.17639242200002));
#183406=CARTESIAN_POINT('Ctrl Pts',(10.1372748349999,15.2,-3.17527878600002));
#183407=CARTESIAN_POINT('Ctrl Pts',(10.1372748349999,11.6,-3.17527878600002));
#183408=CARTESIAN_POINT('Ctrl Pts',(10.1354077839999,15.2,-3.17417024400001));
#183409=CARTESIAN_POINT('Ctrl Pts',(10.1354077839999,11.6,-3.17417024400001));
#183410=CARTESIAN_POINT('Ctrl Pts',(10.1335455409999,15.2,-3.17306679400001));
#183411=CARTESIAN_POINT('Ctrl Pts',(10.1335455409999,11.6,-3.17306679400002));
#183412=CARTESIAN_POINT('Ctrl Pts',(10.1316881249999,15.2,-3.17196843300001));
#183413=CARTESIAN_POINT('Ctrl Pts',(10.1316881249999,11.6,-3.17196843300001));
#183414=CARTESIAN_POINT('Ctrl Pts',(10.1298355529999,15.2,-3.17087516000001));
#183415=CARTESIAN_POINT('Ctrl Pts',(10.1298355529999,11.6,-3.17087516000001));
#183416=CARTESIAN_POINT('Ctrl Pts',(10.1279878419999,15.2,-3.16978697100001));
#183417=CARTESIAN_POINT('Ctrl Pts',(10.1279878419999,11.6,-3.16978697100002));
#183418=CARTESIAN_POINT('Ctrl Pts',(10.1261450119999,15.2,-3.16870386600002));
#183419=CARTESIAN_POINT('Ctrl Pts',(10.1261450119999,11.6,-3.16870386600002));
#183420=CARTESIAN_POINT('Ctrl Pts',(10.1243070779999,15.2,-3.16762584300001));
#183421=CARTESIAN_POINT('Ctrl Pts',(10.1243070779999,11.6,-3.16762584300002));
#183422=CARTESIAN_POINT('Ctrl Pts',(10.1224740599999,15.2,-3.16655289800002));
#183423=CARTESIAN_POINT('Ctrl Pts',(10.1224740599999,11.6,-3.16655289800002));
#183424=CARTESIAN_POINT('Ctrl Pts',(10.1206459739999,15.2,-3.16548503000002));
#183425=CARTESIAN_POINT('Ctrl Pts',(10.1206459739999,11.6,-3.16548503000002));
#183426=CARTESIAN_POINT('Ctrl Pts',(10.1188228389999,15.2,-3.16442223800002));
#183427=CARTESIAN_POINT('Ctrl Pts',(10.1188228389999,11.6,-3.16442223800002));
#183428=CARTESIAN_POINT('Ctrl Pts',(10.1170046749999,15.2,-3.16336451600002));
#183429=CARTESIAN_POINT('Ctrl Pts',(10.1170046749999,11.6,-3.16336451600002));
#183430=CARTESIAN_POINT('Ctrl Pts',(10.1151914959999,15.2,-3.16231186600001));
#183431=CARTESIAN_POINT('Ctrl Pts',(10.1151914959999,11.6,-3.16231186600001));
#183432=CARTESIAN_POINT('Ctrl Pts',(10.1133833219999,15.2,-3.16126428300001));
#183433=CARTESIAN_POINT('Ctrl Pts',(10.1133833219999,11.6,-3.16126428300001));
#183434=CARTESIAN_POINT('Ctrl Pts',(10.1115801729999,15.2,-3.16022176700002));
#183435=CARTESIAN_POINT('Ctrl Pts',(10.1115801729999,11.6,-3.16022176700002));
#183436=CARTESIAN_POINT('Ctrl Pts',(10.1097820639999,15.2,-3.15918431300001));
#183437=CARTESIAN_POINT('Ctrl Pts',(10.1097820639999,11.6,-3.15918431300001));
#183438=CARTESIAN_POINT('Ctrl Pts',(10.1079890159999,15.2,-3.15815192100001));
#183439=CARTESIAN_POINT('Ctrl Pts',(10.1079890159999,11.6,-3.15815192100001));
#183440=CARTESIAN_POINT('Ctrl Pts',(10.1062010459999,15.2,-3.15712458800002));
#183441=CARTESIAN_POINT('Ctrl Pts',(10.1062010459999,11.6,-3.15712458800002));
#183442=CARTESIAN_POINT('Ctrl Pts',(10.1044181719999,15.2,-3.15610231100001));
#183443=CARTESIAN_POINT('Ctrl Pts',(10.1044181719999,11.6,-3.15610231100001));
#183444=CARTESIAN_POINT('Ctrl Pts',(10.1026404129999,15.2,-3.15508509000002));
#183445=CARTESIAN_POINT('Ctrl Pts',(10.1026404129999,11.6,-3.15508509000002));
#183446=CARTESIAN_POINT('Ctrl Pts',(10.1008677879999,15.2,-3.15407291900001));
#183447=CARTESIAN_POINT('Ctrl Pts',(10.1008677879999,11.6,-3.15407291900002));
#183448=CARTESIAN_POINT('Ctrl Pts',(10.0991003149999,15.2,-3.15306579700001));
#183449=CARTESIAN_POINT('Ctrl Pts',(10.0991003149999,11.6,-3.15306579700001));
#183450=CARTESIAN_POINT('Ctrl Pts',(10.0973380129999,15.2,-3.15206372300001));
#183451=CARTESIAN_POINT('Ctrl Pts',(10.0973380129999,11.6,-3.15206372300001));
#183452=CARTESIAN_POINT('Ctrl Pts',(10.0955808999999,15.2,-3.15106669300001));
#183453=CARTESIAN_POINT('Ctrl Pts',(10.0955808999999,11.6,-3.15106669300001));
#183454=CARTESIAN_POINT('Ctrl Pts',(10.0938289959999,15.2,-3.15007470700001));
#183455=CARTESIAN_POINT('Ctrl Pts',(10.0938289959999,11.6,-3.15007470700001));
#183456=CARTESIAN_POINT('Ctrl Pts',(10.0920823179999,15.2,-3.14908775800002));
#183457=CARTESIAN_POINT('Ctrl Pts',(10.0920823179999,11.6,-3.14908775800002));
#183458=CARTESIAN_POINT('Ctrl Pts',(10.0903408869999,15.2,-3.14810584800002));
#183459=CARTESIAN_POINT('Ctrl Pts',(10.0903408869999,11.6,-3.14810584800002));
#183460=CARTESIAN_POINT('Ctrl Pts',(10.0886047199999,15.2,-3.14712897300002));
#183461=CARTESIAN_POINT('Ctrl Pts',(10.0886047199999,11.6,-3.14712897300002));
#183462=CARTESIAN_POINT('Ctrl Pts',(10.0868738369999,15.2,-3.14615712900002));
#183463=CARTESIAN_POINT('Ctrl Pts',(10.0868738369999,11.6,-3.14615712900002));
#183464=CARTESIAN_POINT('Ctrl Pts',(10.0851482559999,15.2,-3.14519031400001));
#183465=CARTESIAN_POINT('Ctrl Pts',(10.0851482559999,11.6,-3.14519031400002));
#183466=CARTESIAN_POINT('Ctrl Pts',(10.0834279989999,15.2,-3.14422852800002));
#183467=CARTESIAN_POINT('Ctrl Pts',(10.0834279989999,11.6,-3.14422852800002));
#183468=CARTESIAN_POINT('Ctrl Pts',(10.0817130829999,15.2,-3.14327176500001));
#183469=CARTESIAN_POINT('Ctrl Pts',(10.0817130829999,11.6,-3.14327176500001));
#183470=CARTESIAN_POINT('Ctrl Pts',(10.0800035259999,15.2,-3.14232002500002));
#183471=CARTESIAN_POINT('Ctrl Pts',(10.0800035259999,11.6,-3.14232002500002));
#183472=CARTESIAN_POINT('Ctrl Pts',(10.0782993499999,15.2,-3.14137330300001));
#183473=CARTESIAN_POINT('Ctrl Pts',(10.0782993499999,11.6,-3.14137330300001));
#183474=CARTESIAN_POINT('Ctrl Pts',(10.0766005729999,15.2,-3.14043159900002));
#183475=CARTESIAN_POINT('Ctrl Pts',(10.0766005729999,11.6,-3.14043159900002));
#183476=CARTESIAN_POINT('Ctrl Pts',(10.0749072159999,15.2,-3.13949490700002));
#183477=CARTESIAN_POINT('Ctrl Pts',(10.0749072159999,11.6,-3.13949490700002));
#183478=CARTESIAN_POINT('Ctrl Pts',(10.0732192959999,15.2,-3.13856322800001));
#183479=CARTESIAN_POINT('Ctrl Pts',(10.0732192959999,11.6,-3.13856322800001));
#183480=CARTESIAN_POINT('Ctrl Pts',(10.0715368339999,15.2,-3.13763655600001));
#183481=CARTESIAN_POINT('Ctrl Pts',(10.0715368339999,11.6,-3.13763655600001));
#183482=CARTESIAN_POINT('Ctrl Pts',(10.0698598489999,15.2,-3.13671489000001));
#183483=CARTESIAN_POINT('Ctrl Pts',(10.0698598489999,11.6,-3.13671489000001));
#183484=CARTESIAN_POINT('Ctrl Pts',(10.0681883619999,15.2,-3.13579822800001));
#183485=CARTESIAN_POINT('Ctrl Pts',(10.0681883619999,11.6,-3.13579822800001));
#183486=CARTESIAN_POINT('Ctrl Pts',(10.0665223919999,15.2,-3.13488656500001));
#183487=CARTESIAN_POINT('Ctrl Pts',(10.0665223919999,11.6,-3.13488656500002));
#183488=CARTESIAN_POINT('Ctrl Pts',(10.0648619579999,15.2,-3.13397990000002));
#183489=CARTESIAN_POINT('Ctrl Pts',(10.0648619579999,11.6,-3.13397990000002));
#183490=CARTESIAN_POINT('Ctrl Pts',(10.0632070809999,15.2,-3.13307822900001));
#183491=CARTESIAN_POINT('Ctrl Pts',(10.0632070809999,11.6,-3.13307822900002));
#183492=CARTESIAN_POINT('Ctrl Pts',(10.0615577799999,15.2,-3.13218155100001));
#183493=CARTESIAN_POINT('Ctrl Pts',(10.0615577799999,11.6,-3.13218155100001));
#183494=CARTESIAN_POINT('Ctrl Pts',(10.0599140779999,15.2,-3.13128986000001));
#183495=CARTESIAN_POINT('Ctrl Pts',(10.0599140779999,11.6,-3.13128986000002));
#183496=CARTESIAN_POINT('Ctrl Pts',(10.0582759909999,15.2,-3.13040315700002));
#183497=CARTESIAN_POINT('Ctrl Pts',(10.0582759909999,11.6,-3.13040315700002));
#183498=CARTESIAN_POINT('Ctrl Pts',(10.0566435409999,15.2,-3.12952143500001));
#183499=CARTESIAN_POINT('Ctrl Pts',(10.0566435409999,11.6,-3.12952143500001));
#183500=CARTESIAN_POINT('Ctrl Pts',(10.0550167499999,15.2,-3.12864469400001));
#183501=CARTESIAN_POINT('Ctrl Pts',(10.0550167499999,11.6,-3.12864469400001));
#183502=CARTESIAN_POINT('Ctrl Pts',(10.0533956349999,15.2,-3.12777293000002));
#183503=CARTESIAN_POINT('Ctrl Pts',(10.0533956349999,11.6,-3.12777293000002));
#183504=CARTESIAN_POINT('Ctrl Pts',(10.0517802179999,15.2,-3.12690614000001));
#183505=CARTESIAN_POINT('Ctrl Pts',(10.0517802179999,11.6,-3.12690614000001));
#183506=CARTESIAN_POINT('Ctrl Pts',(10.0501705219999,15.2,-3.12604432200001));
#183507=CARTESIAN_POINT('Ctrl Pts',(10.0501705219999,11.6,-3.12604432200001));
#183508=CARTESIAN_POINT('Ctrl Pts',(10.0485665629999,15.2,-3.12518747000002));
#183509=CARTESIAN_POINT('Ctrl Pts',(10.0485665629999,11.6,-3.12518747000002));
#183510=CARTESIAN_POINT('Ctrl Pts',(10.0469683629999,15.2,-3.12433558500001));
#183511=CARTESIAN_POINT('Ctrl Pts',(10.0469683629999,11.6,-3.12433558500001));
#183512=CARTESIAN_POINT('Ctrl Pts',(10.0453759449999,15.2,-3.12348866100002));
#183513=CARTESIAN_POINT('Ctrl Pts',(10.0453759449999,11.6,-3.12348866100002));
#183514=CARTESIAN_POINT('Ctrl Pts',(10.0437893269999,15.2,-3.12264669700001));
#183515=CARTESIAN_POINT('Ctrl Pts',(10.0437893269999,11.6,-3.12264669700001));
#183516=CARTESIAN_POINT('Ctrl Pts',(10.0422085329999,15.2,-3.12180968700002));
#183517=CARTESIAN_POINT('Ctrl Pts',(10.0422085329999,11.6,-3.12180968700002));
#183518=CARTESIAN_POINT('Ctrl Pts',(10.0406335799999,15.2,-3.12097763100001));
#183519=CARTESIAN_POINT('Ctrl Pts',(10.0406335799999,11.6,-3.12097763100002));
#183520=CARTESIAN_POINT('Ctrl Pts',(10.0390644919999,15.2,-3.12015052400001));
#183521=CARTESIAN_POINT('Ctrl Pts',(10.0390644919999,11.6,-3.12015052400001));
#183522=CARTESIAN_POINT('Ctrl Pts',(10.0375012879999,15.2,-3.11932836300001));
#183523=CARTESIAN_POINT('Ctrl Pts',(10.0375012879999,11.6,-3.11932836300001));
#183524=CARTESIAN_POINT('Ctrl Pts',(10.0359439909999,15.2,-3.11851114600001));
#183525=CARTESIAN_POINT('Ctrl Pts',(10.0359439909999,11.6,-3.11851114600001));
#183526=CARTESIAN_POINT('Ctrl Pts',(10.0343926209999,15.2,-3.11769886700001));
#183527=CARTESIAN_POINT('Ctrl Pts',(10.0343926209999,11.6,-3.11769886700001));
#183528=CARTESIAN_POINT('Ctrl Pts',(10.0328471999999,15.2,-3.11689152500001));
#183529=CARTESIAN_POINT('Ctrl Pts',(10.0328471999999,11.6,-3.11689152500001));
#183530=CARTESIAN_POINT('Ctrl Pts',(10.0313077479999,15.2,-3.11608911700001));
#183531=CARTESIAN_POINT('Ctrl Pts',(10.0313077479999,11.6,-3.11608911700001));
#183532=CARTESIAN_POINT('Ctrl Pts',(10.0297742879999,15.2,-3.11529163800001));
#183533=CARTESIAN_POINT('Ctrl Pts',(10.0297742879999,11.6,-3.11529163800001));
#183534=CARTESIAN_POINT('Ctrl Pts',(10.0282468409999,15.2,-3.11449908600002));
#183535=CARTESIAN_POINT('Ctrl Pts',(10.0282468409999,11.6,-3.11449908600002));
#183536=CARTESIAN_POINT('Ctrl Pts',(10.0267254279999,15.2,-3.11371145700001));
#183537=CARTESIAN_POINT('Ctrl Pts',(10.0267254279999,11.6,-3.11371145700001));
#183538=CARTESIAN_POINT('Ctrl Pts',(10.0252100719999,15.2,-3.11292874700001));
#183539=CARTESIAN_POINT('Ctrl Pts',(10.0252100719999,11.6,-3.11292874700001));
#183540=CARTESIAN_POINT('Ctrl Pts',(10.0237007949999,15.2,-3.11215095500001));
#183541=CARTESIAN_POINT('Ctrl Pts',(10.0237007949999,11.6,-3.11215095500002));
#183542=CARTESIAN_POINT('Ctrl Pts',(10.0221976149999,15.2,-3.11137807500002));
#183543=CARTESIAN_POINT('Ctrl Pts',(10.0221976149999,11.6,-3.11137807500002));
#183544=CARTESIAN_POINT('Ctrl Pts',(10.0207005589999,15.2,-3.11061010400001));
#183545=CARTESIAN_POINT('Ctrl Pts',(10.0207005589999,11.6,-3.11061010400001));
#183546=CARTESIAN_POINT('Ctrl Pts',(10.0192096459999,15.2,-3.10984703900001));
#183547=CARTESIAN_POINT('Ctrl Pts',(10.0192096459999,11.6,-3.10984703900001));
#183548=CARTESIAN_POINT('Ctrl Pts',(10.0177248989999,15.2,-3.10908887700001));
#183549=CARTESIAN_POINT('Ctrl Pts',(10.0177248989999,11.6,-3.10908887700002));
#183550=CARTESIAN_POINT('Ctrl Pts',(10.0162463389999,15.2,-3.10833561400001));
#183551=CARTESIAN_POINT('Ctrl Pts',(10.0162463389999,11.6,-3.10833561400001));
#183552=CARTESIAN_POINT('Ctrl Pts',(10.0147739889999,15.2,-3.10758724500001));
#183553=CARTESIAN_POINT('Ctrl Pts',(10.0147739889999,11.6,-3.10758724500001));
#183554=CARTESIAN_POINT('Ctrl Pts',(10.0133078739999,15.2,-3.10684376900001));
#183555=CARTESIAN_POINT('Ctrl Pts',(10.0133078739999,11.6,-3.10684376900001));
#183556=CARTESIAN_POINT('Ctrl Pts',(10.0118480119999,15.2,-3.10610517900002));
#183557=CARTESIAN_POINT('Ctrl Pts',(10.0118480119999,11.6,-3.10610517900002));
#183558=CARTESIAN_POINT('Ctrl Pts',(10.0103944279999,15.2,-3.10537147600002));
#183559=CARTESIAN_POINT('Ctrl Pts',(10.0103944279999,11.6,-3.10537147600002));
#183560=CARTESIAN_POINT('Ctrl Pts',(10.0089471439999,15.2,-3.10464265200002));
#183561=CARTESIAN_POINT('Ctrl Pts',(10.0089471439999,11.6,-3.10464265200002));
#183562=CARTESIAN_POINT('Ctrl Pts',(10.0075061829999,15.2,-3.10391870500001));
#183563=CARTESIAN_POINT('Ctrl Pts',(10.0075061829999,11.6,-3.10391870500002));
#183564=CARTESIAN_POINT('Ctrl Pts',(10.0060715669999,15.2,-3.10319963200001));
#183565=CARTESIAN_POINT('Ctrl Pts',(10.0060715669999,11.6,-3.10319963200001));
#183566=CARTESIAN_POINT('Ctrl Pts',(10.0046433189999,15.2,-3.10248542800001));
#183567=CARTESIAN_POINT('Ctrl Pts',(10.0046433189999,11.6,-3.10248542800002));
#183568=CARTESIAN_POINT('Ctrl Pts',(10.0032214629999,15.2,-3.10177609000001));
#183569=CARTESIAN_POINT('Ctrl Pts',(10.0032214629999,11.6,-3.10177609000002));
#183570=CARTESIAN_POINT('Ctrl Pts',(10.0018060209999,15.2,-3.10107161300001));
#183571=CARTESIAN_POINT('Ctrl Pts',(10.0018060209999,11.6,-3.10107161300001));
#183572=CARTESIAN_POINT('Ctrl Pts',(10.0003970159999,15.2,-3.10037199500002));
#183573=CARTESIAN_POINT('Ctrl Pts',(10.0003970159999,11.6,-3.10037199500002));
#183574=CARTESIAN_POINT('Ctrl Pts',(9.99899447199994,15.2,-3.09967723100002));
#183575=CARTESIAN_POINT('Ctrl Pts',(9.99899447199994,11.6,-3.09967723100002));
#183576=CARTESIAN_POINT('Ctrl Pts',(9.99759841199995,15.2,-3.09898731700001));
#183577=CARTESIAN_POINT('Ctrl Pts',(9.99759841199995,11.6,-3.09898731700002));
#183578=CARTESIAN_POINT('Ctrl Pts',(9.99620885899994,15.2,-3.09830225000002));
#183579=CARTESIAN_POINT('Ctrl Pts',(9.99620885899994,11.6,-3.09830225000002));
#183580=CARTESIAN_POINT('Ctrl Pts',(9.99482583599995,15.2,-3.09762202400002));
#183581=CARTESIAN_POINT('Ctrl Pts',(9.99482583599995,11.6,-3.09762202400002));
#183582=CARTESIAN_POINT('Ctrl Pts',(9.99344936799995,15.2,-3.09694663700002));
#183583=CARTESIAN_POINT('Ctrl Pts',(9.99344936799995,11.6,-3.09694663700002));
#183584=CARTESIAN_POINT('Ctrl Pts',(9.99207947699994,15.2,-3.09627608500001));
#183585=CARTESIAN_POINT('Ctrl Pts',(9.99207947699994,11.6,-3.09627608500001));
#183586=CARTESIAN_POINT('Ctrl Pts',(9.99071618799995,15.2,-3.09561036200002));
#183587=CARTESIAN_POINT('Ctrl Pts',(9.99071618799995,11.6,-3.09561036200002));
#183588=CARTESIAN_POINT('Ctrl Pts',(9.98935952599994,15.2,-3.09494946600001));
#183589=CARTESIAN_POINT('Ctrl Pts',(9.98935952599994,11.6,-3.09494946600001));
#183590=CARTESIAN_POINT('Ctrl Pts',(9.98800951199994,15.2,-3.09429339200001));
#183591=CARTESIAN_POINT('Ctrl Pts',(9.98800951199994,11.6,-3.09429339200001));
#183592=CARTESIAN_POINT('Ctrl Pts',(9.98666617099994,15.2,-3.09364213600002));
#183593=CARTESIAN_POINT('Ctrl Pts',(9.98666617099994,11.6,-3.09364213600002));
#183594=CARTESIAN_POINT('Ctrl Pts',(9.98532952799994,15.2,-3.09299569400002));
#183595=CARTESIAN_POINT('Ctrl Pts',(9.98532952799994,11.6,-3.09299569400002));
#183596=CARTESIAN_POINT('Ctrl Pts',(9.98399960699994,15.2,-3.09235406000001));
#183597=CARTESIAN_POINT('Ctrl Pts',(9.98399960699994,11.6,-3.09235406000001));
#183598=CARTESIAN_POINT('Ctrl Pts',(9.98267643199994,15.2,-3.09171723300001));
#183599=CARTESIAN_POINT('Ctrl Pts',(9.98267643199994,11.6,-3.09171723300001));
#183600=CARTESIAN_POINT('Ctrl Pts',(9.98136002599994,15.2,-3.09108520600001));
#183601=CARTESIAN_POINT('Ctrl Pts',(9.98136002599994,11.6,-3.09108520600002));
#183602=CARTESIAN_POINT('Ctrl Pts',(9.98005041699994,15.2,-3.09045797700001));
#183603=CARTESIAN_POINT('Ctrl Pts',(9.98005041699994,11.6,-3.09045797700001));
#183604=CARTESIAN_POINT('Ctrl Pts',(9.97874762699994,15.2,-3.08983553900001));
#183605=CARTESIAN_POINT('Ctrl Pts',(9.97874762699994,11.6,-3.08983553900001));
#183606=CARTESIAN_POINT('Ctrl Pts',(9.97745168099994,15.2,-3.08921789100001));
#183607=CARTESIAN_POINT('Ctrl Pts',(9.97745168099994,11.6,-3.08921789100001));
#183608=CARTESIAN_POINT('Ctrl Pts',(9.97616260499995,15.2,-3.08860502500002));
#183609=CARTESIAN_POINT('Ctrl Pts',(9.97616260499995,11.6,-3.08860502500002));
#183610=CARTESIAN_POINT('Ctrl Pts',(9.97488042199994,15.2,-3.08799693900002));
#183611=CARTESIAN_POINT('Ctrl Pts',(9.97488042199994,11.6,-3.08799693900002));
#183612=CARTESIAN_POINT('Ctrl Pts',(9.97360515799994,15.2,-3.08739362900001));
#183613=CARTESIAN_POINT('Ctrl Pts',(9.97360515799994,11.6,-3.08739362900001));
#183614=CARTESIAN_POINT('Ctrl Pts',(9.97233683899994,15.2,-3.08679508900001));
#183615=CARTESIAN_POINT('Ctrl Pts',(9.97233683899994,11.6,-3.08679508900001));
#183616=CARTESIAN_POINT('Ctrl Pts',(9.97107548799995,15.2,-3.08620131400001));
#183617=CARTESIAN_POINT('Ctrl Pts',(9.97107548799995,11.6,-3.08620131400001));
#183618=CARTESIAN_POINT('Ctrl Pts',(9.96982113299994,15.2,-3.08561230000001));
#183619=CARTESIAN_POINT('Ctrl Pts',(9.96982113299994,11.6,-3.08561230000001));
#183620=CARTESIAN_POINT('Ctrl Pts',(9.96857379799994,15.2,-3.08502804400002));
#183621=CARTESIAN_POINT('Ctrl Pts',(9.96857379799994,11.6,-3.08502804400002));
#183622=CARTESIAN_POINT('Ctrl Pts',(9.96733350799994,15.2,-3.08444853900002));
#183623=CARTESIAN_POINT('Ctrl Pts',(9.96733350799994,11.6,-3.08444853900002));
#183624=CARTESIAN_POINT('Ctrl Pts',(9.96610028899994,15.2,-3.08387378200001));
#183625=CARTESIAN_POINT('Ctrl Pts',(9.96610028899994,11.6,-3.08387378200001));
#183626=CARTESIAN_POINT('Ctrl Pts',(9.96487416899994,15.2,-3.08330376800001));
#183627=CARTESIAN_POINT('Ctrl Pts',(9.96487416899994,11.6,-3.08330376800001));
#183628=CARTESIAN_POINT('Ctrl Pts',(9.96365516999995,15.2,-3.08273849300001));
#183629=CARTESIAN_POINT('Ctrl Pts',(9.96365516999995,11.6,-3.08273849300001));
#183630=CARTESIAN_POINT('Ctrl Pts',(9.96244331999995,15.2,-3.08217795000001));
#183631=CARTESIAN_POINT('Ctrl Pts',(9.96244331999995,11.6,-3.08217795000001));
#183632=CARTESIAN_POINT('Ctrl Pts',(9.96123864599994,15.2,-3.08162213600002));
#183633=CARTESIAN_POINT('Ctrl Pts',(9.96123864599994,11.6,-3.08162213600002));
#183634=CARTESIAN_POINT('Ctrl Pts',(9.96004117299995,15.2,-3.08107104600001));
#183635=CARTESIAN_POINT('Ctrl Pts',(9.96004117299995,11.6,-3.08107104600001));
#183636=CARTESIAN_POINT('Ctrl Pts',(9.95885092599995,15.2,-3.08052467500001));
#183637=CARTESIAN_POINT('Ctrl Pts',(9.95885092599995,11.6,-3.08052467500001));
#183638=CARTESIAN_POINT('Ctrl Pts',(9.95766793399994,15.2,-3.07998301700001));
#183639=CARTESIAN_POINT('Ctrl Pts',(9.95766793399994,11.6,-3.07998301700001));
#183640=CARTESIAN_POINT('Ctrl Pts',(9.95649222199994,15.2,-3.07944607000001));
#183641=CARTESIAN_POINT('Ctrl Pts',(9.95649222199994,11.6,-3.07944607000001));
#183642=CARTESIAN_POINT('Ctrl Pts',(9.95532381799995,15.2,-3.07891382600001));
#183643=CARTESIAN_POINT('Ctrl Pts',(9.95532381799995,11.6,-3.07891382600001));
#183644=CARTESIAN_POINT('Ctrl Pts',(9.95416274699994,15.2,-3.07838628200001));
#183645=CARTESIAN_POINT('Ctrl Pts',(9.95416274699994,11.6,-3.07838628200001));
#183646=CARTESIAN_POINT('Ctrl Pts',(9.95300903599994,15.2,-3.07786343200001));
#183647=CARTESIAN_POINT('Ctrl Pts',(9.95300903599994,11.6,-3.07786343200001));
#183648=CARTESIAN_POINT('Ctrl Pts',(9.95186271399995,15.2,-3.07734527000001));
#183649=CARTESIAN_POINT('Ctrl Pts',(9.95186271399995,11.6,-3.07734527000001));
#183650=CARTESIAN_POINT('Ctrl Pts',(9.95072380599994,15.2,-3.07683179400001));
#183651=CARTESIAN_POINT('Ctrl Pts',(9.95072380599994,11.6,-3.07683179400001));
#183652=CARTESIAN_POINT('Ctrl Pts',(9.94959233999994,15.2,-3.07632299600002));
#183653=CARTESIAN_POINT('Ctrl Pts',(9.94959233999994,11.6,-3.07632299600002));
#183654=CARTESIAN_POINT('Ctrl Pts',(9.94846834299994,15.2,-3.07581887100001));
#183655=CARTESIAN_POINT('Ctrl Pts',(9.94846834299994,11.6,-3.07581887100001));
#183656=CARTESIAN_POINT('Ctrl Pts',(9.94735184299994,15.2,-3.07531941600002));
#183657=CARTESIAN_POINT('Ctrl Pts',(9.94735184299994,11.6,-3.07531941600002));
#183658=CARTESIAN_POINT('Ctrl Pts',(9.94624286799995,15.2,-3.07482462300001));
#183659=CARTESIAN_POINT('Ctrl Pts',(9.94624286799995,11.6,-3.07482462300001));
#183660=CARTESIAN_POINT('Ctrl Pts',(9.94514144399995,15.2,-3.07433448900001));
#183661=CARTESIAN_POINT('Ctrl Pts',(9.94514144399995,11.6,-3.07433448900001));
#183662=CARTESIAN_POINT('Ctrl Pts',(9.94404760099994,15.2,-3.07384900800002));
#183663=CARTESIAN_POINT('Ctrl Pts',(9.94404760099994,11.6,-3.07384900800002));
#183664=CARTESIAN_POINT('Ctrl Pts',(9.94296136499995,15.2,-3.07336817300001));
#183665=CARTESIAN_POINT('Ctrl Pts',(9.94296136499995,11.6,-3.07336817300001));
#183666=CARTESIAN_POINT('Ctrl Pts',(9.94188276499995,15.2,-3.07289198100001));
#183667=CARTESIAN_POINT('Ctrl Pts',(9.94188276499995,11.6,-3.07289198100001));
#183668=CARTESIAN_POINT('Ctrl Pts',(9.94081182899994,15.2,-3.07242042600001));
#183669=CARTESIAN_POINT('Ctrl Pts',(9.94081182899994,11.6,-3.07242042600001));
#183670=CARTESIAN_POINT('Ctrl Pts',(9.93974858499995,15.2,-3.07195350200002));
#183671=CARTESIAN_POINT('Ctrl Pts',(9.93974858499995,11.6,-3.07195350200002));
#183672=CARTESIAN_POINT('Ctrl Pts',(9.93869306299995,15.2,-3.07149120200001));
#183673=CARTESIAN_POINT('Ctrl Pts',(9.93869306299995,11.6,-3.07149120200001));
#183674=CARTESIAN_POINT('Ctrl Pts',(9.93764528999994,15.2,-3.07103352400001));
#183675=CARTESIAN_POINT('Ctrl Pts',(9.93764528999994,11.6,-3.07103352400001));
#183676=CARTESIAN_POINT('Ctrl Pts',(9.93660529499994,15.2,-3.07058045900002));
#183677=CARTESIAN_POINT('Ctrl Pts',(9.93660529499994,11.6,-3.07058045900002));
#183678=CARTESIAN_POINT('Ctrl Pts',(9.93557310799994,15.2,-3.07013200400001));
#183679=CARTESIAN_POINT('Ctrl Pts',(9.93557310799994,11.6,-3.07013200400002));
#183680=CARTESIAN_POINT('Ctrl Pts',(9.93454875699994,15.2,-3.06968815200001));
#183681=CARTESIAN_POINT('Ctrl Pts',(9.93454875699994,11.6,-3.06968815200001));
#183682=CARTESIAN_POINT('Ctrl Pts',(9.93353226999995,15.2,-3.06924889800001));
#183683=CARTESIAN_POINT('Ctrl Pts',(9.93353226999995,11.6,-3.06924889800001));
#183684=CARTESIAN_POINT('Ctrl Pts',(9.93252367799995,15.2,-3.06881423400001));
#183685=CARTESIAN_POINT('Ctrl Pts',(9.93252367799995,11.6,-3.06881423400002));
#183686=CARTESIAN_POINT('Ctrl Pts',(9.93152301099995,15.2,-3.06838415800001));
#183687=CARTESIAN_POINT('Ctrl Pts',(9.93152301099995,11.6,-3.06838415800002));
#183688=CARTESIAN_POINT('Ctrl Pts',(9.93053029599994,15.2,-3.06795866100002));
#183689=CARTESIAN_POINT('Ctrl Pts',(9.93053029599994,11.6,-3.06795866100002));
#183690=CARTESIAN_POINT('Ctrl Pts',(9.92954556499994,15.2,-3.06753773800001));
#183691=CARTESIAN_POINT('Ctrl Pts',(9.92954556499994,11.6,-3.06753773800002));
#183692=CARTESIAN_POINT('Ctrl Pts',(9.92856884499994,15.2,-3.06712138300002));
#183693=CARTESIAN_POINT('Ctrl Pts',(9.92856884499994,11.6,-3.06712138300002));
#183694=CARTESIAN_POINT('Ctrl Pts',(9.92760016999994,15.2,-3.06670959200002));
#183695=CARTESIAN_POINT('Ctrl Pts',(9.92760016999994,11.6,-3.06670959200002));
#183696=CARTESIAN_POINT('Ctrl Pts',(9.92663956699994,15.2,-3.06630235600001));
#183697=CARTESIAN_POINT('Ctrl Pts',(9.92663956699994,11.6,-3.06630235600002));
#183698=CARTESIAN_POINT('Ctrl Pts',(9.92568706699995,15.2,-3.06589967100001));
#183699=CARTESIAN_POINT('Ctrl Pts',(9.92568706699995,11.6,-3.06589967100001));
#183700=CARTESIAN_POINT('Ctrl Pts',(9.92474269999994,15.2,-3.06550153000002));
#183701=CARTESIAN_POINT('Ctrl Pts',(9.92474269999994,11.6,-3.06550153000002));
#183702=CARTESIAN_POINT('Ctrl Pts',(9.92380649799994,15.2,-3.06510792800001));
#183703=CARTESIAN_POINT('Ctrl Pts',(9.92380649799994,11.6,-3.06510792800002));
#183704=CARTESIAN_POINT('Ctrl Pts',(9.92287849099995,15.2,-3.06471885700002));
#183705=CARTESIAN_POINT('Ctrl Pts',(9.92287849099995,11.6,-3.06471885700002));
#183706=CARTESIAN_POINT('Ctrl Pts',(9.92195870799994,15.2,-3.06433431200002));
#183707=CARTESIAN_POINT('Ctrl Pts',(9.92195870799994,11.6,-3.06433431200002));
#183708=CARTESIAN_POINT('Ctrl Pts',(9.92104718299995,15.2,-3.06395428600001));
#183709=CARTESIAN_POINT('Ctrl Pts',(9.92104718299995,11.6,-3.06395428600002));
#183710=CARTESIAN_POINT('Ctrl Pts',(9.92014394399994,15.2,-3.06357877400002));
#183711=CARTESIAN_POINT('Ctrl Pts',(9.92014394399994,11.6,-3.06357877400002));
#183712=CARTESIAN_POINT('Ctrl Pts',(9.91924902499994,15.2,-3.06320776900002));
#183713=CARTESIAN_POINT('Ctrl Pts',(9.91924902499994,11.6,-3.06320776900002));
#183714=CARTESIAN_POINT('Ctrl Pts',(9.91836245599995,15.2,-3.06284126300001));
#183715=CARTESIAN_POINT('Ctrl Pts',(9.91836245599995,11.6,-3.06284126300001));
#183716=CARTESIAN_POINT('Ctrl Pts',(9.91748426799995,15.2,-3.06247925400001));
#183717=CARTESIAN_POINT('Ctrl Pts',(9.91748426799995,11.6,-3.06247925400001));
#183718=CARTESIAN_POINT('Ctrl Pts',(9.91661449399994,15.2,-3.06212173000001));
#183719=CARTESIAN_POINT('Ctrl Pts',(9.91661449399994,11.6,-3.06212173000001));
#183720=CARTESIAN_POINT('Ctrl Pts',(9.91575316499994,15.2,-3.06176868700001));
#183721=CARTESIAN_POINT('Ctrl Pts',(9.91575316499994,11.6,-3.06176868700002));
#183722=CARTESIAN_POINT('Ctrl Pts',(9.91490522599995,15.2,-3.06142212700002));
#183723=CARTESIAN_POINT('Ctrl Pts',(9.91490522599995,11.6,-3.06142212700002));
#183724=CARTESIAN_POINT('Ctrl Pts',(9.91423456699994,15.2,-3.06114880400001));
#183725=CARTESIAN_POINT('Ctrl Pts',(9.91423456699994,11.6,-3.06114880400001));
#183726=CARTESIAN_POINT('Ctrl Pts',(9.91373655899995,15.2,-3.06094627500002));
#183727=CARTESIAN_POINT('Ctrl Pts',(9.91373655899995,11.6,-3.06094627500002));
#183728=CARTESIAN_POINT('Ctrl Pts',(9.91340782499995,15.2,-3.06081277600001));
#183729=CARTESIAN_POINT('Ctrl Pts',(9.91340782499995,11.6,-3.06081277600002));
#183730=CARTESIAN_POINT('Ctrl Pts',(9.91324626499994,15.2,-3.06074721200002));
#183731=CARTESIAN_POINT('Ctrl Pts',(9.91324626499994,11.6,-3.06074721200002));
#183732=CARTESIAN_POINT('',(9.91324626454087,12.2,-3.06074721206411));
#183733=CARTESIAN_POINT('',(9.91324626454087,15.2,-3.06074721206411));
#183734=CARTESIAN_POINT('',(9.91324626399994,12.2,-3.06074721200002));
#183735=CARTESIAN_POINT('Ctrl Pts',(10.8675859439999,12.2,-3.76106045600002));
#183736=CARTESIAN_POINT('Ctrl Pts',(10.8670460909999,12.2,-3.76051902400001));
#183737=CARTESIAN_POINT('Ctrl Pts',(10.8659664939999,12.2,-3.75943667400001));
#183738=CARTESIAN_POINT('Ctrl Pts',(10.8643474199999,12.2,-3.75781469800001));
#183739=CARTESIAN_POINT('Ctrl Pts',(10.8621893019999,12.2,-3.75565515600002));
#183740=CARTESIAN_POINT('Ctrl Pts',(10.8594927299999,12.2,-3.75296088400002));
#183741=CARTESIAN_POINT('Ctrl Pts',(10.8567972349999,12.2,-3.75027176800002));
#183742=CARTESIAN_POINT('Ctrl Pts',(10.8541028209999,12.2,-3.74758780800001));
#183743=CARTESIAN_POINT('Ctrl Pts',(10.8514094899999,12.2,-3.74490900600001));
#183744=CARTESIAN_POINT('Ctrl Pts',(10.8487172499999,12.2,-3.74223536100001));
#183745=CARTESIAN_POINT('Ctrl Pts',(10.8460261069999,12.2,-3.73956687500002));
#183746=CARTESIAN_POINT('Ctrl Pts',(10.8433360699999,12.2,-3.73690354800001));
#183747=CARTESIAN_POINT('Ctrl Pts',(10.8406471529999,12.2,-3.73424538200001));
#183748=CARTESIAN_POINT('Ctrl Pts',(10.8379593649999,12.2,-3.73159237800001));
#183749=CARTESIAN_POINT('Ctrl Pts',(10.8352727169999,12.2,-3.72894453800001));
#183750=CARTESIAN_POINT('Ctrl Pts',(10.8325872199999,12.2,-3.72630186200002));
#183751=CARTESIAN_POINT('Ctrl Pts',(10.8299028829999,12.2,-3.72366435100002));
#183752=CARTESIAN_POINT('Ctrl Pts',(10.8272197149999,12.2,-3.72103200700002));
#183753=CARTESIAN_POINT('Ctrl Pts',(10.8245377239999,12.2,-3.71840483100002));
#183754=CARTESIAN_POINT('Ctrl Pts',(10.8218569179999,12.2,-3.71578282200002));
#183755=CARTESIAN_POINT('Ctrl Pts',(10.8191773059999,12.2,-3.71316598200002));
#183756=CARTESIAN_POINT('Ctrl Pts',(10.8164988939999,12.2,-3.71055431200002));
#183757=CARTESIAN_POINT('Ctrl Pts',(10.8138216939999,12.2,-3.70794781300001));
#183758=CARTESIAN_POINT('Ctrl Pts',(10.8111457129999,12.2,-3.70534648600001));
#183759=CARTESIAN_POINT('Ctrl Pts',(10.8084709609999,12.2,-3.70275033200001));
#183760=CARTESIAN_POINT('Ctrl Pts',(10.8057974489999,12.2,-3.70015935000001));
#183761=CARTESIAN_POINT('Ctrl Pts',(10.8031251839999,12.2,-3.69757354500001));
#183762=CARTESIAN_POINT('Ctrl Pts',(10.8004541779999,12.2,-3.69499291500002));
#183763=CARTESIAN_POINT('Ctrl Pts',(10.7977844379999,12.2,-3.69241746100001));
#183764=CARTESIAN_POINT('Ctrl Pts',(10.7951159729999,12.2,-3.68984718400001));
#183765=CARTESIAN_POINT('Ctrl Pts',(10.7924487949999,12.2,-3.68728208700002));
#183766=CARTESIAN_POINT('Ctrl Pts',(10.7897829079999,12.2,-3.68472216800001));
#183767=CARTESIAN_POINT('Ctrl Pts',(10.7871183259999,12.2,-3.68216742900001));
#183768=CARTESIAN_POINT('Ctrl Pts',(10.7844550569999,12.2,-3.67961787200001));
#183769=CARTESIAN_POINT('Ctrl Pts',(10.7817931069999,12.2,-3.67707349500002));
#183770=CARTESIAN_POINT('Ctrl Pts',(10.7791324889999,12.2,-3.67453430200001));
#183771=CARTESIAN_POINT('Ctrl Pts',(10.7764732109999,12.2,-3.67200029300002));
#183772=CARTESIAN_POINT('Ctrl Pts',(10.7738152829999,12.2,-3.66947146800001));
#183773=CARTESIAN_POINT('Ctrl Pts',(10.7711587129999,12.2,-3.66694782800002));
#183774=CARTESIAN_POINT('Ctrl Pts',(10.7685035109999,12.2,-3.66442937400001));
#183775=CARTESIAN_POINT('Ctrl Pts',(10.7658496859999,12.2,-3.66191610700001));
#183776=CARTESIAN_POINT('Ctrl Pts',(10.7631972489999,12.2,-3.65940802800001));
#183777=CARTESIAN_POINT('Ctrl Pts',(10.7605462079999,12.2,-3.65690513800002));
#183778=CARTESIAN_POINT('Ctrl Pts',(10.7578965719999,12.2,-3.65440743700002));
#183779=CARTESIAN_POINT('Ctrl Pts',(10.7552483519999,12.2,-3.65191492600001));
#183780=CARTESIAN_POINT('Ctrl Pts',(10.7526015559999,12.2,-3.64942760700002));
#183781=CARTESIAN_POINT('Ctrl Pts',(10.7499561929999,12.2,-3.64694547900001));
#183782=CARTESIAN_POINT('Ctrl Pts',(10.7473122739999,12.2,-3.64446854400001));
#183783=CARTESIAN_POINT('Ctrl Pts',(10.7446698079999,12.2,-3.64199680200001));
#183784=CARTESIAN_POINT('Ctrl Pts',(10.7420288039999,12.2,-3.63953025500001));
#183785=CARTESIAN_POINT('Ctrl Pts',(10.7393892719999,12.2,-3.63706890200001));
#183786=CARTESIAN_POINT('Ctrl Pts',(10.7367512209999,12.2,-3.63461274500001));
#183787=CARTESIAN_POINT('Ctrl Pts',(10.7341146619999,12.2,-3.63216178500001));
#183788=CARTESIAN_POINT('Ctrl Pts',(10.7314796019999,12.2,-3.62971602300002));
#183789=CARTESIAN_POINT('Ctrl Pts',(10.7288460529999,12.2,-3.62727545700002));
#183790=CARTESIAN_POINT('Ctrl Pts',(10.7262140239999,12.2,-3.62484009100001));
#183791=CARTESIAN_POINT('Ctrl Pts',(10.7235835239999,12.2,-3.62240992500002));
#183792=CARTESIAN_POINT('Ctrl Pts',(10.7209545619999,12.2,-3.61998495800002));
#183793=CARTESIAN_POINT('Ctrl Pts',(10.7183271499999,12.2,-3.61756519200001));
#183794=CARTESIAN_POINT('Ctrl Pts',(10.7157012959999,12.2,-3.61515062900001));
#183795=CARTESIAN_POINT('Ctrl Pts',(10.7130770099999,12.2,-3.61274126800001));
#183796=CARTESIAN_POINT('Ctrl Pts',(10.7104543019999,12.2,-3.61033710900001));
#183797=CARTESIAN_POINT('Ctrl Pts',(10.7078331809999,12.2,-3.60793815500001));
#183798=CARTESIAN_POINT('Ctrl Pts',(10.7052136559999,12.2,-3.60554440400001));
#183799=CARTESIAN_POINT('Ctrl Pts',(10.7025957399999,12.2,-3.60315585900001));
#183800=CARTESIAN_POINT('Ctrl Pts',(10.6999794399999,12.2,-3.60077252100002));
#183801=CARTESIAN_POINT('Ctrl Pts',(10.6973647669999,12.2,-3.59839438800002));
#183802=CARTESIAN_POINT('Ctrl Pts',(10.6947517299999,12.2,-3.59602146200002));
#183803=CARTESIAN_POINT('Ctrl Pts',(10.6921403399999,12.2,-3.59365374400001));
#183804=CARTESIAN_POINT('Ctrl Pts',(10.6895306049999,12.2,-3.59129123500002));
#183805=CARTESIAN_POINT('Ctrl Pts',(10.6869225359999,12.2,-3.58893393500002));
#183806=CARTESIAN_POINT('Ctrl Pts',(10.6843161429999,12.2,-3.58658184500001));
#183807=CARTESIAN_POINT('Ctrl Pts',(10.6817114369999,12.2,-3.58423496500002));
#183808=CARTESIAN_POINT('Ctrl Pts',(10.6791084249999,12.2,-3.58189329600001));
#183809=CARTESIAN_POINT('Ctrl Pts',(10.6765071199999,12.2,-3.57955683900002));
#183810=CARTESIAN_POINT('Ctrl Pts',(10.6739075299999,12.2,-3.57722559400001));
#183811=CARTESIAN_POINT('Ctrl Pts',(10.6713096659999,12.2,-3.57489956100002));
#183812=CARTESIAN_POINT('Ctrl Pts',(10.6687135369999,12.2,-3.57257874200001));
#183813=CARTESIAN_POINT('Ctrl Pts',(10.6661191539999,12.2,-3.57026313700001));
#183814=CARTESIAN_POINT('Ctrl Pts',(10.6635265279999,12.2,-3.56795274600001));
#183815=CARTESIAN_POINT('Ctrl Pts',(10.6609356659999,12.2,-3.56564757100001));
#183816=CARTESIAN_POINT('Ctrl Pts',(10.6583465819999,12.2,-3.56334761200001));
#183817=CARTESIAN_POINT('Ctrl Pts',(10.6557592819999,12.2,-3.56105286800001));
#183818=CARTESIAN_POINT('Ctrl Pts',(10.6531737789999,12.2,-3.55876334200001));
#183819=CARTESIAN_POINT('Ctrl Pts',(10.6505900819999,12.2,-3.55647903300001));
#183820=CARTESIAN_POINT('Ctrl Pts',(10.6480082019999,12.2,-3.55419994100002));
#183821=CARTESIAN_POINT('Ctrl Pts',(10.6454281479999,12.2,-3.55192606900002));
#183822=CARTESIAN_POINT('Ctrl Pts',(10.6428499309999,12.2,-3.54965741400001));
#183823=CARTESIAN_POINT('Ctrl Pts',(10.6402735619999,12.2,-3.54739398000001));
#183824=CARTESIAN_POINT('Ctrl Pts',(10.6376990499999,12.2,-3.54513576600001));
#183825=CARTESIAN_POINT('Ctrl Pts',(10.6351264049999,12.2,-3.54288277200002));
#183826=CARTESIAN_POINT('Ctrl Pts',(10.6325556389999,12.2,-3.54063499900001));
#183827=CARTESIAN_POINT('Ctrl Pts',(10.6299867589999,12.2,-3.53839244700001));
#183828=CARTESIAN_POINT('Ctrl Pts',(10.6274197799999,12.2,-3.53615511700001));
#183829=CARTESIAN_POINT('Ctrl Pts',(10.6248547079999,12.2,-3.53392301000001));
#183830=CARTESIAN_POINT('Ctrl Pts',(10.6222915559999,12.2,-3.53169612600002));
#183831=CARTESIAN_POINT('Ctrl Pts',(10.6197303339999,12.2,-3.52947446500002));
#183832=CARTESIAN_POINT('Ctrl Pts',(10.6171710509999,12.2,-3.52725802700002));
#183833=CARTESIAN_POINT('Ctrl Pts',(10.6146137189999,12.2,-3.52504681400001));
#183834=CARTESIAN_POINT('Ctrl Pts',(10.6120583479999,12.2,-3.52284082600002));
#183835=CARTESIAN_POINT('Ctrl Pts',(10.6095049489999,12.2,-3.52064006300001));
#183836=CARTESIAN_POINT('Ctrl Pts',(10.6069535309999,12.2,-3.51844452500002));
#183837=CARTESIAN_POINT('Ctrl Pts',(10.6044041049999,12.2,-3.51625421300001));
#183838=CARTESIAN_POINT('Ctrl Pts',(10.6018566829999,12.2,-3.51406912700002));
#183839=CARTESIAN_POINT('Ctrl Pts',(10.5993112729999,12.2,-3.51188926900001));
#183840=CARTESIAN_POINT('Ctrl Pts',(10.5967678879999,12.2,-3.50971463600001));
#183841=CARTESIAN_POINT('Ctrl Pts',(10.5942265379999,12.2,-3.50754523200001));
#183842=CARTESIAN_POINT('Ctrl Pts',(10.5916872319999,12.2,-3.50538105500001));
#183843=CARTESIAN_POINT('Ctrl Pts',(10.5891499829999,12.2,-3.50322210700002));
#183844=CARTESIAN_POINT('Ctrl Pts',(10.5866147999999,12.2,-3.50106838700002));
#183845=CARTESIAN_POINT('Ctrl Pts',(10.5840816949999,12.2,-3.49891989600001));
#183846=CARTESIAN_POINT('Ctrl Pts',(10.5815506769999,12.2,-3.49677663500001));
#183847=CARTESIAN_POINT('Ctrl Pts',(10.5790217569999,12.2,-3.49463860200002));
#183848=CARTESIAN_POINT('Ctrl Pts',(10.5764949479999,12.2,-3.49250580000001));
#183849=CARTESIAN_POINT('Ctrl Pts',(10.5739702579999,12.2,-3.49037822900002));
#183850=CARTESIAN_POINT('Ctrl Pts',(10.5714476989999,12.2,-3.48825588800001));
#183851=CARTESIAN_POINT('Ctrl Pts',(10.5689272829999,12.2,-3.48613877700001));
#183852=CARTESIAN_POINT('Ctrl Pts',(10.5664090179999,12.2,-3.48402689800002));
#183853=CARTESIAN_POINT('Ctrl Pts',(10.5638929169999,12.2,-3.48192025000001));
#183854=CARTESIAN_POINT('Ctrl Pts',(10.5613789899999,12.2,-3.47981883400001));
#183855=CARTESIAN_POINT('Ctrl Pts',(10.5588672479999,12.2,-3.47772265000001));
#183856=CARTESIAN_POINT('Ctrl Pts',(10.5563577029999,12.2,-3.47563169800001));
#183857=CARTESIAN_POINT('Ctrl Pts',(10.5538503639999,12.2,-3.47354597800001));
#183858=CARTESIAN_POINT('Ctrl Pts',(10.5513452449999,12.2,-3.47146549100001));
#183859=CARTESIAN_POINT('Ctrl Pts',(10.5488423529999,12.2,-3.46939023800001));
#183860=CARTESIAN_POINT('Ctrl Pts',(10.5463417019999,12.2,-3.46732021700001));
#183861=CARTESIAN_POINT('Ctrl Pts',(10.5438433009999,12.2,-3.46525543000002));
#183862=CARTESIAN_POINT('Ctrl Pts',(10.5413471629999,12.2,-3.46319587600001));
#183863=CARTESIAN_POINT('Ctrl Pts',(10.5388532969999,12.2,-3.46114155700001));
#183864=CARTESIAN_POINT('Ctrl Pts',(10.5363617169999,12.2,-3.45909247100002));
#183865=CARTESIAN_POINT('Ctrl Pts',(10.5338724319999,12.2,-3.45704862000002));
#183866=CARTESIAN_POINT('Ctrl Pts',(10.5313854529999,12.2,-3.45501000300001));
#183867=CARTESIAN_POINT('Ctrl Pts',(10.5289007929999,12.2,-3.45297662100001));
#183868=CARTESIAN_POINT('Ctrl Pts',(10.5264184599999,12.2,-3.45094847300001));
#183869=CARTESIAN_POINT('Ctrl Pts',(10.5239384669999,12.2,-3.44892556000001));
#183870=CARTESIAN_POINT('Ctrl Pts',(10.5214608269999,12.2,-3.44690788300001));
#183871=CARTESIAN_POINT('Ctrl Pts',(10.5189855499999,12.2,-3.44489544000002));
#183872=CARTESIAN_POINT('Ctrl Pts',(10.5165126449999,12.2,-3.44288823300001));
#183873=CARTESIAN_POINT('Ctrl Pts',(10.5140421269999,12.2,-3.44088626100001));
#183874=CARTESIAN_POINT('Ctrl Pts',(10.5115740039999,12.2,-3.43888952500001));
#183875=CARTESIAN_POINT('Ctrl Pts',(10.5091082899999,12.2,-3.43689802500001));
#183876=CARTESIAN_POINT('Ctrl Pts',(10.5066449939999,12.2,-3.43491176000001));
#183877=CARTESIAN_POINT('Ctrl Pts',(10.5041841299999,12.2,-3.43293073100002));
#183878=CARTESIAN_POINT('Ctrl Pts',(10.5017257079999,12.2,-3.43095493800002));
#183879=CARTESIAN_POINT('Ctrl Pts',(10.4992697399999,12.2,-3.42898438100002));
#183880=CARTESIAN_POINT('Ctrl Pts',(10.4968162359999,12.2,-3.42701906000002));
#183881=CARTESIAN_POINT('Ctrl Pts',(10.4943652099999,12.2,-3.42505897500001));
#183882=CARTESIAN_POINT('Ctrl Pts',(10.4919166709999,12.2,-3.42310412600002));
#183883=CARTESIAN_POINT('Ctrl Pts',(10.4894706319999,12.2,-3.42115451300002));
#183884=CARTESIAN_POINT('Ctrl Pts',(10.4870271039999,12.2,-3.41921013700001));
#183885=CARTESIAN_POINT('Ctrl Pts',(10.4845860999999,12.2,-3.41727099600002));
#183886=CARTESIAN_POINT('Ctrl Pts',(10.4821476289999,12.2,-3.41533709100001));
#183887=CARTESIAN_POINT('Ctrl Pts',(10.4797117049999,12.2,-3.41340842300002));
#183888=CARTESIAN_POINT('Ctrl Pts',(10.4772783389999,12.2,-3.41148499200001));
#183889=CARTESIAN_POINT('Ctrl Pts',(10.4748475419999,12.2,-3.40956679600001));
#183890=CARTESIAN_POINT('Ctrl Pts',(10.4724193259999,12.2,-3.40765383700001));
#183891=CARTESIAN_POINT('Ctrl Pts',(10.4699937039999,12.2,-3.40574611300001));
#183892=CARTESIAN_POINT('Ctrl Pts',(10.4675706859999,12.2,-3.40384362500001));
#183893=CARTESIAN_POINT('Ctrl Pts',(10.4651502849999,12.2,-3.40194637400002));
#183894=CARTESIAN_POINT('Ctrl Pts',(10.4627325119999,12.2,-3.40005435900002));
#183895=CARTESIAN_POINT('Ctrl Pts',(10.4603173799999,12.2,-3.39816757900001));
#183896=CARTESIAN_POINT('Ctrl Pts',(10.4579048999999,12.2,-3.39628603500001));
#183897=CARTESIAN_POINT('Ctrl Pts',(10.4554950839999,12.2,-3.39440972700002));
#183898=CARTESIAN_POINT('Ctrl Pts',(10.4530879439999,12.2,-3.39253865400002));
#183899=CARTESIAN_POINT('Ctrl Pts',(10.4506834919999,12.2,-3.39067281600002));
#183900=CARTESIAN_POINT('Ctrl Pts',(10.4482817399999,12.2,-3.38881221500001));
#183901=CARTESIAN_POINT('Ctrl Pts',(10.4458826999999,12.2,-3.38695684700001));
#183902=CARTESIAN_POINT('Ctrl Pts',(10.4434863849999,12.2,-3.38510671600002));
#183903=CARTESIAN_POINT('Ctrl Pts',(10.4410928049999,12.2,-3.38326181800001));
#183904=CARTESIAN_POINT('Ctrl Pts',(10.4387019739999,12.2,-3.38142215600001));
#183905=CARTESIAN_POINT('Ctrl Pts',(10.4363139019999,12.2,-3.37958772900001));
#183906=CARTESIAN_POINT('Ctrl Pts',(10.4339286029999,12.2,-3.37775853500001));
#183907=CARTESIAN_POINT('Ctrl Pts',(10.4315460899999,12.2,-3.37593457500001));
#183908=CARTESIAN_POINT('Ctrl Pts',(10.4291663729999,12.2,-3.37411585000002));
#183909=CARTESIAN_POINT('Ctrl Pts',(10.4267894639999,12.2,-3.37230235900002));
#183910=CARTESIAN_POINT('Ctrl Pts',(10.4244153789999,12.2,-3.37049410100001));
#183911=CARTESIAN_POINT('Ctrl Pts',(10.4220441259999,12.2,-3.36869107600001));
#183912=CARTESIAN_POINT('Ctrl Pts',(10.4196757189999,12.2,-3.36689328500002));
#183913=CARTESIAN_POINT('Ctrl Pts',(10.4173101699999,12.2,-3.36510072600001));
#183914=CARTESIAN_POINT('Ctrl Pts',(10.4149474929999,12.2,-3.36331340000001));
#183915=CARTESIAN_POINT('Ctrl Pts',(10.4125876979999,12.2,-3.36153130600001));
#183916=CARTESIAN_POINT('Ctrl Pts',(10.4102307989999,12.2,-3.35975444400002));
#183917=CARTESIAN_POINT('Ctrl Pts',(10.4078768069999,12.2,-3.35798281300002));
#183918=CARTESIAN_POINT('Ctrl Pts',(10.4055257379999,12.2,-3.35621641400001));
#183919=CARTESIAN_POINT('Ctrl Pts',(10.4031775999999,12.2,-3.35445524600001));
#183920=CARTESIAN_POINT('Ctrl Pts',(10.4008324069999,12.2,-3.35269930900001));
#183921=CARTESIAN_POINT('Ctrl Pts',(10.3984901739999,12.2,-3.35094860300002));
#183922=CARTESIAN_POINT('Ctrl Pts',(10.3961509099999,12.2,-3.34920312600001));
#183923=CARTESIAN_POINT('Ctrl Pts',(10.3938146309999,12.2,-3.34746287900002));
#183924=CARTESIAN_POINT('Ctrl Pts',(10.3914813469999,12.2,-3.34572786200001));
#183925=CARTESIAN_POINT('Ctrl Pts',(10.3891510709999,12.2,-3.34399807300001));
#183926=CARTESIAN_POINT('Ctrl Pts',(10.3868238179999,12.2,-3.34227351400001));
#183927=CARTESIAN_POINT('Ctrl Pts',(10.3844995979999,12.2,-3.34055418200002));
#183928=CARTESIAN_POINT('Ctrl Pts',(10.3821784259999,12.2,-3.33884007800001));
#183929=CARTESIAN_POINT('Ctrl Pts',(10.3798603139999,12.2,-3.33713120100001));
#183930=CARTESIAN_POINT('Ctrl Pts',(10.3775452729999,12.2,-3.33542755200002));
#183931=CARTESIAN_POINT('Ctrl Pts',(10.3752333189999,12.2,-3.33372913000002));
#183932=CARTESIAN_POINT('Ctrl Pts',(10.3729244619999,12.2,-3.33203593300002));
#183933=CARTESIAN_POINT('Ctrl Pts',(10.3706187169999,12.2,-3.33034796100002));
#183934=CARTESIAN_POINT('Ctrl Pts',(10.3683160969999,12.2,-3.32866521600002));
#183935=CARTESIAN_POINT('Ctrl Pts',(10.3660166129999,12.2,-3.32698769300002));
#183936=CARTESIAN_POINT('Ctrl Pts',(10.3637202799999,12.2,-3.32531539600001));
#183937=CARTESIAN_POINT('Ctrl Pts',(10.3614271109999,12.2,-3.32364832300001));
#183938=CARTESIAN_POINT('Ctrl Pts',(10.3591371169999,12.2,-3.32198647300002));
#183939=CARTESIAN_POINT('Ctrl Pts',(10.3568503129999,12.2,-3.32032984500001));
#183940=CARTESIAN_POINT('Ctrl Pts',(10.3545667119999,12.2,-3.31867843900001));
#183941=CARTESIAN_POINT('Ctrl Pts',(10.3522863269999,12.2,-3.31703225500001));
#183942=CARTESIAN_POINT('Ctrl Pts',(10.3500091699999,12.2,-3.31539129200001));
#183943=CARTESIAN_POINT('Ctrl Pts',(10.3477352559999,12.2,-3.31375555000001));
#183944=CARTESIAN_POINT('Ctrl Pts',(10.3454645979999,12.2,-3.31212502700001));
#183945=CARTESIAN_POINT('Ctrl Pts',(10.3431972079999,12.2,-3.31049972300002));
#183946=CARTESIAN_POINT('Ctrl Pts',(10.3409331009999,12.2,-3.30887963800001));
#183947=CARTESIAN_POINT('Ctrl Pts',(10.3386722889999,12.2,-3.30726477100002));
#183948=CARTESIAN_POINT('Ctrl Pts',(10.3364147869999,12.2,-3.30565512200002));
#183949=CARTESIAN_POINT('Ctrl Pts',(10.3341606059999,12.2,-3.30405069000001));
#183950=CARTESIAN_POINT('Ctrl Pts',(10.3319097619999,12.2,-3.30245147300001));
#183951=CARTESIAN_POINT('Ctrl Pts',(10.3296622669999,12.2,-3.30085747200001));
#183952=CARTESIAN_POINT('Ctrl Pts',(10.3274181339999,12.2,-3.29926868600001));
#183953=CARTESIAN_POINT('Ctrl Pts',(10.3251773799999,12.2,-3.29768511400002));
#183954=CARTESIAN_POINT('Ctrl Pts',(10.3229400139999,12.2,-3.29610675500001));
#183955=CARTESIAN_POINT('Ctrl Pts',(10.3207060529999,12.2,-3.29453360900001));
#183956=CARTESIAN_POINT('Ctrl Pts',(10.3184755079999,12.2,-3.29296567500001));
#183957=CARTESIAN_POINT('Ctrl Pts',(10.3162483959999,12.2,-3.29140295300002));
#183958=CARTESIAN_POINT('Ctrl Pts',(10.3140247269999,12.2,-3.28984544000001));
#183959=CARTESIAN_POINT('Ctrl Pts',(10.3118045179999,12.2,-3.28829313800002));
#183960=CARTESIAN_POINT('Ctrl Pts',(10.3095877799999,12.2,-3.28674604500002));
#183961=CARTESIAN_POINT('Ctrl Pts',(10.3073745299999,12.2,-3.28520415900002));
#183962=CARTESIAN_POINT('Ctrl Pts',(10.3051647789999,12.2,-3.28366748100001));
#183963=CARTESIAN_POINT('Ctrl Pts',(10.3029585419999,12.2,-3.28213601000002));
#183964=CARTESIAN_POINT('Ctrl Pts',(10.3007558329999,12.2,-3.28060974400001));
#183965=CARTESIAN_POINT('Ctrl Pts',(10.2985566669999,12.2,-3.27908868400002));
#183966=CARTESIAN_POINT('Ctrl Pts',(10.2963610559999,12.2,-3.27757282800002));
#183967=CARTESIAN_POINT('Ctrl Pts',(10.2941690149999,12.2,-3.27606217500001));
#183968=CARTESIAN_POINT('Ctrl Pts',(10.2919805579999,12.2,-3.27455672400002));
#183969=CARTESIAN_POINT('Ctrl Pts',(10.2897957009999,12.2,-3.27305647500001));
#183970=CARTESIAN_POINT('Ctrl Pts',(10.2876144549999,12.2,-3.27156142700002));
#183971=CARTESIAN_POINT('Ctrl Pts',(10.2854368349999,12.2,-3.27007157800002));
#183972=CARTESIAN_POINT('Ctrl Pts',(10.2832628569999,12.2,-3.26858692800001));
#183973=CARTESIAN_POINT('Ctrl Pts',(10.2810925339999,12.2,-3.26710747600002));
#183974=CARTESIAN_POINT('Ctrl Pts',(10.2789258799999,12.2,-3.26563322100001));
#183975=CARTESIAN_POINT('Ctrl Pts',(10.2767629099999,12.2,-3.26416416200002));
#183976=CARTESIAN_POINT('Ctrl Pts',(10.2746036379999,12.2,-3.26270029800002));
#183977=CARTESIAN_POINT('Ctrl Pts',(10.2724480789999,12.2,-3.26124162800001));
#183978=CARTESIAN_POINT('Ctrl Pts',(10.2702962469999,12.2,-3.25978815000001));
#183979=CARTESIAN_POINT('Ctrl Pts',(10.2681481549999,12.2,-3.25833986600002));
#183980=CARTESIAN_POINT('Ctrl Pts',(10.2660038209999,12.2,-3.25689677200002));
#183981=CARTESIAN_POINT('Ctrl Pts',(10.2638632559999,12.2,-3.25545886800001));
#183982=CARTESIAN_POINT('Ctrl Pts',(10.2617264769999,12.2,-3.25402615300002));
#183983=CARTESIAN_POINT('Ctrl Pts',(10.2595934979999,12.2,-3.25259862700001));
#183984=CARTESIAN_POINT('Ctrl Pts',(10.2574643339999,12.2,-3.25117628600001));
#183985=CARTESIAN_POINT('Ctrl Pts',(10.2553389979999,12.2,-3.24975913200001));
#183986=CARTESIAN_POINT('Ctrl Pts',(10.2532175069999,12.2,-3.24834716200002));
#183987=CARTESIAN_POINT('Ctrl Pts',(10.2510998739999,12.2,-3.24694037600001));
#183988=CARTESIAN_POINT('Ctrl Pts',(10.2489861149999,12.2,-3.24553877200001));
#183989=CARTESIAN_POINT('Ctrl Pts',(10.2468762449999,12.2,-3.24414235000001));
#183990=CARTESIAN_POINT('Ctrl Pts',(10.2447702779999,12.2,-3.24275110800002));
#183991=CARTESIAN_POINT('Ctrl Pts',(10.2426682289999,12.2,-3.24136504400002));
#183992=CARTESIAN_POINT('Ctrl Pts',(10.2405701139999,12.2,-3.23998415800002));
#183993=CARTESIAN_POINT('Ctrl Pts',(10.2384759469999,12.2,-3.23860844800001));
#183994=CARTESIAN_POINT('Ctrl Pts',(10.2363857439999,12.2,-3.23723791500001));
#183995=CARTESIAN_POINT('Ctrl Pts',(10.2342995189999,12.2,-3.23587255500001));
#183996=CARTESIAN_POINT('Ctrl Pts',(10.2322172889999,12.2,-3.23451236800001));
#183997=CARTESIAN_POINT('Ctrl Pts',(10.2301390659999,12.2,-3.23315735300001));
#183998=CARTESIAN_POINT('Ctrl Pts',(10.2280648689999,12.2,-3.23180750800002));
#183999=CARTESIAN_POINT('Ctrl Pts',(10.2259947109999,12.2,-3.23046283300001));
#184000=CARTESIAN_POINT('Ctrl Pts',(10.2239286079999,12.2,-3.22912332500001));
#184001=CARTESIAN_POINT('Ctrl Pts',(10.2218665749999,12.2,-3.22778898400002));
#184002=CARTESIAN_POINT('Ctrl Pts',(10.2198086269999,12.2,-3.22645980700001));
#184003=CARTESIAN_POINT('Ctrl Pts',(10.2177547809999,12.2,-3.22513579400002));
#184004=CARTESIAN_POINT('Ctrl Pts',(10.2157050509999,12.2,-3.22381694500002));
#184005=CARTESIAN_POINT('Ctrl Pts',(10.2136594529999,12.2,-3.22250325600002));
#184006=CARTESIAN_POINT('Ctrl Pts',(10.2116180039999,12.2,-3.22119472700001));
#184007=CARTESIAN_POINT('Ctrl Pts',(10.2095807169999,12.2,-3.21989135600001));
#184008=CARTESIAN_POINT('Ctrl Pts',(10.2075476089999,12.2,-3.21859314200001));
#184009=CARTESIAN_POINT('Ctrl Pts',(10.2055186959999,12.2,-3.21730008500001));
#184010=CARTESIAN_POINT('Ctrl Pts',(10.2034939929999,12.2,-3.21601218000001));
#184011=CARTESIAN_POINT('Ctrl Pts',(10.2014735169999,12.2,-3.21472942900002));
#184012=CARTESIAN_POINT('Ctrl Pts',(10.1994572829999,12.2,-3.21345182800002));
#184013=CARTESIAN_POINT('Ctrl Pts',(10.1974453069999,12.2,-3.21217937700002));
#184014=CARTESIAN_POINT('Ctrl Pts',(10.1954376039999,12.2,-3.21091207400002));
#184015=CARTESIAN_POINT('Ctrl Pts',(10.1934341909999,12.2,-3.20964991800002));
#184016=CARTESIAN_POINT('Ctrl Pts',(10.1914350849999,12.2,-3.20839290800001));
#184017=CARTESIAN_POINT('Ctrl Pts',(10.1894402999999,12.2,-3.20714104000002));
#184018=CARTESIAN_POINT('Ctrl Pts',(10.1874498539999,12.2,-3.20589431400002));
#184019=CARTESIAN_POINT('Ctrl Pts',(10.1854637609999,12.2,-3.20465272900002));
#184020=CARTESIAN_POINT('Ctrl Pts',(10.1834820399999,12.2,-3.20341628300001));
#184021=CARTESIAN_POINT('Ctrl Pts',(10.1815047049999,12.2,-3.20218497500001));
#184022=CARTESIAN_POINT('Ctrl Pts',(10.1795317729999,12.2,-3.20095880100002));
#184023=CARTESIAN_POINT('Ctrl Pts',(10.1775632609999,12.2,-3.19973776100001));
#184024=CARTESIAN_POINT('Ctrl Pts',(10.1755991829999,12.2,-3.19852185400002));
#184025=CARTESIAN_POINT('Ctrl Pts',(10.1736395589999,12.2,-3.19731107700001));
#184026=CARTESIAN_POINT('Ctrl Pts',(10.1716844029999,12.2,-3.19610542900001));
#184027=CARTESIAN_POINT('Ctrl Pts',(10.1697337309999,12.2,-3.19490490900002));
#184028=CARTESIAN_POINT('Ctrl Pts',(10.1677875629999,12.2,-3.19370951400002));
#184029=CARTESIAN_POINT('Ctrl Pts',(10.1658459129999,12.2,-3.19251924300001));
#184030=CARTESIAN_POINT('Ctrl Pts',(10.1639087969999,12.2,-3.19133409300001));
#184031=CARTESIAN_POINT('Ctrl Pts',(10.1619762339999,12.2,-3.19015406500001));
#184032=CARTESIAN_POINT('Ctrl Pts',(10.1600482389999,12.2,-3.18897915400001));
#184033=CARTESIAN_POINT('Ctrl Pts',(10.1581248299999,12.2,-3.18780935900001));
#184034=CARTESIAN_POINT('Ctrl Pts',(10.1562060229999,12.2,-3.18664468000001));
#184035=CARTESIAN_POINT('Ctrl Pts',(10.1542918349999,12.2,-3.18548511300001));
#184036=CARTESIAN_POINT('Ctrl Pts',(10.1523822839999,12.2,-3.18433065800001));
#184037=CARTESIAN_POINT('Ctrl Pts',(10.1504773859999,12.2,-3.18318131200002));
#184038=CARTESIAN_POINT('Ctrl Pts',(10.1485771589999,12.2,-3.18203707400002));
#184039=CARTESIAN_POINT('Ctrl Pts',(10.1466816179999,12.2,-3.18089793900001));
#184040=CARTESIAN_POINT('Ctrl Pts',(10.1447907829999,12.2,-3.17976391000002));
#184041=CARTESIAN_POINT('Ctrl Pts',(10.1429046699999,12.2,-3.17863498200001));
#184042=CARTESIAN_POINT('Ctrl Pts',(10.1410232959999,12.2,-3.17751115200001));
#184043=CARTESIAN_POINT('Ctrl Pts',(10.1391466789999,12.2,-3.17639242200002));
#184044=CARTESIAN_POINT('Ctrl Pts',(10.1372748349999,12.2,-3.17527878600002));
#184045=CARTESIAN_POINT('Ctrl Pts',(10.1354077839999,12.2,-3.17417024400001));
#184046=CARTESIAN_POINT('Ctrl Pts',(10.1335455409999,12.2,-3.17306679400001));
#184047=CARTESIAN_POINT('Ctrl Pts',(10.1316881249999,12.2,-3.17196843300001));
#184048=CARTESIAN_POINT('Ctrl Pts',(10.1298355529999,12.2,-3.17087516000001));
#184049=CARTESIAN_POINT('Ctrl Pts',(10.1279878419999,12.2,-3.16978697100001));
#184050=CARTESIAN_POINT('Ctrl Pts',(10.1261450119999,12.2,-3.16870386600002));
#184051=CARTESIAN_POINT('Ctrl Pts',(10.1243070779999,12.2,-3.16762584300001));
#184052=CARTESIAN_POINT('Ctrl Pts',(10.1224740599999,12.2,-3.16655289800002));
#184053=CARTESIAN_POINT('Ctrl Pts',(10.1206459739999,12.2,-3.16548503000002));
#184054=CARTESIAN_POINT('Ctrl Pts',(10.1188228389999,12.2,-3.16442223800002));
#184055=CARTESIAN_POINT('Ctrl Pts',(10.1170046749999,12.2,-3.16336451600002));
#184056=CARTESIAN_POINT('Ctrl Pts',(10.1151914959999,12.2,-3.16231186600001));
#184057=CARTESIAN_POINT('Ctrl Pts',(10.1133833219999,12.2,-3.16126428300001));
#184058=CARTESIAN_POINT('Ctrl Pts',(10.1115801729999,12.2,-3.16022176700002));
#184059=CARTESIAN_POINT('Ctrl Pts',(10.1097820639999,12.2,-3.15918431300001));
#184060=CARTESIAN_POINT('Ctrl Pts',(10.1079890159999,12.2,-3.15815192100001));
#184061=CARTESIAN_POINT('Ctrl Pts',(10.1062010459999,12.2,-3.15712458800002));
#184062=CARTESIAN_POINT('Ctrl Pts',(10.1044181719999,12.2,-3.15610231100001));
#184063=CARTESIAN_POINT('Ctrl Pts',(10.1026404129999,12.2,-3.15508509000002));
#184064=CARTESIAN_POINT('Ctrl Pts',(10.1008677879999,12.2,-3.15407291900001));
#184065=CARTESIAN_POINT('Ctrl Pts',(10.0991003149999,12.2,-3.15306579700001));
#184066=CARTESIAN_POINT('Ctrl Pts',(10.0973380129999,12.2,-3.15206372300001));
#184067=CARTESIAN_POINT('Ctrl Pts',(10.0955808999999,12.2,-3.15106669300001));
#184068=CARTESIAN_POINT('Ctrl Pts',(10.0938289959999,12.2,-3.15007470700001));
#184069=CARTESIAN_POINT('Ctrl Pts',(10.0920823179999,12.2,-3.14908775800002));
#184070=CARTESIAN_POINT('Ctrl Pts',(10.0903408869999,12.2,-3.14810584800002));
#184071=CARTESIAN_POINT('Ctrl Pts',(10.0886047199999,12.2,-3.14712897300002));
#184072=CARTESIAN_POINT('Ctrl Pts',(10.0868738369999,12.2,-3.14615712900002));
#184073=CARTESIAN_POINT('Ctrl Pts',(10.0851482559999,12.2,-3.14519031400001));
#184074=CARTESIAN_POINT('Ctrl Pts',(10.0834279989999,12.2,-3.14422852800002));
#184075=CARTESIAN_POINT('Ctrl Pts',(10.0817130829999,12.2,-3.14327176500001));
#184076=CARTESIAN_POINT('Ctrl Pts',(10.0800035259999,12.2,-3.14232002500002));
#184077=CARTESIAN_POINT('Ctrl Pts',(10.0782993499999,12.2,-3.14137330300001));
#184078=CARTESIAN_POINT('Ctrl Pts',(10.0766005729999,12.2,-3.14043159900002));
#184079=CARTESIAN_POINT('Ctrl Pts',(10.0749072159999,12.2,-3.13949490700002));
#184080=CARTESIAN_POINT('Ctrl Pts',(10.0732192959999,12.2,-3.13856322800001));
#184081=CARTESIAN_POINT('Ctrl Pts',(10.0715368339999,12.2,-3.13763655600001));
#184082=CARTESIAN_POINT('Ctrl Pts',(10.0698598489999,12.2,-3.13671489000001));
#184083=CARTESIAN_POINT('Ctrl Pts',(10.0681883619999,12.2,-3.13579822800001));
#184084=CARTESIAN_POINT('Ctrl Pts',(10.0665223919999,12.2,-3.13488656500001));
#184085=CARTESIAN_POINT('Ctrl Pts',(10.0648619579999,12.2,-3.13397990000002));
#184086=CARTESIAN_POINT('Ctrl Pts',(10.0632070809999,12.2,-3.13307822900001));
#184087=CARTESIAN_POINT('Ctrl Pts',(10.0615577799999,12.2,-3.13218155100001));
#184088=CARTESIAN_POINT('Ctrl Pts',(10.0599140779999,12.2,-3.13128986000001));
#184089=CARTESIAN_POINT('Ctrl Pts',(10.0582759909999,12.2,-3.13040315700002));
#184090=CARTESIAN_POINT('Ctrl Pts',(10.0566435409999,12.2,-3.12952143500001));
#184091=CARTESIAN_POINT('Ctrl Pts',(10.0550167499999,12.2,-3.12864469400001));
#184092=CARTESIAN_POINT('Ctrl Pts',(10.0533956349999,12.2,-3.12777293000002));
#184093=CARTESIAN_POINT('Ctrl Pts',(10.0517802179999,12.2,-3.12690614000001));
#184094=CARTESIAN_POINT('Ctrl Pts',(10.0501705219999,12.2,-3.12604432200001));
#184095=CARTESIAN_POINT('Ctrl Pts',(10.0485665629999,12.2,-3.12518747000002));
#184096=CARTESIAN_POINT('Ctrl Pts',(10.0469683629999,12.2,-3.12433558500001));
#184097=CARTESIAN_POINT('Ctrl Pts',(10.0453759449999,12.2,-3.12348866100002));
#184098=CARTESIAN_POINT('Ctrl Pts',(10.0437893269999,12.2,-3.12264669700001));
#184099=CARTESIAN_POINT('Ctrl Pts',(10.0422085329999,12.2,-3.12180968700002));
#184100=CARTESIAN_POINT('Ctrl Pts',(10.0406335799999,12.2,-3.12097763100001));
#184101=CARTESIAN_POINT('Ctrl Pts',(10.0390644919999,12.2,-3.12015052400001));
#184102=CARTESIAN_POINT('Ctrl Pts',(10.0375012879999,12.2,-3.11932836300001));
#184103=CARTESIAN_POINT('Ctrl Pts',(10.0359439909999,12.2,-3.11851114600001));
#184104=CARTESIAN_POINT('Ctrl Pts',(10.0343926209999,12.2,-3.11769886700001));
#184105=CARTESIAN_POINT('Ctrl Pts',(10.0328471999999,12.2,-3.11689152500001));
#184106=CARTESIAN_POINT('Ctrl Pts',(10.0313077479999,12.2,-3.11608911700001));
#184107=CARTESIAN_POINT('Ctrl Pts',(10.0297742879999,12.2,-3.11529163800001));
#184108=CARTESIAN_POINT('Ctrl Pts',(10.0282468409999,12.2,-3.11449908600002));
#184109=CARTESIAN_POINT('Ctrl Pts',(10.0267254279999,12.2,-3.11371145700001));
#184110=CARTESIAN_POINT('Ctrl Pts',(10.0252100719999,12.2,-3.11292874700001));
#184111=CARTESIAN_POINT('Ctrl Pts',(10.0237007949999,12.2,-3.11215095500001));
#184112=CARTESIAN_POINT('Ctrl Pts',(10.0221976149999,12.2,-3.11137807500002));
#184113=CARTESIAN_POINT('Ctrl Pts',(10.0207005589999,12.2,-3.11061010400001));
#184114=CARTESIAN_POINT('Ctrl Pts',(10.0192096459999,12.2,-3.10984703900001));
#184115=CARTESIAN_POINT('Ctrl Pts',(10.0177248989999,12.2,-3.10908887700001));
#184116=CARTESIAN_POINT('Ctrl Pts',(10.0162463389999,12.2,-3.10833561400001));
#184117=CARTESIAN_POINT('Ctrl Pts',(10.0147739889999,12.2,-3.10758724500001));
#184118=CARTESIAN_POINT('Ctrl Pts',(10.0133078739999,12.2,-3.10684376900001));
#184119=CARTESIAN_POINT('Ctrl Pts',(10.0118480119999,12.2,-3.10610517900002));
#184120=CARTESIAN_POINT('Ctrl Pts',(10.0103944279999,12.2,-3.10537147600002));
#184121=CARTESIAN_POINT('Ctrl Pts',(10.0089471439999,12.2,-3.10464265200002));
#184122=CARTESIAN_POINT('Ctrl Pts',(10.0075061829999,12.2,-3.10391870500001));
#184123=CARTESIAN_POINT('Ctrl Pts',(10.0060715669999,12.2,-3.10319963200001));
#184124=CARTESIAN_POINT('Ctrl Pts',(10.0046433189999,12.2,-3.10248542800001));
#184125=CARTESIAN_POINT('Ctrl Pts',(10.0032214629999,12.2,-3.10177609000001));
#184126=CARTESIAN_POINT('Ctrl Pts',(10.0018060209999,12.2,-3.10107161300001));
#184127=CARTESIAN_POINT('Ctrl Pts',(10.0003970159999,12.2,-3.10037199500002));
#184128=CARTESIAN_POINT('Ctrl Pts',(9.99899447199994,12.2,-3.09967723100002));
#184129=CARTESIAN_POINT('Ctrl Pts',(9.99759841199995,12.2,-3.09898731700001));
#184130=CARTESIAN_POINT('Ctrl Pts',(9.99620885899994,12.2,-3.09830225000002));
#184131=CARTESIAN_POINT('Ctrl Pts',(9.99482583599995,12.2,-3.09762202400002));
#184132=CARTESIAN_POINT('Ctrl Pts',(9.99344936799995,12.2,-3.09694663700002));
#184133=CARTESIAN_POINT('Ctrl Pts',(9.99207947699994,12.2,-3.09627608500001));
#184134=CARTESIAN_POINT('Ctrl Pts',(9.99071618799995,12.2,-3.09561036200002));
#184135=CARTESIAN_POINT('Ctrl Pts',(9.98935952599994,12.2,-3.09494946600001));
#184136=CARTESIAN_POINT('Ctrl Pts',(9.98800951199994,12.2,-3.09429339200001));
#184137=CARTESIAN_POINT('Ctrl Pts',(9.98666617099994,12.2,-3.09364213600002));
#184138=CARTESIAN_POINT('Ctrl Pts',(9.98532952799994,12.2,-3.09299569400002));
#184139=CARTESIAN_POINT('Ctrl Pts',(9.98399960699994,12.2,-3.09235406000001));
#184140=CARTESIAN_POINT('Ctrl Pts',(9.98267643199994,12.2,-3.09171723300001));
#184141=CARTESIAN_POINT('Ctrl Pts',(9.98136002599994,12.2,-3.09108520600001));
#184142=CARTESIAN_POINT('Ctrl Pts',(9.98005041699994,12.2,-3.09045797700001));
#184143=CARTESIAN_POINT('Ctrl Pts',(9.97874762699994,12.2,-3.08983553900001));
#184144=CARTESIAN_POINT('Ctrl Pts',(9.97745168099994,12.2,-3.08921789100001));
#184145=CARTESIAN_POINT('Ctrl Pts',(9.97616260499995,12.2,-3.08860502500002));
#184146=CARTESIAN_POINT('Ctrl Pts',(9.97488042199994,12.2,-3.08799693900002));
#184147=CARTESIAN_POINT('Ctrl Pts',(9.97360515799994,12.2,-3.08739362900001));
#184148=CARTESIAN_POINT('Ctrl Pts',(9.97233683899994,12.2,-3.08679508900001));
#184149=CARTESIAN_POINT('Ctrl Pts',(9.97107548799995,12.2,-3.08620131400001));
#184150=CARTESIAN_POINT('Ctrl Pts',(9.96982113299994,12.2,-3.08561230000001));
#184151=CARTESIAN_POINT('Ctrl Pts',(9.96857379799994,12.2,-3.08502804400002));
#184152=CARTESIAN_POINT('Ctrl Pts',(9.96733350799994,12.2,-3.08444853900002));
#184153=CARTESIAN_POINT('Ctrl Pts',(9.96610028899994,12.2,-3.08387378200001));
#184154=CARTESIAN_POINT('Ctrl Pts',(9.96487416899994,12.2,-3.08330376800001));
#184155=CARTESIAN_POINT('Ctrl Pts',(9.96365516999995,12.2,-3.08273849300001));
#184156=CARTESIAN_POINT('Ctrl Pts',(9.96244331999995,12.2,-3.08217795000001));
#184157=CARTESIAN_POINT('Ctrl Pts',(9.96123864599994,12.2,-3.08162213600002));
#184158=CARTESIAN_POINT('Ctrl Pts',(9.96004117299995,12.2,-3.08107104600001));
#184159=CARTESIAN_POINT('Ctrl Pts',(9.95885092599995,12.2,-3.08052467500001));
#184160=CARTESIAN_POINT('Ctrl Pts',(9.95766793399994,12.2,-3.07998301700001));
#184161=CARTESIAN_POINT('Ctrl Pts',(9.95649222199994,12.2,-3.07944607000001));
#184162=CARTESIAN_POINT('Ctrl Pts',(9.95532381799995,12.2,-3.07891382600001));
#184163=CARTESIAN_POINT('Ctrl Pts',(9.95416274699994,12.2,-3.07838628200001));
#184164=CARTESIAN_POINT('Ctrl Pts',(9.95300903599994,12.2,-3.07786343200001));
#184165=CARTESIAN_POINT('Ctrl Pts',(9.95186271399995,12.2,-3.07734527000001));
#184166=CARTESIAN_POINT('Ctrl Pts',(9.95072380599994,12.2,-3.07683179400001));
#184167=CARTESIAN_POINT('Ctrl Pts',(9.94959233999994,12.2,-3.07632299600002));
#184168=CARTESIAN_POINT('Ctrl Pts',(9.94846834299994,12.2,-3.07581887100001));
#184169=CARTESIAN_POINT('Ctrl Pts',(9.94735184299994,12.2,-3.07531941600002));
#184170=CARTESIAN_POINT('Ctrl Pts',(9.94624286799995,12.2,-3.07482462300001));
#184171=CARTESIAN_POINT('Ctrl Pts',(9.94514144399995,12.2,-3.07433448900001));
#184172=CARTESIAN_POINT('Ctrl Pts',(9.94404760099994,12.2,-3.07384900800002));
#184173=CARTESIAN_POINT('Ctrl Pts',(9.94296136499995,12.2,-3.07336817300001));
#184174=CARTESIAN_POINT('Ctrl Pts',(9.94188276499995,12.2,-3.07289198100001));
#184175=CARTESIAN_POINT('Ctrl Pts',(9.94081182899994,12.2,-3.07242042600001));
#184176=CARTESIAN_POINT('Ctrl Pts',(9.93974858499995,12.2,-3.07195350200002));
#184177=CARTESIAN_POINT('Ctrl Pts',(9.93869306299995,12.2,-3.07149120200001));
#184178=CARTESIAN_POINT('Ctrl Pts',(9.93764528999994,12.2,-3.07103352400001));
#184179=CARTESIAN_POINT('Ctrl Pts',(9.93660529499994,12.2,-3.07058045900002));
#184180=CARTESIAN_POINT('Ctrl Pts',(9.93557310799994,12.2,-3.07013200400001));
#184181=CARTESIAN_POINT('Ctrl Pts',(9.93454875699994,12.2,-3.06968815200001));
#184182=CARTESIAN_POINT('Ctrl Pts',(9.93353226999995,12.2,-3.06924889800001));
#184183=CARTESIAN_POINT('Ctrl Pts',(9.93252367799995,12.2,-3.06881423400001));
#184184=CARTESIAN_POINT('Ctrl Pts',(9.93152301099995,12.2,-3.06838415800001));
#184185=CARTESIAN_POINT('Ctrl Pts',(9.93053029599994,12.2,-3.06795866100002));
#184186=CARTESIAN_POINT('Ctrl Pts',(9.92954556499994,12.2,-3.06753773800001));
#184187=CARTESIAN_POINT('Ctrl Pts',(9.92856884499994,12.2,-3.06712138300002));
#184188=CARTESIAN_POINT('Ctrl Pts',(9.92760016999994,12.2,-3.06670959200002));
#184189=CARTESIAN_POINT('Ctrl Pts',(9.92663956699994,12.2,-3.06630235600001));
#184190=CARTESIAN_POINT('Ctrl Pts',(9.92568706699995,12.2,-3.06589967100001));
#184191=CARTESIAN_POINT('Ctrl Pts',(9.92474269999994,12.2,-3.06550153000002));
#184192=CARTESIAN_POINT('Ctrl Pts',(9.92380649799994,12.2,-3.06510792800001));
#184193=CARTESIAN_POINT('Ctrl Pts',(9.92287849099995,12.2,-3.06471885700002));
#184194=CARTESIAN_POINT('Ctrl Pts',(9.92195870799994,12.2,-3.06433431200002));
#184195=CARTESIAN_POINT('Ctrl Pts',(9.92104718299995,12.2,-3.06395428600001));
#184196=CARTESIAN_POINT('Ctrl Pts',(9.92014394399994,12.2,-3.06357877400002));
#184197=CARTESIAN_POINT('Ctrl Pts',(9.91924902499994,12.2,-3.06320776900002));
#184198=CARTESIAN_POINT('Ctrl Pts',(9.91836245599995,12.2,-3.06284126300001));
#184199=CARTESIAN_POINT('Ctrl Pts',(9.91748426799995,12.2,-3.06247925400001));
#184200=CARTESIAN_POINT('Ctrl Pts',(9.91661449399994,12.2,-3.06212173000001));
#184201=CARTESIAN_POINT('Ctrl Pts',(9.91575316499994,12.2,-3.06176868700001));
#184202=CARTESIAN_POINT('Ctrl Pts',(9.91490522599995,12.2,-3.06142212700002));
#184203=CARTESIAN_POINT('Ctrl Pts',(9.91423456699994,12.2,-3.06114880300001));
#184204=CARTESIAN_POINT('Ctrl Pts',(9.91373655899995,12.2,-3.06094627500002));
#184205=CARTESIAN_POINT('Ctrl Pts',(9.91340782499995,12.2,-3.06081277600001));
#184206=CARTESIAN_POINT('Ctrl Pts',(9.91324626499994,12.2,-3.06074721200002));
#184207=CARTESIAN_POINT('Ctrl Pts',(9.91324626499994,15.2,-3.06074721200002));
#184208=CARTESIAN_POINT('Ctrl Pts',(9.91340782499995,15.2,-3.06081277600001));
#184209=CARTESIAN_POINT('Ctrl Pts',(9.91373655899995,15.2,-3.06094627500002));
#184210=CARTESIAN_POINT('Ctrl Pts',(9.91423456699994,15.2,-3.06114880300001));
#184211=CARTESIAN_POINT('Ctrl Pts',(9.91490522599995,15.2,-3.06142212700002));
#184212=CARTESIAN_POINT('Ctrl Pts',(9.91575316499994,15.2,-3.06176868700001));
#184213=CARTESIAN_POINT('Ctrl Pts',(9.91661449399994,15.2,-3.06212173000001));
#184214=CARTESIAN_POINT('Ctrl Pts',(9.91748426799995,15.2,-3.06247925400001));
#184215=CARTESIAN_POINT('Ctrl Pts',(9.91836245599995,15.2,-3.06284126300001));
#184216=CARTESIAN_POINT('Ctrl Pts',(9.91924902499994,15.2,-3.06320776900002));
#184217=CARTESIAN_POINT('Ctrl Pts',(9.92014394399994,15.2,-3.06357877400002));
#184218=CARTESIAN_POINT('Ctrl Pts',(9.92104718299995,15.2,-3.06395428600001));
#184219=CARTESIAN_POINT('Ctrl Pts',(9.92195870799994,15.2,-3.06433431200002));
#184220=CARTESIAN_POINT('Ctrl Pts',(9.92287849099995,15.2,-3.06471885700002));
#184221=CARTESIAN_POINT('Ctrl Pts',(9.92380649799994,15.2,-3.06510792800001));
#184222=CARTESIAN_POINT('Ctrl Pts',(9.92474269999994,15.2,-3.06550153000002));
#184223=CARTESIAN_POINT('Ctrl Pts',(9.92568706699995,15.2,-3.06589967100001));
#184224=CARTESIAN_POINT('Ctrl Pts',(9.92663956699994,15.2,-3.06630235600001));
#184225=CARTESIAN_POINT('Ctrl Pts',(9.92760016999994,15.2,-3.06670959200002));
#184226=CARTESIAN_POINT('Ctrl Pts',(9.92856884499994,15.2,-3.06712138300002));
#184227=CARTESIAN_POINT('Ctrl Pts',(9.92954556499994,15.2,-3.06753773800001));
#184228=CARTESIAN_POINT('Ctrl Pts',(9.93053029599994,15.2,-3.06795866100002));
#184229=CARTESIAN_POINT('Ctrl Pts',(9.93152301099995,15.2,-3.06838415800001));
#184230=CARTESIAN_POINT('Ctrl Pts',(9.93252367799995,15.2,-3.06881423400001));
#184231=CARTESIAN_POINT('Ctrl Pts',(9.93353226999995,15.2,-3.06924889800001));
#184232=CARTESIAN_POINT('Ctrl Pts',(9.93454875699994,15.2,-3.06968815200001));
#184233=CARTESIAN_POINT('Ctrl Pts',(9.93557310799994,15.2,-3.07013200400001));
#184234=CARTESIAN_POINT('Ctrl Pts',(9.93660529499994,15.2,-3.07058045900002));
#184235=CARTESIAN_POINT('Ctrl Pts',(9.93764528999994,15.2,-3.07103352400001));
#184236=CARTESIAN_POINT('Ctrl Pts',(9.93869306299995,15.2,-3.07149120200001));
#184237=CARTESIAN_POINT('Ctrl Pts',(9.93974858499995,15.2,-3.07195350200002));
#184238=CARTESIAN_POINT('Ctrl Pts',(9.94081182899994,15.2,-3.07242042600001));
#184239=CARTESIAN_POINT('Ctrl Pts',(9.94188276499995,15.2,-3.07289198100001));
#184240=CARTESIAN_POINT('Ctrl Pts',(9.94296136499995,15.2,-3.07336817300001));
#184241=CARTESIAN_POINT('Ctrl Pts',(9.94404760099994,15.2,-3.07384900800002));
#184242=CARTESIAN_POINT('Ctrl Pts',(9.94514144399995,15.2,-3.07433448900001));
#184243=CARTESIAN_POINT('Ctrl Pts',(9.94624286799995,15.2,-3.07482462300001));
#184244=CARTESIAN_POINT('Ctrl Pts',(9.94735184299994,15.2,-3.07531941600002));
#184245=CARTESIAN_POINT('Ctrl Pts',(9.94846834299994,15.2,-3.07581887100001));
#184246=CARTESIAN_POINT('Ctrl Pts',(9.94959233999994,15.2,-3.07632299600002));
#184247=CARTESIAN_POINT('Ctrl Pts',(9.95072380599994,15.2,-3.07683179400001));
#184248=CARTESIAN_POINT('Ctrl Pts',(9.95186271399995,15.2,-3.07734527000001));
#184249=CARTESIAN_POINT('Ctrl Pts',(9.95300903599994,15.2,-3.07786343200001));
#184250=CARTESIAN_POINT('Ctrl Pts',(9.95416274699994,15.2,-3.07838628200001));
#184251=CARTESIAN_POINT('Ctrl Pts',(9.95532381799995,15.2,-3.07891382600001));
#184252=CARTESIAN_POINT('Ctrl Pts',(9.95649222199994,15.2,-3.07944607000001));
#184253=CARTESIAN_POINT('Ctrl Pts',(9.95766793399994,15.2,-3.07998301700001));
#184254=CARTESIAN_POINT('Ctrl Pts',(9.95885092599995,15.2,-3.08052467500001));
#184255=CARTESIAN_POINT('Ctrl Pts',(9.96004117299995,15.2,-3.08107104600001));
#184256=CARTESIAN_POINT('Ctrl Pts',(9.96123864599994,15.2,-3.08162213600002));
#184257=CARTESIAN_POINT('Ctrl Pts',(9.96244331999995,15.2,-3.08217795000001));
#184258=CARTESIAN_POINT('Ctrl Pts',(9.96365516999995,15.2,-3.08273849300001));
#184259=CARTESIAN_POINT('Ctrl Pts',(9.96487416899994,15.2,-3.08330376800001));
#184260=CARTESIAN_POINT('Ctrl Pts',(9.96610028899994,15.2,-3.08387378200001));
#184261=CARTESIAN_POINT('Ctrl Pts',(9.96733350799994,15.2,-3.08444853900002));
#184262=CARTESIAN_POINT('Ctrl Pts',(9.96857379799994,15.2,-3.08502804400002));
#184263=CARTESIAN_POINT('Ctrl Pts',(9.96982113299994,15.2,-3.08561230000001));
#184264=CARTESIAN_POINT('Ctrl Pts',(9.97107548799995,15.2,-3.08620131400001));
#184265=CARTESIAN_POINT('Ctrl Pts',(9.97233683899994,15.2,-3.08679508900001));
#184266=CARTESIAN_POINT('Ctrl Pts',(9.97360515799994,15.2,-3.08739362900001));
#184267=CARTESIAN_POINT('Ctrl Pts',(9.97488042199994,15.2,-3.08799693900002));
#184268=CARTESIAN_POINT('Ctrl Pts',(9.97616260499995,15.2,-3.08860502500002));
#184269=CARTESIAN_POINT('Ctrl Pts',(9.97745168099994,15.2,-3.08921789100001));
#184270=CARTESIAN_POINT('Ctrl Pts',(9.97874762699994,15.2,-3.08983553900001));
#184271=CARTESIAN_POINT('Ctrl Pts',(9.98005041699994,15.2,-3.09045797700001));
#184272=CARTESIAN_POINT('Ctrl Pts',(9.98136002599994,15.2,-3.09108520600001));
#184273=CARTESIAN_POINT('Ctrl Pts',(9.98267643199994,15.2,-3.09171723300001));
#184274=CARTESIAN_POINT('Ctrl Pts',(9.98399960699994,15.2,-3.09235406000001));
#184275=CARTESIAN_POINT('Ctrl Pts',(9.98532952799994,15.2,-3.09299569400002));
#184276=CARTESIAN_POINT('Ctrl Pts',(9.98666617099994,15.2,-3.09364213600002));
#184277=CARTESIAN_POINT('Ctrl Pts',(9.98800951199994,15.2,-3.09429339200001));
#184278=CARTESIAN_POINT('Ctrl Pts',(9.98935952599994,15.2,-3.09494946600001));
#184279=CARTESIAN_POINT('Ctrl Pts',(9.99071618799995,15.2,-3.09561036200002));
#184280=CARTESIAN_POINT('Ctrl Pts',(9.99207947699994,15.2,-3.09627608500001));
#184281=CARTESIAN_POINT('Ctrl Pts',(9.99344936799995,15.2,-3.09694663700002));
#184282=CARTESIAN_POINT('Ctrl Pts',(9.99482583599995,15.2,-3.09762202400002));
#184283=CARTESIAN_POINT('Ctrl Pts',(9.99620885899994,15.2,-3.09830225000002));
#184284=CARTESIAN_POINT('Ctrl Pts',(9.99759841199995,15.2,-3.09898731700001));
#184285=CARTESIAN_POINT('Ctrl Pts',(9.99899447199994,15.2,-3.09967723100002));
#184286=CARTESIAN_POINT('Ctrl Pts',(10.0003970159999,15.2,-3.10037199500002));
#184287=CARTESIAN_POINT('Ctrl Pts',(10.0018060209999,15.2,-3.10107161300001));
#184288=CARTESIAN_POINT('Ctrl Pts',(10.0032214629999,15.2,-3.10177609000001));
#184289=CARTESIAN_POINT('Ctrl Pts',(10.0046433189999,15.2,-3.10248542800001));
#184290=CARTESIAN_POINT('Ctrl Pts',(10.0060715669999,15.2,-3.10319963200001));
#184291=CARTESIAN_POINT('Ctrl Pts',(10.0075061829999,15.2,-3.10391870500001));
#184292=CARTESIAN_POINT('Ctrl Pts',(10.0089471439999,15.2,-3.10464265200002));
#184293=CARTESIAN_POINT('Ctrl Pts',(10.0103944279999,15.2,-3.10537147600002));
#184294=CARTESIAN_POINT('Ctrl Pts',(10.0118480119999,15.2,-3.10610517900002));
#184295=CARTESIAN_POINT('Ctrl Pts',(10.0133078739999,15.2,-3.10684376900001));
#184296=CARTESIAN_POINT('Ctrl Pts',(10.0147739889999,15.2,-3.10758724500001));
#184297=CARTESIAN_POINT('Ctrl Pts',(10.0162463389999,15.2,-3.10833561400001));
#184298=CARTESIAN_POINT('Ctrl Pts',(10.0177248989999,15.2,-3.10908887700001));
#184299=CARTESIAN_POINT('Ctrl Pts',(10.0192096459999,15.2,-3.10984703900001));
#184300=CARTESIAN_POINT('Ctrl Pts',(10.0207005589999,15.2,-3.11061010400001));
#184301=CARTESIAN_POINT('Ctrl Pts',(10.0221976149999,15.2,-3.11137807500002));
#184302=CARTESIAN_POINT('Ctrl Pts',(10.0237007949999,15.2,-3.11215095500001));
#184303=CARTESIAN_POINT('Ctrl Pts',(10.0252100719999,15.2,-3.11292874700001));
#184304=CARTESIAN_POINT('Ctrl Pts',(10.0267254279999,15.2,-3.11371145700001));
#184305=CARTESIAN_POINT('Ctrl Pts',(10.0282468409999,15.2,-3.11449908600002));
#184306=CARTESIAN_POINT('Ctrl Pts',(10.0297742879999,15.2,-3.11529163800001));
#184307=CARTESIAN_POINT('Ctrl Pts',(10.0313077479999,15.2,-3.11608911700001));
#184308=CARTESIAN_POINT('Ctrl Pts',(10.0328471999999,15.2,-3.11689152500001));
#184309=CARTESIAN_POINT('Ctrl Pts',(10.0343926209999,15.2,-3.11769886700001));
#184310=CARTESIAN_POINT('Ctrl Pts',(10.0359439909999,15.2,-3.11851114600001));
#184311=CARTESIAN_POINT('Ctrl Pts',(10.0375012879999,15.2,-3.11932836300001));
#184312=CARTESIAN_POINT('Ctrl Pts',(10.0390644919999,15.2,-3.12015052400001));
#184313=CARTESIAN_POINT('Ctrl Pts',(10.0406335799999,15.2,-3.12097763100001));
#184314=CARTESIAN_POINT('Ctrl Pts',(10.0422085329999,15.2,-3.12180968700002));
#184315=CARTESIAN_POINT('Ctrl Pts',(10.0437893269999,15.2,-3.12264669700001));
#184316=CARTESIAN_POINT('Ctrl Pts',(10.0453759449999,15.2,-3.12348866100002));
#184317=CARTESIAN_POINT('Ctrl Pts',(10.0469683629999,15.2,-3.12433558500001));
#184318=CARTESIAN_POINT('Ctrl Pts',(10.0485665629999,15.2,-3.12518747000002));
#184319=CARTESIAN_POINT('Ctrl Pts',(10.0501705219999,15.2,-3.12604432200001));
#184320=CARTESIAN_POINT('Ctrl Pts',(10.0517802179999,15.2,-3.12690614000001));
#184321=CARTESIAN_POINT('Ctrl Pts',(10.0533956349999,15.2,-3.12777293000002));
#184322=CARTESIAN_POINT('Ctrl Pts',(10.0550167499999,15.2,-3.12864469400001));
#184323=CARTESIAN_POINT('Ctrl Pts',(10.0566435409999,15.2,-3.12952143500001));
#184324=CARTESIAN_POINT('Ctrl Pts',(10.0582759909999,15.2,-3.13040315700002));
#184325=CARTESIAN_POINT('Ctrl Pts',(10.0599140779999,15.2,-3.13128986000001));
#184326=CARTESIAN_POINT('Ctrl Pts',(10.0615577799999,15.2,-3.13218155100001));
#184327=CARTESIAN_POINT('Ctrl Pts',(10.0632070809999,15.2,-3.13307822900001));
#184328=CARTESIAN_POINT('Ctrl Pts',(10.0648619579999,15.2,-3.13397990000002));
#184329=CARTESIAN_POINT('Ctrl Pts',(10.0665223919999,15.2,-3.13488656500001));
#184330=CARTESIAN_POINT('Ctrl Pts',(10.0681883619999,15.2,-3.13579822800001));
#184331=CARTESIAN_POINT('Ctrl Pts',(10.0698598489999,15.2,-3.13671489000001));
#184332=CARTESIAN_POINT('Ctrl Pts',(10.0715368339999,15.2,-3.13763655600001));
#184333=CARTESIAN_POINT('Ctrl Pts',(10.0732192959999,15.2,-3.13856322800001));
#184334=CARTESIAN_POINT('Ctrl Pts',(10.0749072159999,15.2,-3.13949490700002));
#184335=CARTESIAN_POINT('Ctrl Pts',(10.0766005729999,15.2,-3.14043159900002));
#184336=CARTESIAN_POINT('Ctrl Pts',(10.0782993499999,15.2,-3.14137330300001));
#184337=CARTESIAN_POINT('Ctrl Pts',(10.0800035259999,15.2,-3.14232002500002));
#184338=CARTESIAN_POINT('Ctrl Pts',(10.0817130829999,15.2,-3.14327176500001));
#184339=CARTESIAN_POINT('Ctrl Pts',(10.0834279989999,15.2,-3.14422852800002));
#184340=CARTESIAN_POINT('Ctrl Pts',(10.0851482559999,15.2,-3.14519031400001));
#184341=CARTESIAN_POINT('Ctrl Pts',(10.0868738369999,15.2,-3.14615712900002));
#184342=CARTESIAN_POINT('Ctrl Pts',(10.0886047199999,15.2,-3.14712897300002));
#184343=CARTESIAN_POINT('Ctrl Pts',(10.0903408869999,15.2,-3.14810584800002));
#184344=CARTESIAN_POINT('Ctrl Pts',(10.0920823179999,15.2,-3.14908775800002));
#184345=CARTESIAN_POINT('Ctrl Pts',(10.0938289959999,15.2,-3.15007470700001));
#184346=CARTESIAN_POINT('Ctrl Pts',(10.0955808999999,15.2,-3.15106669300001));
#184347=CARTESIAN_POINT('Ctrl Pts',(10.0973380129999,15.2,-3.15206372300001));
#184348=CARTESIAN_POINT('Ctrl Pts',(10.0991003149999,15.2,-3.15306579700001));
#184349=CARTESIAN_POINT('Ctrl Pts',(10.1008677879999,15.2,-3.15407291900001));
#184350=CARTESIAN_POINT('Ctrl Pts',(10.1026404129999,15.2,-3.15508509000002));
#184351=CARTESIAN_POINT('Ctrl Pts',(10.1044181719999,15.2,-3.15610231100001));
#184352=CARTESIAN_POINT('Ctrl Pts',(10.1062010459999,15.2,-3.15712458800002));
#184353=CARTESIAN_POINT('Ctrl Pts',(10.1079890159999,15.2,-3.15815192100001));
#184354=CARTESIAN_POINT('Ctrl Pts',(10.1097820639999,15.2,-3.15918431300001));
#184355=CARTESIAN_POINT('Ctrl Pts',(10.1115801729999,15.2,-3.16022176700002));
#184356=CARTESIAN_POINT('Ctrl Pts',(10.1133833219999,15.2,-3.16126428300001));
#184357=CARTESIAN_POINT('Ctrl Pts',(10.1151914959999,15.2,-3.16231186600001));
#184358=CARTESIAN_POINT('Ctrl Pts',(10.1170046749999,15.2,-3.16336451600002));
#184359=CARTESIAN_POINT('Ctrl Pts',(10.1188228389999,15.2,-3.16442223800002));
#184360=CARTESIAN_POINT('Ctrl Pts',(10.1206459739999,15.2,-3.16548503000002));
#184361=CARTESIAN_POINT('Ctrl Pts',(10.1224740599999,15.2,-3.16655289800002));
#184362=CARTESIAN_POINT('Ctrl Pts',(10.1243070779999,15.2,-3.16762584300001));
#184363=CARTESIAN_POINT('Ctrl Pts',(10.1261450119999,15.2,-3.16870386600002));
#184364=CARTESIAN_POINT('Ctrl Pts',(10.1279878419999,15.2,-3.16978697100001));
#184365=CARTESIAN_POINT('Ctrl Pts',(10.1298355529999,15.2,-3.17087516000001));
#184366=CARTESIAN_POINT('Ctrl Pts',(10.1316881249999,15.2,-3.17196843300001));
#184367=CARTESIAN_POINT('Ctrl Pts',(10.1335455409999,15.2,-3.17306679400001));
#184368=CARTESIAN_POINT('Ctrl Pts',(10.1354077839999,15.2,-3.17417024400001));
#184369=CARTESIAN_POINT('Ctrl Pts',(10.1372748349999,15.2,-3.17527878600002));
#184370=CARTESIAN_POINT('Ctrl Pts',(10.1391466789999,15.2,-3.17639242200002));
#184371=CARTESIAN_POINT('Ctrl Pts',(10.1410232959999,15.2,-3.17751115200001));
#184372=CARTESIAN_POINT('Ctrl Pts',(10.1429046699999,15.2,-3.17863498200001));
#184373=CARTESIAN_POINT('Ctrl Pts',(10.1447907829999,15.2,-3.17976391000002));
#184374=CARTESIAN_POINT('Ctrl Pts',(10.1466816179999,15.2,-3.18089793900001));
#184375=CARTESIAN_POINT('Ctrl Pts',(10.1485771589999,15.2,-3.18203707400002));
#184376=CARTESIAN_POINT('Ctrl Pts',(10.1504773859999,15.2,-3.18318131200002));
#184377=CARTESIAN_POINT('Ctrl Pts',(10.1523822839999,15.2,-3.18433065800001));
#184378=CARTESIAN_POINT('Ctrl Pts',(10.1542918349999,15.2,-3.18548511300001));
#184379=CARTESIAN_POINT('Ctrl Pts',(10.1562060229999,15.2,-3.18664468000001));
#184380=CARTESIAN_POINT('Ctrl Pts',(10.1581248299999,15.2,-3.18780935900001));
#184381=CARTESIAN_POINT('Ctrl Pts',(10.1600482389999,15.2,-3.18897915400001));
#184382=CARTESIAN_POINT('Ctrl Pts',(10.1619762339999,15.2,-3.19015406500001));
#184383=CARTESIAN_POINT('Ctrl Pts',(10.1639087969999,15.2,-3.19133409300001));
#184384=CARTESIAN_POINT('Ctrl Pts',(10.1658459129999,15.2,-3.19251924300001));
#184385=CARTESIAN_POINT('Ctrl Pts',(10.1677875629999,15.2,-3.19370951400002));
#184386=CARTESIAN_POINT('Ctrl Pts',(10.1697337309999,15.2,-3.19490490900002));
#184387=CARTESIAN_POINT('Ctrl Pts',(10.1716844029999,15.2,-3.19610542900001));
#184388=CARTESIAN_POINT('Ctrl Pts',(10.1736395589999,15.2,-3.19731107700001));
#184389=CARTESIAN_POINT('Ctrl Pts',(10.1755991829999,15.2,-3.19852185400002));
#184390=CARTESIAN_POINT('Ctrl Pts',(10.1775632609999,15.2,-3.19973776100001));
#184391=CARTESIAN_POINT('Ctrl Pts',(10.1795317729999,15.2,-3.20095880100002));
#184392=CARTESIAN_POINT('Ctrl Pts',(10.1815047049999,15.2,-3.20218497500001));
#184393=CARTESIAN_POINT('Ctrl Pts',(10.1834820399999,15.2,-3.20341628300001));
#184394=CARTESIAN_POINT('Ctrl Pts',(10.1854637609999,15.2,-3.20465272900002));
#184395=CARTESIAN_POINT('Ctrl Pts',(10.1874498539999,15.2,-3.20589431400002));
#184396=CARTESIAN_POINT('Ctrl Pts',(10.1894402999999,15.2,-3.20714104000002));
#184397=CARTESIAN_POINT('Ctrl Pts',(10.1914350849999,15.2,-3.20839290800001));
#184398=CARTESIAN_POINT('Ctrl Pts',(10.1934341909999,15.2,-3.20964991800002));
#184399=CARTESIAN_POINT('Ctrl Pts',(10.1954376039999,15.2,-3.21091207400002));
#184400=CARTESIAN_POINT('Ctrl Pts',(10.1974453069999,15.2,-3.21217937700002));
#184401=CARTESIAN_POINT('Ctrl Pts',(10.1994572829999,15.2,-3.21345182800002));
#184402=CARTESIAN_POINT('Ctrl Pts',(10.2014735169999,15.2,-3.21472942900002));
#184403=CARTESIAN_POINT('Ctrl Pts',(10.2034939929999,15.2,-3.21601218000001));
#184404=CARTESIAN_POINT('Ctrl Pts',(10.2055186959999,15.2,-3.21730008500001));
#184405=CARTESIAN_POINT('Ctrl Pts',(10.2075476089999,15.2,-3.21859314200001));
#184406=CARTESIAN_POINT('Ctrl Pts',(10.2095807169999,15.2,-3.21989135600001));
#184407=CARTESIAN_POINT('Ctrl Pts',(10.2116180039999,15.2,-3.22119472700001));
#184408=CARTESIAN_POINT('Ctrl Pts',(10.2136594529999,15.2,-3.22250325600002));
#184409=CARTESIAN_POINT('Ctrl Pts',(10.2157050509999,15.2,-3.22381694500002));
#184410=CARTESIAN_POINT('Ctrl Pts',(10.2177547809999,15.2,-3.22513579400002));
#184411=CARTESIAN_POINT('Ctrl Pts',(10.2198086269999,15.2,-3.22645980700001));
#184412=CARTESIAN_POINT('Ctrl Pts',(10.2218665749999,15.2,-3.22778898400002));
#184413=CARTESIAN_POINT('Ctrl Pts',(10.2239286079999,15.2,-3.22912332500001));
#184414=CARTESIAN_POINT('Ctrl Pts',(10.2259947109999,15.2,-3.23046283300001));
#184415=CARTESIAN_POINT('Ctrl Pts',(10.2280648689999,15.2,-3.23180750800002));
#184416=CARTESIAN_POINT('Ctrl Pts',(10.2301390659999,15.2,-3.23315735300001));
#184417=CARTESIAN_POINT('Ctrl Pts',(10.2322172889999,15.2,-3.23451236800001));
#184418=CARTESIAN_POINT('Ctrl Pts',(10.2342995189999,15.2,-3.23587255500001));
#184419=CARTESIAN_POINT('Ctrl Pts',(10.2363857439999,15.2,-3.23723791500001));
#184420=CARTESIAN_POINT('Ctrl Pts',(10.2384759469999,15.2,-3.23860844800001));
#184421=CARTESIAN_POINT('Ctrl Pts',(10.2405701139999,15.2,-3.23998415800002));
#184422=CARTESIAN_POINT('Ctrl Pts',(10.2426682289999,15.2,-3.24136504400002));
#184423=CARTESIAN_POINT('Ctrl Pts',(10.2447702779999,15.2,-3.24275110800002));
#184424=CARTESIAN_POINT('Ctrl Pts',(10.2468762449999,15.2,-3.24414235000001));
#184425=CARTESIAN_POINT('Ctrl Pts',(10.2489861149999,15.2,-3.24553877200001));
#184426=CARTESIAN_POINT('Ctrl Pts',(10.2510998739999,15.2,-3.24694037600001));
#184427=CARTESIAN_POINT('Ctrl Pts',(10.2532175069999,15.2,-3.24834716200002));
#184428=CARTESIAN_POINT('Ctrl Pts',(10.2553389979999,15.2,-3.24975913200001));
#184429=CARTESIAN_POINT('Ctrl Pts',(10.2574643339999,15.2,-3.25117628600001));
#184430=CARTESIAN_POINT('Ctrl Pts',(10.2595934979999,15.2,-3.25259862700001));
#184431=CARTESIAN_POINT('Ctrl Pts',(10.2617264769999,15.2,-3.25402615300002));
#184432=CARTESIAN_POINT('Ctrl Pts',(10.2638632559999,15.2,-3.25545886800001));
#184433=CARTESIAN_POINT('Ctrl Pts',(10.2660038209999,15.2,-3.25689677200002));
#184434=CARTESIAN_POINT('Ctrl Pts',(10.2681481549999,15.2,-3.25833986600002));
#184435=CARTESIAN_POINT('Ctrl Pts',(10.2702962469999,15.2,-3.25978815000001));
#184436=CARTESIAN_POINT('Ctrl Pts',(10.2724480789999,15.2,-3.26124162800001));
#184437=CARTESIAN_POINT('Ctrl Pts',(10.2746036379999,15.2,-3.26270029800002));
#184438=CARTESIAN_POINT('Ctrl Pts',(10.2767629099999,15.2,-3.26416416200002));
#184439=CARTESIAN_POINT('Ctrl Pts',(10.2789258799999,15.2,-3.26563322100001));
#184440=CARTESIAN_POINT('Ctrl Pts',(10.2810925339999,15.2,-3.26710747600002));
#184441=CARTESIAN_POINT('Ctrl Pts',(10.2832628569999,15.2,-3.26858692800001));
#184442=CARTESIAN_POINT('Ctrl Pts',(10.2854368349999,15.2,-3.27007157800002));
#184443=CARTESIAN_POINT('Ctrl Pts',(10.2876144549999,15.2,-3.27156142700002));
#184444=CARTESIAN_POINT('Ctrl Pts',(10.2897957009999,15.2,-3.27305647500001));
#184445=CARTESIAN_POINT('Ctrl Pts',(10.2919805579999,15.2,-3.27455672400002));
#184446=CARTESIAN_POINT('Ctrl Pts',(10.2941690149999,15.2,-3.27606217500001));
#184447=CARTESIAN_POINT('Ctrl Pts',(10.2963610559999,15.2,-3.27757282800002));
#184448=CARTESIAN_POINT('Ctrl Pts',(10.2985566669999,15.2,-3.27908868400002));
#184449=CARTESIAN_POINT('Ctrl Pts',(10.3007558329999,15.2,-3.28060974400001));
#184450=CARTESIAN_POINT('Ctrl Pts',(10.3029585419999,15.2,-3.28213601000002));
#184451=CARTESIAN_POINT('Ctrl Pts',(10.3051647789999,15.2,-3.28366748100001));
#184452=CARTESIAN_POINT('Ctrl Pts',(10.3073745299999,15.2,-3.28520415900002));
#184453=CARTESIAN_POINT('Ctrl Pts',(10.3095877799999,15.2,-3.28674604500002));
#184454=CARTESIAN_POINT('Ctrl Pts',(10.3118045179999,15.2,-3.28829313800002));
#184455=CARTESIAN_POINT('Ctrl Pts',(10.3140247269999,15.2,-3.28984544000001));
#184456=CARTESIAN_POINT('Ctrl Pts',(10.3162483959999,15.2,-3.29140295300002));
#184457=CARTESIAN_POINT('Ctrl Pts',(10.3184755079999,15.2,-3.29296567500001));
#184458=CARTESIAN_POINT('Ctrl Pts',(10.3207060529999,15.2,-3.29453360900001));
#184459=CARTESIAN_POINT('Ctrl Pts',(10.3229400139999,15.2,-3.29610675500001));
#184460=CARTESIAN_POINT('Ctrl Pts',(10.3251773799999,15.2,-3.29768511400002));
#184461=CARTESIAN_POINT('Ctrl Pts',(10.3274181339999,15.2,-3.29926868600001));
#184462=CARTESIAN_POINT('Ctrl Pts',(10.3296622669999,15.2,-3.30085747200001));
#184463=CARTESIAN_POINT('Ctrl Pts',(10.3319097619999,15.2,-3.30245147300001));
#184464=CARTESIAN_POINT('Ctrl Pts',(10.3341606059999,15.2,-3.30405069000001));
#184465=CARTESIAN_POINT('Ctrl Pts',(10.3364147869999,15.2,-3.30565512200002));
#184466=CARTESIAN_POINT('Ctrl Pts',(10.3386722889999,15.2,-3.30726477100002));
#184467=CARTESIAN_POINT('Ctrl Pts',(10.3409331009999,15.2,-3.30887963800001));
#184468=CARTESIAN_POINT('Ctrl Pts',(10.3431972079999,15.2,-3.31049972300002));
#184469=CARTESIAN_POINT('Ctrl Pts',(10.3454645979999,15.2,-3.31212502700001));
#184470=CARTESIAN_POINT('Ctrl Pts',(10.3477352559999,15.2,-3.31375555000001));
#184471=CARTESIAN_POINT('Ctrl Pts',(10.3500091699999,15.2,-3.31539129200001));
#184472=CARTESIAN_POINT('Ctrl Pts',(10.3522863269999,15.2,-3.31703225500001));
#184473=CARTESIAN_POINT('Ctrl Pts',(10.3545667119999,15.2,-3.31867843900001));
#184474=CARTESIAN_POINT('Ctrl Pts',(10.3568503129999,15.2,-3.32032984500001));
#184475=CARTESIAN_POINT('Ctrl Pts',(10.3591371169999,15.2,-3.32198647300002));
#184476=CARTESIAN_POINT('Ctrl Pts',(10.3614271109999,15.2,-3.32364832300001));
#184477=CARTESIAN_POINT('Ctrl Pts',(10.3637202799999,15.2,-3.32531539600001));
#184478=CARTESIAN_POINT('Ctrl Pts',(10.3660166129999,15.2,-3.32698769300002));
#184479=CARTESIAN_POINT('Ctrl Pts',(10.3683160969999,15.2,-3.32866521600002));
#184480=CARTESIAN_POINT('Ctrl Pts',(10.3706187169999,15.2,-3.33034796100002));
#184481=CARTESIAN_POINT('Ctrl Pts',(10.3729244619999,15.2,-3.33203593300002));
#184482=CARTESIAN_POINT('Ctrl Pts',(10.3752333189999,15.2,-3.33372913000002));
#184483=CARTESIAN_POINT('Ctrl Pts',(10.3775452729999,15.2,-3.33542755200002));
#184484=CARTESIAN_POINT('Ctrl Pts',(10.3798603139999,15.2,-3.33713120100001));
#184485=CARTESIAN_POINT('Ctrl Pts',(10.3821784259999,15.2,-3.33884007800001));
#184486=CARTESIAN_POINT('Ctrl Pts',(10.3844995979999,15.2,-3.34055418200002));
#184487=CARTESIAN_POINT('Ctrl Pts',(10.3868238179999,15.2,-3.34227351400001));
#184488=CARTESIAN_POINT('Ctrl Pts',(10.3891510709999,15.2,-3.34399807300001));
#184489=CARTESIAN_POINT('Ctrl Pts',(10.3914813469999,15.2,-3.34572786200001));
#184490=CARTESIAN_POINT('Ctrl Pts',(10.3938146309999,15.2,-3.34746287900002));
#184491=CARTESIAN_POINT('Ctrl Pts',(10.3961509099999,15.2,-3.34920312600001));
#184492=CARTESIAN_POINT('Ctrl Pts',(10.3984901739999,15.2,-3.35094860300002));
#184493=CARTESIAN_POINT('Ctrl Pts',(10.4008324069999,15.2,-3.35269930900001));
#184494=CARTESIAN_POINT('Ctrl Pts',(10.4031775999999,15.2,-3.35445524600001));
#184495=CARTESIAN_POINT('Ctrl Pts',(10.4055257379999,15.2,-3.35621641400001));
#184496=CARTESIAN_POINT('Ctrl Pts',(10.4078768069999,15.2,-3.35798281300002));
#184497=CARTESIAN_POINT('Ctrl Pts',(10.4102307989999,15.2,-3.35975444400002));
#184498=CARTESIAN_POINT('Ctrl Pts',(10.4125876979999,15.2,-3.36153130600001));
#184499=CARTESIAN_POINT('Ctrl Pts',(10.4149474929999,15.2,-3.36331340000001));
#184500=CARTESIAN_POINT('Ctrl Pts',(10.4173101699999,15.2,-3.36510072600001));
#184501=CARTESIAN_POINT('Ctrl Pts',(10.4196757189999,15.2,-3.36689328500002));
#184502=CARTESIAN_POINT('Ctrl Pts',(10.4220441259999,15.2,-3.36869107600001));
#184503=CARTESIAN_POINT('Ctrl Pts',(10.4244153789999,15.2,-3.37049410100001));
#184504=CARTESIAN_POINT('Ctrl Pts',(10.4267894639999,15.2,-3.37230235900002));
#184505=CARTESIAN_POINT('Ctrl Pts',(10.4291663729999,15.2,-3.37411585000002));
#184506=CARTESIAN_POINT('Ctrl Pts',(10.4315460899999,15.2,-3.37593457500001));
#184507=CARTESIAN_POINT('Ctrl Pts',(10.4339286029999,15.2,-3.37775853500001));
#184508=CARTESIAN_POINT('Ctrl Pts',(10.4363139019999,15.2,-3.37958772900001));
#184509=CARTESIAN_POINT('Ctrl Pts',(10.4387019739999,15.2,-3.38142215600001));
#184510=CARTESIAN_POINT('Ctrl Pts',(10.4410928049999,15.2,-3.38326181800001));
#184511=CARTESIAN_POINT('Ctrl Pts',(10.4434863849999,15.2,-3.38510671600002));
#184512=CARTESIAN_POINT('Ctrl Pts',(10.4458826999999,15.2,-3.38695684700001));
#184513=CARTESIAN_POINT('Ctrl Pts',(10.4482817399999,15.2,-3.38881221500001));
#184514=CARTESIAN_POINT('Ctrl Pts',(10.4506834919999,15.2,-3.39067281600002));
#184515=CARTESIAN_POINT('Ctrl Pts',(10.4530879439999,15.2,-3.39253865400002));
#184516=CARTESIAN_POINT('Ctrl Pts',(10.4554950839999,15.2,-3.39440972700002));
#184517=CARTESIAN_POINT('Ctrl Pts',(10.4579048999999,15.2,-3.39628603500001));
#184518=CARTESIAN_POINT('Ctrl Pts',(10.4603173799999,15.2,-3.39816757900001));
#184519=CARTESIAN_POINT('Ctrl Pts',(10.4627325119999,15.2,-3.40005435900002));
#184520=CARTESIAN_POINT('Ctrl Pts',(10.4651502849999,15.2,-3.40194637400002));
#184521=CARTESIAN_POINT('Ctrl Pts',(10.4675706859999,15.2,-3.40384362500001));
#184522=CARTESIAN_POINT('Ctrl Pts',(10.4699937039999,15.2,-3.40574611300001));
#184523=CARTESIAN_POINT('Ctrl Pts',(10.4724193259999,15.2,-3.40765383700001));
#184524=CARTESIAN_POINT('Ctrl Pts',(10.4748475419999,15.2,-3.40956679600001));
#184525=CARTESIAN_POINT('Ctrl Pts',(10.4772783389999,15.2,-3.41148499200001));
#184526=CARTESIAN_POINT('Ctrl Pts',(10.4797117049999,15.2,-3.41340842300002));
#184527=CARTESIAN_POINT('Ctrl Pts',(10.4821476289999,15.2,-3.41533709100001));
#184528=CARTESIAN_POINT('Ctrl Pts',(10.4845860999999,15.2,-3.41727099600002));
#184529=CARTESIAN_POINT('Ctrl Pts',(10.4870271039999,15.2,-3.41921013700001));
#184530=CARTESIAN_POINT('Ctrl Pts',(10.4894706319999,15.2,-3.42115451300002));
#184531=CARTESIAN_POINT('Ctrl Pts',(10.4919166709999,15.2,-3.42310412600002));
#184532=CARTESIAN_POINT('Ctrl Pts',(10.4943652099999,15.2,-3.42505897500001));
#184533=CARTESIAN_POINT('Ctrl Pts',(10.4968162359999,15.2,-3.42701906000002));
#184534=CARTESIAN_POINT('Ctrl Pts',(10.4992697399999,15.2,-3.42898438100002));
#184535=CARTESIAN_POINT('Ctrl Pts',(10.5017257079999,15.2,-3.43095493800002));
#184536=CARTESIAN_POINT('Ctrl Pts',(10.5041841299999,15.2,-3.43293073100002));
#184537=CARTESIAN_POINT('Ctrl Pts',(10.5066449939999,15.2,-3.43491176000001));
#184538=CARTESIAN_POINT('Ctrl Pts',(10.5091082899999,15.2,-3.43689802500001));
#184539=CARTESIAN_POINT('Ctrl Pts',(10.5115740039999,15.2,-3.43888952500001));
#184540=CARTESIAN_POINT('Ctrl Pts',(10.5140421269999,15.2,-3.44088626100001));
#184541=CARTESIAN_POINT('Ctrl Pts',(10.5165126449999,15.2,-3.44288823300001));
#184542=CARTESIAN_POINT('Ctrl Pts',(10.5189855499999,15.2,-3.44489544000002));
#184543=CARTESIAN_POINT('Ctrl Pts',(10.5214608269999,15.2,-3.44690788300001));
#184544=CARTESIAN_POINT('Ctrl Pts',(10.5239384669999,15.2,-3.44892556000001));
#184545=CARTESIAN_POINT('Ctrl Pts',(10.5264184599999,15.2,-3.45094847300001));
#184546=CARTESIAN_POINT('Ctrl Pts',(10.5289007929999,15.2,-3.45297662100001));
#184547=CARTESIAN_POINT('Ctrl Pts',(10.5313854529999,15.2,-3.45501000300001));
#184548=CARTESIAN_POINT('Ctrl Pts',(10.5338724319999,15.2,-3.45704862000002));
#184549=CARTESIAN_POINT('Ctrl Pts',(10.5363617169999,15.2,-3.45909247100002));
#184550=CARTESIAN_POINT('Ctrl Pts',(10.5388532969999,15.2,-3.46114155700001));
#184551=CARTESIAN_POINT('Ctrl Pts',(10.5413471629999,15.2,-3.46319587600001));
#184552=CARTESIAN_POINT('Ctrl Pts',(10.5438433009999,15.2,-3.46525543000002));
#184553=CARTESIAN_POINT('Ctrl Pts',(10.5463417019999,15.2,-3.46732021700001));
#184554=CARTESIAN_POINT('Ctrl Pts',(10.5488423529999,15.2,-3.46939023800001));
#184555=CARTESIAN_POINT('Ctrl Pts',(10.5513452449999,15.2,-3.47146549100001));
#184556=CARTESIAN_POINT('Ctrl Pts',(10.5538503639999,15.2,-3.47354597800001));
#184557=CARTESIAN_POINT('Ctrl Pts',(10.5563577029999,15.2,-3.47563169800001));
#184558=CARTESIAN_POINT('Ctrl Pts',(10.5588672479999,15.2,-3.47772265000001));
#184559=CARTESIAN_POINT('Ctrl Pts',(10.5613789899999,15.2,-3.47981883400001));
#184560=CARTESIAN_POINT('Ctrl Pts',(10.5638929169999,15.2,-3.48192025000001));
#184561=CARTESIAN_POINT('Ctrl Pts',(10.5664090179999,15.2,-3.48402689800002));
#184562=CARTESIAN_POINT('Ctrl Pts',(10.5689272829999,15.2,-3.48613877700001));
#184563=CARTESIAN_POINT('Ctrl Pts',(10.5714476989999,15.2,-3.48825588800001));
#184564=CARTESIAN_POINT('Ctrl Pts',(10.5739702579999,15.2,-3.49037822900002));
#184565=CARTESIAN_POINT('Ctrl Pts',(10.5764949479999,15.2,-3.49250580000001));
#184566=CARTESIAN_POINT('Ctrl Pts',(10.5790217569999,15.2,-3.49463860200002));
#184567=CARTESIAN_POINT('Ctrl Pts',(10.5815506769999,15.2,-3.49677663500001));
#184568=CARTESIAN_POINT('Ctrl Pts',(10.5840816949999,15.2,-3.49891989600001));
#184569=CARTESIAN_POINT('Ctrl Pts',(10.5866147999999,15.2,-3.50106838700002));
#184570=CARTESIAN_POINT('Ctrl Pts',(10.5891499829999,15.2,-3.50322210700002));
#184571=CARTESIAN_POINT('Ctrl Pts',(10.5916872319999,15.2,-3.50538105500001));
#184572=CARTESIAN_POINT('Ctrl Pts',(10.5942265379999,15.2,-3.50754523200001));
#184573=CARTESIAN_POINT('Ctrl Pts',(10.5967678879999,15.2,-3.50971463600001));
#184574=CARTESIAN_POINT('Ctrl Pts',(10.5993112729999,15.2,-3.51188926900001));
#184575=CARTESIAN_POINT('Ctrl Pts',(10.6018566829999,15.2,-3.51406912700002));
#184576=CARTESIAN_POINT('Ctrl Pts',(10.6044041049999,15.2,-3.51625421300001));
#184577=CARTESIAN_POINT('Ctrl Pts',(10.6069535309999,15.2,-3.51844452500002));
#184578=CARTESIAN_POINT('Ctrl Pts',(10.6095049489999,15.2,-3.52064006300001));
#184579=CARTESIAN_POINT('Ctrl Pts',(10.6120583479999,15.2,-3.52284082600002));
#184580=CARTESIAN_POINT('Ctrl Pts',(10.6146137189999,15.2,-3.52504681400001));
#184581=CARTESIAN_POINT('Ctrl Pts',(10.6171710509999,15.2,-3.52725802700002));
#184582=CARTESIAN_POINT('Ctrl Pts',(10.6197303339999,15.2,-3.52947446500002));
#184583=CARTESIAN_POINT('Ctrl Pts',(10.6222915559999,15.2,-3.53169612600002));
#184584=CARTESIAN_POINT('Ctrl Pts',(10.6248547079999,15.2,-3.53392301000001));
#184585=CARTESIAN_POINT('Ctrl Pts',(10.6274197799999,15.2,-3.53615511700001));
#184586=CARTESIAN_POINT('Ctrl Pts',(10.6299867589999,15.2,-3.53839244700001));
#184587=CARTESIAN_POINT('Ctrl Pts',(10.6325556389999,15.2,-3.54063499900001));
#184588=CARTESIAN_POINT('Ctrl Pts',(10.6351264049999,15.2,-3.54288277200002));
#184589=CARTESIAN_POINT('Ctrl Pts',(10.6376990499999,15.2,-3.54513576600001));
#184590=CARTESIAN_POINT('Ctrl Pts',(10.6402735619999,15.2,-3.54739398000001));
#184591=CARTESIAN_POINT('Ctrl Pts',(10.6428499309999,15.2,-3.54965741400001));
#184592=CARTESIAN_POINT('Ctrl Pts',(10.6454281479999,15.2,-3.55192606900002));
#184593=CARTESIAN_POINT('Ctrl Pts',(10.6480082019999,15.2,-3.55419994100002));
#184594=CARTESIAN_POINT('Ctrl Pts',(10.6505900819999,15.2,-3.55647903300001));
#184595=CARTESIAN_POINT('Ctrl Pts',(10.6531737789999,15.2,-3.55876334200001));
#184596=CARTESIAN_POINT('Ctrl Pts',(10.6557592819999,15.2,-3.56105286800001));
#184597=CARTESIAN_POINT('Ctrl Pts',(10.6583465819999,15.2,-3.56334761200001));
#184598=CARTESIAN_POINT('Ctrl Pts',(10.6609356659999,15.2,-3.56564757100001));
#184599=CARTESIAN_POINT('Ctrl Pts',(10.6635265279999,15.2,-3.56795274600001));
#184600=CARTESIAN_POINT('Ctrl Pts',(10.6661191539999,15.2,-3.57026313700001));
#184601=CARTESIAN_POINT('Ctrl Pts',(10.6687135369999,15.2,-3.57257874200001));
#184602=CARTESIAN_POINT('Ctrl Pts',(10.6713096659999,15.2,-3.57489956100002));
#184603=CARTESIAN_POINT('Ctrl Pts',(10.6739075299999,15.2,-3.57722559400001));
#184604=CARTESIAN_POINT('Ctrl Pts',(10.6765071199999,15.2,-3.57955683900002));
#184605=CARTESIAN_POINT('Ctrl Pts',(10.6791084249999,15.2,-3.58189329600001));
#184606=CARTESIAN_POINT('Ctrl Pts',(10.6817114369999,15.2,-3.58423496500002));
#184607=CARTESIAN_POINT('Ctrl Pts',(10.6843161429999,15.2,-3.58658184500001));
#184608=CARTESIAN_POINT('Ctrl Pts',(10.6869225359999,15.2,-3.58893393500002));
#184609=CARTESIAN_POINT('Ctrl Pts',(10.6895306049999,15.2,-3.59129123500002));
#184610=CARTESIAN_POINT('Ctrl Pts',(10.6921403399999,15.2,-3.59365374400001));
#184611=CARTESIAN_POINT('Ctrl Pts',(10.6947517299999,15.2,-3.59602146200002));
#184612=CARTESIAN_POINT('Ctrl Pts',(10.6973647669999,15.2,-3.59839438800002));
#184613=CARTESIAN_POINT('Ctrl Pts',(10.6999794399999,15.2,-3.60077252100002));
#184614=CARTESIAN_POINT('Ctrl Pts',(10.7025957399999,15.2,-3.60315585900001));
#184615=CARTESIAN_POINT('Ctrl Pts',(10.7052136559999,15.2,-3.60554440400001));
#184616=CARTESIAN_POINT('Ctrl Pts',(10.7078331809999,15.2,-3.60793815500001));
#184617=CARTESIAN_POINT('Ctrl Pts',(10.7104543019999,15.2,-3.61033710900001));
#184618=CARTESIAN_POINT('Ctrl Pts',(10.7130770099999,15.2,-3.61274126800001));
#184619=CARTESIAN_POINT('Ctrl Pts',(10.7157012959999,15.2,-3.61515062900001));
#184620=CARTESIAN_POINT('Ctrl Pts',(10.7183271499999,15.2,-3.61756519200001));
#184621=CARTESIAN_POINT('Ctrl Pts',(10.7209545619999,15.2,-3.61998495800002));
#184622=CARTESIAN_POINT('Ctrl Pts',(10.7235835239999,15.2,-3.62240992500002));
#184623=CARTESIAN_POINT('Ctrl Pts',(10.7262140239999,15.2,-3.62484009100001));
#184624=CARTESIAN_POINT('Ctrl Pts',(10.7288460529999,15.2,-3.62727545700002));
#184625=CARTESIAN_POINT('Ctrl Pts',(10.7314796019999,15.2,-3.62971602300002));
#184626=CARTESIAN_POINT('Ctrl Pts',(10.7341146619999,15.2,-3.63216178500001));
#184627=CARTESIAN_POINT('Ctrl Pts',(10.7367512209999,15.2,-3.63461274500001));
#184628=CARTESIAN_POINT('Ctrl Pts',(10.7393892719999,15.2,-3.63706890200001));
#184629=CARTESIAN_POINT('Ctrl Pts',(10.7420288039999,15.2,-3.63953025500001));
#184630=CARTESIAN_POINT('Ctrl Pts',(10.7446698079999,15.2,-3.64199680200001));
#184631=CARTESIAN_POINT('Ctrl Pts',(10.7473122739999,15.2,-3.64446854400001));
#184632=CARTESIAN_POINT('Ctrl Pts',(10.7499561929999,15.2,-3.64694547900001));
#184633=CARTESIAN_POINT('Ctrl Pts',(10.7526015559999,15.2,-3.64942760700002));
#184634=CARTESIAN_POINT('Ctrl Pts',(10.7552483519999,15.2,-3.65191492600001));
#184635=CARTESIAN_POINT('Ctrl Pts',(10.7578965719999,15.2,-3.65440743700002));
#184636=CARTESIAN_POINT('Ctrl Pts',(10.7605462079999,15.2,-3.65690513800002));
#184637=CARTESIAN_POINT('Ctrl Pts',(10.7631972489999,15.2,-3.65940802800001));
#184638=CARTESIAN_POINT('Ctrl Pts',(10.7658496859999,15.2,-3.66191610700001));
#184639=CARTESIAN_POINT('Ctrl Pts',(10.7685035109999,15.2,-3.66442937400001));
#184640=CARTESIAN_POINT('Ctrl Pts',(10.7711587129999,15.2,-3.66694782800002));
#184641=CARTESIAN_POINT('Ctrl Pts',(10.7738152829999,15.2,-3.66947146800001));
#184642=CARTESIAN_POINT('Ctrl Pts',(10.7764732109999,15.2,-3.67200029300002));
#184643=CARTESIAN_POINT('Ctrl Pts',(10.7791324889999,15.2,-3.67453430200001));
#184644=CARTESIAN_POINT('Ctrl Pts',(10.7817931069999,15.2,-3.67707349500002));
#184645=CARTESIAN_POINT('Ctrl Pts',(10.7844550569999,15.2,-3.67961787200001));
#184646=CARTESIAN_POINT('Ctrl Pts',(10.7871183259999,15.2,-3.68216742900001));
#184647=CARTESIAN_POINT('Ctrl Pts',(10.7897829079999,15.2,-3.68472216800001));
#184648=CARTESIAN_POINT('Ctrl Pts',(10.7924487949999,15.2,-3.68728208700002));
#184649=CARTESIAN_POINT('Ctrl Pts',(10.7951159729999,15.2,-3.68984718400001));
#184650=CARTESIAN_POINT('Ctrl Pts',(10.7977844379999,15.2,-3.69241746100001));
#184651=CARTESIAN_POINT('Ctrl Pts',(10.8004541779999,15.2,-3.69499291500002));
#184652=CARTESIAN_POINT('Ctrl Pts',(10.8031251839999,15.2,-3.69757354500001));
#184653=CARTESIAN_POINT('Ctrl Pts',(10.8057974489999,15.2,-3.70015935000001));
#184654=CARTESIAN_POINT('Ctrl Pts',(10.8084709609999,15.2,-3.70275033200001));
#184655=CARTESIAN_POINT('Ctrl Pts',(10.8111457129999,15.2,-3.70534648600001));
#184656=CARTESIAN_POINT('Ctrl Pts',(10.8138216939999,15.2,-3.70794781300001));
#184657=CARTESIAN_POINT('Ctrl Pts',(10.8164988939999,15.2,-3.71055431200002));
#184658=CARTESIAN_POINT('Ctrl Pts',(10.8191773059999,15.2,-3.71316598200002));
#184659=CARTESIAN_POINT('Ctrl Pts',(10.8218569179999,15.2,-3.71578282200002));
#184660=CARTESIAN_POINT('Ctrl Pts',(10.8245377239999,15.2,-3.71840483100002));
#184661=CARTESIAN_POINT('Ctrl Pts',(10.8272197149999,15.2,-3.72103200700002));
#184662=CARTESIAN_POINT('Ctrl Pts',(10.8299028829999,15.2,-3.72366435100002));
#184663=CARTESIAN_POINT('Ctrl Pts',(10.8325872199999,15.2,-3.72630186200002));
#184664=CARTESIAN_POINT('Ctrl Pts',(10.8352727169999,15.2,-3.72894453800001));
#184665=CARTESIAN_POINT('Ctrl Pts',(10.8379593649999,15.2,-3.73159237800001));
#184666=CARTESIAN_POINT('Ctrl Pts',(10.8406471529999,15.2,-3.73424538200001));
#184667=CARTESIAN_POINT('Ctrl Pts',(10.8433360699999,15.2,-3.73690354800001));
#184668=CARTESIAN_POINT('Ctrl Pts',(10.8460261069999,15.2,-3.73956687500002));
#184669=CARTESIAN_POINT('Ctrl Pts',(10.8487172499999,15.2,-3.74223536100001));
#184670=CARTESIAN_POINT('Ctrl Pts',(10.8514094899999,15.2,-3.74490900600001));
#184671=CARTESIAN_POINT('Ctrl Pts',(10.8541028209999,15.2,-3.74758780800001));
#184672=CARTESIAN_POINT('Ctrl Pts',(10.8567972349999,15.2,-3.75027176800002));
#184673=CARTESIAN_POINT('Ctrl Pts',(10.8594927299999,15.2,-3.75296088400002));
#184674=CARTESIAN_POINT('Ctrl Pts',(10.8621893019999,15.2,-3.75565515600002));
#184675=CARTESIAN_POINT('Ctrl Pts',(10.8643474199999,15.2,-3.75781469800001));
#184676=CARTESIAN_POINT('Ctrl Pts',(10.8659664939999,15.2,-3.75943667400001));
#184677=CARTESIAN_POINT('Ctrl Pts',(10.8670460909999,15.2,-3.76051902400001));
#184678=CARTESIAN_POINT('Ctrl Pts',(10.8675859439999,15.2,-3.76106045600002));
#184679=CARTESIAN_POINT('Origin',(-5.66257110645729E-14,15.2,-1.77635683940025E-14));
#184680=CARTESIAN_POINT('',(10.0330625574591,15.2,-2.64164356403315));
#184681=CARTESIAN_POINT('',(10.0330625574591,12.2,-2.64164356403315));
#184682=CARTESIAN_POINT('',(10.0330625569999,15.2,-2.64164356400002));
#184683=CARTESIAN_POINT('Origin',(-5.66257110645729E-14,12.2,-1.77635683940025E-14));
#184684=CARTESIAN_POINT('Origin',(-5.66257110645729E-14,15.2,-1.77635683940025E-14));
#184685=CARTESIAN_POINT('Origin',(-5.66257110645729E-14,15.2,-1.77635683940025E-14));
#184686=CARTESIAN_POINT('',(11.2133565919999,15.2,-2.55159439000002));
#184687=CARTESIAN_POINT('',(11.2922242989999,15.2,-2.17615954700001));
#184688=CARTESIAN_POINT('Origin',(-5.66257110645729E-14,15.2,-1.77635683940025E-14));
#184689=CARTESIAN_POINT('',(11.2922242989999,12.2,-2.17615954700001));
#184690=CARTESIAN_POINT('',(11.2922242989999,15.2,-2.17615954700001));
#184691=CARTESIAN_POINT('',(11.2133565919999,12.2,-2.55159439000002));
#184692=CARTESIAN_POINT('Origin',(-5.66257110645729E-14,12.2,-1.77635683940025E-14));
#184693=CARTESIAN_POINT('',(11.2133565919999,15.2,-2.55159439000002));
#184694=CARTESIAN_POINT('Ctrl Pts',(11.2922242989999,15.2,-2.17615954700001));
#184695=CARTESIAN_POINT('Ctrl Pts',(11.2922242989999,11.6,-2.17615954700001));
#184696=CARTESIAN_POINT('Ctrl Pts',(11.2916128879999,15.2,-2.17570045500001));
#184697=CARTESIAN_POINT('Ctrl Pts',(11.2916128879999,11.6,-2.17570045500001));
#184698=CARTESIAN_POINT('Ctrl Pts',(11.2903902449999,15.2,-2.17478276600001));
#184699=CARTESIAN_POINT('Ctrl Pts',(11.2903902449999,11.6,-2.17478276600001));
#184700=CARTESIAN_POINT('Ctrl Pts',(11.2885568199999,15.2,-2.17340771600002));
#184701=CARTESIAN_POINT('Ctrl Pts',(11.2885568199999,11.6,-2.17340771600002));
#184702=CARTESIAN_POINT('Ctrl Pts',(11.2861133329999,15.2,-2.17157728800002));
#184703=CARTESIAN_POINT('Ctrl Pts',(11.2861133329999,11.6,-2.17157728800002));
#184704=CARTESIAN_POINT('Ctrl Pts',(11.2830607729999,15.2,-2.16929420200001));
#184705=CARTESIAN_POINT('Ctrl Pts',(11.2830607729999,11.6,-2.16929420200001));
#184706=CARTESIAN_POINT('Ctrl Pts',(11.2800100139999,15.2,-2.16701606700001));
#184707=CARTESIAN_POINT('Ctrl Pts',(11.2800100139999,11.6,-2.16701606700001));
#184708=CARTESIAN_POINT('Ctrl Pts',(11.2769610569999,15.2,-2.16474288000001));
#184709=CARTESIAN_POINT('Ctrl Pts',(11.2769610569999,11.6,-2.16474288000002));
#184710=CARTESIAN_POINT('Ctrl Pts',(11.2739139069999,15.2,-2.16247464600002));
#184711=CARTESIAN_POINT('Ctrl Pts',(11.2739139069999,11.6,-2.16247464600002));
#184712=CARTESIAN_POINT('Ctrl Pts',(11.2708685709999,15.2,-2.16021135900001));
#184713=CARTESIAN_POINT('Ctrl Pts',(11.2708685709999,11.6,-2.16021135900002));
#184714=CARTESIAN_POINT('Ctrl Pts',(11.2678250539999,15.2,-2.15795302400001));
#184715=CARTESIAN_POINT('Ctrl Pts',(11.2678250539999,11.6,-2.15795302400001));
#184716=CARTESIAN_POINT('Ctrl Pts',(11.2647833679999,15.2,-2.15569963800001));
#184717=CARTESIAN_POINT('Ctrl Pts',(11.2647833679999,11.6,-2.15569963800002));
#184718=CARTESIAN_POINT('Ctrl Pts',(11.2617435239999,15.2,-2.15345120200002));
#184719=CARTESIAN_POINT('Ctrl Pts',(11.2617435239999,11.6,-2.15345120200002));
#184720=CARTESIAN_POINT('Ctrl Pts',(11.2587055319999,15.2,-2.15120771400001));
#184721=CARTESIAN_POINT('Ctrl Pts',(11.2587055319999,11.6,-2.15120771400001));
#184722=CARTESIAN_POINT('Ctrl Pts',(11.2556694029999,15.2,-2.14896917500001));
#184723=CARTESIAN_POINT('Ctrl Pts',(11.2556694029999,11.6,-2.14896917500001));
#184724=CARTESIAN_POINT('Ctrl Pts',(11.2526351489999,15.2,-2.14673558300001));
#184725=CARTESIAN_POINT('Ctrl Pts',(11.2526351489999,11.6,-2.14673558300001));
#184726=CARTESIAN_POINT('Ctrl Pts',(11.2496027769999,15.2,-2.14450693900002));
#184727=CARTESIAN_POINT('Ctrl Pts',(11.2496027769999,11.6,-2.14450693900002));
#184728=CARTESIAN_POINT('Ctrl Pts',(11.2465722989999,15.2,-2.14228324400001));
#184729=CARTESIAN_POINT('Ctrl Pts',(11.2465722989999,11.6,-2.14228324400001));
#184730=CARTESIAN_POINT('Ctrl Pts',(11.2435437199999,15.2,-2.14006449500001));
#184731=CARTESIAN_POINT('Ctrl Pts',(11.2435437199999,11.6,-2.14006449500001));
#184732=CARTESIAN_POINT('Ctrl Pts',(11.2405170499999,15.2,-2.13785069200001));
#184733=CARTESIAN_POINT('Ctrl Pts',(11.2405170499999,11.6,-2.13785069200001));
#184734=CARTESIAN_POINT('Ctrl Pts',(11.2374922969999,15.2,-2.13564183800001));
#184735=CARTESIAN_POINT('Ctrl Pts',(11.2374922969999,11.6,-2.13564183800001));
#184736=CARTESIAN_POINT('Ctrl Pts',(11.2344694679999,15.2,-2.13343792800002));
#184737=CARTESIAN_POINT('Ctrl Pts',(11.2344694679999,11.6,-2.13343792800002));
#184738=CARTESIAN_POINT('Ctrl Pts',(11.2314485739999,15.2,-2.13123896500001));
#184739=CARTESIAN_POINT('Ctrl Pts',(11.2314485739999,11.6,-2.13123896500001));
#184740=CARTESIAN_POINT('Ctrl Pts',(11.2284296229999,15.2,-2.12904494700001));
#184741=CARTESIAN_POINT('Ctrl Pts',(11.2284296229999,11.6,-2.12904494700001));
#184742=CARTESIAN_POINT('Ctrl Pts',(11.2254126259999,15.2,-2.12685587500001));
#184743=CARTESIAN_POINT('Ctrl Pts',(11.2254126259999,11.6,-2.12685587500001));
#184744=CARTESIAN_POINT('Ctrl Pts',(11.2223975909999,15.2,-2.12467174800001));
#184745=CARTESIAN_POINT('Ctrl Pts',(11.2223975909999,11.6,-2.12467174800001));
#184746=CARTESIAN_POINT('Ctrl Pts',(11.2193845279999,15.2,-2.12249256400002));
#184747=CARTESIAN_POINT('Ctrl Pts',(11.2193845279999,11.6,-2.12249256400002));
#184748=CARTESIAN_POINT('Ctrl Pts',(11.2163734459999,15.2,-2.12031832500001));
#184749=CARTESIAN_POINT('Ctrl Pts',(11.2163734459999,11.6,-2.12031832500002));
#184750=CARTESIAN_POINT('Ctrl Pts',(11.2133643549999,15.2,-2.11814902900001));
#184751=CARTESIAN_POINT('Ctrl Pts',(11.2133643549999,11.6,-2.11814902900001));
#184752=CARTESIAN_POINT('Ctrl Pts',(11.2103572639999,15.2,-2.11598467700002));
#184753=CARTESIAN_POINT('Ctrl Pts',(11.2103572639999,11.6,-2.11598467700002));
#184754=CARTESIAN_POINT('Ctrl Pts',(11.2073521809999,15.2,-2.11382526700001));
#184755=CARTESIAN_POINT('Ctrl Pts',(11.2073521809999,11.6,-2.11382526700001));
#184756=CARTESIAN_POINT('Ctrl Pts',(11.2043491159999,15.2,-2.11167080000001));
#184757=CARTESIAN_POINT('Ctrl Pts',(11.2043491159999,11.6,-2.11167080000001));
#184758=CARTESIAN_POINT('Ctrl Pts',(11.2013480779999,15.2,-2.10952127400001));
#184759=CARTESIAN_POINT('Ctrl Pts',(11.2013480779999,11.6,-2.10952127400002));
#184760=CARTESIAN_POINT('Ctrl Pts',(11.1983490759999,15.2,-2.10737669000002));
#184761=CARTESIAN_POINT('Ctrl Pts',(11.1983490759999,11.6,-2.10737669000002));
#184762=CARTESIAN_POINT('Ctrl Pts',(11.1953521189999,15.2,-2.10523704700002));
#184763=CARTESIAN_POINT('Ctrl Pts',(11.1953521189999,11.6,-2.10523704700002));
#184764=CARTESIAN_POINT('Ctrl Pts',(11.1923572179999,15.2,-2.10310234400001));
#184765=CARTESIAN_POINT('Ctrl Pts',(11.1923572179999,11.6,-2.10310234400001));
#184766=CARTESIAN_POINT('Ctrl Pts',(11.1893643799999,15.2,-2.10097258200001));
#184767=CARTESIAN_POINT('Ctrl Pts',(11.1893643799999,11.6,-2.10097258200001));
#184768=CARTESIAN_POINT('Ctrl Pts',(11.1863736159999,15.2,-2.09884776000001));
#184769=CARTESIAN_POINT('Ctrl Pts',(11.1863736159999,11.6,-2.09884776000001));
#184770=CARTESIAN_POINT('Ctrl Pts',(11.1833849349999,15.2,-2.09672787600002));
#184771=CARTESIAN_POINT('Ctrl Pts',(11.1833849349999,11.6,-2.09672787600002));
#184772=CARTESIAN_POINT('Ctrl Pts',(11.1803983459999,15.2,-2.09461293100001));
#184773=CARTESIAN_POINT('Ctrl Pts',(11.1803983459999,11.6,-2.09461293100001));
#184774=CARTESIAN_POINT('Ctrl Pts',(11.1774138589999,15.2,-2.09250292400001));
#184775=CARTESIAN_POINT('Ctrl Pts',(11.1774138589999,11.6,-2.09250292400002));
#184776=CARTESIAN_POINT('Ctrl Pts',(11.1744314829999,15.2,-2.09039785500002));
#184777=CARTESIAN_POINT('Ctrl Pts',(11.1744314829999,11.6,-2.09039785500002));
#184778=CARTESIAN_POINT('Ctrl Pts',(11.1714512269999,15.2,-2.08829772200001));
#184779=CARTESIAN_POINT('Ctrl Pts',(11.1714512269999,11.6,-2.08829772200001));
#184780=CARTESIAN_POINT('Ctrl Pts',(11.1684731009999,15.2,-2.08620252800001));
#184781=CARTESIAN_POINT('Ctrl Pts',(11.1684731009999,11.6,-2.08620252800001));
#184782=CARTESIAN_POINT('Ctrl Pts',(11.1654971139999,15.2,-2.08411226800001));
#184783=CARTESIAN_POINT('Ctrl Pts',(11.1654971139999,11.6,-2.08411226800001));
#184784=CARTESIAN_POINT('Ctrl Pts',(11.1625232759999,15.2,-2.08202694400001));
#184785=CARTESIAN_POINT('Ctrl Pts',(11.1625232759999,11.6,-2.08202694400002));
#184786=CARTESIAN_POINT('Ctrl Pts',(11.1595515959999,15.2,-2.07994655500002));
#184787=CARTESIAN_POINT('Ctrl Pts',(11.1595515959999,11.6,-2.07994655500002));
#184788=CARTESIAN_POINT('Ctrl Pts',(11.1565820829999,15.2,-2.07787110100002));
#184789=CARTESIAN_POINT('Ctrl Pts',(11.1565820829999,11.6,-2.07787110100002));
#184790=CARTESIAN_POINT('Ctrl Pts',(11.1536147479999,15.2,-2.07580058000001));
#184791=CARTESIAN_POINT('Ctrl Pts',(11.1536147479999,11.6,-2.07580058000001));
#184792=CARTESIAN_POINT('Ctrl Pts',(11.1506495989999,15.2,-2.07373499200001));
#184793=CARTESIAN_POINT('Ctrl Pts',(11.1506495989999,11.6,-2.07373499200001));
#184794=CARTESIAN_POINT('Ctrl Pts',(11.1476866469999,15.2,-2.07167433800001));
#184795=CARTESIAN_POINT('Ctrl Pts',(11.1476866469999,11.6,-2.07167433800001));
#184796=CARTESIAN_POINT('Ctrl Pts',(11.1447258999999,15.2,-2.06961861400002));
#184797=CARTESIAN_POINT('Ctrl Pts',(11.1447258999999,11.6,-2.06961861400002));
#184798=CARTESIAN_POINT('Ctrl Pts',(11.1417673689999,15.2,-2.06756782300001));
#184799=CARTESIAN_POINT('Ctrl Pts',(11.1417673689999,11.6,-2.06756782300001));
#184800=CARTESIAN_POINT('Ctrl Pts',(11.1388110619999,15.2,-2.06552196300001));
#184801=CARTESIAN_POINT('Ctrl Pts',(11.1388110619999,11.6,-2.06552196300001));
#184802=CARTESIAN_POINT('Ctrl Pts',(11.1358569909999,15.2,-2.06348103200002));
#184803=CARTESIAN_POINT('Ctrl Pts',(11.1358569909999,11.6,-2.06348103200002));
#184804=CARTESIAN_POINT('Ctrl Pts',(11.1329051619999,15.2,-2.06144503100001));
#184805=CARTESIAN_POINT('Ctrl Pts',(11.1329051619999,11.6,-2.06144503100001));
#184806=CARTESIAN_POINT('Ctrl Pts',(11.1299555879999,15.2,-2.05941396000001));
#184807=CARTESIAN_POINT('Ctrl Pts',(11.1299555879999,11.6,-2.05941396000001));
#184808=CARTESIAN_POINT('Ctrl Pts',(11.1270082769999,15.2,-2.05738781600001));
#184809=CARTESIAN_POINT('Ctrl Pts',(11.1270082769999,11.6,-2.05738781600001));
#184810=CARTESIAN_POINT('Ctrl Pts',(11.1240632389999,15.2,-2.05536660000002));
#184811=CARTESIAN_POINT('Ctrl Pts',(11.1240632389999,11.6,-2.05536660000002));
#184812=CARTESIAN_POINT('Ctrl Pts',(11.1211204849999,15.2,-2.05335031100002));
#184813=CARTESIAN_POINT('Ctrl Pts',(11.1211204849999,11.6,-2.05335031100002));
#184814=CARTESIAN_POINT('Ctrl Pts',(11.1181800219999,15.2,-2.05133894900001));
#184815=CARTESIAN_POINT('Ctrl Pts',(11.1181800219999,11.6,-2.05133894900001));
#184816=CARTESIAN_POINT('Ctrl Pts',(11.1152418619999,15.2,-2.04933251100002));
#184817=CARTESIAN_POINT('Ctrl Pts',(11.1152418619999,11.6,-2.04933251100002));
#184818=CARTESIAN_POINT('Ctrl Pts',(11.1123060129999,15.2,-2.04733099900002));
#184819=CARTESIAN_POINT('Ctrl Pts',(11.1123060129999,11.6,-2.04733099900002));
#184820=CARTESIAN_POINT('Ctrl Pts',(11.1093724859999,15.2,-2.04533441000001));
#184821=CARTESIAN_POINT('Ctrl Pts',(11.1093724859999,11.6,-2.04533441000002));
#184822=CARTESIAN_POINT('Ctrl Pts',(11.1064412909999,15.2,-2.04334274600001));
#184823=CARTESIAN_POINT('Ctrl Pts',(11.1064412909999,11.6,-2.04334274600001));
#184824=CARTESIAN_POINT('Ctrl Pts',(11.1035124359999,15.2,-2.04135600400001));
#184825=CARTESIAN_POINT('Ctrl Pts',(11.1035124359999,11.6,-2.04135600400001));
#184826=CARTESIAN_POINT('Ctrl Pts',(11.1005859329999,15.2,-2.03937418500002));
#184827=CARTESIAN_POINT('Ctrl Pts',(11.1005859329999,11.6,-2.03937418500002));
#184828=CARTESIAN_POINT('Ctrl Pts',(11.0976617909999,15.2,-2.03739728600001));
#184829=CARTESIAN_POINT('Ctrl Pts',(11.0976617909999,11.6,-2.03739728600001));
#184830=CARTESIAN_POINT('Ctrl Pts',(11.0947400189999,15.2,-2.03542530800001));
#184831=CARTESIAN_POINT('Ctrl Pts',(11.0947400189999,11.6,-2.03542530800001));
#184832=CARTESIAN_POINT('Ctrl Pts',(11.0918206279999,15.2,-2.03345825000001));
#184833=CARTESIAN_POINT('Ctrl Pts',(11.0918206279999,11.6,-2.03345825000001));
#184834=CARTESIAN_POINT('Ctrl Pts',(11.0889036269999,15.2,-2.03149611000002));
#184835=CARTESIAN_POINT('Ctrl Pts',(11.0889036269999,11.6,-2.03149611000002));
#184836=CARTESIAN_POINT('Ctrl Pts',(11.0859890259999,15.2,-2.02953888900002));
#184837=CARTESIAN_POINT('Ctrl Pts',(11.0859890259999,11.6,-2.02953888900002));
#184838=CARTESIAN_POINT('Ctrl Pts',(11.0830768349999,15.2,-2.02758658500001));
#184839=CARTESIAN_POINT('Ctrl Pts',(11.0830768349999,11.6,-2.02758658500001));
#184840=CARTESIAN_POINT('Ctrl Pts',(11.0801670649999,15.2,-2.02563919800001));
#184841=CARTESIAN_POINT('Ctrl Pts',(11.0801670649999,11.6,-2.02563919800001));
#184842=CARTESIAN_POINT('Ctrl Pts',(11.0772597239999,15.2,-2.02369672700002));
#184843=CARTESIAN_POINT('Ctrl Pts',(11.0772597239999,11.6,-2.02369672700002));
#184844=CARTESIAN_POINT('Ctrl Pts',(11.0743548239999,15.2,-2.02175917000002));
#184845=CARTESIAN_POINT('Ctrl Pts',(11.0743548239999,11.6,-2.02175917000002));
#184846=CARTESIAN_POINT('Ctrl Pts',(11.0714523729999,15.2,-2.01982652800002));
#184847=CARTESIAN_POINT('Ctrl Pts',(11.0714523729999,11.6,-2.01982652800002));
#184848=CARTESIAN_POINT('Ctrl Pts',(11.0685523819999,15.2,-2.01789879900002));
#184849=CARTESIAN_POINT('Ctrl Pts',(11.0685523819999,11.6,-2.01789879900002));
#184850=CARTESIAN_POINT('Ctrl Pts',(11.0656548619999,15.2,-2.01597598400001));
#184851=CARTESIAN_POINT('Ctrl Pts',(11.0656548619999,11.6,-2.01597598400001));
#184852=CARTESIAN_POINT('Ctrl Pts',(11.0627598219999,15.2,-2.01405807900001));
#184853=CARTESIAN_POINT('Ctrl Pts',(11.0627598219999,11.6,-2.01405807900001));
#184854=CARTESIAN_POINT('Ctrl Pts',(11.0598672709999,15.2,-2.01214508500001));
#184855=CARTESIAN_POINT('Ctrl Pts',(11.0598672709999,11.6,-2.01214508500001));
#184856=CARTESIAN_POINT('Ctrl Pts',(11.0569772199999,15.2,-2.01023700100002));
#184857=CARTESIAN_POINT('Ctrl Pts',(11.0569772199999,11.6,-2.01023700100002));
#184858=CARTESIAN_POINT('Ctrl Pts',(11.0540896799999,15.2,-2.00833382500001));
#184859=CARTESIAN_POINT('Ctrl Pts',(11.0540896799999,11.6,-2.00833382500001));
#184860=CARTESIAN_POINT('Ctrl Pts',(11.0512046609999,15.2,-2.00643555900001));
#184861=CARTESIAN_POINT('Ctrl Pts',(11.0512046609999,11.6,-2.00643555900002));
#184862=CARTESIAN_POINT('Ctrl Pts',(11.0483221709999,15.2,-2.00454219900001));
#184863=CARTESIAN_POINT('Ctrl Pts',(11.0483221709999,11.6,-2.00454219900001));
#184864=CARTESIAN_POINT('Ctrl Pts',(11.0454422219999,15.2,-2.00265374600002));
#184865=CARTESIAN_POINT('Ctrl Pts',(11.0454422219999,11.6,-2.00265374600002));
#184866=CARTESIAN_POINT('Ctrl Pts',(11.0425648239999,15.2,-2.00077019700001));
#184867=CARTESIAN_POINT('Ctrl Pts',(11.0425648239999,11.6,-2.00077019700002));
#184868=CARTESIAN_POINT('Ctrl Pts',(11.0396899859999,15.2,-1.99889155300002));
#184869=CARTESIAN_POINT('Ctrl Pts',(11.0396899859999,11.6,-1.99889155300002));
#184870=CARTESIAN_POINT('Ctrl Pts',(11.0368177199999,15.2,-1.99701781300002));
#184871=CARTESIAN_POINT('Ctrl Pts',(11.0368177199999,11.6,-1.99701781300002));
#184872=CARTESIAN_POINT('Ctrl Pts',(11.0339480349999,15.2,-1.99514897500002));
#184873=CARTESIAN_POINT('Ctrl Pts',(11.0339480349999,11.6,-1.99514897500002));
#184874=CARTESIAN_POINT('Ctrl Pts',(11.0310809409999,15.2,-1.99328503900002));
#184875=CARTESIAN_POINT('Ctrl Pts',(11.0310809409999,11.6,-1.99328503900002));
#184876=CARTESIAN_POINT('Ctrl Pts',(11.0282164499999,15.2,-1.99142600400001));
#184877=CARTESIAN_POINT('Ctrl Pts',(11.0282164499999,11.6,-1.99142600400001));
#184878=CARTESIAN_POINT('Ctrl Pts',(11.0253545699999,15.2,-1.98957186700001));
#184879=CARTESIAN_POINT('Ctrl Pts',(11.0253545699999,11.6,-1.98957186700001));
#184880=CARTESIAN_POINT('Ctrl Pts',(11.0224953139999,15.2,-1.98772263000001));
#184881=CARTESIAN_POINT('Ctrl Pts',(11.0224953139999,11.6,-1.98772263000001));
#184882=CARTESIAN_POINT('Ctrl Pts',(11.0196386889999,15.2,-1.98587829000001));
#184883=CARTESIAN_POINT('Ctrl Pts',(11.0196386889999,11.6,-1.98587829000001));
#184884=CARTESIAN_POINT('Ctrl Pts',(11.0167847069999,15.2,-1.98403884600001));
#184885=CARTESIAN_POINT('Ctrl Pts',(11.0167847069999,11.6,-1.98403884600001));
#184886=CARTESIAN_POINT('Ctrl Pts',(11.0139333789999,15.2,-1.98220429900001));
#184887=CARTESIAN_POINT('Ctrl Pts',(11.0139333789999,11.6,-1.98220429900001));
#184888=CARTESIAN_POINT('Ctrl Pts',(11.0110847139999,15.2,-1.98037464500001));
#184889=CARTESIAN_POINT('Ctrl Pts',(11.0110847139999,11.6,-1.98037464500001));
#184890=CARTESIAN_POINT('Ctrl Pts',(11.0082387239999,15.2,-1.97854988600001));
#184891=CARTESIAN_POINT('Ctrl Pts',(11.0082387239999,11.6,-1.97854988600001));
#184892=CARTESIAN_POINT('Ctrl Pts',(11.0053954179999,15.2,-1.97673001800001));
#184893=CARTESIAN_POINT('Ctrl Pts',(11.0053954179999,11.6,-1.97673001800002));
#184894=CARTESIAN_POINT('Ctrl Pts',(11.0025548069999,15.2,-1.97491504200002));
#184895=CARTESIAN_POINT('Ctrl Pts',(11.0025548069999,11.6,-1.97491504200002));
#184896=CARTESIAN_POINT('Ctrl Pts',(10.9997169009999,15.2,-1.97310495600002));
#184897=CARTESIAN_POINT('Ctrl Pts',(10.9997169009999,11.6,-1.97310495600002));
#184898=CARTESIAN_POINT('Ctrl Pts',(10.9968817109999,15.2,-1.97129976000001));
#184899=CARTESIAN_POINT('Ctrl Pts',(10.9968817109999,11.6,-1.97129976000001));
#184900=CARTESIAN_POINT('Ctrl Pts',(10.9940492479999,15.2,-1.96949945100001));
#184901=CARTESIAN_POINT('Ctrl Pts',(10.9940492479999,11.6,-1.96949945100001));
#184902=CARTESIAN_POINT('Ctrl Pts',(10.9912195209999,15.2,-1.96770403000002));
#184903=CARTESIAN_POINT('Ctrl Pts',(10.9912195209999,11.6,-1.96770403000002));
#184904=CARTESIAN_POINT('Ctrl Pts',(10.9883925419999,15.2,-1.96591349300002));
#184905=CARTESIAN_POINT('Ctrl Pts',(10.9883925419999,11.6,-1.96591349300002));
#184906=CARTESIAN_POINT('Ctrl Pts',(10.9855683189999,15.2,-1.96412784200001));
#184907=CARTESIAN_POINT('Ctrl Pts',(10.9855683189999,11.6,-1.96412784200001));
#184908=CARTESIAN_POINT('Ctrl Pts',(10.9827468659999,15.2,-1.96234707600001));
#184909=CARTESIAN_POINT('Ctrl Pts',(10.9827468659999,11.6,-1.96234707600001));
#184910=CARTESIAN_POINT('Ctrl Pts',(10.9799281919999,15.2,-1.96057119000002));
#184911=CARTESIAN_POINT('Ctrl Pts',(10.9799281919999,11.6,-1.96057119000002));
#184912=CARTESIAN_POINT('Ctrl Pts',(10.9771123069999,15.2,-1.95880018600001));
#184913=CARTESIAN_POINT('Ctrl Pts',(10.9771123069999,11.6,-1.95880018600001));
#184914=CARTESIAN_POINT('Ctrl Pts',(10.9742992229999,15.2,-1.95703406200002));
#184915=CARTESIAN_POINT('Ctrl Pts',(10.9742992229999,11.6,-1.95703406200002));
#184916=CARTESIAN_POINT('Ctrl Pts',(10.9714889499999,15.2,-1.95527281700001));
#184917=CARTESIAN_POINT('Ctrl Pts',(10.9714889499999,11.6,-1.95527281700001));
#184918=CARTESIAN_POINT('Ctrl Pts',(10.9686814969999,15.2,-1.95351645000001));
#184919=CARTESIAN_POINT('Ctrl Pts',(10.9686814969999,11.6,-1.95351645000002));
#184920=CARTESIAN_POINT('Ctrl Pts',(10.9658768769999,15.2,-1.95176496000002));
#184921=CARTESIAN_POINT('Ctrl Pts',(10.9658768769999,11.6,-1.95176496000002));
#184922=CARTESIAN_POINT('Ctrl Pts',(10.9630750999999,15.2,-1.95001834400002));
#184923=CARTESIAN_POINT('Ctrl Pts',(10.9630750999999,11.6,-1.95001834400002));
#184924=CARTESIAN_POINT('Ctrl Pts',(10.9602761759999,15.2,-1.94827660300001));
#184925=CARTESIAN_POINT('Ctrl Pts',(10.9602761759999,11.6,-1.94827660300001));
#184926=CARTESIAN_POINT('Ctrl Pts',(10.9574801169999,15.2,-1.94653973400001));
#184927=CARTESIAN_POINT('Ctrl Pts',(10.9574801169999,11.6,-1.94653973400001));
#184928=CARTESIAN_POINT('Ctrl Pts',(10.9546869339999,15.2,-1.94480773700001));
#184929=CARTESIAN_POINT('Ctrl Pts',(10.9546869339999,11.6,-1.94480773700001));
#184930=CARTESIAN_POINT('Ctrl Pts',(10.9518966359999,15.2,-1.94308061000001));
#184931=CARTESIAN_POINT('Ctrl Pts',(10.9518966359999,11.6,-1.94308061000001));
#184932=CARTESIAN_POINT('Ctrl Pts',(10.9491092339999,15.2,-1.94135835200001));
#184933=CARTESIAN_POINT('Ctrl Pts',(10.9491092339999,11.6,-1.94135835200001));
#184934=CARTESIAN_POINT('Ctrl Pts',(10.9463247409999,15.2,-1.93964096300002));
#184935=CARTESIAN_POINT('Ctrl Pts',(10.9463247409999,11.6,-1.93964096300002));
#184936=CARTESIAN_POINT('Ctrl Pts',(10.9435431659999,15.2,-1.93792843900002));
#184937=CARTESIAN_POINT('Ctrl Pts',(10.9435431659999,11.6,-1.93792843900002));
#184938=CARTESIAN_POINT('Ctrl Pts',(10.9407645199999,15.2,-1.93622078000002));
#184939=CARTESIAN_POINT('Ctrl Pts',(10.9407645199999,11.6,-1.93622078000002));
#184940=CARTESIAN_POINT('Ctrl Pts',(10.9379888129999,15.2,-1.93451798600002));
#184941=CARTESIAN_POINT('Ctrl Pts',(10.9379888129999,11.6,-1.93451798600002));
#184942=CARTESIAN_POINT('Ctrl Pts',(10.9352160579999,15.2,-1.93282005400001));
#184943=CARTESIAN_POINT('Ctrl Pts',(10.9352160579999,11.6,-1.93282005400001));
#184944=CARTESIAN_POINT('Ctrl Pts',(10.9324462649999,15.2,-1.93112698300002));
#184945=CARTESIAN_POINT('Ctrl Pts',(10.9324462649999,11.6,-1.93112698300002));
#184946=CARTESIAN_POINT('Ctrl Pts',(10.9296794449999,15.2,-1.92943877200001));
#184947=CARTESIAN_POINT('Ctrl Pts',(10.9296794449999,11.6,-1.92943877200001));
#184948=CARTESIAN_POINT('Ctrl Pts',(10.9269156089999,15.2,-1.92775541900001));
#184949=CARTESIAN_POINT('Ctrl Pts',(10.9269156089999,11.6,-1.92775541900002));
#184950=CARTESIAN_POINT('Ctrl Pts',(10.9241547679999,15.2,-1.92607692400002));
#184951=CARTESIAN_POINT('Ctrl Pts',(10.9241547679999,11.6,-1.92607692400002));
#184952=CARTESIAN_POINT('Ctrl Pts',(10.9213969329999,15.2,-1.92440328400002));
#184953=CARTESIAN_POINT('Ctrl Pts',(10.9213969329999,11.6,-1.92440328400002));
#184954=CARTESIAN_POINT('Ctrl Pts',(10.9186421139999,15.2,-1.92273449800001));
#184955=CARTESIAN_POINT('Ctrl Pts',(10.9186421139999,11.6,-1.92273449800001));
#184956=CARTESIAN_POINT('Ctrl Pts',(10.9158903239999,15.2,-1.92107056500001));
#184957=CARTESIAN_POINT('Ctrl Pts',(10.9158903239999,11.6,-1.92107056500001));
#184958=CARTESIAN_POINT('Ctrl Pts',(10.9131415729999,15.2,-1.91941148400002));
#184959=CARTESIAN_POINT('Ctrl Pts',(10.9131415729999,11.6,-1.91941148400002));
#184960=CARTESIAN_POINT('Ctrl Pts',(10.9103958719999,15.2,-1.91775725300001));
#184961=CARTESIAN_POINT('Ctrl Pts',(10.9103958719999,11.6,-1.91775725300001));
#184962=CARTESIAN_POINT('Ctrl Pts',(10.9076532319999,15.2,-1.91610787000001));
#184963=CARTESIAN_POINT('Ctrl Pts',(10.9076532319999,11.6,-1.91610787000001));
#184964=CARTESIAN_POINT('Ctrl Pts',(10.9049136649999,15.2,-1.91446333400001));
#184965=CARTESIAN_POINT('Ctrl Pts',(10.9049136649999,11.6,-1.91446333400001));
#184966=CARTESIAN_POINT('Ctrl Pts',(10.9021771809999,15.2,-1.91282364500001));
#184967=CARTESIAN_POINT('Ctrl Pts',(10.9021771809999,11.6,-1.91282364500002));
#184968=CARTESIAN_POINT('Ctrl Pts',(10.8994437919999,15.2,-1.91118879900001));
#184969=CARTESIAN_POINT('Ctrl Pts',(10.8994437919999,11.6,-1.91118879900001));
#184970=CARTESIAN_POINT('Ctrl Pts',(10.8967135099999,15.2,-1.90955879600001));
#184971=CARTESIAN_POINT('Ctrl Pts',(10.8967135099999,11.6,-1.90955879600002));
#184972=CARTESIAN_POINT('Ctrl Pts',(10.8939863439999,15.2,-1.90793363400001));
#184973=CARTESIAN_POINT('Ctrl Pts',(10.8939863439999,11.6,-1.90793363400001));
#184974=CARTESIAN_POINT('Ctrl Pts',(10.8912623069999,15.2,-1.90631331100001));
#184975=CARTESIAN_POINT('Ctrl Pts',(10.8912623069999,11.6,-1.90631331100001));
#184976=CARTESIAN_POINT('Ctrl Pts',(10.8885414099999,15.2,-1.90469782700001));
#184977=CARTESIAN_POINT('Ctrl Pts',(10.8885414099999,11.6,-1.90469782700002));
#184978=CARTESIAN_POINT('Ctrl Pts',(10.8858236639999,15.2,-1.90308718000002));
#184979=CARTESIAN_POINT('Ctrl Pts',(10.8858236639999,11.6,-1.90308718000002));
#184980=CARTESIAN_POINT('Ctrl Pts',(10.8831090799999,15.2,-1.90148136800001));
#184981=CARTESIAN_POINT('Ctrl Pts',(10.8831090799999,11.6,-1.90148136800001));
#184982=CARTESIAN_POINT('Ctrl Pts',(10.8803976699999,15.2,-1.89988038900001));
#184983=CARTESIAN_POINT('Ctrl Pts',(10.8803976699999,11.6,-1.89988038900002));
#184984=CARTESIAN_POINT('Ctrl Pts',(10.8776894459999,15.2,-1.89828424200002));
#184985=CARTESIAN_POINT('Ctrl Pts',(10.8776894459999,11.6,-1.89828424200002));
#184986=CARTESIAN_POINT('Ctrl Pts',(10.8749844169999,15.2,-1.89669292500001));
#184987=CARTESIAN_POINT('Ctrl Pts',(10.8749844169999,11.6,-1.89669292500001));
#184988=CARTESIAN_POINT('Ctrl Pts',(10.8722825979999,15.2,-1.89510643700002));
#184989=CARTESIAN_POINT('Ctrl Pts',(10.8722825979999,11.6,-1.89510643700002));
#184990=CARTESIAN_POINT('Ctrl Pts',(10.8695839969999,15.2,-1.89352477600002));
#184991=CARTESIAN_POINT('Ctrl Pts',(10.8695839969999,11.6,-1.89352477600002));
#184992=CARTESIAN_POINT('Ctrl Pts',(10.8668886269999,15.2,-1.89194794100001));
#184993=CARTESIAN_POINT('Ctrl Pts',(10.8668886269999,11.6,-1.89194794100001));
#184994=CARTESIAN_POINT('Ctrl Pts',(10.8641964999999,15.2,-1.89037593000001));
#184995=CARTESIAN_POINT('Ctrl Pts',(10.8641964999999,11.6,-1.89037593000001));
#184996=CARTESIAN_POINT('Ctrl Pts',(10.8615076259999,15.2,-1.88880873900001));
#184997=CARTESIAN_POINT('Ctrl Pts',(10.8615076259999,11.6,-1.88880873900001));
#184998=CARTESIAN_POINT('Ctrl Pts',(10.8588220189999,15.2,-1.88724637100002));
#184999=CARTESIAN_POINT('Ctrl Pts',(10.8588220189999,11.6,-1.88724637100002));
#185000=CARTESIAN_POINT('Ctrl Pts',(10.8561396869999,15.2,-1.88568882100002));
#185001=CARTESIAN_POINT('Ctrl Pts',(10.8561396869999,11.6,-1.88568882100002));
#185002=CARTESIAN_POINT('Ctrl Pts',(10.8534606449999,15.2,-1.88413608800001));
#185003=CARTESIAN_POINT('Ctrl Pts',(10.8534606449999,11.6,-1.88413608800001));
#185004=CARTESIAN_POINT('Ctrl Pts',(10.8507849019999,15.2,-1.88258817100001));
#185005=CARTESIAN_POINT('Ctrl Pts',(10.8507849019999,11.6,-1.88258817100001));
#185006=CARTESIAN_POINT('Ctrl Pts',(10.8481124719999,15.2,-1.88104506700002));
#185007=CARTESIAN_POINT('Ctrl Pts',(10.8481124719999,11.6,-1.88104506700002));
#185008=CARTESIAN_POINT('Ctrl Pts',(10.8454433649999,15.2,-1.87950677600002));
#185009=CARTESIAN_POINT('Ctrl Pts',(10.8454433649999,11.6,-1.87950677600002));
#185010=CARTESIAN_POINT('Ctrl Pts',(10.8427775919999,15.2,-1.87797329500001));
#185011=CARTESIAN_POINT('Ctrl Pts',(10.8427775919999,11.6,-1.87797329500001));
#185012=CARTESIAN_POINT('Ctrl Pts',(10.8401151679999,15.2,-1.87644462300002));
#185013=CARTESIAN_POINT('Ctrl Pts',(10.8401151679999,11.6,-1.87644462300002));
#185014=CARTESIAN_POINT('Ctrl Pts',(10.8374561019999,15.2,-1.87492075600002));
#185015=CARTESIAN_POINT('Ctrl Pts',(10.8374561019999,11.6,-1.87492075600002));
#185016=CARTESIAN_POINT('Ctrl Pts',(10.8348004049999,15.2,-1.87340169600001));
#185017=CARTESIAN_POINT('Ctrl Pts',(10.8348004049999,11.6,-1.87340169600001));
#185018=CARTESIAN_POINT('Ctrl Pts',(10.8321480909999,15.2,-1.87188743700001));
#185019=CARTESIAN_POINT('Ctrl Pts',(10.8321480909999,11.6,-1.87188743700002));
#185020=CARTESIAN_POINT('Ctrl Pts',(10.8294991699999,15.2,-1.87037798100001));
#185021=CARTESIAN_POINT('Ctrl Pts',(10.8294991699999,11.6,-1.87037798100001));
#185022=CARTESIAN_POINT('Ctrl Pts',(10.8268536559999,15.2,-1.86887332500001));
#185023=CARTESIAN_POINT('Ctrl Pts',(10.8268536559999,11.6,-1.86887332500001));
#185024=CARTESIAN_POINT('Ctrl Pts',(10.8242115599999,15.2,-1.86737346600002));
#185025=CARTESIAN_POINT('Ctrl Pts',(10.8242115599999,11.6,-1.86737346600002));
#185026=CARTESIAN_POINT('Ctrl Pts',(10.8215728919999,15.2,-1.86587840300001));
#185027=CARTESIAN_POINT('Ctrl Pts',(10.8215728919999,11.6,-1.86587840300001));
#185028=CARTESIAN_POINT('Ctrl Pts',(10.8189376659999,15.2,-1.86438813400001));
#185029=CARTESIAN_POINT('Ctrl Pts',(10.8189376659999,11.6,-1.86438813400002));
#185030=CARTESIAN_POINT('Ctrl Pts',(10.8163058929999,15.2,-1.86290265800002));
#185031=CARTESIAN_POINT('Ctrl Pts',(10.8163058929999,11.6,-1.86290265800002));
#185032=CARTESIAN_POINT('Ctrl Pts',(10.8136775859999,15.2,-1.86142197100001));
#185033=CARTESIAN_POINT('Ctrl Pts',(10.8136775859999,11.6,-1.86142197100002));
#185034=CARTESIAN_POINT('Ctrl Pts',(10.8110527559999,15.2,-1.85994607300001));
#185035=CARTESIAN_POINT('Ctrl Pts',(10.8110527559999,11.6,-1.85994607300001));
#185036=CARTESIAN_POINT('Ctrl Pts',(10.8084314149999,15.2,-1.85847496100001));
#185037=CARTESIAN_POINT('Ctrl Pts',(10.8084314149999,11.6,-1.85847496100001));
#185038=CARTESIAN_POINT('Ctrl Pts',(10.8058135739999,15.2,-1.85700863500001));
#185039=CARTESIAN_POINT('Ctrl Pts',(10.8058135739999,11.6,-1.85700863500002));
#185040=CARTESIAN_POINT('Ctrl Pts',(10.8031992479999,15.2,-1.85554709000002));
#185041=CARTESIAN_POINT('Ctrl Pts',(10.8031992479999,11.6,-1.85554709000002));
#185042=CARTESIAN_POINT('Ctrl Pts',(10.8005884479999,15.2,-1.85409032700001));
#185043=CARTESIAN_POINT('Ctrl Pts',(10.8005884479999,11.6,-1.85409032700001));
#185044=CARTESIAN_POINT('Ctrl Pts',(10.7979811829999,15.2,-1.85263834300001));
#185045=CARTESIAN_POINT('Ctrl Pts',(10.7979811829999,11.6,-1.85263834300002));
#185046=CARTESIAN_POINT('Ctrl Pts',(10.7953774699999,15.2,-1.85119113400001));
#185047=CARTESIAN_POINT('Ctrl Pts',(10.7953774699999,11.6,-1.85119113400001));
#185048=CARTESIAN_POINT('Ctrl Pts',(10.7927773169999,15.2,-1.84974870100001));
#185049=CARTESIAN_POINT('Ctrl Pts',(10.7927773169999,11.6,-1.84974870100001));
#185050=CARTESIAN_POINT('Ctrl Pts',(10.7901807389999,15.2,-1.84831104100001));
#185051=CARTESIAN_POINT('Ctrl Pts',(10.7901807389999,11.6,-1.84831104100002));
#185052=CARTESIAN_POINT('Ctrl Pts',(10.7875877469999,15.2,-1.84687815000002));
#185053=CARTESIAN_POINT('Ctrl Pts',(10.7875877469999,11.6,-1.84687815000002));
#185054=CARTESIAN_POINT('Ctrl Pts',(10.7849983529999,15.2,-1.84545003000002));
#185055=CARTESIAN_POINT('Ctrl Pts',(10.7849983529999,11.6,-1.84545003000002));
#185056=CARTESIAN_POINT('Ctrl Pts',(10.7824125699999,15.2,-1.84402667500001));
#185057=CARTESIAN_POINT('Ctrl Pts',(10.7824125699999,11.6,-1.84402667500001));
#185058=CARTESIAN_POINT('Ctrl Pts',(10.7798304099999,15.2,-1.84260808500001));
#185059=CARTESIAN_POINT('Ctrl Pts',(10.7798304099999,11.6,-1.84260808500001));
#185060=CARTESIAN_POINT('Ctrl Pts',(10.7772518849999,15.2,-1.84119425700001));
#185061=CARTESIAN_POINT('Ctrl Pts',(10.7772518849999,11.6,-1.84119425700001));
#185062=CARTESIAN_POINT('Ctrl Pts',(10.7746770079999,15.2,-1.83978519100001));
#185063=CARTESIAN_POINT('Ctrl Pts',(10.7746770079999,11.6,-1.83978519100001));
#185064=CARTESIAN_POINT('Ctrl Pts',(10.7721057909999,15.2,-1.83838088200002));
#185065=CARTESIAN_POINT('Ctrl Pts',(10.7721057909999,11.6,-1.83838088200002));
#185066=CARTESIAN_POINT('Ctrl Pts',(10.7695382459999,15.2,-1.83698133000001));
#185067=CARTESIAN_POINT('Ctrl Pts',(10.7695382459999,11.6,-1.83698133000001));
#185068=CARTESIAN_POINT('Ctrl Pts',(10.7669743859999,15.2,-1.83558653200001));
#185069=CARTESIAN_POINT('Ctrl Pts',(10.7669743859999,11.6,-1.83558653200001));
#185070=CARTESIAN_POINT('Ctrl Pts',(10.7644142219999,15.2,-1.83419648500001));
#185071=CARTESIAN_POINT('Ctrl Pts',(10.7644142219999,11.6,-1.83419648500002));
#185072=CARTESIAN_POINT('Ctrl Pts',(10.7618577699999,15.2,-1.83281118900001));
#185073=CARTESIAN_POINT('Ctrl Pts',(10.7618577699999,11.6,-1.83281118900001));
#185074=CARTESIAN_POINT('Ctrl Pts',(10.7593050389999,15.2,-1.83143064000001));
#185075=CARTESIAN_POINT('Ctrl Pts',(10.7593050389999,11.6,-1.83143064000001));
#185076=CARTESIAN_POINT('Ctrl Pts',(10.7567560429999,15.2,-1.83005483600001));
#185077=CARTESIAN_POINT('Ctrl Pts',(10.7567560429999,11.6,-1.83005483600002));
#185078=CARTESIAN_POINT('Ctrl Pts',(10.7542107949999,15.2,-1.82868377600002));
#185079=CARTESIAN_POINT('Ctrl Pts',(10.7542107949999,11.6,-1.82868377600002));
#185080=CARTESIAN_POINT('Ctrl Pts',(10.7516693049999,15.2,-1.82731745700002));
#185081=CARTESIAN_POINT('Ctrl Pts',(10.7516693049999,11.6,-1.82731745700002));
#185082=CARTESIAN_POINT('Ctrl Pts',(10.7491315889999,15.2,-1.82595587600002));
#185083=CARTESIAN_POINT('Ctrl Pts',(10.7491315889999,11.6,-1.82595587600002));
#185084=CARTESIAN_POINT('Ctrl Pts',(10.7465976589999,15.2,-1.82459903200002));
#185085=CARTESIAN_POINT('Ctrl Pts',(10.7465976589999,11.6,-1.82459903200002));
#185086=CARTESIAN_POINT('Ctrl Pts',(10.7440675249999,15.2,-1.82324692100002));
#185087=CARTESIAN_POINT('Ctrl Pts',(10.7440675249999,11.6,-1.82324692100002));
#185088=CARTESIAN_POINT('Ctrl Pts',(10.7415412029999,15.2,-1.82189954400001));
#185089=CARTESIAN_POINT('Ctrl Pts',(10.7415412029999,11.6,-1.82189954400001));
#185090=CARTESIAN_POINT('Ctrl Pts',(10.7390187039999,15.2,-1.82055689500002));
#185091=CARTESIAN_POINT('Ctrl Pts',(10.7390187039999,11.6,-1.82055689500002));
#185092=CARTESIAN_POINT('Ctrl Pts',(10.7365000409999,15.2,-1.81921897400001));
#185093=CARTESIAN_POINT('Ctrl Pts',(10.7365000409999,11.6,-1.81921897400001));
#185094=CARTESIAN_POINT('Ctrl Pts',(10.7339852259999,15.2,-1.81788577800001));
#185095=CARTESIAN_POINT('Ctrl Pts',(10.7339852259999,11.6,-1.81788577800001));
#185096=CARTESIAN_POINT('Ctrl Pts',(10.7314742729999,15.2,-1.81655730500001));
#185097=CARTESIAN_POINT('Ctrl Pts',(10.7314742729999,11.6,-1.81655730500002));
#185098=CARTESIAN_POINT('Ctrl Pts',(10.7289671959999,15.2,-1.81523355200001));
#185099=CARTESIAN_POINT('Ctrl Pts',(10.7289671959999,11.6,-1.81523355200001));
#185100=CARTESIAN_POINT('Ctrl Pts',(10.7264640049999,15.2,-1.81391451700001));
#185101=CARTESIAN_POINT('Ctrl Pts',(10.7264640049999,11.6,-1.81391451700002));
#185102=CARTESIAN_POINT('Ctrl Pts',(10.7239647149999,15.2,-1.81260019700002));
#185103=CARTESIAN_POINT('Ctrl Pts',(10.7239647149999,11.6,-1.81260019700002));
#185104=CARTESIAN_POINT('Ctrl Pts',(10.7214693369999,15.2,-1.81129059100002));
#185105=CARTESIAN_POINT('Ctrl Pts',(10.7214693369999,11.6,-1.81129059100002));
#185106=CARTESIAN_POINT('Ctrl Pts',(10.7189778869999,15.2,-1.80998569500002));
#185107=CARTESIAN_POINT('Ctrl Pts',(10.7189778869999,11.6,-1.80998569500002));
#185108=CARTESIAN_POINT('Ctrl Pts',(10.7164903759999,15.2,-1.80868550800001));
#185109=CARTESIAN_POINT('Ctrl Pts',(10.7164903759999,11.6,-1.80868550800001));
#185110=CARTESIAN_POINT('Ctrl Pts',(10.7140068169999,15.2,-1.80739002600002));
#185111=CARTESIAN_POINT('Ctrl Pts',(10.7140068169999,11.6,-1.80739002600002));
#185112=CARTESIAN_POINT('Ctrl Pts',(10.7115272219999,15.2,-1.80609924900001));
#185113=CARTESIAN_POINT('Ctrl Pts',(10.7115272219999,11.6,-1.80609924900002));
#185114=CARTESIAN_POINT('Ctrl Pts',(10.7090516069999,15.2,-1.80481317100002));
#185115=CARTESIAN_POINT('Ctrl Pts',(10.7090516069999,11.6,-1.80481317100002));
#185116=CARTESIAN_POINT('Ctrl Pts',(10.7065799829999,15.2,-1.80353179300001));
#185117=CARTESIAN_POINT('Ctrl Pts',(10.7065799829999,11.6,-1.80353179300001));
#185118=CARTESIAN_POINT('Ctrl Pts',(10.7041123629999,15.2,-1.80225511000002));
#185119=CARTESIAN_POINT('Ctrl Pts',(10.7041123629999,11.6,-1.80225511000002));
#185120=CARTESIAN_POINT('Ctrl Pts',(10.7016487619999,15.2,-1.80098312100001));
#185121=CARTESIAN_POINT('Ctrl Pts',(10.7016487619999,11.6,-1.80098312100002));
#185122=CARTESIAN_POINT('Ctrl Pts',(10.6991891909999,15.2,-1.79971582200002));
#185123=CARTESIAN_POINT('Ctrl Pts',(10.6991891909999,11.6,-1.79971582200002));
#185124=CARTESIAN_POINT('Ctrl Pts',(10.6967336649999,15.2,-1.79845321200002));
#185125=CARTESIAN_POINT('Ctrl Pts',(10.6967336649999,11.6,-1.79845321200002));
#185126=CARTESIAN_POINT('Ctrl Pts',(10.6942821969999,15.2,-1.79719528800002));
#185127=CARTESIAN_POINT('Ctrl Pts',(10.6942821969999,11.6,-1.79719528800002));
#185128=CARTESIAN_POINT('Ctrl Pts',(10.6918347989999,15.2,-1.79594204600001));
#185129=CARTESIAN_POINT('Ctrl Pts',(10.6918347989999,11.6,-1.79594204600001));
#185130=CARTESIAN_POINT('Ctrl Pts',(10.6893914849999,15.2,-1.79469348500001));
#185131=CARTESIAN_POINT('Ctrl Pts',(10.6893914849999,11.6,-1.79469348500001));
#185132=CARTESIAN_POINT('Ctrl Pts',(10.6869522689999,15.2,-1.79344960200002));
#185133=CARTESIAN_POINT('Ctrl Pts',(10.6869522689999,11.6,-1.79344960200002));
#185134=CARTESIAN_POINT('Ctrl Pts',(10.6845171639999,15.2,-1.79221039500002));
#185135=CARTESIAN_POINT('Ctrl Pts',(10.6845171639999,11.6,-1.79221039500002));
#185136=CARTESIAN_POINT('Ctrl Pts',(10.6820861829999,15.2,-1.79097585900001));
#185137=CARTESIAN_POINT('Ctrl Pts',(10.6820861829999,11.6,-1.79097585900002));
#185138=CARTESIAN_POINT('Ctrl Pts',(10.6796593399999,15.2,-1.78974599400001));
#185139=CARTESIAN_POINT('Ctrl Pts',(10.6796593399999,11.6,-1.78974599400001));
#185140=CARTESIAN_POINT('Ctrl Pts',(10.6772366489999,15.2,-1.78852079700001));
#185141=CARTESIAN_POINT('Ctrl Pts',(10.6772366489999,11.6,-1.78852079700001));
#185142=CARTESIAN_POINT('Ctrl Pts',(10.6748181209999,15.2,-1.78730026200002));
#185143=CARTESIAN_POINT('Ctrl Pts',(10.6748181209999,11.6,-1.78730026200002));
#185144=CARTESIAN_POINT('Ctrl Pts',(10.6724037739999,15.2,-1.78608439100001));
#185145=CARTESIAN_POINT('Ctrl Pts',(10.6724037739999,11.6,-1.78608439100001));
#185146=CARTESIAN_POINT('Ctrl Pts',(10.6699936169999,15.2,-1.78487317800001));
#185147=CARTESIAN_POINT('Ctrl Pts',(10.6699936169999,11.6,-1.78487317800002));
#185148=CARTESIAN_POINT('Ctrl Pts',(10.6675876659999,15.2,-1.78366662200002));
#185149=CARTESIAN_POINT('Ctrl Pts',(10.6675876659999,11.6,-1.78366662200002));
#185150=CARTESIAN_POINT('Ctrl Pts',(10.6651859349999,15.2,-1.78246471900001));
#185151=CARTESIAN_POINT('Ctrl Pts',(10.6651859349999,11.6,-1.78246471900001));
#185152=CARTESIAN_POINT('Ctrl Pts',(10.6627884359999,15.2,-1.78126746700002));
#185153=CARTESIAN_POINT('Ctrl Pts',(10.6627884359999,11.6,-1.78126746700002));
#185154=CARTESIAN_POINT('Ctrl Pts',(10.6603951839999,15.2,-1.78007486200002));
#185155=CARTESIAN_POINT('Ctrl Pts',(10.6603951839999,11.6,-1.78007486200002));
#185156=CARTESIAN_POINT('Ctrl Pts',(10.6580061929999,15.2,-1.77888690400001));
#185157=CARTESIAN_POINT('Ctrl Pts',(10.6580061929999,11.6,-1.77888690400001));
#185158=CARTESIAN_POINT('Ctrl Pts',(10.6556214759999,15.2,-1.77770358600001));
#185159=CARTESIAN_POINT('Ctrl Pts',(10.6556214759999,11.6,-1.77770358600001));
#185160=CARTESIAN_POINT('Ctrl Pts',(10.6532410469999,15.2,-1.77652490900002));
#185161=CARTESIAN_POINT('Ctrl Pts',(10.6532410469999,11.6,-1.77652490900002));
#185162=CARTESIAN_POINT('Ctrl Pts',(10.6508649199999,15.2,-1.77535086800002));
#185163=CARTESIAN_POINT('Ctrl Pts',(10.6508649199999,11.6,-1.77535086800002));
#185164=CARTESIAN_POINT('Ctrl Pts',(10.6484931079999,15.2,-1.77418146100001));
#185165=CARTESIAN_POINT('Ctrl Pts',(10.6484931079999,11.6,-1.77418146100001));
#185166=CARTESIAN_POINT('Ctrl Pts',(10.6461256269999,15.2,-1.77301668400001));
#185167=CARTESIAN_POINT('Ctrl Pts',(10.6461256269999,11.6,-1.77301668400002));
#185168=CARTESIAN_POINT('Ctrl Pts',(10.6437624889999,15.2,-1.77185653600001));
#185169=CARTESIAN_POINT('Ctrl Pts',(10.6437624889999,11.6,-1.77185653600001));
#185170=CARTESIAN_POINT('Ctrl Pts',(10.6414037079999,15.2,-1.77070101100002));
#185171=CARTESIAN_POINT('Ctrl Pts',(10.6414037079999,11.6,-1.77070101100002));
#185172=CARTESIAN_POINT('Ctrl Pts',(10.6390492989999,15.2,-1.76955010900001));
#185173=CARTESIAN_POINT('Ctrl Pts',(10.6390492989999,11.6,-1.76955010900001));
#185174=CARTESIAN_POINT('Ctrl Pts',(10.6366992769999,15.2,-1.76840382600002));
#185175=CARTESIAN_POINT('Ctrl Pts',(10.6366992769999,11.6,-1.76840382600002));
#185176=CARTESIAN_POINT('Ctrl Pts',(10.6343536529999,15.2,-1.76726215800001));
#185177=CARTESIAN_POINT('Ctrl Pts',(10.6343536529999,11.6,-1.76726215800001));
#185178=CARTESIAN_POINT('Ctrl Pts',(10.6320124439999,15.2,-1.76612510300002));
#185179=CARTESIAN_POINT('Ctrl Pts',(10.6320124439999,11.6,-1.76612510300002));
#185180=CARTESIAN_POINT('Ctrl Pts',(10.6296756629999,15.2,-1.76499265800001));
#185181=CARTESIAN_POINT('Ctrl Pts',(10.6296756629999,11.6,-1.76499265800001));
#185182=CARTESIAN_POINT('Ctrl Pts',(10.6273433229999,15.2,-1.76386482000002));
#185183=CARTESIAN_POINT('Ctrl Pts',(10.6273433229999,11.6,-1.76386482000002));
#185184=CARTESIAN_POINT('Ctrl Pts',(10.6250154409999,15.2,-1.76274158600001));
#185185=CARTESIAN_POINT('Ctrl Pts',(10.6250154409999,11.6,-1.76274158600001));
#185186=CARTESIAN_POINT('Ctrl Pts',(10.6226920299999,15.2,-1.76162295100001));
#185187=CARTESIAN_POINT('Ctrl Pts',(10.6226920299999,11.6,-1.76162295100002));
#185188=CARTESIAN_POINT('Ctrl Pts',(10.6203731039999,15.2,-1.76050891500001));
#185189=CARTESIAN_POINT('Ctrl Pts',(10.6203731039999,11.6,-1.76050891500001));
#185190=CARTESIAN_POINT('Ctrl Pts',(10.6180586769999,15.2,-1.75939947300002));
#185191=CARTESIAN_POINT('Ctrl Pts',(10.6180586769999,11.6,-1.75939947300002));
#185192=CARTESIAN_POINT('Ctrl Pts',(10.6157487639999,15.2,-1.75829462200001));
#185193=CARTESIAN_POINT('Ctrl Pts',(10.6157487639999,11.6,-1.75829462200001));
#185194=CARTESIAN_POINT('Ctrl Pts',(10.6134433789999,15.2,-1.75719435900001));
#185195=CARTESIAN_POINT('Ctrl Pts',(10.6134433789999,11.6,-1.75719435900001));
#185196=CARTESIAN_POINT('Ctrl Pts',(10.6111425369999,15.2,-1.75609868000001));
#185197=CARTESIAN_POINT('Ctrl Pts',(10.6111425369999,11.6,-1.75609868000001));
#185198=CARTESIAN_POINT('Ctrl Pts',(10.6088462529999,15.2,-1.75500758300001));
#185199=CARTESIAN_POINT('Ctrl Pts',(10.6088462529999,11.6,-1.75500758300001));
#185200=CARTESIAN_POINT('Ctrl Pts',(10.6065545399999,15.2,-1.75392106500002));
#185201=CARTESIAN_POINT('Ctrl Pts',(10.6065545399999,11.6,-1.75392106500002));
#185202=CARTESIAN_POINT('Ctrl Pts',(10.6042674129999,15.2,-1.75283912300001));
#185203=CARTESIAN_POINT('Ctrl Pts',(10.6042674129999,11.6,-1.75283912300001));
#185204=CARTESIAN_POINT('Ctrl Pts',(10.6019848869999,15.2,-1.75176175100002));
#185205=CARTESIAN_POINT('Ctrl Pts',(10.6019848869999,11.6,-1.75176175100002));
#185206=CARTESIAN_POINT('Ctrl Pts',(10.5997069769999,15.2,-1.75068894800001));
#185207=CARTESIAN_POINT('Ctrl Pts',(10.5997069769999,11.6,-1.75068894800001));
#185208=CARTESIAN_POINT('Ctrl Pts',(10.5974336969999,15.2,-1.74962071100001));
#185209=CARTESIAN_POINT('Ctrl Pts',(10.5974336969999,11.6,-1.74962071100001));
#185210=CARTESIAN_POINT('Ctrl Pts',(10.5951650619999,15.2,-1.74855703600001));
#185211=CARTESIAN_POINT('Ctrl Pts',(10.5951650619999,11.6,-1.74855703600001));
#185212=CARTESIAN_POINT('Ctrl Pts',(10.5929010879999,15.2,-1.74749791900001));
#185213=CARTESIAN_POINT('Ctrl Pts',(10.5929010879999,11.6,-1.74749791900001));
#185214=CARTESIAN_POINT('Ctrl Pts',(10.5906417869999,15.2,-1.74644335800001));
#185215=CARTESIAN_POINT('Ctrl Pts',(10.5906417869999,11.6,-1.74644335800001));
#185216=CARTESIAN_POINT('Ctrl Pts',(10.5883871749999,15.2,-1.74539334800001));
#185217=CARTESIAN_POINT('Ctrl Pts',(10.5883871749999,11.6,-1.74539334800001));
#185218=CARTESIAN_POINT('Ctrl Pts',(10.5861372679999,15.2,-1.74434788600002));
#185219=CARTESIAN_POINT('Ctrl Pts',(10.5861372679999,11.6,-1.74434788600002));
#185220=CARTESIAN_POINT('Ctrl Pts',(10.5838920789999,15.2,-1.74330697000002));
#185221=CARTESIAN_POINT('Ctrl Pts',(10.5838920789999,11.6,-1.74330697000002));
#185222=CARTESIAN_POINT('Ctrl Pts',(10.5816516249999,15.2,-1.74227059600002));
#185223=CARTESIAN_POINT('Ctrl Pts',(10.5816516249999,11.6,-1.74227059600002));
#185224=CARTESIAN_POINT('Ctrl Pts',(10.5794159199999,15.2,-1.74123876000001));
#185225=CARTESIAN_POINT('Ctrl Pts',(10.5794159199999,11.6,-1.74123876000001));
#185226=CARTESIAN_POINT('Ctrl Pts',(10.5771849789999,15.2,-1.74021145700001));
#185227=CARTESIAN_POINT('Ctrl Pts',(10.5771849789999,11.6,-1.74021145700001));
#185228=CARTESIAN_POINT('Ctrl Pts',(10.5749588169999,15.2,-1.73918868600001));
#185229=CARTESIAN_POINT('Ctrl Pts',(10.5749588169999,11.6,-1.73918868600001));
#185230=CARTESIAN_POINT('Ctrl Pts',(10.5727374489999,15.2,-1.73817044400002));
#185231=CARTESIAN_POINT('Ctrl Pts',(10.5727374489999,11.6,-1.73817044400002));
#185232=CARTESIAN_POINT('Ctrl Pts',(10.5705208909999,15.2,-1.73715672500002));
#185233=CARTESIAN_POINT('Ctrl Pts',(10.5705208909999,11.6,-1.73715672500002));
#185234=CARTESIAN_POINT('Ctrl Pts',(10.5683091569999,15.2,-1.73614752600002));
#185235=CARTESIAN_POINT('Ctrl Pts',(10.5683091569999,11.6,-1.73614752600002));
#185236=CARTESIAN_POINT('Ctrl Pts',(10.5661022619999,15.2,-1.73514284500001));
#185237=CARTESIAN_POINT('Ctrl Pts',(10.5661022619999,11.6,-1.73514284500001));
#185238=CARTESIAN_POINT('Ctrl Pts',(10.5639002229999,15.2,-1.73414267600001));
#185239=CARTESIAN_POINT('Ctrl Pts',(10.5639002229999,11.6,-1.73414267600001));
#185240=CARTESIAN_POINT('Ctrl Pts',(10.5617030549999,15.2,-1.73314701800001));
#185241=CARTESIAN_POINT('Ctrl Pts',(10.5617030549999,11.6,-1.73314701800001));
#185242=CARTESIAN_POINT('Ctrl Pts',(10.5595107719999,15.2,-1.73215586600001));
#185243=CARTESIAN_POINT('Ctrl Pts',(10.5595107719999,11.6,-1.73215586600001));
#185244=CARTESIAN_POINT('Ctrl Pts',(10.5573233899999,15.2,-1.73116921600001));
#185245=CARTESIAN_POINT('Ctrl Pts',(10.5573233899999,11.6,-1.73116921600002));
#185246=CARTESIAN_POINT('Ctrl Pts',(10.5551409249999,15.2,-1.73018706400001));
#185247=CARTESIAN_POINT('Ctrl Pts',(10.5551409249999,11.6,-1.73018706400002));
#185248=CARTESIAN_POINT('Ctrl Pts',(10.5529633919999,15.2,-1.72920940800001));
#185249=CARTESIAN_POINT('Ctrl Pts',(10.5529633919999,11.6,-1.72920940800001));
#185250=CARTESIAN_POINT('Ctrl Pts',(10.5507908049999,15.2,-1.72823624300001));
#185251=CARTESIAN_POINT('Ctrl Pts',(10.5507908049999,11.6,-1.72823624300001));
#185252=CARTESIAN_POINT('Ctrl Pts',(10.5486231829999,15.2,-1.72726756600001));
#185253=CARTESIAN_POINT('Ctrl Pts',(10.5486231829999,11.6,-1.72726756600001));
#185254=CARTESIAN_POINT('Ctrl Pts',(10.5464605389999,15.2,-1.72630337200002));
#185255=CARTESIAN_POINT('Ctrl Pts',(10.5464605389999,11.6,-1.72630337200002));
#185256=CARTESIAN_POINT('Ctrl Pts',(10.5443028889999,15.2,-1.72534365700002));
#185257=CARTESIAN_POINT('Ctrl Pts',(10.5443028889999,11.6,-1.72534365700002));
#185258=CARTESIAN_POINT('Ctrl Pts',(10.5421502479999,15.2,-1.72438842000001));
#185259=CARTESIAN_POINT('Ctrl Pts',(10.5421502479999,11.6,-1.72438842000001));
#185260=CARTESIAN_POINT('Ctrl Pts',(10.5400026339999,15.2,-1.72343765400001));
#185261=CARTESIAN_POINT('Ctrl Pts',(10.5400026339999,11.6,-1.72343765400001));
#185262=CARTESIAN_POINT('Ctrl Pts',(10.5378600619999,15.2,-1.72249135700001));
#185263=CARTESIAN_POINT('Ctrl Pts',(10.5378600619999,11.6,-1.72249135700001));
#185264=CARTESIAN_POINT('Ctrl Pts',(10.5357225459999,15.2,-1.72154952500001));
#185265=CARTESIAN_POINT('Ctrl Pts',(10.5357225459999,11.6,-1.72154952500002));
#185266=CARTESIAN_POINT('Ctrl Pts',(10.5335901039999,15.2,-1.72061215300001));
#185267=CARTESIAN_POINT('Ctrl Pts',(10.5335901039999,11.6,-1.72061215300001));
#185268=CARTESIAN_POINT('Ctrl Pts',(10.5314627509999,15.2,-1.71967923800001));
#185269=CARTESIAN_POINT('Ctrl Pts',(10.5314627509999,11.6,-1.71967923800001));
#185270=CARTESIAN_POINT('Ctrl Pts',(10.5293405029999,15.2,-1.71875077500002));
#185271=CARTESIAN_POINT('Ctrl Pts',(10.5293405029999,11.6,-1.71875077500002));
#185272=CARTESIAN_POINT('Ctrl Pts',(10.5272233759999,15.2,-1.71782676100001));
#185273=CARTESIAN_POINT('Ctrl Pts',(10.5272233759999,11.6,-1.71782676100001));
#185274=CARTESIAN_POINT('Ctrl Pts',(10.5251113859999,15.2,-1.71690719200001));
#185275=CARTESIAN_POINT('Ctrl Pts',(10.5251113859999,11.6,-1.71690719200001));
#185276=CARTESIAN_POINT('Ctrl Pts',(10.5230045489999,15.2,-1.71599206300002));
#185277=CARTESIAN_POINT('Ctrl Pts',(10.5230045489999,11.6,-1.71599206300002));
#185278=CARTESIAN_POINT('Ctrl Pts',(10.5209028819999,15.2,-1.71508137300002));
#185279=CARTESIAN_POINT('Ctrl Pts',(10.5209028819999,11.6,-1.71508137300002));
#185280=CARTESIAN_POINT('Ctrl Pts',(10.5188063989999,15.2,-1.71417511400001));
#185281=CARTESIAN_POINT('Ctrl Pts',(10.5188063989999,11.6,-1.71417511400001));
#185282=CARTESIAN_POINT('Ctrl Pts',(10.5167151179999,15.2,-1.71327328300002));
#185283=CARTESIAN_POINT('Ctrl Pts',(10.5167151179999,11.6,-1.71327328300002));
#185284=CARTESIAN_POINT('Ctrl Pts',(10.5146290569999,15.2,-1.71237587700002));
#185285=CARTESIAN_POINT('Ctrl Pts',(10.5146290569999,11.6,-1.71237587700002));
#185286=CARTESIAN_POINT('Ctrl Pts',(10.5125482279999,15.2,-1.71148289200001));
#185287=CARTESIAN_POINT('Ctrl Pts',(10.5125482279999,11.6,-1.71148289200001));
#185288=CARTESIAN_POINT('Ctrl Pts',(10.5104726499999,15.2,-1.71059432200002));
#185289=CARTESIAN_POINT('Ctrl Pts',(10.5104726499999,11.6,-1.71059432200002));
#185290=CARTESIAN_POINT('Ctrl Pts',(10.5084023389999,15.2,-1.70971016400001));
#185291=CARTESIAN_POINT('Ctrl Pts',(10.5084023389999,11.6,-1.70971016400001));
#185292=CARTESIAN_POINT('Ctrl Pts',(10.5063373119999,15.2,-1.70883041400002));
#185293=CARTESIAN_POINT('Ctrl Pts',(10.5063373119999,11.6,-1.70883041400002));
#185294=CARTESIAN_POINT('Ctrl Pts',(10.5042775849999,15.2,-1.70795506700001));
#185295=CARTESIAN_POINT('Ctrl Pts',(10.5042775849999,11.6,-1.70795506700001));
#185296=CARTESIAN_POINT('Ctrl Pts',(10.5022231739999,15.2,-1.70708412100002));
#185297=CARTESIAN_POINT('Ctrl Pts',(10.5022231739999,11.6,-1.70708412100002));
#185298=CARTESIAN_POINT('Ctrl Pts',(10.5001740959999,15.2,-1.70621756800001));
#185299=CARTESIAN_POINT('Ctrl Pts',(10.5001740959999,11.6,-1.70621756800002));
#185300=CARTESIAN_POINT('Ctrl Pts',(10.4981303679999,15.2,-1.70535540700001));
#185301=CARTESIAN_POINT('Ctrl Pts',(10.4981303679999,11.6,-1.70535540700001));
#185302=CARTESIAN_POINT('Ctrl Pts',(10.4960920059999,15.2,-1.70449763100001));
#185303=CARTESIAN_POINT('Ctrl Pts',(10.4960920059999,11.6,-1.70449763100002));
#185304=CARTESIAN_POINT('Ctrl Pts',(10.4940590279999,15.2,-1.70364423800001));
#185305=CARTESIAN_POINT('Ctrl Pts',(10.4940590279999,11.6,-1.70364423800002));
#185306=CARTESIAN_POINT('Ctrl Pts',(10.4920314479999,15.2,-1.70279522300001));
#185307=CARTESIAN_POINT('Ctrl Pts',(10.4920314479999,11.6,-1.70279522300001));
#185308=CARTESIAN_POINT('Ctrl Pts',(10.4900092879999,15.2,-1.70195058100001));
#185309=CARTESIAN_POINT('Ctrl Pts',(10.4900092879999,11.6,-1.70195058100001));
#185310=CARTESIAN_POINT('Ctrl Pts',(10.4879925589999,15.2,-1.70111030700001));
#185311=CARTESIAN_POINT('Ctrl Pts',(10.4879925589999,11.6,-1.70111030700001));
#185312=CARTESIAN_POINT('Ctrl Pts',(10.4859812819999,15.2,-1.70027439800001));
#185313=CARTESIAN_POINT('Ctrl Pts',(10.4859812819999,11.6,-1.70027439800002));
#185314=CARTESIAN_POINT('Ctrl Pts',(10.4839754719999,15.2,-1.69944284800001));
#185315=CARTESIAN_POINT('Ctrl Pts',(10.4839754719999,11.6,-1.69944284800001));
#185316=CARTESIAN_POINT('Ctrl Pts',(10.4819751459999,15.2,-1.69861565400002));
#185317=CARTESIAN_POINT('Ctrl Pts',(10.4819751459999,11.6,-1.69861565400002));
#185318=CARTESIAN_POINT('Ctrl Pts',(10.4799803229999,15.2,-1.69779281100002));
#185319=CARTESIAN_POINT('Ctrl Pts',(10.4799803229999,11.6,-1.69779281100002));
#185320=CARTESIAN_POINT('Ctrl Pts',(10.4779910179999,15.2,-1.69697431400001));
#185321=CARTESIAN_POINT('Ctrl Pts',(10.4779910179999,11.6,-1.69697431400001));
#185322=CARTESIAN_POINT('Ctrl Pts',(10.4760072489999,15.2,-1.69616015900001));
#185323=CARTESIAN_POINT('Ctrl Pts',(10.4760072489999,11.6,-1.69616015900001));
#185324=CARTESIAN_POINT('Ctrl Pts',(10.4740290339999,15.2,-1.69535034000001));
#185325=CARTESIAN_POINT('Ctrl Pts',(10.4740290339999,11.6,-1.69535034000001));
#185326=CARTESIAN_POINT('Ctrl Pts',(10.4720563889999,15.2,-1.69454485500002));
#185327=CARTESIAN_POINT('Ctrl Pts',(10.4720563889999,11.6,-1.69454485500002));
#185328=CARTESIAN_POINT('Ctrl Pts',(10.4700893329999,15.2,-1.69374369700002));
#185329=CARTESIAN_POINT('Ctrl Pts',(10.4700893329999,11.6,-1.69374369700002));
#185330=CARTESIAN_POINT('Ctrl Pts',(10.4681278809999,15.2,-1.69294686200002));
#185331=CARTESIAN_POINT('Ctrl Pts',(10.4681278809999,11.6,-1.69294686200002));
#185332=CARTESIAN_POINT('Ctrl Pts',(10.4661720519999,15.2,-1.69215434500002));
#185333=CARTESIAN_POINT('Ctrl Pts',(10.4661720519999,11.6,-1.69215434500002));
#185334=CARTESIAN_POINT('Ctrl Pts',(10.4642218629999,15.2,-1.69136614200001));
#185335=CARTESIAN_POINT('Ctrl Pts',(10.4642218629999,11.6,-1.69136614200002));
#185336=CARTESIAN_POINT('Ctrl Pts',(10.4622773339999,15.2,-1.69058224900001));
#185337=CARTESIAN_POINT('Ctrl Pts',(10.4622773339999,11.6,-1.69058224900001));
#185338=CARTESIAN_POINT('Ctrl Pts',(10.4603384779999,15.2,-1.68980265900001));
#185339=CARTESIAN_POINT('Ctrl Pts',(10.4603384779999,11.6,-1.68980265900002));
#185340=CARTESIAN_POINT('Ctrl Pts',(10.4584053159999,15.2,-1.68902736800002));
#185341=CARTESIAN_POINT('Ctrl Pts',(10.4584053159999,11.6,-1.68902736800002));
#185342=CARTESIAN_POINT('Ctrl Pts',(10.4564778639999,15.2,-1.68825637300001));
#185343=CARTESIAN_POINT('Ctrl Pts',(10.4564778639999,11.6,-1.68825637300001));
#185344=CARTESIAN_POINT('Ctrl Pts',(10.4545561419999,15.2,-1.68748966700001));
#185345=CARTESIAN_POINT('Ctrl Pts',(10.4545561419999,11.6,-1.68748966700001));
#185346=CARTESIAN_POINT('Ctrl Pts',(10.4526401659999,15.2,-1.68672724400002));
#185347=CARTESIAN_POINT('Ctrl Pts',(10.4526401659999,11.6,-1.68672724400002));
#185348=CARTESIAN_POINT('Ctrl Pts',(10.4507299549999,15.2,-1.68596910300002));
#185349=CARTESIAN_POINT('Ctrl Pts',(10.4507299549999,11.6,-1.68596910300002));
#185350=CARTESIAN_POINT('Ctrl Pts',(10.4488255249999,15.2,-1.68521523500001));
#185351=CARTESIAN_POINT('Ctrl Pts',(10.4488255249999,11.6,-1.68521523500001));
#185352=CARTESIAN_POINT('Ctrl Pts',(10.4469268959999,15.2,-1.68446563800002));
#185353=CARTESIAN_POINT('Ctrl Pts',(10.4469268959999,11.6,-1.68446563800002));
#185354=CARTESIAN_POINT('Ctrl Pts',(10.4450340849999,15.2,-1.68372030600001));
#185355=CARTESIAN_POINT('Ctrl Pts',(10.4450340849999,11.6,-1.68372030600001));
#185356=CARTESIAN_POINT('Ctrl Pts',(10.4431471089999,15.2,-1.68297923300001));
#185357=CARTESIAN_POINT('Ctrl Pts',(10.4431471089999,11.6,-1.68297923300001));
#185358=CARTESIAN_POINT('Ctrl Pts',(10.4412659899999,15.2,-1.68224241600001));
#185359=CARTESIAN_POINT('Ctrl Pts',(10.4412659899999,11.6,-1.68224241600001));
#185360=CARTESIAN_POINT('Ctrl Pts',(10.4393907419999,15.2,-1.68150984700001));
#185361=CARTESIAN_POINT('Ctrl Pts',(10.4393907419999,11.6,-1.68150984700001));
#185362=CARTESIAN_POINT('Ctrl Pts',(10.4375213869999,15.2,-1.68078152300001));
#185363=CARTESIAN_POINT('Ctrl Pts',(10.4375213869999,11.6,-1.68078152300001));
#185364=CARTESIAN_POINT('Ctrl Pts',(10.4356579399999,15.2,-1.68005743800002));
#185365=CARTESIAN_POINT('Ctrl Pts',(10.4356579399999,11.6,-1.68005743800002));
#185366=CARTESIAN_POINT('Ctrl Pts',(10.4338004199999,15.2,-1.67933758800002));
#185367=CARTESIAN_POINT('Ctrl Pts',(10.4338004199999,11.6,-1.67933758800002));
#185368=CARTESIAN_POINT('Ctrl Pts',(10.4319488479999,15.2,-1.67862196700002));
#185369=CARTESIAN_POINT('Ctrl Pts',(10.4319488479999,11.6,-1.67862196700002));
#185370=CARTESIAN_POINT('Ctrl Pts',(10.4301032399999,15.2,-1.67791057000001));
#185371=CARTESIAN_POINT('Ctrl Pts',(10.4301032399999,11.6,-1.67791057000001));
#185372=CARTESIAN_POINT('Ctrl Pts',(10.4282636149999,15.2,-1.67720339000001));
#185373=CARTESIAN_POINT('Ctrl Pts',(10.4282636149999,11.6,-1.67720339000002));
#185374=CARTESIAN_POINT('Ctrl Pts',(10.4264299929999,15.2,-1.67650042400001));
#185375=CARTESIAN_POINT('Ctrl Pts',(10.4264299929999,11.6,-1.67650042400001));
#185376=CARTESIAN_POINT('Ctrl Pts',(10.4246023919999,15.2,-1.67580166600001));
#185377=CARTESIAN_POINT('Ctrl Pts',(10.4246023919999,11.6,-1.67580166600001));
#185378=CARTESIAN_POINT('Ctrl Pts',(10.4227808289999,15.2,-1.67510711000002));
#185379=CARTESIAN_POINT('Ctrl Pts',(10.4227808289999,11.6,-1.67510711000002));
#185380=CARTESIAN_POINT('Ctrl Pts',(10.4209653239999,15.2,-1.67441675200001));
#185381=CARTESIAN_POINT('Ctrl Pts',(10.4209653239999,11.6,-1.67441675200001));
#185382=CARTESIAN_POINT('Ctrl Pts',(10.4191558969999,15.2,-1.67373058500001));
#185383=CARTESIAN_POINT('Ctrl Pts',(10.4191558969999,11.6,-1.67373058500001));
#185384=CARTESIAN_POINT('Ctrl Pts',(10.4173525659999,15.2,-1.67304860400002));
#185385=CARTESIAN_POINT('Ctrl Pts',(10.4173525659999,11.6,-1.67304860400002));
#185386=CARTESIAN_POINT('Ctrl Pts',(10.4155553499999,15.2,-1.67237080400001));
#185387=CARTESIAN_POINT('Ctrl Pts',(10.4155553499999,11.6,-1.67237080400001));
#185388=CARTESIAN_POINT('Ctrl Pts',(10.4137642679999,15.2,-1.67169718000002));
#185389=CARTESIAN_POINT('Ctrl Pts',(10.4137642679999,11.6,-1.67169718000002));
#185390=CARTESIAN_POINT('Ctrl Pts',(10.4119793389999,15.2,-1.67102772400002));
#185391=CARTESIAN_POINT('Ctrl Pts',(10.4119793389999,11.6,-1.67102772400002));
#185392=CARTESIAN_POINT('Ctrl Pts',(10.4102005829999,15.2,-1.67036243400001));
#185393=CARTESIAN_POINT('Ctrl Pts',(10.4102005829999,11.6,-1.67036243400001));
#185394=CARTESIAN_POINT('Ctrl Pts',(10.4084280179999,15.2,-1.66970130200002));
#185395=CARTESIAN_POINT('Ctrl Pts',(10.4084280179999,11.6,-1.66970130200002));
#185396=CARTESIAN_POINT('Ctrl Pts',(10.4066616649999,15.2,-1.66904432200001));
#185397=CARTESIAN_POINT('Ctrl Pts',(10.4066616649999,11.6,-1.66904432200001));
#185398=CARTESIAN_POINT('Ctrl Pts',(10.4049015419999,15.2,-1.66839149000001));
#185399=CARTESIAN_POINT('Ctrl Pts',(10.4049015419999,11.6,-1.66839149000001));
#185400=CARTESIAN_POINT('Ctrl Pts',(10.4031476679999,15.2,-1.66774280000002));
#185401=CARTESIAN_POINT('Ctrl Pts',(10.4031476679999,11.6,-1.66774280000002));
#185402=CARTESIAN_POINT('Ctrl Pts',(10.4014000639999,15.2,-1.66709824500002));
#185403=CARTESIAN_POINT('Ctrl Pts',(10.4014000639999,11.6,-1.66709824500002));
#185404=CARTESIAN_POINT('Ctrl Pts',(10.3996587479999,15.2,-1.66645782000002));
#185405=CARTESIAN_POINT('Ctrl Pts',(10.3996587479999,11.6,-1.66645782000002));
#185406=CARTESIAN_POINT('Ctrl Pts',(10.3979237409999,15.2,-1.66582151900001));
#185407=CARTESIAN_POINT('Ctrl Pts',(10.3979237409999,11.6,-1.66582151900002));
#185408=CARTESIAN_POINT('Ctrl Pts',(10.3961950619999,15.2,-1.66518933700001));
#185409=CARTESIAN_POINT('Ctrl Pts',(10.3961950619999,11.6,-1.66518933700001));
#185410=CARTESIAN_POINT('Ctrl Pts',(10.3944727309999,15.2,-1.66456126800002));
#185411=CARTESIAN_POINT('Ctrl Pts',(10.3944727309999,11.6,-1.66456126800002));
#185412=CARTESIAN_POINT('Ctrl Pts',(10.3927567679999,15.2,-1.66393730500001));
#185413=CARTESIAN_POINT('Ctrl Pts',(10.3927567679999,11.6,-1.66393730500001));
#185414=CARTESIAN_POINT('Ctrl Pts',(10.3910471929999,15.2,-1.66331744300001));
#185415=CARTESIAN_POINT('Ctrl Pts',(10.3910471929999,11.6,-1.66331744300001));
#185416=CARTESIAN_POINT('Ctrl Pts',(10.3893440259999,15.2,-1.66270167600001));
#185417=CARTESIAN_POINT('Ctrl Pts',(10.3893440259999,11.6,-1.66270167600001));
#185418=CARTESIAN_POINT('Ctrl Pts',(10.3876472859999,15.2,-1.66208999800002));
#185419=CARTESIAN_POINT('Ctrl Pts',(10.3876472859999,11.6,-1.66208999800002));
#185420=CARTESIAN_POINT('Ctrl Pts',(10.3859569939999,15.2,-1.66148240200001));
#185421=CARTESIAN_POINT('Ctrl Pts',(10.3859569939999,11.6,-1.66148240200001));
#185422=CARTESIAN_POINT('Ctrl Pts',(10.3842731709999,15.2,-1.66087888300002));
#185423=CARTESIAN_POINT('Ctrl Pts',(10.3842731709999,11.6,-1.66087888300002));
#185424=CARTESIAN_POINT('Ctrl Pts',(10.3825958339999,15.2,-1.66027943500001));
#185425=CARTESIAN_POINT('Ctrl Pts',(10.3825958339999,11.6,-1.66027943500001));
#185426=CARTESIAN_POINT('Ctrl Pts',(10.3809250079999,15.2,-1.65968405100001));
#185427=CARTESIAN_POINT('Ctrl Pts',(10.3809250079999,11.6,-1.65968405100001));
#185428=CARTESIAN_POINT('Ctrl Pts',(10.3792607089999,15.2,-1.65909272500001));
#185429=CARTESIAN_POINT('Ctrl Pts',(10.3792607089999,11.6,-1.65909272500001));
#185430=CARTESIAN_POINT('Ctrl Pts',(10.3776029619999,15.2,-1.65850545200001));
#185431=CARTESIAN_POINT('Ctrl Pts',(10.3776029619999,11.6,-1.65850545200001));
#185432=CARTESIAN_POINT('Ctrl Pts',(10.3759517829999,15.2,-1.65792222500002));
#185433=CARTESIAN_POINT('Ctrl Pts',(10.3759517829999,11.6,-1.65792222500002));
#185434=CARTESIAN_POINT('Ctrl Pts',(10.3743071949999,15.2,-1.65734303700001));
#185435=CARTESIAN_POINT('Ctrl Pts',(10.3743071949999,11.6,-1.65734303700001));
#185436=CARTESIAN_POINT('Ctrl Pts',(10.3726692179999,15.2,-1.65676788300001));
#185437=CARTESIAN_POINT('Ctrl Pts',(10.3726692179999,11.6,-1.65676788300001));
#185438=CARTESIAN_POINT('Ctrl Pts',(10.3710378729999,15.2,-1.65619675500002));
#185439=CARTESIAN_POINT('Ctrl Pts',(10.3710378729999,11.6,-1.65619675500002));
#185440=CARTESIAN_POINT('Ctrl Pts',(10.3694131819999,15.2,-1.65562964900001));
#185441=CARTESIAN_POINT('Ctrl Pts',(10.3694131819999,11.6,-1.65562964900001));
#185442=CARTESIAN_POINT('Ctrl Pts',(10.3677951629999,15.2,-1.65506655600002));
#185443=CARTESIAN_POINT('Ctrl Pts',(10.3677951629999,11.6,-1.65506655600002));
#185444=CARTESIAN_POINT('Ctrl Pts',(10.3661838399999,15.2,-1.65450747100001));
#185445=CARTESIAN_POINT('Ctrl Pts',(10.3661838399999,11.6,-1.65450747100001));
#185446=CARTESIAN_POINT('Ctrl Pts',(10.3645792329999,15.2,-1.65395238800001));
#185447=CARTESIAN_POINT('Ctrl Pts',(10.3645792329999,11.6,-1.65395238800001));
#185448=CARTESIAN_POINT('Ctrl Pts',(10.3629813619999,15.2,-1.65340129900001));
#185449=CARTESIAN_POINT('Ctrl Pts',(10.3629813619999,11.6,-1.65340129900002));
#185450=CARTESIAN_POINT('Ctrl Pts',(10.3613902499999,15.2,-1.65285419800002));
#185451=CARTESIAN_POINT('Ctrl Pts',(10.3613902499999,11.6,-1.65285419800002));
#185452=CARTESIAN_POINT('Ctrl Pts',(10.3598059159999,15.2,-1.65231108000001));
#185453=CARTESIAN_POINT('Ctrl Pts',(10.3598059159999,11.6,-1.65231108000001));
#185454=CARTESIAN_POINT('Ctrl Pts',(10.3582283849999,15.2,-1.65177193600002));
#185455=CARTESIAN_POINT('Ctrl Pts',(10.3582283849999,11.6,-1.65177193600002));
#185456=CARTESIAN_POINT('Ctrl Pts',(10.3566576739999,15.2,-1.65123676100002));
#185457=CARTESIAN_POINT('Ctrl Pts',(10.3566576739999,11.6,-1.65123676100002));
#185458=CARTESIAN_POINT('Ctrl Pts',(10.3550938079999,15.2,-1.65070554700002));
#185459=CARTESIAN_POINT('Ctrl Pts',(10.3550938079999,11.6,-1.65070554700002));
#185460=CARTESIAN_POINT('Ctrl Pts',(10.3535368059999,15.2,-1.65017828800002));
#185461=CARTESIAN_POINT('Ctrl Pts',(10.3535368059999,11.6,-1.65017828800002));
#185462=CARTESIAN_POINT('Ctrl Pts',(10.3519866919999,15.2,-1.64965497700001));
#185463=CARTESIAN_POINT('Ctrl Pts',(10.3519866919999,11.6,-1.64965497700001));
#185464=CARTESIAN_POINT('Ctrl Pts',(10.3504434859999,15.2,-1.64913560700001));
#185465=CARTESIAN_POINT('Ctrl Pts',(10.3504434859999,11.6,-1.64913560700001));
#185466=CARTESIAN_POINT('Ctrl Pts',(10.3489072109999,15.2,-1.64862017200001));
#185467=CARTESIAN_POINT('Ctrl Pts',(10.3489072109999,11.6,-1.64862017200001));
#185468=CARTESIAN_POINT('Ctrl Pts',(10.3473778879999,15.2,-1.64810866500002));
#185469=CARTESIAN_POINT('Ctrl Pts',(10.3473778879999,11.6,-1.64810866500002));
#185470=CARTESIAN_POINT('Ctrl Pts',(10.3458555399999,15.2,-1.64760107700001));
#185471=CARTESIAN_POINT('Ctrl Pts',(10.3458555399999,11.6,-1.64760107700001));
#185472=CARTESIAN_POINT('Ctrl Pts',(10.3443401869999,15.2,-1.64709740400002));
#185473=CARTESIAN_POINT('Ctrl Pts',(10.3443401869999,11.6,-1.64709740400002));
#185474=CARTESIAN_POINT('Ctrl Pts',(10.3428318549999,15.2,-1.64659763700001));
#185475=CARTESIAN_POINT('Ctrl Pts',(10.3428318549999,11.6,-1.64659763700001));
#185476=CARTESIAN_POINT('Ctrl Pts',(10.3413305619999,15.2,-1.64610176900001));
#185477=CARTESIAN_POINT('Ctrl Pts',(10.3413305619999,11.6,-1.64610176900002));
#185478=CARTESIAN_POINT('Ctrl Pts',(10.3398363339999,15.2,-1.64560979500001));
#185479=CARTESIAN_POINT('Ctrl Pts',(10.3398363339999,11.6,-1.64560979500001));
#185480=CARTESIAN_POINT('Ctrl Pts',(10.3383491889999,15.2,-1.64512170500001));
#185481=CARTESIAN_POINT('Ctrl Pts',(10.3383491889999,11.6,-1.64512170500001));
#185482=CARTESIAN_POINT('Ctrl Pts',(10.3368691539999,15.2,-1.64463749400001));
#185483=CARTESIAN_POINT('Ctrl Pts',(10.3368691539999,11.6,-1.64463749400001));
#185484=CARTESIAN_POINT('Ctrl Pts',(10.3353962489999,15.2,-1.64415715300001));
#185485=CARTESIAN_POINT('Ctrl Pts',(10.3353962489999,11.6,-1.64415715300001));
#185486=CARTESIAN_POINT('Ctrl Pts',(10.3339304969999,15.2,-1.64368067500002));
#185487=CARTESIAN_POINT('Ctrl Pts',(10.3339304969999,11.6,-1.64368067500002));
#185488=CARTESIAN_POINT('Ctrl Pts',(10.3324719229999,15.2,-1.64320805500001));
#185489=CARTESIAN_POINT('Ctrl Pts',(10.3324719229999,11.6,-1.64320805500001));
#185490=CARTESIAN_POINT('Ctrl Pts',(10.3310205459999,15.2,-1.64273928400001));
#185491=CARTESIAN_POINT('Ctrl Pts',(10.3310205459999,11.6,-1.64273928400001));
#185492=CARTESIAN_POINT('Ctrl Pts',(10.3295763909999,15.2,-1.64227435400001));
#185493=CARTESIAN_POINT('Ctrl Pts',(10.3295763909999,11.6,-1.64227435400001));
#185494=CARTESIAN_POINT('Ctrl Pts',(10.3281394819999,15.2,-1.64181325700001));
#185495=CARTESIAN_POINT('Ctrl Pts',(10.3281394819999,11.6,-1.64181325700001));
#185496=CARTESIAN_POINT('Ctrl Pts',(10.3267098399999,15.2,-1.64135598800002));
#185497=CARTESIAN_POINT('Ctrl Pts',(10.3267098399999,11.6,-1.64135598800002));
#185498=CARTESIAN_POINT('Ctrl Pts',(10.3252874889999,15.2,-1.64090253800001));
#185499=CARTESIAN_POINT('Ctrl Pts',(10.3252874889999,11.6,-1.64090253800001));
#185500=CARTESIAN_POINT('Ctrl Pts',(10.3238724529999,15.2,-1.64045290000002));
#185501=CARTESIAN_POINT('Ctrl Pts',(10.3238724529999,11.6,-1.64045290000002));
#185502=CARTESIAN_POINT('Ctrl Pts',(10.3224647549999,15.2,-1.64000706600001));
#185503=CARTESIAN_POINT('Ctrl Pts',(10.3224647549999,11.6,-1.64000706600001));
#185504=CARTESIAN_POINT('Ctrl Pts',(10.3210644169999,15.2,-1.63956502700001));
#185505=CARTESIAN_POINT('Ctrl Pts',(10.3210644169999,11.6,-1.63956502700001));
#185506=CARTESIAN_POINT('Ctrl Pts',(10.3196714649999,15.2,-1.63912677800001));
#185507=CARTESIAN_POINT('Ctrl Pts',(10.3196714649999,11.6,-1.63912677800001));
#185508=CARTESIAN_POINT('Ctrl Pts',(10.3182859209999,15.2,-1.63869230900001));
#185509=CARTESIAN_POINT('Ctrl Pts',(10.3182859209999,11.6,-1.63869230900001));
#185510=CARTESIAN_POINT('Ctrl Pts',(10.3169078099999,15.2,-1.63826161400001));
#185511=CARTESIAN_POINT('Ctrl Pts',(10.3169078099999,11.6,-1.63826161400001));
#185512=CARTESIAN_POINT('Ctrl Pts',(10.3155371549999,15.2,-1.63783468500001));
#185513=CARTESIAN_POINT('Ctrl Pts',(10.3155371549999,11.6,-1.63783468500002));
#185514=CARTESIAN_POINT('Ctrl Pts',(10.3141739779999,15.2,-1.63741151200002));
#185515=CARTESIAN_POINT('Ctrl Pts',(10.3141739779999,11.6,-1.63741151200002));
#185516=CARTESIAN_POINT('Ctrl Pts',(10.3128183069999,15.2,-1.63699208900002));
#185517=CARTESIAN_POINT('Ctrl Pts',(10.3128183069999,11.6,-1.63699208900002));
#185518=CARTESIAN_POINT('Ctrl Pts',(10.3114701629999,15.2,-1.63657640900002));
#185519=CARTESIAN_POINT('Ctrl Pts',(10.3114701629999,11.6,-1.63657640900002));
#185520=CARTESIAN_POINT('Ctrl Pts',(10.3101295719999,15.2,-1.63616446000002));
#185521=CARTESIAN_POINT('Ctrl Pts',(10.3101295719999,11.6,-1.63616446000002));
#185522=CARTESIAN_POINT('Ctrl Pts',(10.3087965579999,15.2,-1.63575623800002));
#185523=CARTESIAN_POINT('Ctrl Pts',(10.3087965579999,11.6,-1.63575623800002));
#185524=CARTESIAN_POINT('Ctrl Pts',(10.3074711439999,15.2,-1.63535173400001));
#185525=CARTESIAN_POINT('Ctrl Pts',(10.3074711439999,11.6,-1.63535173400001));
#185526=CARTESIAN_POINT('Ctrl Pts',(10.3061533569999,15.2,-1.63495093800002));
#185527=CARTESIAN_POINT('Ctrl Pts',(10.3061533569999,11.6,-1.63495093800002));
#185528=CARTESIAN_POINT('Ctrl Pts',(10.3048432199999,15.2,-1.63455384400002));
#185529=CARTESIAN_POINT('Ctrl Pts',(10.3048432199999,11.6,-1.63455384400002));
#185530=CARTESIAN_POINT('Ctrl Pts',(10.3035407569999,15.2,-1.63416044200002));
#185531=CARTESIAN_POINT('Ctrl Pts',(10.3035407569999,11.6,-1.63416044200002));
#185532=CARTESIAN_POINT('Ctrl Pts',(10.3022459949999,15.2,-1.63377072600001));
#185533=CARTESIAN_POINT('Ctrl Pts',(10.3022459949999,11.6,-1.63377072600001));
#185534=CARTESIAN_POINT('Ctrl Pts',(10.3009589569999,15.2,-1.63338468500001));
#185535=CARTESIAN_POINT('Ctrl Pts',(10.3009589569999,11.6,-1.63338468500001));
#185536=CARTESIAN_POINT('Ctrl Pts',(10.2996796679999,15.2,-1.63300231200001));
#185537=CARTESIAN_POINT('Ctrl Pts',(10.2996796679999,11.6,-1.63300231200001));
#185538=CARTESIAN_POINT('Ctrl Pts',(10.2984081549999,15.2,-1.63262359900001));
#185539=CARTESIAN_POINT('Ctrl Pts',(10.2984081549999,11.6,-1.63262359900001));
#185540=CARTESIAN_POINT('Ctrl Pts',(10.2971444419999,15.2,-1.63224853600001));
#185541=CARTESIAN_POINT('Ctrl Pts',(10.2971444419999,11.6,-1.63224853600001));
#185542=CARTESIAN_POINT('Ctrl Pts',(10.2958885549999,15.2,-1.63187711700001));
#185543=CARTESIAN_POINT('Ctrl Pts',(10.2958885549999,11.6,-1.63187711700001));
#185544=CARTESIAN_POINT('Ctrl Pts',(10.2946405169999,15.2,-1.63150933000002));
#185545=CARTESIAN_POINT('Ctrl Pts',(10.2946405169999,11.6,-1.63150933000002));
#185546=CARTESIAN_POINT('Ctrl Pts',(10.2934003569999,15.2,-1.63114516800002));
#185547=CARTESIAN_POINT('Ctrl Pts',(10.2934003569999,11.6,-1.63114516800002));
#185548=CARTESIAN_POINT('Ctrl Pts',(10.2921680989999,15.2,-1.63078462400001));
#185549=CARTESIAN_POINT('Ctrl Pts',(10.2921680989999,11.6,-1.63078462400002));
#185550=CARTESIAN_POINT('Ctrl Pts',(10.2909437679999,15.2,-1.63042768700001));
#185551=CARTESIAN_POINT('Ctrl Pts',(10.2909437679999,11.6,-1.63042768700001));
#185552=CARTESIAN_POINT('Ctrl Pts',(10.2897273919999,15.2,-1.63007434800001));
#185553=CARTESIAN_POINT('Ctrl Pts',(10.2897273919999,11.6,-1.63007434800001));
#185554=CARTESIAN_POINT('Ctrl Pts',(10.2885189949999,15.2,-1.62972460000002));
#185555=CARTESIAN_POINT('Ctrl Pts',(10.2885189949999,11.6,-1.62972460000002));
#185556=CARTESIAN_POINT('Ctrl Pts',(10.2873186039999,15.2,-1.62937843300002));
#185557=CARTESIAN_POINT('Ctrl Pts',(10.2873186039999,11.6,-1.62937843300002));
#185558=CARTESIAN_POINT('Ctrl Pts',(10.2861262449999,15.2,-1.62903583900002));
#185559=CARTESIAN_POINT('Ctrl Pts',(10.2861262449999,11.6,-1.62903583900002));
#185560=CARTESIAN_POINT('Ctrl Pts',(10.2849419449999,15.2,-1.62869680700001));
#185561=CARTESIAN_POINT('Ctrl Pts',(10.2849419449999,11.6,-1.62869680700001));
#185562=CARTESIAN_POINT('Ctrl Pts',(10.2837657299999,15.2,-1.62836132900001));
#185563=CARTESIAN_POINT('Ctrl Pts',(10.2837657299999,11.6,-1.62836132900001));
#185564=CARTESIAN_POINT('Ctrl Pts',(10.2825976249999,15.2,-1.62802939700001));
#185565=CARTESIAN_POINT('Ctrl Pts',(10.2825976249999,11.6,-1.62802939700002));
#185566=CARTESIAN_POINT('Ctrl Pts',(10.2814376589999,15.2,-1.62770100000001));
#185567=CARTESIAN_POINT('Ctrl Pts',(10.2814376589999,11.6,-1.62770100000001));
#185568=CARTESIAN_POINT('Ctrl Pts',(10.2802858579999,15.2,-1.62737613100001));
#185569=CARTESIAN_POINT('Ctrl Pts',(10.2802858579999,11.6,-1.62737613100001));
#185570=CARTESIAN_POINT('Ctrl Pts',(10.2791422489999,15.2,-1.62705477900001));
#185571=CARTESIAN_POINT('Ctrl Pts',(10.2791422489999,11.6,-1.62705477900001));
#185572=CARTESIAN_POINT('Ctrl Pts',(10.2780068579999,15.2,-1.62673693400002));
#185573=CARTESIAN_POINT('Ctrl Pts',(10.2780068579999,11.6,-1.62673693400002));
#185574=CARTESIAN_POINT('Ctrl Pts',(10.2768797139999,15.2,-1.62642258900001));
#185575=CARTESIAN_POINT('Ctrl Pts',(10.2768797139999,11.6,-1.62642258900001));
#185576=CARTESIAN_POINT('Ctrl Pts',(10.2757608429999,15.2,-1.62611173200002));
#185577=CARTESIAN_POINT('Ctrl Pts',(10.2757608429999,11.6,-1.62611173200002));
#185578=CARTESIAN_POINT('Ctrl Pts',(10.2746502719999,15.2,-1.62580435500002));
#185579=CARTESIAN_POINT('Ctrl Pts',(10.2746502719999,11.6,-1.62580435500002));
#185580=CARTESIAN_POINT('Ctrl Pts',(10.2735480289999,15.2,-1.62550044900001));
#185581=CARTESIAN_POINT('Ctrl Pts',(10.2735480289999,11.6,-1.62550044900002));
#185582=CARTESIAN_POINT('Ctrl Pts',(10.2724541419999,15.2,-1.62520000200002));
#185583=CARTESIAN_POINT('Ctrl Pts',(10.2724541419999,11.6,-1.62520000200002));
#185584=CARTESIAN_POINT('Ctrl Pts',(10.2713686389999,15.2,-1.62490300700001));
#185585=CARTESIAN_POINT('Ctrl Pts',(10.2713686389999,11.6,-1.62490300700001));
#185586=CARTESIAN_POINT('Ctrl Pts',(10.2702915479999,15.2,-1.62460945400001));
#185587=CARTESIAN_POINT('Ctrl Pts',(10.2702915479999,11.6,-1.62460945400001));
#185588=CARTESIAN_POINT('Ctrl Pts',(10.2692228959999,15.2,-1.62431933100001));
#185589=CARTESIAN_POINT('Ctrl Pts',(10.2692228959999,11.6,-1.62431933100002));
#185590=CARTESIAN_POINT('Ctrl Pts',(10.2681627099999,15.2,-1.62403262900002));
#185591=CARTESIAN_POINT('Ctrl Pts',(10.2681627099999,11.6,-1.62403262900002));
#185592=CARTESIAN_POINT('Ctrl Pts',(10.2671110219999,15.2,-1.62374934000002));
#185593=CARTESIAN_POINT('Ctrl Pts',(10.2671110219999,11.6,-1.62374934000002));
#185594=CARTESIAN_POINT('Ctrl Pts',(10.2660678569999,15.2,-1.62346945200001));
#185595=CARTESIAN_POINT('Ctrl Pts',(10.2660678569999,11.6,-1.62346945200001));
#185596=CARTESIAN_POINT('Ctrl Pts',(10.2650332449999,15.2,-1.62319295600001));
#185597=CARTESIAN_POINT('Ctrl Pts',(10.2650332449999,11.6,-1.62319295600002));
#185598=CARTESIAN_POINT('Ctrl Pts',(10.2640072149999,15.2,-1.62291984100001));
#185599=CARTESIAN_POINT('Ctrl Pts',(10.2640072149999,11.6,-1.62291984100001));
#185600=CARTESIAN_POINT('Ctrl Pts',(10.2629897939999,15.2,-1.62265009700001));
#185601=CARTESIAN_POINT('Ctrl Pts',(10.2629897939999,11.6,-1.62265009700001));
#185602=CARTESIAN_POINT('Ctrl Pts',(10.2619810129999,15.2,-1.62238371500001));
#185603=CARTESIAN_POINT('Ctrl Pts',(10.2619810129999,11.6,-1.62238371500001));
#185604=CARTESIAN_POINT('Ctrl Pts',(10.2609808999999,15.2,-1.62212068400001));
#185605=CARTESIAN_POINT('Ctrl Pts',(10.2609808999999,11.6,-1.62212068400002));
#185606=CARTESIAN_POINT('Ctrl Pts',(10.2599894849999,15.2,-1.62186099200001));
#185607=CARTESIAN_POINT('Ctrl Pts',(10.2599894849999,11.6,-1.62186099200001));
#185608=CARTESIAN_POINT('Ctrl Pts',(10.2590067959999,15.2,-1.62160463100002));
#185609=CARTESIAN_POINT('Ctrl Pts',(10.2590067959999,11.6,-1.62160463100002));
#185610=CARTESIAN_POINT('Ctrl Pts',(10.2580328639999,15.2,-1.62135159000002));
#185611=CARTESIAN_POINT('Ctrl Pts',(10.2580328639999,11.6,-1.62135159000002));
#185612=CARTESIAN_POINT('Ctrl Pts',(10.2570677169999,15.2,-1.62110185800001));
#185613=CARTESIAN_POINT('Ctrl Pts',(10.2570677169999,11.6,-1.62110185800001));
#185614=CARTESIAN_POINT('Ctrl Pts',(10.2561113859999,15.2,-1.62085542400002));
#185615=CARTESIAN_POINT('Ctrl Pts',(10.2561113859999,11.6,-1.62085542400002));
#185616=CARTESIAN_POINT('Ctrl Pts',(10.2551638999999,15.2,-1.62061227900002));
#185617=CARTESIAN_POINT('Ctrl Pts',(10.2551638999999,11.6,-1.62061227900002));
#185618=CARTESIAN_POINT('Ctrl Pts',(10.2542252899999,15.2,-1.62037241000001));
#185619=CARTESIAN_POINT('Ctrl Pts',(10.2542252899999,11.6,-1.62037241000002));
#185620=CARTESIAN_POINT('Ctrl Pts',(10.2532955859999,15.2,-1.62013580700001));
#185621=CARTESIAN_POINT('Ctrl Pts',(10.2532955859999,11.6,-1.62013580700001));
#185622=CARTESIAN_POINT('Ctrl Pts',(10.2523748169999,15.2,-1.61990246000002));
#185623=CARTESIAN_POINT('Ctrl Pts',(10.2523748169999,11.6,-1.61990246000002));
#185624=CARTESIAN_POINT('Ctrl Pts',(10.2514630149999,15.2,-1.61967235800001));
#185625=CARTESIAN_POINT('Ctrl Pts',(10.2514630149999,11.6,-1.61967235800002));
#185626=CARTESIAN_POINT('Ctrl Pts',(10.2505602109999,15.2,-1.61944548900002));
#185627=CARTESIAN_POINT('Ctrl Pts',(10.2505602109999,11.6,-1.61944548900002));
#185628=CARTESIAN_POINT('Ctrl Pts',(10.2496715819999,15.2,-1.61922313000002));
#185629=CARTESIAN_POINT('Ctrl Pts',(10.2496715819999,11.6,-1.61922313000002));
#185630=CARTESIAN_POINT('Ctrl Pts',(10.2489688509999,15.2,-1.61904803300001));
#185631=CARTESIAN_POINT('Ctrl Pts',(10.2489688509999,11.6,-1.61904803300001));
#185632=CARTESIAN_POINT('Ctrl Pts',(10.2484470889999,15.2,-1.61891844100001));
#185633=CARTESIAN_POINT('Ctrl Pts',(10.2484470889999,11.6,-1.61891844100001));
#185634=CARTESIAN_POINT('Ctrl Pts',(10.2481027029999,15.2,-1.61883308400002));
#185635=CARTESIAN_POINT('Ctrl Pts',(10.2481027029999,11.6,-1.61883308400002));
#185636=CARTESIAN_POINT('Ctrl Pts',(10.2479334559999,15.2,-1.61879118000002));
#185637=CARTESIAN_POINT('Ctrl Pts',(10.2479334559999,11.6,-1.61879118000002));
#185638=CARTESIAN_POINT('',(10.2479334559999,12.2,-1.61879118000002));
#185639=CARTESIAN_POINT('',(10.2479334559999,15.2,-1.61879118000002));
#185640=CARTESIAN_POINT('',(10.2479334559999,12.2,-1.61879118000002));
#185641=CARTESIAN_POINT('Ctrl Pts',(11.2922242989999,12.2,-2.17615954700001));
#185642=CARTESIAN_POINT('Ctrl Pts',(11.2891672434446,12.2,-2.17386408658301));
#185643=CARTESIAN_POINT('Ctrl Pts',(11.2861128828178,12.2,-2.17157605041022));
#185644=CARTESIAN_POINT('Ctrl Pts',(11.2830612235708,12.2,-2.16929543995597));
#185645=CARTESIAN_POINT('Ctrl Pts',(11.2800095643238,12.2,-2.16701482950172));
#185646=CARTESIAN_POINT('Ctrl Pts',(11.2769606036145,12.2,-2.16474164385347));
#185647=CARTESIAN_POINT('Ctrl Pts',(11.2739143610727,12.2,-2.16247588328007));
#185648=CARTESIAN_POINT('Ctrl Pts',(11.2708681185308,12.2,-2.16021012270667));
#185649=CARTESIAN_POINT('Ctrl Pts',(11.2678245931694,12.2,-2.15795178692656));
#185650=CARTESIAN_POINT('Ctrl Pts',(11.2647838291545,12.2,-2.15570087596567));
#185651=CARTESIAN_POINT('Ctrl Pts',(11.2617430645872,12.2,-2.15344996459586));
#185652=CARTESIAN_POINT('Ctrl Pts',(11.2587050621956,12.2,-2.15120647715313));
#185653=CARTESIAN_POINT('Ctrl Pts',(11.2556698710466,12.2,-2.14897041128751));
#185654=CARTESIAN_POINT('Ctrl Pts',(11.2526346804489,12.2,-2.1467343458281));
#185655=CARTESIAN_POINT('Ctrl Pts',(11.2496023012261,12.2,-2.14450570232663));
#185656=CARTESIAN_POINT('Ctrl Pts',(11.2465727734614,12.2,-2.14228448028298));
#185657=CARTESIAN_POINT('Ctrl Pts',(11.2435432456967,12.2,-2.14006325823933));
#185658=CARTESIAN_POINT('Ctrl Pts',(11.2405165681844,12.2,-2.13784945607778));
#185659=CARTESIAN_POINT('Ctrl Pts',(11.2374927780305,12.2,-2.13564307406463));
#185660=CARTESIAN_POINT('Ctrl Pts',(11.2334610580085,12.2,-2.13270123151403));
#185661=CARTESIAN_POINT('Ctrl Pts',(11.2294344705125,12.2,-2.12977257764798));
#185662=CARTESIAN_POINT('Ctrl Pts',(11.2254131171741,12.2,-2.12685711171831));
#185663=CARTESIAN_POINT('Ctrl Pts',(11.2223971014853,12.2,-2.12467051177452));
#185664=CARTESIAN_POINT('Ctrl Pts',(11.2193840292308,12.2,-2.12249132815782));
#185665=CARTESIAN_POINT('Ctrl Pts',(11.2163739430854,12.2,-2.12031956030152));
#185666=CARTESIAN_POINT('Ctrl Pts',(11.2133638574868,12.2,-2.11814779283977));
#185667=CARTESIAN_POINT('Ctrl Pts',(11.2103567582631,12.2,-2.11598344095264));
#185668=CARTESIAN_POINT('Ctrl Pts',(11.2073526851642,12.2,-2.11382650248998));
#185669=CARTESIAN_POINT('Ctrl Pts',(11.2043486120653,12.2,-2.11166956402733));
#185670=CARTESIAN_POINT('Ctrl Pts',(11.2013475658352,12.2,-2.10952003876322));
#185671=CARTESIAN_POINT('Ctrl Pts',(11.1983495872639,12.2,-2.10737792524802));
#185672=CARTESIAN_POINT('Ctrl Pts',(11.1953516086925,12.2,-2.10523581173282));
#185673=CARTESIAN_POINT('Ctrl Pts',(11.1923566985575,12.2,-2.10310110905096));
#185674=CARTESIAN_POINT('Ctrl Pts',(11.189364898486,12.2,-2.10097381699356));
#185675=CARTESIAN_POINT('Ctrl Pts',(11.1863730984144,12.2,-2.09884652493616));
#185676=CARTESIAN_POINT('Ctrl Pts',(11.1833844089172,12.2,-2.09672664170424));
#185677=CARTESIAN_POINT('Ctrl Pts',(11.1803988718171,12.2,-2.09461416573868));
#185678=CARTESIAN_POINT('Ctrl Pts',(11.1774133347169,12.2,-2.09250168977312));
#185679=CARTESIAN_POINT('Ctrl Pts',(11.1744309502416,12.2,-2.09039662064872));
#185680=CARTESIAN_POINT('Ctrl Pts',(11.1714517601411,12.2,-2.08829895714059));
#185681=CARTESIAN_POINT('Ctrl Pts',(11.1684725694993,12.2,-2.08620129325139));
#185682=CARTESIAN_POINT('Ctrl Pts',(11.1654965735335,12.2,-2.08411103414762));
#185683=CARTESIAN_POINT('Ctrl Pts',(11.1625238148519,12.2,-2.08202817730424));
#185684=CARTESIAN_POINT('Ctrl Pts',(11.1595510567103,12.2,-2.07994532083926));
#185685=CARTESIAN_POINT('Ctrl Pts',(11.1565815351994,12.2,-2.07786986734391));
#185686=CARTESIAN_POINT('Ctrl Pts',(11.1536152939511,12.2,-2.07580181285825));
#185687=CARTESIAN_POINT('Ctrl Pts',(11.1506490527027,12.2,-2.07373375837259));
#185688=CARTESIAN_POINT('Ctrl Pts',(11.1476860917529,12.2,-2.0716731043677));
#185689=CARTESIAN_POINT('Ctrl Pts',(11.1447264536524,12.2,-2.06961984698462));
#185690=CARTESIAN_POINT('Ctrl Pts',(11.1417668155519,12.2,-2.06756658960153));
#185691=CARTESIAN_POINT('Ctrl Pts',(11.1388105006593,12.2,-2.0655207303759));
#185692=CARTESIAN_POINT('Ctrl Pts',(11.1358575515583,12.2,-2.06348226449162));
#185693=CARTESIAN_POINT('Ctrl Pts',(11.1329046024572,12.2,-2.06144379860735));
#185694=CARTESIAN_POINT('Ctrl Pts',(11.1299550190977,12.2,-2.05941272813111));
#185695=CARTESIAN_POINT('Ctrl Pts',(11.1270088455794,12.2,-2.057389048204));
#185696=CARTESIAN_POINT('Ctrl Pts',(11.1240626720612,12.2,-2.05536536827689));
#185697=CARTESIAN_POINT('Ctrl Pts',(11.1211199089177,12.2,-2.05334908044925));
#185698=CARTESIAN_POINT('Ctrl Pts',(11.1181805983574,12.2,-2.05134018047958));
#185699=CARTESIAN_POINT('Ctrl Pts',(11.115241287263,12.2,-2.04933128014495));
#185700=CARTESIAN_POINT('Ctrl Pts',(11.1123054290197,12.2,-2.04732976760407));
#185701=CARTESIAN_POINT('Ctrl Pts',(11.109373068344,12.2,-2.04533564077359));
#185702=CARTESIAN_POINT('Ctrl Pts',(11.106440708201,12.2,-2.04334151430537));
#185703=CARTESIAN_POINT('Ctrl Pts',(11.1035118444734,12.2,-2.04135477375985));
#185704=CARTESIAN_POINT('Ctrl Pts',(11.100586522684,12.2,-2.03937541465041));
#185705=CARTESIAN_POINT('Ctrl Pts',(11.0976612008945,12.2,-2.03739605554096));
#185706=CARTESIAN_POINT('Ctrl Pts',(11.0947394202922,12.2,-2.03542407828059));
#185707=CARTESIAN_POINT('Ctrl Pts',(11.0918212251902,12.2,-2.03345947931095));
#185708=CARTESIAN_POINT('Ctrl Pts',(11.0889030300882,12.2,-2.0314948803413));
#185709=CARTESIAN_POINT('Ctrl Pts',(11.0859884198275,12.2,-2.02953765971245));
#185710=CARTESIAN_POINT('Ctrl Pts',(11.0830774402249,12.2,-2.02758781424162));
#185711=CARTESIAN_POINT('Ctrl Pts',(11.0801664606223,12.2,-2.0256379687708));
#185712=CARTESIAN_POINT('Ctrl Pts',(11.0772591111946,12.2,-2.02369549840801));
#185713=CARTESIAN_POINT('Ctrl Pts',(11.0743554365915,12.2,-2.02176039893602));
#185714=CARTESIAN_POINT('Ctrl Pts',(11.0714517619883,12.2,-2.01982529946402));
#185715=CARTESIAN_POINT('Ctrl Pts',(11.0685517618502,12.2,-2.01789757206525));
#185716=CARTESIAN_POINT('Ctrl Pts',(11.0656554825603,12.2,-2.01597721191324));
#185717=CARTESIAN_POINT('Ctrl Pts',(11.0627592032704,12.2,-2.01405685176123));
#185718=CARTESIAN_POINT('Ctrl Pts',(11.0598666428919,12.2,-2.0121438583805));
#185719=CARTESIAN_POINT('Ctrl Pts',(11.0569778483713,12.2,-2.01023822844873));
#185720=CARTESIAN_POINT('Ctrl Pts',(11.054089053326,12.2,-2.00833259817078));
#185721=CARTESIAN_POINT('Ctrl Pts',(11.0512040246067,12.2,-2.00643433216156));
#185722=CARTESIAN_POINT('Ctrl Pts',(11.0483228056052,12.2,-2.00454342530442));
#185723=CARTESIAN_POINT('Ctrl Pts',(11.0444811811421,12.2,-2.00202221673409));
#185724=CARTESIAN_POINT('Ctrl Pts',(11.0406463315365,12.2,-1.99951409062871));
#185725=CARTESIAN_POINT('Ctrl Pts',(11.0368183655713,12.2,-1.99701903872073));
#185726=CARTESIAN_POINT('Ctrl Pts',(11.0339473909669,12.2,-1.99514774970476));
#185727=CARTESIAN_POINT('Ctrl Pts',(11.0310802880101,12.2,-1.99328381496872));
#185728=CARTESIAN_POINT('Ctrl Pts',(11.0282171033456,12.2,-1.99142722890091));
#185729=CARTESIAN_POINT('Ctrl Pts',(11.0253539186811,12.2,-1.9895706428331));
#185730=CARTESIAN_POINT('Ctrl Pts',(11.0224946528025,12.2,-1.98772140635225));
#185731=CARTESIAN_POINT('Ctrl Pts',(11.019639350364,12.2,-1.98587951441817));
#185732=CARTESIAN_POINT('Ctrl Pts',(11.0167840474069,12.2,-1.98403762214947));
#185733=CARTESIAN_POINT('Ctrl Pts',(11.0139327091425,12.2,-1.98220307514953));
#185734=CARTESIAN_POINT('Ctrl Pts',(11.0110853821042,12.2,-1.98037586830164));
#185735=CARTESIAN_POINT('Ctrl Pts',(11.0072889469153,12.2,-1.97793959305769));
#185736=CARTESIAN_POINT('Ctrl Pts',(11.0034996427782,12.2,-1.97551636664261));
#185737=CARTESIAN_POINT('Ctrl Pts',(10.9997175803092,12.2,-1.97310617867212));
#185738=CARTESIAN_POINT('Ctrl Pts',(10.9968810333285,12.2,-1.97129853761216));
#185739=CARTESIAN_POINT('Ctrl Pts',(10.9940485607195,12.2,-1.96949823050554));
#185740=CARTESIAN_POINT('Ctrl Pts',(10.9912202085138,12.2,-1.96770525139693));
#185741=CARTESIAN_POINT('Ctrl Pts',(10.9883918563082,12.2,-1.96591227228832));
#185742=CARTESIAN_POINT('Ctrl Pts',(10.9855676239795,12.2,-1.96412662250736));
#185743=CARTESIAN_POINT('Ctrl Pts',(10.982747561373,12.2,-1.96234829644598));
#185744=CARTESIAN_POINT('Ctrl Pts',(10.9789874775562,12.2,-1.95997719481543));
#185745=CARTESIAN_POINT('Ctrl Pts',(10.9752348046818,12.2,-1.95761911140555));
#185746=CARTESIAN_POINT('Ctrl Pts',(10.9714896550332,12.2,-1.95527403649996));
#185747=CARTESIAN_POINT('Ctrl Pts',(10.9677445053847,12.2,-1.95292896159437));
#185748=CARTESIAN_POINT('Ctrl Pts',(10.9640068792231,12.2,-1.95059689427086));
#185749=CARTESIAN_POINT('Ctrl Pts',(10.9602768916317,12.2,-1.9482778206458));
#185750=CARTESIAN_POINT('Ctrl Pts',(10.9565469045485,12.2,-1.94595874733671));
#185751=CARTESIAN_POINT('Ctrl Pts',(10.9528245563768,12.2,-1.94365266726341));
#185752=CARTESIAN_POINT('Ctrl Pts',(10.9491099612191,12.2,-1.9413595692182));
#185753=CARTESIAN_POINT('Ctrl Pts',(10.9453953655553,12.2,-1.93906647086055));
#185754=CARTESIAN_POINT('Ctrl Pts',(10.9416885239598,12.2,-1.93678635215709));
#185755=CARTESIAN_POINT('Ctrl Pts',(10.9379895503701,12.2,-1.93451920114596));
#185756=CARTESIAN_POINT('Ctrl Pts',(10.9342905772844,12.2,-1.93225205044372));
#185757=CARTESIAN_POINT('Ctrl Pts',(10.9305994745283,12.2,-1.9299978656426));
#185758=CARTESIAN_POINT('Ctrl Pts',(10.9269163580511,12.2,-1.92775663365831));
#185759=CARTESIAN_POINT('Ctrl Pts',(10.923233241072,12.2,-1.92551540136864));
#185760=CARTESIAN_POINT('Ctrl Pts',(10.9195581097752,12.2,-1.92328712073386));
#185761=CARTESIAN_POINT('Ctrl Pts',(10.9158910832262,12.2,-1.92107177767024));
#185762=CARTESIAN_POINT('Ctrl Pts',(10.9122240571768,12.2,-1.91885643490846));
#185763=CARTESIAN_POINT('Ctrl Pts',(10.9085651352116,12.2,-1.91665402927315));
#185764=CARTESIAN_POINT('Ctrl Pts',(10.9049144360651,12.2,-1.91446454589574));
#185765=CARTESIAN_POINT('Ctrl Pts',(10.9012637364212,12.2,-1.91227506222002));
#185766=CARTESIAN_POINT('Ctrl Pts',(10.8976212601338,12.2,-1.91009850048474));
#185767=CARTESIAN_POINT('Ctrl Pts',(10.8939871259362,12.2,-1.90793484358987));
#185768=CARTESIAN_POINT('Ctrl Pts',(10.8903529922338,12.2,-1.9057711869898));
#185769=CARTESIAN_POINT('Ctrl Pts',(10.8867272019106,12.2,-1.90362043733507));
#185770=CARTESIAN_POINT('Ctrl Pts',(10.8831098740249,12.2,-1.90148257656859));
#185771=CARTESIAN_POINT('Ctrl Pts',(10.8794925456463,12.2,-1.89934471551082));
#185772=CARTESIAN_POINT('Ctrl Pts',(10.8758836812763,12.2,-1.89721974320003));
#185773=CARTESIAN_POINT('Ctrl Pts',(10.8722834022473,12.2,-1.89510764358576));
#185774=CARTESIAN_POINT('Ctrl Pts',(10.8686831237089,12.2,-1.89299554425926));
#185775=CARTESIAN_POINT('Ctrl Pts',(10.8650914291048,12.2,-1.89089631763295));
#185776=CARTESIAN_POINT('Ctrl Pts',(10.8615084432857,12.2,-1.88880994502443));
#185777=CARTESIAN_POINT('Ctrl Pts',(10.8579254569785,12.2,-1.88672357213163));
#185778=CARTESIAN_POINT('Ctrl Pts',(10.854351177758,12.2,-1.88465005522851));
#185779=CARTESIAN_POINT('Ctrl Pts',(10.8507857302142,12.2,-1.88258937427356));
#185780=CARTESIAN_POINT('Ctrl Pts',(10.8472202831561,12.2,-1.88052869359938));
#185781=CARTESIAN_POINT('Ctrl Pts',(10.8436636666964,12.2,-1.87848085057874));
#185782=CARTESIAN_POINT('Ctrl Pts',(10.8401160080966,12.2,-1.87644582463269));
#185783=CARTESIAN_POINT('Ctrl Pts',(10.8365683490135,12.2,-1.87441079840937));
#185784=CARTESIAN_POINT('Ctrl Pts',(10.8330296438617,12.2,-1.87238858944281));
#185785=CARTESIAN_POINT('Ctrl Pts',(10.8295000217249,12.2,-1.87037918099996));
#185786=CARTESIAN_POINT('Ctrl Pts',(10.8259703995881,12.2,-1.86836977255711));
#185787=CARTESIAN_POINT('Ctrl Pts',(10.8224498602162,12.2,-1.8663731622852));
#185788=CARTESIAN_POINT('Ctrl Pts',(10.8189385286925,12.2,-1.86438933190062));
#185789=CARTESIAN_POINT('Ctrl Pts',(10.8154271976471,12.2,-1.86240550178633));
#185790=CARTESIAN_POINT('Ctrl Pts',(10.8119250765895,12.2,-1.86043444973703));
#185791=CARTESIAN_POINT('Ctrl Pts',(10.8084322903189,12.2,-1.85847615761851));
#185792=CARTESIAN_POINT('Ctrl Pts',(10.8049395035723,12.2,-1.85651786523317));
#185793=CARTESIAN_POINT('Ctrl Pts',(10.8014560547274,12.2,-1.85457233221203));
#185794=CARTESIAN_POINT('Ctrl Pts',(10.7979820704209,12.2,-1.85263953651124));
#185795=CARTESIAN_POINT('Ctrl Pts',(10.7945080865877,12.2,-1.85070674107379));
#185796=CARTESIAN_POINT('Ctrl Pts',(10.7910435691201,12.2,-1.84878668357314));
#185797=CARTESIAN_POINT('Ctrl Pts',(10.7875886467908,12.2,-1.84687934283934));
#185798=CARTESIAN_POINT('Ctrl Pts',(10.7841337239907,12.2,-1.84497200184567));
#185799=CARTESIAN_POINT('Ctrl Pts',(10.7806883968419,12.2,-1.84307737701742));
#185800=CARTESIAN_POINT('Ctrl Pts',(10.7772527967108,12.2,-1.84119544730457));
#185801=CARTESIAN_POINT('Ctrl Pts',(10.7738171970479,12.2,-1.83931351784814));
#185802=CARTESIAN_POINT('Ctrl Pts',(10.7703913249296,12.2,-1.83744428348651));
#185803=CARTESIAN_POINT('Ctrl Pts',(10.7669753105373,12.2,-1.83558772004443));
#185804=CARTESIAN_POINT('Ctrl Pts',(10.7635592956796,12.2,-1.8337311563494));
#185805=CARTESIAN_POINT('Ctrl Pts',(10.7601531412707,12.2,-1.83188726482158));
#185806=CARTESIAN_POINT('Ctrl Pts',(10.7567569796974,12.2,-1.83005602183371));
#185807=CARTESIAN_POINT('Ctrl Pts',(10.7533608185868,12.2,-1.82822477909535));
#185808=CARTESIAN_POINT('Ctrl Pts',(10.7499746495492,12.2,-1.82640618560724));
#185809=CARTESIAN_POINT('Ctrl Pts',(10.7465986086019,12.2,-1.82460021558692));
#185810=CARTESIAN_POINT('Ctrl Pts',(10.7432225671946,12.2,-1.82279424532054));
#185811=CARTESIAN_POINT('Ctrl Pts',(10.7398566537679,12.2,-1.82100090030663));
#185812=CARTESIAN_POINT('Ctrl Pts',(10.7365010030143,12.2,-1.81922015525709));
#185813=CARTESIAN_POINT('Ctrl Pts',(10.7331453527178,12.2,-1.81743941045017));
#185814=CARTESIAN_POINT('Ctrl Pts',(10.7297999663791,12.2,-1.81567126613366));
#185815=CARTESIAN_POINT('Ctrl Pts',(10.7264649807619,12.2,-1.81391569605368));
#185816=CARTESIAN_POINT('Ctrl Pts',(10.7231299946902,12.2,-1.8121601257345));
#185817=CARTESIAN_POINT('Ctrl Pts',(10.71980540945,12.2,-1.81041713059982));
#185818=CARTESIAN_POINT('Ctrl Pts',(10.7164913639916,12.2,-1.80868668428329));
#185819=CARTESIAN_POINT('Ctrl Pts',(10.7131773185332,12.2,-1.80695623796676));
#185820=CARTESIAN_POINT('Ctrl Pts',(10.7098738114344,12.2,-1.80523834092947));
#185821=CARTESIAN_POINT('Ctrl Pts',(10.7065809834782,12.2,-1.80353296650448));
#185822=CARTESIAN_POINT('Ctrl Pts',(10.7032881559707,12.2,-1.80182759231183));
#185823=CARTESIAN_POINT('Ctrl Pts',(10.7000060071857,12.2,-1.80013473975198));
#185824=CARTESIAN_POINT('Ctrl Pts',(10.6967346794938,12.2,-1.79845438349278));
#185825=CARTESIAN_POINT('Ctrl Pts',(10.6934633513562,12.2,-1.79677402700463));
#185826=CARTESIAN_POINT('Ctrl Pts',(10.6902028422835,12.2,-1.79510616451548));
#185827=CARTESIAN_POINT('Ctrl Pts',(10.6869532962186,12.2,-1.79345077070432));
#185828=CARTESIAN_POINT('Ctrl Pts',(10.6828913638589,12.2,-1.79138152855314));
#185829=CARTESIAN_POINT('Ctrl Pts',(10.678846559605,12.2,-1.78933176627727));
#185830=CARTESIAN_POINT('Ctrl Pts',(10.6748191656481,12.2,-1.78730142766774));
#185831=CARTESIAN_POINT('Ctrl Pts',(10.671597250746,12.2,-1.7856771569129));
#185832=CARTESIAN_POINT('Ctrl Pts',(10.6683864779468,12.2,-1.78406531861094));
#185833=CARTESIAN_POINT('Ctrl Pts',(10.6651869930271,12.2,-1.78246588173439));
#185834=CARTESIAN_POINT('Ctrl Pts',(10.6619875076715,12.2,-1.78086644463992));
#185835=CARTESIAN_POINT('Ctrl Pts',(10.6587993100969,12.2,-1.77927940958262));
#185836=CARTESIAN_POINT('Ctrl Pts',(10.6556225474805,12.2,-1.77770474594252));
#185837=CARTESIAN_POINT('Ctrl Pts',(10.6524457852969,12.2,-1.77613008251696));
#185838=CARTESIAN_POINT('Ctrl Pts',(10.649280457323,12.2,-1.77456779159811));
#185839=CARTESIAN_POINT('Ctrl Pts',(10.6461267130245,12.2,-1.77301784133512));
#185840=CARTESIAN_POINT('Ctrl Pts',(10.6429729682963,12.2,-1.77146789086096));
#185841=CARTESIAN_POINT('Ctrl Pts',(10.6398308055328,12.2,-1.76993028070364));
#185842=CARTESIAN_POINT('Ctrl Pts',(10.6367003760957,12.2,-1.76840497954537));
#185843=CARTESIAN_POINT('Ctrl Pts',(10.6335699470851,12.2,-1.76687967859492));
#185844=CARTESIAN_POINT('Ctrl Pts',(10.6304512504675,12.2,-1.76536668609533));
#185845=CARTESIAN_POINT('Ctrl Pts',(10.6273444377207,12.2,-1.7638659711061));
#185846=CARTESIAN_POINT('Ctrl Pts',(10.6242376245506,12.2,-1.7623652559124));
#185847=CARTESIAN_POINT('Ctrl Pts',(10.6211426971291,12.2,-1.76087681637573));
#185848=CARTESIAN_POINT('Ctrl Pts',(10.6180598052397,12.2,-1.7594006206294));
#185849=CARTESIAN_POINT('Ctrl Pts',(10.6149769137702,12.2,-1.75792442508422));
#185850=CARTESIAN_POINT('Ctrl Pts',(10.6119060592254,12.2,-1.75646047158226));
#185851=CARTESIAN_POINT('Ctrl Pts',(10.6088473962105,12.2,-1.75500872796069));
#185852=CARTESIAN_POINT('Ctrl Pts',(10.6057887327788,12.2,-1.75355698414132));
#185853=CARTESIAN_POINT('Ctrl Pts',(10.6027422594804,12.2,-1.75211744984096));
#185854=CARTESIAN_POINT('Ctrl Pts',(10.5997081342603,12.2,-1.75069008937506));
#185855=CARTESIAN_POINT('Ctrl Pts',(10.5966740094536,12.2,-1.74926272910364));
#185856=CARTESIAN_POINT('Ctrl Pts',(10.5936522330527,12.2,-1.74784754366035));
#185857=CARTESIAN_POINT('Ctrl Pts',(10.5906429597419,12.2,-1.74644449599604));
#185858=CARTESIAN_POINT('Ctrl Pts',(10.5868813677959,12.2,-1.74469068627227));
#185859=CARTESIAN_POINT('Ctrl Pts',(10.5831393145361,12.2,-1.74295584315294));
#185860=CARTESIAN_POINT('Ctrl Pts',(10.5794171114321,12.2,-1.74123989348256));
#185861=CARTESIAN_POINT('Ctrl Pts',(10.575694908328,12.2,-1.73952394381218));
#185862=CARTESIAN_POINT('Ctrl Pts',(10.5719925556196,12.2,-1.73782688946638));
#185863=CARTESIAN_POINT('Ctrl Pts',(10.5683103670075,12.2,-1.73614865557651));
#185864=CARTESIAN_POINT('Ctrl Pts',(10.5646281783953,12.2,-1.73447042168664));
#185865=CARTESIAN_POINT('Ctrl Pts',(10.5609661564948,12.2,-1.73281100937503));
#185866=CARTESIAN_POINT('Ctrl Pts',(10.5573246194798,12.2,-1.73117034062405));
#185867=CARTESIAN_POINT('Ctrl Pts',(10.5536830824649,12.2,-1.72952967187307));
#185868=CARTESIAN_POINT('Ctrl Pts',(10.5500620305754,12.2,-1.72790774972813));
#185869=CARTESIAN_POINT('Ctrl Pts',(10.5464617877271,12.2,-1.72630449187994));
#185870=CARTESIAN_POINT('Ctrl Pts',(10.5428615448789,12.2,-1.72470123403175));
#185871=CARTESIAN_POINT('Ctrl Pts',(10.5392821105347,12.2,-1.72311664391354));
#185872=CARTESIAN_POINT('Ctrl Pts',(10.5357238144768,12.2,-1.72155064001749));
#185873=CARTESIAN_POINT('Ctrl Pts',(10.532165518419,12.2,-1.71998463612144));
#185874=CARTESIAN_POINT('Ctrl Pts',(10.5286283611332,12.2,-1.71843721744996));
#185875=CARTESIAN_POINT('Ctrl Pts',(10.5251126742582,12.2,-1.7169083020333));
#185876=CARTESIAN_POINT('Ctrl Pts',(10.5215969873832,12.2,-1.71537938661663));
#185877=CARTESIAN_POINT('Ctrl Pts',(10.5181027712526,12.2,-1.71386897543366));
#185878=CARTESIAN_POINT('Ctrl Pts',(10.5146303650563,12.2,-1.71237698223249));
#185879=CARTESIAN_POINT('Ctrl Pts',(10.5111579588601,12.2,-1.71088498903132));
#185880=CARTESIAN_POINT('Ctrl Pts',(10.5077073598247,12.2,-1.70941141196506));
#185881=CARTESIAN_POINT('Ctrl Pts',(10.5042789137841,12.2,-1.70795616710491));
#185882=CARTESIAN_POINT('Ctrl Pts',(10.5008504677436,12.2,-1.70650092224475));
#185883=CARTESIAN_POINT('Ctrl Pts',(10.4974441731775,12.2,-1.70506400643413));
#185884=CARTESIAN_POINT('Ctrl Pts',(10.4940603773454,12.2,-1.7036453324073));
#185885=CARTESIAN_POINT('Ctrl Pts',(10.4906765815132,12.2,-1.70222665838047));
#185886=CARTESIAN_POINT('Ctrl Pts',(10.4873152869609,12.2,-1.70082622411292));
#185887=CARTESIAN_POINT('Ctrl Pts',(10.4839768426291,12.2,-1.69944393682291));
#185888=CARTESIAN_POINT('Ctrl Pts',(10.4806383982972,12.2,-1.69806164953289));
#185889=CARTESIAN_POINT('Ctrl Pts',(10.4773228069951,12.2,-1.69669751057243));
#185890=CARTESIAN_POINT('Ctrl Pts',(10.4740304260943,12.2,-1.69535142328224));
#185891=CARTESIAN_POINT('Ctrl Pts',(10.4700795691567,12.2,-1.69373611859271));
#185892=CARTESIAN_POINT('Ctrl Pts',(10.4661621343579,12.2,-1.69214680864117));
#185893=CARTESIAN_POINT('Ctrl Pts',(10.4622787523148,12.2,-1.69058332477426));
#185894=CARTESIAN_POINT('Ctrl Pts',(10.4590426004946,12.2,-1.68928042150451));
#185895=CARTESIAN_POINT('Ctrl Pts',(10.4558300937513,12.2,-1.68799545171071));
#185896=CARTESIAN_POINT('Ctrl Pts',(10.4526416070165,12.2,-1.68672831435054));
#185897=CARTESIAN_POINT('Ctrl Pts',(10.4494531202817,12.2,-1.68546117699037));
#185898=CARTESIAN_POINT('Ctrl Pts',(10.4462886496434,12.2,-1.68421187264083));
#185899=CARTESIAN_POINT('Ctrl Pts',(10.443148572978,12.2,-1.68298029687786));
#185900=CARTESIAN_POINT('Ctrl Pts',(10.4400084963126,12.2,-1.6817487211149));
#185901=CARTESIAN_POINT('Ctrl Pts',(10.4368928141828,12.2,-1.68053487177526));
#185902=CARTESIAN_POINT('Ctrl Pts',(10.4338019065995,12.2,-1.67933864511951));
#185903=CARTESIAN_POINT('Ctrl Pts',(10.4294746362525,12.2,-1.67766392790576));
#185904=CARTESIAN_POINT('Ctrl Pts',(10.4251959272567,12.2,-1.67602374681866));
#185905=CARTESIAN_POINT('Ctrl Pts',(10.4209668438783,12.2,-1.67441779991668));
#185906=CARTESIAN_POINT('Ctrl Pts',(10.417341914845,12.2,-1.67304127383994));
#185907=CARTESIAN_POINT('Ctrl Pts',(10.4137534485502,12.2,-1.67168989669216));
#185908=CARTESIAN_POINT('Ctrl Pts',(10.4102021304314,12.2,-1.67036347338839));
#185909=CARTESIAN_POINT('Ctrl Pts',(10.4066508126352,12.2,-1.66903705020509));
#185910=CARTESIAN_POINT('Ctrl Pts',(10.4031366447736,12.2,-1.66773557787858));
#185911=CARTESIAN_POINT('Ctrl Pts',(10.3996603252332,12.2,-1.6664588510083));
#185912=CARTESIAN_POINT('Ctrl Pts',(10.3961840056929,12.2,-1.66518212413803));
#185913=CARTESIAN_POINT('Ctrl Pts',(10.3927455368108,12.2,-1.66393014446191));
#185914=CARTESIAN_POINT('Ctrl Pts',(10.3893456330955,12.2,-1.66270269836044));
#185915=CARTESIAN_POINT('Ctrl Pts',(10.3859457290715,12.2,-1.66147525214747));
#185916=CARTESIAN_POINT('Ctrl Pts',(10.3825843893245,12.2,-1.66027233816742));
#185917=CARTESIAN_POINT('Ctrl Pts',(10.3792623465628,12.2,-1.65909373810484));
#185918=CARTESIAN_POINT('Ctrl Pts',(10.3759403041029,12.2,-1.65791513814932));
#185919=CARTESIAN_POINT('Ctrl Pts',(10.3726575564452,12.2,-1.65676085241348));
#185920=CARTESIAN_POINT('Ctrl Pts',(10.3694148500484,12.2,-1.65563065228279));
#185921=CARTESIAN_POINT('Ctrl Pts',(10.3661721436516,12.2,-1.65450045215211));
#185922=CARTESIAN_POINT('Ctrl Pts',(10.3629694782426,12.2,-1.65339433672077));
#185923=CARTESIAN_POINT('Ctrl Pts',(10.3598076168557,12.2,-1.65231207359239));
#185924=CARTESIAN_POINT('Ctrl Pts',(10.3566457551816,12.2,-1.6512298103657));
#185925=CARTESIAN_POINT('Ctrl Pts',(10.3535246958959,12.2,-1.65017139676697));
#185926=CARTESIAN_POINT('Ctrl Pts',(10.3504452183975,12.2,-1.64913659062885));
#185927=CARTESIAN_POINT('Ctrl Pts',(10.3473657411789,12.2,-1.64810178458472));
#185928=CARTESIAN_POINT('Ctrl Pts',(10.3443278454199,12.2,-1.6470905856764));
#185929=CARTESIAN_POINT('Ctrl Pts',(10.3413323281818,12.2,-1.64610274245786));
#185930=CARTESIAN_POINT('Ctrl Pts',(10.3383368109438,12.2,-1.64511489923932));
#185931=CARTESIAN_POINT('Ctrl Pts',(10.3353836696881,12.2,-1.64415040969318));
#185932=CARTESIAN_POINT('Ctrl Pts',(10.3324737224586,12.2,-1.64320901730971));
#185933=CARTESIAN_POINT('Ctrl Pts',(10.3295637749649,12.2,-1.64226762484074));
#185934=CARTESIAN_POINT('Ctrl Pts',(10.3266970175847,12.2,-1.64134932435795));
#185935=CARTESIAN_POINT('Ctrl Pts',(10.3238742871839,12.2,-1.64045385089404));
#185936=CARTESIAN_POINT('Ctrl Pts',(10.3210515570394,12.2,-1.63955837751147));
#185937=CARTESIAN_POINT('Ctrl Pts',(10.3182728521331,12.2,-1.63868572728853));
#185938=CARTESIAN_POINT('Ctrl Pts',(10.3155390244011,12.2,-1.63783562398707));
#185939=CARTESIAN_POINT('Ctrl Pts',(10.312805196669,12.2,-1.63698552068561));
#185940=CARTESIAN_POINT('Ctrl Pts',(10.3101162476,12.2,-1.63615796238233));
#185941=CARTESIAN_POINT('Ctrl Pts',(10.3074730508608,12.2,-1.63535266107729));
#185942=CARTESIAN_POINT('Ctrl Pts',(10.3048298541215,12.2,-1.63454735977225));
#185943=CARTESIAN_POINT('Ctrl Pts',(10.3022324099134,12.2,-1.63376431454012));
#185944=CARTESIAN_POINT('Ctrl Pts',(10.2996816122529,12.2,-1.63300322706627));
#185945=CARTESIAN_POINT('Ctrl Pts',(10.2971308143607,12.2,-1.63224213952329));
#185946=CARTESIAN_POINT('Ctrl Pts',(10.2946266653563,12.2,-1.63150300843246));
#185947=CARTESIAN_POINT('Ctrl Pts',(10.2921700806412,12.2,-1.63078552572763));
#185948=CARTESIAN_POINT('Ctrl Pts',(10.2897134961492,12.2,-1.63006804308798));
#185949=CARTESIAN_POINT('Ctrl Pts',(10.2873044769177,12.2,-1.62937220681223));
#185950=CARTESIAN_POINT('Ctrl Pts',(10.2849439662426,12.2,-1.62869769550029));
#185951=CARTESIAN_POINT('Ctrl Pts',(10.2825834555675,12.2,-1.62802318418834));
#185952=CARTESIAN_POINT('Ctrl Pts',(10.2802714503093,12.2,-1.62737000058902));
#185953=CARTESIAN_POINT('Ctrl Pts',(10.2780089199715,12.2,-1.62673780902723));
#185954=CARTESIAN_POINT('Ctrl Pts',(10.2757463894281,12.2,-1.62610561740801));
#185955=CARTESIAN_POINT('Ctrl Pts',(10.2735333314221,12.2,-1.62549441732006));
#185956=CARTESIAN_POINT('Ctrl Pts',(10.2713707417824,12.2,-1.62490386742623));
#185957=CARTESIAN_POINT('Ctrl Pts',(10.2692081523392,12.2,-1.62431331758605));
#185958=CARTESIAN_POINT('Ctrl Pts',(10.2670960277416,12.2,-1.62374341398834));
#185959=CARTESIAN_POINT('Ctrl Pts',(10.2650353904832,12.2,-1.62319380125831));
#185960=CARTESIAN_POINT('Ctrl Pts',(10.2629747532247,12.2,-1.62264418852828));
#185961=CARTESIAN_POINT('Ctrl Pts',(10.2609656015273,12.2,-1.62211486489073));
#185962=CARTESIAN_POINT('Ctrl Pts',(10.2590089854143,12.2,-1.62160546104931));
#185963=CARTESIAN_POINT('Ctrl Pts',(10.2570523691235,12.2,-1.62109605716161));
#185964=CARTESIAN_POINT('Ctrl Pts',(10.255148287587,12.2,-1.62060657271471));
#185965=CARTESIAN_POINT('Ctrl Pts',(10.2532978195732,12.2,-1.62013662094043));
#185966=CARTESIAN_POINT('Ctrl Pts',(10.2514562326224,12.2,-1.61966892463414));
#185967=CARTESIAN_POINT('Ctrl Pts',(10.2496677474645,12.2,-1.61922057460985));
#185968=CARTESIAN_POINT('Ctrl Pts',(10.2479334559999,12.2,-1.61879118000002));
#185969=CARTESIAN_POINT('Ctrl Pts',(10.2479334559999,15.2,-1.61879118000002));
#185970=CARTESIAN_POINT('Ctrl Pts',(10.2496677474645,15.2,-1.61922057460985));
#185971=CARTESIAN_POINT('Ctrl Pts',(10.2514562326224,15.2,-1.61966892463414));
#185972=CARTESIAN_POINT('Ctrl Pts',(10.2532978195732,15.2,-1.62013662094043));
#185973=CARTESIAN_POINT('Ctrl Pts',(10.2551482875871,15.2,-1.62060657271471));
#185974=CARTESIAN_POINT('Ctrl Pts',(10.2570523691235,15.2,-1.62109605716161));
#185975=CARTESIAN_POINT('Ctrl Pts',(10.2590089854143,15.2,-1.62160546104931));
#185976=CARTESIAN_POINT('Ctrl Pts',(10.2609656015273,15.2,-1.62211486489073));
#185977=CARTESIAN_POINT('Ctrl Pts',(10.2629747532247,15.2,-1.62264418852828));
#185978=CARTESIAN_POINT('Ctrl Pts',(10.2650353904832,15.2,-1.62319380125831));
#185979=CARTESIAN_POINT('Ctrl Pts',(10.2670960277416,15.2,-1.62374341398834));
#185980=CARTESIAN_POINT('Ctrl Pts',(10.2692081523392,15.2,-1.62431331758605));
#185981=CARTESIAN_POINT('Ctrl Pts',(10.2713707417824,15.2,-1.62490386742623));
#185982=CARTESIAN_POINT('Ctrl Pts',(10.2735333314221,15.2,-1.62549441732006));
#185983=CARTESIAN_POINT('Ctrl Pts',(10.2757463894281,15.2,-1.62610561740801));
#185984=CARTESIAN_POINT('Ctrl Pts',(10.2780089199715,15.2,-1.62673780902722));
#185985=CARTESIAN_POINT('Ctrl Pts',(10.2802714503093,15.2,-1.62737000058902));
#185986=CARTESIAN_POINT('Ctrl Pts',(10.2825834555675,15.2,-1.62802318418834));
#185987=CARTESIAN_POINT('Ctrl Pts',(10.2849439662426,15.2,-1.62869769550028));
#185988=CARTESIAN_POINT('Ctrl Pts',(10.2873044769177,15.2,-1.62937220681223));
#185989=CARTESIAN_POINT('Ctrl Pts',(10.2897134961492,15.2,-1.63006804308797));
#185990=CARTESIAN_POINT('Ctrl Pts',(10.2921700806412,15.2,-1.63078552572763));
#185991=CARTESIAN_POINT('Ctrl Pts',(10.2946266653563,15.2,-1.63150300843246));
#185992=CARTESIAN_POINT('Ctrl Pts',(10.2971308143607,15.2,-1.6322421395233));
#185993=CARTESIAN_POINT('Ctrl Pts',(10.2996816122529,15.2,-1.63300322706627));
#185994=CARTESIAN_POINT('Ctrl Pts',(10.3022324099134,15.2,-1.63376431454011));
#185995=CARTESIAN_POINT('Ctrl Pts',(10.3048298541215,15.2,-1.63454735977225));
#185996=CARTESIAN_POINT('Ctrl Pts',(10.3074730508608,15.2,-1.63535266107729));
#185997=CARTESIAN_POINT('Ctrl Pts',(10.3101162476,15.2,-1.63615796238233));
#185998=CARTESIAN_POINT('Ctrl Pts',(10.312805196669,15.2,-1.63698552068561));
#185999=CARTESIAN_POINT('Ctrl Pts',(10.3155390244011,15.2,-1.63783562398707));
#186000=CARTESIAN_POINT('Ctrl Pts',(10.3182728521331,15.2,-1.63868572728853));
#186001=CARTESIAN_POINT('Ctrl Pts',(10.3210515570394,15.2,-1.63955837751146));
#186002=CARTESIAN_POINT('Ctrl Pts',(10.3238742871839,15.2,-1.64045385089404));
#186003=CARTESIAN_POINT('Ctrl Pts',(10.3266970175847,15.2,-1.64134932435796));
#186004=CARTESIAN_POINT('Ctrl Pts',(10.3295637749648,15.2,-1.64226762484073));
#186005=CARTESIAN_POINT('Ctrl Pts',(10.3324737224586,15.2,-1.64320901730971));
#186006=CARTESIAN_POINT('Ctrl Pts',(10.3353836696881,15.2,-1.64415040969318));
#186007=CARTESIAN_POINT('Ctrl Pts',(10.3383368109438,15.2,-1.64511489923932));
#186008=CARTESIAN_POINT('Ctrl Pts',(10.3413323281818,15.2,-1.64610274245786));
#186009=CARTESIAN_POINT('Ctrl Pts',(10.3443278454199,15.2,-1.64709058567641));
#186010=CARTESIAN_POINT('Ctrl Pts',(10.3473657411789,15.2,-1.64810178458472));
#186011=CARTESIAN_POINT('Ctrl Pts',(10.3504452183975,15.2,-1.64913659062885));
#186012=CARTESIAN_POINT('Ctrl Pts',(10.3535246958959,15.2,-1.65017139676697));
#186013=CARTESIAN_POINT('Ctrl Pts',(10.3566457551816,15.2,-1.6512298103657));
#186014=CARTESIAN_POINT('Ctrl Pts',(10.3598076168557,15.2,-1.65231207359239));
#186015=CARTESIAN_POINT('Ctrl Pts',(10.3629694782426,15.2,-1.65339433672077));
#186016=CARTESIAN_POINT('Ctrl Pts',(10.3661721436516,15.2,-1.65450045215211));
#186017=CARTESIAN_POINT('Ctrl Pts',(10.3694148500484,15.2,-1.65563065228279));
#186018=CARTESIAN_POINT('Ctrl Pts',(10.3726575564452,15.2,-1.65676085241347));
#186019=CARTESIAN_POINT('Ctrl Pts',(10.3759403041029,15.2,-1.65791513814932));
#186020=CARTESIAN_POINT('Ctrl Pts',(10.3792623465628,15.2,-1.65909373810484));
#186021=CARTESIAN_POINT('Ctrl Pts',(10.3825843893245,15.2,-1.66027233816742));
#186022=CARTESIAN_POINT('Ctrl Pts',(10.3859457290715,15.2,-1.66147525214747));
#186023=CARTESIAN_POINT('Ctrl Pts',(10.3893456330955,15.2,-1.66270269836044));
#186024=CARTESIAN_POINT('Ctrl Pts',(10.3927455368108,15.2,-1.66393014446192));
#186025=CARTESIAN_POINT('Ctrl Pts',(10.3961840056929,15.2,-1.66518212413802));
#186026=CARTESIAN_POINT('Ctrl Pts',(10.3996603252332,15.2,-1.6664588510083));
#186027=CARTESIAN_POINT('Ctrl Pts',(10.4031366447736,15.2,-1.66773557787858));
#186028=CARTESIAN_POINT('Ctrl Pts',(10.4066508126352,15.2,-1.66903705020509));
#186029=CARTESIAN_POINT('Ctrl Pts',(10.4102021304314,15.2,-1.67036347338839));
#186030=CARTESIAN_POINT('Ctrl Pts',(10.4137534485502,15.2,-1.67168989669217));
#186031=CARTESIAN_POINT('Ctrl Pts',(10.417341914845,15.2,-1.67304127383995));
#186032=CARTESIAN_POINT('Ctrl Pts',(10.4209668438783,15.2,-1.67441779991668));
#186033=CARTESIAN_POINT('Ctrl Pts',(10.4258000822603,15.2,-1.67625316789396));
#186034=CARTESIAN_POINT('Ctrl Pts',(10.4306981370547,15.2,-1.67813324902336));
#186035=CARTESIAN_POINT('Ctrl Pts',(10.4356594221266,15.2,-1.68005849687305));
#186036=CARTESIAN_POINT('Ctrl Pts',(10.4387602253388,15.2,-1.6812617767955));
#186037=CARTESIAN_POINT('Ctrl Pts',(10.4418857244099,15.2,-1.6824826994772));
#186038=CARTESIAN_POINT('Ctrl Pts',(10.4450355442036,15.2,-1.68372137093699));
#186039=CARTESIAN_POINT('Ctrl Pts',(10.4481853639972,15.2,-1.68496004239679));
#186040=CARTESIAN_POINT('Ctrl Pts',(10.4513594997051,15.2,-1.68621646330408));
#186041=CARTESIAN_POINT('Ctrl Pts',(10.4545575789432,15.2,-1.68749073795832));
#186042=CARTESIAN_POINT('Ctrl Pts',(10.4577556578327,15.2,-1.68876501247365));
#186043=CARTESIAN_POINT('Ctrl Pts',(10.4609776818311,15.2,-1.69005713868399));
#186044=CARTESIAN_POINT('Ctrl Pts',(10.464223277517,15.2,-1.69136721930362));
#186045=CARTESIAN_POINT('Ctrl Pts',(10.4674688735568,15.2,-1.69267730006604));
#186046=CARTESIAN_POINT('Ctrl Pts',(10.4707380451934,15.2,-1.69400533599205));
#186047=CARTESIAN_POINT('Ctrl Pts',(10.4740304260942,15.2,-1.69535142328224));
#186048=CARTESIAN_POINT('Ctrl Pts',(10.4773228069951,15.2,-1.69669751057243));
#186049=CARTESIAN_POINT('Ctrl Pts',(10.4806383982972,15.2,-1.69806164953288));
#186050=CARTESIAN_POINT('Ctrl Pts',(10.4839768426291,15.2,-1.6994439368229));
#186051=CARTESIAN_POINT('Ctrl Pts',(10.487315286961,15.2,-1.70082622411293));
#186052=CARTESIAN_POINT('Ctrl Pts',(10.4906765815132,15.2,-1.70222665838047));
#186053=CARTESIAN_POINT('Ctrl Pts',(10.4940603773454,15.2,-1.7036453324073));
#186054=CARTESIAN_POINT('Ctrl Pts',(10.4974441731776,15.2,-1.70506400643413));
#186055=CARTESIAN_POINT('Ctrl Pts',(10.5008504677436,15.2,-1.70650092224475));
#186056=CARTESIAN_POINT('Ctrl Pts',(10.5042789137841,15.2,-1.7079561671049));
#186057=CARTESIAN_POINT('Ctrl Pts',(10.5077073598246,15.2,-1.70941141196506));
#186058=CARTESIAN_POINT('Ctrl Pts',(10.5111579588601,15.2,-1.71088498903132));
#186059=CARTESIAN_POINT('Ctrl Pts',(10.5146303650563,15.2,-1.71237698223249));
#186060=CARTESIAN_POINT('Ctrl Pts',(10.5187972523405,15.2,-1.71416737400885));
#186061=CARTESIAN_POINT('Ctrl Pts',(10.5229955456113,15.2,-1.71598428835948));
#186062=CARTESIAN_POINT('Ctrl Pts',(10.5272246597889,15.2,-1.71782787204069));
#186063=CARTESIAN_POINT('Ctrl Pts',(10.5307489217316,15.2,-1.71936419183085));
#186064=CARTESIAN_POINT('Ctrl Pts',(10.5342945876647,15.2,-1.7209190315234));
#186065=CARTESIAN_POINT('Ctrl Pts',(10.5378613256193,15.2,-1.72249247305905));
#186066=CARTESIAN_POINT('Ctrl Pts',(10.5414280635738,15.2,-1.72406591459469));
#186067=CARTESIAN_POINT('Ctrl Pts',(10.545015874304,15.2,-1.72565796019572));
#186068=CARTESIAN_POINT('Ctrl Pts',(10.548624427289,15.2,-1.72726868665307));
#186069=CARTESIAN_POINT('Ctrl Pts',(10.5536764015467,15.2,-1.72952370372847));
#186070=CARTESIAN_POINT('Ctrl Pts',(10.5587690353144,15.2,-1.73181533826371));
#186071=CARTESIAN_POINT('Ctrl Pts',(10.5639014407416,15.2,-1.73414380371663));
#186072=CARTESIAN_POINT('Ctrl Pts',(10.568300645165,15.2,-1.73613963114411));
#186073=CARTESIAN_POINT('Ctrl Pts',(10.5727290727597,15.2,-1.73816251542536));
#186074=CARTESIAN_POINT('Ctrl Pts',(10.5771861733188,15.2,-1.74021258978505));
#186075=CARTESIAN_POINT('Ctrl Pts',(10.5809004239196,15.2,-1.74192098514686));
#186076=CARTESIAN_POINT('Ctrl Pts',(10.5846345871611,15.2,-1.74364825788131));
#186077=CARTESIAN_POINT('Ctrl Pts',(10.5883883509795,15.2,-1.74539448489421));
#186078=CARTESIAN_POINT('Ctrl Pts',(10.5921421147979,15.2,-1.74714071190711));
#186079=CARTESIAN_POINT('Ctrl Pts',(10.5959154779418,15.2,-1.74890588888993));
#186080=CARTESIAN_POINT('Ctrl Pts',(10.5997081342603,15.2,-1.75069008937506));
#186081=CARTESIAN_POINT('Ctrl Pts',(10.6027422594805,15.2,-1.75211744984096));
#186082=CARTESIAN_POINT('Ctrl Pts',(10.6057887327788,15.2,-1.75355698414132));
#186083=CARTESIAN_POINT('Ctrl Pts',(10.6088473962105,15.2,-1.75500872796069));
#186084=CARTESIAN_POINT('Ctrl Pts',(10.6119060592254,15.2,-1.75646047158226));
#186085=CARTESIAN_POINT('Ctrl Pts',(10.6149769137702,15.2,-1.75792442508421));
#186086=CARTESIAN_POINT('Ctrl Pts',(10.6180598052397,15.2,-1.7594006206294));
#186087=CARTESIAN_POINT('Ctrl Pts',(10.6211426971291,15.2,-1.76087681637573));
#186088=CARTESIAN_POINT('Ctrl Pts',(10.6242376245506,15.2,-1.7623652559124));
#186089=CARTESIAN_POINT('Ctrl Pts',(10.6273444377207,15.2,-1.7638659711061));
#186090=CARTESIAN_POINT('Ctrl Pts',(10.6304512504675,15.2,-1.76536668609533));
#186091=CARTESIAN_POINT('Ctrl Pts',(10.6335699470852,15.2,-1.76687967859493));
#186092=CARTESIAN_POINT('Ctrl Pts',(10.6367003760957,15.2,-1.76840497954537));
#186093=CARTESIAN_POINT('Ctrl Pts',(10.6398308055328,15.2,-1.76993028070363));
#186094=CARTESIAN_POINT('Ctrl Pts',(10.6429729682963,15.2,-1.77146789086095));
#186095=CARTESIAN_POINT('Ctrl Pts',(10.6461267130245,15.2,-1.77301784133512));
#186096=CARTESIAN_POINT('Ctrl Pts',(10.649280457323,15.2,-1.77456779159811));
#186097=CARTESIAN_POINT('Ctrl Pts',(10.6524457852969,15.2,-1.77613008251696));
#186098=CARTESIAN_POINT('Ctrl Pts',(10.6556225474805,15.2,-1.77770474594252));
#186099=CARTESIAN_POINT('Ctrl Pts',(10.6587993100969,15.2,-1.77927940958262));
#186100=CARTESIAN_POINT('Ctrl Pts',(10.6619875076715,15.2,-1.78086644463991));
#186101=CARTESIAN_POINT('Ctrl Pts',(10.6651869930271,15.2,-1.78246588173439));
#186102=CARTESIAN_POINT('Ctrl Pts',(10.6683864779468,15.2,-1.78406531861095));
#186103=CARTESIAN_POINT('Ctrl Pts',(10.671597250746,15.2,-1.7856771569129));
#186104=CARTESIAN_POINT('Ctrl Pts',(10.6748191656481,15.2,-1.78730142766774));
#186105=CARTESIAN_POINT('Ctrl Pts',(10.678846559605,15.2,-1.78933176627727));
#186106=CARTESIAN_POINT('Ctrl Pts',(10.6828913638589,15.2,-1.79138152855313));
#186107=CARTESIAN_POINT('Ctrl Pts',(10.6869532962186,15.2,-1.79345077070432));
#186108=CARTESIAN_POINT('Ctrl Pts',(10.6902028422835,15.2,-1.79510616451548));
#186109=CARTESIAN_POINT('Ctrl Pts',(10.6934633513562,15.2,-1.79677402700464));
#186110=CARTESIAN_POINT('Ctrl Pts',(10.6967346794938,15.2,-1.79845438349278));
#186111=CARTESIAN_POINT('Ctrl Pts',(10.7000060071857,15.2,-1.80013473975198));
#186112=CARTESIAN_POINT('Ctrl Pts',(10.7032881559707,15.2,-1.80182759231183));
#186113=CARTESIAN_POINT('Ctrl Pts',(10.7065809834782,15.2,-1.80353296650448));
#186114=CARTESIAN_POINT('Ctrl Pts',(10.7106970181991,15.2,-1.80566468441955));
#186115=CARTESIAN_POINT('Ctrl Pts',(10.7148297387252,15.2,-1.80781596909539));
#186116=CARTESIAN_POINT('Ctrl Pts',(10.7189788712239,15.2,-1.80998687194102));
#186117=CARTESIAN_POINT('Ctrl Pts',(10.7222981774037,15.2,-1.81172359431217));
#186118=CARTESIAN_POINT('Ctrl Pts',(10.7256279900688,15.2,-1.81347287244432));
#186119=CARTESIAN_POINT('Ctrl Pts',(10.7289681675438,15.2,-1.81523473149283));
#186120=CARTESIAN_POINT('Ctrl Pts',(10.7323083445638,15.2,-1.81699659030129));
#186121=CARTESIAN_POINT('Ctrl Pts',(10.7356588894401,15.2,-1.81877102999683));
#186122=CARTESIAN_POINT('Ctrl Pts',(10.7390196624421,15.2,-1.82055807668279));
#186123=CARTESIAN_POINT('Ctrl Pts',(10.743220629038,15.2,-1.82279188522286));
#186124=CARTESIAN_POINT('Ctrl Pts',(10.747437578192,15.2,-1.82504539094313));
#186125=CARTESIAN_POINT('Ctrl Pts',(10.7516702479129,15.2,-1.8273186412193));
#186126=CARTESIAN_POINT('Ctrl Pts',(10.7559029176339,15.2,-1.82959189149547));
#186127=CARTESIAN_POINT('Ctrl Pts',(10.7601513043042,15.2,-1.83188488622295));
#186128=CARTESIAN_POINT('Ctrl Pts',(10.7644151494467,15.2,-1.83419767244822));
#186129=CARTESIAN_POINT('Ctrl Pts',(10.7678262257466,15.2,-1.83604790152928));
#186130=CARTESIAN_POINT('Ctrl Pts',(10.7712471950929,15.2,-1.83791079673092));
#186131=CARTESIAN_POINT('Ctrl Pts',(10.7746779232805,15.2,-1.83978638044508));
#186132=CARTESIAN_POINT('Ctrl Pts',(10.7781086510006,15.2,-1.84166196390369));
#186133=CARTESIAN_POINT('Ctrl Pts',(10.7815491388494,15.2,-1.8435502374792));
#186134=CARTESIAN_POINT('Ctrl Pts',(10.7849992551775,15.2,-1.84545122098916));
#186135=CARTESIAN_POINT('Ctrl Pts',(10.7884493719756,15.2,-1.84735220475813));
#186136=CARTESIAN_POINT('Ctrl Pts',(10.7919091171335,15.2,-1.84926589974306));
#186137=CARTESIAN_POINT('Ctrl Pts',(10.7953783600606,15.2,-1.85119232796794));
#186138=CARTESIAN_POINT('Ctrl Pts',(10.798847602515,15.2,-1.85311875593035));
#186139=CARTESIAN_POINT('Ctrl Pts',(10.8023263425435,15.2,-1.85505791591948));
#186140=CARTESIAN_POINT('Ctrl Pts',(10.8058144521463,15.2,-1.85700982998083));
#186141=CARTESIAN_POINT('Ctrl Pts',(10.8093025622243,15.2,-1.85896174430813));
#186142=CARTESIAN_POINT('Ctrl Pts',(10.8128000406254,15.2,-1.8609264129533));
#186143=CARTESIAN_POINT('Ctrl Pts',(10.8163067594832,15.2,-1.86290385528329));
#186144=CARTESIAN_POINT('Ctrl Pts',(10.8215668372922,15.2,-1.86587001850886));
#186145=CARTESIAN_POINT('Ctrl Pts',(10.8268477058994,15.2,-1.86886492240721));
#186146=CARTESIAN_POINT('Ctrl Pts',(10.8321489387054,15.2,-1.87188863737872));
#186147=CARTESIAN_POINT('Ctrl Pts',(10.8356830942304,15.2,-1.87390444754283));
#186148=CARTESIAN_POINT('Ctrl Pts',(10.8392262989926,15.2,-1.87593306149467));
#186149=CARTESIAN_POINT('Ctrl Pts',(10.8427784292023,15.2,-1.87797449722636));
#186150=CARTESIAN_POINT('Ctrl Pts',(10.8463305589281,15.2,-1.8800159326799));
#186151=CARTESIAN_POINT('Ctrl Pts',(10.8498916141118,15.2,-1.88207019159341));
#186152=CARTESIAN_POINT('Ctrl Pts',(10.8534614692079,15.2,-1.88413729164533));
#186153=CARTESIAN_POINT('Ctrl Pts',(10.8579237884429,15.2,-1.88672116692147));
#186154=CARTESIAN_POINT('Ctrl Pts',(10.8623998578415,15.2,-1.88932510789172));
#186155=CARTESIAN_POINT('Ctrl Pts',(10.866889437146,15.2,-1.89194914664008));
#186156=CARTESIAN_POINT('Ctrl Pts',(10.8713790164505,15.2,-1.89457318538844));
#186157=CARTESIAN_POINT('Ctrl Pts',(10.8758821055176,15.2,-1.89721732467573));
#186158=CARTESIAN_POINT('Ctrl Pts',(10.8803984659507,15.2,-1.89988159668242));
#186159=CARTESIAN_POINT('Ctrl Pts',(10.884011554494,15.2,-1.90201301440394));
#186160=CARTESIAN_POINT('Ctrl Pts',(10.8876331373206,15.2,-1.90415731601359));
#186161=CARTESIAN_POINT('Ctrl Pts',(10.8912630922967,15.2,-1.90631452090977));
#186162=CARTESIAN_POINT('Ctrl Pts',(10.8948930467783,15.2,-1.90847172551203));
#186163=CARTESIAN_POINT('Ctrl Pts',(10.898531373786,15.2,-1.91064183205061));
#186164=CARTESIAN_POINT('Ctrl Pts',(10.9021779541537,15.2,-1.91282485542638));
#186165=CARTESIAN_POINT('Ctrl Pts',(10.9058245350183,15.2,-1.91500787909959));
#186166=CARTESIAN_POINT('Ctrl Pts',(10.9094793685083,15.2,-1.91720382148212));
#186167=CARTESIAN_POINT('Ctrl Pts',(10.9131423355024,15.2,-1.91941269650147));
#186168=CARTESIAN_POINT('Ctrl Pts',(10.9168053019974,15.2,-1.92162157121986));
#186169=CARTESIAN_POINT('Ctrl Pts',(10.920476403025,15.2,-1.92384338069638));
#186170=CARTESIAN_POINT('Ctrl Pts',(10.9241555188901,15.2,-1.92607813740126));
#186171=CARTESIAN_POINT('Ctrl Pts',(10.9287544140974,15.2,-1.92887158351071));
#186172=CARTESIAN_POINT('Ctrl Pts',(10.933365833635,15.2,-1.93168526253651));
#186173=CARTESIAN_POINT('Ctrl Pts',(10.9379895503701,15.2,-1.93451920114596));
#186174=CARTESIAN_POINT('Ctrl Pts',(10.9416885239598,15.2,-1.93678635215708));
#186175=CARTESIAN_POINT('Ctrl Pts',(10.9453953655553,15.2,-1.93906647086055));
#186176=CARTESIAN_POINT('Ctrl Pts',(10.9491099612191,15.2,-1.94135956921819));
#186177=CARTESIAN_POINT('Ctrl Pts',(10.9528245563768,15.2,-1.9436526672634));
#186178=CARTESIAN_POINT('Ctrl Pts',(10.9565469045485,15.2,-1.94595874733671));
#186179=CARTESIAN_POINT('Ctrl Pts',(10.9602768916317,15.2,-1.9482778206458));
#186180=CARTESIAN_POINT('Ctrl Pts',(10.9640068792231,15.2,-1.95059689427087));
#186181=CARTESIAN_POINT('Ctrl Pts',(10.9677445053847,15.2,-1.95292896159437));
#186182=CARTESIAN_POINT('Ctrl Pts',(10.9714896550332,15.2,-1.95527403649996));
#186183=CARTESIAN_POINT('Ctrl Pts',(10.9752348046818,15.2,-1.95761911140555));
#186184=CARTESIAN_POINT('Ctrl Pts',(10.9789874775562,15.2,-1.95997719481541));
#186185=CARTESIAN_POINT('Ctrl Pts',(10.982747561373,15.2,-1.96234829644598));
#186186=CARTESIAN_POINT('Ctrl Pts',(10.9855676239795,15.2,-1.96412662250737));
#186187=CARTESIAN_POINT('Ctrl Pts',(10.9883918563082,15.2,-1.96591227228832));
#186188=CARTESIAN_POINT('Ctrl Pts',(10.9912202085138,15.2,-1.96770525139694));
#186189=CARTESIAN_POINT('Ctrl Pts',(10.9940485607195,15.2,-1.96949823050555));
#186190=CARTESIAN_POINT('Ctrl Pts',(10.9968810333286,15.2,-1.97129853761216));
#186191=CARTESIAN_POINT('Ctrl Pts',(10.9997175803092,15.2,-1.97310617867212));
#186192=CARTESIAN_POINT('Ctrl Pts',(11.0025541272898,15.2,-1.97491381973208));
#186193=CARTESIAN_POINT('Ctrl Pts',(11.0053947479533,15.2,-1.97672879523283));
#186194=CARTESIAN_POINT('Ctrl Pts',(11.0082393950166,15.2,-1.97855110879162));
#186195=CARTESIAN_POINT('Ctrl Pts',(11.0110840420799,15.2,-1.98037342235041));
#186196=CARTESIAN_POINT('Ctrl Pts',(11.0139327161097,15.2,-1.98220307445057));
#186197=CARTESIAN_POINT('Ctrl Pts',(11.0167853701724,15.2,-1.98404007000819));
#186198=CARTESIAN_POINT('Ctrl Pts',(11.0205889092681,15.2,-1.98648939764082));
#186199=CARTESIAN_POINT('Ctrl Pts',(11.0243995234462,15.2,-1.98895178058563));
#186200=CARTESIAN_POINT('Ctrl Pts',(11.0282171033456,15.2,-1.9914272289009));
#186201=CARTESIAN_POINT('Ctrl Pts',(11.03108028801,15.2,-1.99328381496872));
#186202=CARTESIAN_POINT('Ctrl Pts',(11.0339473909669,15.2,-1.99514774970475));
#186203=CARTESIAN_POINT('Ctrl Pts',(11.0368183655713,15.2,-1.99701903872073));
#186204=CARTESIAN_POINT('Ctrl Pts',(11.0406463315365,15.2,-1.99951409062871));
#186205=CARTESIAN_POINT('Ctrl Pts',(11.0444811811421,15.2,-2.00202221673409));
#186206=CARTESIAN_POINT('Ctrl Pts',(11.0483228056052,15.2,-2.00454342530442));
#186207=CARTESIAN_POINT('Ctrl Pts',(11.0512040246067,15.2,-2.00643433216157));
#186208=CARTESIAN_POINT('Ctrl Pts',(11.054089053326,15.2,-2.00833259817077));
#186209=CARTESIAN_POINT('Ctrl Pts',(11.0569778483713,15.2,-2.01023822844873));
#186210=CARTESIAN_POINT('Ctrl Pts',(11.0598666428919,15.2,-2.0121438583805));
#186211=CARTESIAN_POINT('Ctrl Pts',(11.0627592032704,15.2,-2.01405685176123));
#186212=CARTESIAN_POINT('Ctrl Pts',(11.0656554825603,15.2,-2.01597721191324));
#186213=CARTESIAN_POINT('Ctrl Pts',(11.0685517618502,15.2,-2.01789757206525));
#186214=CARTESIAN_POINT('Ctrl Pts',(11.0714517619883,15.2,-2.01982529946402));
#186215=CARTESIAN_POINT('Ctrl Pts',(11.0743554365915,15.2,-2.02176039893602));
#186216=CARTESIAN_POINT('Ctrl Pts',(11.0772591111946,15.2,-2.02369549840801));
#186217=CARTESIAN_POINT('Ctrl Pts',(11.0801664606224,15.2,-2.0256379687708));
#186218=CARTESIAN_POINT('Ctrl Pts',(11.0830774402249,15.2,-2.02758781424162));
#186219=CARTESIAN_POINT('Ctrl Pts',(11.0869587467142,15.2,-2.03018760843886));
#186220=CARTESIAN_POINT('Ctrl Pts',(11.0908465071015,15.2,-2.03280051410986));
#186221=CARTESIAN_POINT('Ctrl Pts',(11.0947406148699,15.2,-2.03542653842099));
#186222=CARTESIAN_POINT('Ctrl Pts',(11.0996082487847,15.2,-2.03870906827322));
#186223=CARTESIAN_POINT('Ctrl Pts',(11.1044858017942,15.2,-2.04201209690141));
#186224=CARTESIAN_POINT('Ctrl Pts',(11.109373068344,15.2,-2.04533564077359));
#186225=CARTESIAN_POINT('Ctrl Pts',(11.1123054290197,15.2,-2.04732976760406));
#186226=CARTESIAN_POINT('Ctrl Pts',(11.115241287263,15.2,-2.04933128014494));
#186227=CARTESIAN_POINT('Ctrl Pts',(11.1181805983574,15.2,-2.05134018047957));
#186228=CARTESIAN_POINT('Ctrl Pts',(11.1211199089177,15.2,-2.05334908044926));
#186229=CARTESIAN_POINT('Ctrl Pts',(11.1240626720612,15.2,-2.05536536827688));
#186230=CARTESIAN_POINT('Ctrl Pts',(11.1270088455794,15.2,-2.057389048204));
#186231=CARTESIAN_POINT('Ctrl Pts',(11.1299550190977,15.2,-2.05941272813112));
#186232=CARTESIAN_POINT('Ctrl Pts',(11.1329046024572,15.2,-2.06144379860736));
#186233=CARTESIAN_POINT('Ctrl Pts',(11.1358575515583,15.2,-2.06348226449163));
#186234=CARTESIAN_POINT('Ctrl Pts',(11.1388105006593,15.2,-2.0655207303759));
#186235=CARTESIAN_POINT('Ctrl Pts',(11.1417668155519,15.2,-2.06756658960153));
#186236=CARTESIAN_POINT('Ctrl Pts',(11.1447264536524,15.2,-2.06961984698462));
#186237=CARTESIAN_POINT('Ctrl Pts',(11.1486726381448,15.2,-2.07235752374407));
#186238=CARTESIAN_POINT('Ctrl Pts',(11.1526247300242,15.2,-2.07510835093346));
#186239=CARTESIAN_POINT('Ctrl Pts',(11.1565826280493,15.2,-2.07787233466777));
#186240=CARTESIAN_POINT('Ctrl Pts',(11.160540525535,15.2,-2.08063631802549));
#186241=CARTESIAN_POINT('Ctrl Pts',(11.1645042281476,15.2,-2.08341345872595));
#186242=CARTESIAN_POINT('Ctrl Pts',(11.1684736354338,15.2,-2.08620376133031));
#186243=CARTESIAN_POINT('Ctrl Pts',(11.1714506910337,15.2,-2.08829648837863));
#186244=CARTESIAN_POINT('Ctrl Pts',(11.1744309554584,15.2,-2.09039662001811));
#186245=CARTESIAN_POINT('Ctrl Pts',(11.1774143860995,15.2,-2.09250415802386));
#186246=CARTESIAN_POINT('Ctrl Pts',(11.1823867706822,15.2,-2.09601672149441));
#186247=CARTESIAN_POINT('Ctrl Pts',(11.1873679517054,15.2,-2.0995498578114));
#186248=CARTESIAN_POINT('Ctrl Pts',(11.192357733204,15.2,-2.10310357882084));
#186249=CARTESIAN_POINT('Ctrl Pts',(11.1953516019945,15.2,-2.10523581134903));
#186250=CARTESIAN_POINT('Ctrl Pts',(11.1983485672053,15.2,-2.10737545409427));
#186251=CARTESIAN_POINT('Ctrl Pts',(11.2013485863459,15.2,-2.10952250901525));
#186252=CARTESIAN_POINT('Ctrl Pts',(11.2043486060315,15.2,-2.11166956432628));
#186253=CARTESIAN_POINT('Ctrl Pts',(11.2073516799846,15.2,-2.11382403163939));
#186254=CARTESIAN_POINT('Ctrl Pts',(11.2103577666719,15.2,-2.11598591299626));
#186255=CARTESIAN_POINT('Ctrl Pts',(11.2133638528131,15.2,-2.11814779396038));
#186256=CARTESIAN_POINT('Ctrl Pts',(11.2163729519875,15.2,-2.12031708903246));
#186257=CARTESIAN_POINT('Ctrl Pts',(11.2193850235866,15.2,-2.12249380045402));
#186258=CARTESIAN_POINT('Ctrl Pts',(11.2223970951858,15.2,-2.12467051187558));
#186259=CARTESIAN_POINT('Ctrl Pts',(11.2254121383653,15.2,-2.12685463855492));
#186260=CARTESIAN_POINT('Ctrl Pts',(11.2284301114777,15.2,-2.12904618348529));
#186261=CARTESIAN_POINT('Ctrl Pts',(11.2314480845901,15.2,-2.13123772841565));
#186262=CARTESIAN_POINT('Ctrl Pts',(11.2344689878767,15.2,-2.13343669205148));
#186263=CARTESIAN_POINT('Ctrl Pts',(11.2374927780305,15.2,-2.13564307406463));
#186264=CARTESIAN_POINT('Ctrl Pts',(11.2405165681844,15.2,-2.13784945607777));
#186265=CARTESIAN_POINT('Ctrl Pts',(11.2435432456968,15.2,-2.14006325823933));
#186266=CARTESIAN_POINT('Ctrl Pts',(11.2465727734614,15.2,-2.14228448028297));
#186267=CARTESIAN_POINT('Ctrl Pts',(11.2496023012261,15.2,-2.14450570232662));
#186268=CARTESIAN_POINT('Ctrl Pts',(11.2526346804489,15.2,-2.14673434582808));
#186269=CARTESIAN_POINT('Ctrl Pts',(11.2556698710466,15.2,-2.14897041128751));
#186270=CARTESIAN_POINT('Ctrl Pts',(11.2597167922111,15.2,-2.15195183217089));
#186271=CARTESIAN_POINT('Ctrl Pts',(11.2637687107826,15.2,-2.1549464469966));
#186272=CARTESIAN_POINT('Ctrl Pts',(11.2678255117444,15.2,-2.15795426128535));
#186273=CARTESIAN_POINT('Ctrl Pts',(11.2718823121534,15.2,-2.16096207516428));
#186274=CARTESIAN_POINT('Ctrl Pts',(11.2759439872013,15.2,-2.16398308926437));
#186275=CARTESIAN_POINT('Ctrl Pts',(11.2800104638684,15.2,-2.16701730357055));
#186276=CARTESIAN_POINT('Ctrl Pts',(11.2840769410895,15.2,-2.17005151829013));
#186277=CARTESIAN_POINT('Ctrl Pts',(11.2881482245559,15.2,-2.17309893283267));
#186278=CARTESIAN_POINT('Ctrl Pts',(11.2922242989999,15.2,-2.17615954700001));
#186279=CARTESIAN_POINT('Ctrl Pts',(10.0330625579999,15.2,-2.64164356400002));
#186280=CARTESIAN_POINT('Ctrl Pts',(10.0330625579999,11.6,-2.64164356400002));
#186281=CARTESIAN_POINT('Ctrl Pts',(10.0332343599999,15.2,-2.64167330400001));
#186282=CARTESIAN_POINT('Ctrl Pts',(10.0332343599999,11.6,-2.64167330400001));
#186283=CARTESIAN_POINT('Ctrl Pts',(10.0335839819999,15.2,-2.64173373800002));
#186284=CARTESIAN_POINT('Ctrl Pts',(10.0335839819999,11.6,-2.64173373800002));
#186285=CARTESIAN_POINT('Ctrl Pts',(10.0341137859999,15.2,-2.64182504800001));
#186286=CARTESIAN_POINT('Ctrl Pts',(10.0341137859999,11.6,-2.64182504800001));
#186287=CARTESIAN_POINT('Ctrl Pts',(10.0348275719999,15.2,-2.64194751900002));
#186288=CARTESIAN_POINT('Ctrl Pts',(10.0348275719999,11.6,-2.64194751900002));
#186289=CARTESIAN_POINT('Ctrl Pts',(10.0357305589999,15.2,-2.64210152600001));
#186290=CARTESIAN_POINT('Ctrl Pts',(10.0357305589999,11.6,-2.64210152600001));
#186291=CARTESIAN_POINT('Ctrl Pts',(10.0366483389999,15.2,-2.64225710800002));
#186292=CARTESIAN_POINT('Ctrl Pts',(10.0366483389999,11.6,-2.64225710800002));
#186293=CARTESIAN_POINT('Ctrl Pts',(10.0375756569999,15.2,-2.64241335000001));
#186294=CARTESIAN_POINT('Ctrl Pts',(10.0375756569999,11.6,-2.64241335000001));
#186295=CARTESIAN_POINT('Ctrl Pts',(10.0385124889999,15.2,-2.64257022900001));
#186296=CARTESIAN_POINT('Ctrl Pts',(10.0385124889999,11.6,-2.64257022900001));
#186297=CARTESIAN_POINT('Ctrl Pts',(10.0394588109999,15.2,-2.64272772400002));
#186298=CARTESIAN_POINT('Ctrl Pts',(10.0394588109999,11.6,-2.64272772400002));
#186299=CARTESIAN_POINT('Ctrl Pts',(10.0404146009999,15.2,-2.64288581300002));
#186300=CARTESIAN_POINT('Ctrl Pts',(10.0404146009999,11.6,-2.64288581300002));
#186301=CARTESIAN_POINT('Ctrl Pts',(10.0413798349999,15.2,-2.64304447300002));
#186302=CARTESIAN_POINT('Ctrl Pts',(10.0413798349999,11.6,-2.64304447300002));
#186303=CARTESIAN_POINT('Ctrl Pts',(10.0423544889999,15.2,-2.64320368200002));
#186304=CARTESIAN_POINT('Ctrl Pts',(10.0423544889999,11.6,-2.64320368200002));
#186305=CARTESIAN_POINT('Ctrl Pts',(10.0433385409999,15.2,-2.64336341800002));
#186306=CARTESIAN_POINT('Ctrl Pts',(10.0433385409999,11.6,-2.64336341800002));
#186307=CARTESIAN_POINT('Ctrl Pts',(10.0443319679999,15.2,-2.64352366000002));
#186308=CARTESIAN_POINT('Ctrl Pts',(10.0443319679999,11.6,-2.64352366000002));
#186309=CARTESIAN_POINT('Ctrl Pts',(10.0453347469999,15.2,-2.64368438700001));
#186310=CARTESIAN_POINT('Ctrl Pts',(10.0453347469999,11.6,-2.64368438700001));
#186311=CARTESIAN_POINT('Ctrl Pts',(10.0463468539999,15.2,-2.64384557600001));
#186312=CARTESIAN_POINT('Ctrl Pts',(10.0463468539999,11.6,-2.64384557600002));
#186313=CARTESIAN_POINT('Ctrl Pts',(10.0473682679999,15.2,-2.64400720800001));
#186314=CARTESIAN_POINT('Ctrl Pts',(10.0473682679999,11.6,-2.64400720800001));
#186315=CARTESIAN_POINT('Ctrl Pts',(10.0483989659999,15.2,-2.64416925900001));
#186316=CARTESIAN_POINT('Ctrl Pts',(10.0483989659999,11.6,-2.64416925900001));
#186317=CARTESIAN_POINT('Ctrl Pts',(10.0494389259999,15.2,-2.64433171000002));
#186318=CARTESIAN_POINT('Ctrl Pts',(10.0494389259999,11.6,-2.64433171000002));
#186319=CARTESIAN_POINT('Ctrl Pts',(10.0504881239999,15.2,-2.64449453900002));
#186320=CARTESIAN_POINT('Ctrl Pts',(10.0504881239999,11.6,-2.64449453900002));
#186321=CARTESIAN_POINT('Ctrl Pts',(10.0515465379999,15.2,-2.64465772600001));
#186322=CARTESIAN_POINT('Ctrl Pts',(10.0515465379999,11.6,-2.64465772600001));
#186323=CARTESIAN_POINT('Ctrl Pts',(10.0526141479999,15.2,-2.64482124900002));
#186324=CARTESIAN_POINT('Ctrl Pts',(10.0526141479999,11.6,-2.64482124900002));
#186325=CARTESIAN_POINT('Ctrl Pts',(10.0536909299999,15.2,-2.64498508700001));
#186326=CARTESIAN_POINT('Ctrl Pts',(10.0536909299999,11.6,-2.64498508700001));
#186327=CARTESIAN_POINT('Ctrl Pts',(10.0547768619999,15.2,-2.64514922200001));
#186328=CARTESIAN_POINT('Ctrl Pts',(10.0547768619999,11.6,-2.64514922200001));
#186329=CARTESIAN_POINT('Ctrl Pts',(10.0558719239999,15.2,-2.64531363100001));
#186330=CARTESIAN_POINT('Ctrl Pts',(10.0558719239999,11.6,-2.64531363100002));
#186331=CARTESIAN_POINT('Ctrl Pts',(10.0569760909999,15.2,-2.64547829500001));
#186332=CARTESIAN_POINT('Ctrl Pts',(10.0569760909999,11.6,-2.64547829500001));
#186333=CARTESIAN_POINT('Ctrl Pts',(10.0580893439999,15.2,-2.64564319300002));
#186334=CARTESIAN_POINT('Ctrl Pts',(10.0580893439999,11.6,-2.64564319300002));
#186335=CARTESIAN_POINT('Ctrl Pts',(10.0592116599999,15.2,-2.64580830600002));
#186336=CARTESIAN_POINT('Ctrl Pts',(10.0592116599999,11.6,-2.64580830600002));
#186337=CARTESIAN_POINT('Ctrl Pts',(10.0603430189999,15.2,-2.64597361200002));
#186338=CARTESIAN_POINT('Ctrl Pts',(10.0603430189999,11.6,-2.64597361200002));
#186339=CARTESIAN_POINT('Ctrl Pts',(10.0614833969999,15.2,-2.64613909300001));
#186340=CARTESIAN_POINT('Ctrl Pts',(10.0614833969999,11.6,-2.64613909300001));
#186341=CARTESIAN_POINT('Ctrl Pts',(10.0626327749999,15.2,-2.64630472800001));
#186342=CARTESIAN_POINT('Ctrl Pts',(10.0626327749999,11.6,-2.64630472800001));
#186343=CARTESIAN_POINT('Ctrl Pts',(10.0637911309999,15.2,-2.64647049800002));
#186344=CARTESIAN_POINT('Ctrl Pts',(10.0637911309999,11.6,-2.64647049800002));
#186345=CARTESIAN_POINT('Ctrl Pts',(10.0649584439999,15.2,-2.64663638300001));
#186346=CARTESIAN_POINT('Ctrl Pts',(10.0649584439999,11.6,-2.64663638300001));
#186347=CARTESIAN_POINT('Ctrl Pts',(10.0661346919999,15.2,-2.64680236400002));
#186348=CARTESIAN_POINT('Ctrl Pts',(10.0661346919999,11.6,-2.64680236400002));
#186349=CARTESIAN_POINT('Ctrl Pts',(10.0673198549999,15.2,-2.64696842100001));
#186350=CARTESIAN_POINT('Ctrl Pts',(10.0673198549999,11.6,-2.64696842100001));
#186351=CARTESIAN_POINT('Ctrl Pts',(10.0685139109999,15.2,-2.64713453500002));
#186352=CARTESIAN_POINT('Ctrl Pts',(10.0685139109999,11.6,-2.64713453500002));
#186353=CARTESIAN_POINT('Ctrl Pts',(10.0697168409999,15.2,-2.64730068700001));
#186354=CARTESIAN_POINT('Ctrl Pts',(10.0697168409999,11.6,-2.64730068700001));
#186355=CARTESIAN_POINT('Ctrl Pts',(10.0709286239999,15.2,-2.64746685700001));
#186356=CARTESIAN_POINT('Ctrl Pts',(10.0709286239999,11.6,-2.64746685700001));
#186357=CARTESIAN_POINT('Ctrl Pts',(10.0721492369999,15.2,-2.64763302600001));
#186358=CARTESIAN_POINT('Ctrl Pts',(10.0721492369999,11.6,-2.64763302600001));
#186359=CARTESIAN_POINT('Ctrl Pts',(10.0733786619999,15.2,-2.64779917600002));
#186360=CARTESIAN_POINT('Ctrl Pts',(10.0733786619999,11.6,-2.64779917600002));
#186361=CARTESIAN_POINT('Ctrl Pts',(10.0746168779999,15.2,-2.64796528800002));
#186362=CARTESIAN_POINT('Ctrl Pts',(10.0746168779999,11.6,-2.64796528800002));
#186363=CARTESIAN_POINT('Ctrl Pts',(10.0758638629999,15.2,-2.64813134200002));
#186364=CARTESIAN_POINT('Ctrl Pts',(10.0758638629999,11.6,-2.64813134200002));
#186365=CARTESIAN_POINT('Ctrl Pts',(10.0771195969999,15.2,-2.64829732100001));
#186366=CARTESIAN_POINT('Ctrl Pts',(10.0771195969999,11.6,-2.64829732100001));
#186367=CARTESIAN_POINT('Ctrl Pts',(10.0783840629999,15.2,-2.64846320600002));
#186368=CARTESIAN_POINT('Ctrl Pts',(10.0783840629999,11.6,-2.64846320600002));
#186369=CARTESIAN_POINT('Ctrl Pts',(10.0796572369999,15.2,-2.64862897800001));
#186370=CARTESIAN_POINT('Ctrl Pts',(10.0796572369999,11.6,-2.64862897800001));
#186371=CARTESIAN_POINT('Ctrl Pts',(10.0809390999999,15.2,-2.64879461900001));
#186372=CARTESIAN_POINT('Ctrl Pts',(10.0809390999999,11.6,-2.64879461900001));
#186373=CARTESIAN_POINT('Ctrl Pts',(10.0822296339999,15.2,-2.64896011100001));
#186374=CARTESIAN_POINT('Ctrl Pts',(10.0822296339999,11.6,-2.64896011100001));
#186375=CARTESIAN_POINT('Ctrl Pts',(10.0835288159999,15.2,-2.64912543500001));
#186376=CARTESIAN_POINT('Ctrl Pts',(10.0835288159999,11.6,-2.64912543500001));
#186377=CARTESIAN_POINT('Ctrl Pts',(10.0848366279999,15.2,-2.64929057400002));
#186378=CARTESIAN_POINT('Ctrl Pts',(10.0848366279999,11.6,-2.64929057400002));
#186379=CARTESIAN_POINT('Ctrl Pts',(10.0861530489999,15.2,-2.64945550800002));
#186380=CARTESIAN_POINT('Ctrl Pts',(10.0861530489999,11.6,-2.64945550800002));
#186381=CARTESIAN_POINT('Ctrl Pts',(10.0874780619999,15.2,-2.64962022200002));
#186382=CARTESIAN_POINT('Ctrl Pts',(10.0874780619999,11.6,-2.64962022200002));
#186383=CARTESIAN_POINT('Ctrl Pts',(10.0888116439999,15.2,-2.64978469600001));
#186384=CARTESIAN_POINT('Ctrl Pts',(10.0888116439999,11.6,-2.64978469600001));
#186385=CARTESIAN_POINT('Ctrl Pts',(10.0901537779999,15.2,-2.64994891200002));
#186386=CARTESIAN_POINT('Ctrl Pts',(10.0901537779999,11.6,-2.64994891200002));
#186387=CARTESIAN_POINT('Ctrl Pts',(10.0915044419999,15.2,-2.65011285400002));
#186388=CARTESIAN_POINT('Ctrl Pts',(10.0915044419999,11.6,-2.65011285400002));
#186389=CARTESIAN_POINT('Ctrl Pts',(10.0928636199999,15.2,-2.65027650400001));
#186390=CARTESIAN_POINT('Ctrl Pts',(10.0928636199999,11.6,-2.65027650400001));
#186391=CARTESIAN_POINT('Ctrl Pts',(10.0942312899999,15.2,-2.65043984300001));
#186392=CARTESIAN_POINT('Ctrl Pts',(10.0942312899999,11.6,-2.65043984300001));
#186393=CARTESIAN_POINT('Ctrl Pts',(10.0956074329999,15.2,-2.65060285500001));
#186394=CARTESIAN_POINT('Ctrl Pts',(10.0956074329999,11.6,-2.65060285500002));
#186395=CARTESIAN_POINT('Ctrl Pts',(10.0969920309999,15.2,-2.65076552200001));
#186396=CARTESIAN_POINT('Ctrl Pts',(10.0969920309999,11.6,-2.65076552200001));
#186397=CARTESIAN_POINT('Ctrl Pts',(10.0983850649999,15.2,-2.65092782800001));
#186398=CARTESIAN_POINT('Ctrl Pts',(10.0983850649999,11.6,-2.65092782800001));
#186399=CARTESIAN_POINT('Ctrl Pts',(10.0997865139999,15.2,-2.65108975600001));
#186400=CARTESIAN_POINT('Ctrl Pts',(10.0997865139999,11.6,-2.65108975600001));
#186401=CARTESIAN_POINT('Ctrl Pts',(10.1011963619999,15.2,-2.65125128600001));
#186402=CARTESIAN_POINT('Ctrl Pts',(10.1011963619999,11.6,-2.65125128600001));
#186403=CARTESIAN_POINT('Ctrl Pts',(10.1026145869999,15.2,-2.65141240300002));
#186404=CARTESIAN_POINT('Ctrl Pts',(10.1026145869999,11.6,-2.65141240300002));
#186405=CARTESIAN_POINT('Ctrl Pts',(10.1040411729999,15.2,-2.65157309000001));
#186406=CARTESIAN_POINT('Ctrl Pts',(10.1040411729999,11.6,-2.65157309000001));
#186407=CARTESIAN_POINT('Ctrl Pts',(10.1054760989999,15.2,-2.65173333000002));
#186408=CARTESIAN_POINT('Ctrl Pts',(10.1054760989999,11.6,-2.65173333000002));
#186409=CARTESIAN_POINT('Ctrl Pts',(10.1069193469999,15.2,-2.65189310700002));
#186410=CARTESIAN_POINT('Ctrl Pts',(10.1069193469999,11.6,-2.65189310700002));
#186411=CARTESIAN_POINT('Ctrl Pts',(10.1083708989999,15.2,-2.65205240400002));
#186412=CARTESIAN_POINT('Ctrl Pts',(10.1083708989999,11.6,-2.65205240400002));
#186413=CARTESIAN_POINT('Ctrl Pts',(10.1098307359999,15.2,-2.65221120400001));
#186414=CARTESIAN_POINT('Ctrl Pts',(10.1098307359999,11.6,-2.65221120400001));
#186415=CARTESIAN_POINT('Ctrl Pts',(10.1112988399999,15.2,-2.65236949000001));
#186416=CARTESIAN_POINT('Ctrl Pts',(10.1112988399999,11.6,-2.65236949000002));
#186417=CARTESIAN_POINT('Ctrl Pts',(10.1127751919999,15.2,-2.65252724600002));
#186418=CARTESIAN_POINT('Ctrl Pts',(10.1127751919999,11.6,-2.65252724600002));
#186419=CARTESIAN_POINT('Ctrl Pts',(10.1142597739999,15.2,-2.65268445700002));
#186420=CARTESIAN_POINT('Ctrl Pts',(10.1142597739999,11.6,-2.65268445700002));
#186421=CARTESIAN_POINT('Ctrl Pts',(10.1157525679999,15.2,-2.65284110400001));
#186422=CARTESIAN_POINT('Ctrl Pts',(10.1157525679999,11.6,-2.65284110400001));
#186423=CARTESIAN_POINT('Ctrl Pts',(10.1172535539999,15.2,-2.65299717300001));
#186424=CARTESIAN_POINT('Ctrl Pts',(10.1172535539999,11.6,-2.65299717300001));
#186425=CARTESIAN_POINT('Ctrl Pts',(10.1187627169999,15.2,-2.65315264700002));
#186426=CARTESIAN_POINT('Ctrl Pts',(10.1187627169999,11.6,-2.65315264700002));
#186427=CARTESIAN_POINT('Ctrl Pts',(10.1202800349999,15.2,-2.65330750900001));
#186428=CARTESIAN_POINT('Ctrl Pts',(10.1202800349999,11.6,-2.65330750900001));
#186429=CARTESIAN_POINT('Ctrl Pts',(10.1218054939999,15.2,-2.65346174700001));
#186430=CARTESIAN_POINT('Ctrl Pts',(10.1218054939999,11.6,-2.65346174700001));
#186431=CARTESIAN_POINT('Ctrl Pts',(10.1233390739999,15.2,-2.65361533900002));
#186432=CARTESIAN_POINT('Ctrl Pts',(10.1233390739999,11.6,-2.65361533900002));
#186433=CARTESIAN_POINT('Ctrl Pts',(10.1248807569999,15.2,-2.65376827500001));
#186434=CARTESIAN_POINT('Ctrl Pts',(10.1248807569999,11.6,-2.65376827500001));
#186435=CARTESIAN_POINT('Ctrl Pts',(10.1264305249999,15.2,-2.65392053400001));
#186436=CARTESIAN_POINT('Ctrl Pts',(10.1264305249999,11.6,-2.65392053400001));
#186437=CARTESIAN_POINT('Ctrl Pts',(10.1279883609999,15.2,-2.65407210400001));
#186438=CARTESIAN_POINT('Ctrl Pts',(10.1279883609999,11.6,-2.65407210400001));
#186439=CARTESIAN_POINT('Ctrl Pts',(10.1295542479999,15.2,-2.65422296900002));
#186440=CARTESIAN_POINT('Ctrl Pts',(10.1295542479999,11.6,-2.65422296900002));
#186441=CARTESIAN_POINT('Ctrl Pts',(10.1311281659999,15.2,-2.65437311200001));
#186442=CARTESIAN_POINT('Ctrl Pts',(10.1311281659999,11.6,-2.65437311200001));
#186443=CARTESIAN_POINT('Ctrl Pts',(10.1327100999999,15.2,-2.65452251800002));
#186444=CARTESIAN_POINT('Ctrl Pts',(10.1327100999999,11.6,-2.65452251800002));
#186445=CARTESIAN_POINT('Ctrl Pts',(10.1343000309999,15.2,-2.65467117300001));
#186446=CARTESIAN_POINT('Ctrl Pts',(10.1343000309999,11.6,-2.65467117300001));
#186447=CARTESIAN_POINT('Ctrl Pts',(10.1358979419999,15.2,-2.65481905900002));
#186448=CARTESIAN_POINT('Ctrl Pts',(10.1358979419999,11.6,-2.65481905900002));
#186449=CARTESIAN_POINT('Ctrl Pts',(10.1375038149999,15.2,-2.65496616300001));
#186450=CARTESIAN_POINT('Ctrl Pts',(10.1375038149999,11.6,-2.65496616300001));
#186451=CARTESIAN_POINT('Ctrl Pts',(10.1391176329999,15.2,-2.65511246900001));
#186452=CARTESIAN_POINT('Ctrl Pts',(10.1391176329999,11.6,-2.65511246900001));
#186453=CARTESIAN_POINT('Ctrl Pts',(10.1407393799999,15.2,-2.65525796100002));
#186454=CARTESIAN_POINT('Ctrl Pts',(10.1407393799999,11.6,-2.65525796100002));
#186455=CARTESIAN_POINT('Ctrl Pts',(10.1423690359999,15.2,-2.65540262600001));
#186456=CARTESIAN_POINT('Ctrl Pts',(10.1423690359999,11.6,-2.65540262600001));
#186457=CARTESIAN_POINT('Ctrl Pts',(10.1440065869999,15.2,-2.65554644800002));
#186458=CARTESIAN_POINT('Ctrl Pts',(10.1440065869999,11.6,-2.65554644800002));
#186459=CARTESIAN_POINT('Ctrl Pts',(10.1456520129999,15.2,-2.65568941000002));
#186460=CARTESIAN_POINT('Ctrl Pts',(10.1456520129999,11.6,-2.65568941000002));
#186461=CARTESIAN_POINT('Ctrl Pts',(10.1473052979999,15.2,-2.65583150200001));
#186462=CARTESIAN_POINT('Ctrl Pts',(10.1473052979999,11.6,-2.65583150200001));
#186463=CARTESIAN_POINT('Ctrl Pts',(10.1489664269999,15.2,-2.65597270400002));
#186464=CARTESIAN_POINT('Ctrl Pts',(10.1489664269999,11.6,-2.65597270400002));
#186465=CARTESIAN_POINT('Ctrl Pts',(10.1506353799999,15.2,-2.65611300300002));
#186466=CARTESIAN_POINT('Ctrl Pts',(10.1506353799999,11.6,-2.65611300300002));
#186467=CARTESIAN_POINT('Ctrl Pts',(10.1523121419999,15.2,-2.65625238700002));
#186468=CARTESIAN_POINT('Ctrl Pts',(10.1523121419999,11.6,-2.65625238700002));
#186469=CARTESIAN_POINT('Ctrl Pts',(10.1539966949999,15.2,-2.65639083800002));
#186470=CARTESIAN_POINT('Ctrl Pts',(10.1539966949999,11.6,-2.65639083800002));
#186471=CARTESIAN_POINT('Ctrl Pts',(10.1556890229999,15.2,-2.65652834200001));
#186472=CARTESIAN_POINT('Ctrl Pts',(10.1556890229999,11.6,-2.65652834200001));
#186473=CARTESIAN_POINT('Ctrl Pts',(10.1573891099999,15.2,-2.65666488700001));
#186474=CARTESIAN_POINT('Ctrl Pts',(10.1573891099999,11.6,-2.65666488700001));
#186475=CARTESIAN_POINT('Ctrl Pts',(10.1590969379999,15.2,-2.65680045500002));
#186476=CARTESIAN_POINT('Ctrl Pts',(10.1590969379999,11.6,-2.65680045500002));
#186477=CARTESIAN_POINT('Ctrl Pts',(10.1608124909999,15.2,-2.65693503500001));
#186478=CARTESIAN_POINT('Ctrl Pts',(10.1608124909999,11.6,-2.65693503500001));
#186479=CARTESIAN_POINT('Ctrl Pts',(10.1625357519999,15.2,-2.65706861000002));
#186480=CARTESIAN_POINT('Ctrl Pts',(10.1625357519999,11.6,-2.65706861000002));
#186481=CARTESIAN_POINT('Ctrl Pts',(10.1642667059999,15.2,-2.65720116800002));
#186482=CARTESIAN_POINT('Ctrl Pts',(10.1642667059999,11.6,-2.65720116800002));
#186483=CARTESIAN_POINT('Ctrl Pts',(10.1660053339999,15.2,-2.65733269300001));
#186484=CARTESIAN_POINT('Ctrl Pts',(10.1660053339999,11.6,-2.65733269300001));
#186485=CARTESIAN_POINT('Ctrl Pts',(10.1677516209999,15.2,-2.65746317300001));
#186486=CARTESIAN_POINT('Ctrl Pts',(10.1677516209999,11.6,-2.65746317300001));
#186487=CARTESIAN_POINT('Ctrl Pts',(10.1695055519999,15.2,-2.65759259200001));
#186488=CARTESIAN_POINT('Ctrl Pts',(10.1695055519999,11.6,-2.65759259200001));
#186489=CARTESIAN_POINT('Ctrl Pts',(10.1712671079999,15.2,-2.65772093700001));
#186490=CARTESIAN_POINT('Ctrl Pts',(10.1712671079999,11.6,-2.65772093700001));
#186491=CARTESIAN_POINT('Ctrl Pts',(10.1730362739999,15.2,-2.65784819400002));
#186492=CARTESIAN_POINT('Ctrl Pts',(10.1730362739999,11.6,-2.65784819400002));
#186493=CARTESIAN_POINT('Ctrl Pts',(10.1748130349999,15.2,-2.65797434800001));
#186494=CARTESIAN_POINT('Ctrl Pts',(10.1748130349999,11.6,-2.65797434800001));
#186495=CARTESIAN_POINT('Ctrl Pts',(10.1765973729999,15.2,-2.65809938700002));
#186496=CARTESIAN_POINT('Ctrl Pts',(10.1765973729999,11.6,-2.65809938700002));
#186497=CARTESIAN_POINT('Ctrl Pts',(10.1783892739999,15.2,-2.65822329700002));
#186498=CARTESIAN_POINT('Ctrl Pts',(10.1783892739999,11.6,-2.65822329700002));
#186499=CARTESIAN_POINT('Ctrl Pts',(10.1801887189999,15.2,-2.65834606300002));
#186500=CARTESIAN_POINT('Ctrl Pts',(10.1801887189999,11.6,-2.65834606300002));
#186501=CARTESIAN_POINT('Ctrl Pts',(10.1819956949999,15.2,-2.65846767300001));
#186502=CARTESIAN_POINT('Ctrl Pts',(10.1819956949999,11.6,-2.65846767300001));
#186503=CARTESIAN_POINT('Ctrl Pts',(10.1838101829999,15.2,-2.65858811100002));
#186504=CARTESIAN_POINT('Ctrl Pts',(10.1838101829999,11.6,-2.65858811100002));
#186505=CARTESIAN_POINT('Ctrl Pts',(10.1856321709999,15.2,-2.65870736700001));
#186506=CARTESIAN_POINT('Ctrl Pts',(10.1856321709999,11.6,-2.65870736700002));
#186507=CARTESIAN_POINT('Ctrl Pts',(10.1874616389999,15.2,-2.65882542500002));
#186508=CARTESIAN_POINT('Ctrl Pts',(10.1874616389999,11.6,-2.65882542500002));
#186509=CARTESIAN_POINT('Ctrl Pts',(10.1892985749999,15.2,-2.65894227200001));
#186510=CARTESIAN_POINT('Ctrl Pts',(10.1892985749999,11.6,-2.65894227200001));
#186511=CARTESIAN_POINT('Ctrl Pts',(10.1911429609999,15.2,-2.65905789600001));
#186512=CARTESIAN_POINT('Ctrl Pts',(10.1911429609999,11.6,-2.65905789600001));
#186513=CARTESIAN_POINT('Ctrl Pts',(10.1929947809999,15.2,-2.65917228300002));
#186514=CARTESIAN_POINT('Ctrl Pts',(10.1929947809999,11.6,-2.65917228300002));
#186515=CARTESIAN_POINT('Ctrl Pts',(10.1948540199999,15.2,-2.65928541800001));
#186516=CARTESIAN_POINT('Ctrl Pts',(10.1948540199999,11.6,-2.65928541800002));
#186517=CARTESIAN_POINT('Ctrl Pts',(10.1967206629999,15.2,-2.65939729100001));
#186518=CARTESIAN_POINT('Ctrl Pts',(10.1967206629999,11.6,-2.65939729100001));
#186519=CARTESIAN_POINT('Ctrl Pts',(10.1985946949999,15.2,-2.65950788700001));
#186520=CARTESIAN_POINT('Ctrl Pts',(10.1985946949999,11.6,-2.65950788700001));
#186521=CARTESIAN_POINT('Ctrl Pts',(10.2004760989999,15.2,-2.65961719300002));
#186522=CARTESIAN_POINT('Ctrl Pts',(10.2004760989999,11.6,-2.65961719300002));
#186523=CARTESIAN_POINT('Ctrl Pts',(10.2023648589999,15.2,-2.65972519600002));
#186524=CARTESIAN_POINT('Ctrl Pts',(10.2023648589999,11.6,-2.65972519600002));
#186525=CARTESIAN_POINT('Ctrl Pts',(10.2042609619999,15.2,-2.65983188400002));
#186526=CARTESIAN_POINT('Ctrl Pts',(10.2042609619999,11.6,-2.65983188400002));
#186527=CARTESIAN_POINT('Ctrl Pts',(10.2061643889999,15.2,-2.65993724300001));
#186528=CARTESIAN_POINT('Ctrl Pts',(10.2061643889999,11.6,-2.65993724300001));
#186529=CARTESIAN_POINT('Ctrl Pts',(10.2080751289999,15.2,-2.66004126100002));
#186530=CARTESIAN_POINT('Ctrl Pts',(10.2080751289999,11.6,-2.66004126100002));
#186531=CARTESIAN_POINT('Ctrl Pts',(10.2099931639999,15.2,-2.66014392600002));
#186532=CARTESIAN_POINT('Ctrl Pts',(10.2099931639999,11.6,-2.66014392600002));
#186533=CARTESIAN_POINT('Ctrl Pts',(10.2119184799999,15.2,-2.66024522300001));
#186534=CARTESIAN_POINT('Ctrl Pts',(10.2119184799999,11.6,-2.66024522300001));
#186535=CARTESIAN_POINT('Ctrl Pts',(10.2138510599999,15.2,-2.66034514000001));
#186536=CARTESIAN_POINT('Ctrl Pts',(10.2138510599999,11.6,-2.66034514000001));
#186537=CARTESIAN_POINT('Ctrl Pts',(10.2157908909999,15.2,-2.66044366600001));
#186538=CARTESIAN_POINT('Ctrl Pts',(10.2157908909999,11.6,-2.66044366600001));
#186539=CARTESIAN_POINT('Ctrl Pts',(10.2177379569999,15.2,-2.66054078700002));
#186540=CARTESIAN_POINT('Ctrl Pts',(10.2177379569999,11.6,-2.66054078700002));
#186541=CARTESIAN_POINT('Ctrl Pts',(10.2196922419999,15.2,-2.66063649100001));
#186542=CARTESIAN_POINT('Ctrl Pts',(10.2196922419999,11.6,-2.66063649100001));
#186543=CARTESIAN_POINT('Ctrl Pts',(10.2216537329999,15.2,-2.66073076600001));
#186544=CARTESIAN_POINT('Ctrl Pts',(10.2216537329999,11.6,-2.66073076600002));
#186545=CARTESIAN_POINT('Ctrl Pts',(10.2236224129999,15.2,-2.66082359800001));
#186546=CARTESIAN_POINT('Ctrl Pts',(10.2236224129999,11.6,-2.66082359800001));
#186547=CARTESIAN_POINT('Ctrl Pts',(10.2255982689999,15.2,-2.66091497700002));
#186548=CARTESIAN_POINT('Ctrl Pts',(10.2255982689999,11.6,-2.66091497700002));
#186549=CARTESIAN_POINT('Ctrl Pts',(10.2275812839999,15.2,-2.66100488900001));
#186550=CARTESIAN_POINT('Ctrl Pts',(10.2275812839999,11.6,-2.66100488900001));
#186551=CARTESIAN_POINT('Ctrl Pts',(10.2295714459999,15.2,-2.66109332200001));
#186552=CARTESIAN_POINT('Ctrl Pts',(10.2295714459999,11.6,-2.66109332200001));
#186553=CARTESIAN_POINT('Ctrl Pts',(10.2315687369999,15.2,-2.66118026400001));
#186554=CARTESIAN_POINT('Ctrl Pts',(10.2315687369999,11.6,-2.66118026400001));
#186555=CARTESIAN_POINT('Ctrl Pts',(10.2335731439999,15.2,-2.66126570200001));
#186556=CARTESIAN_POINT('Ctrl Pts',(10.2335731439999,11.6,-2.66126570200001));
#186557=CARTESIAN_POINT('Ctrl Pts',(10.2355846529999,15.2,-2.66134962600002));
#186558=CARTESIAN_POINT('Ctrl Pts',(10.2355846529999,11.6,-2.66134962600002));
#186559=CARTESIAN_POINT('Ctrl Pts',(10.2376032469999,15.2,-2.66143202200002));
#186560=CARTESIAN_POINT('Ctrl Pts',(10.2376032469999,11.6,-2.66143202200002));
#186561=CARTESIAN_POINT('Ctrl Pts',(10.2396289129999,15.2,-2.66151288000001));
#186562=CARTESIAN_POINT('Ctrl Pts',(10.2396289129999,11.6,-2.66151288000001));
#186563=CARTESIAN_POINT('Ctrl Pts',(10.2416616369999,15.2,-2.66159218500002));
#186564=CARTESIAN_POINT('Ctrl Pts',(10.2416616369999,11.6,-2.66159218500002));
#186565=CARTESIAN_POINT('Ctrl Pts',(10.2437014029999,15.2,-2.66166992700001));
#186566=CARTESIAN_POINT('Ctrl Pts',(10.2437014029999,11.6,-2.66166992700001));
#186567=CARTESIAN_POINT('Ctrl Pts',(10.2457481969999,15.2,-2.66174609500001));
#186568=CARTESIAN_POINT('Ctrl Pts',(10.2457481969999,11.6,-2.66174609500002));
#186569=CARTESIAN_POINT('Ctrl Pts',(10.2478020049999,15.2,-2.66182067600001));
#186570=CARTESIAN_POINT('Ctrl Pts',(10.2478020049999,11.6,-2.66182067600001));
#186571=CARTESIAN_POINT('Ctrl Pts',(10.2498628119999,15.2,-2.66189365800001));
#186572=CARTESIAN_POINT('Ctrl Pts',(10.2498628119999,11.6,-2.66189365800001));
#186573=CARTESIAN_POINT('Ctrl Pts',(10.2519306029999,15.2,-2.66196503000002));
#186574=CARTESIAN_POINT('Ctrl Pts',(10.2519306029999,11.6,-2.66196503000002));
#186575=CARTESIAN_POINT('Ctrl Pts',(10.2540053659999,15.2,-2.66203478000001));
#186576=CARTESIAN_POINT('Ctrl Pts',(10.2540053659999,11.6,-2.66203478000001));
#186577=CARTESIAN_POINT('Ctrl Pts',(10.2560870839999,15.2,-2.66210289700001));
#186578=CARTESIAN_POINT('Ctrl Pts',(10.2560870839999,11.6,-2.66210289700001));
#186579=CARTESIAN_POINT('Ctrl Pts',(10.2581757429999,15.2,-2.66216936800001));
#186580=CARTESIAN_POINT('Ctrl Pts',(10.2581757429999,11.6,-2.66216936800001));
#186581=CARTESIAN_POINT('Ctrl Pts',(10.2602713319999,15.2,-2.66223418300001));
#186582=CARTESIAN_POINT('Ctrl Pts',(10.2602713319999,11.6,-2.66223418300001));
#186583=CARTESIAN_POINT('Ctrl Pts',(10.2623738329999,15.2,-2.66229733000001));
#186584=CARTESIAN_POINT('Ctrl Pts',(10.2623738329999,11.6,-2.66229733000001));
#186585=CARTESIAN_POINT('Ctrl Pts',(10.2644832329999,15.2,-2.66235879800002));
#186586=CARTESIAN_POINT('Ctrl Pts',(10.2644832329999,11.6,-2.66235879800002));
#186587=CARTESIAN_POINT('Ctrl Pts',(10.2665995189999,15.2,-2.66241857400002));
#186588=CARTESIAN_POINT('Ctrl Pts',(10.2665995189999,11.6,-2.66241857400002));
#186589=CARTESIAN_POINT('Ctrl Pts',(10.2687226749999,15.2,-2.66247664800002));
#186590=CARTESIAN_POINT('Ctrl Pts',(10.2687226749999,11.6,-2.66247664800002));
#186591=CARTESIAN_POINT('Ctrl Pts',(10.2708526889999,15.2,-2.66253300900001));
#186592=CARTESIAN_POINT('Ctrl Pts',(10.2708526889999,11.6,-2.66253300900001));
#186593=CARTESIAN_POINT('Ctrl Pts',(10.2729895449999,15.2,-2.66258764600002));
#186594=CARTESIAN_POINT('Ctrl Pts',(10.2729895449999,11.6,-2.66258764600002));
#186595=CARTESIAN_POINT('Ctrl Pts',(10.2751332309999,15.2,-2.66264054600001));
#186596=CARTESIAN_POINT('Ctrl Pts',(10.2751332309999,11.6,-2.66264054600002));
#186597=CARTESIAN_POINT('Ctrl Pts',(10.2772837319999,15.2,-2.66269169900001));
#186598=CARTESIAN_POINT('Ctrl Pts',(10.2772837319999,11.6,-2.66269169900002));
#186599=CARTESIAN_POINT('Ctrl Pts',(10.2794410339999,15.2,-2.66274109400001));
#186600=CARTESIAN_POINT('Ctrl Pts',(10.2794410339999,11.6,-2.66274109400001));
#186601=CARTESIAN_POINT('Ctrl Pts',(10.2816051239999,15.2,-2.66278872000001));
#186602=CARTESIAN_POINT('Ctrl Pts',(10.2816051239999,11.6,-2.66278872000001));
#186603=CARTESIAN_POINT('Ctrl Pts',(10.2837759869999,15.2,-2.66283456600001));
#186604=CARTESIAN_POINT('Ctrl Pts',(10.2837759869999,11.6,-2.66283456600001));
#186605=CARTESIAN_POINT('Ctrl Pts',(10.2859536089999,15.2,-2.66287862000001));
#186606=CARTESIAN_POINT('Ctrl Pts',(10.2859536089999,11.6,-2.66287862000001));
#186607=CARTESIAN_POINT('Ctrl Pts',(10.2881379789999,15.2,-2.66292087100001));
#186608=CARTESIAN_POINT('Ctrl Pts',(10.2881379789999,11.6,-2.66292087100001));
#186609=CARTESIAN_POINT('Ctrl Pts',(10.2903290789999,15.2,-2.66296131100002));
#186610=CARTESIAN_POINT('Ctrl Pts',(10.2903290789999,11.6,-2.66296131100002));
#186611=CARTESIAN_POINT('Ctrl Pts',(10.2925268989999,15.2,-2.66299992600001));
#186612=CARTESIAN_POINT('Ctrl Pts',(10.2925268989999,11.6,-2.66299992600001));
#186613=CARTESIAN_POINT('Ctrl Pts',(10.2947314239999,15.2,-2.66303670600001));
#186614=CARTESIAN_POINT('Ctrl Pts',(10.2947314239999,11.6,-2.66303670600002));
#186615=CARTESIAN_POINT('Ctrl Pts',(10.2969426399999,15.2,-2.66307164000001));
#186616=CARTESIAN_POINT('Ctrl Pts',(10.2969426399999,11.6,-2.66307164000001));
#186617=CARTESIAN_POINT('Ctrl Pts',(10.2991605329999,15.2,-2.66310471900002));
#186618=CARTESIAN_POINT('Ctrl Pts',(10.2991605329999,11.6,-2.66310471900002));
#186619=CARTESIAN_POINT('Ctrl Pts',(10.3013850909999,15.2,-2.66313593100001));
#186620=CARTESIAN_POINT('Ctrl Pts',(10.3013850909999,11.6,-2.66313593100001));
#186621=CARTESIAN_POINT('Ctrl Pts',(10.3036162999999,15.2,-2.66316526500002));
#186622=CARTESIAN_POINT('Ctrl Pts',(10.3036162999999,11.6,-2.66316526500002));
#186623=CARTESIAN_POINT('Ctrl Pts',(10.3058541459999,15.2,-2.66319271100001));
#186624=CARTESIAN_POINT('Ctrl Pts',(10.3058541459999,11.6,-2.66319271100001));
#186625=CARTESIAN_POINT('Ctrl Pts',(10.3080986159999,15.2,-2.66321825900001));
#186626=CARTESIAN_POINT('Ctrl Pts',(10.3080986159999,11.6,-2.66321825900001));
#186627=CARTESIAN_POINT('Ctrl Pts',(10.3103496959999,15.2,-2.66324189700001));
#186628=CARTESIAN_POINT('Ctrl Pts',(10.3103496959999,11.6,-2.66324189700002));
#186629=CARTESIAN_POINT('Ctrl Pts',(10.3126073739999,15.2,-2.66326361500001));
#186630=CARTESIAN_POINT('Ctrl Pts',(10.3126073739999,11.6,-2.66326361500001));
#186631=CARTESIAN_POINT('Ctrl Pts',(10.3148716349999,15.2,-2.66328340400001));
#186632=CARTESIAN_POINT('Ctrl Pts',(10.3148716349999,11.6,-2.66328340400001));
#186633=CARTESIAN_POINT('Ctrl Pts',(10.3171424659999,15.2,-2.66330125200001));
#186634=CARTESIAN_POINT('Ctrl Pts',(10.3171424659999,11.6,-2.66330125200001));
#186635=CARTESIAN_POINT('Ctrl Pts',(10.3194198549999,15.2,-2.66331714900002));
#186636=CARTESIAN_POINT('Ctrl Pts',(10.3194198549999,11.6,-2.66331714900002));
#186637=CARTESIAN_POINT('Ctrl Pts',(10.3217037879999,15.2,-2.66333108500001));
#186638=CARTESIAN_POINT('Ctrl Pts',(10.3217037879999,11.6,-2.66333108500001));
#186639=CARTESIAN_POINT('Ctrl Pts',(10.3239942509999,15.2,-2.66334305000001));
#186640=CARTESIAN_POINT('Ctrl Pts',(10.3239942509999,11.6,-2.66334305000001));
#186641=CARTESIAN_POINT('Ctrl Pts',(10.3262912319999,15.2,-2.66335303400002));
#186642=CARTESIAN_POINT('Ctrl Pts',(10.3262912319999,11.6,-2.66335303400002));
#186643=CARTESIAN_POINT('Ctrl Pts',(10.3285947179999,15.2,-2.66336102400002));
#186644=CARTESIAN_POINT('Ctrl Pts',(10.3285947179999,11.6,-2.66336102400002));
#186645=CARTESIAN_POINT('Ctrl Pts',(10.3309046949999,15.2,-2.66336701400002));
#186646=CARTESIAN_POINT('Ctrl Pts',(10.3309046949999,11.6,-2.66336701400002));
#186647=CARTESIAN_POINT('Ctrl Pts',(10.3332211489999,15.2,-2.66337099000001));
#186648=CARTESIAN_POINT('Ctrl Pts',(10.3332211489999,11.6,-2.66337099000001));
#186649=CARTESIAN_POINT('Ctrl Pts',(10.3355440699999,15.2,-2.66337294600001));
#186650=CARTESIAN_POINT('Ctrl Pts',(10.3355440699999,11.6,-2.66337294600001));
#186651=CARTESIAN_POINT('Ctrl Pts',(10.3378734419999,15.2,-2.66337286900002));
#186652=CARTESIAN_POINT('Ctrl Pts',(10.3378734419999,11.6,-2.66337286900002));
#186653=CARTESIAN_POINT('Ctrl Pts',(10.3402092539999,15.2,-2.66337074900001));
#186654=CARTESIAN_POINT('Ctrl Pts',(10.3402092539999,11.6,-2.66337074900001));
#186655=CARTESIAN_POINT('Ctrl Pts',(10.3425514919999,15.2,-2.66336657700001));
#186656=CARTESIAN_POINT('Ctrl Pts',(10.3425514919999,11.6,-2.66336657700002));
#186657=CARTESIAN_POINT('Ctrl Pts',(10.3449001429999,15.2,-2.66336034300001));
#186658=CARTESIAN_POINT('Ctrl Pts',(10.3449001429999,11.6,-2.66336034300001));
#186659=CARTESIAN_POINT('Ctrl Pts',(10.3472551949999,15.2,-2.66335203800002));
#186660=CARTESIAN_POINT('Ctrl Pts',(10.3472551949999,11.6,-2.66335203800002));
#186661=CARTESIAN_POINT('Ctrl Pts',(10.3496166339999,15.2,-2.66334165000002));
#186662=CARTESIAN_POINT('Ctrl Pts',(10.3496166339999,11.6,-2.66334165000002));
#186663=CARTESIAN_POINT('Ctrl Pts',(10.3519844489999,15.2,-2.66332917100002));
#186664=CARTESIAN_POINT('Ctrl Pts',(10.3519844489999,11.6,-2.66332917100002));
#186665=CARTESIAN_POINT('Ctrl Pts',(10.3543586239999,15.2,-2.66331459100002));
#186666=CARTESIAN_POINT('Ctrl Pts',(10.3543586239999,11.6,-2.66331459100002));
#186667=CARTESIAN_POINT('Ctrl Pts',(10.3567391499999,15.2,-2.66329790000002));
#186668=CARTESIAN_POINT('Ctrl Pts',(10.3567391499999,11.6,-2.66329790000002));
#186669=CARTESIAN_POINT('Ctrl Pts',(10.3591260109999,15.2,-2.66327908600001));
#186670=CARTESIAN_POINT('Ctrl Pts',(10.3591260109999,11.6,-2.66327908600001));
#186671=CARTESIAN_POINT('Ctrl Pts',(10.3615191969999,15.2,-2.66325814300002));
#186672=CARTESIAN_POINT('Ctrl Pts',(10.3615191969999,11.6,-2.66325814300002));
#186673=CARTESIAN_POINT('Ctrl Pts',(10.3639186939999,15.2,-2.66323506100001));
#186674=CARTESIAN_POINT('Ctrl Pts',(10.3639186939999,11.6,-2.66323506100001));
#186675=CARTESIAN_POINT('Ctrl Pts',(10.3663244889999,15.2,-2.66320982800002));
#186676=CARTESIAN_POINT('Ctrl Pts',(10.3663244889999,11.6,-2.66320982800002));
#186677=CARTESIAN_POINT('Ctrl Pts',(10.3687365709999,15.2,-2.66318243600002));
#186678=CARTESIAN_POINT('Ctrl Pts',(10.3687365709999,11.6,-2.66318243600002));
#186679=CARTESIAN_POINT('Ctrl Pts',(10.3711549249999,15.2,-2.66315287500001));
#186680=CARTESIAN_POINT('Ctrl Pts',(10.3711549249999,11.6,-2.66315287500001));
#186681=CARTESIAN_POINT('Ctrl Pts',(10.3735795409999,15.2,-2.66312113600002));
#186682=CARTESIAN_POINT('Ctrl Pts',(10.3735795409999,11.6,-2.66312113600002));
#186683=CARTESIAN_POINT('Ctrl Pts',(10.3760104039999,15.2,-2.66308720900001));
#186684=CARTESIAN_POINT('Ctrl Pts',(10.3760104039999,11.6,-2.66308720900002));
#186685=CARTESIAN_POINT('Ctrl Pts',(10.3784475029999,15.2,-2.66305108600001));
#186686=CARTESIAN_POINT('Ctrl Pts',(10.3784475029999,11.6,-2.66305108600001));
#186687=CARTESIAN_POINT('Ctrl Pts',(10.3808908259999,15.2,-2.66301275600001));
#186688=CARTESIAN_POINT('Ctrl Pts',(10.3808908259999,11.6,-2.66301275600001));
#186689=CARTESIAN_POINT('Ctrl Pts',(10.3833403579999,15.2,-2.66297221000002));
#186690=CARTESIAN_POINT('Ctrl Pts',(10.3833403579999,11.6,-2.66297221000002));
#186691=CARTESIAN_POINT('Ctrl Pts',(10.3857960899999,15.2,-2.66292943900002));
#186692=CARTESIAN_POINT('Ctrl Pts',(10.3857960899999,11.6,-2.66292943900002));
#186693=CARTESIAN_POINT('Ctrl Pts',(10.3882580069999,15.2,-2.66288443300001));
#186694=CARTESIAN_POINT('Ctrl Pts',(10.3882580069999,11.6,-2.66288443300001));
#186695=CARTESIAN_POINT('Ctrl Pts',(10.3907260989999,15.2,-2.66283718400001));
#186696=CARTESIAN_POINT('Ctrl Pts',(10.3907260989999,11.6,-2.66283718400001));
#186697=CARTESIAN_POINT('Ctrl Pts',(10.3932003519999,15.2,-2.66278768200001));
#186698=CARTESIAN_POINT('Ctrl Pts',(10.3932003519999,11.6,-2.66278768200001));
#186699=CARTESIAN_POINT('Ctrl Pts',(10.3956807539999,15.2,-2.66273591800001));
#186700=CARTESIAN_POINT('Ctrl Pts',(10.3956807539999,11.6,-2.66273591800001));
#186701=CARTESIAN_POINT('Ctrl Pts',(10.3981672919999,15.2,-2.66268188300002));
#186702=CARTESIAN_POINT('Ctrl Pts',(10.3981672919999,11.6,-2.66268188300002));
#186703=CARTESIAN_POINT('Ctrl Pts',(10.4006599549999,15.2,-2.66262556800001));
#186704=CARTESIAN_POINT('Ctrl Pts',(10.4006599549999,11.6,-2.66262556800001));
#186705=CARTESIAN_POINT('Ctrl Pts',(10.4031587299999,15.2,-2.66256696400001));
#186706=CARTESIAN_POINT('Ctrl Pts',(10.4031587299999,11.6,-2.66256696400002));
#186707=CARTESIAN_POINT('Ctrl Pts',(10.4056636059999,15.2,-2.66250606100002));
#186708=CARTESIAN_POINT('Ctrl Pts',(10.4056636059999,11.6,-2.66250606100002));
#186709=CARTESIAN_POINT('Ctrl Pts',(10.4081745689999,15.2,-2.66244285100001));
#186710=CARTESIAN_POINT('Ctrl Pts',(10.4081745689999,11.6,-2.66244285100001));
#186711=CARTESIAN_POINT('Ctrl Pts',(10.4106916089999,15.2,-2.66237732400001));
#186712=CARTESIAN_POINT('Ctrl Pts',(10.4106916089999,11.6,-2.66237732400001));
#186713=CARTESIAN_POINT('Ctrl Pts',(10.4132147119999,15.2,-2.66230947300001));
#186714=CARTESIAN_POINT('Ctrl Pts',(10.4132147119999,11.6,-2.66230947300001));
#186715=CARTESIAN_POINT('Ctrl Pts',(10.4157438659999,15.2,-2.66223928800001));
#186716=CARTESIAN_POINT('Ctrl Pts',(10.4157438659999,11.6,-2.66223928800001));
#186717=CARTESIAN_POINT('Ctrl Pts',(10.4182790609999,15.2,-2.66216675900001));
#186718=CARTESIAN_POINT('Ctrl Pts',(10.4182790609999,11.6,-2.66216675900001));
#186719=CARTESIAN_POINT('Ctrl Pts',(10.4208202819999,15.2,-2.66209187800001));
#186720=CARTESIAN_POINT('Ctrl Pts',(10.4208202819999,11.6,-2.66209187800001));
#186721=CARTESIAN_POINT('Ctrl Pts',(10.4233675199999,15.2,-2.66201463800002));
#186722=CARTESIAN_POINT('Ctrl Pts',(10.4233675199999,11.6,-2.66201463800002));
#186723=CARTESIAN_POINT('Ctrl Pts',(10.4259207609999,15.2,-2.66193502800002));
#186724=CARTESIAN_POINT('Ctrl Pts',(10.4259207609999,11.6,-2.66193502800002));
#186725=CARTESIAN_POINT('Ctrl Pts',(10.4284799939999,15.2,-2.66185304000001));
#186726=CARTESIAN_POINT('Ctrl Pts',(10.4284799939999,11.6,-2.66185304000001));
#186727=CARTESIAN_POINT('Ctrl Pts',(10.4310452059999,15.2,-2.66176866400002));
#186728=CARTESIAN_POINT('Ctrl Pts',(10.4310452059999,11.6,-2.66176866400002));
#186729=CARTESIAN_POINT('Ctrl Pts',(10.4336163859999,15.2,-2.66168189400001));
#186730=CARTESIAN_POINT('Ctrl Pts',(10.4336163859999,11.6,-2.66168189400001));
#186731=CARTESIAN_POINT('Ctrl Pts',(10.4361935219999,15.2,-2.66159272000001));
#186732=CARTESIAN_POINT('Ctrl Pts',(10.4361935219999,11.6,-2.66159272000001));
#186733=CARTESIAN_POINT('Ctrl Pts',(10.4387766019999,15.2,-2.66150113300001));
#186734=CARTESIAN_POINT('Ctrl Pts',(10.4387766019999,11.6,-2.66150113300002));
#186735=CARTESIAN_POINT('Ctrl Pts',(10.4413656149999,15.2,-2.66140712400002));
#186736=CARTESIAN_POINT('Ctrl Pts',(10.4413656149999,11.6,-2.66140712400002));
#186737=CARTESIAN_POINT('Ctrl Pts',(10.4439605469999,15.2,-2.66131068600002));
#186738=CARTESIAN_POINT('Ctrl Pts',(10.4439605469999,11.6,-2.66131068600002));
#186739=CARTESIAN_POINT('Ctrl Pts',(10.4465613889999,15.2,-2.66121180900001));
#186740=CARTESIAN_POINT('Ctrl Pts',(10.4465613889999,11.6,-2.66121180900001));
#186741=CARTESIAN_POINT('Ctrl Pts',(10.4491681279999,15.2,-2.66111048600001));
#186742=CARTESIAN_POINT('Ctrl Pts',(10.4491681279999,11.6,-2.66111048600001));
#186743=CARTESIAN_POINT('Ctrl Pts',(10.4517807519999,15.2,-2.66100670700002));
#186744=CARTESIAN_POINT('Ctrl Pts',(10.4517807519999,11.6,-2.66100670700002));
#186745=CARTESIAN_POINT('Ctrl Pts',(10.4543992489999,15.2,-2.66090046400001));
#186746=CARTESIAN_POINT('Ctrl Pts',(10.4543992489999,11.6,-2.66090046400001));
#186747=CARTESIAN_POINT('Ctrl Pts',(10.4570236089999,15.2,-2.66079175000002));
#186748=CARTESIAN_POINT('Ctrl Pts',(10.4570236089999,11.6,-2.66079175000002));
#186749=CARTESIAN_POINT('Ctrl Pts',(10.4596538179999,15.2,-2.66068055600002));
#186750=CARTESIAN_POINT('Ctrl Pts',(10.4596538179999,11.6,-2.66068055600002));
#186751=CARTESIAN_POINT('Ctrl Pts',(10.4622898669999,15.2,-2.66056687100001));
#186752=CARTESIAN_POINT('Ctrl Pts',(10.4622898669999,11.6,-2.66056687100001));
#186753=CARTESIAN_POINT('Ctrl Pts',(10.4649317429999,15.2,-2.66045069100001));
#186754=CARTESIAN_POINT('Ctrl Pts',(10.4649317429999,11.6,-2.66045069100001));
#186755=CARTESIAN_POINT('Ctrl Pts',(10.4675794329999,15.2,-2.66033200500001));
#186756=CARTESIAN_POINT('Ctrl Pts',(10.4675794329999,11.6,-2.66033200500001));
#186757=CARTESIAN_POINT('Ctrl Pts',(10.4702329269999,15.2,-2.66021080500002));
#186758=CARTESIAN_POINT('Ctrl Pts',(10.4702329269999,11.6,-2.66021080500002));
#186759=CARTESIAN_POINT('Ctrl Pts',(10.4728922149999,15.2,-2.66008708400001));
#186760=CARTESIAN_POINT('Ctrl Pts',(10.4728922149999,11.6,-2.66008708400001));
#186761=CARTESIAN_POINT('Ctrl Pts',(10.4755572819999,15.2,-2.65996083200001));
#186762=CARTESIAN_POINT('Ctrl Pts',(10.4755572819999,11.6,-2.65996083200001));
#186763=CARTESIAN_POINT('Ctrl Pts',(10.4782281199999,15.2,-2.65983204300001));
#186764=CARTESIAN_POINT('Ctrl Pts',(10.4782281199999,11.6,-2.65983204300001));
#186765=CARTESIAN_POINT('Ctrl Pts',(10.4809047149999,15.2,-2.65970070700002));
#186766=CARTESIAN_POINT('Ctrl Pts',(10.4809047149999,11.6,-2.65970070700002));
#186767=CARTESIAN_POINT('Ctrl Pts',(10.4835870569999,15.2,-2.65956681700001));
#186768=CARTESIAN_POINT('Ctrl Pts',(10.4835870569999,11.6,-2.65956681700001));
#186769=CARTESIAN_POINT('Ctrl Pts',(10.4862751339999,15.2,-2.65943036500001));
#186770=CARTESIAN_POINT('Ctrl Pts',(10.4862751339999,11.6,-2.65943036500001));
#186771=CARTESIAN_POINT('Ctrl Pts',(10.4889689349999,15.2,-2.65929134100002));
#186772=CARTESIAN_POINT('Ctrl Pts',(10.4889689349999,11.6,-2.65929134100002));
#186773=CARTESIAN_POINT('Ctrl Pts',(10.4916684479999,15.2,-2.65914974000002));
#186774=CARTESIAN_POINT('Ctrl Pts',(10.4916684479999,11.6,-2.65914974000002));
#186775=CARTESIAN_POINT('Ctrl Pts',(10.4943736619999,15.2,-2.65900555300002));
#186776=CARTESIAN_POINT('Ctrl Pts',(10.4943736619999,11.6,-2.65900555300002));
#186777=CARTESIAN_POINT('Ctrl Pts',(10.4970845659999,15.2,-2.65885877000001));
#186778=CARTESIAN_POINT('Ctrl Pts',(10.4970845659999,11.6,-2.65885877000001));
#186779=CARTESIAN_POINT('Ctrl Pts',(10.4998011489999,15.2,-2.65870938600001));
#186780=CARTESIAN_POINT('Ctrl Pts',(10.4998011489999,11.6,-2.65870938600001));
#186781=CARTESIAN_POINT('Ctrl Pts',(10.5025233979999,15.2,-2.65855739100001));
#186782=CARTESIAN_POINT('Ctrl Pts',(10.5025233979999,11.6,-2.65855739100001));
#186783=CARTESIAN_POINT('Ctrl Pts',(10.5052513029999,15.2,-2.65840277900002));
#186784=CARTESIAN_POINT('Ctrl Pts',(10.5052513029999,11.6,-2.65840277900002));
#186785=CARTESIAN_POINT('Ctrl Pts',(10.5079848529999,15.2,-2.65824554000002));
#186786=CARTESIAN_POINT('Ctrl Pts',(10.5079848529999,11.6,-2.65824554000002));
#186787=CARTESIAN_POINT('Ctrl Pts',(10.5107240369999,15.2,-2.65808566900001));
#186788=CARTESIAN_POINT('Ctrl Pts',(10.5107240369999,11.6,-2.65808566900001));
#186789=CARTESIAN_POINT('Ctrl Pts',(10.5134688429999,15.2,-2.65792315500001));
#186790=CARTESIAN_POINT('Ctrl Pts',(10.5134688429999,11.6,-2.65792315500002));
#186791=CARTESIAN_POINT('Ctrl Pts',(10.5162192599999,15.2,-2.65775799100001));
#186792=CARTESIAN_POINT('Ctrl Pts',(10.5162192599999,11.6,-2.65775799100001));
#186793=CARTESIAN_POINT('Ctrl Pts',(10.5189752759999,15.2,-2.65759017200002));
#186794=CARTESIAN_POINT('Ctrl Pts',(10.5189752759999,11.6,-2.65759017200002));
#186795=CARTESIAN_POINT('Ctrl Pts',(10.5217368829999,15.2,-2.65741968800001));
#186796=CARTESIAN_POINT('Ctrl Pts',(10.5217368829999,11.6,-2.65741968800001));
#186797=CARTESIAN_POINT('Ctrl Pts',(10.5245040669999,15.2,-2.65724653000001));
#186798=CARTESIAN_POINT('Ctrl Pts',(10.5245040669999,11.6,-2.65724653000001));
#186799=CARTESIAN_POINT('Ctrl Pts',(10.5272768169999,15.2,-2.65707069400001));
#186800=CARTESIAN_POINT('Ctrl Pts',(10.5272768169999,11.6,-2.65707069400001));
#186801=CARTESIAN_POINT('Ctrl Pts',(10.5300551229999,15.2,-2.65689217000002));
#186802=CARTESIAN_POINT('Ctrl Pts',(10.5300551229999,11.6,-2.65689217000002));
#186803=CARTESIAN_POINT('Ctrl Pts',(10.5328389739999,15.2,-2.65671095100001));
#186804=CARTESIAN_POINT('Ctrl Pts',(10.5328389739999,11.6,-2.65671095100001));
#186805=CARTESIAN_POINT('Ctrl Pts',(10.5356283589999,15.2,-2.65652702800002));
#186806=CARTESIAN_POINT('Ctrl Pts',(10.5356283589999,11.6,-2.65652702800002));
#186807=CARTESIAN_POINT('Ctrl Pts',(10.5384232659999,15.2,-2.65634039600001));
#186808=CARTESIAN_POINT('Ctrl Pts',(10.5384232659999,11.6,-2.65634039600001));
#186809=CARTESIAN_POINT('Ctrl Pts',(10.5412236849999,15.2,-2.65615104500001));
#186810=CARTESIAN_POINT('Ctrl Pts',(10.5412236849999,11.6,-2.65615104500002));
#186811=CARTESIAN_POINT('Ctrl Pts',(10.5440296059999,15.2,-2.65595897000001));
#186812=CARTESIAN_POINT('Ctrl Pts',(10.5440296059999,11.6,-2.65595897000001));
#186813=CARTESIAN_POINT('Ctrl Pts',(10.5468410149999,15.2,-2.65576416200001));
#186814=CARTESIAN_POINT('Ctrl Pts',(10.5468410149999,11.6,-2.65576416200001));
#186815=CARTESIAN_POINT('Ctrl Pts',(10.5496579039999,15.2,-2.65556661400002));
#186816=CARTESIAN_POINT('Ctrl Pts',(10.5496579039999,11.6,-2.65556661400002));
#186817=CARTESIAN_POINT('Ctrl Pts',(10.5524802599999,15.2,-2.65536631800002));
#186818=CARTESIAN_POINT('Ctrl Pts',(10.5524802599999,11.6,-2.65536631800002));
#186819=CARTESIAN_POINT('Ctrl Pts',(10.5553080749999,15.2,-2.65516326700002));
#186820=CARTESIAN_POINT('Ctrl Pts',(10.5553080749999,11.6,-2.65516326700002));
#186821=CARTESIAN_POINT('Ctrl Pts',(10.5581413349999,15.2,-2.65495745500001));
#186822=CARTESIAN_POINT('Ctrl Pts',(10.5581413349999,11.6,-2.65495745500001));
#186823=CARTESIAN_POINT('Ctrl Pts',(10.5609800309999,15.2,-2.65474887200002));
#186824=CARTESIAN_POINT('Ctrl Pts',(10.5609800309999,11.6,-2.65474887200002));
#186825=CARTESIAN_POINT('Ctrl Pts',(10.5638241519999,15.2,-2.65453751200001));
#186826=CARTESIAN_POINT('Ctrl Pts',(10.5638241519999,11.6,-2.65453751200001));
#186827=CARTESIAN_POINT('Ctrl Pts',(10.5666736869999,15.2,-2.65432336900002));
#186828=CARTESIAN_POINT('Ctrl Pts',(10.5666736869999,11.6,-2.65432336900002));
#186829=CARTESIAN_POINT('Ctrl Pts',(10.5695286259999,15.2,-2.65410643300001));
#186830=CARTESIAN_POINT('Ctrl Pts',(10.5695286259999,11.6,-2.65410643300001));
#186831=CARTESIAN_POINT('Ctrl Pts',(10.5723889559999,15.2,-2.65388670000001));
#186832=CARTESIAN_POINT('Ctrl Pts',(10.5723889559999,11.6,-2.65388670000001));
#186833=CARTESIAN_POINT('Ctrl Pts',(10.5752546689999,15.2,-2.65366416100001));
#186834=CARTESIAN_POINT('Ctrl Pts',(10.5752546689999,11.6,-2.65366416100001));
#186835=CARTESIAN_POINT('Ctrl Pts',(10.5781257519999,15.2,-2.65343880800001));
#186836=CARTESIAN_POINT('Ctrl Pts',(10.5781257519999,11.6,-2.65343880800002));
#186837=CARTESIAN_POINT('Ctrl Pts',(10.5810021969999,15.2,-2.65321063600001));
#186838=CARTESIAN_POINT('Ctrl Pts',(10.5810021969999,11.6,-2.65321063600001));
#186839=CARTESIAN_POINT('Ctrl Pts',(10.5838839899999,15.2,-2.65297963500001));
#186840=CARTESIAN_POINT('Ctrl Pts',(10.5838839899999,11.6,-2.65297963500001));
#186841=CARTESIAN_POINT('Ctrl Pts',(10.5867711239999,15.2,-2.65274580100002));
#186842=CARTESIAN_POINT('Ctrl Pts',(10.5867711239999,11.6,-2.65274580100002));
#186843=CARTESIAN_POINT('Ctrl Pts',(10.5896635859999,15.2,-2.65250912500001));
#186844=CARTESIAN_POINT('Ctrl Pts',(10.5896635859999,11.6,-2.65250912500001));
#186845=CARTESIAN_POINT('Ctrl Pts',(10.5925613649999,15.2,-2.65226960100001));
#186846=CARTESIAN_POINT('Ctrl Pts',(10.5925613649999,11.6,-2.65226960100002));
#186847=CARTESIAN_POINT('Ctrl Pts',(10.5954644519999,15.2,-2.65202722100002));
#186848=CARTESIAN_POINT('Ctrl Pts',(10.5954644519999,11.6,-2.65202722100002));
#186849=CARTESIAN_POINT('Ctrl Pts',(10.5983728359999,15.2,-2.65178197900001));
#186850=CARTESIAN_POINT('Ctrl Pts',(10.5983728359999,11.6,-2.65178197900001));
#186851=CARTESIAN_POINT('Ctrl Pts',(10.6012865059999,15.2,-2.65153386700002));
#186852=CARTESIAN_POINT('Ctrl Pts',(10.6012865059999,11.6,-2.65153386700002));
#186853=CARTESIAN_POINT('Ctrl Pts',(10.6042054519999,15.2,-2.65128287800001));
#186854=CARTESIAN_POINT('Ctrl Pts',(10.6042054519999,11.6,-2.65128287800001));
#186855=CARTESIAN_POINT('Ctrl Pts',(10.6071296629999,15.2,-2.65102900700001));
#186856=CARTESIAN_POINT('Ctrl Pts',(10.6071296629999,11.6,-2.65102900700001));
#186857=CARTESIAN_POINT('Ctrl Pts',(10.6100591289999,15.2,-2.65077224400001));
#186858=CARTESIAN_POINT('Ctrl Pts',(10.6100591289999,11.6,-2.65077224400002));
#186859=CARTESIAN_POINT('Ctrl Pts',(10.6129938389999,15.2,-2.65051258500002));
#186860=CARTESIAN_POINT('Ctrl Pts',(10.6129938389999,11.6,-2.65051258500002));
#186861=CARTESIAN_POINT('Ctrl Pts',(10.6159337839999,15.2,-2.65025002200002));
#186862=CARTESIAN_POINT('Ctrl Pts',(10.6159337839999,11.6,-2.65025002200002));
#186863=CARTESIAN_POINT('Ctrl Pts',(10.6188789509999,15.2,-2.64998454800002));
#186864=CARTESIAN_POINT('Ctrl Pts',(10.6188789509999,11.6,-2.64998454800002));
#186865=CARTESIAN_POINT('Ctrl Pts',(10.6218293329999,15.2,-2.64971615600002));
#186866=CARTESIAN_POINT('Ctrl Pts',(10.6218293329999,11.6,-2.64971615600002));
#186867=CARTESIAN_POINT('Ctrl Pts',(10.6247849159999,15.2,-2.64944484000001));
#186868=CARTESIAN_POINT('Ctrl Pts',(10.6247849159999,11.6,-2.64944484000001));
#186869=CARTESIAN_POINT('Ctrl Pts',(10.6277456919999,15.2,-2.64917059200001));
#186870=CARTESIAN_POINT('Ctrl Pts',(10.6277456919999,11.6,-2.64917059200001));
#186871=CARTESIAN_POINT('Ctrl Pts',(10.6307116499999,15.2,-2.64889340600002));
#186872=CARTESIAN_POINT('Ctrl Pts',(10.6307116499999,11.6,-2.64889340600002));
#186873=CARTESIAN_POINT('Ctrl Pts',(10.6336827789999,15.2,-2.64861327700002));
#186874=CARTESIAN_POINT('Ctrl Pts',(10.6336827789999,11.6,-2.64861327700002));
#186875=CARTESIAN_POINT('Ctrl Pts',(10.6366590699999,15.2,-2.64833019500001));
#186876=CARTESIAN_POINT('Ctrl Pts',(10.6366590699999,11.6,-2.64833019500002));
#186877=CARTESIAN_POINT('Ctrl Pts',(10.6396405129999,15.2,-2.64804415600001));
#186878=CARTESIAN_POINT('Ctrl Pts',(10.6396405129999,11.6,-2.64804415600001));
#186879=CARTESIAN_POINT('Ctrl Pts',(10.6426270949999,15.2,-2.64775515100002));
#186880=CARTESIAN_POINT('Ctrl Pts',(10.6426270949999,11.6,-2.64775515100002));
#186881=CARTESIAN_POINT('Ctrl Pts',(10.6456188079999,15.2,-2.64746317600002));
#186882=CARTESIAN_POINT('Ctrl Pts',(10.6456188079999,11.6,-2.64746317600002));
#186883=CARTESIAN_POINT('Ctrl Pts',(10.6486156409999,15.2,-2.64716822200001));
#186884=CARTESIAN_POINT('Ctrl Pts',(10.6486156409999,11.6,-2.64716822200001));
#186885=CARTESIAN_POINT('Ctrl Pts',(10.6516175849999,15.2,-2.64687028400001));
#186886=CARTESIAN_POINT('Ctrl Pts',(10.6516175849999,11.6,-2.64687028400001));
#186887=CARTESIAN_POINT('Ctrl Pts',(10.6546246289999,15.2,-2.64656935600001));
#186888=CARTESIAN_POINT('Ctrl Pts',(10.6546246289999,11.6,-2.64656935600002));
#186889=CARTESIAN_POINT('Ctrl Pts',(10.6576367619999,15.2,-2.64626542900002));
#186890=CARTESIAN_POINT('Ctrl Pts',(10.6576367619999,11.6,-2.64626542900002));
#186891=CARTESIAN_POINT('Ctrl Pts',(10.6606539749999,15.2,-2.64595849900001));
#186892=CARTESIAN_POINT('Ctrl Pts',(10.6606539749999,11.6,-2.64595849900001));
#186893=CARTESIAN_POINT('Ctrl Pts',(10.6636762569999,15.2,-2.64564855800002));
#186894=CARTESIAN_POINT('Ctrl Pts',(10.6636762569999,11.6,-2.64564855800002));
#186895=CARTESIAN_POINT('Ctrl Pts',(10.6667035989999,15.2,-2.64533559900002));
#186896=CARTESIAN_POINT('Ctrl Pts',(10.6667035989999,11.6,-2.64533559900002));
#186897=CARTESIAN_POINT('Ctrl Pts',(10.6697359889999,15.2,-2.64501961700002));
#186898=CARTESIAN_POINT('Ctrl Pts',(10.6697359889999,11.6,-2.64501961700002));
#186899=CARTESIAN_POINT('Ctrl Pts',(10.6727734179999,15.2,-2.64470060600001));
#186900=CARTESIAN_POINT('Ctrl Pts',(10.6727734179999,11.6,-2.64470060600001));
#186901=CARTESIAN_POINT('Ctrl Pts',(10.6758158769999,15.2,-2.64437855800002));
#186902=CARTESIAN_POINT('Ctrl Pts',(10.6758158769999,11.6,-2.64437855800002));
#186903=CARTESIAN_POINT('Ctrl Pts',(10.6788633539999,15.2,-2.64405346800002));
#186904=CARTESIAN_POINT('Ctrl Pts',(10.6788633539999,11.6,-2.64405346800002));
#186905=CARTESIAN_POINT('Ctrl Pts',(10.6819158399999,15.2,-2.64372532800001));
#186906=CARTESIAN_POINT('Ctrl Pts',(10.6819158399999,11.6,-2.64372532800001));
#186907=CARTESIAN_POINT('Ctrl Pts',(10.6849733239999,15.2,-2.64339413300001));
#186908=CARTESIAN_POINT('Ctrl Pts',(10.6849733239999,11.6,-2.64339413300001));
#186909=CARTESIAN_POINT('Ctrl Pts',(10.6880357989999,15.2,-2.64305987600002));
#186910=CARTESIAN_POINT('Ctrl Pts',(10.6880357989999,11.6,-2.64305987600002));
#186911=CARTESIAN_POINT('Ctrl Pts',(10.6911032509999,15.2,-2.64272255200002));
#186912=CARTESIAN_POINT('Ctrl Pts',(10.6911032509999,11.6,-2.64272255200002));
#186913=CARTESIAN_POINT('Ctrl Pts',(10.6941756719999,15.2,-2.64238215300002));
#186914=CARTESIAN_POINT('Ctrl Pts',(10.6941756719999,11.6,-2.64238215300002));
#186915=CARTESIAN_POINT('Ctrl Pts',(10.6972530529999,15.2,-2.64203867300001));
#186916=CARTESIAN_POINT('Ctrl Pts',(10.6972530529999,11.6,-2.64203867300001));
#186917=CARTESIAN_POINT('Ctrl Pts',(10.7003353819999,15.2,-2.64169210700001));
#186918=CARTESIAN_POINT('Ctrl Pts',(10.7003353819999,11.6,-2.64169210700001));
#186919=CARTESIAN_POINT('Ctrl Pts',(10.7034226499999,15.2,-2.64134244800001));
#186920=CARTESIAN_POINT('Ctrl Pts',(10.7034226499999,11.6,-2.64134244800002));
#186921=CARTESIAN_POINT('Ctrl Pts',(10.7065148479999,15.2,-2.64098969000001));
#186922=CARTESIAN_POINT('Ctrl Pts',(10.7065148479999,11.6,-2.64098969000001));
#186923=CARTESIAN_POINT('Ctrl Pts',(10.7096119649999,15.2,-2.64063382700002));
#186924=CARTESIAN_POINT('Ctrl Pts',(10.7096119649999,11.6,-2.64063382700002));
#186925=CARTESIAN_POINT('Ctrl Pts',(10.7127139909999,15.2,-2.64027485300002));
#186926=CARTESIAN_POINT('Ctrl Pts',(10.7127139909999,11.6,-2.64027485300002));
#186927=CARTESIAN_POINT('Ctrl Pts',(10.7158209159999,15.2,-2.63991276000001));
#186928=CARTESIAN_POINT('Ctrl Pts',(10.7158209159999,11.6,-2.63991276000001));
#186929=CARTESIAN_POINT('Ctrl Pts',(10.7189327309999,15.2,-2.63954754400002));
#186930=CARTESIAN_POINT('Ctrl Pts',(10.7189327309999,11.6,-2.63954754400002));
#186931=CARTESIAN_POINT('Ctrl Pts',(10.7220494259999,15.2,-2.63917919900001));
#186932=CARTESIAN_POINT('Ctrl Pts',(10.7220494259999,11.6,-2.63917919900001));
#186933=CARTESIAN_POINT('Ctrl Pts',(10.7251709909999,15.2,-2.63880771700002));
#186934=CARTESIAN_POINT('Ctrl Pts',(10.7251709909999,11.6,-2.63880771700002));
#186935=CARTESIAN_POINT('Ctrl Pts',(10.7282974159999,15.2,-2.63843309400002));
#186936=CARTESIAN_POINT('Ctrl Pts',(10.7282974159999,11.6,-2.63843309400002));
#186937=CARTESIAN_POINT('Ctrl Pts',(10.7314286909999,15.2,-2.63805532300001));
#186938=CARTESIAN_POINT('Ctrl Pts',(10.7314286909999,11.6,-2.63805532300002));
#186939=CARTESIAN_POINT('Ctrl Pts',(10.7345648079999,15.2,-2.63767439800001));
#186940=CARTESIAN_POINT('Ctrl Pts',(10.7345648079999,11.6,-2.63767439800001));
#186941=CARTESIAN_POINT('Ctrl Pts',(10.7377057549999,15.2,-2.63729031300001));
#186942=CARTESIAN_POINT('Ctrl Pts',(10.7377057549999,11.6,-2.63729031300001));
#186943=CARTESIAN_POINT('Ctrl Pts',(10.7408515229999,15.2,-2.63690306300001));
#186944=CARTESIAN_POINT('Ctrl Pts',(10.7408515229999,11.6,-2.63690306300001));
#186945=CARTESIAN_POINT('Ctrl Pts',(10.7440021029999,15.2,-2.63651264000002));
#186946=CARTESIAN_POINT('Ctrl Pts',(10.7440021029999,11.6,-2.63651264000002));
#186947=CARTESIAN_POINT('Ctrl Pts',(10.7471574849999,15.2,-2.63611904100001));
#186948=CARTESIAN_POINT('Ctrl Pts',(10.7471574849999,11.6,-2.63611904100001));
#186949=CARTESIAN_POINT('Ctrl Pts',(10.7503176589999,15.2,-2.63572225700001));
#186950=CARTESIAN_POINT('Ctrl Pts',(10.7503176589999,11.6,-2.63572225700001));
#186951=CARTESIAN_POINT('Ctrl Pts',(10.7534826149999,15.2,-2.63532228500001));
#186952=CARTESIAN_POINT('Ctrl Pts',(10.7534826149999,11.6,-2.63532228500001));
#186953=CARTESIAN_POINT('Ctrl Pts',(10.7566523439999,15.2,-2.63491911700001));
#186954=CARTESIAN_POINT('Ctrl Pts',(10.7566523439999,11.6,-2.63491911700001));
#186955=CARTESIAN_POINT('Ctrl Pts',(10.7598268359999,15.2,-2.63451274700001));
#186956=CARTESIAN_POINT('Ctrl Pts',(10.7598268359999,11.6,-2.63451274700001));
#186957=CARTESIAN_POINT('Ctrl Pts',(10.7630060819999,15.2,-2.63410317200002));
#186958=CARTESIAN_POINT('Ctrl Pts',(10.7630060819999,11.6,-2.63410317200002));
#186959=CARTESIAN_POINT('Ctrl Pts',(10.7661900709999,15.2,-2.63369038300001));
#186960=CARTESIAN_POINT('Ctrl Pts',(10.7661900709999,11.6,-2.63369038300001));
#186961=CARTESIAN_POINT('Ctrl Pts',(10.7693787949999,15.2,-2.63327437600001));
#186962=CARTESIAN_POINT('Ctrl Pts',(10.7693787949999,11.6,-2.63327437600001));
#186963=CARTESIAN_POINT('Ctrl Pts',(10.7725722439999,15.2,-2.63285514400001));
#186964=CARTESIAN_POINT('Ctrl Pts',(10.7725722439999,11.6,-2.63285514400002));
#186965=CARTESIAN_POINT('Ctrl Pts',(10.7757704079999,15.2,-2.63243268200001));
#186966=CARTESIAN_POINT('Ctrl Pts',(10.7757704079999,11.6,-2.63243268200001));
#186967=CARTESIAN_POINT('Ctrl Pts',(10.7789732769999,15.2,-2.63200698600001));
#186968=CARTESIAN_POINT('Ctrl Pts',(10.7789732769999,11.6,-2.63200698600001));
#186969=CARTESIAN_POINT('Ctrl Pts',(10.7821808439999,15.2,-2.63157804700001));
#186970=CARTESIAN_POINT('Ctrl Pts',(10.7821808439999,11.6,-2.63157804700001));
#186971=CARTESIAN_POINT('Ctrl Pts',(10.7853930959999,15.2,-2.63114586100002));
#186972=CARTESIAN_POINT('Ctrl Pts',(10.7853930959999,11.6,-2.63114586100002));
#186973=CARTESIAN_POINT('Ctrl Pts',(10.7886100249999,15.2,-2.63071042400002));
#186974=CARTESIAN_POINT('Ctrl Pts',(10.7886100249999,11.6,-2.63071042400002));
#186975=CARTESIAN_POINT('Ctrl Pts',(10.7918316229999,15.2,-2.63027172700002));
#186976=CARTESIAN_POINT('Ctrl Pts',(10.7918316229999,11.6,-2.63027172700002));
#186977=CARTESIAN_POINT('Ctrl Pts',(10.7950578779999,15.2,-2.62982976600002));
#186978=CARTESIAN_POINT('Ctrl Pts',(10.7950578779999,11.6,-2.62982976600002));
#186979=CARTESIAN_POINT('Ctrl Pts',(10.7982887819999,15.2,-2.62938453500002));
#186980=CARTESIAN_POINT('Ctrl Pts',(10.7982887819999,11.6,-2.62938453500002));
#186981=CARTESIAN_POINT('Ctrl Pts',(10.8015243249999,15.2,-2.62893603000002));
#186982=CARTESIAN_POINT('Ctrl Pts',(10.8015243249999,11.6,-2.62893603000002));
#186983=CARTESIAN_POINT('Ctrl Pts',(10.8047644979999,15.2,-2.62848424300001));
#186984=CARTESIAN_POINT('Ctrl Pts',(10.8047644979999,11.6,-2.62848424300001));
#186985=CARTESIAN_POINT('Ctrl Pts',(10.8080092919999,15.2,-2.62802917000001));
#186986=CARTESIAN_POINT('Ctrl Pts',(10.8080092919999,11.6,-2.62802917000002));
#186987=CARTESIAN_POINT('Ctrl Pts',(10.8112586969999,15.2,-2.62757080500001));
#186988=CARTESIAN_POINT('Ctrl Pts',(10.8112586969999,11.6,-2.62757080500002));
#186989=CARTESIAN_POINT('Ctrl Pts',(10.8145127039999,15.2,-2.62710914400001));
#186990=CARTESIAN_POINT('Ctrl Pts',(10.8145127039999,11.6,-2.62710914400001));
#186991=CARTESIAN_POINT('Ctrl Pts',(10.8177713029999,15.2,-2.62664417900002));
#186992=CARTESIAN_POINT('Ctrl Pts',(10.8177713029999,11.6,-2.62664417900002));
#186993=CARTESIAN_POINT('Ctrl Pts',(10.8210344849999,15.2,-2.62617590500001));
#186994=CARTESIAN_POINT('Ctrl Pts',(10.8210344849999,11.6,-2.62617590500001));
#186995=CARTESIAN_POINT('Ctrl Pts',(10.8243022389999,15.2,-2.62570431800001));
#186996=CARTESIAN_POINT('Ctrl Pts',(10.8243022389999,11.6,-2.62570431800001));
#186997=CARTESIAN_POINT('Ctrl Pts',(10.8275745599999,15.2,-2.62522941200002));
#186998=CARTESIAN_POINT('Ctrl Pts',(10.8275745599999,11.6,-2.62522941200002));
#186999=CARTESIAN_POINT('Ctrl Pts',(10.8308514339999,15.2,-2.62475118200001));
#187000=CARTESIAN_POINT('Ctrl Pts',(10.8308514339999,11.6,-2.62475118200001));
#187001=CARTESIAN_POINT('Ctrl Pts',(10.8341328539999,15.2,-2.62426962100001));
#187002=CARTESIAN_POINT('Ctrl Pts',(10.8341328539999,11.6,-2.62426962100002));
#187003=CARTESIAN_POINT('Ctrl Pts',(10.8374188119999,15.2,-2.62378472500002));
#187004=CARTESIAN_POINT('Ctrl Pts',(10.8374188119999,11.6,-2.62378472500002));
#187005=CARTESIAN_POINT('Ctrl Pts',(10.8407092959999,15.2,-2.62329648600002));
#187006=CARTESIAN_POINT('Ctrl Pts',(10.8407092959999,11.6,-2.62329648600002));
#187007=CARTESIAN_POINT('Ctrl Pts',(10.8440042969999,15.2,-2.62280490300002));
#187008=CARTESIAN_POINT('Ctrl Pts',(10.8440042969999,11.6,-2.62280490300002));
#187009=CARTESIAN_POINT('Ctrl Pts',(10.8473038089999,15.2,-2.62230996900001));
#187010=CARTESIAN_POINT('Ctrl Pts',(10.8473038089999,11.6,-2.62230996900001));
#187011=CARTESIAN_POINT('Ctrl Pts',(10.8506078189999,15.2,-2.62181167700001));
#187012=CARTESIAN_POINT('Ctrl Pts',(10.8506078189999,11.6,-2.62181167700001));
#187013=CARTESIAN_POINT('Ctrl Pts',(10.8539163189999,15.2,-2.62131002300002));
#187014=CARTESIAN_POINT('Ctrl Pts',(10.8539163189999,11.6,-2.62131002300002));
#187015=CARTESIAN_POINT('Ctrl Pts',(10.8572292999999,15.2,-2.62080500200002));
#187016=CARTESIAN_POINT('Ctrl Pts',(10.8572292999999,11.6,-2.62080500200002));
#187017=CARTESIAN_POINT('Ctrl Pts',(10.8605467539999,15.2,-2.62029660800001));
#187018=CARTESIAN_POINT('Ctrl Pts',(10.8605467539999,11.6,-2.62029660800001));
#187019=CARTESIAN_POINT('Ctrl Pts',(10.8638686699999,15.2,-2.61978483700001));
#187020=CARTESIAN_POINT('Ctrl Pts',(10.8638686699999,11.6,-2.61978483700001));
#187021=CARTESIAN_POINT('Ctrl Pts',(10.8671950389999,15.2,-2.61926968300001));
#187022=CARTESIAN_POINT('Ctrl Pts',(10.8671950389999,11.6,-2.61926968300001));
#187023=CARTESIAN_POINT('Ctrl Pts',(10.8705258539999,15.2,-2.61875113900001));
#187024=CARTESIAN_POINT('Ctrl Pts',(10.8705258539999,11.6,-2.61875113900001));
#187025=CARTESIAN_POINT('Ctrl Pts',(10.8738611029999,15.2,-2.61822920300002));
#187026=CARTESIAN_POINT('Ctrl Pts',(10.8738611029999,11.6,-2.61822920300002));
#187027=CARTESIAN_POINT('Ctrl Pts',(10.8772007789999,15.2,-2.61770386800002));
#187028=CARTESIAN_POINT('Ctrl Pts',(10.8772007789999,11.6,-2.61770386800002));
#187029=CARTESIAN_POINT('Ctrl Pts',(10.8805448709999,15.2,-2.61717512900002));
#187030=CARTESIAN_POINT('Ctrl Pts',(10.8805448709999,11.6,-2.61717512900002));
#187031=CARTESIAN_POINT('Ctrl Pts',(10.8838933719999,15.2,-2.61664298100001));
#187032=CARTESIAN_POINT('Ctrl Pts',(10.8838933719999,11.6,-2.61664298100001));
#187033=CARTESIAN_POINT('Ctrl Pts',(10.8872462719999,15.2,-2.61610741800002));
#187034=CARTESIAN_POINT('Ctrl Pts',(10.8872462719999,11.6,-2.61610741800002));
#187035=CARTESIAN_POINT('Ctrl Pts',(10.8906035619999,15.2,-2.61556843700002));
#187036=CARTESIAN_POINT('Ctrl Pts',(10.8906035619999,11.6,-2.61556843700002));
#187037=CARTESIAN_POINT('Ctrl Pts',(10.8939652319999,15.2,-2.61502603200002));
#187038=CARTESIAN_POINT('Ctrl Pts',(10.8939652319999,11.6,-2.61502603200002));
#187039=CARTESIAN_POINT('Ctrl Pts',(10.8973312739999,15.2,-2.61448019700001));
#187040=CARTESIAN_POINT('Ctrl Pts',(10.8973312739999,11.6,-2.61448019700001));
#187041=CARTESIAN_POINT('Ctrl Pts',(10.9007016779999,15.2,-2.61393092800001));
#187042=CARTESIAN_POINT('Ctrl Pts',(10.9007016779999,11.6,-2.61393092800001));
#187043=CARTESIAN_POINT('Ctrl Pts',(10.9040764379999,15.2,-2.61337822000002));
#187044=CARTESIAN_POINT('Ctrl Pts',(10.9040764379999,11.6,-2.61337822000002));
#187045=CARTESIAN_POINT('Ctrl Pts',(10.9074555409999,15.2,-2.61282206600002));
#187046=CARTESIAN_POINT('Ctrl Pts',(10.9074555409999,11.6,-2.61282206600002));
#187047=CARTESIAN_POINT('Ctrl Pts',(10.9108389799999,15.2,-2.61226246400001));
#187048=CARTESIAN_POINT('Ctrl Pts',(10.9108389799999,11.6,-2.61226246400002));
#187049=CARTESIAN_POINT('Ctrl Pts',(10.9142267459999,15.2,-2.61169940700002));
#187050=CARTESIAN_POINT('Ctrl Pts',(10.9142267459999,11.6,-2.61169940700002));
#187051=CARTESIAN_POINT('Ctrl Pts',(10.9176188299999,15.2,-2.61113289100001));
#187052=CARTESIAN_POINT('Ctrl Pts',(10.9176188299999,11.6,-2.61113289100001));
#187053=CARTESIAN_POINT('Ctrl Pts',(10.9210152229999,15.2,-2.61056291100001));
#187054=CARTESIAN_POINT('Ctrl Pts',(10.9210152229999,11.6,-2.61056291100001));
#187055=CARTESIAN_POINT('Ctrl Pts',(10.9244159159999,15.2,-2.60998946000001));
#187056=CARTESIAN_POINT('Ctrl Pts',(10.9244159159999,11.6,-2.60998946000001));
#187057=CARTESIAN_POINT('Ctrl Pts',(10.9278208999999,15.2,-2.60941253700001));
#187058=CARTESIAN_POINT('Ctrl Pts',(10.9278208999999,11.6,-2.60941253700001));
#187059=CARTESIAN_POINT('Ctrl Pts',(10.9312301659999,15.2,-2.60883213400001));
#187060=CARTESIAN_POINT('Ctrl Pts',(10.9312301659999,11.6,-2.60883213400001));
#187061=CARTESIAN_POINT('Ctrl Pts',(10.9346437049999,15.2,-2.60824824600002));
#187062=CARTESIAN_POINT('Ctrl Pts',(10.9346437049999,11.6,-2.60824824600002));
#187063=CARTESIAN_POINT('Ctrl Pts',(10.9380615099999,15.2,-2.60766087000002));
#187064=CARTESIAN_POINT('Ctrl Pts',(10.9380615099999,11.6,-2.60766087000002));
#187065=CARTESIAN_POINT('Ctrl Pts',(10.9414835689999,15.2,-2.60707000100002));
#187066=CARTESIAN_POINT('Ctrl Pts',(10.9414835689999,11.6,-2.60707000100002));
#187067=CARTESIAN_POINT('Ctrl Pts',(10.9449098759999,15.2,-2.60647563300001));
#187068=CARTESIAN_POINT('Ctrl Pts',(10.9449098759999,11.6,-2.60647563300001));
#187069=CARTESIAN_POINT('Ctrl Pts',(10.9483404199999,15.2,-2.60587776100001));
#187070=CARTESIAN_POINT('Ctrl Pts',(10.9483404199999,11.6,-2.60587776100001));
#187071=CARTESIAN_POINT('Ctrl Pts',(10.9517751929999,15.2,-2.60527638200001));
#187072=CARTESIAN_POINT('Ctrl Pts',(10.9517751929999,11.6,-2.60527638200002));
#187073=CARTESIAN_POINT('Ctrl Pts',(10.9552141859999,15.2,-2.60467148900001));
#187074=CARTESIAN_POINT('Ctrl Pts',(10.9552141859999,11.6,-2.60467148900001));
#187075=CARTESIAN_POINT('Ctrl Pts',(10.9586573909999,15.2,-2.60406307900002));
#187076=CARTESIAN_POINT('Ctrl Pts',(10.9586573909999,11.6,-2.60406307900002));
#187077=CARTESIAN_POINT('Ctrl Pts',(10.9621047989999,15.2,-2.60345114600002));
#187078=CARTESIAN_POINT('Ctrl Pts',(10.9621047989999,11.6,-2.60345114600002));
#187079=CARTESIAN_POINT('Ctrl Pts',(10.9655563999999,15.2,-2.60283568600002));
#187080=CARTESIAN_POINT('Ctrl Pts',(10.9655563999999,11.6,-2.60283568600002));
#187081=CARTESIAN_POINT('Ctrl Pts',(10.9690121869999,15.2,-2.60221669400002));
#187082=CARTESIAN_POINT('Ctrl Pts',(10.9690121869999,11.6,-2.60221669400002));
#187083=CARTESIAN_POINT('Ctrl Pts',(10.9724721499999,15.2,-2.60159416500001));
#187084=CARTESIAN_POINT('Ctrl Pts',(10.9724721499999,11.6,-2.60159416500001));
#187085=CARTESIAN_POINT('Ctrl Pts',(10.9759362809999,15.2,-2.60096809500002));
#187086=CARTESIAN_POINT('Ctrl Pts',(10.9759362809999,11.6,-2.60096809500002));
#187087=CARTESIAN_POINT('Ctrl Pts',(10.9794045699999,15.2,-2.60033848000001));
#187088=CARTESIAN_POINT('Ctrl Pts',(10.9794045699999,11.6,-2.60033848000001));
#187089=CARTESIAN_POINT('Ctrl Pts',(10.9828770099999,15.2,-2.59970531200001));
#187090=CARTESIAN_POINT('Ctrl Pts',(10.9828770099999,11.6,-2.59970531200001));
#187091=CARTESIAN_POINT('Ctrl Pts',(10.9863535909999,15.2,-2.59906859100001));
#187092=CARTESIAN_POINT('Ctrl Pts',(10.9863535909999,11.6,-2.59906859100001));
#187093=CARTESIAN_POINT('Ctrl Pts',(10.9898343049999,15.2,-2.59842830900002));
#187094=CARTESIAN_POINT('Ctrl Pts',(10.9898343049999,11.6,-2.59842830900002));
#187095=CARTESIAN_POINT('Ctrl Pts',(10.9933191429999,15.2,-2.59778446200002));
#187096=CARTESIAN_POINT('Ctrl Pts',(10.9933191429999,11.6,-2.59778446200002));
#187097=CARTESIAN_POINT('Ctrl Pts',(10.9968080969999,15.2,-2.59713704600002));
#187098=CARTESIAN_POINT('Ctrl Pts',(10.9968080969999,11.6,-2.59713704600002));
#187099=CARTESIAN_POINT('Ctrl Pts',(11.0003011569999,15.2,-2.59648605600002));
#187100=CARTESIAN_POINT('Ctrl Pts',(11.0003011569999,11.6,-2.59648605600002));
#187101=CARTESIAN_POINT('Ctrl Pts',(11.0037983149999,15.2,-2.59583148900001));
#187102=CARTESIAN_POINT('Ctrl Pts',(11.0037983149999,11.6,-2.59583148900001));
#187103=CARTESIAN_POINT('Ctrl Pts',(11.0072995639999,15.2,-2.59517333800002));
#187104=CARTESIAN_POINT('Ctrl Pts',(11.0072995639999,11.6,-2.59517333800002));
#187105=CARTESIAN_POINT('Ctrl Pts',(11.0108048919999,15.2,-2.59451160000001));
#187106=CARTESIAN_POINT('Ctrl Pts',(11.0108048919999,11.6,-2.59451160000001));
#187107=CARTESIAN_POINT('Ctrl Pts',(11.0143142939999,15.2,-2.59384627000002));
#187108=CARTESIAN_POINT('Ctrl Pts',(11.0143142939999,11.6,-2.59384627000002));
#187109=CARTESIAN_POINT('Ctrl Pts',(11.0178277579999,15.2,-2.59317734300001));
#187110=CARTESIAN_POINT('Ctrl Pts',(11.0178277579999,11.6,-2.59317734300002));
#187111=CARTESIAN_POINT('Ctrl Pts',(11.0213452789999,15.2,-2.59250481600001));
#187112=CARTESIAN_POINT('Ctrl Pts',(11.0213452789999,11.6,-2.59250481600001));
#187113=CARTESIAN_POINT('Ctrl Pts',(11.0248668449999,15.2,-2.59182868300002));
#187114=CARTESIAN_POINT('Ctrl Pts',(11.0248668449999,11.6,-2.59182868300002));
#187115=CARTESIAN_POINT('Ctrl Pts',(11.0283924499999,15.2,-2.59114894000001));
#187116=CARTESIAN_POINT('Ctrl Pts',(11.0283924499999,11.6,-2.59114894000001));
#187117=CARTESIAN_POINT('Ctrl Pts',(11.0319220829999,15.2,-2.59046558300001));
#187118=CARTESIAN_POINT('Ctrl Pts',(11.0319220829999,11.6,-2.59046558300001));
#187119=CARTESIAN_POINT('Ctrl Pts',(11.0354557389999,15.2,-2.58977860600002));
#187120=CARTESIAN_POINT('Ctrl Pts',(11.0354557389999,11.6,-2.58977860600002));
#187121=CARTESIAN_POINT('Ctrl Pts',(11.0389934059999,15.2,-2.58908800800001));
#187122=CARTESIAN_POINT('Ctrl Pts',(11.0389934059999,11.6,-2.58908800800001));
#187123=CARTESIAN_POINT('Ctrl Pts',(11.0425350769999,15.2,-2.58839378100001));
#187124=CARTESIAN_POINT('Ctrl Pts',(11.0425350769999,11.6,-2.58839378100001));
#187125=CARTESIAN_POINT('Ctrl Pts',(11.0460807439999,15.2,-2.58769592200002));
#187126=CARTESIAN_POINT('Ctrl Pts',(11.0460807439999,11.6,-2.58769592200002));
#187127=CARTESIAN_POINT('Ctrl Pts',(11.0496303969999,15.2,-2.58699442700001));
#187128=CARTESIAN_POINT('Ctrl Pts',(11.0496303969999,11.6,-2.58699442700001));
#187129=CARTESIAN_POINT('Ctrl Pts',(11.0531840289999,15.2,-2.58628929200002));
#187130=CARTESIAN_POINT('Ctrl Pts',(11.0531840289999,11.6,-2.58628929200002));
#187131=CARTESIAN_POINT('Ctrl Pts',(11.0567416309999,15.2,-2.58558051000001));
#187132=CARTESIAN_POINT('Ctrl Pts',(11.0567416309999,11.6,-2.58558051000001));
#187133=CARTESIAN_POINT('Ctrl Pts',(11.0603031939999,15.2,-2.58486808000002));
#187134=CARTESIAN_POINT('Ctrl Pts',(11.0603031939999,11.6,-2.58486808000002));
#187135=CARTESIAN_POINT('Ctrl Pts',(11.0638687099999,15.2,-2.58415199700002));
#187136=CARTESIAN_POINT('Ctrl Pts',(11.0638687099999,11.6,-2.58415199700002));
#187137=CARTESIAN_POINT('Ctrl Pts',(11.0674381719999,15.2,-2.58343225400001));
#187138=CARTESIAN_POINT('Ctrl Pts',(11.0674381719999,11.6,-2.58343225400001));
#187139=CARTESIAN_POINT('Ctrl Pts',(11.0710115679999,15.2,-2.58270885000002));
#187140=CARTESIAN_POINT('Ctrl Pts',(11.0710115679999,11.6,-2.58270885000002));
#187141=CARTESIAN_POINT('Ctrl Pts',(11.0745888929999,15.2,-2.58198177900002));
#187142=CARTESIAN_POINT('Ctrl Pts',(11.0745888929999,11.6,-2.58198177900002));
#187143=CARTESIAN_POINT('Ctrl Pts',(11.0781701369999,15.2,-2.58125103800001));
#187144=CARTESIAN_POINT('Ctrl Pts',(11.0781701369999,11.6,-2.58125103800001));
#187145=CARTESIAN_POINT('Ctrl Pts',(11.0817552919999,15.2,-2.58051662100002));
#187146=CARTESIAN_POINT('Ctrl Pts',(11.0817552919999,11.6,-2.58051662100002));
#187147=CARTESIAN_POINT('Ctrl Pts',(11.0853443499999,15.2,-2.57977852500002));
#187148=CARTESIAN_POINT('Ctrl Pts',(11.0853443499999,11.6,-2.57977852500002));
#187149=CARTESIAN_POINT('Ctrl Pts',(11.0889373019999,15.2,-2.57903674500001));
#187150=CARTESIAN_POINT('Ctrl Pts',(11.0889373019999,11.6,-2.57903674500001));
#187151=CARTESIAN_POINT('Ctrl Pts',(11.0925341399999,15.2,-2.57829127800001));
#187152=CARTESIAN_POINT('Ctrl Pts',(11.0925341399999,11.6,-2.57829127800001));
#187153=CARTESIAN_POINT('Ctrl Pts',(11.0961348549999,15.2,-2.57754211900002));
#187154=CARTESIAN_POINT('Ctrl Pts',(11.0961348549999,11.6,-2.57754211900002));
#187155=CARTESIAN_POINT('Ctrl Pts',(11.0997394399999,15.2,-2.57678926400001));
#187156=CARTESIAN_POINT('Ctrl Pts',(11.0997394399999,11.6,-2.57678926400001));
#187157=CARTESIAN_POINT('Ctrl Pts',(11.1033478849999,15.2,-2.57603270800002));
#187158=CARTESIAN_POINT('Ctrl Pts',(11.1033478849999,11.6,-2.57603270800002));
#187159=CARTESIAN_POINT('Ctrl Pts',(11.1069601819999,15.2,-2.57527244800002));
#187160=CARTESIAN_POINT('Ctrl Pts',(11.1069601819999,11.6,-2.57527244800002));
#187161=CARTESIAN_POINT('Ctrl Pts',(11.1105763249999,15.2,-2.57450847900001));
#187162=CARTESIAN_POINT('Ctrl Pts',(11.1105763249999,11.6,-2.57450847900001));
#187163=CARTESIAN_POINT('Ctrl Pts',(11.1141963019999,15.2,-2.57374079800002));
#187164=CARTESIAN_POINT('Ctrl Pts',(11.1141963019999,11.6,-2.57374079800002));
#187165=CARTESIAN_POINT('Ctrl Pts',(11.1178201069999,15.2,-2.57296939900002));
#187166=CARTESIAN_POINT('Ctrl Pts',(11.1178201069999,11.6,-2.57296939900002));
#187167=CARTESIAN_POINT('Ctrl Pts',(11.1214477319999,15.2,-2.57219428100001));
#187168=CARTESIAN_POINT('Ctrl Pts',(11.1214477319999,11.6,-2.57219428100001));
#187169=CARTESIAN_POINT('Ctrl Pts',(11.1250791699999,15.2,-2.57141543700001));
#187170=CARTESIAN_POINT('Ctrl Pts',(11.1250791699999,11.6,-2.57141543700001));
#187171=CARTESIAN_POINT('Ctrl Pts',(11.1287144089999,15.2,-2.57063286400002));
#187172=CARTESIAN_POINT('Ctrl Pts',(11.1287144089999,11.6,-2.57063286400002));
#187173=CARTESIAN_POINT('Ctrl Pts',(11.1323534439999,15.2,-2.56984655900002));
#187174=CARTESIAN_POINT('Ctrl Pts',(11.1323534439999,11.6,-2.56984655900002));
#187175=CARTESIAN_POINT('Ctrl Pts',(11.1359962649999,15.2,-2.56905651800002));
#187176=CARTESIAN_POINT('Ctrl Pts',(11.1359962649999,11.6,-2.56905651800002));
#187177=CARTESIAN_POINT('Ctrl Pts',(11.1396428639999,15.2,-2.56826273300002));
#187178=CARTESIAN_POINT('Ctrl Pts',(11.1396428639999,11.6,-2.56826273300002));
#187179=CARTESIAN_POINT('Ctrl Pts',(11.1432932319999,15.2,-2.56746520500001));
#187180=CARTESIAN_POINT('Ctrl Pts',(11.1432932319999,11.6,-2.56746520500002));
#187181=CARTESIAN_POINT('Ctrl Pts',(11.1469473609999,15.2,-2.56666392500001));
#187182=CARTESIAN_POINT('Ctrl Pts',(11.1469473609999,11.6,-2.56666392500001));
#187183=CARTESIAN_POINT('Ctrl Pts',(11.1506052429999,15.2,-2.56585889300001));
#187184=CARTESIAN_POINT('Ctrl Pts',(11.1506052429999,11.6,-2.56585889300002));
#187185=CARTESIAN_POINT('Ctrl Pts',(11.1542668699999,15.2,-2.56505010300002));
#187186=CARTESIAN_POINT('Ctrl Pts',(11.1542668699999,11.6,-2.56505010300002));
#187187=CARTESIAN_POINT('Ctrl Pts',(11.1579322339999,15.2,-2.56423755300001));
#187188=CARTESIAN_POINT('Ctrl Pts',(11.1579322339999,11.6,-2.56423755300002));
#187189=CARTESIAN_POINT('Ctrl Pts',(11.1616013289999,15.2,-2.56342123900001));
#187190=CARTESIAN_POINT('Ctrl Pts',(11.1616013289999,11.6,-2.56342123900001));
#187191=CARTESIAN_POINT('Ctrl Pts',(11.1652741469999,15.2,-2.56260115600002));
#187192=CARTESIAN_POINT('Ctrl Pts',(11.1652741469999,11.6,-2.56260115600002));
#187193=CARTESIAN_POINT('Ctrl Pts',(11.1689506789999,15.2,-2.56177730200001));
#187194=CARTESIAN_POINT('Ctrl Pts',(11.1689506789999,11.6,-2.56177730200001));
#187195=CARTESIAN_POINT('Ctrl Pts',(11.1726309199999,15.2,-2.56094967200001));
#187196=CARTESIAN_POINT('Ctrl Pts',(11.1726309199999,11.6,-2.56094967200002));
#187197=CARTESIAN_POINT('Ctrl Pts',(11.1763148559999,15.2,-2.56011826200002));
#187198=CARTESIAN_POINT('Ctrl Pts',(11.1763148559999,11.6,-2.56011826200002));
#187199=CARTESIAN_POINT('Ctrl Pts',(11.1800024799999,15.2,-2.55928306600001));
#187200=CARTESIAN_POINT('Ctrl Pts',(11.1800024799999,11.6,-2.55928306600001));
#187201=CARTESIAN_POINT('Ctrl Pts',(11.1836937809999,15.2,-2.55844408100002));
#187202=CARTESIAN_POINT('Ctrl Pts',(11.1836937809999,11.6,-2.55844408100002));
#187203=CARTESIAN_POINT('Ctrl Pts',(11.1873887489999,15.2,-2.55760130200001));
#187204=CARTESIAN_POINT('Ctrl Pts',(11.1873887489999,11.6,-2.55760130200001));
#187205=CARTESIAN_POINT('Ctrl Pts',(11.1910873769999,15.2,-2.55675472300001));
#187206=CARTESIAN_POINT('Ctrl Pts',(11.1910873769999,11.6,-2.55675472300001));
#187207=CARTESIAN_POINT('Ctrl Pts',(11.1947896549999,15.2,-2.55590434200001));
#187208=CARTESIAN_POINT('Ctrl Pts',(11.1947896549999,11.6,-2.55590434200002));
#187209=CARTESIAN_POINT('Ctrl Pts',(11.1984955799999,15.2,-2.55505015600002));
#187210=CARTESIAN_POINT('Ctrl Pts',(11.1984955799999,11.6,-2.55505015600002));
#187211=CARTESIAN_POINT('Ctrl Pts',(11.2022051459999,15.2,-2.55419216300002));
#187212=CARTESIAN_POINT('Ctrl Pts',(11.2022051459999,11.6,-2.55419216300002));
#187213=CARTESIAN_POINT('Ctrl Pts',(11.2059183529999,15.2,-2.55333036400001));
#187214=CARTESIAN_POINT('Ctrl Pts',(11.2059183529999,11.6,-2.55333036400002));
#187215=CARTESIAN_POINT('Ctrl Pts',(11.2088918289999,15.2,-2.55263787800001));
#187216=CARTESIAN_POINT('Ctrl Pts',(11.2088918289999,11.6,-2.55263787800002));
#187217=CARTESIAN_POINT('Ctrl Pts',(11.2111235739999,15.2,-2.55211680100001));
#187218=CARTESIAN_POINT('Ctrl Pts',(11.2111235739999,11.6,-2.55211680100001));
#187219=CARTESIAN_POINT('Ctrl Pts',(11.2126121319999,15.2,-2.55176865400002));
#187220=CARTESIAN_POINT('Ctrl Pts',(11.2126121319999,11.6,-2.55176865400002));
#187221=CARTESIAN_POINT('Ctrl Pts',(11.2133565919999,15.2,-2.55159439000002));
#187222=CARTESIAN_POINT('Ctrl Pts',(11.2133565919999,11.6,-2.55159439000002));
#187223=CARTESIAN_POINT('Ctrl Pts',(10.0330625579999,15.2,-2.64164356400002));
#187224=CARTESIAN_POINT('Ctrl Pts',(10.0348230291495,15.2,-2.6419483125593));
#187225=CARTESIAN_POINT('Ctrl Pts',(10.0366407489629,15.2,-2.64225752130091));
#187226=CARTESIAN_POINT('Ctrl Pts',(10.0385148613113,15.2,-2.64257038295741));
#187227=CARTESIAN_POINT('Ctrl Pts',(10.0403980115767,15.2,-2.64288475339096));
#187228=CARTESIAN_POINT('Ctrl Pts',(10.0423381038896,15.2,-2.64320281589738));
#187229=CARTESIAN_POINT('Ctrl Pts',(10.0443343061848,15.2,-2.6435237812644));
#187230=CARTESIAN_POINT('Ctrl Pts',(10.0463305082985,15.2,-2.64384474660228));
#187231=CARTESIAN_POINT('Ctrl Pts',(10.0483828195931,15.2,-2.64416861599519));
#187232=CARTESIAN_POINT('Ctrl Pts',(10.0504904280165,15.2,-2.64449462848334));
#187233=CARTESIAN_POINT('Ctrl Pts',(10.0525980364399,15.2,-2.64482064097149));
#187234=CARTESIAN_POINT('Ctrl Pts',(10.0547609457251,15.1999999999999,-2.64514879481373));
#187235=CARTESIAN_POINT('Ctrl Pts',(10.0569783622521,15.2,-2.6454783534848));
#187236=CARTESIAN_POINT('Ctrl Pts',(10.0591957789806,15.2,-2.64580791218582));
#187237=CARTESIAN_POINT('Ctrl Pts',(10.061467704948,15.2,-2.64613887502637));
#187238=CARTESIAN_POINT('Ctrl Pts',(10.063793370495,15.2,-2.6464705267945));
#187239=CARTESIAN_POINT('Ctrl Pts',(10.0661190358309,15.2,-2.6468021785325));
#187240=CARTESIAN_POINT('Ctrl Pts',(10.0684984390365,15.2,-2.6471345208524));
#187241=CARTESIAN_POINT('Ctrl Pts',(10.0709308315426,15.2,-2.6474668567585));
#187242=CARTESIAN_POINT('Ctrl Pts',(10.0737686229471,15.2,-2.64785458200241));
#187243=CARTESIAN_POINT('Ctrl Pts',(10.0766785365834,15.2,-2.64824230028018));
#187244=CARTESIAN_POINT('Ctrl Pts',(10.0796594095367,15.2,-2.64862894528614));
#187245=CARTESIAN_POINT('Ctrl Pts',(10.0822144433641,15.2,-2.64896035527404));
#187246=CARTESIAN_POINT('Ctrl Pts',(10.0848216127188,15.2,-2.64929097719397));
#187247=CARTESIAN_POINT('Ctrl Pts',(10.0874802043011,15.2,-2.64962016201683));
#187248=CARTESIAN_POINT('Ctrl Pts',(10.0901387958833,15.2,-2.6499493468397));
#187249=CARTESIAN_POINT('Ctrl Pts',(10.0928488087771,15.2,-2.650277092594));
#187250=CARTESIAN_POINT('Ctrl Pts',(10.0956095465913,15.2,-2.65060276874893));
#187251=CARTESIAN_POINT('Ctrl Pts',(10.0983702846562,15.2,-2.65092844493343));
#187252=CARTESIAN_POINT('Ctrl Pts',(10.1011817494274,15.2,-2.65125205402602));
#187253=CARTESIAN_POINT('Ctrl Pts',(10.1040432583368,15.2,-2.65157297829333));
#187254=CARTESIAN_POINT('Ctrl Pts',(10.1069047669862,15.2,-2.65189390253149));
#187255=CARTESIAN_POINT('Ctrl Pts',(10.1098163187669,15.2,-2.65221214557876));
#187256=CARTESIAN_POINT('Ctrl Pts',(10.1127772496614,15.2,-2.65252710973384));
#187257=CARTESIAN_POINT('Ctrl Pts',(10.115738180556,15.2,-2.65284207388892));
#187258=CARTESIAN_POINT('Ctrl Pts',(10.11874848838,15.2,-2.65315375826091));
#187259=CARTESIAN_POINT('Ctrl Pts',(10.1218075241,15.2,-2.65346158558323));
#187260=CARTESIAN_POINT('Ctrl Pts',(10.1248665598201,15.2,-2.65376941290554));
#187261=CARTESIAN_POINT('Ctrl Pts',(10.1279743205738,15.2,-2.65407338115295));
#187262=CARTESIAN_POINT('Ctrl Pts',(10.1311301696225,15.2,-2.6543729277257));
#187263=CARTESIAN_POINT('Ctrl Pts',(10.1342860189579,15.2,-2.65467247432566));
#187264=CARTESIAN_POINT('Ctrl Pts',(10.1374899571313,15.2,-2.65496759964189));
#187265=CARTESIAN_POINT('Ctrl Pts',(10.1407413574773,15.2,-2.65525775424082));
#187266=CARTESIAN_POINT('Ctrl Pts',(10.1445346577332,15.2,-2.65559626792639));
#187267=CARTESIAN_POINT('Ctrl Pts',(10.148392559207,15.2,-2.65592801608681));
#187268=CARTESIAN_POINT('Ctrl Pts',(10.1523140901329,15.2,-2.65625215381364));
#187269=CARTESIAN_POINT('Ctrl Pts',(10.1556754021806,15.2,-2.6565299861365));
#187270=CARTESIAN_POINT('Ctrl Pts',(10.1590834633618,15.2,-2.65680222507444));
#187271=CARTESIAN_POINT('Ctrl Pts',(10.162537675405,15.2,-2.65706835573117));
#187272=CARTESIAN_POINT('Ctrl Pts',(10.1665675896645,15.2,-2.65737884151348));
#187273=CARTESIAN_POINT('Ctrl Pts',(10.1706603172142,15.2,-2.65768101328449));
#187274=CARTESIAN_POINT('Ctrl Pts',(10.1748149296714,15.2,-2.65797406926074));
#187275=CARTESIAN_POINT('Ctrl Pts',(10.1783760258784,15.2,-2.65822526008449));
#187276=CARTESIAN_POINT('Ctrl Pts',(10.1819825880631,15.2,-2.65846975596353));
#187277=CARTESIAN_POINT('Ctrl Pts',(10.1856340412657,15.2,-2.65870706753793));
#187278=CARTESIAN_POINT('Ctrl Pts',(10.1892854944683,15.2,-2.65894437911233));
#187279=CARTESIAN_POINT('Ctrl Pts',(10.192981837834,15.2,-2.65917450509562));
#187280=CARTESIAN_POINT('Ctrl Pts',(10.1967225100295,15.2,-2.65939697175454));
#187281=CARTESIAN_POINT('Ctrl Pts',(10.200463182225,15.2,-2.65961943841345));
#187282=CARTESIAN_POINT('Ctrl Pts',(10.2042481801746,15.2,-2.65983424195945));
#187283=CARTESIAN_POINT('Ctrl Pts',(10.2080769523659,15.2,-2.6600409227025));
#187284=CARTESIAN_POINT('Ctrl Pts',(10.2119057249049,15.2,-2.66024760346432));
#187285=CARTESIAN_POINT('Ctrl Pts',(10.2157782699648,15.2,-2.66044615690037));
#187286=CARTESIAN_POINT('Ctrl Pts',(10.2196940436801,15.2,-2.66063613374368));
#187287=CARTESIAN_POINT('Ctrl Pts',(10.2236098170397,15.2,-2.66082611056973));
#187288=CARTESIAN_POINT('Ctrl Pts',(10.2275688203671,15.2,-2.66100750994708));
#187289=CARTESIAN_POINT('Ctrl Pts',(10.2315705159897,15.2,-2.66117988802495));
#187290=CARTESIAN_POINT('Ctrl Pts',(10.2349052624631,15.2,-2.6613235364284));
#187291=CARTESIAN_POINT('Ctrl Pts',(10.2382696579332,15.2,-2.66146092320003));
#187292=CARTESIAN_POINT('Ctrl Pts',(10.2416633975165,15.2,-2.6615917942417));
#187293=CARTESIAN_POINT('Ctrl Pts',(10.2450571370999,15.2,-2.66172266528337));
#187294=CARTESIAN_POINT('Ctrl Pts',(10.2484802196249,15.2,-2.66184702443847));
#187295=CARTESIAN_POINT('Ctrl Pts',(10.2519323459601,15.2,-2.66196462450843));
#187296=CARTESIAN_POINT('Ctrl Pts',(10.2553844722953,15.2,-2.66208222457839));
#187297=CARTESIAN_POINT('Ctrl Pts',(10.2588656422836,15.2,-2.66219306607381));
#187298=CARTESIAN_POINT('Ctrl Pts',(10.2623755579796,15.2,-2.66229691024011));
#187299=CARTESIAN_POINT('Ctrl Pts',(10.2658854736755,15.2,-2.66240075440641));
#187300=CARTESIAN_POINT('Ctrl Pts',(10.2694241362485,15.2,-2.66249759921178));
#187301=CARTESIAN_POINT('Ctrl Pts',(10.2729912527083,15.2,-2.66258721178085));
#187302=CARTESIAN_POINT('Ctrl Pts',(10.2765583691681,15.2,-2.66267682434992));
#187303=CARTESIAN_POINT('Ctrl Pts',(10.2801539412488,15.2,-2.66275920294437));
#187304=CARTESIAN_POINT('Ctrl Pts',(10.2837776771956,15.2,-2.66283411801704));
#187305=CARTESIAN_POINT('Ctrl Pts',(10.2874014131425,15.2,-2.66290903308971));
#187306=CARTESIAN_POINT('Ctrl Pts',(10.2910533150067,15.2,-2.66297648424737));
#187307=CARTESIAN_POINT('Ctrl Pts',(10.2947330972312,15.2,-2.66303624452451));
#187308=CARTESIAN_POINT('Ctrl Pts',(10.2984128794557,15.2,-2.66309600480166));
#187309=CARTESIAN_POINT('Ctrl Pts',(10.3021205410195,15.2,-2.6631480763509));
#187310=CARTESIAN_POINT('Ctrl Pts',(10.3058558024801,15.2,-2.66319223648914));
#187311=CARTESIAN_POINT('Ctrl Pts',(10.3095910635336,15.2,-2.66323639662256));
#187312=CARTESIAN_POINT('Ctrl Pts',(10.313353923875,15.2,-2.66327264480431));
#187313=CARTESIAN_POINT('Ctrl Pts',(10.3171441049875,15.2,-2.66330076424635));
#187314=CARTESIAN_POINT('Ctrl Pts',(10.320934286513,15.2,-2.66332888369147));
#187315=CARTESIAN_POINT('Ctrl Pts',(10.3247517896936,15.2,-2.66334887532005));
#187316=CARTESIAN_POINT('Ctrl Pts',(10.328596340247,15.2,-2.66336052393184));
#187317=CARTESIAN_POINT('Ctrl Pts',(10.3324408908004,15.2,-2.66337217254364));
#187318=CARTESIAN_POINT('Ctrl Pts',(10.3363124867379,15.2,-2.66337548064473));
#187319=CARTESIAN_POINT('Ctrl Pts',(10.3402108600558,15.2,-2.66337023599228));
#187320=CARTESIAN_POINT('Ctrl Pts',(10.3441092333737,15.2,-2.66336499133984));
#187321=CARTESIAN_POINT('Ctrl Pts',(10.3480343822041,15.2,-2.66335119630656));
#187322=CARTESIAN_POINT('Ctrl Pts',(10.3519860387999,15.2,-2.66332864575146));
#187323=CARTESIAN_POINT('Ctrl Pts',(10.3559376953958,15.2,-2.66330609519636));
#187324=CARTESIAN_POINT('Ctrl Pts',(10.3599158599229,15.2,-2.66327478717437));
#187325=CARTESIAN_POINT('Ctrl Pts',(10.3639202682548,15.2,-2.66323452328595));
#187326=CARTESIAN_POINT('Ctrl Pts',(10.3679246765868,15.2,-2.66319425939753));
#187327=CARTESIAN_POINT('Ctrl Pts',(10.371955329325,15.2,-2.66314503629776));
#187328=CARTESIAN_POINT('Ctrl Pts',(10.3760119627264,15.2,-2.6630866599788));
#187329=CARTESIAN_POINT('Ctrl Pts',(10.3800685961278,15.2,-2.66302828365983));
#187330=CARTESIAN_POINT('Ctrl Pts',(10.3841512115291,15.2,-2.6629607526504));
#187331=CARTESIAN_POINT('Ctrl Pts',(10.3882595507143,15.2,-2.66288387223341));
#187332=CARTESIAN_POINT('Ctrl Pts',(10.3923678898996,15.2,-2.66280699181642));
#187333=CARTESIAN_POINT('Ctrl Pts',(10.3965019530165,15.2,-2.66272076289449));
#187334=CARTESIAN_POINT('Ctrl Pts',(10.4006614830165,15.2,-2.66262499574171));
#187335=CARTESIAN_POINT('Ctrl Pts',(10.4039891071979,15.2,-2.66254838201531));
#187336=CARTESIAN_POINT('Ctrl Pts',(10.4073330312423,15.2,-2.66246566257709));
#187337=CARTESIAN_POINT('Ctrl Pts',(10.4106931253159,15.2,-2.6623767429605));
#187338=CARTESIAN_POINT('Ctrl Pts',(10.4140532189318,15.2,-2.66228782335602));
#187339=CARTESIAN_POINT('Ctrl Pts',(10.4174294817457,15.2,-2.66219270320892));
#187340=CARTESIAN_POINT('Ctrl Pts',(10.4208217862059,15.2,-2.66209128821677));
#187341=CARTESIAN_POINT('Ctrl Pts',(10.4242140911284,15.2,-2.66198987321081));
#187342=CARTESIAN_POINT('Ctrl Pts',(10.4276224383076,15.2,-2.66188216367714));
#187343=CARTESIAN_POINT('Ctrl Pts',(10.4310466985514,15.2,-2.66176806544805));
#187344=CARTESIAN_POINT('Ctrl Pts',(10.4344709583287,15.2,-2.6616539672345));
#187345=CARTESIAN_POINT('Ctrl Pts',(10.4379111327372,15.2,-2.66153348233567));
#187346=CARTESIAN_POINT('Ctrl Pts',(10.4413670945092,15.2,-2.66140651673536));
#187347=CARTESIAN_POINT('Ctrl Pts',(10.444823056752,15.2,-2.66127955111776));
#187348=CARTESIAN_POINT('Ctrl Pts',(10.4482948076293,15.2,-2.66114610650321));
#187349=CARTESIAN_POINT('Ctrl Pts',(10.4517822207727,15.2,-2.66100609098802));
#187350=CARTESIAN_POINT('Ctrl Pts',(10.4552696334409,15.2,-2.6608660754919));
#187351=CARTESIAN_POINT('Ctrl Pts',(10.4587727085288,15.2,-2.66071949135787));
#187352=CARTESIAN_POINT('Ctrl Pts',(10.4622913234624,15.2,-2.66056624720417));
#187353=CARTESIAN_POINT('Ctrl Pts',(10.4658099388754,15.2,-2.66041300302959));
#187354=CARTESIAN_POINT('Ctrl Pts',(10.4693440911819,15.2,-2.66025310083476));
#187355=CARTESIAN_POINT('Ctrl Pts',(10.4728936600985,15.2,-2.66008645126969));
#187356=CARTESIAN_POINT('Ctrl Pts',(10.4764432285316,15.2,-2.65991980172731));
#187357=CARTESIAN_POINT('Ctrl Pts',(10.4800082122984,15.2,-2.65974640550317));
#187358=CARTESIAN_POINT('Ctrl Pts',(10.4835884902388,15.2,-2.65956617650949));
#187359=CARTESIAN_POINT('Ctrl Pts',(10.487168768667,15.2,-2.65938594749125));
#187360=CARTESIAN_POINT('Ctrl Pts',(10.4907643404863,15.2,-2.65919888487014));
#187361=CARTESIAN_POINT('Ctrl Pts',(10.4943750847952,15.2,-2.65900490402579));
#187362=CARTESIAN_POINT('Ctrl Pts',(10.4979858286121,15.2,-2.65881092320786));
#187363=CARTESIAN_POINT('Ctrl Pts',(10.501611745176,15.2,-2.65861002380798));
#187364=CARTESIAN_POINT('Ctrl Pts',(10.5052527136546,15.2,-2.6584021223257));
#187365=CARTESIAN_POINT('Ctrl Pts',(10.5088936826293,15.2,-2.65819422081508));
#187366=CARTESIAN_POINT('Ctrl Pts',(10.5125497053467,15.2,-2.65797931672135));
#187367=CARTESIAN_POINT('Ctrl Pts',(10.5162206597857,15.2,-2.65775732720822));
#187368=CARTESIAN_POINT('Ctrl Pts',(10.5198916137246,15.2,-2.65753533772534));
#187369=CARTESIAN_POINT('Ctrl Pts',(10.5235775028572,15.2,-2.65730626298806));
#187370=CARTESIAN_POINT('Ctrl Pts',(10.5272782053865,15.2,-2.65707002206366));
#187371=CARTESIAN_POINT('Ctrl Pts',(10.53097890842,15.2,-2.65683378110708));
#187372=CARTESIAN_POINT('Ctrl Pts',(10.5346944275744,15.2,-2.65659037247204));
#187373=CARTESIAN_POINT('Ctrl Pts',(10.5384246439999,15.2,-2.65633971629171));
#187374=CARTESIAN_POINT('Ctrl Pts',(10.5421548604254,15.2,-2.65608906011138));
#187375=CARTESIAN_POINT('Ctrl Pts',(10.5458997756999,15.2,-2.65583115714687));
#187376=CARTESIAN_POINT('Ctrl Pts',(10.5496592714062,15.2,-2.65556592696501));
#187377=CARTESIAN_POINT('Ctrl Pts',(10.5534187666004,15.2,-2.65530069681928));
#187378=CARTESIAN_POINT('Ctrl Pts',(10.5571928440954,15.2,-2.65502814039526));
#187379=CARTESIAN_POINT('Ctrl Pts',(10.5609813872473,15.2,-2.65474817775023));
#187380=CARTESIAN_POINT('Ctrl Pts',(10.5647699309154,15.2,-2.65446821506707));
#187381=CARTESIAN_POINT('Ctrl Pts',(10.5685729412895,15.2,-2.65418084742145));
#187382=CARTESIAN_POINT('Ctrl Pts',(10.5723903023324,15.2,-2.65388599846017));
#187383=CARTESIAN_POINT('Ctrl Pts',(10.5771620033759,15.2,-2.65351743727865));
#187384=CARTESIAN_POINT('Ctrl Pts',(10.5819561283114,15.2,-2.65313718318306));
#187385=CARTESIAN_POINT('Ctrl Pts',(10.5867724566465,15.2,-2.65274509047376));
#187386=CARTESIAN_POINT('Ctrl Pts',(10.5906255189997,15.2,-2.65243141633196));
#187387=CARTESIAN_POINT('Ctrl Pts',(10.5944927896386,15.2,-2.65211016498318));
#187388=CARTESIAN_POINT('Ctrl Pts',(10.5983741575056,15.2,-2.6517812615086));
#187389=CARTESIAN_POINT('Ctrl Pts',(10.6032258677359,15.2,-2.65137013213177));
#187390=CARTESIAN_POINT('Ctrl Pts',(10.608099603411,15.2,-2.65094704505005));
#187391=CARTESIAN_POINT('Ctrl Pts',(10.6129951477165,15.2,-2.65051185900838));
#187392=CARTESIAN_POINT('Ctrl Pts',(10.6169115833744,15.2,-2.65016371015607));
#187393=CARTESIAN_POINT('Ctrl Pts',(10.6208419763756,15.2,-2.64980781708898));
#187394=CARTESIAN_POINT('Ctrl Pts',(10.6247862148698,15.2,-2.64944410695724));
#187395=CARTESIAN_POINT('Ctrl Pts',(10.6287304528265,15.2,-2.64908039687506));
#187396=CARTESIAN_POINT('Ctrl Pts',(10.63268853689,15.2,-2.64870887040154));
#187397=CARTESIAN_POINT('Ctrl Pts',(10.6366603579722,15.2,-2.64832945570864));
#187398=CARTESIAN_POINT('Ctrl Pts',(10.6406321795955,15.2,-2.64795004096404));
#187399=CARTESIAN_POINT('Ctrl Pts',(10.6446177356122,15.2,-2.64756273789388));
#187400=CARTESIAN_POINT('Ctrl Pts',(10.6486169193871,15.2,-2.64716747592708));
#187401=CARTESIAN_POINT('Ctrl Pts',(10.6526161026171,15.2,-2.64677221401414));
#187402=CARTESIAN_POINT('Ctrl Pts',(10.6566289133787,15.2,-2.64636899442445));
#187403=CARTESIAN_POINT('Ctrl Pts',(10.6606552419375,15.2,-2.64595774629192));
#187404=CARTESIAN_POINT('Ctrl Pts',(10.664681571045,15.2,-2.64554649810337));
#187405=CARTESIAN_POINT('Ctrl Pts',(10.6687214180846,15.2,-2.64512722015274));
#187406=CARTESIAN_POINT('Ctrl Pts',(10.6727746758064,15.2,-2.64469984674003));
#187407=CARTESIAN_POINT('Ctrl Pts',(10.6768279329759,15.2,-2.64427247338555));
#187408=CARTESIAN_POINT('Ctrl Pts',(10.6808945997305,15.2,-2.64383700289956));
#187409=CARTESIAN_POINT('Ctrl Pts',(10.6849745710996,15.2,-2.64339336758104));
#187410=CARTESIAN_POINT('Ctrl Pts',(10.6890545430246,15.2,-2.64294973220208));
#187411=CARTESIAN_POINT('Ctrl Pts',(10.6931478179694,15.2,-2.64249793280464));
#187412=CARTESIAN_POINT('Ctrl Pts',(10.6972542903607,15.2,-2.64203790144569));
#187413=CARTESIAN_POINT('Ctrl Pts',(10.7013607621925,15.2,-2.64157787014943));
#187414=CARTESIAN_POINT('Ctrl Pts',(10.7054804310245,15.2,-2.64110960804926));
#187415=CARTESIAN_POINT('Ctrl Pts',(10.7096131915742,15.2,-2.64063304931129));
#187416=CARTESIAN_POINT('Ctrl Pts',(10.713745952687,15.2,-2.64015649050839));
#187417=CARTESIAN_POINT('Ctrl Pts',(10.7178918043683,15.2,-2.63967163347886));
#187418=CARTESIAN_POINT('Ctrl Pts',(10.7220506435027,15.2,-2.63917841478304));
#187419=CARTESIAN_POINT('Ctrl Pts',(10.7272491921375,15.2,-2.63856189144688));
#187420=CARTESIAN_POINT('Ctrl Pts',(10.7324680326749,15.2,-2.63793230175307));
#187421=CARTESIAN_POINT('Ctrl Pts',(10.7377069605926,15.2,-2.63728952168293));
#187422=CARTESIAN_POINT('Ctrl Pts',(10.7418981025842,15.2,-2.63677529766886));
#187423=CARTESIAN_POINT('Ctrl Pts',(10.746102101887,15.2,-2.6362526312787));
#187424=CARTESIAN_POINT('Ctrl Pts',(10.7503188538188,15.2,-2.63572146004522));
#187425=CARTESIAN_POINT('Ctrl Pts',(10.7545356063251,15.2,-2.63519028873936));
#187426=CARTESIAN_POINT('Ctrl Pts',(10.7587651119162,15.2,-2.63465061196263));
#187427=CARTESIAN_POINT('Ctrl Pts',(10.7630072677778,15.2,-2.63410236854134));
#187428=CARTESIAN_POINT('Ctrl Pts',(10.7672494230614,15.2,-2.63355412519475));
#187429=CARTESIAN_POINT('Ctrl Pts',(10.7715042295384,15.2,-2.63299731289261));
#187430=CARTESIAN_POINT('Ctrl Pts',(10.7757715835772,15.2,-2.63243187355083));
#187431=CARTESIAN_POINT('Ctrl Pts',(10.7800389381974,15.2,-2.631866434132));
#187432=CARTESIAN_POINT('Ctrl Pts',(10.7843188417604,15.2,-2.63129236579571));
#187433=CARTESIAN_POINT('Ctrl Pts',(10.7886111922166,15.2,-2.63070960904172));
#187434=CARTESIAN_POINT('Ctrl Pts',(10.7929035426727,15.2,-2.63012685228774));
#187435=CARTESIAN_POINT('Ctrl Pts',(10.7972083399692,15.2,-2.62953540480219));
#187436=CARTESIAN_POINT('Ctrl Pts',(10.8015254832058,15.2,-2.62893520943525));
#187437=CARTESIAN_POINT('Ctrl Pts',(10.8058426258541,15.2,-2.62833501415008));
#187438=CARTESIAN_POINT('Ctrl Pts',(10.8101721160628,15.2,-2.62772606936663));
#187439=CARTESIAN_POINT('Ctrl Pts',(10.8145138520053,15.2,-2.62710831802547));
#187440=CARTESIAN_POINT('Ctrl Pts',(10.8188555885394,15.2,-2.62649056660014));
#187441=CARTESIAN_POINT('Ctrl Pts',(10.8232095699496,15.2,-2.62586400558169));
#187442=CARTESIAN_POINT('Ctrl Pts',(10.8275756990221,15.2,-2.62522858087949));
#187443=CARTESIAN_POINT('Ctrl Pts',(10.8319418274997,15.2,-2.62459315626386));
#187444=CARTESIAN_POINT('Ctrl Pts',(10.8363201027758,15.2,-2.6239488650605));
#187445=CARTESIAN_POINT('Ctrl Pts',(10.8407104249161,15.2,-2.62329565000337));
#187446=CARTESIAN_POINT('Ctrl Pts',(10.8440031666709,15.2,-2.62280573868827));
#187447=CARTESIAN_POINT('Ctrl Pts',(10.847302686516,15.2,-2.62231080996962));
#187448=CARTESIAN_POINT('Ctrl Pts',(10.850608940852,15.2,-2.6218108365884));
#187449=CARTESIAN_POINT('Ctrl Pts',(10.855017280367,15.2,-2.62114420535288));
#187450=CARTESIAN_POINT('Ctrl Pts',(10.8594375942756,15.2,-2.62046860861245));
#187451=CARTESIAN_POINT('Ctrl Pts',(10.863869783629,15.2,-2.61978399118566));
#187452=CARTESIAN_POINT('Ctrl Pts',(10.8671939253422,15.2,-2.61927052816221));
#187453=CARTESIAN_POINT('Ctrl Pts',(10.8705247480878,15.2,-2.61875198924769));
#187454=CARTESIAN_POINT('Ctrl Pts',(10.8738622097166,15.2,-2.61822835326672));
#187455=CARTESIAN_POINT('Ctrl Pts',(10.8783121589591,15.2,-2.61753017189534));
#187456=CARTESIAN_POINT('Ctrl Pts',(10.8827739110335,15.2,-2.61682292656456));
#187457=CARTESIAN_POINT('Ctrl Pts',(10.887247370223,15.2,-2.61610656335792));
#187458=CARTESIAN_POINT('Ctrl Pts',(10.8906024643103,15.2,-2.61556929100174));
#187459=CARTESIAN_POINT('Ctrl Pts',(10.893964142805,15.2,-2.61502689076879));
#187460=CARTESIAN_POINT('Ctrl Pts',(10.897332365185,15.2,-2.61447933838573));
#187461=CARTESIAN_POINT('Ctrl Pts',(10.900700587565,15.2,-2.61393178600267));
#187462=CARTESIAN_POINT('Ctrl Pts',(10.9040753551409,15.2,-2.61337908225267));
#187463=CARTESIAN_POINT('Ctrl Pts',(10.9074566253519,15.2,-2.61282120389749));
#187464=CARTESIAN_POINT('Ctrl Pts',(10.910837895563,15.2,-2.61226332554231));
#187465=CARTESIAN_POINT('Ctrl Pts',(10.9142256696232,15.2,-2.61170027346274));
#187466=CARTESIAN_POINT('Ctrl Pts',(10.9176199072499,15.2,-2.61113202498339));
#187467=CARTESIAN_POINT('Ctrl Pts',(10.9221455578299,15.2,-2.61037436027543));
#187468=CARTESIAN_POINT('Ctrl Pts',(10.9266826989834,15.2,-2.6096074571275));
#187469=CARTESIAN_POINT('Ctrl Pts',(10.9312312350103,15.2,-2.6088312626398));
#187470=CARTESIAN_POINT('Ctrl Pts',(10.9346426367205,15.2,-2.60824911682691));
#187471=CARTESIAN_POINT('Ctrl Pts',(10.9380604492817,15.2,-2.6076617451107));
#187472=CARTESIAN_POINT('Ctrl Pts',(10.9414846316208,15.2,-2.60706912614368));
#187473=CARTESIAN_POINT('Ctrl Pts',(10.9471916023932,15.2,-2.60608142782943));
#187474=CARTESIAN_POINT('Ctrl Pts',(10.9529162663107,15.2,-2.60507915132934));
#187475=CARTESIAN_POINT('Ctrl Pts',(10.9586584424927,15.2,-2.6040621981337));
#187476=CARTESIAN_POINT('Ctrl Pts',(10.9621037480767,15.2,-2.60345202623848));
#187477=CARTESIAN_POINT('Ctrl Pts',(10.9655553572687,15.2,-2.60283657054354));
#187478=CARTESIAN_POINT('Ctrl Pts',(10.9690132313936,15.2,-2.60221580969063));
#187479=CARTESIAN_POINT('Ctrl Pts',(10.9724711055185,15.2,-2.60159504883773));
#187480=CARTESIAN_POINT('Ctrl Pts',(10.9759352440467,15.2,-2.60096898362943));
#187481=CARTESIAN_POINT('Ctrl Pts',(10.9794056077281,15.2,-2.60033759181614));
#187482=CARTESIAN_POINT('Ctrl Pts',(10.9828759714094,15.2,-2.59970620000286));
#187483=CARTESIAN_POINT('Ctrl Pts',(10.9863525608242,15.2,-2.59906948256353));
#187484=CARTESIAN_POINT('Ctrl Pts',(10.9898353360051,15.2,-2.59842741775064));
#187485=CARTESIAN_POINT('Ctrl Pts',(10.993318111186,15.2,-2.59778535293774));
#187486=CARTESIAN_POINT('Ctrl Pts',(10.9968070728799,15.2,-2.59713794068027));
#187487=CARTESIAN_POINT('Ctrl Pts',(11.0003021811274,15.2,-2.59648516178778));
#187488=CARTESIAN_POINT('Ctrl Pts',(11.0037972893748,15.2,-2.5958323828953));
#187489=CARTESIAN_POINT('Ctrl Pts',(11.0072985455136,15.2,-2.59517423653652));
#187490=CARTESIAN_POINT('Ctrl Pts',(11.010805909677,15.2,-2.5945107021447));
#187491=CARTESIAN_POINT('Ctrl Pts',(11.0143132744775,15.2,-2.59384716763233));
#187492=CARTESIAN_POINT('Ctrl Pts',(11.0178267478048,15.2,-2.59317824488512));
#187493=CARTESIAN_POINT('Ctrl Pts',(11.0213462910672,15.2,-2.59250391436971));
#187494=CARTESIAN_POINT('Ctrl Pts',(11.0248658336901,15.2,-2.59182958397681));
#187495=CARTESIAN_POINT('Ctrl Pts',(11.0283914454127,15.2,-2.59114984523419));
#187496=CARTESIAN_POINT('Ctrl Pts',(11.0319230890766,15.2,-2.59046467796694));
#187497=CARTESIAN_POINT('Ctrl Pts',(11.0354547327405,15.2,-2.5897795106997));
#187498=CARTESIAN_POINT('Ctrl Pts',(11.0389924078491,15.2,-2.58908891626064));
#187499=CARTESIAN_POINT('Ctrl Pts',(11.0425360759865,15.2,-2.58839287299108));
#187500=CARTESIAN_POINT('Ctrl Pts',(11.0460797441238,15.2,-2.58769682972152));
#187501=CARTESIAN_POINT('Ctrl Pts',(11.0496294053597,15.2,-2.58699533911152));
#187502=CARTESIAN_POINT('Ctrl Pts',(11.0531850214967,15.2,-2.58628838030069));
#187503=CARTESIAN_POINT('Ctrl Pts',(11.0579258434432,15.2,-2.5853457684673));
#187504=CARTESIAN_POINT('Ctrl Pts',(11.0626772516873,15.2,-2.5843934369934));
#187505=CARTESIAN_POINT('Ctrl Pts',(11.0674391563368,15.2,-2.58343133855108));
#187506=CARTESIAN_POINT('Ctrl Pts',(11.0710105844995,15.2,-2.58270976478488));
#187507=CARTESIAN_POINT('Ctrl Pts',(11.0745879164369,15.2,-2.58198269829397));
#187508=CARTESIAN_POINT('Ctrl Pts',(11.0781711151406,15.2,-2.58125011894511));
#187509=CARTESIAN_POINT('Ctrl Pts',(11.0817543138442,15.2,-2.58051753959624));
#187510=CARTESIAN_POINT('Ctrl Pts',(11.0853433793174,15.2,-2.57977944704243));
#187511=CARTESIAN_POINT('Ctrl Pts',(11.0889382734948,15.2,-2.57903582323271));
#187512=CARTESIAN_POINT('Ctrl Pts',(11.0925331676723,15.2,-2.57829219942299));
#187513=CARTESIAN_POINT('Ctrl Pts',(11.096133890878,15.2,-2.57754304457672));
#187514=CARTESIAN_POINT('Ctrl Pts',(11.0997404050133,15.2,-2.5767883387674));
#187515=CARTESIAN_POINT('Ctrl Pts',(11.1033469191486,15.2,-2.57603363295809));
#187516=CARTESIAN_POINT('Ctrl Pts',(11.1069592240376,15.2,-2.57527337640512));
#187517=CARTESIAN_POINT('Ctrl Pts',(11.1105772831556,15.2,-2.57450755105843));
#187518=CARTESIAN_POINT('Ctrl Pts',(11.1141953422737,15.2,-2.57374172571175));
#187519=CARTESIAN_POINT('Ctrl Pts',(11.1178191538413,15.2,-2.57297033109044));
#187520=CARTESIAN_POINT('Ctrl Pts',(11.121448684417,15.2,-2.57219334970276));
#187521=CARTESIAN_POINT('Ctrl Pts',(11.125078215652,15.2,-2.57141636817394));
#187522=CARTESIAN_POINT('Ctrl Pts',(11.1287134635304,15.2,-2.57063379841021));
#187523=CARTESIAN_POINT('Ctrl Pts',(11.1323543913103,15.2,-2.56984562479489));
#187524=CARTESIAN_POINT('Ctrl Pts',(11.1372089605811,15.2,-2.56879472687978));
#187525=CARTESIAN_POINT('Ctrl Pts',(11.1420736265119,15.2,-2.56773386186806));
#187526=CARTESIAN_POINT('Ctrl Pts',(11.1469482992466,15.2,-2.56666298695078));
#187527=CARTESIAN_POINT('Ctrl Pts',(11.1506043039637,15.2,-2.56585983072634));
#187528=CARTESIAN_POINT('Ctrl Pts',(11.1542659375507,15.2,-2.56505104442532));
#187529=CARTESIAN_POINT('Ctrl Pts',(11.1579331663336,15.2,-2.5642366120804));
#187530=CARTESIAN_POINT('Ctrl Pts',(11.1616003951165,15.2,-2.56342217973548));
#187531=CARTESIAN_POINT('Ctrl Pts',(11.1652732197991,15.2,-2.56260210053262));
#187532=CARTESIAN_POINT('Ctrl Pts',(11.168951605373,15.2,-2.56177635818839));
#187533=CARTESIAN_POINT('Ctrl Pts',(11.1726299916152,15.2,-2.56095061569416));
#187534=CARTESIAN_POINT('Ctrl Pts',(11.1763139379006,15.2,-2.56011920950666));
#187535=CARTESIAN_POINT('Ctrl Pts',(11.1800034000625,15.2,-2.5592821185509));
#187536=CARTESIAN_POINT('Ctrl Pts',(11.1836928615542,15.2,-2.5584450277472));
#187537=CARTESIAN_POINT('Ctrl Pts',(11.1873878377649,15.2,-2.55760225254806));
#187538=CARTESIAN_POINT('Ctrl Pts',(11.1910882902742,15.2,-2.5567537723275));
#187539=CARTESIAN_POINT('Ctrl Pts',(11.1947887427836,15.2,-2.55590529210695));
#187540=CARTESIAN_POINT('Ctrl Pts',(11.1984946703957,15.2,-2.55505110740725));
#187541=CARTESIAN_POINT('Ctrl Pts',(11.2022060566279,15.2,-2.55419121137746));
#187542=CARTESIAN_POINT('Ctrl Pts',(11.20591744286,15.2,-2.55333131534767));
#187543=CARTESIAN_POINT('Ctrl Pts',(11.2096342913237,15.2,-2.5524657101583));
#187544=CARTESIAN_POINT('Ctrl Pts',(11.2133565919999,15.2,-2.55159439000002));
#187545=CARTESIAN_POINT('Ctrl Pts',(10.0330625579999,12.2,-2.64164356400002));
#187546=CARTESIAN_POINT('Ctrl Pts',(10.0348230291495,12.2,-2.6419483125593));
#187547=CARTESIAN_POINT('Ctrl Pts',(10.0366407489629,12.2,-2.64225752130091));
#187548=CARTESIAN_POINT('Ctrl Pts',(10.0385148613113,12.2,-2.64257038295741));
#187549=CARTESIAN_POINT('Ctrl Pts',(10.0403980115767,12.2,-2.64288475339096));
#187550=CARTESIAN_POINT('Ctrl Pts',(10.0423381038896,12.2,-2.64320281589738));
#187551=CARTESIAN_POINT('Ctrl Pts',(10.0443343061848,12.2,-2.6435237812644));
#187552=CARTESIAN_POINT('Ctrl Pts',(10.0463305082985,12.2,-2.64384474660227));
#187553=CARTESIAN_POINT('Ctrl Pts',(10.0483828195931,12.2,-2.64416861599519));
#187554=CARTESIAN_POINT('Ctrl Pts',(10.0504904280165,12.2,-2.64449462848334));
#187555=CARTESIAN_POINT('Ctrl Pts',(10.0525980364399,12.2,-2.6448206409715));
#187556=CARTESIAN_POINT('Ctrl Pts',(10.0547609457251,12.2,-2.64514879481372));
#187557=CARTESIAN_POINT('Ctrl Pts',(10.0569783622521,12.2,-2.6454783534848));
#187558=CARTESIAN_POINT('Ctrl Pts',(10.0591957789806,12.2,-2.64580791218581));
#187559=CARTESIAN_POINT('Ctrl Pts',(10.061467704948,12.2,-2.64613887502637));
#187560=CARTESIAN_POINT('Ctrl Pts',(10.063793370495,12.2,-2.6464705267945));
#187561=CARTESIAN_POINT('Ctrl Pts',(10.0661190358309,12.2,-2.64680217853249));
#187562=CARTESIAN_POINT('Ctrl Pts',(10.0684984390365,12.2,-2.6471345208524));
#187563=CARTESIAN_POINT('Ctrl Pts',(10.0709308315426,12.2,-2.6474668567585));
#187564=CARTESIAN_POINT('Ctrl Pts',(10.0733632240487,12.2,-2.6477991926646));
#187565=CARTESIAN_POINT('Ctrl Pts',(10.0758486035812,12.2,-2.64813152383563));
#187566=CARTESIAN_POINT('Ctrl Pts',(10.0783862399034,12.2,-2.64846317774027));
#187567=CARTESIAN_POINT('Ctrl Pts',(10.0809238764561,12.2,-2.64879483167505));
#187568=CARTESIAN_POINT('Ctrl Pts',(10.0835137664236,12.2,-2.64912580789308));
#187569=CARTESIAN_POINT('Ctrl Pts',(10.0861551972378,12.2,-2.64945545299428));
#187570=CARTESIAN_POINT('Ctrl Pts',(10.088796627812,12.2,-2.64978509806555));
#187571=CARTESIAN_POINT('Ctrl Pts',(10.0914895985887,12.2,-2.65011341309641));
#187572=CARTESIAN_POINT('Ctrl Pts',(10.0942334084079,12.2,-2.65043976125113));
#187573=CARTESIAN_POINT('Ctrl Pts',(10.0969772182271,12.2,-2.65076610940585));
#187574=CARTESIAN_POINT('Ctrl Pts',(10.0997718692422,12.2,-2.65109049432738));
#187575=CARTESIAN_POINT('Ctrl Pts',(10.1026166770534,12.2,-2.65141229548247));
#187576=CARTESIAN_POINT('Ctrl Pts',(10.1054614848645,12.2,-2.65173409663756));
#187577=CARTESIAN_POINT('Ctrl Pts',(10.1083564488809,12.2,-2.65205331806851));
#187578=CARTESIAN_POINT('Ctrl Pts',(10.1113009016873,12.2,-2.65236935747391));
#187579=CARTESIAN_POINT('Ctrl Pts',(10.114245354761,12.2,-2.65268539690801));
#187580=CARTESIAN_POINT('Ctrl Pts',(10.1172392960313,12.2,-2.65299825575017));
#187581=CARTESIAN_POINT('Ctrl Pts',(10.1202820703659,12.2,-2.65330735293352));
#187582=CARTESIAN_POINT('Ctrl Pts',(10.1233248444241,12.2,-2.65361645008879));
#187583=CARTESIAN_POINT('Ctrl Pts',(10.1264164538067,12.2,-2.65392178319278));
#187584=CARTESIAN_POINT('Ctrl Pts',(10.1295562557901,12.2,-2.65422278851655));
#187585=CARTESIAN_POINT('Ctrl Pts',(10.1326960577735,12.2,-2.65452379384033));
#187586=CARTESIAN_POINT('Ctrl Pts',(10.1358840529847,12.2,-2.65482046992015));
#187587=CARTESIAN_POINT('Ctrl Pts',(10.1391196148639,12.2,-2.65511226549322));
#187588=CARTESIAN_POINT('Ctrl Pts',(10.142355177037,12.2,-2.65540406109279));
#187589=CARTESIAN_POINT('Ctrl Pts',(10.1456383039564,12.2,-2.6556909793419));
#187590=CARTESIAN_POINT('Ctrl Pts',(10.1489683832232,12.2,-2.65597247827368));
#187591=CARTESIAN_POINT('Ctrl Pts',(10.1522984621876,12.2,-2.65625397717988));
#187592=CARTESIAN_POINT('Ctrl Pts',(10.1556754910989,12.2,-2.65653006229181));
#187593=CARTESIAN_POINT('Ctrl Pts',(10.15909886924,12.2,-2.6568002079499));
#187594=CARTESIAN_POINT('Ctrl Pts',(10.162522247381,12.2,-2.657070353608));
#187595=CARTESIAN_POINT('Ctrl Pts',(10.1659919738642,12.2,-2.65733456172252));
#187596=CARTESIAN_POINT('Ctrl Pts',(10.1695074579,12.2,-2.65759232346359));
#187597=CARTESIAN_POINT('Ctrl Pts',(10.1730229422551,12.2,-2.65785008522808));
#187598=CARTESIAN_POINT('Ctrl Pts',(10.1765841833362,12.2,-2.65810140029853));
#187599=CARTESIAN_POINT('Ctrl Pts',(10.1801906020489,12.2,-2.65834577399032));
#187600=CARTESIAN_POINT('Ctrl Pts',(10.1837970204339,12.2,-2.65859014765991));
#187601=CARTESIAN_POINT('Ctrl Pts',(10.1874486162258,12.2,-2.65882757816672));
#187602=CARTESIAN_POINT('Ctrl Pts',(10.1911448195082,12.2,-2.6590575867417));
#187603=CARTESIAN_POINT('Ctrl Pts',(10.1948410227905,12.2,-2.65928759531668));
#187604=CARTESIAN_POINT('Ctrl Pts',(10.1985818339515,12.2,-2.65951017837586));
#187605=CARTESIAN_POINT('Ctrl Pts',(10.2023666943338,12.2,-2.65972486721258));
#187606=CARTESIAN_POINT('Ctrl Pts',(10.20615155506,12.2,-2.65993955606879));
#187607=CARTESIAN_POINT('Ctrl Pts',(10.2099804643496,12.2,-2.66014635131974));
#187608=CARTESIAN_POINT('Ctrl Pts',(10.213852873147,12.2,-2.66034479224666));
#187609=CARTESIAN_POINT('Ctrl Pts',(10.2177252815926,12.2,-2.66054323315555));
#187610=CARTESIAN_POINT('Ctrl Pts',(10.2216411903358,12.2,-2.66073332143923));
#187611=CARTESIAN_POINT('Ctrl Pts',(10.2256000587933,12.2,-2.66091461026678));
#187612=CARTESIAN_POINT('Ctrl Pts',(10.2302187389002,12.2,-2.6611261139099));
#187613=CARTESIAN_POINT('Ctrl Pts',(10.2348958924318,12.2,-2.6613256374042));
#187614=CARTESIAN_POINT('Ctrl Pts',(10.2396306779256,12.2,-2.66151249180915));
#187615=CARTESIAN_POINT('Ctrl Pts',(10.2430126675113,12.2,-2.66164595923918));
#187616=CARTESIAN_POINT('Ctrl Pts',(10.2464240620142,12.2,-2.6617729621052));
#187617=CARTESIAN_POINT('Ctrl Pts',(10.2498645584749,12.2,-2.66189325550743));
#187618=CARTESIAN_POINT('Ctrl Pts',(10.2533050545606,12.2,-2.66201354889655));
#187619=CARTESIAN_POINT('Ctrl Pts',(10.2567746537871,12.2,-2.66212713260269));
#187620=CARTESIAN_POINT('Ctrl Pts',(10.260273059584,12.2,-2.66223376599441));
#187621=CARTESIAN_POINT('Ctrl Pts',(10.2637714657622,12.2,-2.66234039939776));
#187622=CARTESIAN_POINT('Ctrl Pts',(10.2672986760149,12.2,-2.66244008130401));
#187623=CARTESIAN_POINT('Ctrl Pts',(10.2708543990681,12.2,-2.66253257797127));
#187624=CARTESIAN_POINT('Ctrl Pts',(10.2744101221214,12.2,-2.66262507463852));
#187625=CARTESIAN_POINT('Ctrl Pts',(10.277994357841,12.2,-2.66271038324212));
#187626=CARTESIAN_POINT('Ctrl Pts',(10.281606816839,12.2,-2.66278827498263));
#187627=CARTESIAN_POINT('Ctrl Pts',(10.2852192758369,12.2,-2.66286616672315));
#187628=CARTESIAN_POINT('Ctrl Pts',(10.2888599562005,12.2,-2.66293663952882));
#187629=CARTESIAN_POINT('Ctrl Pts',(10.2925285750184,12.2,-2.66299946723755));
#187630=CARTESIAN_POINT('Ctrl Pts',(10.2961971938364,12.2,-2.66306229494628));
#187631=CARTESIAN_POINT('Ctrl Pts',(10.2998937483913,12.2,-2.66311747771871));
#187632=CARTESIAN_POINT('Ctrl Pts',(10.3036179590148,12.2,-2.66316479299689));
#187633=CARTESIAN_POINT('Ctrl Pts',(10.3080870116007,12.2,-2.66322157132866));
#187634=CARTESIAN_POINT('Ctrl Pts',(10.3125958873221,12.2,-2.66326702091345));
#187635=CARTESIAN_POINT('Ctrl Pts',(10.3171441049875,12.2,-2.66330076424635));
#187636=CARTESIAN_POINT('Ctrl Pts',(10.320934286513,12.2,-2.66332888369147));
#187637=CARTESIAN_POINT('Ctrl Pts',(10.3247517896936,12.2,-2.66334887532005));
#187638=CARTESIAN_POINT('Ctrl Pts',(10.328596340247,12.2,-2.66336052393185));
#187639=CARTESIAN_POINT('Ctrl Pts',(10.3332098011625,12.2,-2.66337450226676));
#187640=CARTESIAN_POINT('Ctrl Pts',(10.3378622083032,12.2,-2.66337646909247));
#187641=CARTESIAN_POINT('Ctrl Pts',(10.3425530957121,12.2,-2.66336606150733));
#187642=CARTESIAN_POINT('Ctrl Pts',(10.3464621683398,12.2,-2.66335738852019));
#187643=CARTESIAN_POINT('Ctrl Pts',(10.3503979631104,12.2,-2.66334012392512));
#187644=CARTESIAN_POINT('Ctrl Pts',(10.3543602122098,12.2,-2.66331406322996));
#187645=CARTESIAN_POINT('Ctrl Pts',(10.3583224613092,12.2,-2.6632880025348));
#187646=CARTESIAN_POINT('Ctrl Pts',(10.3623111655451,12.2,-2.66325314364504));
#187647=CARTESIAN_POINT('Ctrl Pts',(10.3663260612417,12.2,-2.66320928822763));
#187648=CARTESIAN_POINT('Ctrl Pts',(10.3703409569383,12.2,-2.66316543281023));
#187649=CARTESIAN_POINT('Ctrl Pts',(10.3743820430464,12.2,-2.66311257981489));
#187650=CARTESIAN_POINT('Ctrl Pts',(10.3784490595069,12.2,-2.66305053425859));
#187651=CARTESIAN_POINT('Ctrl Pts',(10.382516075524,12.2,-2.66298848870904));
#187652=CARTESIAN_POINT('Ctrl Pts',(10.3866090201511,12.2,-2.66291724791214));
#187653=CARTESIAN_POINT('Ctrl Pts',(10.3907276387278,12.2,-2.66283662076891));
#187654=CARTESIAN_POINT('Ctrl Pts',(10.3948462577535,12.2,-2.6627559936169));
#187655=CARTESIAN_POINT('Ctrl Pts',(10.398990547251,12.2,-2.66266597969561));
#187656=CARTESIAN_POINT('Ctrl Pts',(10.4031602546795,12.2,-2.66256638927973));
#187657=CARTESIAN_POINT('Ctrl Pts',(10.4064960208041,12.2,-2.66248671694268));
#187658=CARTESIAN_POINT('Ctrl Pts',(10.4098480544588,12.2,-2.66240091461654));
#187659=CARTESIAN_POINT('Ctrl Pts',(10.4132162247688,12.2,-2.66230888949997));
#187660=CARTESIAN_POINT('Ctrl Pts',(10.41658439462,12.2,-2.66221686439595));
#187661=CARTESIAN_POINT('Ctrl Pts',(10.4199687025541,12.2,-2.66211861325516));
#187662=CARTESIAN_POINT('Ctrl Pts',(10.4233690202189,12.2,-2.66201404554213));
#187663=CARTESIAN_POINT('Ctrl Pts',(10.4267693383471,12.2,-2.66190947781486));
#187664=CARTESIAN_POINT('Ctrl Pts',(10.4301856654795,12.2,-2.66179859007033));
#187665=CARTESIAN_POINT('Ctrl Pts',(10.4336178749999,12.2,-2.66168129300838));
#187666=CARTESIAN_POINT('Ctrl Pts',(10.4370500845203,12.2,-2.66156399594643));
#187667=CARTESIAN_POINT('Ctrl Pts',(10.4404981767314,12.2,-2.66144028720596));
#187668=CARTESIAN_POINT('Ctrl Pts',(10.4439620250329,12.2,-2.66131007625375));
#187669=CARTESIAN_POINT('Ctrl Pts',(10.4474258728624,12.2,-2.66117986531928));
#187670=CARTESIAN_POINT('Ctrl Pts',(10.4509054783174,12.2,-2.66104315177794));
#187671=CARTESIAN_POINT('Ctrl Pts',(10.4544007147142,12.2,-2.66089984623347));
#187672=CARTESIAN_POINT('Ctrl Pts',(10.4578959515872,12.2,-2.66075654066948));
#187673=CARTESIAN_POINT('Ctrl Pts',(10.4614068208521,12.2,-2.66060664289754));
#187674=CARTESIAN_POINT('Ctrl Pts',(10.4649331971015,12.2,-2.66045006449944));
#187675=CARTESIAN_POINT('Ctrl Pts',(10.4684595728703,12.2,-2.66029348612266));
#187676=CARTESIAN_POINT('Ctrl Pts',(10.4720014559233,12.2,-2.66013022593842));
#187677=CARTESIAN_POINT('Ctrl Pts',(10.4755587244092,12.2,-2.65996019773054));
#187678=CARTESIAN_POINT('Ctrl Pts',(10.4791159933799,12.2,-2.6597901694995));
#187679=CARTESIAN_POINT('Ctrl Pts',(10.4826886477473,12.2,-2.6596133735348));
#187680=CARTESIAN_POINT('Ctrl Pts',(10.4862765655123,12.2,-2.65942972201502));
#187681=CARTESIAN_POINT('Ctrl Pts',(10.4898644827884,12.2,-2.65924607052027));
#187682=CARTESIAN_POINT('Ctrl Pts',(10.493467662401,12.2,-2.65905556520786));
#187683=CARTESIAN_POINT('Ctrl Pts',(10.4970859854376,12.2,-2.65885811972445));
#187684=CARTESIAN_POINT('Ctrl Pts',(10.5007043089671,12.2,-2.65866067421414));
#187685=CARTESIAN_POINT('Ctrl Pts',(10.5043377735346,12.2,-2.65845628950023));
#187686=CARTESIAN_POINT('Ctrl Pts',(10.50798626179,12.2,-2.6582448819327));
#187687=CARTESIAN_POINT('Ctrl Pts',(10.5125468718606,12.2,-2.65798062248768));
#187688=CARTESIAN_POINT('Ctrl Pts',(10.5171309534808,12.2,-2.65770538875962));
#187689=CARTESIAN_POINT('Ctrl Pts',(10.5217382778098,12.2,-2.65741901950843));
#187690=CARTESIAN_POINT('Ctrl Pts',(10.5254241369717,12.2,-2.6571899241262));
#187691=CARTESIAN_POINT('Ctrl Pts',(10.5291248681038,12.2,-2.65695370381061));
#187692=CARTESIAN_POINT('Ctrl Pts',(10.532840357188,12.2,-2.65671027505321));
#187693=CARTESIAN_POINT('Ctrl Pts',(10.5365558467784,12.2,-2.65646684626264));
#187694=CARTESIAN_POINT('Ctrl Pts',(10.5402860927067,12.2,-2.65621620964898));
#187695=CARTESIAN_POINT('Ctrl Pts',(10.5440309783562,12.2,-2.65595828674555));
#187696=CARTESIAN_POINT('Ctrl Pts',(10.5477758634954,12.2,-2.65570036387728));
#187697=CARTESIAN_POINT('Ctrl Pts',(10.551535387143,12.2,-2.65543515296914));
#187698=CARTESIAN_POINT('Ctrl Pts',(10.555309435744,12.2,-2.65516257675622));
#187699=CARTESIAN_POINT('Ctrl Pts',(10.5590834848592,12.2,-2.65489000050617));
#187700=CARTESIAN_POINT('Ctrl Pts',(10.5628720566888,12.2,-2.65461005757041));
#187701=CARTESIAN_POINT('Ctrl Pts',(10.5666750382859,12.2,-2.65432267077648));
#187702=CARTESIAN_POINT('Ctrl Pts',(10.5704780193649,12.2,-2.65403528402171));
#187703=CARTESIAN_POINT('Ctrl Pts',(10.574295408027,12.2,-2.65374045406565));
#187704=CARTESIAN_POINT('Ctrl Pts',(10.5781270918234,12.2,-2.65343810325781));
#187705=CARTESIAN_POINT('Ctrl Pts',(10.5819587761419,12.2,-2.65313575240877));
#187706=CARTESIAN_POINT('Ctrl Pts',(10.5858047554857,12.2,-2.65282588044637));
#187707=CARTESIAN_POINT('Ctrl Pts',(10.5896649152692,12.2,-2.65250841298316));
#187708=CARTESIAN_POINT('Ctrl Pts',(10.5935250745268,12.2,-2.6521909455632));
#187709=CARTESIAN_POINT('Ctrl Pts',(10.5973994151751,12.2,-2.65186588245979));
#187710=CARTESIAN_POINT('Ctrl Pts',(10.6012878243558,12.2,-2.65153314782111));
#187711=CARTESIAN_POINT('Ctrl Pts',(10.606148336229,12.2,-2.65111722948876));
#187712=CARTESIAN_POINT('Ctrl Pts',(10.6110308302991,12.2,-2.65068932611216));
#187713=CARTESIAN_POINT('Ctrl Pts',(10.6159350889084,12.2,-2.6502492943076));
#187714=CARTESIAN_POINT('Ctrl Pts',(10.6198584960097,12.2,-2.64989726884476));
#187715=CARTESIAN_POINT('Ctrl Pts',(10.6237958324915,12.2,-2.64953748080764));
#187716=CARTESIAN_POINT('Ctrl Pts',(10.6277469875026,12.2,-2.64916985750813));
#187717=CARTESIAN_POINT('Ctrl Pts',(10.6316981419753,12.2,-2.64880223425871));
#187718=CARTESIAN_POINT('Ctrl Pts',(10.635663115301,12.2,-2.64842677796113));
#187719=CARTESIAN_POINT('Ctrl Pts',(10.6396417971411,12.2,-2.64804341460439));
#187720=CARTESIAN_POINT('Ctrl Pts',(10.6436204795231,12.2,-2.64766005119542));
#187721=CARTESIAN_POINT('Ctrl Pts',(10.6476128690038,12.2,-2.64726878133014));
#187722=CARTESIAN_POINT('Ctrl Pts',(10.6516188599999,12.2,-2.64686953647505));
#187723=CARTESIAN_POINT('Ctrl Pts',(10.6566263484721,12.2,-2.64637048043338));
#187724=CARTESIAN_POINT('Ctrl Pts',(10.6616550858166,12.2,-2.64585896150561));
#187725=CARTESIAN_POINT('Ctrl Pts',(10.6667048610249,12.2,-2.64533484324172));
#187726=CARTESIAN_POINT('Ctrl Pts',(10.6707446814117,12.2,-2.64491554860775));
#187727=CARTESIAN_POINT('Ctrl Pts',(10.6747979657862,12.2,-2.6444881928673));
#187728=CARTESIAN_POINT('Ctrl Pts',(10.6788646068981,12.2,-2.64405270545384));
#187729=CARTESIAN_POINT('Ctrl Pts',(10.6829312474559,12.2,-2.64361721809972));
#187730=CARTESIAN_POINT('Ctrl Pts',(10.6870112458326,12.2,-2.64317359934322));
#187731=CARTESIAN_POINT('Ctrl Pts',(10.6911044932388,12.2,-2.64272178326702));
#187732=CARTESIAN_POINT('Ctrl Pts',(10.6951977412026,12.2,-2.64226996712926));
#187733=CARTESIAN_POINT('Ctrl Pts',(10.699304240042,12.2,-2.64180995186651));
#187734=CARTESIAN_POINT('Ctrl Pts',(10.7034238831568,12.2,-2.64134167317348));
#187735=CARTESIAN_POINT('Ctrl Pts',(10.7075435257102,12.2,-2.64087339454425));
#187736=CARTESIAN_POINT('Ctrl Pts',(10.7116763128814,12.2,-2.64039685245498));
#187737=CARTESIAN_POINT('Ctrl Pts',(10.7158221381528,12.2,-2.63991197927294));
#187738=CARTESIAN_POINT('Ctrl Pts',(10.719967963989,12.2,-2.63942710602484));
#187739=CARTESIAN_POINT('Ctrl Pts',(10.7241268296851,12.2,-2.6389339037109));
#187740=CARTESIAN_POINT('Ctrl Pts',(10.728298629122,12.2,-2.63843230693555));
#187741=CARTESIAN_POINT('Ctrl Pts',(10.7324704279905,12.2,-2.63793071022855));
#187742=CARTESIAN_POINT('Ctrl Pts',(10.7366551617147,12.2,-2.63742071906886));
#187743=CARTESIAN_POINT('Ctrl Pts',(10.7408527256485,12.2,-2.63690226983402));
#187744=CARTESIAN_POINT('Ctrl Pts',(10.7450502901542,12.2,-2.63638382052854));
#187745=CARTESIAN_POINT('Ctrl Pts',(10.7492606860782,12.2,-2.63585691344704));
#187746=CARTESIAN_POINT('Ctrl Pts',(10.7534838085869,12.2,-2.63532148597286));
#187747=CARTESIAN_POINT('Ctrl Pts',(10.7577069305203,12.2,-2.63478605857163));
#187748=CARTESIAN_POINT('Ctrl Pts',(10.7619427799196,12.2,-2.63424210981464));
#187749=CARTESIAN_POINT('Ctrl Pts',(10.7661912541168,12.2,-2.63368957855518));
#187750=CARTESIAN_POINT('Ctrl Pts',(10.7704397288928,12.2,-2.63313704722043));
#187751=CARTESIAN_POINT('Ctrl Pts',(10.7747008286768,12.2,-2.63257593266556));
#187752=CARTESIAN_POINT('Ctrl Pts',(10.7789744517994,12.2,-2.63200617524506));
#187753=CARTESIAN_POINT('Ctrl Pts',(10.7832480743397,12.2,-2.63143641790218));
#187754=CARTESIAN_POINT('Ctrl Pts',(10.7875342193775,12.2,-2.63085801691937));
#187755=CARTESIAN_POINT('Ctrl Pts',(10.7918327865804,12.2,-2.63027091107937));
#187756=CARTESIAN_POINT('Ctrl Pts',(10.796131354369,12.2,-2.62968380515938));
#187757=CARTESIAN_POINT('Ctrl Pts',(10.8004423427114,12.2,-2.62908799540758));
#187758=CARTESIAN_POINT('Ctrl Pts',(10.8047656532445,12.2,-2.62848342148297));
#187759=CARTESIAN_POINT('Ctrl Pts',(10.8090889631885,12.2,-2.62787884764073));
#187760=CARTESIAN_POINT('Ctrl Pts',(10.8134245954902,12.2,-2.62726551164167));
#187761=CARTESIAN_POINT('Ctrl Pts',(10.8177724480224,12.2,-2.6266433518601));
#187762=CARTESIAN_POINT('Ctrl Pts',(10.822120301147,12.2,-2.62602119199376));
#187763=CARTESIAN_POINT('Ctrl Pts',(10.8264803750866,12.2,-2.6253902105877));
#187764=CARTESIAN_POINT('Ctrl Pts',(10.8308525704916,12.2,-2.62475034927505));
#187765=CARTESIAN_POINT('Ctrl Pts',(10.8363178144499,12.2,-2.62395052267783));
#187766=CARTESIAN_POINT('Ctrl Pts',(10.8418019999779,12.2,-2.62313681862562));
#187767=CARTESIAN_POINT('Ctrl Pts',(10.8473049335446,12.2,-2.6223091295246));
#187768=CARTESIAN_POINT('Ctrl Pts',(10.8506066935646,12.2,-2.62181251608203));
#187769=CARTESIAN_POINT('Ctrl Pts',(10.853915201619,12.2,-2.62131086666771));
#187770=CARTESIAN_POINT('Ctrl Pts',(10.8572304182219,12.2,-2.62080415876718));
#187771=CARTESIAN_POINT('Ctrl Pts',(10.8605456348248,12.2,-2.62029745086664));
#187772=CARTESIAN_POINT('Ctrl Pts',(10.8638675590087,12.2,-2.61978568495375));
#187773=CARTESIAN_POINT('Ctrl Pts',(10.8671961500955,12.2,-2.61926883559797));
#187774=CARTESIAN_POINT('Ctrl Pts',(10.8705247411823,12.2,-2.61875198624219));
#187775=CARTESIAN_POINT('Ctrl Pts',(10.873859999177,12.2,-2.61823005451176));
#187776=CARTESIAN_POINT('Ctrl Pts',(10.8772018823047,12.2,-2.61770301711494));
#187777=CARTESIAN_POINT('Ctrl Pts',(10.8805437660395,12.2,-2.61717597962238));
#187778=CARTESIAN_POINT('Ctrl Pts',(10.8838922755261,12.2,-2.6166438358117));
#187779=CARTESIAN_POINT('Ctrl Pts',(10.887247370223,12.2,-2.61610656335792));
#187780=CARTESIAN_POINT('Ctrl Pts',(10.8906024643103,12.2,-2.61556929100174));
#187781=CARTESIAN_POINT('Ctrl Pts',(10.893964142805,12.2,-2.61502689076879));
#187782=CARTESIAN_POINT('Ctrl Pts',(10.897332365185,12.2,-2.61447933838573));
#187783=CARTESIAN_POINT('Ctrl Pts',(10.9007005875649,12.2,-2.61393178600267));
#187784=CARTESIAN_POINT('Ctrl Pts',(10.9040753551409,12.2,-2.61337908225267));
#187785=CARTESIAN_POINT('Ctrl Pts',(10.9074566253519,12.2,-2.61282120389749));
#187786=CARTESIAN_POINT('Ctrl Pts',(10.910837895563,12.2,-2.61226332554231));
#187787=CARTESIAN_POINT('Ctrl Pts',(10.9142256696232,12.2,-2.61170027346274));
#187788=CARTESIAN_POINT('Ctrl Pts',(10.9176199072499,12.2,-2.61113202498339));
#187789=CARTESIAN_POINT('Ctrl Pts',(10.9210141448766,12.2,-2.61056377650403));
#187790=CARTESIAN_POINT('Ctrl Pts',(10.924414846003,12.2,-2.60999033060822));
#187791=CARTESIAN_POINT('Ctrl Pts',(10.9278219701286,12.2,-2.60941166708804));
#187792=CARTESIAN_POINT('Ctrl Pts',(10.9312290942543,12.2,-2.60883300356785));
#187793=CARTESIAN_POINT('Ctrl Pts',(10.9346426415924,12.2,-2.6082491198214));
#187794=CARTESIAN_POINT('Ctrl Pts',(10.9380625728883,12.2,-2.60765999685565));
#187795=CARTESIAN_POINT('Ctrl Pts',(10.9414825041842,12.2,-2.6070708738899));
#187796=CARTESIAN_POINT('Ctrl Pts',(10.9449088188272,12.2,-2.60647651024159));
#187797=CARTESIAN_POINT('Ctrl Pts',(10.9483414764933,12.2,-2.60587688434743));
#187798=CARTESIAN_POINT('Ctrl Pts',(10.9517741347829,12.2,-2.60527725834434));
#187799=CARTESIAN_POINT('Ctrl Pts',(10.9552131362827,12.2,-2.60467237013976));
#187800=CARTESIAN_POINT('Ctrl Pts',(10.9586584424927,12.2,-2.6040621981337));
#187801=CARTESIAN_POINT('Ctrl Pts',(10.9621037480767,12.2,-2.60345202623848));
#187802=CARTESIAN_POINT('Ctrl Pts',(10.9655553572687,12.2,-2.60283657054354));
#187803=CARTESIAN_POINT('Ctrl Pts',(10.9690132313936,12.2,-2.60221580969063));
#187804=CARTESIAN_POINT('Ctrl Pts',(10.9724711055185,12.2,-2.60159504883773));
#187805=CARTESIAN_POINT('Ctrl Pts',(10.9759352440467,12.2,-2.60096898362943));
#187806=CARTESIAN_POINT('Ctrl Pts',(10.9794056077281,12.2,-2.60033759181614));
#187807=CARTESIAN_POINT('Ctrl Pts',(10.9840327590931,12.2,-2.59949573610333));
#187808=CARTESIAN_POINT('Ctrl Pts',(10.9886709779376,12.2,-2.59864441231112));
#187809=CARTESIAN_POINT('Ctrl Pts',(10.9933201712231,12.2,-2.59778356988246));
#187810=CARTESIAN_POINT('Ctrl Pts',(10.996807066979,12.2,-2.59713793791436));
#187811=CARTESIAN_POINT('Ctrl Pts',(11.0003001352533,12.2,-2.59648695240308));
#187812=CARTESIAN_POINT('Ctrl Pts',(11.0037993384711,12.2,-2.59583059289029));
#187813=CARTESIAN_POINT('Ctrl Pts',(11.0072985410531,12.2,-2.59517423349675));
#187814=CARTESIAN_POINT('Ctrl Pts',(11.0108038777765,12.2,-2.59451249950347));
#187815=CARTESIAN_POINT('Ctrl Pts',(11.0143153099411,12.2,-2.59384537069391));
#187816=CARTESIAN_POINT('Ctrl Pts',(11.0178267421057,12.2,-2.59317824188435));
#187817=CARTESIAN_POINT('Ctrl Pts',(11.0213442700446,12.2,-2.59250571880876));
#187818=CARTESIAN_POINT('Ctrl Pts',(11.0248678547082,12.2,-2.59182778050006));
#187819=CARTESIAN_POINT('Ctrl Pts',(11.0283914393719,12.2,-2.59114984219136));
#187820=CARTESIAN_POINT('Ctrl Pts',(11.0319210808269,12.2,-2.59046648861621));
#187821=CARTESIAN_POINT('Ctrl Pts',(11.0354567414063,12.2,-2.58977770076671));
#187822=CARTESIAN_POINT('Ctrl Pts',(11.0389924019856,12.2,-2.58908891291721));
#187823=CARTESIAN_POINT('Ctrl Pts',(11.0425340804993,12.2,-2.5883946904776));
#187824=CARTESIAN_POINT('Ctrl Pts',(11.0460817398386,12.2,-2.58769501313537));
#187825=CARTESIAN_POINT('Ctrl Pts',(11.0496293991779,12.2,-2.58699533579314));
#187826=CARTESIAN_POINT('Ctrl Pts',(11.0531830388207,12.2,-2.58629020434506));
#187827=CARTESIAN_POINT('Ctrl Pts',(11.0567426204823,12.2,-2.58557959812163));
#187828=CARTESIAN_POINT('Ctrl Pts',(11.0626752568003,12.2,-2.58439525437287));
#187829=CARTESIAN_POINT('Ctrl Pts',(11.0686243990709,12.2,-2.58319570559104));
#187830=CARTESIAN_POINT('Ctrl Pts',(11.0745898719863,12.2,-2.58198086163395));
#187831=CARTESIAN_POINT('Ctrl Pts',(11.0781691562557,12.2,-2.58125195515377));
#187832=CARTESIAN_POINT('Ctrl Pts',(11.0817543194767,12.2,-2.58051754229703));
#187833=CARTESIAN_POINT('Ctrl Pts',(11.0853453242911,12.2,-2.57977760385541));
#187834=CARTESIAN_POINT('Ctrl Pts',(11.0889363284531,12.2,-2.57903766554821));
#187835=CARTESIAN_POINT('Ctrl Pts',(11.0925331738306,12.2,-2.57829220223224));
#187836=CARTESIAN_POINT('Ctrl Pts',(11.096135823172,12.2,-2.57754119484637));
#187837=CARTESIAN_POINT('Ctrl Pts',(11.0997384725134,12.2,-2.57679018746049));
#187838=CARTESIAN_POINT('Ctrl Pts',(11.1033469247248,12.2,-2.57603363548969));
#187839=CARTESIAN_POINT('Ctrl Pts',(11.106961143844,12.2,-2.57527152068356));
#187840=CARTESIAN_POINT('Ctrl Pts',(11.1105753629631,12.2,-2.57450940587743));
#187841=CARTESIAN_POINT('Ctrl Pts',(11.114195347765,12.2,-2.5737417280053));
#187842=CARTESIAN_POINT('Ctrl Pts',(11.1178210620082,12.2,-2.57296846920006));
#187843=CARTESIAN_POINT('Ctrl Pts',(11.1214467762515,12.2,-2.57219521039482));
#187844=CARTESIAN_POINT('Ctrl Pts',(11.1250782213195,12.2,-2.57141637033981));
#187845=CARTESIAN_POINT('Ctrl Pts',(11.1287153575619,12.2,-2.57063193107713));
#187846=CARTESIAN_POINT('Ctrl Pts',(11.1323524938042,12.2,-2.56984749181445));
#187847=CARTESIAN_POINT('Ctrl Pts',(11.1359953227117,12.2,-2.56905745416413));
#187848=CARTESIAN_POINT('Ctrl Pts',(11.1396438055524,12.2,-2.56826179732061));
#187849=CARTESIAN_POINT('Ctrl Pts',(11.1432922883931,12.2,-2.56746614047708));
#187850=CARTESIAN_POINT('Ctrl Pts',(11.1469464247525,12.2,-2.56666486501253));
#187851=CARTESIAN_POINT('Ctrl Pts',(11.1506061784521,12.2,-2.56585795370929));
#187852=CARTESIAN_POINT('Ctrl Pts',(11.1542659328165,12.2,-2.56505104225945));
#187853=CARTESIAN_POINT('Ctrl Pts',(11.1579313042159,12.2,-2.56423849550803));
#187854=CARTESIAN_POINT('Ctrl Pts',(11.1616022605418,12.2,-2.56342029659668));
#187855=CARTESIAN_POINT('Ctrl Pts',(11.1652732162009,12.2,-2.56260209783397));
#187856=CARTESIAN_POINT('Ctrl Pts',(11.168949756718,12.2,-2.5617782472799));
#187857=CARTESIAN_POINT('Ctrl Pts',(11.1726318442097,12.2,-2.56094872689288));
#187858=CARTESIAN_POINT('Ctrl Pts',(11.1763139317014,12.2,-2.56011920650586));
#187859=CARTESIAN_POINT('Ctrl Pts',(11.180001564104,12.2,-2.55928401492258));
#187860=CARTESIAN_POINT('Ctrl Pts',(11.1836946977783,12.2,-2.55844313249096));
#187861=CARTESIAN_POINT('Ctrl Pts',(11.1873878314526,12.2,-2.55760225005933));
#187862=CARTESIAN_POINT('Ctrl Pts',(11.1910864657143,12.2,-2.55675567444037));
#187863=CARTESIAN_POINT('Ctrl Pts',(11.1947905667215,12.2,-2.55590339075916));
#187864=CARTESIAN_POINT('Ctrl Pts',(11.2009640686245,12.2,-2.55448291790553));
#187865=CARTESIAN_POINT('Ctrl Pts',(11.2071527573142,12.2,-2.55304659031659));
#187866=CARTESIAN_POINT('Ctrl Pts',(11.2133565919999,12.2,-2.55159439000002));
#187867=CARTESIAN_POINT('Origin',(-5.66257110645729E-14,15.2,-1.77635683940025E-14));
#187868=CARTESIAN_POINT('',(10.3068855235888,15.2,-1.18690176536278));
#187869=CARTESIAN_POINT('',(10.3068855235888,12.2,-1.18690176536278));
#187870=CARTESIAN_POINT('',(10.3068855229999,15.2,-1.18690176500001));
#187871=CARTESIAN_POINT('Origin',(-5.66257110645729E-14,12.2,-1.77635683940025E-14));
#187872=CARTESIAN_POINT('Origin',(-5.66257110645729E-14,15.2,-1.77635683940025E-14));
#187873=CARTESIAN_POINT('Origin',(-5.66257110645729E-14,15.2,-1.77635683940025E-14));
#187874=CARTESIAN_POINT('',(11.4623505329999,15.2,-0.929795809000016));
#187875=CARTESIAN_POINT('',(11.4869855316539,15.2,-0.54695830599941));
#187876=CARTESIAN_POINT('Origin',(-5.66257110645729E-14,15.2,-1.77635683940025E-14));
#187877=CARTESIAN_POINT('',(11.4869855316539,12.2,-0.54695830599941));
#187878=CARTESIAN_POINT('',(11.4869855319999,15.2,-0.546958306000014));
#187879=CARTESIAN_POINT('',(11.4623505329999,12.2,-0.929795809000016));
#187880=CARTESIAN_POINT('Origin',(-5.66257110645729E-14,12.2,-1.77635683940025E-14));
#187881=CARTESIAN_POINT('',(11.4623505329999,15.2,-0.929795809000016));
#187882=CARTESIAN_POINT('Ctrl Pts',(10.3068855239999,15.2,-1.18690176600001));
#187883=CARTESIAN_POINT('Ctrl Pts',(10.3068855239999,11.6,-1.18690176600001));
#187884=CARTESIAN_POINT('Ctrl Pts',(10.3070598099999,15.2,-1.18690675400002));
#187885=CARTESIAN_POINT('Ctrl Pts',(10.3070598099999,11.6,-1.18690675400002));
#187886=CARTESIAN_POINT('Ctrl Pts',(10.3074144739999,15.2,-1.18691681500001));
#187887=CARTESIAN_POINT('Ctrl Pts',(10.3074144739999,11.6,-1.18691681500001));
#187888=CARTESIAN_POINT('Ctrl Pts',(10.3079518789999,15.2,-1.18693179700001));
#187889=CARTESIAN_POINT('Ctrl Pts',(10.3079518789999,11.6,-1.18693179700002));
#187890=CARTESIAN_POINT('Ctrl Pts',(10.3086758299999,15.2,-1.18695143900001));
#187891=CARTESIAN_POINT('Ctrl Pts',(10.3086758299999,11.6,-1.18695143900002));
#187892=CARTESIAN_POINT('Ctrl Pts',(10.3095915439999,15.2,-1.18697537100001));
#187893=CARTESIAN_POINT('Ctrl Pts',(10.3095915439999,11.6,-1.18697537100001));
#187894=CARTESIAN_POINT('Ctrl Pts',(10.3105221239999,15.2,-1.18699875500001));
#187895=CARTESIAN_POINT('Ctrl Pts',(10.3105221239999,11.6,-1.18699875500001));
#187896=CARTESIAN_POINT('Ctrl Pts',(10.3114622379999,15.2,-1.18702143600002));
#187897=CARTESIAN_POINT('Ctrl Pts',(10.3114622379999,11.6,-1.18702143600002));
#187898=CARTESIAN_POINT('Ctrl Pts',(10.3124118609999,15.2,-1.18704339300002));
#187899=CARTESIAN_POINT('Ctrl Pts',(10.3124118609999,11.6,-1.18704339300002));
#187900=CARTESIAN_POINT('Ctrl Pts',(10.3133709649999,15.2,-1.18706461000002));
#187901=CARTESIAN_POINT('Ctrl Pts',(10.3133709649999,11.6,-1.18706461000002));
#187902=CARTESIAN_POINT('Ctrl Pts',(10.3143395239999,15.2,-1.18708506500001));
#187903=CARTESIAN_POINT('Ctrl Pts',(10.3143395239999,11.6,-1.18708506500001));
#187904=CARTESIAN_POINT('Ctrl Pts',(10.3153175129999,15.2,-1.18710474300002));
#187905=CARTESIAN_POINT('Ctrl Pts',(10.3153175129999,11.6,-1.18710474300002));
#187906=CARTESIAN_POINT('Ctrl Pts',(10.3163049049999,15.2,-1.18712362400001));
#187907=CARTESIAN_POINT('Ctrl Pts',(10.3163049049999,11.6,-1.18712362400002));
#187908=CARTESIAN_POINT('Ctrl Pts',(10.3173016729999,15.2,-1.18714169000001));
#187909=CARTESIAN_POINT('Ctrl Pts',(10.3173016729999,11.6,-1.18714169000001));
#187910=CARTESIAN_POINT('Ctrl Pts',(10.3183077929999,15.2,-1.18715892100001));
#187911=CARTESIAN_POINT('Ctrl Pts',(10.3183077929999,11.6,-1.18715892100001));
#187912=CARTESIAN_POINT('Ctrl Pts',(10.3193232389999,15.2,-1.18717530300001));
#187913=CARTESIAN_POINT('Ctrl Pts',(10.3193232389999,11.6,-1.18717530300001));
#187914=CARTESIAN_POINT('Ctrl Pts',(10.3203479849999,15.2,-1.18719081300001));
#187915=CARTESIAN_POINT('Ctrl Pts',(10.3203479849999,11.6,-1.18719081300001));
#187916=CARTESIAN_POINT('Ctrl Pts',(10.3213820039999,15.2,-1.18720543700002));
#187917=CARTESIAN_POINT('Ctrl Pts',(10.3213820039999,11.6,-1.18720543700002));
#187918=CARTESIAN_POINT('Ctrl Pts',(10.3224252739999,15.2,-1.18721915500001));
#187919=CARTESIAN_POINT('Ctrl Pts',(10.3224252739999,11.6,-1.18721915500001));
#187920=CARTESIAN_POINT('Ctrl Pts',(10.3234777669999,15.2,-1.18723195000001));
#187921=CARTESIAN_POINT('Ctrl Pts',(10.3234777669999,11.6,-1.18723195000001));
#187922=CARTESIAN_POINT('Ctrl Pts',(10.3245394589999,15.2,-1.18724380600002));
#187923=CARTESIAN_POINT('Ctrl Pts',(10.3245394589999,11.6,-1.18724380600002));
#187924=CARTESIAN_POINT('Ctrl Pts',(10.3256103239999,15.2,-1.18725470300001));
#187925=CARTESIAN_POINT('Ctrl Pts',(10.3256103239999,11.6,-1.18725470300001));
#187926=CARTESIAN_POINT('Ctrl Pts',(10.3266903399999,15.2,-1.18726462500002));
#187927=CARTESIAN_POINT('Ctrl Pts',(10.3266903399999,11.6,-1.18726462500002));
#187928=CARTESIAN_POINT('Ctrl Pts',(10.3277794779999,15.2,-1.18727355500001));
#187929=CARTESIAN_POINT('Ctrl Pts',(10.3277794779999,11.6,-1.18727355500001));
#187930=CARTESIAN_POINT('Ctrl Pts',(10.3288777159999,15.2,-1.18728147400001));
#187931=CARTESIAN_POINT('Ctrl Pts',(10.3288777159999,11.6,-1.18728147400002));
#187932=CARTESIAN_POINT('Ctrl Pts',(10.3299850289999,15.2,-1.18728836600001));
#187933=CARTESIAN_POINT('Ctrl Pts',(10.3299850289999,11.6,-1.18728836600001));
#187934=CARTESIAN_POINT('Ctrl Pts',(10.3311013919999,15.2,-1.18729421400001));
#187935=CARTESIAN_POINT('Ctrl Pts',(10.3311013919999,11.6,-1.18729421400001));
#187936=CARTESIAN_POINT('Ctrl Pts',(10.3322267799999,15.2,-1.18729900100002));
#187937=CARTESIAN_POINT('Ctrl Pts',(10.3322267799999,11.6,-1.18729900100002));
#187938=CARTESIAN_POINT('Ctrl Pts',(10.3333611709999,15.2,-1.18730271200001));
#187939=CARTESIAN_POINT('Ctrl Pts',(10.3333611709999,11.6,-1.18730271200001));
#187940=CARTESIAN_POINT('Ctrl Pts',(10.3345045389999,15.2,-1.18730532600001));
#187941=CARTESIAN_POINT('Ctrl Pts',(10.3345045389999,11.6,-1.18730532600001));
#187942=CARTESIAN_POINT('Ctrl Pts',(10.3356568609999,15.2,-1.18730683000001));
#187943=CARTESIAN_POINT('Ctrl Pts',(10.3356568609999,11.6,-1.18730683000001));
#187944=CARTESIAN_POINT('Ctrl Pts',(10.3368181129999,15.2,-1.18730720600002));
#187945=CARTESIAN_POINT('Ctrl Pts',(10.3368181129999,11.6,-1.18730720600002));
#187946=CARTESIAN_POINT('Ctrl Pts',(10.3379882699999,15.2,-1.18730643700002));
#187947=CARTESIAN_POINT('Ctrl Pts',(10.3379882699999,11.6,-1.18730643700002));
#187948=CARTESIAN_POINT('Ctrl Pts',(10.3391673089999,15.2,-1.18730450800001));
#187949=CARTESIAN_POINT('Ctrl Pts',(10.3391673089999,11.6,-1.18730450800001));
#187950=CARTESIAN_POINT('Ctrl Pts',(10.3403552059999,15.2,-1.18730140200002));
#187951=CARTESIAN_POINT('Ctrl Pts',(10.3403552059999,11.6,-1.18730140200002));
#187952=CARTESIAN_POINT('Ctrl Pts',(10.3415519369999,15.2,-1.18729710200002));
#187953=CARTESIAN_POINT('Ctrl Pts',(10.3415519369999,11.6,-1.18729710200002));
#187954=CARTESIAN_POINT('Ctrl Pts',(10.3427574809999,15.2,-1.18729159300001));
#187955=CARTESIAN_POINT('Ctrl Pts',(10.3427574809999,11.6,-1.18729159300001));
#187956=CARTESIAN_POINT('Ctrl Pts',(10.3439718129999,15.2,-1.18728485900002));
#187957=CARTESIAN_POINT('Ctrl Pts',(10.3439718129999,11.6,-1.18728485900002));
#187958=CARTESIAN_POINT('Ctrl Pts',(10.3451949089999,15.2,-1.18727688200002));
#187959=CARTESIAN_POINT('Ctrl Pts',(10.3451949089999,11.6,-1.18727688200002));
#187960=CARTESIAN_POINT('Ctrl Pts',(10.3464267469999,15.2,-1.18726764900002));
#187961=CARTESIAN_POINT('Ctrl Pts',(10.3464267469999,11.6,-1.18726764900002));
#187962=CARTESIAN_POINT('Ctrl Pts',(10.3476673029999,15.2,-1.18725714300002));
#187963=CARTESIAN_POINT('Ctrl Pts',(10.3476673029999,11.6,-1.18725714300002));
#187964=CARTESIAN_POINT('Ctrl Pts',(10.3489165549999,15.2,-1.18724534800001));
#187965=CARTESIAN_POINT('Ctrl Pts',(10.3489165549999,11.6,-1.18724534800001));
#187966=CARTESIAN_POINT('Ctrl Pts',(10.3501744809999,15.2,-1.18723224800001));
#187967=CARTESIAN_POINT('Ctrl Pts',(10.3501744809999,11.6,-1.18723224800001));
#187968=CARTESIAN_POINT('Ctrl Pts',(10.3514410549999,15.2,-1.18721782700002));
#187969=CARTESIAN_POINT('Ctrl Pts',(10.3514410549999,11.6,-1.18721782700002));
#187970=CARTESIAN_POINT('Ctrl Pts',(10.3527162579999,15.2,-1.18720207200001));
#187971=CARTESIAN_POINT('Ctrl Pts',(10.3527162579999,11.6,-1.18720207200001));
#187972=CARTESIAN_POINT('Ctrl Pts',(10.3540000639999,15.2,-1.18718496500001));
#187973=CARTESIAN_POINT('Ctrl Pts',(10.3540000639999,11.6,-1.18718496500001));
#187974=CARTESIAN_POINT('Ctrl Pts',(10.3552924529999,15.2,-1.18716649100001));
#187975=CARTESIAN_POINT('Ctrl Pts',(10.3552924529999,11.6,-1.18716649100001));
#187976=CARTESIAN_POINT('Ctrl Pts',(10.3565934029999,15.2,-1.18714663700001));
#187977=CARTESIAN_POINT('Ctrl Pts',(10.3565934029999,11.6,-1.18714663700001));
#187978=CARTESIAN_POINT('Ctrl Pts',(10.3579028899999,15.2,-1.18712538500001));
#187979=CARTESIAN_POINT('Ctrl Pts',(10.3579028899999,11.6,-1.18712538500001));
#187980=CARTESIAN_POINT('Ctrl Pts',(10.3592208919999,15.2,-1.18710272100001));
#187981=CARTESIAN_POINT('Ctrl Pts',(10.3592208919999,11.6,-1.18710272100001));
#187982=CARTESIAN_POINT('Ctrl Pts',(10.3605473869999,15.2,-1.18707863200001));
#187983=CARTESIAN_POINT('Ctrl Pts',(10.3605473869999,11.6,-1.18707863200001));
#187984=CARTESIAN_POINT('Ctrl Pts',(10.3618823529999,15.2,-1.18705310000002));
#187985=CARTESIAN_POINT('Ctrl Pts',(10.3618823529999,11.6,-1.18705310000002));
#187986=CARTESIAN_POINT('Ctrl Pts',(10.3632257689999,15.2,-1.18702611100002));
#187987=CARTESIAN_POINT('Ctrl Pts',(10.3632257689999,11.6,-1.18702611100002));
#187988=CARTESIAN_POINT('Ctrl Pts',(10.3645776119999,15.2,-1.18699765000001));
#187989=CARTESIAN_POINT('Ctrl Pts',(10.3645776119999,11.6,-1.18699765000002));
#187990=CARTESIAN_POINT('Ctrl Pts',(10.3659378599999,15.2,-1.18696770300001));
#187991=CARTESIAN_POINT('Ctrl Pts',(10.3659378599999,11.6,-1.18696770300002));
#187992=CARTESIAN_POINT('Ctrl Pts',(10.3673064919999,15.2,-1.18693625600002));
#187993=CARTESIAN_POINT('Ctrl Pts',(10.3673064919999,11.6,-1.18693625600002));
#187994=CARTESIAN_POINT('Ctrl Pts',(10.3686834869999,15.2,-1.18690329300001));
#187995=CARTESIAN_POINT('Ctrl Pts',(10.3686834869999,11.6,-1.18690329300001));
#187996=CARTESIAN_POINT('Ctrl Pts',(10.3700688229999,15.2,-1.18686880000002));
#187997=CARTESIAN_POINT('Ctrl Pts',(10.3700688229999,11.6,-1.18686880000002));
#187998=CARTESIAN_POINT('Ctrl Pts',(10.3714624779999,15.2,-1.18683276400001));
#187999=CARTESIAN_POINT('Ctrl Pts',(10.3714624779999,11.6,-1.18683276400001));
#188000=CARTESIAN_POINT('Ctrl Pts',(10.3728644309999,15.2,-1.18679516800002));
#188001=CARTESIAN_POINT('Ctrl Pts',(10.3728644309999,11.6,-1.18679516800002));
#188002=CARTESIAN_POINT('Ctrl Pts',(10.3742746599999,15.2,-1.18675600000001));
#188003=CARTESIAN_POINT('Ctrl Pts',(10.3742746599999,11.6,-1.18675600000001));
#188004=CARTESIAN_POINT('Ctrl Pts',(10.3756931459999,15.2,-1.18671524300002));
#188005=CARTESIAN_POINT('Ctrl Pts',(10.3756931459999,11.6,-1.18671524300002));
#188006=CARTESIAN_POINT('Ctrl Pts',(10.3771198649999,15.2,-1.18667288700002));
#188007=CARTESIAN_POINT('Ctrl Pts',(10.3771198649999,11.6,-1.18667288700002));
#188008=CARTESIAN_POINT('Ctrl Pts',(10.3785547979999,15.2,-1.18662891400001));
#188009=CARTESIAN_POINT('Ctrl Pts',(10.3785547979999,11.6,-1.18662891400001));
#188010=CARTESIAN_POINT('Ctrl Pts',(10.3799979229999,15.2,-1.18658331200002));
#188011=CARTESIAN_POINT('Ctrl Pts',(10.3799979229999,11.6,-1.18658331200002));
#188012=CARTESIAN_POINT('Ctrl Pts',(10.3814492199999,15.2,-1.18653606700001));
#188013=CARTESIAN_POINT('Ctrl Pts',(10.3814492199999,11.6,-1.18653606700002));
#188014=CARTESIAN_POINT('Ctrl Pts',(10.3829086669999,15.2,-1.18648716400001));
#188015=CARTESIAN_POINT('Ctrl Pts',(10.3829086669999,11.6,-1.18648716400001));
#188016=CARTESIAN_POINT('Ctrl Pts',(10.3843762449999,15.2,-1.18643659100002));
#188017=CARTESIAN_POINT('Ctrl Pts',(10.3843762449999,11.6,-1.18643659100002));
#188018=CARTESIAN_POINT('Ctrl Pts',(10.3858519319999,15.2,-1.18638433300001));
#188019=CARTESIAN_POINT('Ctrl Pts',(10.3858519319999,11.6,-1.18638433300002));
#188020=CARTESIAN_POINT('Ctrl Pts',(10.3873357079999,15.2,-1.18633037800001));
#188021=CARTESIAN_POINT('Ctrl Pts',(10.3873357079999,11.6,-1.18633037800001));
#188022=CARTESIAN_POINT('Ctrl Pts',(10.3888275529999,15.2,-1.18627470900002));
#188023=CARTESIAN_POINT('Ctrl Pts',(10.3888275529999,11.6,-1.18627470900002));
#188024=CARTESIAN_POINT('Ctrl Pts',(10.3903274449999,15.2,-1.18621731600001));
#188025=CARTESIAN_POINT('Ctrl Pts',(10.3903274449999,11.6,-1.18621731600001));
#188026=CARTESIAN_POINT('Ctrl Pts',(10.3918353649999,15.2,-1.18615818300002));
#188027=CARTESIAN_POINT('Ctrl Pts',(10.3918353649999,11.6,-1.18615818300002));
#188028=CARTESIAN_POINT('Ctrl Pts',(10.3933512919999,15.2,-1.18609729900002));
#188029=CARTESIAN_POINT('Ctrl Pts',(10.3933512919999,11.6,-1.18609729900002));
#188030=CARTESIAN_POINT('Ctrl Pts',(10.3948752069999,15.2,-1.18603464900001));
#188031=CARTESIAN_POINT('Ctrl Pts',(10.3948752069999,11.6,-1.18603464900001));
#188032=CARTESIAN_POINT('Ctrl Pts',(10.3964070879999,15.2,-1.18597021900001));
#188033=CARTESIAN_POINT('Ctrl Pts',(10.3964070879999,11.6,-1.18597021900001));
#188034=CARTESIAN_POINT('Ctrl Pts',(10.3979469159999,15.2,-1.18590399800001));
#188035=CARTESIAN_POINT('Ctrl Pts',(10.3979469159999,11.6,-1.18590399800001));
#188036=CARTESIAN_POINT('Ctrl Pts',(10.3994946729999,15.2,-1.18583597200002));
#188037=CARTESIAN_POINT('Ctrl Pts',(10.3994946729999,11.6,-1.18583597200002));
#188038=CARTESIAN_POINT('Ctrl Pts',(10.4010503359999,15.2,-1.18576612800001));
#188039=CARTESIAN_POINT('Ctrl Pts',(10.4010503359999,11.6,-1.18576612800001));
#188040=CARTESIAN_POINT('Ctrl Pts',(10.4026138859999,15.2,-1.18569445100002));
#188041=CARTESIAN_POINT('Ctrl Pts',(10.4026138859999,11.6,-1.18569445100002));
#188042=CARTESIAN_POINT('Ctrl Pts',(10.4041853039999,15.2,-1.18562093200001));
#188043=CARTESIAN_POINT('Ctrl Pts',(10.4041853039999,11.6,-1.18562093200001));
#188044=CARTESIAN_POINT('Ctrl Pts',(10.4057645699999,15.2,-1.18554555400001));
#188045=CARTESIAN_POINT('Ctrl Pts',(10.4057645699999,11.6,-1.18554555400001));
#188046=CARTESIAN_POINT('Ctrl Pts',(10.4073516649999,15.2,-1.18546830700001));
#188047=CARTESIAN_POINT('Ctrl Pts',(10.4073516649999,11.6,-1.18546830700002));
#188048=CARTESIAN_POINT('Ctrl Pts',(10.4089465679999,15.2,-1.18538917800001));
#188049=CARTESIAN_POINT('Ctrl Pts',(10.4089465679999,11.6,-1.18538917800001));
#188050=CARTESIAN_POINT('Ctrl Pts',(10.4105492599999,15.2,-1.18530815300002));
#188051=CARTESIAN_POINT('Ctrl Pts',(10.4105492599999,11.6,-1.18530815300002));
#188052=CARTESIAN_POINT('Ctrl Pts',(10.4121597229999,15.2,-1.18522521900001));
#188053=CARTESIAN_POINT('Ctrl Pts',(10.4121597229999,11.6,-1.18522521900001));
#188054=CARTESIAN_POINT('Ctrl Pts',(10.4137779369999,15.2,-1.18514036600001));
#188055=CARTESIAN_POINT('Ctrl Pts',(10.4137779369999,11.6,-1.18514036600002));
#188056=CARTESIAN_POINT('Ctrl Pts',(10.4154038819999,15.2,-1.18505358000002));
#188057=CARTESIAN_POINT('Ctrl Pts',(10.4154038819999,11.6,-1.18505358000002));
#188058=CARTESIAN_POINT('Ctrl Pts',(10.4170375389999,15.2,-1.18496484700001));
#188059=CARTESIAN_POINT('Ctrl Pts',(10.4170375389999,11.6,-1.18496484700001));
#188060=CARTESIAN_POINT('Ctrl Pts',(10.4186788889999,15.2,-1.18487415700002));
#188061=CARTESIAN_POINT('Ctrl Pts',(10.4186788889999,11.6,-1.18487415700002));
#188062=CARTESIAN_POINT('Ctrl Pts',(10.4203279129999,15.2,-1.18478149600001));
#188063=CARTESIAN_POINT('Ctrl Pts',(10.4203279129999,11.6,-1.18478149600001));
#188064=CARTESIAN_POINT('Ctrl Pts',(10.4219845919999,15.2,-1.18468685300002));
#188065=CARTESIAN_POINT('Ctrl Pts',(10.4219845919999,11.6,-1.18468685300002));
#188066=CARTESIAN_POINT('Ctrl Pts',(10.4236489079999,15.2,-1.18459021500001));
#188067=CARTESIAN_POINT('Ctrl Pts',(10.4236489079999,11.6,-1.18459021500001));
#188068=CARTESIAN_POINT('Ctrl Pts',(10.4253208399999,15.2,-1.18449157100001));
#188069=CARTESIAN_POINT('Ctrl Pts',(10.4253208399999,11.6,-1.18449157100002));
#188070=CARTESIAN_POINT('Ctrl Pts',(10.4270003709999,15.2,-1.18439090700001));
#188071=CARTESIAN_POINT('Ctrl Pts',(10.4270003709999,11.6,-1.18439090700001));
#188072=CARTESIAN_POINT('Ctrl Pts',(10.4286874819999,15.2,-1.18428821100002));
#188073=CARTESIAN_POINT('Ctrl Pts',(10.4286874819999,11.6,-1.18428821100002));
#188074=CARTESIAN_POINT('Ctrl Pts',(10.4303821539999,15.2,-1.18418347300001));
#188075=CARTESIAN_POINT('Ctrl Pts',(10.4303821539999,11.6,-1.18418347300001));
#188076=CARTESIAN_POINT('Ctrl Pts',(10.4320843689999,15.2,-1.18407668000001));
#188077=CARTESIAN_POINT('Ctrl Pts',(10.4320843689999,11.6,-1.18407668000002));
#188078=CARTESIAN_POINT('Ctrl Pts',(10.4337941069999,15.2,-1.18396782000001));
#188079=CARTESIAN_POINT('Ctrl Pts',(10.4337941069999,11.6,-1.18396782000001));
#188080=CARTESIAN_POINT('Ctrl Pts',(10.4355113499999,15.2,-1.18385688100001));
#188081=CARTESIAN_POINT('Ctrl Pts',(10.4355113499999,11.6,-1.18385688100001));
#188082=CARTESIAN_POINT('Ctrl Pts',(10.4372360809999,15.2,-1.18374385200001));
#188083=CARTESIAN_POINT('Ctrl Pts',(10.4372360809999,11.6,-1.18374385200001));
#188084=CARTESIAN_POINT('Ctrl Pts',(10.4389682809999,15.2,-1.18362871900001));
#188085=CARTESIAN_POINT('Ctrl Pts',(10.4389682809999,11.6,-1.18362871900001));
#188086=CARTESIAN_POINT('Ctrl Pts',(10.4407079299999,15.2,-1.18351147300002));
#188087=CARTESIAN_POINT('Ctrl Pts',(10.4407079299999,11.6,-1.18351147300002));
#188088=CARTESIAN_POINT('Ctrl Pts',(10.4424550129999,15.2,-1.18339210200002));
#188089=CARTESIAN_POINT('Ctrl Pts',(10.4424550129999,11.6,-1.18339210200002));
#188090=CARTESIAN_POINT('Ctrl Pts',(10.4442095079999,15.2,-1.18327059300002));
#188091=CARTESIAN_POINT('Ctrl Pts',(10.4442095079999,11.6,-1.18327059300002));
#188092=CARTESIAN_POINT('Ctrl Pts',(10.4459713999999,15.2,-1.18314693600002));
#188093=CARTESIAN_POINT('Ctrl Pts',(10.4459713999999,11.6,-1.18314693600002));
#188094=CARTESIAN_POINT('Ctrl Pts',(10.4477406689999,15.2,-1.18302111900002));
#188095=CARTESIAN_POINT('Ctrl Pts',(10.4477406689999,11.6,-1.18302111900002));
#188096=CARTESIAN_POINT('Ctrl Pts',(10.4495172989999,15.2,-1.18289313000002));
#188097=CARTESIAN_POINT('Ctrl Pts',(10.4495172989999,11.6,-1.18289313000002));
#188098=CARTESIAN_POINT('Ctrl Pts',(10.4513012699999,15.2,-1.18276295800001));
#188099=CARTESIAN_POINT('Ctrl Pts',(10.4513012699999,11.6,-1.18276295800001));
#188100=CARTESIAN_POINT('Ctrl Pts',(10.4530925649999,15.2,-1.18263059300002));
#188101=CARTESIAN_POINT('Ctrl Pts',(10.4530925649999,11.6,-1.18263059300002));
#188102=CARTESIAN_POINT('Ctrl Pts',(10.4548911669999,15.2,-1.18249602100001));
#188103=CARTESIAN_POINT('Ctrl Pts',(10.4548911669999,11.6,-1.18249602100002));
#188104=CARTESIAN_POINT('Ctrl Pts',(10.4566970559999,15.2,-1.18235923400002));
#188105=CARTESIAN_POINT('Ctrl Pts',(10.4566970559999,11.6,-1.18235923400002));
#188106=CARTESIAN_POINT('Ctrl Pts',(10.4585102169999,15.2,-1.18222021800001));
#188107=CARTESIAN_POINT('Ctrl Pts',(10.4585102169999,11.6,-1.18222021800001));
#188108=CARTESIAN_POINT('Ctrl Pts',(10.4603306309999,15.2,-1.18207896400001));
#188109=CARTESIAN_POINT('Ctrl Pts',(10.4603306309999,11.6,-1.18207896400001));
#188110=CARTESIAN_POINT('Ctrl Pts',(10.4621582789999,15.2,-1.18193546000001));
#188111=CARTESIAN_POINT('Ctrl Pts',(10.4621582789999,11.6,-1.18193546000001));
#188112=CARTESIAN_POINT('Ctrl Pts',(10.4639931469999,15.2,-1.18178969500002));
#188113=CARTESIAN_POINT('Ctrl Pts',(10.4639931469999,11.6,-1.18178969500002));
#188114=CARTESIAN_POINT('Ctrl Pts',(10.4658352139999,15.2,-1.18164165800001));
#188115=CARTESIAN_POINT('Ctrl Pts',(10.4658352139999,11.6,-1.18164165800001));
#188116=CARTESIAN_POINT('Ctrl Pts',(10.4676844649999,15.2,-1.18149133900001));
#188117=CARTESIAN_POINT('Ctrl Pts',(10.4676844649999,11.6,-1.18149133900001));
#188118=CARTESIAN_POINT('Ctrl Pts',(10.4695408809999,15.2,-1.18133872700001));
#188119=CARTESIAN_POINT('Ctrl Pts',(10.4695408809999,11.6,-1.18133872700001));
#188120=CARTESIAN_POINT('Ctrl Pts',(10.4714044449999,15.2,-1.18118380800002));
#188121=CARTESIAN_POINT('Ctrl Pts',(10.4714044449999,11.6,-1.18118380800002));
#188122=CARTESIAN_POINT('Ctrl Pts',(10.4732751399999,15.2,-1.18102657700002));
#188123=CARTESIAN_POINT('Ctrl Pts',(10.4732751399999,11.6,-1.18102657700002));
#188124=CARTESIAN_POINT('Ctrl Pts',(10.4751529499999,15.2,-1.18086701800001));
#188125=CARTESIAN_POINT('Ctrl Pts',(10.4751529499999,11.6,-1.18086701800001));
#188126=CARTESIAN_POINT('Ctrl Pts',(10.4770378569999,15.2,-1.18070512400001));
#188127=CARTESIAN_POINT('Ctrl Pts',(10.4770378569999,11.6,-1.18070512400001));
#188128=CARTESIAN_POINT('Ctrl Pts',(10.4789298419999,15.2,-1.18054088200001));
#188129=CARTESIAN_POINT('Ctrl Pts',(10.4789298419999,11.6,-1.18054088200001));
#188130=CARTESIAN_POINT('Ctrl Pts',(10.4808288909999,15.2,-1.18037428300001));
#188131=CARTESIAN_POINT('Ctrl Pts',(10.4808288909999,11.6,-1.18037428300001));
#188132=CARTESIAN_POINT('Ctrl Pts',(10.4827349849999,15.2,-1.18020531600001));
#188133=CARTESIAN_POINT('Ctrl Pts',(10.4827349849999,11.6,-1.18020531600001));
#188134=CARTESIAN_POINT('Ctrl Pts',(10.4846481079999,15.2,-1.18003397000002));
#188135=CARTESIAN_POINT('Ctrl Pts',(10.4846481079999,11.6,-1.18003397000002));
#188136=CARTESIAN_POINT('Ctrl Pts',(10.4865682419999,15.2,-1.17986023500002));
#188137=CARTESIAN_POINT('Ctrl Pts',(10.4865682419999,11.6,-1.17986023500002));
#188138=CARTESIAN_POINT('Ctrl Pts',(10.4884953719999,15.2,-1.17968410100001));
#188139=CARTESIAN_POINT('Ctrl Pts',(10.4884953719999,11.6,-1.17968410100001));
#188140=CARTESIAN_POINT('Ctrl Pts',(10.4904294789999,15.2,-1.17950555700002));
#188141=CARTESIAN_POINT('Ctrl Pts',(10.4904294789999,11.6,-1.17950555700002));
#188142=CARTESIAN_POINT('Ctrl Pts',(10.4923705489999,15.2,-1.17932459300001));
#188143=CARTESIAN_POINT('Ctrl Pts',(10.4923705489999,11.6,-1.17932459300001));
#188144=CARTESIAN_POINT('Ctrl Pts',(10.4943185629999,15.2,-1.17914119900002));
#188145=CARTESIAN_POINT('Ctrl Pts',(10.4943185629999,11.6,-1.17914119900002));
#188146=CARTESIAN_POINT('Ctrl Pts',(10.4962735059999,15.2,-1.17895536500002));
#188147=CARTESIAN_POINT('Ctrl Pts',(10.4962735059999,11.6,-1.17895536500002));
#188148=CARTESIAN_POINT('Ctrl Pts',(10.4982353589999,15.2,-1.17876708100002));
#188149=CARTESIAN_POINT('Ctrl Pts',(10.4982353589999,11.6,-1.17876708100002));
#188150=CARTESIAN_POINT('Ctrl Pts',(10.5002041069999,15.2,-1.17857633500002));
#188151=CARTESIAN_POINT('Ctrl Pts',(10.5002041069999,11.6,-1.17857633500002));
#188152=CARTESIAN_POINT('Ctrl Pts',(10.5021797349999,15.2,-1.17838311900002));
#188153=CARTESIAN_POINT('Ctrl Pts',(10.5021797349999,11.6,-1.17838311900002));
#188154=CARTESIAN_POINT('Ctrl Pts',(10.5041622239999,15.2,-1.17818742300001));
#188155=CARTESIAN_POINT('Ctrl Pts',(10.5041622239999,11.6,-1.17818742300001));
#188156=CARTESIAN_POINT('Ctrl Pts',(10.5061515589999,15.2,-1.17798923500001));
#188157=CARTESIAN_POINT('Ctrl Pts',(10.5061515589999,11.6,-1.17798923500001));
#188158=CARTESIAN_POINT('Ctrl Pts',(10.5081477229999,15.2,-1.17778854800001));
#188159=CARTESIAN_POINT('Ctrl Pts',(10.5081477229999,11.6,-1.17778854800001));
#188160=CARTESIAN_POINT('Ctrl Pts',(10.5101507009999,15.2,-1.17758535000001));
#188161=CARTESIAN_POINT('Ctrl Pts',(10.5101507009999,11.6,-1.17758535000001));
#188162=CARTESIAN_POINT('Ctrl Pts',(10.5121604749999,15.2,-1.17737963100002));
#188163=CARTESIAN_POINT('Ctrl Pts',(10.5121604749999,11.6,-1.17737963100002));
#188164=CARTESIAN_POINT('Ctrl Pts',(10.5141770299999,15.2,-1.17717138300002));
#188165=CARTESIAN_POINT('Ctrl Pts',(10.5141770299999,11.6,-1.17717138300002));
#188166=CARTESIAN_POINT('Ctrl Pts',(10.5162003509999,15.2,-1.17696059400001));
#188167=CARTESIAN_POINT('Ctrl Pts',(10.5162003509999,11.6,-1.17696059400001));
#188168=CARTESIAN_POINT('Ctrl Pts',(10.5182304179999,15.2,-1.17674725700001));
#188169=CARTESIAN_POINT('Ctrl Pts',(10.5182304179999,11.6,-1.17674725700002));
#188170=CARTESIAN_POINT('Ctrl Pts',(10.5202672189999,15.2,-1.17653135900001));
#188171=CARTESIAN_POINT('Ctrl Pts',(10.5202672189999,11.6,-1.17653135900001));
#188172=CARTESIAN_POINT('Ctrl Pts',(10.5223107349999,15.2,-1.17631289400002));
#188173=CARTESIAN_POINT('Ctrl Pts',(10.5223107349999,11.6,-1.17631289400002));
#188174=CARTESIAN_POINT('Ctrl Pts',(10.5243609529999,15.2,-1.17609185000001));
#188175=CARTESIAN_POINT('Ctrl Pts',(10.5243609529999,11.6,-1.17609185000001));
#188176=CARTESIAN_POINT('Ctrl Pts',(10.5264178549999,15.2,-1.17586821900002));
#188177=CARTESIAN_POINT('Ctrl Pts',(10.5264178549999,11.6,-1.17586821900002));
#188178=CARTESIAN_POINT('Ctrl Pts',(10.5284814249999,15.2,-1.17564198900002));
#188179=CARTESIAN_POINT('Ctrl Pts',(10.5284814249999,11.6,-1.17564198900002));
#188180=CARTESIAN_POINT('Ctrl Pts',(10.5305516489999,15.2,-1.17541315300001));
#188181=CARTESIAN_POINT('Ctrl Pts',(10.5305516489999,11.6,-1.17541315300001));
#188182=CARTESIAN_POINT('Ctrl Pts',(10.5326285089999,15.2,-1.17518170100002));
#188183=CARTESIAN_POINT('Ctrl Pts',(10.5326285089999,11.6,-1.17518170100002));
#188184=CARTESIAN_POINT('Ctrl Pts',(10.5347119909999,15.2,-1.17494762200002));
#188185=CARTESIAN_POINT('Ctrl Pts',(10.5347119909999,11.6,-1.17494762200002));
#188186=CARTESIAN_POINT('Ctrl Pts',(10.5368020779999,15.2,-1.17471091000001));
#188187=CARTESIAN_POINT('Ctrl Pts',(10.5368020779999,11.6,-1.17471091000001));
#188188=CARTESIAN_POINT('Ctrl Pts',(10.5388987559999,15.2,-1.17447155300002));
#188189=CARTESIAN_POINT('Ctrl Pts',(10.5388987559999,11.6,-1.17447155300002));
#188190=CARTESIAN_POINT('Ctrl Pts',(10.5410020069999,15.2,-1.17422954100002));
#188191=CARTESIAN_POINT('Ctrl Pts',(10.5410020069999,11.6,-1.17422954100002));
#188192=CARTESIAN_POINT('Ctrl Pts',(10.5431118179999,15.2,-1.17398486800001));
#188193=CARTESIAN_POINT('Ctrl Pts',(10.5431118179999,11.6,-1.17398486800001));
#188194=CARTESIAN_POINT('Ctrl Pts',(10.5452281719999,15.2,-1.17373752300002));
#188195=CARTESIAN_POINT('Ctrl Pts',(10.5452281719999,11.6,-1.17373752300002));
#188196=CARTESIAN_POINT('Ctrl Pts',(10.5473510539999,15.2,-1.17348749700001));
#188197=CARTESIAN_POINT('Ctrl Pts',(10.5473510539999,11.6,-1.17348749700001));
#188198=CARTESIAN_POINT('Ctrl Pts',(10.5494804499999,15.2,-1.17323478000001));
#188199=CARTESIAN_POINT('Ctrl Pts',(10.5494804499999,11.6,-1.17323478000001));
#188200=CARTESIAN_POINT('Ctrl Pts',(10.5516163409999,15.2,-1.17297936500002));
#188201=CARTESIAN_POINT('Ctrl Pts',(10.5516163409999,11.6,-1.17297936500002));
#188202=CARTESIAN_POINT('Ctrl Pts',(10.5537587149999,15.2,-1.17272124100001));
#188203=CARTESIAN_POINT('Ctrl Pts',(10.5537587149999,11.6,-1.17272124100001));
#188204=CARTESIAN_POINT('Ctrl Pts',(10.5559075549999,15.2,-1.17246040000001));
#188205=CARTESIAN_POINT('Ctrl Pts',(10.5559075549999,11.6,-1.17246040000001));
#188206=CARTESIAN_POINT('Ctrl Pts',(10.5580628449999,15.2,-1.17219683300001));
#188207=CARTESIAN_POINT('Ctrl Pts',(10.5580628449999,11.6,-1.17219683300001));
#188208=CARTESIAN_POINT('Ctrl Pts',(10.5602245729999,15.2,-1.17193053100001));
#188209=CARTESIAN_POINT('Ctrl Pts',(10.5602245729999,11.6,-1.17193053100001));
#188210=CARTESIAN_POINT('Ctrl Pts',(10.5623927209999,15.2,-1.17166148400001));
#188211=CARTESIAN_POINT('Ctrl Pts',(10.5623927209999,11.6,-1.17166148400001));
#188212=CARTESIAN_POINT('Ctrl Pts',(10.5645672749999,15.2,-1.17138968500001));
#188213=CARTESIAN_POINT('Ctrl Pts',(10.5645672749999,11.6,-1.17138968500001));
#188214=CARTESIAN_POINT('Ctrl Pts',(10.5667482189999,15.2,-1.17111512500002));
#188215=CARTESIAN_POINT('Ctrl Pts',(10.5667482189999,11.6,-1.17111512500002));
#188216=CARTESIAN_POINT('Ctrl Pts',(10.5689355399999,15.2,-1.17083779400001));
#188217=CARTESIAN_POINT('Ctrl Pts',(10.5689355399999,11.6,-1.17083779400002));
#188218=CARTESIAN_POINT('Ctrl Pts',(10.5711292199999,15.2,-1.17055768500002));
#188219=CARTESIAN_POINT('Ctrl Pts',(10.5711292199999,11.6,-1.17055768500002));
#188220=CARTESIAN_POINT('Ctrl Pts',(10.5733292469999,15.2,-1.17027478700001));
#188221=CARTESIAN_POINT('Ctrl Pts',(10.5733292469999,11.6,-1.17027478700001));
#188222=CARTESIAN_POINT('Ctrl Pts',(10.5755356029999,15.2,-1.16998909400001));
#188223=CARTESIAN_POINT('Ctrl Pts',(10.5755356029999,11.6,-1.16998909400001));
#188224=CARTESIAN_POINT('Ctrl Pts',(10.5777482769999,15.2,-1.16970059500002));
#188225=CARTESIAN_POINT('Ctrl Pts',(10.5777482769999,11.6,-1.16970059500002));
#188226=CARTESIAN_POINT('Ctrl Pts',(10.5799672509999,15.2,-1.16940928300002));
#188227=CARTESIAN_POINT('Ctrl Pts',(10.5799672509999,11.6,-1.16940928300002));
#188228=CARTESIAN_POINT('Ctrl Pts',(10.5821925109999,15.2,-1.16911515000002));
#188229=CARTESIAN_POINT('Ctrl Pts',(10.5821925109999,11.6,-1.16911515000002));
#188230=CARTESIAN_POINT('Ctrl Pts',(10.5844240429999,15.2,-1.16881818500001));
#188231=CARTESIAN_POINT('Ctrl Pts',(10.5844240429999,11.6,-1.16881818500001));
#188232=CARTESIAN_POINT('Ctrl Pts',(10.5866618309999,15.2,-1.16851838200001));
#188233=CARTESIAN_POINT('Ctrl Pts',(10.5866618309999,11.6,-1.16851838200001));
#188234=CARTESIAN_POINT('Ctrl Pts',(10.5889058619999,15.2,-1.16821573000002));
#188235=CARTESIAN_POINT('Ctrl Pts',(10.5889058619999,11.6,-1.16821573000002));
#188236=CARTESIAN_POINT('Ctrl Pts',(10.5911561199999,15.2,-1.16791022400001));
#188237=CARTESIAN_POINT('Ctrl Pts',(10.5911561199999,11.6,-1.16791022400002));
#188238=CARTESIAN_POINT('Ctrl Pts',(10.5934125899999,15.2,-1.16760185300001));
#188239=CARTESIAN_POINT('Ctrl Pts',(10.5934125899999,11.6,-1.16760185300001));
#188240=CARTESIAN_POINT('Ctrl Pts',(10.5956752579999,15.2,-1.16729060900001));
#188241=CARTESIAN_POINT('Ctrl Pts',(10.5956752579999,11.6,-1.16729060900001));
#188242=CARTESIAN_POINT('Ctrl Pts',(10.5979441109999,15.2,-1.16697648600002));
#188243=CARTESIAN_POINT('Ctrl Pts',(10.5979441109999,11.6,-1.16697648600002));
#188244=CARTESIAN_POINT('Ctrl Pts',(10.6002191329999,15.2,-1.16665947300001));
#188245=CARTESIAN_POINT('Ctrl Pts',(10.6002191329999,11.6,-1.16665947300001));
#188246=CARTESIAN_POINT('Ctrl Pts',(10.6025003099999,15.2,-1.16633956200001));
#188247=CARTESIAN_POINT('Ctrl Pts',(10.6025003099999,11.6,-1.16633956200001));
#188248=CARTESIAN_POINT('Ctrl Pts',(10.6047876269999,15.2,-1.16601674700001));
#188249=CARTESIAN_POINT('Ctrl Pts',(10.6047876269999,11.6,-1.16601674700001));
#188250=CARTESIAN_POINT('Ctrl Pts',(10.6070810689999,15.2,-1.16569101700001));
#188251=CARTESIAN_POINT('Ctrl Pts',(10.6070810689999,11.6,-1.16569101700001));
#188252=CARTESIAN_POINT('Ctrl Pts',(10.6093806239999,15.2,-1.16536236600002));
#188253=CARTESIAN_POINT('Ctrl Pts',(10.6093806239999,11.6,-1.16536236600002));
#188254=CARTESIAN_POINT('Ctrl Pts',(10.6116862759999,15.2,-1.16503078600001));
#188255=CARTESIAN_POINT('Ctrl Pts',(10.6116862759999,11.6,-1.16503078600001));
#188256=CARTESIAN_POINT('Ctrl Pts',(10.6139980099999,15.2,-1.16469626700002));
#188257=CARTESIAN_POINT('Ctrl Pts',(10.6139980099999,11.6,-1.16469626700002));
#188258=CARTESIAN_POINT('Ctrl Pts',(10.6163158139999,15.2,-1.16435880300001));
#188259=CARTESIAN_POINT('Ctrl Pts',(10.6163158139999,11.6,-1.16435880300001));
#188260=CARTESIAN_POINT('Ctrl Pts',(10.6186396719999,15.2,-1.16401838500002));
#188261=CARTESIAN_POINT('Ctrl Pts',(10.6186396719999,11.6,-1.16401838500002));
#188262=CARTESIAN_POINT('Ctrl Pts',(10.6209695709999,15.2,-1.16367500400001));
#188263=CARTESIAN_POINT('Ctrl Pts',(10.6209695709999,11.6,-1.16367500400001));
#188264=CARTESIAN_POINT('Ctrl Pts',(10.6233054959999,15.2,-1.16332865400001));
#188265=CARTESIAN_POINT('Ctrl Pts',(10.6233054959999,11.6,-1.16332865400001));
#188266=CARTESIAN_POINT('Ctrl Pts',(10.6256474329999,15.2,-1.16297932800002));
#188267=CARTESIAN_POINT('Ctrl Pts',(10.6256474329999,11.6,-1.16297932800002));
#188268=CARTESIAN_POINT('Ctrl Pts',(10.6279953679999,15.2,-1.16262701600002));
#188269=CARTESIAN_POINT('Ctrl Pts',(10.6279953679999,11.6,-1.16262701600002));
#188270=CARTESIAN_POINT('Ctrl Pts',(10.6303492879999,15.2,-1.16227170900002));
#188271=CARTESIAN_POINT('Ctrl Pts',(10.6303492879999,11.6,-1.16227170900002));
#188272=CARTESIAN_POINT('Ctrl Pts',(10.6327091779999,15.2,-1.16191340300002));
#188273=CARTESIAN_POINT('Ctrl Pts',(10.6327091779999,11.6,-1.16191340300002));
#188274=CARTESIAN_POINT('Ctrl Pts',(10.6350750239999,15.2,-1.16155208700001));
#188275=CARTESIAN_POINT('Ctrl Pts',(10.6350750239999,11.6,-1.16155208700001));
#188276=CARTESIAN_POINT('Ctrl Pts',(10.6374468119999,15.2,-1.16118775500002));
#188277=CARTESIAN_POINT('Ctrl Pts',(10.6374468119999,11.6,-1.16118775500002));
#188278=CARTESIAN_POINT('Ctrl Pts',(10.6398245289999,15.2,-1.16082039900002));
#188279=CARTESIAN_POINT('Ctrl Pts',(10.6398245289999,11.6,-1.16082039900002));
#188280=CARTESIAN_POINT('Ctrl Pts',(10.6422081599999,15.2,-1.16045001000002));
#188281=CARTESIAN_POINT('Ctrl Pts',(10.6422081599999,11.6,-1.16045001000002));
#188282=CARTESIAN_POINT('Ctrl Pts',(10.6445976929999,15.2,-1.16007658200001));
#188283=CARTESIAN_POINT('Ctrl Pts',(10.6445976929999,11.6,-1.16007658200001));
#188284=CARTESIAN_POINT('Ctrl Pts',(10.6469931119999,15.2,-1.15970010800002));
#188285=CARTESIAN_POINT('Ctrl Pts',(10.6469931119999,11.6,-1.15970010800002));
#188286=CARTESIAN_POINT('Ctrl Pts',(10.6493944039999,15.2,-1.15932057900002));
#188287=CARTESIAN_POINT('Ctrl Pts',(10.6493944039999,11.6,-1.15932057900002));
#188288=CARTESIAN_POINT('Ctrl Pts',(10.6518015559999,15.2,-1.15893798700001));
#188289=CARTESIAN_POINT('Ctrl Pts',(10.6518015559999,11.6,-1.15893798700002));
#188290=CARTESIAN_POINT('Ctrl Pts',(10.6542145539999,15.2,-1.15855232600001));
#188291=CARTESIAN_POINT('Ctrl Pts',(10.6542145539999,11.6,-1.15855232600001));
#188292=CARTESIAN_POINT('Ctrl Pts',(10.6566333849999,15.2,-1.15816358900001));
#188293=CARTESIAN_POINT('Ctrl Pts',(10.6566333849999,11.6,-1.15816358900001));
#188294=CARTESIAN_POINT('Ctrl Pts',(10.6590580339999,15.2,-1.15777176500002));
#188295=CARTESIAN_POINT('Ctrl Pts',(10.6590580339999,11.6,-1.15777176500002));
#188296=CARTESIAN_POINT('Ctrl Pts',(10.6614884869999,15.2,-1.15737685100001));
#188297=CARTESIAN_POINT('Ctrl Pts',(10.6614884869999,11.6,-1.15737685100001));
#188298=CARTESIAN_POINT('Ctrl Pts',(10.6639247329999,15.2,-1.15697883600001));
#188299=CARTESIAN_POINT('Ctrl Pts',(10.6639247329999,11.6,-1.15697883600001));
#188300=CARTESIAN_POINT('Ctrl Pts',(10.6663667569999,15.2,-1.15657771500001));
#188301=CARTESIAN_POINT('Ctrl Pts',(10.6663667569999,11.6,-1.15657771500001));
#188302=CARTESIAN_POINT('Ctrl Pts',(10.6688145439999,15.2,-1.15617348100002));
#188303=CARTESIAN_POINT('Ctrl Pts',(10.6688145439999,11.6,-1.15617348100002));
#188304=CARTESIAN_POINT('Ctrl Pts',(10.6712680829999,15.2,-1.15576612400002));
#188305=CARTESIAN_POINT('Ctrl Pts',(10.6712680829999,11.6,-1.15576612400002));
#188306=CARTESIAN_POINT('Ctrl Pts',(10.6737273609999,15.2,-1.15535563900002));
#188307=CARTESIAN_POINT('Ctrl Pts',(10.6737273609999,11.6,-1.15535563900002));
#188308=CARTESIAN_POINT('Ctrl Pts',(10.6761923619999,15.2,-1.15494201900002));
#188309=CARTESIAN_POINT('Ctrl Pts',(10.6761923619999,11.6,-1.15494201900002));
#188310=CARTESIAN_POINT('Ctrl Pts',(10.6786630739999,15.2,-1.15452525500002));
#188311=CARTESIAN_POINT('Ctrl Pts',(10.6786630739999,11.6,-1.15452525500002));
#188312=CARTESIAN_POINT('Ctrl Pts',(10.6811394829999,15.2,-1.15410534100001));
#188313=CARTESIAN_POINT('Ctrl Pts',(10.6811394829999,11.6,-1.15410534100001));
#188314=CARTESIAN_POINT('Ctrl Pts',(10.6836215769999,15.2,-1.15368227000001));
#188315=CARTESIAN_POINT('Ctrl Pts',(10.6836215769999,11.6,-1.15368227000001));
#188316=CARTESIAN_POINT('Ctrl Pts',(10.6861093419999,15.2,-1.15325603400001));
#188317=CARTESIAN_POINT('Ctrl Pts',(10.6861093419999,11.6,-1.15325603400001));
#188318=CARTESIAN_POINT('Ctrl Pts',(10.6886027649999,15.2,-1.15282662600002));
#188319=CARTESIAN_POINT('Ctrl Pts',(10.6886027649999,11.6,-1.15282662600002));
#188320=CARTESIAN_POINT('Ctrl Pts',(10.6911018329999,15.2,-1.15239404100001));
#188321=CARTESIAN_POINT('Ctrl Pts',(10.6911018329999,11.6,-1.15239404100001));
#188322=CARTESIAN_POINT('Ctrl Pts',(10.6936065319999,15.2,-1.15195826900001));
#188323=CARTESIAN_POINT('Ctrl Pts',(10.6936065319999,11.6,-1.15195826900001));
#188324=CARTESIAN_POINT('Ctrl Pts',(10.6961168509999,15.2,-1.15151930500001));
#188325=CARTESIAN_POINT('Ctrl Pts',(10.6961168509999,11.6,-1.15151930500002));
#188326=CARTESIAN_POINT('Ctrl Pts',(10.6986327729999,15.2,-1.15107714100001));
#188327=CARTESIAN_POINT('Ctrl Pts',(10.6986327729999,11.6,-1.15107714100001));
#188328=CARTESIAN_POINT('Ctrl Pts',(10.7011542889999,15.2,-1.15063177000001));
#188329=CARTESIAN_POINT('Ctrl Pts',(10.7011542889999,11.6,-1.15063177000002));
#188330=CARTESIAN_POINT('Ctrl Pts',(10.7036813819999,15.2,-1.15018318700002));
#188331=CARTESIAN_POINT('Ctrl Pts',(10.7036813819999,11.6,-1.15018318700002));
#188332=CARTESIAN_POINT('Ctrl Pts',(10.7062140429999,15.2,-1.14973138100002));
#188333=CARTESIAN_POINT('Ctrl Pts',(10.7062140429999,11.6,-1.14973138100002));
#188334=CARTESIAN_POINT('Ctrl Pts',(10.7087522569999,15.2,-1.14927635000001));
#188335=CARTESIAN_POINT('Ctrl Pts',(10.7087522569999,11.6,-1.14927635000001));
#188336=CARTESIAN_POINT('Ctrl Pts',(10.7112960109999,15.2,-1.14881808400002));
#188337=CARTESIAN_POINT('Ctrl Pts',(10.7112960109999,11.6,-1.14881808400002));
#188338=CARTESIAN_POINT('Ctrl Pts',(10.7138452919999,15.2,-1.14835657800001));
#188339=CARTESIAN_POINT('Ctrl Pts',(10.7138452919999,11.6,-1.14835657800001));
#188340=CARTESIAN_POINT('Ctrl Pts',(10.7164000879999,15.2,-1.14789182400001));
#188341=CARTESIAN_POINT('Ctrl Pts',(10.7164000879999,11.6,-1.14789182400001));
#188342=CARTESIAN_POINT('Ctrl Pts',(10.7189603849999,15.2,-1.14742381500001));
#188343=CARTESIAN_POINT('Ctrl Pts',(10.7189603849999,11.6,-1.14742381500002));
#188344=CARTESIAN_POINT('Ctrl Pts',(10.7215261719999,15.2,-1.14695254600001));
#188345=CARTESIAN_POINT('Ctrl Pts',(10.7215261719999,11.6,-1.14695254600001));
#188346=CARTESIAN_POINT('Ctrl Pts',(10.7240974329999,15.2,-1.14647800800002));
#188347=CARTESIAN_POINT('Ctrl Pts',(10.7240974329999,11.6,-1.14647800800002));
#188348=CARTESIAN_POINT('Ctrl Pts',(10.7266741579999,15.2,-1.14600019600001));
#188349=CARTESIAN_POINT('Ctrl Pts',(10.7266741579999,11.6,-1.14600019600001));
#188350=CARTESIAN_POINT('Ctrl Pts',(10.7292563339999,15.2,-1.14551910300001));
#188351=CARTESIAN_POINT('Ctrl Pts',(10.7292563339999,11.6,-1.14551910300001));
#188352=CARTESIAN_POINT('Ctrl Pts',(10.7318439469999,15.2,-1.14503472200001));
#188353=CARTESIAN_POINT('Ctrl Pts',(10.7318439469999,11.6,-1.14503472200001));
#188354=CARTESIAN_POINT('Ctrl Pts',(10.7344369859999,15.2,-1.14454704700002));
#188355=CARTESIAN_POINT('Ctrl Pts',(10.7344369859999,11.6,-1.14454704700002));
#188356=CARTESIAN_POINT('Ctrl Pts',(10.7370354359999,15.2,-1.14405607000001));
#188357=CARTESIAN_POINT('Ctrl Pts',(10.7370354359999,11.6,-1.14405607000002));
#188358=CARTESIAN_POINT('Ctrl Pts',(10.7396392859999,15.2,-1.14356178700001));
#188359=CARTESIAN_POINT('Ctrl Pts',(10.7396392859999,11.6,-1.14356178700001));
#188360=CARTESIAN_POINT('Ctrl Pts',(10.7422485239999,15.2,-1.14306418900001));
#188361=CARTESIAN_POINT('Ctrl Pts',(10.7422485239999,11.6,-1.14306418900001));
#188362=CARTESIAN_POINT('Ctrl Pts',(10.7448631359999,15.2,-1.14256327100001));
#188363=CARTESIAN_POINT('Ctrl Pts',(10.7448631359999,11.6,-1.14256327100001));
#188364=CARTESIAN_POINT('Ctrl Pts',(10.7474831099999,15.2,-1.14205902600002));
#188365=CARTESIAN_POINT('Ctrl Pts',(10.7474831099999,11.6,-1.14205902600002));
#188366=CARTESIAN_POINT('Ctrl Pts',(10.7501084329999,15.2,-1.14155144700002));
#188367=CARTESIAN_POINT('Ctrl Pts',(10.7501084329999,11.6,-1.14155144700002));
#188368=CARTESIAN_POINT('Ctrl Pts',(10.7527390939999,15.2,-1.14104053000001));
#188369=CARTESIAN_POINT('Ctrl Pts',(10.7527390939999,11.6,-1.14104053000002));
#188370=CARTESIAN_POINT('Ctrl Pts',(10.7553750779999,15.2,-1.14052626500001));
#188371=CARTESIAN_POINT('Ctrl Pts',(10.7553750779999,11.6,-1.14052626500001));
#188372=CARTESIAN_POINT('Ctrl Pts',(10.7580163749999,15.2,-1.14000864800001));
#188373=CARTESIAN_POINT('Ctrl Pts',(10.7580163749999,11.6,-1.14000864800001));
#188374=CARTESIAN_POINT('Ctrl Pts',(10.7606629729999,15.2,-1.13948767300001));
#188375=CARTESIAN_POINT('Ctrl Pts',(10.7606629729999,11.6,-1.13948767300002));
#188376=CARTESIAN_POINT('Ctrl Pts',(10.7633148559999,15.2,-1.13896333100001));
#188377=CARTESIAN_POINT('Ctrl Pts',(10.7633148559999,11.6,-1.13896333100001));
#188378=CARTESIAN_POINT('Ctrl Pts',(10.7659720149999,15.2,-1.13843562000001));
#188379=CARTESIAN_POINT('Ctrl Pts',(10.7659720149999,11.6,-1.13843562000001));
#188380=CARTESIAN_POINT('Ctrl Pts',(10.7686344369999,15.2,-1.13790452900002));
#188381=CARTESIAN_POINT('Ctrl Pts',(10.7686344369999,11.6,-1.13790452900002));
#188382=CARTESIAN_POINT('Ctrl Pts',(10.7713021079999,15.2,-1.13737005600001));
#188383=CARTESIAN_POINT('Ctrl Pts',(10.7713021079999,11.6,-1.13737005600001));
#188384=CARTESIAN_POINT('Ctrl Pts',(10.7739750179999,15.2,-1.13683219200002));
#188385=CARTESIAN_POINT('Ctrl Pts',(10.7739750179999,11.6,-1.13683219200002));
#188386=CARTESIAN_POINT('Ctrl Pts',(10.7766531539999,15.2,-1.13629093100001));
#188387=CARTESIAN_POINT('Ctrl Pts',(10.7766531539999,11.6,-1.13629093100002));
#188388=CARTESIAN_POINT('Ctrl Pts',(10.7793365029999,15.2,-1.13574626900002));
#188389=CARTESIAN_POINT('Ctrl Pts',(10.7793365029999,11.6,-1.13574626900002));
#188390=CARTESIAN_POINT('Ctrl Pts',(10.7820250529999,15.2,-1.13519819700001));
#188391=CARTESIAN_POINT('Ctrl Pts',(10.7820250529999,11.6,-1.13519819700001));
#188392=CARTESIAN_POINT('Ctrl Pts',(10.7847187929999,15.2,-1.13464671100001));
#188393=CARTESIAN_POINT('Ctrl Pts',(10.7847187929999,11.6,-1.13464671100001));
#188394=CARTESIAN_POINT('Ctrl Pts',(10.7874177099999,15.2,-1.13409180400001));
#188395=CARTESIAN_POINT('Ctrl Pts',(10.7874177099999,11.6,-1.13409180400002));
#188396=CARTESIAN_POINT('Ctrl Pts',(10.7901217899999,15.2,-1.13353347000002));
#188397=CARTESIAN_POINT('Ctrl Pts',(10.7901217899999,11.6,-1.13353347000002));
#188398=CARTESIAN_POINT('Ctrl Pts',(10.7928310259999,15.2,-1.13297170300001));
#188399=CARTESIAN_POINT('Ctrl Pts',(10.7928310259999,11.6,-1.13297170300001));
#188400=CARTESIAN_POINT('Ctrl Pts',(10.7955453999999,15.2,-1.13240649900002));
#188401=CARTESIAN_POINT('Ctrl Pts',(10.7955453999999,11.6,-1.13240649900002));
#188402=CARTESIAN_POINT('Ctrl Pts',(10.7982649039999,15.2,-1.13183784800002));
#188403=CARTESIAN_POINT('Ctrl Pts',(10.7982649039999,11.6,-1.13183784800002));
#188404=CARTESIAN_POINT('Ctrl Pts',(10.8009895249999,15.2,-1.13126574700001));
#188405=CARTESIAN_POINT('Ctrl Pts',(10.8009895249999,11.6,-1.13126574700001));
#188406=CARTESIAN_POINT('Ctrl Pts',(10.8037192499999,15.2,-1.13069018800001));
#188407=CARTESIAN_POINT('Ctrl Pts',(10.8037192499999,11.6,-1.13069018800001));
#188408=CARTESIAN_POINT('Ctrl Pts',(10.8064540679999,15.2,-1.13011116700001));
#188409=CARTESIAN_POINT('Ctrl Pts',(10.8064540679999,11.6,-1.13011116700001));
#188410=CARTESIAN_POINT('Ctrl Pts',(10.8091939669999,15.2,-1.12952867800002));
#188411=CARTESIAN_POINT('Ctrl Pts',(10.8091939669999,11.6,-1.12952867800002));
#188412=CARTESIAN_POINT('Ctrl Pts',(10.8119389339999,15.2,-1.12894271400001));
#188413=CARTESIAN_POINT('Ctrl Pts',(10.8119389339999,11.6,-1.12894271400001));
#188414=CARTESIAN_POINT('Ctrl Pts',(10.8146889589999,15.2,-1.12835326900001));
#188415=CARTESIAN_POINT('Ctrl Pts',(10.8146889589999,11.6,-1.12835326900001));
#188416=CARTESIAN_POINT('Ctrl Pts',(10.8174440279999,15.2,-1.12776033900001));
#188417=CARTESIAN_POINT('Ctrl Pts',(10.8174440279999,11.6,-1.12776033900001));
#188418=CARTESIAN_POINT('Ctrl Pts',(10.8202041309999,15.2,-1.12716391700001));
#188419=CARTESIAN_POINT('Ctrl Pts',(10.8202041309999,11.6,-1.12716391700001));
#188420=CARTESIAN_POINT('Ctrl Pts',(10.8229692549999,15.2,-1.12656399600001));
#188421=CARTESIAN_POINT('Ctrl Pts',(10.8229692549999,11.6,-1.12656399600001));
#188422=CARTESIAN_POINT('Ctrl Pts',(10.8257393889999,15.2,-1.12596057200001));
#188423=CARTESIAN_POINT('Ctrl Pts',(10.8257393889999,11.6,-1.12596057200001));
#188424=CARTESIAN_POINT('Ctrl Pts',(10.8285145199999,15.2,-1.12535363900002));
#188425=CARTESIAN_POINT('Ctrl Pts',(10.8285145199999,11.6,-1.12535363900002));
#188426=CARTESIAN_POINT('Ctrl Pts',(10.8312946379999,15.2,-1.12474319100001));
#188427=CARTESIAN_POINT('Ctrl Pts',(10.8312946379999,11.6,-1.12474319100001));
#188428=CARTESIAN_POINT('Ctrl Pts',(10.8340797309999,15.2,-1.12412922200001));
#188429=CARTESIAN_POINT('Ctrl Pts',(10.8340797309999,11.6,-1.12412922200001));
#188430=CARTESIAN_POINT('Ctrl Pts',(10.8368697859999,15.2,-1.12351172700001));
#188431=CARTESIAN_POINT('Ctrl Pts',(10.8368697859999,11.6,-1.12351172700001));
#188432=CARTESIAN_POINT('Ctrl Pts',(10.8396647919999,15.2,-1.12289070000001));
#188433=CARTESIAN_POINT('Ctrl Pts',(10.8396647919999,11.6,-1.12289070000001));
#188434=CARTESIAN_POINT('Ctrl Pts',(10.8424647369999,15.2,-1.12226613600001));
#188435=CARTESIAN_POINT('Ctrl Pts',(10.8424647369999,11.6,-1.12226613600001));
#188436=CARTESIAN_POINT('Ctrl Pts',(10.8452696099999,15.2,-1.12163802800001));
#188437=CARTESIAN_POINT('Ctrl Pts',(10.8452696099999,11.6,-1.12163802800001));
#188438=CARTESIAN_POINT('Ctrl Pts',(10.8480793999999,15.2,-1.12100637100002));
#188439=CARTESIAN_POINT('Ctrl Pts',(10.8480793999999,11.6,-1.12100637100002));
#188440=CARTESIAN_POINT('Ctrl Pts',(10.8508940929999,15.2,-1.12037116000002));
#188441=CARTESIAN_POINT('Ctrl Pts',(10.8508940929999,11.6,-1.12037116000002));
#188442=CARTESIAN_POINT('Ctrl Pts',(10.8537136799999,15.2,-1.11973239000001));
#188443=CARTESIAN_POINT('Ctrl Pts',(10.8537136799999,11.6,-1.11973239000001));
#188444=CARTESIAN_POINT('Ctrl Pts',(10.8565381479999,15.2,-1.11909005300001));
#188445=CARTESIAN_POINT('Ctrl Pts',(10.8565381479999,11.6,-1.11909005300001));
#188446=CARTESIAN_POINT('Ctrl Pts',(10.8593674859999,15.2,-1.11844414700002));
#188447=CARTESIAN_POINT('Ctrl Pts',(10.8593674859999,11.6,-1.11844414700002));
#188448=CARTESIAN_POINT('Ctrl Pts',(10.8622016829999,15.2,-1.11779466300002));
#188449=CARTESIAN_POINT('Ctrl Pts',(10.8622016829999,11.6,-1.11779466300002));
#188450=CARTESIAN_POINT('Ctrl Pts',(10.8650407269999,15.2,-1.11714159800002));
#188451=CARTESIAN_POINT('Ctrl Pts',(10.8650407269999,11.6,-1.11714159800002));
#188452=CARTESIAN_POINT('Ctrl Pts',(10.8678846049999,15.2,-1.11648494500002));
#188453=CARTESIAN_POINT('Ctrl Pts',(10.8678846049999,11.6,-1.11648494500002));
#188454=CARTESIAN_POINT('Ctrl Pts',(10.8707333089999,15.2,-1.11582470100001));
#188455=CARTESIAN_POINT('Ctrl Pts',(10.8707333089999,11.6,-1.11582470100001));
#188456=CARTESIAN_POINT('Ctrl Pts',(10.8735868239999,15.2,-1.11516085700002));
#188457=CARTESIAN_POINT('Ctrl Pts',(10.8735868239999,11.6,-1.11516085700002));
#188458=CARTESIAN_POINT('Ctrl Pts',(10.8764451419999,15.2,-1.11449341100001));
#188459=CARTESIAN_POINT('Ctrl Pts',(10.8764451419999,11.6,-1.11449341100002));
#188460=CARTESIAN_POINT('Ctrl Pts',(10.8793082489999,15.2,-1.11382235600002));
#188461=CARTESIAN_POINT('Ctrl Pts',(10.8793082489999,11.6,-1.11382235600002));
#188462=CARTESIAN_POINT('Ctrl Pts',(10.8821761349999,15.2,-1.11314768700002));
#188463=CARTESIAN_POINT('Ctrl Pts',(10.8821761349999,11.6,-1.11314768700002));
#188464=CARTESIAN_POINT('Ctrl Pts',(10.8850487879999,15.2,-1.11246939900001));
#188465=CARTESIAN_POINT('Ctrl Pts',(10.8850487879999,11.6,-1.11246939900001));
#188466=CARTESIAN_POINT('Ctrl Pts',(10.8879261969999,15.2,-1.11178748600001));
#188467=CARTESIAN_POINT('Ctrl Pts',(10.8879261969999,11.6,-1.11178748600001));
#188468=CARTESIAN_POINT('Ctrl Pts',(10.8908083519999,15.2,-1.11110194200001));
#188469=CARTESIAN_POINT('Ctrl Pts',(10.8908083519999,11.6,-1.11110194200001));
#188470=CARTESIAN_POINT('Ctrl Pts',(10.8936952389999,15.2,-1.11041276400002));
#188471=CARTESIAN_POINT('Ctrl Pts',(10.8936952389999,11.6,-1.11041276400002));
#188472=CARTESIAN_POINT('Ctrl Pts',(10.8965868489999,15.2,-1.10971994600002));
#188473=CARTESIAN_POINT('Ctrl Pts',(10.8965868489999,11.6,-1.10971994600002));
#188474=CARTESIAN_POINT('Ctrl Pts',(10.8994831699999,15.2,-1.10902348200002));
#188475=CARTESIAN_POINT('Ctrl Pts',(10.8994831699999,11.6,-1.10902348200002));
#188476=CARTESIAN_POINT('Ctrl Pts',(10.9023841919999,15.2,-1.10832336700001));
#188477=CARTESIAN_POINT('Ctrl Pts',(10.9023841919999,11.6,-1.10832336700002));
#188478=CARTESIAN_POINT('Ctrl Pts',(10.9052899019999,15.2,-1.10761959600001));
#188479=CARTESIAN_POINT('Ctrl Pts',(10.9052899019999,11.6,-1.10761959600001));
#188480=CARTESIAN_POINT('Ctrl Pts',(10.9082002889999,15.2,-1.10691216500001));
#188481=CARTESIAN_POINT('Ctrl Pts',(10.9082002889999,11.6,-1.10691216500001));
#188482=CARTESIAN_POINT('Ctrl Pts',(10.9111153429999,15.2,-1.10620106900001));
#188483=CARTESIAN_POINT('Ctrl Pts',(10.9111153429999,11.6,-1.10620106900001));
#188484=CARTESIAN_POINT('Ctrl Pts',(10.9140350519999,15.2,-1.10548629900002));
#188485=CARTESIAN_POINT('Ctrl Pts',(10.9140350519999,11.6,-1.10548629900002));
#188486=CARTESIAN_POINT('Ctrl Pts',(10.9169594059999,15.2,-1.10476785400001));
#188487=CARTESIAN_POINT('Ctrl Pts',(10.9169594059999,11.6,-1.10476785400001));
#188488=CARTESIAN_POINT('Ctrl Pts',(10.9198883929999,15.2,-1.10404572800002));
#188489=CARTESIAN_POINT('Ctrl Pts',(10.9198883929999,11.6,-1.10404572800002));
#188490=CARTESIAN_POINT('Ctrl Pts',(10.9228220029999,15.2,-1.10331991500002));
#188491=CARTESIAN_POINT('Ctrl Pts',(10.9228220029999,11.6,-1.10331991500002));
#188492=CARTESIAN_POINT('Ctrl Pts',(10.9257602229999,15.2,-1.10259041100001));
#188493=CARTESIAN_POINT('Ctrl Pts',(10.9257602229999,11.6,-1.10259041100001));
#188494=CARTESIAN_POINT('Ctrl Pts',(10.9287030449999,15.2,-1.10185721000001));
#188495=CARTESIAN_POINT('Ctrl Pts',(10.9287030449999,11.6,-1.10185721000002));
#188496=CARTESIAN_POINT('Ctrl Pts',(10.9316504549999,15.2,-1.10112030800002));
#188497=CARTESIAN_POINT('Ctrl Pts',(10.9316504549999,11.6,-1.10112030800002));
#188498=CARTESIAN_POINT('Ctrl Pts',(10.9346024439999,15.2,-1.10037969900001));
#188499=CARTESIAN_POINT('Ctrl Pts',(10.9346024439999,11.6,-1.10037969900001));
#188500=CARTESIAN_POINT('Ctrl Pts',(10.9375589989999,15.2,-1.09963538000001));
#188501=CARTESIAN_POINT('Ctrl Pts',(10.9375589989999,11.6,-1.09963538000002));
#188502=CARTESIAN_POINT('Ctrl Pts',(10.9405201119999,15.2,-1.09888734500001));
#188503=CARTESIAN_POINT('Ctrl Pts',(10.9405201119999,11.6,-1.09888734500002));
#188504=CARTESIAN_POINT('Ctrl Pts',(10.9434857709999,15.2,-1.09813558700001));
#188505=CARTESIAN_POINT('Ctrl Pts',(10.9434857709999,11.6,-1.09813558700001));
#188506=CARTESIAN_POINT('Ctrl Pts',(10.9464559649999,15.2,-1.09738010500001));
#188507=CARTESIAN_POINT('Ctrl Pts',(10.9464559649999,11.6,-1.09738010500001));
#188508=CARTESIAN_POINT('Ctrl Pts',(10.9494306809999,15.2,-1.09662089000001));
#188509=CARTESIAN_POINT('Ctrl Pts',(10.9494306809999,11.6,-1.09662089000001));
#188510=CARTESIAN_POINT('Ctrl Pts',(10.9524099109999,15.2,-1.09585794100001));
#188511=CARTESIAN_POINT('Ctrl Pts',(10.9524099109999,11.6,-1.09585794100001));
#188512=CARTESIAN_POINT('Ctrl Pts',(10.9553936439999,15.2,-1.09509125200002));
#188513=CARTESIAN_POINT('Ctrl Pts',(10.9553936439999,11.6,-1.09509125200002));
#188514=CARTESIAN_POINT('Ctrl Pts',(10.9583818679999,15.2,-1.09432081700001));
#188515=CARTESIAN_POINT('Ctrl Pts',(10.9583818679999,11.6,-1.09432081700001));
#188516=CARTESIAN_POINT('Ctrl Pts',(10.9613745729999,15.2,-1.09354663200001));
#188517=CARTESIAN_POINT('Ctrl Pts',(10.9613745729999,11.6,-1.09354663200001));
#188518=CARTESIAN_POINT('Ctrl Pts',(10.9643717479999,15.2,-1.09276869100002));
#188519=CARTESIAN_POINT('Ctrl Pts',(10.9643717479999,11.6,-1.09276869100002));
#188520=CARTESIAN_POINT('Ctrl Pts',(10.9673733819999,15.2,-1.09198699100002));
#188521=CARTESIAN_POINT('Ctrl Pts',(10.9673733819999,11.6,-1.09198699100002));
#188522=CARTESIAN_POINT('Ctrl Pts',(10.9703794639999,15.2,-1.09120152700001));
#188523=CARTESIAN_POINT('Ctrl Pts',(10.9703794639999,11.6,-1.09120152700001));
#188524=CARTESIAN_POINT('Ctrl Pts',(10.9733899849999,15.2,-1.09041229500002));
#188525=CARTESIAN_POINT('Ctrl Pts',(10.9733899849999,11.6,-1.09041229500002));
#188526=CARTESIAN_POINT('Ctrl Pts',(10.9764049329999,15.2,-1.08961928800001));
#188527=CARTESIAN_POINT('Ctrl Pts',(10.9764049329999,11.6,-1.08961928800001));
#188528=CARTESIAN_POINT('Ctrl Pts',(10.9794242969999,15.2,-1.08882250200002));
#188529=CARTESIAN_POINT('Ctrl Pts',(10.9794242969999,11.6,-1.08882250200002));
#188530=CARTESIAN_POINT('Ctrl Pts',(10.9824480679999,15.2,-1.08802193400001));
#188531=CARTESIAN_POINT('Ctrl Pts',(10.9824480679999,11.6,-1.08802193400001));
#188532=CARTESIAN_POINT('Ctrl Pts',(10.9854762329999,15.2,-1.08721757800001));
#188533=CARTESIAN_POINT('Ctrl Pts',(10.9854762329999,11.6,-1.08721757800002));
#188534=CARTESIAN_POINT('Ctrl Pts',(10.9885087839999,15.2,-1.08640943000001));
#188535=CARTESIAN_POINT('Ctrl Pts',(10.9885087839999,11.6,-1.08640943000002));
#188536=CARTESIAN_POINT('Ctrl Pts',(10.9915457079999,15.2,-1.08559748400001));
#188537=CARTESIAN_POINT('Ctrl Pts',(10.9915457079999,11.6,-1.08559748400001));
#188538=CARTESIAN_POINT('Ctrl Pts',(10.9945869969999,15.2,-1.08478173800002));
#188539=CARTESIAN_POINT('Ctrl Pts',(10.9945869969999,11.6,-1.08478173800002));
#188540=CARTESIAN_POINT('Ctrl Pts',(10.9976326369999,15.2,-1.08396218400001));
#188541=CARTESIAN_POINT('Ctrl Pts',(10.9976326369999,11.6,-1.08396218400001));
#188542=CARTESIAN_POINT('Ctrl Pts',(11.0006826209999,15.2,-1.08313882100001));
#188543=CARTESIAN_POINT('Ctrl Pts',(11.0006826209999,11.6,-1.08313882100001));
#188544=CARTESIAN_POINT('Ctrl Pts',(11.0037369369999,15.2,-1.08231164300001));
#188545=CARTESIAN_POINT('Ctrl Pts',(11.0037369369999,11.6,-1.08231164300001));
#188546=CARTESIAN_POINT('Ctrl Pts',(11.0067955739999,15.2,-1.08148064400002));
#188547=CARTESIAN_POINT('Ctrl Pts',(11.0067955739999,11.6,-1.08148064400002));
#188548=CARTESIAN_POINT('Ctrl Pts',(11.0098585239999,15.2,-1.08064582200001));
#188549=CARTESIAN_POINT('Ctrl Pts',(11.0098585239999,11.6,-1.08064582200001));
#188550=CARTESIAN_POINT('Ctrl Pts',(11.0129257729999,15.2,-1.07980717100002));
#188551=CARTESIAN_POINT('Ctrl Pts',(11.0129257729999,11.6,-1.07980717100002));
#188552=CARTESIAN_POINT('Ctrl Pts',(11.0159973129999,15.2,-1.07896468600002));
#188553=CARTESIAN_POINT('Ctrl Pts',(11.0159973129999,11.6,-1.07896468600002));
#188554=CARTESIAN_POINT('Ctrl Pts',(11.0190731309999,15.2,-1.07811836400002));
#188555=CARTESIAN_POINT('Ctrl Pts',(11.0190731309999,11.6,-1.07811836400002));
#188556=CARTESIAN_POINT('Ctrl Pts',(11.0221532199999,15.2,-1.07726820000002));
#188557=CARTESIAN_POINT('Ctrl Pts',(11.0221532199999,11.6,-1.07726820000002));
#188558=CARTESIAN_POINT('Ctrl Pts',(11.0252375679999,15.2,-1.07641419000001));
#188559=CARTESIAN_POINT('Ctrl Pts',(11.0252375679999,11.6,-1.07641419000002));
#188560=CARTESIAN_POINT('Ctrl Pts',(11.0283261659999,15.2,-1.07555632900001));
#188561=CARTESIAN_POINT('Ctrl Pts',(11.0283261659999,11.6,-1.07555632900001));
#188562=CARTESIAN_POINT('Ctrl Pts',(11.0314190009999,15.2,-1.07469461300001));
#188563=CARTESIAN_POINT('Ctrl Pts',(11.0314190009999,11.6,-1.07469461300001));
#188564=CARTESIAN_POINT('Ctrl Pts',(11.0345160639999,15.2,-1.07382903800001));
#188565=CARTESIAN_POINT('Ctrl Pts',(11.0345160639999,11.6,-1.07382903800001));
#188566=CARTESIAN_POINT('Ctrl Pts',(11.0376173449999,15.2,-1.07295959800001));
#188567=CARTESIAN_POINT('Ctrl Pts',(11.0376173449999,11.6,-1.07295959800001));
#188568=CARTESIAN_POINT('Ctrl Pts',(11.0407228349999,15.2,-1.07208629100001));
#188569=CARTESIAN_POINT('Ctrl Pts',(11.0407228349999,11.6,-1.07208629100001));
#188570=CARTESIAN_POINT('Ctrl Pts',(11.0438325199999,15.2,-1.07120911000001));
#188571=CARTESIAN_POINT('Ctrl Pts',(11.0438325199999,11.6,-1.07120911000001));
#188572=CARTESIAN_POINT('Ctrl Pts',(11.0469463939999,15.2,-1.07032805400001));
#188573=CARTESIAN_POINT('Ctrl Pts',(11.0469463939999,11.6,-1.07032805400001));
#188574=CARTESIAN_POINT('Ctrl Pts',(11.0500644439999,15.2,-1.06944311600001));
#188575=CARTESIAN_POINT('Ctrl Pts',(11.0500644439999,11.6,-1.06944311600001));
#188576=CARTESIAN_POINT('Ctrl Pts',(11.0531866599999,15.2,-1.06855429300001));
#188577=CARTESIAN_POINT('Ctrl Pts',(11.0531866599999,11.6,-1.06855429300001));
#188578=CARTESIAN_POINT('Ctrl Pts',(11.0563130319999,15.2,-1.06766158000001));
#188579=CARTESIAN_POINT('Ctrl Pts',(11.0563130319999,11.6,-1.06766158000001));
#188580=CARTESIAN_POINT('Ctrl Pts',(11.0594435509999,15.2,-1.06676497400001));
#188581=CARTESIAN_POINT('Ctrl Pts',(11.0594435509999,11.6,-1.06676497400001));
#188582=CARTESIAN_POINT('Ctrl Pts',(11.0625782069999,15.2,-1.06586447000002));
#188583=CARTESIAN_POINT('Ctrl Pts',(11.0625782069999,11.6,-1.06586447000002));
#188584=CARTESIAN_POINT('Ctrl Pts',(11.0657169879999,15.2,-1.06496006400001));
#188585=CARTESIAN_POINT('Ctrl Pts',(11.0657169879999,11.6,-1.06496006400001));
#188586=CARTESIAN_POINT('Ctrl Pts',(11.0688598849999,15.2,-1.06405175100001));
#188587=CARTESIAN_POINT('Ctrl Pts',(11.0688598849999,11.6,-1.06405175100001));
#188588=CARTESIAN_POINT('Ctrl Pts',(11.0720068879999,15.2,-1.06313952900001));
#188589=CARTESIAN_POINT('Ctrl Pts',(11.0720068879999,11.6,-1.06313952900001));
#188590=CARTESIAN_POINT('Ctrl Pts',(11.0751579869999,15.2,-1.06222339000002));
#188591=CARTESIAN_POINT('Ctrl Pts',(11.0751579869999,11.6,-1.06222339000002));
#188592=CARTESIAN_POINT('Ctrl Pts',(11.0783131709999,15.2,-1.06130333400001));
#188593=CARTESIAN_POINT('Ctrl Pts',(11.0783131709999,11.6,-1.06130333400001));
#188594=CARTESIAN_POINT('Ctrl Pts',(11.0814724299999,15.2,-1.06037935500002));
#188595=CARTESIAN_POINT('Ctrl Pts',(11.0814724299999,11.6,-1.06037935500002));
#188596=CARTESIAN_POINT('Ctrl Pts',(11.0846357549999,15.2,-1.05945144900002));
#188597=CARTESIAN_POINT('Ctrl Pts',(11.0846357549999,11.6,-1.05945144900002));
#188598=CARTESIAN_POINT('Ctrl Pts',(11.0878031359999,15.2,-1.05851961200001));
#188599=CARTESIAN_POINT('Ctrl Pts',(11.0878031359999,11.6,-1.05851961200001));
#188600=CARTESIAN_POINT('Ctrl Pts',(11.0909745619999,15.2,-1.05758384000001));
#188601=CARTESIAN_POINT('Ctrl Pts',(11.0909745619999,11.6,-1.05758384000001));
#188602=CARTESIAN_POINT('Ctrl Pts',(11.0941500229999,15.2,-1.05664412900001));
#188603=CARTESIAN_POINT('Ctrl Pts',(11.0941500229999,11.6,-1.05664412900001));
#188604=CARTESIAN_POINT('Ctrl Pts',(11.0973295109999,15.2,-1.05570047500001));
#188605=CARTESIAN_POINT('Ctrl Pts',(11.0973295109999,11.6,-1.05570047500001));
#188606=CARTESIAN_POINT('Ctrl Pts',(11.1005130129999,15.2,-1.05475287300001));
#188607=CARTESIAN_POINT('Ctrl Pts',(11.1005130129999,11.6,-1.05475287300001));
#188608=CARTESIAN_POINT('Ctrl Pts',(11.1037005219999,15.2,-1.05380132100001));
#188609=CARTESIAN_POINT('Ctrl Pts',(11.1037005219999,11.6,-1.05380132100001));
#188610=CARTESIAN_POINT('Ctrl Pts',(11.1068920249999,15.2,-1.05284581400001));
#188611=CARTESIAN_POINT('Ctrl Pts',(11.1068920249999,11.6,-1.05284581400001));
#188612=CARTESIAN_POINT('Ctrl Pts',(11.1100875149999,15.2,-1.05188634700002));
#188613=CARTESIAN_POINT('Ctrl Pts',(11.1100875149999,11.6,-1.05188634700002));
#188614=CARTESIAN_POINT('Ctrl Pts',(11.1132869809999,15.2,-1.05092291700001));
#188615=CARTESIAN_POINT('Ctrl Pts',(11.1132869809999,11.6,-1.05092291700001));
#188616=CARTESIAN_POINT('Ctrl Pts',(11.1164904129999,15.2,-1.04995552100001));
#188617=CARTESIAN_POINT('Ctrl Pts',(11.1164904129999,11.6,-1.04995552100001));
#188618=CARTESIAN_POINT('Ctrl Pts',(11.1196978009999,15.2,-1.04898415400001));
#188619=CARTESIAN_POINT('Ctrl Pts',(11.1196978009999,11.6,-1.04898415400001));
#188620=CARTESIAN_POINT('Ctrl Pts',(11.1229091349999,15.2,-1.04800881300001));
#188621=CARTESIAN_POINT('Ctrl Pts',(11.1229091349999,11.6,-1.04800881300001));
#188622=CARTESIAN_POINT('Ctrl Pts',(11.1261244069999,15.2,-1.04702949200002));
#188623=CARTESIAN_POINT('Ctrl Pts',(11.1261244069999,11.6,-1.04702949200002));
#188624=CARTESIAN_POINT('Ctrl Pts',(11.1293436049999,15.2,-1.04604618900002));
#188625=CARTESIAN_POINT('Ctrl Pts',(11.1293436049999,11.6,-1.04604618900002));
#188626=CARTESIAN_POINT('Ctrl Pts',(11.1325667189999,15.2,-1.04505890000001));
#188627=CARTESIAN_POINT('Ctrl Pts',(11.1325667189999,11.6,-1.04505890000001));
#188628=CARTESIAN_POINT('Ctrl Pts',(11.1357937419999,15.2,-1.04406762000002));
#188629=CARTESIAN_POINT('Ctrl Pts',(11.1357937419999,11.6,-1.04406762000002));
#188630=CARTESIAN_POINT('Ctrl Pts',(11.1390246609999,15.2,-1.04307234700002));
#188631=CARTESIAN_POINT('Ctrl Pts',(11.1390246609999,11.6,-1.04307234700002));
#188632=CARTESIAN_POINT('Ctrl Pts',(11.1422594689999,15.2,-1.04207307500001));
#188633=CARTESIAN_POINT('Ctrl Pts',(11.1422594689999,11.6,-1.04207307500001));
#188634=CARTESIAN_POINT('Ctrl Pts',(11.1454981539999,15.2,-1.04106980300001));
#188635=CARTESIAN_POINT('Ctrl Pts',(11.1454981539999,11.6,-1.04106980300001));
#188636=CARTESIAN_POINT('Ctrl Pts',(11.1487407069999,15.2,-1.04006252500001));
#188637=CARTESIAN_POINT('Ctrl Pts',(11.1487407069999,11.6,-1.04006252500001));
#188638=CARTESIAN_POINT('Ctrl Pts',(11.1519871189999,15.2,-1.03905123800001));
#188639=CARTESIAN_POINT('Ctrl Pts',(11.1519871189999,11.6,-1.03905123800002));
#188640=CARTESIAN_POINT('Ctrl Pts',(11.1552373799999,15.2,-1.03803593800002));
#188641=CARTESIAN_POINT('Ctrl Pts',(11.1552373799999,11.6,-1.03803593800002));
#188642=CARTESIAN_POINT('Ctrl Pts',(11.1584914799999,15.2,-1.03701662100002));
#188643=CARTESIAN_POINT('Ctrl Pts',(11.1584914799999,11.6,-1.03701662100002));
#188644=CARTESIAN_POINT('Ctrl Pts',(11.1617494109999,15.2,-1.03599328400001));
#188645=CARTESIAN_POINT('Ctrl Pts',(11.1617494109999,11.6,-1.03599328400001));
#188646=CARTESIAN_POINT('Ctrl Pts',(11.1650111599999,15.2,-1.03496592300001));
#188647=CARTESIAN_POINT('Ctrl Pts',(11.1650111599999,11.6,-1.03496592300001));
#188648=CARTESIAN_POINT('Ctrl Pts',(11.1682767209999,15.2,-1.03393453400002));
#188649=CARTESIAN_POINT('Ctrl Pts',(11.1682767209999,11.6,-1.03393453400002));
#188650=CARTESIAN_POINT('Ctrl Pts',(11.1715460819999,15.2,-1.03289911400001));
#188651=CARTESIAN_POINT('Ctrl Pts',(11.1715460819999,11.6,-1.03289911400001));
#188652=CARTESIAN_POINT('Ctrl Pts',(11.1748192339999,15.2,-1.03185965900002));
#188653=CARTESIAN_POINT('Ctrl Pts',(11.1748192339999,11.6,-1.03185965900002));
#188654=CARTESIAN_POINT('Ctrl Pts',(11.1780961679999,15.2,-1.03081616500001));
#188655=CARTESIAN_POINT('Ctrl Pts',(11.1780961679999,11.6,-1.03081616500001));
#188656=CARTESIAN_POINT('Ctrl Pts',(11.1813768729999,15.2,-1.02976862900002));
#188657=CARTESIAN_POINT('Ctrl Pts',(11.1813768729999,11.6,-1.02976862900002));
#188658=CARTESIAN_POINT('Ctrl Pts',(11.1846613419999,15.2,-1.02871704700001));
#188659=CARTESIAN_POINT('Ctrl Pts',(11.1846613419999,11.6,-1.02871704700001));
#188660=CARTESIAN_POINT('Ctrl Pts',(11.1879495629999,15.2,-1.02766141500001));
#188661=CARTESIAN_POINT('Ctrl Pts',(11.1879495629999,11.6,-1.02766141500001));
#188662=CARTESIAN_POINT('Ctrl Pts',(11.1912415279999,15.2,-1.02660173100002));
#188663=CARTESIAN_POINT('Ctrl Pts',(11.1912415279999,11.6,-1.02660173100002));
#188664=CARTESIAN_POINT('Ctrl Pts',(11.1945372269999,15.2,-1.02553798900002));
#188665=CARTESIAN_POINT('Ctrl Pts',(11.1945372269999,11.6,-1.02553798900002));
#188666=CARTESIAN_POINT('Ctrl Pts',(11.1978366499999,15.2,-1.02447018800001));
#188667=CARTESIAN_POINT('Ctrl Pts',(11.1978366499999,11.6,-1.02447018800001));
#188668=CARTESIAN_POINT('Ctrl Pts',(11.2011397889999,15.2,-1.02339832200002));
#188669=CARTESIAN_POINT('Ctrl Pts',(11.2011397889999,11.6,-1.02339832200002));
#188670=CARTESIAN_POINT('Ctrl Pts',(11.2044466319999,15.2,-1.02232239100001));
#188671=CARTESIAN_POINT('Ctrl Pts',(11.2044466319999,11.6,-1.02232239100001));
#188672=CARTESIAN_POINT('Ctrl Pts',(11.2077571719999,15.2,-1.02124238700001));
#188673=CARTESIAN_POINT('Ctrl Pts',(11.2077571719999,11.6,-1.02124238700001));
#188674=CARTESIAN_POINT('Ctrl Pts',(11.2110713989999,15.2,-1.02015830900001));
#188675=CARTESIAN_POINT('Ctrl Pts',(11.2110713989999,11.6,-1.02015830900001));
#188676=CARTESIAN_POINT('Ctrl Pts',(11.2143893039999,15.2,-1.01907015400001));
#188677=CARTESIAN_POINT('Ctrl Pts',(11.2143893039999,11.6,-1.01907015400002));
#188678=CARTESIAN_POINT('Ctrl Pts',(11.2177108769999,15.2,-1.01797791700001));
#188679=CARTESIAN_POINT('Ctrl Pts',(11.2177108769999,11.6,-1.01797791700002));
#188680=CARTESIAN_POINT('Ctrl Pts',(11.2210361069999,15.2,-1.01688159500001));
#188681=CARTESIAN_POINT('Ctrl Pts',(11.2210361069999,11.6,-1.01688159500001));
#188682=CARTESIAN_POINT('Ctrl Pts',(11.2243649869999,15.2,-1.01578118600001));
#188683=CARTESIAN_POINT('Ctrl Pts',(11.2243649869999,11.6,-1.01578118600001));
#188684=CARTESIAN_POINT('Ctrl Pts',(11.2276975069999,15.2,-1.01467668400002));
#188685=CARTESIAN_POINT('Ctrl Pts',(11.2276975069999,11.6,-1.01467668400002));
#188686=CARTESIAN_POINT('Ctrl Pts',(11.2310336579999,15.2,-1.01356808800002));
#188687=CARTESIAN_POINT('Ctrl Pts',(11.2310336579999,11.6,-1.01356808800002));
#188688=CARTESIAN_POINT('Ctrl Pts',(11.2343734289999,15.2,-1.01245539300002));
#188689=CARTESIAN_POINT('Ctrl Pts',(11.2343734289999,11.6,-1.01245539300002));
#188690=CARTESIAN_POINT('Ctrl Pts',(11.2377168129999,15.2,-1.01133859700001));
#188691=CARTESIAN_POINT('Ctrl Pts',(11.2377168129999,11.6,-1.01133859700001));
#188692=CARTESIAN_POINT('Ctrl Pts',(11.2410637989999,15.2,-1.01021769500001));
#188693=CARTESIAN_POINT('Ctrl Pts',(11.2410637989999,11.6,-1.01021769500001));
#188694=CARTESIAN_POINT('Ctrl Pts',(11.2444143789999,15.2,-1.00909268500001));
#188695=CARTESIAN_POINT('Ctrl Pts',(11.2444143789999,11.6,-1.00909268500002));
#188696=CARTESIAN_POINT('Ctrl Pts',(11.2477685419999,15.2,-1.00796356400001));
#188697=CARTESIAN_POINT('Ctrl Pts',(11.2477685419999,11.6,-1.00796356400001));
#188698=CARTESIAN_POINT('Ctrl Pts',(11.2511262799999,15.2,-1.00683032600001));
#188699=CARTESIAN_POINT('Ctrl Pts',(11.2511262799999,11.6,-1.00683032600001));
#188700=CARTESIAN_POINT('Ctrl Pts',(11.2544875849999,15.2,-1.00569297000002));
#188701=CARTESIAN_POINT('Ctrl Pts',(11.2544875849999,11.6,-1.00569297000002));
#188702=CARTESIAN_POINT('Ctrl Pts',(11.2578524459999,15.2,-1.00455149200001));
#188703=CARTESIAN_POINT('Ctrl Pts',(11.2578524459999,11.6,-1.00455149200001));
#188704=CARTESIAN_POINT('Ctrl Pts',(11.2612208539999,15.2,-1.00340589000002));
#188705=CARTESIAN_POINT('Ctrl Pts',(11.2612208539999,11.6,-1.00340589000002));
#188706=CARTESIAN_POINT('Ctrl Pts',(11.2645927989999,15.2,-1.00225615800001));
#188707=CARTESIAN_POINT('Ctrl Pts',(11.2645927989999,11.6,-1.00225615800001));
#188708=CARTESIAN_POINT('Ctrl Pts',(11.2679682739999,15.2,-1.00110229500002));
#188709=CARTESIAN_POINT('Ctrl Pts',(11.2679682739999,11.6,-1.00110229500002));
#188710=CARTESIAN_POINT('Ctrl Pts',(11.2713472679999,15.2,-0.999944297000015));
#188711=CARTESIAN_POINT('Ctrl Pts',(11.2713472679999,11.6,-0.999944297000015));
#188712=CARTESIAN_POINT('Ctrl Pts',(11.2747297729999,15.2,-0.998782161000014));
#188713=CARTESIAN_POINT('Ctrl Pts',(11.2747297729999,11.6,-0.998782161000014));
#188714=CARTESIAN_POINT('Ctrl Pts',(11.2781157789999,15.2,-0.997615884000016));
#188715=CARTESIAN_POINT('Ctrl Pts',(11.2781157789999,11.6,-0.997615884000016));
#188716=CARTESIAN_POINT('Ctrl Pts',(11.2815052779999,15.2,-0.996445462000013));
#188717=CARTESIAN_POINT('Ctrl Pts',(11.2815052779999,11.6,-0.996445462000013));
#188718=CARTESIAN_POINT('Ctrl Pts',(11.2848982589999,15.2,-0.995270892000013));
#188719=CARTESIAN_POINT('Ctrl Pts',(11.2848982589999,11.6,-0.995270892000014));
#188720=CARTESIAN_POINT('Ctrl Pts',(11.2882947149999,15.2,-0.994092171000016));
#188721=CARTESIAN_POINT('Ctrl Pts',(11.2882947149999,11.6,-0.994092171000017));
#188722=CARTESIAN_POINT('Ctrl Pts',(11.2916946349999,15.2,-0.992909297000013));
#188723=CARTESIAN_POINT('Ctrl Pts',(11.2916946349999,11.6,-0.992909297000014));
#188724=CARTESIAN_POINT('Ctrl Pts',(11.2950980119999,15.2,-0.991722263000017));
#188725=CARTESIAN_POINT('Ctrl Pts',(11.2950980119999,11.6,-0.991722263000017));
#188726=CARTESIAN_POINT('Ctrl Pts',(11.2985048339999,15.2,-0.990531071000014));
#188727=CARTESIAN_POINT('Ctrl Pts',(11.2985048339999,11.6,-0.990531071000014));
#188728=CARTESIAN_POINT('Ctrl Pts',(11.3019150959999,15.2,-0.989335715000017));
#188729=CARTESIAN_POINT('Ctrl Pts',(11.3019150959999,11.6,-0.989335715000017));
#188730=CARTESIAN_POINT('Ctrl Pts',(11.3053287859999,15.2,-0.988136191000013));
#188731=CARTESIAN_POINT('Ctrl Pts',(11.3053287859999,11.6,-0.988136191000013));
#188732=CARTESIAN_POINT('Ctrl Pts',(11.3087458949999,15.2,-0.986932498000015));
#188733=CARTESIAN_POINT('Ctrl Pts',(11.3087458949999,11.6,-0.986932498000015));
#188734=CARTESIAN_POINT('Ctrl Pts',(11.3121664159999,15.2,-0.985724632000018));
#188735=CARTESIAN_POINT('Ctrl Pts',(11.3121664159999,11.6,-0.985724632000018));
#188736=CARTESIAN_POINT('Ctrl Pts',(11.3155903389999,15.2,-0.984512590000013));
#188737=CARTESIAN_POINT('Ctrl Pts',(11.3155903389999,11.6,-0.984512590000013));
#188738=CARTESIAN_POINT('Ctrl Pts',(11.3190176529999,15.2,-0.983296370000013));
#188739=CARTESIAN_POINT('Ctrl Pts',(11.3190176529999,11.6,-0.983296370000013));
#188740=CARTESIAN_POINT('Ctrl Pts',(11.3224483519999,15.2,-0.982075966000018));
#188741=CARTESIAN_POINT('Ctrl Pts',(11.3224483519999,11.6,-0.982075966000018));
#188742=CARTESIAN_POINT('Ctrl Pts',(11.3258824259999,15.2,-0.980851377000014));
#188743=CARTESIAN_POINT('Ctrl Pts',(11.3258824259999,11.6,-0.980851377000014));
#188744=CARTESIAN_POINT('Ctrl Pts',(11.3293198659999,15.2,-0.979622601000014));
#188745=CARTESIAN_POINT('Ctrl Pts',(11.3293198659999,11.6,-0.979622601000015));
#188746=CARTESIAN_POINT('Ctrl Pts',(11.3327606619999,15.2,-0.978389632000014));
#188747=CARTESIAN_POINT('Ctrl Pts',(11.3327606619999,11.6,-0.978389632000014));
#188748=CARTESIAN_POINT('Ctrl Pts',(11.3362048069999,15.2,-0.977152470000018));
#188749=CARTESIAN_POINT('Ctrl Pts',(11.3362048069999,11.6,-0.977152470000018));
#188750=CARTESIAN_POINT('Ctrl Pts',(11.3396522919999,15.2,-0.975911111000016));
#188751=CARTESIAN_POINT('Ctrl Pts',(11.3396522919999,11.6,-0.975911111000017));
#188752=CARTESIAN_POINT('Ctrl Pts',(11.3431031069999,15.2,-0.974665551000014));
#188753=CARTESIAN_POINT('Ctrl Pts',(11.3431031069999,11.6,-0.974665551000014));
#188754=CARTESIAN_POINT('Ctrl Pts',(11.3465572429999,15.2,-0.973415788000014));
#188755=CARTESIAN_POINT('Ctrl Pts',(11.3465572429999,11.6,-0.973415788000014));
#188756=CARTESIAN_POINT('Ctrl Pts',(11.3500146919999,15.2,-0.972161819000017));
#188757=CARTESIAN_POINT('Ctrl Pts',(11.3500146919999,11.6,-0.972161819000017));
#188758=CARTESIAN_POINT('Ctrl Pts',(11.3534754439999,15.2,-0.970903641000014));
#188759=CARTESIAN_POINT('Ctrl Pts',(11.3534754439999,11.6,-0.970903641000014));
#188760=CARTESIAN_POINT('Ctrl Pts',(11.3569394909999,15.2,-0.969641251000013));
#188761=CARTESIAN_POINT('Ctrl Pts',(11.3569394909999,11.6,-0.969641251000013));
#188762=CARTESIAN_POINT('Ctrl Pts',(11.3604068239999,15.2,-0.968374645000014));
#188763=CARTESIAN_POINT('Ctrl Pts',(11.3604068239999,11.6,-0.968374645000015));
#188764=CARTESIAN_POINT('Ctrl Pts',(11.3638774359999,15.2,-0.967103822000013));
#188765=CARTESIAN_POINT('Ctrl Pts',(11.3638774359999,11.6,-0.967103822000013));
#188766=CARTESIAN_POINT('Ctrl Pts',(11.3673513139999,15.2,-0.965828778000013));
#188767=CARTESIAN_POINT('Ctrl Pts',(11.3673513139999,11.6,-0.965828778000013));
#188768=CARTESIAN_POINT('Ctrl Pts',(11.3708284529999,15.2,-0.964549510000015));
#188769=CARTESIAN_POINT('Ctrl Pts',(11.3708284529999,11.6,-0.964549510000015));
#188770=CARTESIAN_POINT('Ctrl Pts',(11.3743088439999,15.2,-0.963266017000013));
#188771=CARTESIAN_POINT('Ctrl Pts',(11.3743088439999,11.6,-0.963266017000013));
#188772=CARTESIAN_POINT('Ctrl Pts',(11.3777924759999,15.2,-0.961978293000012));
#188773=CARTESIAN_POINT('Ctrl Pts',(11.3777924759999,11.6,-0.961978293000012));
#188774=CARTESIAN_POINT('Ctrl Pts',(11.3812793429999,15.2,-0.960686338000016));
#188775=CARTESIAN_POINT('Ctrl Pts',(11.3812793429999,11.6,-0.960686338000017));
#188776=CARTESIAN_POINT('Ctrl Pts',(11.3847694349999,15.2,-0.959390147000012));
#188777=CARTESIAN_POINT('Ctrl Pts',(11.3847694349999,11.6,-0.959390147000013));
#188778=CARTESIAN_POINT('Ctrl Pts',(11.3882627429999,15.2,-0.958089719000017));
#188779=CARTESIAN_POINT('Ctrl Pts',(11.3882627429999,11.6,-0.958089719000017));
#188780=CARTESIAN_POINT('Ctrl Pts',(11.3917592569999,15.2,-0.956785049000013));
#188781=CARTESIAN_POINT('Ctrl Pts',(11.3917592569999,11.6,-0.956785049000013));
#188782=CARTESIAN_POINT('Ctrl Pts',(11.3952589699999,15.2,-0.955476136000013));
#188783=CARTESIAN_POINT('Ctrl Pts',(11.3952589699999,11.6,-0.955476136000013));
#188784=CARTESIAN_POINT('Ctrl Pts',(11.3987618709999,15.2,-0.954162977000017));
#188785=CARTESIAN_POINT('Ctrl Pts',(11.3987618709999,11.6,-0.954162977000018));
#188786=CARTESIAN_POINT('Ctrl Pts',(11.4022679529999,15.2,-0.952845568000011));
#188787=CARTESIAN_POINT('Ctrl Pts',(11.4022679529999,11.6,-0.952845568000012));
#188788=CARTESIAN_POINT('Ctrl Pts',(11.4057772069999,15.2,-0.951523906000014));
#188789=CARTESIAN_POINT('Ctrl Pts',(11.4057772069999,11.6,-0.951523906000014));
#188790=CARTESIAN_POINT('Ctrl Pts',(11.4092896249999,15.2,-0.950197991000015));
#188791=CARTESIAN_POINT('Ctrl Pts',(11.4092896249999,11.6,-0.950197991000015));
#188792=CARTESIAN_POINT('Ctrl Pts',(11.4128051999999,15.2,-0.948867819000014));
#188793=CARTESIAN_POINT('Ctrl Pts',(11.4128051999999,11.6,-0.948867819000015));
#188794=CARTESIAN_POINT('Ctrl Pts',(11.4163239239999,15.2,-0.947533387000017));
#188795=CARTESIAN_POINT('Ctrl Pts',(11.4163239239999,11.6,-0.947533387000017));
#188796=CARTESIAN_POINT('Ctrl Pts',(11.4198457879999,15.2,-0.946194694000013));
#188797=CARTESIAN_POINT('Ctrl Pts',(11.4198457879999,11.6,-0.946194694000014));
#188798=CARTESIAN_POINT('Ctrl Pts',(11.4233707839999,15.2,-0.944851734000016));
#188799=CARTESIAN_POINT('Ctrl Pts',(11.4233707839999,11.6,-0.944851734000017));
#188800=CARTESIAN_POINT('Ctrl Pts',(11.4268989019999,15.2,-0.943504507000017));
#188801=CARTESIAN_POINT('Ctrl Pts',(11.4268989019999,11.6,-0.943504507000017));
#188802=CARTESIAN_POINT('Ctrl Pts',(11.4304301309999,15.2,-0.942153010000015));
#188803=CARTESIAN_POINT('Ctrl Pts',(11.4304301309999,11.6,-0.942153010000016));
#188804=CARTESIAN_POINT('Ctrl Pts',(11.4339644589999,15.2,-0.940797237000015));
#188805=CARTESIAN_POINT('Ctrl Pts',(11.4339644589999,11.6,-0.940797237000015));
#188806=CARTESIAN_POINT('Ctrl Pts',(11.4375018779999,15.2,-0.939437187000016));
#188807=CARTESIAN_POINT('Ctrl Pts',(11.4375018779999,11.6,-0.939437187000017));
#188808=CARTESIAN_POINT('Ctrl Pts',(11.4410423789999,15.2,-0.938072856000014));
#188809=CARTESIAN_POINT('Ctrl Pts',(11.4410423789999,11.6,-0.938072856000014));
#188810=CARTESIAN_POINT('Ctrl Pts',(11.4445859519999,15.2,-0.936704241000013));
#188811=CARTESIAN_POINT('Ctrl Pts',(11.4445859519999,11.6,-0.936704241000013));
#188812=CARTESIAN_POINT('Ctrl Pts',(11.4481325909999,15.2,-0.935331342000012));
#188813=CARTESIAN_POINT('Ctrl Pts',(11.4481325909999,11.6,-0.935331342000012));
#188814=CARTESIAN_POINT('Ctrl Pts',(11.4516822949999,15.2,-0.933954156000016));
#188815=CARTESIAN_POINT('Ctrl Pts',(11.4516822949999,11.6,-0.933954156000017));
#188816=CARTESIAN_POINT('Ctrl Pts',(11.4552350599999,15.2,-0.932572684000017));
#188817=CARTESIAN_POINT('Ctrl Pts',(11.4552350599999,11.6,-0.932572684000017));
#188818=CARTESIAN_POINT('Ctrl Pts',(11.4580797199999,15.2,-0.931464077000013));
#188819=CARTESIAN_POINT('Ctrl Pts',(11.4580797199999,11.6,-0.931464077000013));
#188820=CARTESIAN_POINT('Ctrl Pts',(11.4602145909999,15.2,-0.930630693000012));
#188821=CARTESIAN_POINT('Ctrl Pts',(11.4602145909999,11.6,-0.930630693000012));
#188822=CARTESIAN_POINT('Ctrl Pts',(11.4616384499999,15.2,-0.930074246000014));
#188823=CARTESIAN_POINT('Ctrl Pts',(11.4616384499999,11.6,-0.930074246000015));
#188824=CARTESIAN_POINT('Ctrl Pts',(11.4623505329999,15.2,-0.929795809000016));
#188825=CARTESIAN_POINT('Ctrl Pts',(11.4623505329999,11.6,-0.929795809000016));
#188826=CARTESIAN_POINT('Ctrl Pts',(10.3068855239999,15.2,-1.18690176600001));
#188827=CARTESIAN_POINT('Ctrl Pts',(10.3086714467389,15.2,-1.1869528784395));
#188828=CARTESIAN_POINT('Ctrl Pts',(10.3105146691063,15.2,-1.18700024430173));
#188829=CARTESIAN_POINT('Ctrl Pts',(10.3124142310585,15.2,-1.18704320794532));
#188830=CARTESIAN_POINT('Ctrl Pts',(10.3143229536586,15.2,-1.18708637878131));
#188831=CARTESIAN_POINT('Ctrl Pts',(10.3162885628145,15.2,-1.18712509875838));
#188832=CARTESIAN_POINT('Ctrl Pts',(10.3183101246955,15.2,-1.18715870867826));
#188833=CARTESIAN_POINT('Ctrl Pts',(10.3206686132814,15.2,-1.18719792024688));
#188834=CARTESIAN_POINT('Ctrl Pts',(10.3231032554094,15.2,-1.18723017361547));
#188835=CARTESIAN_POINT('Ctrl Pts',(10.3256126114571,15.2,-1.18725445923942));
#188836=CARTESIAN_POINT('Ctrl Pts',(10.3277634883206,15.2,-1.18727527549095));
#188837=CARTESIAN_POINT('Ctrl Pts',(10.3299692556961,15.2,-1.18729023695032));
#188838=CARTESIAN_POINT('Ctrl Pts',(10.3322290309353,15.2,-1.18729873195083));
#188839=CARTESIAN_POINT('Ctrl Pts',(10.3344888059692,15.2,-1.18730722695057));
#188840=CARTESIAN_POINT('Ctrl Pts',(10.3368025915859,15.2,-1.18730925158318));
#188841=CARTESIAN_POINT('Ctrl Pts',(10.3391695234998,15.2,-1.18730421375003));
#188842=CARTESIAN_POINT('Ctrl Pts',(10.3419309442095,15.2,-1.18729833627771));
#188843=CARTESIAN_POINT('Ctrl Pts',(10.3447647053247,15.2,-1.18728284169453));
#188844=CARTESIAN_POINT('Ctrl Pts',(10.3476694772408,15.2,-1.18725682074785));
#188845=CARTESIAN_POINT('Ctrl Pts',(10.3501592816111,15.2,-1.18723451708043));
#188846=CARTESIAN_POINT('Ctrl Pts',(10.3527012581607,15.2,-1.1872044765403));
#188847=CARTESIAN_POINT('Ctrl Pts',(10.3552945932332,15.2,-1.18716614595836));
#188848=CARTESIAN_POINT('Ctrl Pts',(10.3578879283056,15.2,-1.18712781537642));
#188849=CARTESIAN_POINT('Ctrl Pts',(10.3605326202138,15.2,-1.18708119543062));
#188850=CARTESIAN_POINT('Ctrl Pts',(10.3632278754976,15.2,-1.18702574301371));
#188851=CARTESIAN_POINT('Ctrl Pts',(10.3659231310262,15.2,-1.18697029059176));
#188852=CARTESIAN_POINT('Ctrl Pts',(10.3686689482239,15.2,-1.18690600845499));
#188853=CARTESIAN_POINT('Ctrl Pts',(10.3714645527963,15.2,-1.18683237403367));
#188854=CARTESIAN_POINT('Ctrl Pts',(10.3742601571147,15.2,-1.18675873961904));
#188855=CARTESIAN_POINT('Ctrl Pts',(10.3771055475764,15.2,-1.18667575065539));
#188856=CARTESIAN_POINT('Ctrl Pts',(10.3799999659845,15.2,-1.18658290124166));
#188857=CARTESIAN_POINT('Ctrl Pts',(10.3828943843926,15.2,-1.18649005182792));
#188858=CARTESIAN_POINT('Ctrl Pts',(10.3858378311395,15.2,-1.18638734211826));
#188859=CARTESIAN_POINT('Ctrl Pts',(10.388829564612,15.2,-1.18627427795615));
#188860=CARTESIAN_POINT('Ctrl Pts',(10.3918212983563,15.2,-1.18616121378377));
#188861=CARTESIAN_POINT('Ctrl Pts',(10.3948613167899,15.2,-1.18603779600178));
#188862=CARTESIAN_POINT('Ctrl Pts',(10.3979488985448,15.2,-1.18590354674373));
#188863=CARTESIAN_POINT('Ctrl Pts',(10.4010364800191,15.2,-1.18576929749787));
#188864=CARTESIAN_POINT('Ctrl Pts',(10.4041716226371,15.2,-1.18562421472794));
#188865=CARTESIAN_POINT('Ctrl Pts',(10.4073536171901,15.2,-1.18546783648313));
#188866=CARTESIAN_POINT('Ctrl Pts',(10.4105356117432,15.2,-1.18531145823832));
#188867=CARTESIAN_POINT('Ctrl Pts',(10.4137644583592,15.2,-1.1851437827194));
#188868=CARTESIAN_POINT('Ctrl Pts',(10.4170394620716,15.2,-1.18496435772643));
#188869=CARTESIAN_POINT('Ctrl Pts',(10.4214061337872,15.2,-1.18472512439704));
#188870=CARTESIAN_POINT('Ctrl Pts',(10.4258548607992,15.2,-1.18446500339921));
#188871=CARTESIAN_POINT('Ctrl Pts',(10.4303840394047,15.2,-1.1841829592788));
#188872=CARTESIAN_POINT('Ctrl Pts',(10.4343470708002,15.2,-1.18393617066624));
#188873=CARTESIAN_POINT('Ctrl Pts',(10.4383716952584,15.2,-1.18367259643219));
#188874=CARTESIAN_POINT('Ctrl Pts',(10.4424568660582,15.2,-1.18339156752504));
#188875=CARTESIAN_POINT('Ctrl Pts',(10.4465420368579,15.2,-1.18311053861789));
#188876=CARTESIAN_POINT('Ctrl Pts',(10.4506877527646,15.2,-1.18281205483429));
#188877=CARTESIAN_POINT('Ctrl Pts',(10.4548929891403,15.2,-1.18249546717376));
#188878=CARTESIAN_POINT('Ctrl Pts',(10.4584974772753,15.2,-1.18222410633595));
#188879=CARTESIAN_POINT('Ctrl Pts',(10.462145694934,15.2,-1.18193944523087));
#188880=CARTESIAN_POINT('Ctrl Pts',(10.4658370099665,15.2,-1.18164108749171));
#188881=CARTESIAN_POINT('Ctrl Pts',(10.4701435443947,15.2,-1.18129300344462));
#188882=CARTESIAN_POINT('Ctrl Pts',(10.4745087382407,15.2,-1.18092627583869));
#188883=CARTESIAN_POINT('Ctrl Pts',(10.478931608325,15.2,-1.18054029270133));
#188884=CARTESIAN_POINT('Ctrl Pts',(10.4827226396292,15.2,-1.18020945002934));
#188885=CARTESIAN_POINT('Ctrl Pts',(10.486556045599,15.2,-1.17986446165365));
#188886=CARTESIAN_POINT('Ctrl Pts',(10.4904312197082,15.2,-1.17950495200004));
#188887=CARTESIAN_POINT('Ctrl Pts',(10.496243980872,15.2,-1.17896568751964));
#188888=CARTESIAN_POINT('Ctrl Pts',(10.5021507173861,15.2,-1.17839375053718));
#188889=CARTESIAN_POINT('Ctrl Pts',(10.508149426039,15.2,-1.17778792031073));
#188890=CARTESIAN_POINT('Ctrl Pts',(10.5121485655041,15.2,-1.17738403345641));
#188891=CARTESIAN_POINT('Ctrl Pts',(10.516188583465,15.2,-1.17696508170065));
#188892=CARTESIAN_POINT('Ctrl Pts',(10.5202688980224,15.2,-1.1765307171763));
#188893=CARTESIAN_POINT('Ctrl Pts',(10.5250292644502,15.2,-1.17602395862375));
#188894=CARTESIAN_POINT('Ctrl Pts',(10.5298444813069,15.2,-1.17549622163256));
#188895=CARTESIAN_POINT('Ctrl Pts',(10.53471364182,15.2,-1.17494696375136));
#188896=CARTESIAN_POINT('Ctrl Pts',(10.5388872084614,15.2,-1.17447617122677));
#188897=CARTESIAN_POINT('Ctrl Pts',(10.5431004072067,15.2,-1.17398956869235));
#188898=CARTESIAN_POINT('Ctrl Pts',(10.5473526826901,15.2,-1.17348682424757));
#188899=CARTESIAN_POINT('Ctrl Pts',(10.5516049577873,15.2,-1.17298407984847));
#188900=CARTESIAN_POINT('Ctrl Pts',(10.5558963048357,15.2,-1.17246519517489));
#188901=CARTESIAN_POINT('Ctrl Pts',(10.5602261780312,15.2,-1.17192984477528));
#188902=CARTESIAN_POINT('Ctrl Pts',(10.5645560512268,15.2,-1.17139449437567));
#188903=CARTESIAN_POINT('Ctrl Pts',(10.5689244484073,15.2,-1.17084268066522));
#188904=CARTESIAN_POINT('Ctrl Pts',(10.5733308288279,15.2,-1.17027408827035));
#188905=CARTESIAN_POINT('Ctrl Pts',(10.5777372096488,15.2,-1.16970549582383));
#188906=CARTESIAN_POINT('Ctrl Pts',(10.5821815751048,15.2,-1.16912012613898));
#188907=CARTESIAN_POINT('Ctrl Pts',(10.5866633921585,15.2,-1.16851766974172));
#188908=CARTESIAN_POINT('Ctrl Pts',(10.5903982394997,15.2,-1.16801562277137));
#188909=CARTESIAN_POINT('Ctrl Pts',(10.5941590933431,15.2,-1.16750171144334));
#188910=CARTESIAN_POINT('Ctrl Pts',(10.5979456537618,15.2,-1.16697576345625));
#188911=CARTESIAN_POINT('Ctrl Pts',(10.6024895260993,15.2,-1.16634462589466));
#188912=CARTESIAN_POINT('Ctrl Pts',(10.6070704129237,15.2,-1.16569615159527));
#188913=CARTESIAN_POINT('Ctrl Pts',(10.611687796527,15.2,-1.16503005128308));
#188914=CARTESIAN_POINT('Ctrl Pts',(10.6170747443438,15.2,-1.16425293421184));
#188915=CARTESIAN_POINT('Ctrl Pts',(10.6225113698796,15.2,-1.16345182399275));
#188916=CARTESIAN_POINT('Ctrl Pts',(10.6279968647457,15.2,-1.16262626721458));
#188917=CARTESIAN_POINT('Ctrl Pts',(10.632698717244,15.2,-1.16191864715573));
#188918=CARTESIAN_POINT('Ctrl Pts',(10.6374364739733,15.2,-1.16119306829803));
#188919=CARTESIAN_POINT('Ctrl Pts',(10.6422096354665,15.2,-1.16044925024172));
#188920=CARTESIAN_POINT('Ctrl Pts',(10.6469827969598,15.2,-1.15970543218541));
#188921=CARTESIAN_POINT('Ctrl Pts',(10.6517913613925,15.2,-1.1589433795684));
#188922=CARTESIAN_POINT('Ctrl Pts',(10.6566348390398,15.2,-1.15816281739218));
#188923=CARTESIAN_POINT('Ctrl Pts',(10.6606710705592,15.2,-1.15751234888836));
#188924=CARTESIAN_POINT('Ctrl Pts',(10.6647315450508,15.2,-1.15684902721018));
#188925=CARTESIAN_POINT('Ctrl Pts',(10.6688159817162,15.2,-1.15617270033587));
#188926=CARTESIAN_POINT('Ctrl Pts',(10.6729004183816,15.2,-1.15549637346155));
#188927=CARTESIAN_POINT('Ctrl Pts',(10.6770088199366,15.2,-1.15480704032856));
#188928=CARTESIAN_POINT('Ctrl Pts',(10.6811409039631,15.2,-1.15410455178758));
#188929=CARTESIAN_POINT('Ctrl Pts',(10.6844465713645,15.2,-1.15354256092416));
#188930=CARTESIAN_POINT('Ctrl Pts',(10.6877673976315,15.2,-1.15297214976888));
#188931=CARTESIAN_POINT('Ctrl Pts',(10.691103241259,15.2,-1.15239324420766));
#188932=CARTESIAN_POINT('Ctrl Pts',(10.6952730455662,15.2,-1.15166961229559));
#188933=CARTESIAN_POINT('Ctrl Pts',(10.6994663144995,15.2,-1.15093270629744));
#188934=CARTESIAN_POINT('Ctrl Pts',(10.7036827745014,15.2,-1.1501823812269));
#188935=CARTESIAN_POINT('Ctrl Pts',(10.7070559422272,15.2,-1.14958212121954));
#188936=CARTESIAN_POINT('Ctrl Pts',(10.7104439541788,15.2,-1.14897327350774));
#188937=CARTESIAN_POINT('Ctrl Pts',(10.7138466704552,15.2,-1.14835576605878));
#188938=CARTESIAN_POINT('Ctrl Pts',(10.7172493871952,15.2,-1.14773825852569));
#188939=CARTESIAN_POINT('Ctrl Pts',(10.7206668097243,15.2,-1.14711209012495));
#188940=CARTESIAN_POINT('Ctrl Pts',(10.724098799473,15.2,-1.14647718939121));
#188941=CARTESIAN_POINT('Ctrl Pts',(10.727530788754,15.2,-1.14584228874397));
#188942=CARTESIAN_POINT('Ctrl Pts',(10.7309773475621,15.2,-1.14519865686606));
#188943=CARTESIAN_POINT('Ctrl Pts',(10.7344383385004,15.2,-1.14454622158664));
#188944=CARTESIAN_POINT('Ctrl Pts',(10.7396298256153,15.2,-1.14356756853417));
#188945=CARTESIAN_POINT('Ctrl Pts',(10.7448537859175,15.2,-1.14256910956257));
#188946=CARTESIAN_POINT('Ctrl Pts',(10.7501097680395,15.2,-1.14155061233903));
#188947=CARTESIAN_POINT('Ctrl Pts',(10.7536137556434,15.2,-1.14087161428251));
#188948=CARTESIAN_POINT('Ctrl Pts',(10.7571319753008,15.2,-1.14018370986613));
#188949=CARTESIAN_POINT('Ctrl Pts',(10.7606642943058,15.2,-1.13948683130886));
#188950=CARTESIAN_POINT('Ctrl Pts',(10.7641966137921,15.2,-1.13878995265663));
#188951=CARTESIAN_POINT('Ctrl Pts',(10.767743032056,15.2,-1.13808410036471));
#188952=CARTESIAN_POINT('Ctrl Pts',(10.771303418307,15.2,-1.13736920815816));
#188953=CARTESIAN_POINT('Ctrl Pts',(10.7757539008782,15.2,-1.13647559294867));
#188954=CARTESIAN_POINT('Ctrl Pts',(10.7802262088693,15.2,-1.13556785070839));
#188955=CARTESIAN_POINT('Ctrl Pts',(10.7847200878294,15.2,-1.13464585563778));
#188956=CARTESIAN_POINT('Ctrl Pts',(10.7883151907035,15.2,-1.13390825964159));
#188957=CARTESIAN_POINT('Ctrl Pts',(10.7919240985688,15.2,-1.13316154130606));
#188958=CARTESIAN_POINT('Ctrl Pts',(10.7955466824558,15.2,-1.1324056373089));
#188959=CARTESIAN_POINT('Ctrl Pts',(10.7991692668363,15.2,-1.13164973320875));
#188960=CARTESIAN_POINT('Ctrl Pts',(10.8028055286936,15.2,-1.13088464063048));
#188961=CARTESIAN_POINT('Ctrl Pts',(10.8064553388383,15.2,-1.13011029986511));
#188962=CARTESIAN_POINT('Ctrl Pts',(10.8101051484858,15.2,-1.12933595920524));
#188963=CARTESIAN_POINT('Ctrl Pts',(10.8137685064204,15.2,-1.12855236811046));
#188964=CARTESIAN_POINT('Ctrl Pts',(10.8174452861744,15.2,-1.12775946606478));
#188965=CARTESIAN_POINT('Ctrl Pts',(10.8229604560561,15.2,-1.12657011294224));
#188966=CARTESIAN_POINT('Ctrl Pts',(10.8285058251134,15.2,-1.12535980549642));
#188967=CARTESIAN_POINT('Ctrl Pts',(10.8340809709089,15.2,-1.12412834062594));
#188968=CARTESIAN_POINT('Ctrl Pts',(10.8396561172107,15.2,-1.1228968756436));
#188969=CARTESIAN_POINT('Ctrl Pts',(10.8452610382988,15.2,-1.12164425230923));
#188970=CARTESIAN_POINT('Ctrl Pts',(10.8508953167738,15.2,-1.12037027015553));
#188971=CARTESIAN_POINT('Ctrl Pts',(10.8555905485804,15.2,-1.11930861841864));
#188972=CARTESIAN_POINT('Ctrl Pts',(10.8603061689784,15.2,-1.11823213332331));
#188973=CARTESIAN_POINT('Ctrl Pts',(10.8650419360914,15.2,-1.11714070090664));
#188974=CARTESIAN_POINT('Ctrl Pts',(10.8688305494721,15.2,-1.11626755504467));
#188975=CARTESIAN_POINT('Ctrl Pts',(10.8726320572842,15.2,-1.11538484343267));
#188976=CARTESIAN_POINT('Ctrl Pts',(10.8764463389715,15.2,-1.11449250883958));
#188977=CARTESIAN_POINT('Ctrl Pts',(10.8812141914705,15.2,-1.11337709050703));
#188978=CARTESIAN_POINT('Ctrl Pts',(10.8860020013255,15.2,-1.11224663584076));
#188979=CARTESIAN_POINT('Ctrl Pts',(10.8908095347273,15.2,-1.11110103354988));
#188980=CARTESIAN_POINT('Ctrl Pts',(10.895617068129,15.2,-1.10995543125901));
#188981=CARTESIAN_POINT('Ctrl Pts',(10.9004443251919,15.2,-1.10879468328933));
#188982=CARTESIAN_POINT('Ctrl Pts',(10.9052910712556,15.2,-1.10761868099236));
#188983=CARTESIAN_POINT('Ctrl Pts',(10.9091684683178,15.2,-1.10667787910351));
#188984=CARTESIAN_POINT('Ctrl Pts',(10.9130583385795,15.2,-1.1057273149797));
#188985=CARTESIAN_POINT('Ctrl Pts',(10.9169605649046,15.2,-1.10476693359302));
#188986=CARTESIAN_POINT('Ctrl Pts',(10.920862790698,15.2,-1.1038065523372));
#188987=CARTESIAN_POINT('Ctrl Pts',(10.9247773719869,15.2,-1.10283635395487));
#188988=CARTESIAN_POINT('Ctrl Pts',(10.9287041917207,15.2,-1.10185628481341));
#188989=CARTESIAN_POINT('Ctrl Pts',(10.9355761269235,15.2,-1.10014116364895));
#188990=CARTESIAN_POINT('Ctrl Pts',(10.9424855408517,15.2,-1.09839581517403));
#188991=CARTESIAN_POINT('Ctrl Pts',(10.9494318094776,15.2,-1.09661995645769));
#188992=CARTESIAN_POINT('Ctrl Pts',(10.9563780781035,15.2,-1.09484409774136));
#188993=CARTESIAN_POINT('Ctrl Pts',(10.9633612061443,15.2,-1.09303773123659));
#188994=CARTESIAN_POINT('Ctrl Pts',(10.9703805743807,15.2,-1.09120058480341));
#188995=CARTESIAN_POINT('Ctrl Pts',(10.974391641554,15.2,-1.09015078694376));
#188996=CARTESIAN_POINT('Ctrl Pts',(10.9784145437091,15.2,-1.08909093690485));
#188997=CARTESIAN_POINT('Ctrl Pts',(10.9824491662118,15.2,-1.08802098710409));
#188998=CARTESIAN_POINT('Ctrl Pts',(10.9874924447526,15.2,-1.08668354974381));
#188999=CARTESIAN_POINT('Ctrl Pts',(10.9925540375852,15.2,-1.08533032970142));
#189000=CARTESIAN_POINT('Ctrl Pts',(10.9976337229555,15.2,-1.08396123170913));
#189001=CARTESIAN_POINT('Ctrl Pts',(11.0016974714731,15.2,-1.08286595325561));
#189002=CARTESIAN_POINT('Ctrl Pts',(11.0057728011331,15.2,-1.0817605139156));
#189003=CARTESIAN_POINT('Ctrl Pts',(11.0098595994681,15.2,-1.08064486457597));
#189004=CARTESIAN_POINT('Ctrl Pts',(11.0139463972463,15.2,-1.07952921538835));
#189005=CARTESIAN_POINT('Ctrl Pts',(11.0180446612757,15.2,-1.07840335499095));
#189006=CARTESIAN_POINT('Ctrl Pts',(11.0221542844391,15.2,-1.0772672385845));
#189007=CARTESIAN_POINT('Ctrl Pts',(11.0262639081623,15.2,-1.07613112202326));
#189008=CARTESIAN_POINT('Ctrl Pts',(11.0303848903975,15.2,-1.07498474884832));
#189009=CARTESIAN_POINT('Ctrl Pts',(11.0345171191079,15.2,-1.07382807161549));
#189010=CARTESIAN_POINT('Ctrl Pts',(11.0386493472553,15.2,-1.07267139454025));
#189011=CARTESIAN_POINT('Ctrl Pts',(11.0427928233035,15.2,-1.0715044134215));
#189012=CARTESIAN_POINT('Ctrl Pts',(11.0469474376854,15.2,-1.07032708362953));
#189013=CARTESIAN_POINT('Ctrl Pts',(11.0511020526333,15.2,-1.06914975367716));
#189014=CARTESIAN_POINT('Ctrl Pts',(11.0552678032353,15.2,-1.06796207330966));
#189015=CARTESIAN_POINT('Ctrl Pts',(11.0594445855748,15.2,-1.06676399941035));
#189016=CARTESIAN_POINT('Ctrl Pts',(11.0646655632146,15.2,-1.06526640711783));
#189017=CARTESIAN_POINT('Ctrl Pts',(11.0699037742296,15.2,-1.06375257351661));
#189018=CARTESIAN_POINT('Ctrl Pts',(11.0751590088683,15.2,-1.06222241052237));
#189019=CARTESIAN_POINT('Ctrl Pts',(11.0804142435071,15.2,-1.06069224752812));
#189020=CARTESIAN_POINT('Ctrl Pts',(11.085686500207,15.2,-1.05914575810252));
#189021=CARTESIAN_POINT('Ctrl Pts',(11.0909755714584,15.2,-1.05758285504562));
#189022=CARTESIAN_POINT('Ctrl Pts',(11.0962646427098,15.2,-1.05601995198873));
#189023=CARTESIAN_POINT('Ctrl Pts',(11.1015705294947,15.2,-1.05444063603155));
#189024=CARTESIAN_POINT('Ctrl Pts',(11.1068930224128,15.2,-1.05284482380798));
#189025=CARTESIAN_POINT('Ctrl Pts',(11.1100865180475,15.2,-1.05188733650863));
#189026=CARTESIAN_POINT('Ctrl Pts',(11.1132859934091,15.2,-1.05092390992634));
#189027=CARTESIAN_POINT('Ctrl Pts',(11.1164914026201,15.2,-1.04995452807911));
#189028=CARTESIAN_POINT('Ctrl Pts',(11.1196968118311,15.2,-1.04898514623188));
#189029=CARTESIAN_POINT('Ctrl Pts',(11.1229081549004,15.2,-1.04800980859119));
#189030=CARTESIAN_POINT('Ctrl Pts',(11.1261253888673,15.2,-1.04702849637633));
#189031=CARTESIAN_POINT('Ctrl Pts',(11.1304150339618,15.2,-1.04572008014927));
#189032=CARTESIAN_POINT('Ctrl Pts',(11.1347151492458,15.2,-1.04440104445489));
#189033=CARTESIAN_POINT('Ctrl Pts',(11.1390256325035,15.2,-1.04307134750912));
#189034=CARTESIAN_POINT('Ctrl Pts',(11.1422584956809,15.2,-1.04207407457334));
#189035=CARTESIAN_POINT('Ctrl Pts',(11.1454971902682,15.2,-1.04107080546086));
#189036=CARTESIAN_POINT('Ctrl Pts',(11.1487416724489,15.2,-1.04006152252169));
#189037=CARTESIAN_POINT('Ctrl Pts',(11.1530676477074,15.2,-1.03871581224173));
#189038=CARTESIAN_POINT('Ctrl Pts',(11.1574039136131,15.2,-1.03735941033984));
#189039=CARTESIAN_POINT('Ctrl Pts',(11.1617503655553,15.2,-1.03599227800099));
#189040=CARTESIAN_POINT('Ctrl Pts',(11.1660968180896,15.2,-1.03462514547586));
#189041=CARTESIAN_POINT('Ctrl Pts',(11.1704534570693,15.2,-1.03324728216368));
#189042=CARTESIAN_POINT('Ctrl Pts',(11.1748201801972,15.2,-1.03185864903134));
#189043=CARTESIAN_POINT('Ctrl Pts',(11.1780952222457,15.2,-1.03081717427669));
#189044=CARTESIAN_POINT('Ctrl Pts',(11.1813759363438,15.2,-1.02976964161403));
#189045=CARTESIAN_POINT('Ctrl Pts',(11.1846622803915,15.2,-1.02871603440178));
#189046=CARTESIAN_POINT('Ctrl Pts',(11.1890440722562,15.2,-1.02731122484925));
#189047=CARTESIAN_POINT('Ctrl Pts',(11.1934358715798,15.2,-1.02589561696069));
#189048=CARTESIAN_POINT('Ctrl Pts',(11.1978375783279,15.2,-1.02446917200698));
#189049=CARTESIAN_POINT('Ctrl Pts',(11.2011388585389,15.2,-1.02339933824311));
#189050=CARTESIAN_POINT('Ctrl Pts',(11.2044457104489,15.2,-1.02232340984579));
#189051=CARTESIAN_POINT('Ctrl Pts',(11.2077580930361,15.2,-1.02124136871927));
#189052=CARTESIAN_POINT('Ctrl Pts',(11.2121746035536,15.2,-1.0197986470862));
#189053=CARTESIAN_POINT('Ctrl Pts',(11.2166009468442,15.2,-1.01834506107432));
#189054=CARTESIAN_POINT('Ctrl Pts',(11.2210370194749,15.2,-1.01688057321673));
#189055=CARTESIAN_POINT('Ctrl Pts',(11.2243640736457,15.2,-1.0157822074233));
#189056=CARTESIAN_POINT('Ctrl Pts',(11.2276966025412,15.2,-1.01467770914679));
#189057=CARTESIAN_POINT('Ctrl Pts',(11.2310345626695,15.2,-1.01356706339602));
#189058=CARTESIAN_POINT('Ctrl Pts',(11.2354851765781,15.2,-1.01208620226047));
#189059=CARTESIAN_POINT('Ctrl Pts',(11.2399454473447,15.2,-1.01059441166486));
#189060=CARTESIAN_POINT('Ctrl Pts',(11.2444152754236,15.2,-1.00909165700694));
#189061=CARTESIAN_POINT('Ctrl Pts',(11.2500025602176,15.2,-1.00721321378691));
#189062=CARTESIAN_POINT('Ctrl Pts',(11.2556047793556,15.2,-1.00531763611238));
#189063=CARTESIAN_POINT('Ctrl Pts',(11.2612217390096,15.2,-1.00340485729153));
#189064=CARTESIAN_POINT('Ctrl Pts',(11.2657153063654,15.2,-1.00187463435994));
#189065=CARTESIAN_POINT('Ctrl Pts',(11.2702183086006,15.2,-1.00033340146312));
#189066=CARTESIAN_POINT('Ctrl Pts',(11.2747306478978,15.2,-0.998781125868518));
#189067=CARTESIAN_POINT('Ctrl Pts',(11.2803710724804,15.2,-0.99684078121664));
#189068=CARTESIAN_POINT('Ctrl Pts',(11.2860260859911,15.2,-0.994883180883756));
#189069=CARTESIAN_POINT('Ctrl Pts',(11.2916954988375,15.2,-0.992908257204114));
#189070=CARTESIAN_POINT('Ctrl Pts',(11.2950971464218,15.2,-0.991723303039382));
#189071=CARTESIAN_POINT('Ctrl Pts',(11.2985039771939,15.2,-0.990532113480597));
#189072=CARTESIAN_POINT('Ctrl Pts',(11.3019159523648,15.2,-0.989334673256673));
#189073=CARTESIAN_POINT('Ctrl Pts',(11.3064652530059,15.2,-0.987738086146419));
#189074=CARTESIAN_POINT('Ctrl Pts',(11.3110236965266,15.2,-0.986130387201012));
#189075=CARTESIAN_POINT('Ctrl Pts',(11.3155911871651,15.2,-0.984511545334278));
#189076=CARTESIAN_POINT('Ctrl Pts',(11.3190168048327,15.2,-0.983297414044511));
#189077=CARTESIAN_POINT('Ctrl Pts',(11.3224475114081,15.2,-0.982077013005494));
#189078=CARTESIAN_POINT('Ctrl Pts',(11.3258832674916,15.2,-0.980850330216728));
#189079=CARTESIAN_POINT('Ctrl Pts',(11.330464276019,15.2,-0.979214753016476));
#189080=CARTESIAN_POINT('Ctrl Pts',(11.3350542593975,15.2,-0.977568006920488));
#189081=CARTESIAN_POINT('Ctrl Pts',(11.3396531252602,15.2,-0.975910060495646));
#189082=CARTESIAN_POINT('Ctrl Pts',(11.3431022743439,15.2,-0.974666600789963));
#189083=CARTESIAN_POINT('Ctrl Pts',(11.3465564186382,15.2,-0.973416840274823));
#189084=CARTESIAN_POINT('Ctrl Pts',(11.3500155184359,15.2,-0.972160766506979));
#189085=CARTESIAN_POINT('Ctrl Pts',(11.35462765129,15.2,-0.970486001559251));
#189086=CARTESIAN_POINT('Ctrl Pts',(11.3592485935672,15.2,-0.968800011813104));
#189087=CARTESIAN_POINT('Ctrl Pts',(11.3638782521882,15.2,-0.967102766897035));
#189088=CARTESIAN_POINT('Ctrl Pts',(11.3673504963116,15.2,-0.96582983315217));
#189089=CARTESIAN_POINT('Ctrl Pts',(11.370827642868,15.2,-0.964550568282739));
#189090=CARTESIAN_POINT('Ctrl Pts',(11.3743096535325,15.2,-0.963264959580315));
#189091=CARTESIAN_POINT('Ctrl Pts',(11.3789523348402,15.2,-0.961550814488047));
#189092=CARTESIAN_POINT('Ctrl Pts',(11.383603663864,15.2,-0.95982539096812));
#189093=CARTESIAN_POINT('Ctrl Pts',(11.3882635445281,15.2,-0.958088658532206));
#189094=CARTESIAN_POINT('Ctrl Pts',(11.3917584547087,15.2,-0.956786109323585));
#189095=CARTESIAN_POINT('Ctrl Pts',(11.3952581755082,15.2,-0.955477198759407));
#189096=CARTESIAN_POINT('Ctrl Pts',(11.3987626662301,15.2,-0.954161914509585));
#189097=CARTESIAN_POINT('Ctrl Pts',(11.402267156952,15.2,-0.952846630259763));
#189098=CARTESIAN_POINT('Ctrl Pts',(11.4057764181117,15.2,-0.9515249706459));
#189099=CARTESIAN_POINT('Ctrl Pts',(11.4092904138586,15.2,-0.950196926903042));
#189100=CARTESIAN_POINT('Ctrl Pts',(11.4128044096055,15.2,-0.948868883160183));
#189101=CARTESIAN_POINT('Ctrl Pts',(11.4163231410938,15.2,-0.947534454292763));
#189102=CARTESIAN_POINT('Ctrl Pts',(11.4198465702151,15.2,-0.946193627592354));
#189103=CARTESIAN_POINT('Ctrl Pts',(11.4233699999766,15.2,-0.944852800648362));
#189104=CARTESIAN_POINT('Ctrl Pts',(11.4268981283727,15.2,-0.9435055762359));
#189105=CARTESIAN_POINT('Ctrl Pts',(11.4304309065534,15.2,-0.942151940746629));
#189106=CARTESIAN_POINT('Ctrl Pts',(11.4339636840923,15.2,-0.940798305503269));
#189107=CARTESIAN_POINT('Ctrl Pts',(11.4375011113365,15.2,-0.939438257904982));
#189108=CARTESIAN_POINT('Ctrl Pts',(11.4410431477186,15.2,-0.938071784760617));
#189109=CARTESIAN_POINT('Ctrl Pts',(11.4445851841007,15.2,-0.936705311616251));
#189110=CARTESIAN_POINT('Ctrl Pts',(11.4481318265055,15.2,-0.935332413272528));
#189111=CARTESIAN_POINT('Ctrl Pts',(11.4516830606605,15.2,-0.933953084335651));
#189112=CARTESIAN_POINT('Ctrl Pts',(11.4552342948154,15.2,-0.932573755398775));
#189113=CARTESIAN_POINT('Ctrl Pts',(11.4587901173531,15.2,-0.931187994252923));
#189114=CARTESIAN_POINT('Ctrl Pts',(11.4623505329999,15.2,-0.929795809000016));
#189115=CARTESIAN_POINT('Ctrl Pts',(10.3068855239999,12.2,-1.18690176600001));
#189116=CARTESIAN_POINT('Ctrl Pts',(10.3086714467389,12.2,-1.1869528784395));
#189117=CARTESIAN_POINT('Ctrl Pts',(10.3105146691063,12.2,-1.18700024430173));
#189118=CARTESIAN_POINT('Ctrl Pts',(10.3124142310585,12.2,-1.18704320794532));
#189119=CARTESIAN_POINT('Ctrl Pts',(10.3143229536586,12.2,-1.18708637878131));
#189120=CARTESIAN_POINT('Ctrl Pts',(10.3162885628145,12.2,-1.18712509875838));
#189121=CARTESIAN_POINT('Ctrl Pts',(10.3183101246955,12.2,-1.18715870867826));
#189122=CARTESIAN_POINT('Ctrl Pts',(10.320331686393,12.2,-1.18719231859509));
#189123=CARTESIAN_POINT('Ctrl Pts',(10.3224091993606,12.2,-1.18722081628418));
#189124=CARTESIAN_POINT('Ctrl Pts',(10.3245417522832,12.2,-1.18724356628336));
#189125=CARTESIAN_POINT('Ctrl Pts',(10.3266743052057,12.2,-1.18726631628253));
#189126=CARTESIAN_POINT('Ctrl Pts',(10.3288619009474,12.2,-1.1872833164318));
#189127=CARTESIAN_POINT('Ctrl Pts',(10.3311036480581,12.2,-1.18729394876565));
#189128=CARTESIAN_POINT('Ctrl Pts',(10.3333453953725,12.2,-1.18730458110046));
#189129=CARTESIAN_POINT('Ctrl Pts',(10.3356412985326,12.2,-1.18730884765036));
#189130=CARTESIAN_POINT('Ctrl Pts',(10.3379904907476,12.2,-1.18730614698306));
#189131=CARTESIAN_POINT('Ctrl Pts',(10.3403396827492,12.2,-1.18730344631602));
#189132=CARTESIAN_POINT('Ctrl Pts',(10.3427421643956,12.2,-1.18729378046616));
#189133=CARTESIAN_POINT('Ctrl Pts',(10.3451970944843,12.2,-1.18727656796669));
#189134=CARTESIAN_POINT('Ctrl Pts',(10.347652024573,12.2,-1.18725935546722));
#189135=CARTESIAN_POINT('Ctrl Pts',(10.3501594035892,12.2,-1.18723459877524));
#189136=CARTESIAN_POINT('Ctrl Pts',(10.3527184086606,12.2,-1.18720173402679));
#189137=CARTESIAN_POINT('Ctrl Pts',(10.3557039147322,12.2,-1.18716339181826));
#189138=CARTESIAN_POINT('Ctrl Pts',(10.3587596906992,12.2,-1.18711401306237));
#189139=CARTESIAN_POINT('Ctrl Pts',(10.3618844654844,12.2,-1.18705273574167));
#189140=CARTESIAN_POINT('Ctrl Pts',(10.3645628437327,12.2,-1.18700021232666));
#189141=CARTESIAN_POINT('Ctrl Pts',(10.3672919152934,12.2,-1.18693894571754));
#189142=CARTESIAN_POINT('Ctrl Pts',(10.3700709026069,12.2,-1.1868684142205));
#189143=CARTESIAN_POINT('Ctrl Pts',(10.3747025482978,12.2,-1.18675086172117));
#189144=CARTESIAN_POINT('Ctrl Pts',(10.3794728364098,12.2,-1.18660755852582));
#189145=CARTESIAN_POINT('Ctrl Pts',(10.3843782722652,12.2,-1.18643616977508));
#189146=CARTESIAN_POINT('Ctrl Pts',(10.3878120774175,12.2,-1.18631619764769));
#189147=CARTESIAN_POINT('Ctrl Pts',(10.3913121072864,12.2,-1.18618246645147));
#189148=CARTESIAN_POINT('Ctrl Pts',(10.3948771986916,12.2,-1.18603420401806));
#189149=CARTESIAN_POINT('Ctrl Pts',(10.3984422898192,12.2,-1.1858859415962));
#189150=CARTESIAN_POINT('Ctrl Pts',(10.4020724431775,12.2,-1.18572315146579));
#189151=CARTESIAN_POINT('Ctrl Pts',(10.4057665268881,12.2,-1.18554508674167));
#189152=CARTESIAN_POINT('Ctrl Pts',(10.4094606108863,12.2,-1.18536702200368));
#189153=CARTESIAN_POINT('Ctrl Pts',(10.4132186242088,12.2,-1.18517368689576));
#189154=CARTESIAN_POINT('Ctrl Pts',(10.4170394620716,12.2,-1.18496435772643));
#189155=CARTESIAN_POINT('Ctrl Pts',(10.4203144660814,12.2,-1.18478493271717));
#189156=CARTESIAN_POINT('Ctrl Pts',(10.4236356273469,12.2,-1.18459376083978));
#189157=CARTESIAN_POINT('Ctrl Pts',(10.4270022663668,12.2,-1.18439039899453));
#189158=CARTESIAN_POINT('Ctrl Pts',(10.4303689050809,12.2,-1.18418703716776));
#189159=CARTESIAN_POINT('Ctrl Pts',(10.4337810208038,12.2,-1.18397148993814));
#189160=CARTESIAN_POINT('Ctrl Pts',(10.4372379484301,12.2,-1.18374332602921));
#189161=CARTESIAN_POINT('Ctrl Pts',(10.4406948760565,12.2,-1.18351516212029));
#189162=CARTESIAN_POINT('Ctrl Pts',(10.4441966131543,12.2,-1.18327438392903));
#189163=CARTESIAN_POINT('Ctrl Pts',(10.4477425090235,12.2,-1.18302057602215));
#189164=CARTESIAN_POINT('Ctrl Pts',(10.4512884048927,12.2,-1.18276676811527));
#189165=CARTESIAN_POINT('Ctrl Pts',(10.4548784581555,12.2,-1.18249993024449));
#189166=CARTESIAN_POINT('Ctrl Pts',(10.4585120298538,12.2,-1.18221965850558));
#189167=CARTESIAN_POINT('Ctrl Pts',(10.4621456018822,12.2,-1.18193938674122));
#189168=CARTESIAN_POINT('Ctrl Pts',(10.4658226908315,12.2,-1.18164568290891));
#189169=CARTESIAN_POINT('Ctrl Pts',(10.4695426682028,12.2,-1.18133815030822));
#189170=CARTESIAN_POINT('Ctrl Pts',(10.4738826412958,12.2,-1.18097936231598));
#189171=CARTESIAN_POINT('Ctrl Pts',(10.4782809922367,12.2,-1.1806017551446));
#189172=CARTESIAN_POINT('Ctrl Pts',(10.4827367418169,12.2,-1.18020472129546));
#189173=CARTESIAN_POINT('Ctrl Pts',(10.4865559561889,12.2,-1.17986440652789));
#189174=CARTESIAN_POINT('Ctrl Pts',(10.4904173410482,12.2,-1.17950981866728));
#189175=CARTESIAN_POINT('Ctrl Pts',(10.4943202954294,12.2,-1.17914058897986));
#189176=CARTESIAN_POINT('Ctrl Pts',(10.4982232494561,12.2,-1.17877135932597));
#189177=CARTESIAN_POINT('Ctrl Pts',(10.5021677700582,12.2,-1.17838748677917));
#189178=CARTESIAN_POINT('Ctrl Pts',(10.5061532662647,12.2,-1.17798861020855));
#189179=CARTESIAN_POINT('Ctrl Pts',(10.5101387624713,12.2,-1.17758973363794));
#189180=CARTESIAN_POINT('Ctrl Pts',(10.5141652357321,12.2,-1.17717585342185));
#189181=CARTESIAN_POINT('Ctrl Pts',(10.5182321009983,12.2,-1.17674661685516));
#189182=CARTESIAN_POINT('Ctrl Pts',(10.5216211555099,12.2,-1.17638891970325));
#189183=CARTESIAN_POINT('Ctrl Pts',(10.5250382617855,12.2,-1.17602056038444));
#189184=CARTESIAN_POINT('Ctrl Pts',(10.5284830880667,12.2,-1.17564133751903));
#189185=CARTESIAN_POINT('Ctrl Pts',(10.531927914348,12.2,-1.17526211465361));
#189186=CARTESIAN_POINT('Ctrl Pts',(10.5354004603837,12.2,-1.17487203125341));
#189187=CARTESIAN_POINT('Ctrl Pts',(10.5389003990628,12.2,-1.17447088930954));
#189188=CARTESIAN_POINT('Ctrl Pts',(10.5424003377419,12.2,-1.17406974736568));
#189189=CARTESIAN_POINT('Ctrl Pts',(10.5459276698968,12.2,-1.17365755007708));
#189190=CARTESIAN_POINT('Ctrl Pts',(10.5494820735759,12.2,-1.17323410549433));
#189191=CARTESIAN_POINT('Ctrl Pts',(10.5530364772551,12.2,-1.17281066091159));
#189192=CARTESIAN_POINT('Ctrl Pts',(10.5566179502372,12.2,-1.1723759701245));
#189193=CARTESIAN_POINT('Ctrl Pts',(10.5602261780312,12.2,-1.17192984477528));
#189194=CARTESIAN_POINT('Ctrl Pts',(10.5645560512268,12.2,-1.17139449437567));
#189195=CARTESIAN_POINT('Ctrl Pts',(10.5689244484073,12.2,-1.17084268066522));
#189196=CARTESIAN_POINT('Ctrl Pts',(10.5733308288279,12.2,-1.17027408827035));
#189197=CARTESIAN_POINT('Ctrl Pts',(10.5770028126452,12.2,-1.16980026125741));
#189198=CARTESIAN_POINT('Ctrl Pts',(10.5807011750889,12.2,-1.16931478338731));
#189199=CARTESIAN_POINT('Ctrl Pts',(10.5844256065926,12.2,-1.16881747551607));
#189200=CARTESIAN_POINT('Ctrl Pts',(10.5881500380963,12.2,-1.16832016764482));
#189201=CARTESIAN_POINT('Ctrl Pts',(10.5919005384933,12.2,-1.16781102958898));
#189202=CARTESIAN_POINT('Ctrl Pts',(10.5956768039781,12.2,-1.16728988924239));
#189203=CARTESIAN_POINT('Ctrl Pts',(10.6002083228068,12.2,-1.16666452079239));
#189204=CARTESIAN_POINT('Ctrl Pts',(10.6047769440901,12.2,-1.16602186619859));
#189205=CARTESIAN_POINT('Ctrl Pts',(10.6093821487602,12.2,-1.16536163366141));
#189206=CARTESIAN_POINT('Ctrl Pts',(10.6132198186912,12.2,-1.16481143997038));
#189207=CARTESIAN_POINT('Ctrl Pts',(10.6170828927727,12.2,-1.16424903848934));
#189208=CARTESIAN_POINT('Ctrl Pts',(10.6209710769996,12.2,-1.16367426181689));
#189209=CARTESIAN_POINT('Ctrl Pts',(10.6256368988348,12.2,-1.16298452969717));
#189210=CARTESIAN_POINT('Ctrl Pts',(10.6303388777568,12.2,-1.16227698215076));
#189211=CARTESIAN_POINT('Ctrl Pts',(10.6350765097666,12.2,-1.16155133294376));
#189212=CARTESIAN_POINT('Ctrl Pts',(10.6390245362262,12.2,-1.16094662530421));
#189213=CARTESIAN_POINT('Ctrl Pts',(10.6429973231491,12.2,-1.16032934789832));
#189214=CARTESIAN_POINT('Ctrl Pts',(10.6469945805114,12.2,-1.1596993442171));
#189215=CARTESIAN_POINT('Ctrl Pts',(10.6509918378738,12.2,-1.15906934053588));
#189216=CARTESIAN_POINT('Ctrl Pts',(10.6550135686936,12.2,-1.1584266083631));
#189217=CARTESIAN_POINT('Ctrl Pts',(10.6590594854946,12.2,-1.15777099235723));
#189218=CARTESIAN_POINT('Ctrl Pts',(10.6631054022957,12.2,-1.15711537635136));
#189219=CARTESIAN_POINT('Ctrl Pts',(10.6671755061057,12.2,-1.15644687772863));
#189220=CARTESIAN_POINT('Ctrl Pts',(10.6712695182604,12.2,-1.15576534189423));
#189221=CARTESIAN_POINT('Ctrl Pts',(10.6745447277164,12.2,-1.15522011327129));
#189222=CARTESIAN_POINT('Ctrl Pts',(10.6778352370121,12.2,-1.15466654257442));
#189223=CARTESIAN_POINT('Ctrl Pts',(10.6811409039631,12.2,-1.15410455178758));
#189224=CARTESIAN_POINT('Ctrl Pts',(10.6844465713645,12.2,-1.15354256092416));
#189225=CARTESIAN_POINT('Ctrl Pts',(10.6877673976315,12.2,-1.15297214976888));
#189226=CARTESIAN_POINT('Ctrl Pts',(10.691103241259,12.2,-1.15239324420766));
#189227=CARTESIAN_POINT('Ctrl Pts',(10.6944390844321,12.2,-1.15181433872533));
#189228=CARTESIAN_POINT('Ctrl Pts',(10.6977899454288,12.2,-1.15122693717163));
#189229=CARTESIAN_POINT('Ctrl Pts',(10.7011556830415,12.2,-1.15063096699869));
#189230=CARTESIAN_POINT('Ctrl Pts',(10.7045214211129,12.2,-1.15003499674455));
#189231=CARTESIAN_POINT('Ctrl Pts',(10.7079020375721,12.2,-1.14943045601438));
#189232=CARTESIAN_POINT('Ctrl Pts',(10.7112973930359,12.2,-1.14881727392484));
#189233=CARTESIAN_POINT('Ctrl Pts',(10.7146927480371,12.2,-1.14820409191885));
#189234=CARTESIAN_POINT('Ctrl Pts',(10.7181028429409,12.2,-1.1475822676318));
#189235=CARTESIAN_POINT('Ctrl Pts',(10.721527540053,12.2,-1.14695172887483));
#189236=CARTESIAN_POINT('Ctrl Pts',(10.7249522376317,12.2,-1.14632119003194));
#189237=CARTESIAN_POINT('Ctrl Pts',(10.7283915370043,12.2,-1.14568193657732));
#189238=CARTESIAN_POINT('Ctrl Pts',(10.731845303749,12.2,-1.14503389843032));
#189239=CARTESIAN_POINT('Ctrl Pts',(10.7352990700232,12.2,-1.14438586037162));
#189240=CARTESIAN_POINT('Ctrl Pts',(10.7387673020111,12.2,-1.14372903703689));
#189241=CARTESIAN_POINT('Ctrl Pts',(10.7422498669472,12.2,-1.14306335909222));
#189242=CARTESIAN_POINT('Ctrl Pts',(10.7457324323577,12.2,-1.14239768105684));
#189243=CARTESIAN_POINT('Ctrl Pts',(10.7492293293088,12.2,-1.14172314853441));
#189244=CARTESIAN_POINT('Ctrl Pts',(10.7527404247939,12.2,-1.14103969304958));
#189245=CARTESIAN_POINT('Ctrl Pts',(10.7562515198007,12.2,-1.14035623765788));
#189246=CARTESIAN_POINT('Ctrl Pts',(10.7597768145676,12.2,-1.13966385812035));
#189247=CARTESIAN_POINT('Ctrl Pts',(10.7633161743879,12.2,-1.13896248878972));
#189248=CARTESIAN_POINT('Ctrl Pts',(10.7668555346904,12.2,-1.13826111936352));
#189249=CARTESIAN_POINT('Ctrl Pts',(10.7704089617499,12.2,-1.13755076002815));
#189250=CARTESIAN_POINT('Ctrl Pts',(10.7739763244999,12.2,-1.13683134276672));
#189251=CARTESIAN_POINT('Ctrl Pts',(10.7775436872499,12.2,-1.13611192550529));
#189252=CARTESIAN_POINT('Ctrl Pts',(10.7811249844654,12.2,-1.13538345173447));
#189253=CARTESIAN_POINT('Ctrl Pts',(10.7847200878294,12.2,-1.13464585563778));
#189254=CARTESIAN_POINT('Ctrl Pts',(10.7883151907035,12.2,-1.13390825964159));
#189255=CARTESIAN_POINT('Ctrl Pts',(10.7919240985688,12.2,-1.13316154130606));
#189256=CARTESIAN_POINT('Ctrl Pts',(10.7955466824558,12.2,-1.1324056373089));
#189257=CARTESIAN_POINT('Ctrl Pts',(10.7991692668363,12.2,-1.13164973320875));
#189258=CARTESIAN_POINT('Ctrl Pts',(10.8028055286936,12.2,-1.13088464063048));
#189259=CARTESIAN_POINT('Ctrl Pts',(10.8064553388383,12.2,-1.13011029986511));
#189260=CARTESIAN_POINT('Ctrl Pts',(10.8101051484858,12.2,-1.12933595920524));
#189261=CARTESIAN_POINT('Ctrl Pts',(10.8137685064204,12.2,-1.12855236811046));
#189262=CARTESIAN_POINT('Ctrl Pts',(10.8174452861744,12.2,-1.12775946606478));
#189263=CARTESIAN_POINT('Ctrl Pts',(10.8211220664295,12.2,-1.12696656391107));
#189264=CARTESIAN_POINT('Ctrl Pts',(10.8248122687716,12.2,-1.12616434821782));
#189265=CARTESIAN_POINT('Ctrl Pts',(10.8285157672707,12.2,-1.12535276013223));
#189266=CARTESIAN_POINT('Ctrl Pts',(10.8322192652652,12.2,-1.12454117215722));
#189267=CARTESIAN_POINT('Ctrl Pts',(10.8359360607037,12.2,-1.12372021039935));
#189268=CARTESIAN_POINT('Ctrl Pts',(10.8396660264534,12.2,-1.12288981580118));
#189269=CARTESIAN_POINT('Ctrl Pts',(10.8433959927114,12.2,-1.12205942108987));
#189270=CARTESIAN_POINT('Ctrl Pts',(10.8471391311238,12.2,-1.12121959159133));
#189271=CARTESIAN_POINT('Ctrl Pts',(10.8508953167738,12.2,-1.12037027015553));
#189272=CARTESIAN_POINT('Ctrl Pts',(10.854651501912,12.2,-1.11952094883545));
#189273=CARTESIAN_POINT('Ctrl Pts',(10.8584207350364,12.2,-1.11866213436979));
#189274=CARTESIAN_POINT('Ctrl Pts',(10.8622028941928,12.2,-1.11779376784267));
#189275=CARTESIAN_POINT('Ctrl Pts',(10.8669305935248,12.2,-1.11670830959504));
#189276=CARTESIAN_POINT('Ctrl Pts',(10.8716784864726,12.2,-1.11560792717213));
#189277=CARTESIAN_POINT('Ctrl Pts',(10.8764463389715,12.2,-1.11449250883958));
#189278=CARTESIAN_POINT('Ctrl Pts',(10.8812141914705,12.2,-1.11337709050703));
#189279=CARTESIAN_POINT('Ctrl Pts',(10.8860020013255,12.2,-1.11224663584076));
#189280=CARTESIAN_POINT('Ctrl Pts',(10.8908095347273,12.2,-1.11110103354988));
#189281=CARTESIAN_POINT('Ctrl Pts',(10.8946555616583,12.2,-1.11018455166724));
#189282=CARTESIAN_POINT('Ctrl Pts',(10.8985142108396,12.2,-1.10925837747114));
#189283=CARTESIAN_POINT('Ctrl Pts',(10.9023853645784,12.2,-1.10832245287252));
#189284=CARTESIAN_POINT('Ctrl Pts',(10.9062565177897,12.2,-1.10738652840143));
#189285=CARTESIAN_POINT('Ctrl Pts',(10.9101401724564,12.2,-1.10644085726321));
#189286=CARTESIAN_POINT('Ctrl Pts',(10.9140362129148,12.2,-1.1054853802864));
#189287=CARTESIAN_POINT('Ctrl Pts',(10.9179322539042,12.2,-1.10452990317942));
#189288=CARTESIAN_POINT('Ctrl Pts',(10.9218406801116,12.2,-1.10356462396292));
#189289=CARTESIAN_POINT('Ctrl Pts',(10.9257613737705,12.2,-1.10258948668691));
#189290=CARTESIAN_POINT('Ctrl Pts',(10.9296820668953,12.2,-1.10161434954376));
#189291=CARTESIAN_POINT('Ctrl Pts',(10.9336150272564,12.2,-1.10062935446093));
#189292=CARTESIAN_POINT('Ctrl Pts',(10.9375601378215,12.2,-1.09963445115438));
#189293=CARTESIAN_POINT('Ctrl Pts',(10.9415052489242,12.2,-1.09863954771228));
#189294=CARTESIAN_POINT('Ctrl Pts',(10.9454625129654,12.2,-1.09763473290653));
#189295=CARTESIAN_POINT('Ctrl Pts',(10.9494318094776,12.2,-1.09661995645769));
#189296=CARTESIAN_POINT('Ctrl Pts',(10.953401105449,12.2,-1.09560518014712));
#189297=CARTESIAN_POINT('Ctrl Pts',(10.9573824380636,12.2,-1.09458044427528));
#189298=CARTESIAN_POINT('Ctrl Pts',(10.961375689847,12.2,-1.09354569319423));
#189299=CARTESIAN_POINT('Ctrl Pts',(10.9653689421745,12.2,-1.0925109419722));
#189300=CARTESIAN_POINT('Ctrl Pts',(10.9693741134838,12.2,-1.09146617794366));
#189301=CARTESIAN_POINT('Ctrl Pts',(10.9733910917582,12.2,-1.09041135127506));
#189302=CARTESIAN_POINT('Ctrl Pts',(10.9774080700327,12.2,-1.08935652460646));
#189303=CARTESIAN_POINT('Ctrl Pts',(10.9814368537308,12.2,-1.08829163308946));
#189304=CARTESIAN_POINT('Ctrl Pts',(10.9854773301189,12.2,-1.08721662980762));
#189305=CARTESIAN_POINT('Ctrl Pts',(10.9895178059564,12.2,-1.08614162667225));
#189306=CARTESIAN_POINT('Ctrl Pts',(10.9935699749915,12.2,-1.08505651001342));
#189307=CARTESIAN_POINT('Ctrl Pts',(10.9976337229555,12.2,-1.08396123170913));
#189308=CARTESIAN_POINT('Ctrl Pts',(11.0016974714731,12.2,-1.08286595325561));
#189309=CARTESIAN_POINT('Ctrl Pts',(11.0057728011331,12.2,-1.0817605139156));
#189310=CARTESIAN_POINT('Ctrl Pts',(11.0098595994681,12.2,-1.08064486457597));
#189311=CARTESIAN_POINT('Ctrl Pts',(11.0139463972463,12.2,-1.07952921538835));
#189312=CARTESIAN_POINT('Ctrl Pts',(11.0180446612757,12.2,-1.07840335499096));
#189313=CARTESIAN_POINT('Ctrl Pts',(11.0221542844391,12.2,-1.0772672385845));
#189314=CARTESIAN_POINT('Ctrl Pts',(11.0262639081623,12.2,-1.07613112202326));
#189315=CARTESIAN_POINT('Ctrl Pts',(11.0303848903975,12.2,-1.07498474884832));
#189316=CARTESIAN_POINT('Ctrl Pts',(11.0345171191079,12.2,-1.07382807161549));
#189317=CARTESIAN_POINT('Ctrl Pts',(11.0386493472553,12.2,-1.07267139454025));
#189318=CARTESIAN_POINT('Ctrl Pts',(11.0427928233035,12.2,-1.0715044134215));
#189319=CARTESIAN_POINT('Ctrl Pts',(11.0469474376854,12.2,-1.07032708362954));
#189320=CARTESIAN_POINT('Ctrl Pts',(11.0521407060873,12.2,-1.06885542126927));
#189321=CARTESIAN_POINT('Ctrl Pts',(11.0573513752257,12.2,-1.06736758688081));
#189322=CARTESIAN_POINT('Ctrl Pts',(11.0625792379331,12.2,-1.06586349458999));
#189323=CARTESIAN_POINT('Ctrl Pts',(11.066761528327,12.2,-1.06466022069176));
#189324=CARTESIAN_POINT('Ctrl Pts',(11.0709548209282,12.2,-1.06344654098448));
#189325=CARTESIAN_POINT('Ctrl Pts',(11.0751590088683,12.2,-1.06222241052237));
#189326=CARTESIAN_POINT('Ctrl Pts',(11.0793631962356,12.2,-1.06099828022705));
#189327=CARTESIAN_POINT('Ctrl Pts',(11.0835782770924,12.2,-1.05976370136038));
#189328=CARTESIAN_POINT('Ctrl Pts',(11.0878041469129,12.2,-1.05851862835174));
#189329=CARTESIAN_POINT('Ctrl Pts',(11.0930864846203,12.2,-1.05696228696371));
#189330=CARTESIAN_POINT('Ctrl Pts',(11.0983856782588,12.2,-1.05538954888081));
#189331=CARTESIAN_POINT('Ctrl Pts',(11.1037015202023,12.2,-1.05380033235389));
#189332=CARTESIAN_POINT('Ctrl Pts',(11.1068910252526,12.2,-1.05284680247239));
#189333=CARTESIAN_POINT('Ctrl Pts',(11.110086523671,12.2,-1.05188733901591));
#189334=CARTESIAN_POINT('Ctrl Pts',(11.1132879718806,12.2,-1.05092192567011));
#189335=CARTESIAN_POINT('Ctrl Pts',(11.1164894200902,12.2,-1.04995651232432));
#189336=CARTESIAN_POINT('Ctrl Pts',(11.119696816717,12.2,-1.04898514954345));
#189337=CARTESIAN_POINT('Ctrl Pts',(11.1229101187661,12.2,-1.04800781824644));
#189338=CARTESIAN_POINT('Ctrl Pts',(11.1261234213989,12.2,-1.04703048677189));
#189339=CARTESIAN_POINT('Ctrl Pts',(11.1293426287668,12.2,-1.04604718699565));
#189340=CARTESIAN_POINT('Ctrl Pts',(11.132567696903,12.2,-1.04505790205939));
#189341=CARTESIAN_POINT('Ctrl Pts',(11.1357927644532,12.2,-1.04406861730285));
#189342=CARTESIAN_POINT('Ctrl Pts',(11.1390236931199,12.2,-1.04307334710496));
#189343=CARTESIAN_POINT('Ctrl Pts',(11.1422604386278,12.2,-1.04207207484915));
#189344=CARTESIAN_POINT('Ctrl Pts',(11.1454971841357,12.2,-1.04107080259334));
#189345=CARTESIAN_POINT('Ctrl Pts',(11.1487397456894,12.2,-1.04006352855028));
#189346=CARTESIAN_POINT('Ctrl Pts',(11.1519880812529,12.2,-1.03905023474914));
#189347=CARTESIAN_POINT('Ctrl Pts',(11.1552364168163,12.2,-1.03803694094799));
#189348=CARTESIAN_POINT('Ctrl Pts',(11.1584905264506,12.2,-1.03701762730169));
#189349=CARTESIAN_POINT('Ctrl Pts',(11.1617503655553,12.2,-1.03599227800099));
#189350=CARTESIAN_POINT('Ctrl Pts',(11.1650102046599,12.2,-1.03496692870028));
#189351=CARTESIAN_POINT('Ctrl Pts',(11.1682757737628,12.2,-1.03393554315815));
#189352=CARTESIAN_POINT('Ctrl Pts',(11.1715470293934,12.2,-1.03289810536304));
#189353=CARTESIAN_POINT('Ctrl Pts',(11.1748182850241,12.2,-1.03186066756792));
#189354=CARTESIAN_POINT('Ctrl Pts',(11.1780952271543,12.2,-1.03081717702322));
#189355=CARTESIAN_POINT('Ctrl Pts',(11.1813778132426,12.2,-1.02976761772886));
#189356=CARTESIAN_POINT('Ctrl Pts',(11.1846603999273,12.2,-1.02871805824382));
#189357=CARTESIAN_POINT('Ctrl Pts',(11.1879486305718,12.2,-1.02766242975706));
#189358=CARTESIAN_POINT('Ctrl Pts',(11.191242462218,12.2,-1.02660071631026));
#189359=CARTESIAN_POINT('Ctrl Pts',(11.1945362932657,12.2,-1.02553900305635));
#189360=CARTESIAN_POINT('Ctrl Pts',(11.197835725427,12.2,-1.02447120432423));
#189361=CARTESIAN_POINT('Ctrl Pts',(11.2011407156811,12.2,-1.02339730547556));
#189362=CARTESIAN_POINT('Ctrl Pts',(11.2044457059351,12.2,-1.02232340662689));
#189363=CARTESIAN_POINT('Ctrl Pts',(11.2077562537648,12.2,-1.0212434064093));
#189364=CARTESIAN_POINT('Ctrl Pts',(11.2110723188531,12.2,-1.0201572896149));
#189365=CARTESIAN_POINT('Ctrl Pts',(11.2143883839414,12.2,-1.0190711728205));
#189366=CARTESIAN_POINT('Ctrl Pts',(11.2177099653041,12.2,-1.01797893901015));
#189367=CARTESIAN_POINT('Ctrl Pts',(11.2210370194749,12.2,-1.01688057321673));
#189368=CARTESIAN_POINT('Ctrl Pts',(11.2243640736457,12.2,-1.0157822074233));
#189369=CARTESIAN_POINT('Ctrl Pts',(11.2276966025412,12.2,-1.01467770914679));
#189370=CARTESIAN_POINT('Ctrl Pts',(11.2310345626695,12.2,-1.01356706339602));
#189371=CARTESIAN_POINT('Ctrl Pts',(11.2343725227977,12.2,-1.01245641764524));
#189372=CARTESIAN_POINT('Ctrl Pts',(11.2377159145737,12.2,-1.01133962443184));
#189373=CARTESIAN_POINT('Ctrl Pts',(11.2410646968271,12.2,-1.01021666820893));
#189374=CARTESIAN_POINT('Ctrl Pts',(11.2444134790804,12.2,-1.00909371198601));
#189375=CARTESIAN_POINT('Ctrl Pts',(11.247767650407,12.2,-1.00796459388879));
#189376=CARTESIAN_POINT('Ctrl Pts',(11.2511271709925,12.2,-1.00682929672255));
#189377=CARTESIAN_POINT('Ctrl Pts',(11.2544866921884,12.2,-1.00569399935006));
#189378=CARTESIAN_POINT('Ctrl Pts',(11.2578515627274,12.2,-1.00455252475083));
#189379=CARTESIAN_POINT('Ctrl Pts',(11.2612217390096,12.2,-1.00340485729153));
#189380=CARTESIAN_POINT('Ctrl Pts',(11.2657153063654,12.2,-1.00187463435994));
#189381=CARTESIAN_POINT('Ctrl Pts',(11.2702183086006,12.2,-1.00033340146312));
#189382=CARTESIAN_POINT('Ctrl Pts',(11.2747306478978,12.2,-0.998781125868519));
#189383=CARTESIAN_POINT('Ctrl Pts',(11.2781149025244,12.2,-0.997616919119692));
#189384=CARTESIAN_POINT('Ctrl Pts',(11.2815044093506,12.2,-0.996446500179626));
#189385=CARTESIAN_POINT('Ctrl Pts',(11.2848991269765,12.2,-0.995269854514894));
#189386=CARTESIAN_POINT('Ctrl Pts',(11.2882938452192,12.2,-0.994093208636405));
#189387=CARTESIAN_POINT('Ctrl Pts',(11.2916937747633,12.2,-0.992910336514494));
#189388=CARTESIAN_POINT('Ctrl Pts',(11.2950988740506,12.2,-0.991721223174159));
#189389=CARTESIAN_POINT('Ctrl Pts',(11.2985039727192,12.2,-0.990532110049847));
#189390=CARTESIAN_POINT('Ctrl Pts',(11.301914242547,12.2,-0.989336757217945));
#189391=CARTESIAN_POINT('Ctrl Pts',(11.3053296414274,12.2,-0.988135148492515));
#189392=CARTESIAN_POINT('Ctrl Pts',(11.3087450403079,12.2,-0.986933539767085));
#189393=CARTESIAN_POINT('Ctrl Pts',(11.3121655694974,12.2,-0.985725676624046));
#189394=CARTESIAN_POINT('Ctrl Pts',(11.3155911871651,12.2,-0.984511545334279));
#189395=CARTESIAN_POINT('Ctrl Pts',(11.3190168048327,12.2,-0.983297414044512));
#189396=CARTESIAN_POINT('Ctrl Pts',(11.3224475114081,12.2,-0.982077013005498));
#189397=CARTESIAN_POINT('Ctrl Pts',(11.3258832674916,12.2,-0.980850330216732));
#189398=CARTESIAN_POINT('Ctrl Pts',(11.3293190235751,12.2,-0.979623647427967));
#189399=CARTESIAN_POINT('Ctrl Pts',(11.3327598275334,12.2,-0.978390681672795));
#189400=CARTESIAN_POINT('Ctrl Pts',(11.3362056416161,12.2,-0.977151420885035));
#189401=CARTESIAN_POINT('Ctrl Pts',(11.3396514556988,12.2,-0.975912160097274));
#189402=CARTESIAN_POINT('Ctrl Pts',(11.3431022787682,12.2,-0.974666603008525));
#189403=CARTESIAN_POINT('Ctrl Pts',(11.3465580705647,12.2,-0.973414736742201));
#189404=CARTESIAN_POINT('Ctrl Pts',(11.3500138623612,12.2,-0.972162870475877));
#189405=CARTESIAN_POINT('Ctrl Pts',(11.3534746225543,12.2,-0.970904695462241));
#189406=CARTESIAN_POINT('Ctrl Pts',(11.3569403117611,12.2,-0.969640197300713));
#189407=CARTESIAN_POINT('Ctrl Pts',(11.3604060015974,12.2,-0.968375698909467));
#189408=CARTESIAN_POINT('Ctrl Pts',(11.3638766215518,12.2,-0.967104878091442));
#189409=CARTESIAN_POINT('Ctrl Pts',(11.3673521299742,12.2,-0.965827721738297));
#189410=CARTESIAN_POINT('Ctrl Pts',(11.3719861401519,12.2,-0.964124846987467));
#189411=CARTESIAN_POINT('Ctrl Pts',(11.3766288443144,12.2,-0.962410710032548));
#189412=CARTESIAN_POINT('Ctrl Pts',(11.3812801488781,12.2,-0.960685279174338));
#189413=CARTESIAN_POINT('Ctrl Pts',(11.3847686274593,12.2,-0.959391205971909));
#189414=CARTESIAN_POINT('Ctrl Pts',(11.3882619432427,12.2,-0.958090780169896));
#189415=CARTESIAN_POINT('Ctrl Pts',(11.3917600560398,12.2,-0.956783988486161));
#189416=CARTESIAN_POINT('Ctrl Pts',(11.3952581688369,12.2,-0.955477196802426));
#189417=CARTESIAN_POINT('Ctrl Pts',(11.39876107808,12.2,-0.9541640406389));
#189418=CARTESIAN_POINT('Ctrl Pts',(11.4022687452436,12.2,-0.952844505062712));
#189419=CARTESIAN_POINT('Ctrl Pts',(11.4057764130444,12.2,-0.951524969246809));
#189420=CARTESIAN_POINT('Ctrl Pts',(11.4092888387048,12.2,-0.950199056087446));
#189421=CARTESIAN_POINT('Ctrl Pts',(11.4128059880083,12.2,-0.948866753726278));
#189422=CARTESIAN_POINT('Ctrl Pts',(11.4163231366728,12.2,-0.947534451607146));
#189423=CARTESIAN_POINT('Ctrl Pts',(11.4198450088788,12.2,-0.94619576065502));
#189424=CARTESIAN_POINT('Ctrl Pts',(11.4233715648761,12.2,-0.944850667078338));
#189425=CARTESIAN_POINT('Ctrl Pts',(11.4268981208733,12.2,-0.943505573501657));
#189426=CARTESIAN_POINT('Ctrl Pts',(11.4304293590655,12.2,-0.942154079389015));
#189427=CARTESIAN_POINT('Ctrl Pts',(11.4339652317448,12.2,-0.940796167723825));
#189428=CARTESIAN_POINT('Ctrl Pts',(11.4375011044241,12.2,-0.939438256058633));
#189429=CARTESIAN_POINT('Ctrl Pts',(11.4410416129428,12.2,-0.938073927057691));
#189430=CARTESIAN_POINT('Ctrl Pts',(11.4445867185384,12.2,-0.936703169976301));
#189431=CARTESIAN_POINT('Ctrl Pts',(11.450495228079,12.2,-0.934418574757642));
#189432=CARTESIAN_POINT('Ctrl Pts',(11.4564165067063,12.2,-0.932116117839165));
#189433=CARTESIAN_POINT('Ctrl Pts',(11.4623505329999,12.2,-0.929795809000016));
#189434=CARTESIAN_POINT('Ctrl Pts',(11.4869855309999,15.2,-0.546958306000014));
#189435=CARTESIAN_POINT('Ctrl Pts',(11.4869855309999,11.6,-0.546958306000014));
#189436=CARTESIAN_POINT('Ctrl Pts',(11.4863150069999,15.2,-0.546590899000012));
#189437=CARTESIAN_POINT('Ctrl Pts',(11.4863150069999,11.6,-0.546590899000013));
#189438=CARTESIAN_POINT('Ctrl Pts',(11.4849742089999,15.2,-0.545856552000017));
#189439=CARTESIAN_POINT('Ctrl Pts',(11.4849742089999,11.6,-0.545856552000017));
#189440=CARTESIAN_POINT('Ctrl Pts',(11.4829637559999,15.2,-0.544756422000017));
#189441=CARTESIAN_POINT('Ctrl Pts',(11.4829637559999,11.6,-0.544756422000017));
#189442=CARTESIAN_POINT('Ctrl Pts',(11.4802846429999,15.2,-0.543292368000015));
#189443=CARTESIAN_POINT('Ctrl Pts',(11.4802846429999,11.6,-0.543292368000015));
#189444=CARTESIAN_POINT('Ctrl Pts',(11.4769382369999,15.2,-0.541466945000018));
#189445=CARTESIAN_POINT('Ctrl Pts',(11.4769382369999,11.6,-0.541466945000018));
#189446=CARTESIAN_POINT('Ctrl Pts',(11.4735943179999,15.2,-0.539646167000014));
#189447=CARTESIAN_POINT('Ctrl Pts',(11.4735943179999,11.6,-0.539646167000015));
#189448=CARTESIAN_POINT('Ctrl Pts',(11.4702528869999,15.2,-0.537830030000013));
#189449=CARTESIAN_POINT('Ctrl Pts',(11.4702528869999,11.6,-0.537830030000013));
#189450=CARTESIAN_POINT('Ctrl Pts',(11.4669139489999,15.2,-0.536018536000018));
#189451=CARTESIAN_POINT('Ctrl Pts',(11.4669139489999,11.6,-0.536018536000018));
#189452=CARTESIAN_POINT('Ctrl Pts',(11.4635775099999,15.2,-0.534211685000017));
#189453=CARTESIAN_POINT('Ctrl Pts',(11.4635775099999,11.6,-0.534211685000017));
#189454=CARTESIAN_POINT('Ctrl Pts',(11.4602435779999,15.2,-0.532409474000013));
#189455=CARTESIAN_POINT('Ctrl Pts',(11.4602435779999,11.6,-0.532409474000013));
#189456=CARTESIAN_POINT('Ctrl Pts',(11.4569121619999,15.2,-0.530611901000011));
#189457=CARTESIAN_POINT('Ctrl Pts',(11.4569121619999,11.6,-0.530611901000011));
#189458=CARTESIAN_POINT('Ctrl Pts',(11.4535832719999,15.2,-0.528818965000015));
#189459=CARTESIAN_POINT('Ctrl Pts',(11.4535832719999,11.6,-0.528818965000016));
#189460=CARTESIAN_POINT('Ctrl Pts',(11.4502569209999,15.2,-0.527030665000012));
#189461=CARTESIAN_POINT('Ctrl Pts',(11.4502569209999,11.6,-0.527030665000013));
#189462=CARTESIAN_POINT('Ctrl Pts',(11.4469331179999,15.2,-0.525246997000015));
#189463=CARTESIAN_POINT('Ctrl Pts',(11.4469331179999,11.6,-0.525246997000016));
#189464=CARTESIAN_POINT('Ctrl Pts',(11.4436118749999,15.2,-0.523467959000015));
#189465=CARTESIAN_POINT('Ctrl Pts',(11.4436118749999,11.6,-0.523467959000015));
#189466=CARTESIAN_POINT('Ctrl Pts',(11.4402931999999,15.2,-0.521693551000015));
#189467=CARTESIAN_POINT('Ctrl Pts',(11.4402931999999,11.6,-0.521693551000016));
#189468=CARTESIAN_POINT('Ctrl Pts',(11.4369771019999,15.2,-0.519923772000013));
#189469=CARTESIAN_POINT('Ctrl Pts',(11.4369771019999,11.6,-0.519923772000013));
#189470=CARTESIAN_POINT('Ctrl Pts',(11.4336635899999,15.2,-0.518158618000015));
#189471=CARTESIAN_POINT('Ctrl Pts',(11.4336635899999,11.6,-0.518158618000016));
#189472=CARTESIAN_POINT('Ctrl Pts',(11.4303526699999,15.2,-0.516398090000014));
#189473=CARTESIAN_POINT('Ctrl Pts',(11.4303526699999,11.6,-0.516398090000015));
#189474=CARTESIAN_POINT('Ctrl Pts',(11.4270443509999,15.2,-0.514642184000014));
#189475=CARTESIAN_POINT('Ctrl Pts',(11.4270443509999,11.6,-0.514642184000014));
#189476=CARTESIAN_POINT('Ctrl Pts',(11.4237386419999,15.2,-0.512890901000014));
#189477=CARTESIAN_POINT('Ctrl Pts',(11.4237386419999,11.6,-0.512890901000014));
#189478=CARTESIAN_POINT('Ctrl Pts',(11.4204355509999,15.2,-0.511144238000014));
#189479=CARTESIAN_POINT('Ctrl Pts',(11.4204355509999,11.6,-0.511144238000015));
#189480=CARTESIAN_POINT('Ctrl Pts',(11.4171350879999,15.2,-0.509402194000015));
#189481=CARTESIAN_POINT('Ctrl Pts',(11.4171350879999,11.6,-0.509402194000015));
#189482=CARTESIAN_POINT('Ctrl Pts',(11.4138372609999,15.2,-0.507664766000016));
#189483=CARTESIAN_POINT('Ctrl Pts',(11.4138372609999,11.6,-0.507664766000016));
#189484=CARTESIAN_POINT('Ctrl Pts',(11.4105420809999,15.2,-0.505931955000012));
#189485=CARTESIAN_POINT('Ctrl Pts',(11.4105420809999,11.6,-0.505931955000012));
#189486=CARTESIAN_POINT('Ctrl Pts',(11.4072495559999,15.2,-0.504203755000017));
#189487=CARTESIAN_POINT('Ctrl Pts',(11.4072495559999,11.6,-0.504203755000017));
#189488=CARTESIAN_POINT('Ctrl Pts',(11.4039596959999,15.2,-0.502480169000012));
#189489=CARTESIAN_POINT('Ctrl Pts',(11.4039596959999,11.6,-0.502480169000013));
#189490=CARTESIAN_POINT('Ctrl Pts',(11.4006725109999,15.2,-0.500761191000016));
#189491=CARTESIAN_POINT('Ctrl Pts',(11.4006725109999,11.6,-0.500761191000017));
#189492=CARTESIAN_POINT('Ctrl Pts',(11.3973880069999,15.2,-0.499046823000011));
#189493=CARTESIAN_POINT('Ctrl Pts',(11.3973880069999,11.6,-0.499046823000012));
#189494=CARTESIAN_POINT('Ctrl Pts',(11.3941061959999,15.2,-0.497337061000014));
#189495=CARTESIAN_POINT('Ctrl Pts',(11.3941061959999,11.6,-0.497337061000014));
#189496=CARTESIAN_POINT('Ctrl Pts',(11.3908270859999,15.2,-0.495631903000016));
#189497=CARTESIAN_POINT('Ctrl Pts',(11.3908270859999,11.6,-0.495631903000016));
#189498=CARTESIAN_POINT('Ctrl Pts',(11.3875506839999,15.2,-0.493931349000012));
#189499=CARTESIAN_POINT('Ctrl Pts',(11.3875506839999,11.6,-0.493931349000012));
#189500=CARTESIAN_POINT('Ctrl Pts',(11.3842770019999,15.2,-0.492235396000016));
#189501=CARTESIAN_POINT('Ctrl Pts',(11.3842770019999,11.6,-0.492235396000016));
#189502=CARTESIAN_POINT('Ctrl Pts',(11.3810060469999,15.2,-0.490544043000014));
#189503=CARTESIAN_POINT('Ctrl Pts',(11.3810060469999,11.6,-0.490544043000015));
#189504=CARTESIAN_POINT('Ctrl Pts',(11.3777378289999,15.2,-0.488857287000015));
#189505=CARTESIAN_POINT('Ctrl Pts',(11.3777378289999,11.6,-0.488857287000016));
#189506=CARTESIAN_POINT('Ctrl Pts',(11.3744723579999,15.2,-0.487175129000015));
#189507=CARTESIAN_POINT('Ctrl Pts',(11.3744723579999,11.6,-0.487175129000015));
#189508=CARTESIAN_POINT('Ctrl Pts',(11.3712096409999,15.2,-0.485497564000017));
#189509=CARTESIAN_POINT('Ctrl Pts',(11.3712096409999,11.6,-0.485497564000017));
#189510=CARTESIAN_POINT('Ctrl Pts',(11.3679496899999,15.2,-0.483824591000013));
#189511=CARTESIAN_POINT('Ctrl Pts',(11.3679496899999,11.6,-0.483824591000013));
#189512=CARTESIAN_POINT('Ctrl Pts',(11.3646925119999,15.2,-0.482156209000015));
#189513=CARTESIAN_POINT('Ctrl Pts',(11.3646925119999,11.6,-0.482156209000016));
#189514=CARTESIAN_POINT('Ctrl Pts',(11.3614381179999,15.2,-0.480492415000011));
#189515=CARTESIAN_POINT('Ctrl Pts',(11.3614381179999,11.6,-0.480492415000012));
#189516=CARTESIAN_POINT('Ctrl Pts',(11.3581865149999,15.2,-0.478833210000014));
#189517=CARTESIAN_POINT('Ctrl Pts',(11.3581865149999,11.6,-0.478833210000014));
#189518=CARTESIAN_POINT('Ctrl Pts',(11.3549377139999,15.2,-0.477178588000013));
#189519=CARTESIAN_POINT('Ctrl Pts',(11.3549377139999,11.6,-0.477178588000014));
#189520=CARTESIAN_POINT('Ctrl Pts',(11.3516917239999,15.2,-0.475528551000015));
#189521=CARTESIAN_POINT('Ctrl Pts',(11.3516917239999,11.6,-0.475528551000016));
#189522=CARTESIAN_POINT('Ctrl Pts',(11.3484485529999,15.2,-0.473883094000014));
#189523=CARTESIAN_POINT('Ctrl Pts',(11.3484485529999,11.6,-0.473883094000014));
#189524=CARTESIAN_POINT('Ctrl Pts',(11.3452082119999,15.2,-0.472242217000014));
#189525=CARTESIAN_POINT('Ctrl Pts',(11.3452082119999,11.6,-0.472242217000014));
#189526=CARTESIAN_POINT('Ctrl Pts',(11.3419707089999,15.2,-0.470605918000011));
#189527=CARTESIAN_POINT('Ctrl Pts',(11.3419707089999,11.6,-0.470605918000012));
#189528=CARTESIAN_POINT('Ctrl Pts',(11.3387360539999,15.2,-0.468974194000014));
#189529=CARTESIAN_POINT('Ctrl Pts',(11.3387360539999,11.6,-0.468974194000014));
#189530=CARTESIAN_POINT('Ctrl Pts',(11.3355042559999,15.2,-0.467347044000017));
#189531=CARTESIAN_POINT('Ctrl Pts',(11.3355042559999,11.6,-0.467347044000018));
#189532=CARTESIAN_POINT('Ctrl Pts',(11.3322753239999,15.2,-0.465724466000013));
#189533=CARTESIAN_POINT('Ctrl Pts',(11.3322753239999,11.6,-0.465724466000013));
#189534=CARTESIAN_POINT('Ctrl Pts',(11.3290492679999,15.2,-0.464106457000018));
#189535=CARTESIAN_POINT('Ctrl Pts',(11.3290492679999,11.6,-0.464106457000018));
#189536=CARTESIAN_POINT('Ctrl Pts',(11.3258260979999,15.2,-0.462493017000014));
#189537=CARTESIAN_POINT('Ctrl Pts',(11.3258260979999,11.6,-0.462493017000015));
#189538=CARTESIAN_POINT('Ctrl Pts',(11.3226058229999,15.2,-0.460884143000015));
#189539=CARTESIAN_POINT('Ctrl Pts',(11.3226058229999,11.6,-0.460884143000016));
#189540=CARTESIAN_POINT('Ctrl Pts',(11.3193884509999,15.2,-0.459279832000017));
#189541=CARTESIAN_POINT('Ctrl Pts',(11.3193884509999,11.6,-0.459279832000017));
#189542=CARTESIAN_POINT('Ctrl Pts',(11.3161739919999,15.2,-0.457680084000014));
#189543=CARTESIAN_POINT('Ctrl Pts',(11.3161739919999,11.6,-0.457680084000014));
#189544=CARTESIAN_POINT('Ctrl Pts',(11.3129624559999,15.2,-0.456084896000015));
#189545=CARTESIAN_POINT('Ctrl Pts',(11.3129624559999,11.6,-0.456084896000016));
#189546=CARTESIAN_POINT('Ctrl Pts',(11.3097538529999,15.2,-0.454494266000012));
#189547=CARTESIAN_POINT('Ctrl Pts',(11.3097538529999,11.6,-0.454494266000012));
#189548=CARTESIAN_POINT('Ctrl Pts',(11.3065481919999,15.2,-0.452908191000017));
#189549=CARTESIAN_POINT('Ctrl Pts',(11.3065481919999,11.6,-0.452908191000017));
#189550=CARTESIAN_POINT('Ctrl Pts',(11.3033454809999,15.2,-0.451326671000012));
#189551=CARTESIAN_POINT('Ctrl Pts',(11.3033454809999,11.6,-0.451326671000012));
#189552=CARTESIAN_POINT('Ctrl Pts',(11.3001457309999,15.2,-0.449749702000015));
#189553=CARTESIAN_POINT('Ctrl Pts',(11.3001457309999,11.6,-0.449749702000016));
#189554=CARTESIAN_POINT('Ctrl Pts',(11.2969489509999,15.2,-0.448177284000018));
#189555=CARTESIAN_POINT('Ctrl Pts',(11.2969489509999,11.6,-0.448177284000018));
#189556=CARTESIAN_POINT('Ctrl Pts',(11.2937551509999,15.2,-0.446609413000014));
#189557=CARTESIAN_POINT('Ctrl Pts',(11.2937551509999,11.6,-0.446609413000015));
#189558=CARTESIAN_POINT('Ctrl Pts',(11.2905643409999,15.2,-0.445046088000014));
#189559=CARTESIAN_POINT('Ctrl Pts',(11.2905643409999,11.6,-0.445046088000014));
#189560=CARTESIAN_POINT('Ctrl Pts',(11.2873765289999,15.2,-0.443487307000012));
#189561=CARTESIAN_POINT('Ctrl Pts',(11.2873765289999,11.6,-0.443487307000013));
#189562=CARTESIAN_POINT('Ctrl Pts',(11.2841917249999,15.2,-0.441933067000013));
#189563=CARTESIAN_POINT('Ctrl Pts',(11.2841917249999,11.6,-0.441933067000014));
#189564=CARTESIAN_POINT('Ctrl Pts',(11.2810099399999,15.2,-0.440383367000017));
#189565=CARTESIAN_POINT('Ctrl Pts',(11.2810099399999,11.6,-0.440383367000017));
#189566=CARTESIAN_POINT('Ctrl Pts',(11.2778311809999,15.2,-0.438838205000014));
#189567=CARTESIAN_POINT('Ctrl Pts',(11.2778311809999,11.6,-0.438838205000014));
#189568=CARTESIAN_POINT('Ctrl Pts',(11.2746554609999,15.2,-0.437297577000013));
#189569=CARTESIAN_POINT('Ctrl Pts',(11.2746554609999,11.6,-0.437297577000014));
#189570=CARTESIAN_POINT('Ctrl Pts',(11.2714827859999,15.2,-0.435761482000014));
#189571=CARTESIAN_POINT('Ctrl Pts',(11.2714827859999,11.6,-0.435761482000015));
#189572=CARTESIAN_POINT('Ctrl Pts',(11.2683131689999,15.2,-0.434229918000018));
#189573=CARTESIAN_POINT('Ctrl Pts',(11.2683131689999,11.6,-0.434229918000018));
#189574=CARTESIAN_POINT('Ctrl Pts',(11.2651466169999,15.2,-0.432702883000013));
#189575=CARTESIAN_POINT('Ctrl Pts',(11.2651466169999,11.6,-0.432702883000014));
#189576=CARTESIAN_POINT('Ctrl Pts',(11.2619831409999,15.2,-0.431180374000015));
#189577=CARTESIAN_POINT('Ctrl Pts',(11.2619831409999,11.6,-0.431180374000016));
#189578=CARTESIAN_POINT('Ctrl Pts',(11.2588227499999,15.2,-0.429662390000014));
#189579=CARTESIAN_POINT('Ctrl Pts',(11.2588227499999,11.6,-0.429662390000014));
#189580=CARTESIAN_POINT('Ctrl Pts',(11.2556654559999,15.2,-0.428148928000014));
#189581=CARTESIAN_POINT('Ctrl Pts',(11.2556654559999,11.6,-0.428148928000014));
#189582=CARTESIAN_POINT('Ctrl Pts',(11.2525112649999,15.2,-0.426639986000015));
#189583=CARTESIAN_POINT('Ctrl Pts',(11.2525112649999,11.6,-0.426639986000015));
#189584=CARTESIAN_POINT('Ctrl Pts',(11.2493601889999,15.2,-0.425135562000012));
#189585=CARTESIAN_POINT('Ctrl Pts',(11.2493601889999,11.6,-0.425135562000012));
#189586=CARTESIAN_POINT('Ctrl Pts',(11.2462122379999,15.2,-0.423635653000014));
#189587=CARTESIAN_POINT('Ctrl Pts',(11.2462122379999,11.6,-0.423635653000014));
#189588=CARTESIAN_POINT('Ctrl Pts',(11.2430674209999,15.2,-0.422140257000017));
#189589=CARTESIAN_POINT('Ctrl Pts',(11.2430674209999,11.6,-0.422140257000017));
#189590=CARTESIAN_POINT('Ctrl Pts',(11.2399257469999,15.2,-0.420649373000015));
#189591=CARTESIAN_POINT('Ctrl Pts',(11.2399257469999,11.6,-0.420649373000015));
#189592=CARTESIAN_POINT('Ctrl Pts',(11.2367872269999,15.2,-0.419162996000013));
#189593=CARTESIAN_POINT('Ctrl Pts',(11.2367872269999,11.6,-0.419162996000014));
#189594=CARTESIAN_POINT('Ctrl Pts',(11.2336518709999,15.2,-0.417681128000016));
#189595=CARTESIAN_POINT('Ctrl Pts',(11.2336518709999,11.6,-0.417681128000016));
#189596=CARTESIAN_POINT('Ctrl Pts',(11.2305196889999,15.2,-0.416203762000014));
#189597=CARTESIAN_POINT('Ctrl Pts',(11.2305196889999,11.6,-0.416203762000014));
#189598=CARTESIAN_POINT('Ctrl Pts',(11.2273906889999,15.2,-0.414730898000015));
#189599=CARTESIAN_POINT('Ctrl Pts',(11.2273906889999,11.6,-0.414730898000016));
#189600=CARTESIAN_POINT('Ctrl Pts',(11.2242648839999,15.2,-0.413262534000012));
#189601=CARTESIAN_POINT('Ctrl Pts',(11.2242648839999,11.6,-0.413262534000012));
#189602=CARTESIAN_POINT('Ctrl Pts',(11.2211422809999,15.2,-0.411798667000016));
#189603=CARTESIAN_POINT('Ctrl Pts',(11.2211422809999,11.6,-0.411798667000017));
#189604=CARTESIAN_POINT('Ctrl Pts',(11.2180228899999,15.2,-0.410339294000015));
#189605=CARTESIAN_POINT('Ctrl Pts',(11.2180228899999,11.6,-0.410339294000015));
#189606=CARTESIAN_POINT('Ctrl Pts',(11.2149067229999,15.2,-0.408884414000017));
#189607=CARTESIAN_POINT('Ctrl Pts',(11.2149067229999,11.6,-0.408884414000017));
#189608=CARTESIAN_POINT('Ctrl Pts',(11.2117937879999,15.2,-0.407434024000013));
#189609=CARTESIAN_POINT('Ctrl Pts',(11.2117937879999,11.6,-0.407434024000013));
#189610=CARTESIAN_POINT('Ctrl Pts',(11.2086840959999,15.2,-0.405988122000016));
#189611=CARTESIAN_POINT('Ctrl Pts',(11.2086840959999,11.6,-0.405988122000017));
#189612=CARTESIAN_POINT('Ctrl Pts',(11.2055776569999,15.2,-0.404546706000013));
#189613=CARTESIAN_POINT('Ctrl Pts',(11.2055776569999,11.6,-0.404546706000013));
#189614=CARTESIAN_POINT('Ctrl Pts',(11.2024744809999,15.2,-0.403109771000012));
#189615=CARTESIAN_POINT('Ctrl Pts',(11.2024744809999,11.6,-0.403109771000012));
#189616=CARTESIAN_POINT('Ctrl Pts',(11.1993745769999,15.2,-0.401677318000013));
#189617=CARTESIAN_POINT('Ctrl Pts',(11.1993745769999,11.6,-0.401677318000014));
#189618=CARTESIAN_POINT('Ctrl Pts',(11.1962779569999,15.2,-0.400249342000016));
#189619=CARTESIAN_POINT('Ctrl Pts',(11.1962779569999,11.6,-0.400249342000017));
#189620=CARTESIAN_POINT('Ctrl Pts',(11.1931846289999,15.2,-0.398825842000012));
#189621=CARTESIAN_POINT('Ctrl Pts',(11.1931846289999,11.6,-0.398825842000013));
#189622=CARTESIAN_POINT('Ctrl Pts',(11.1900946029999,15.2,-0.397406815000014));
#189623=CARTESIAN_POINT('Ctrl Pts',(11.1900946029999,11.6,-0.397406815000015));
#189624=CARTESIAN_POINT('Ctrl Pts',(11.1870078909999,15.2,-0.395992258000017));
#189625=CARTESIAN_POINT('Ctrl Pts',(11.1870078909999,11.6,-0.395992258000018));
#189626=CARTESIAN_POINT('Ctrl Pts',(11.1839245019999,15.2,-0.394582170000017));
#189627=CARTESIAN_POINT('Ctrl Pts',(11.1839245019999,11.6,-0.394582170000018));
#189628=CARTESIAN_POINT('Ctrl Pts',(11.1808444459999,15.2,-0.393176547000014));
#189629=CARTESIAN_POINT('Ctrl Pts',(11.1808444459999,11.6,-0.393176547000014));
#189630=CARTESIAN_POINT('Ctrl Pts',(11.1777677329999,15.2,-0.391775387000015));
#189631=CARTESIAN_POINT('Ctrl Pts',(11.1777677329999,11.6,-0.391775387000016));
#189632=CARTESIAN_POINT('Ctrl Pts',(11.1746943739999,15.2,-0.390378688000013));
#189633=CARTESIAN_POINT('Ctrl Pts',(11.1746943739999,11.6,-0.390378688000013));
#189634=CARTESIAN_POINT('Ctrl Pts',(11.1716243779999,15.2,-0.388986447000015));
#189635=CARTESIAN_POINT('Ctrl Pts',(11.1716243779999,11.6,-0.388986447000015));
#189636=CARTESIAN_POINT('Ctrl Pts',(11.1685577559999,15.2,-0.387598660000013));
#189637=CARTESIAN_POINT('Ctrl Pts',(11.1685577559999,11.6,-0.387598660000013));
#189638=CARTESIAN_POINT('Ctrl Pts',(11.1654945179999,15.2,-0.386215328000015));
#189639=CARTESIAN_POINT('Ctrl Pts',(11.1654945179999,11.6,-0.386215328000015));
#189640=CARTESIAN_POINT('Ctrl Pts',(11.1624346739999,15.2,-0.384836446000012));
#189641=CARTESIAN_POINT('Ctrl Pts',(11.1624346739999,11.6,-0.384836446000012));
#189642=CARTESIAN_POINT('Ctrl Pts',(11.1593782349999,15.2,-0.383462011000013));
#189643=CARTESIAN_POINT('Ctrl Pts',(11.1593782349999,11.6,-0.383462011000014));
#189644=CARTESIAN_POINT('Ctrl Pts',(11.1563252099999,15.2,-0.382092022000013));
#189645=CARTESIAN_POINT('Ctrl Pts',(11.1563252099999,11.6,-0.382092022000014));
#189646=CARTESIAN_POINT('Ctrl Pts',(11.1532756099999,15.2,-0.380726475000017));
#189647=CARTESIAN_POINT('Ctrl Pts',(11.1532756099999,11.6,-0.380726475000018));
#189648=CARTESIAN_POINT('Ctrl Pts',(11.1502294459999,15.2,-0.379365367000015));
#189649=CARTESIAN_POINT('Ctrl Pts',(11.1502294459999,11.6,-0.379365367000016));
#189650=CARTESIAN_POINT('Ctrl Pts',(11.1471867269999,15.2,-0.378008697000016));
#189651=CARTESIAN_POINT('Ctrl Pts',(11.1471867269999,11.6,-0.378008697000017));
#189652=CARTESIAN_POINT('Ctrl Pts',(11.1441474629999,15.2,-0.376656462000016));
#189653=CARTESIAN_POINT('Ctrl Pts',(11.1441474629999,11.6,-0.376656462000016));
#189654=CARTESIAN_POINT('Ctrl Pts',(11.1411116659999,15.2,-0.375308658000013));
#189655=CARTESIAN_POINT('Ctrl Pts',(11.1411116659999,11.6,-0.375308658000014));
#189656=CARTESIAN_POINT('Ctrl Pts',(11.1380793459999,15.2,-0.373965284000013));
#189657=CARTESIAN_POINT('Ctrl Pts',(11.1380793459999,11.6,-0.373965284000013));
#189658=CARTESIAN_POINT('Ctrl Pts',(11.1350505129999,15.2,-0.372626336000015));
#189659=CARTESIAN_POINT('Ctrl Pts',(11.1350505129999,11.6,-0.372626336000015));
#189660=CARTESIAN_POINT('Ctrl Pts',(11.1320251769999,15.2,-0.371291812000014));
#189661=CARTESIAN_POINT('Ctrl Pts',(11.1320251769999,11.6,-0.371291812000015));
#189662=CARTESIAN_POINT('Ctrl Pts',(11.1290033489999,15.2,-0.369961709000015));
#189663=CARTESIAN_POINT('Ctrl Pts',(11.1290033489999,11.6,-0.369961709000016));
#189664=CARTESIAN_POINT('Ctrl Pts',(11.1259850389999,15.2,-0.368636024000013));
#189665=CARTESIAN_POINT('Ctrl Pts',(11.1259850389999,11.6,-0.368636024000013));
#189666=CARTESIAN_POINT('Ctrl Pts',(11.1229702569999,15.2,-0.367314755000017));
#189667=CARTESIAN_POINT('Ctrl Pts',(11.1229702569999,11.6,-0.367314755000017));
#189668=CARTESIAN_POINT('Ctrl Pts',(11.1199590149999,15.2,-0.365997899000017));
#189669=CARTESIAN_POINT('Ctrl Pts',(11.1199590149999,11.6,-0.365997899000017));
#189670=CARTESIAN_POINT('Ctrl Pts',(11.1169513219999,15.2,-0.364685453000018));
#189671=CARTESIAN_POINT('Ctrl Pts',(11.1169513219999,11.6,-0.364685453000018));
#189672=CARTESIAN_POINT('Ctrl Pts',(11.1139471899999,15.2,-0.363377413000014));
#189673=CARTESIAN_POINT('Ctrl Pts',(11.1139471899999,11.6,-0.363377413000015));
#189674=CARTESIAN_POINT('Ctrl Pts',(11.1109466279999,15.2,-0.362073779000016));
#189675=CARTESIAN_POINT('Ctrl Pts',(11.1109466279999,11.6,-0.362073779000017));
#189676=CARTESIAN_POINT('Ctrl Pts',(11.1079496479999,15.2,-0.360774546000013));
#189677=CARTESIAN_POINT('Ctrl Pts',(11.1079496479999,11.6,-0.360774546000014));
#189678=CARTESIAN_POINT('Ctrl Pts',(11.1049562589999,15.2,-0.359479712000015));
#189679=CARTESIAN_POINT('Ctrl Pts',(11.1049562589999,11.6,-0.359479712000015));
#189680=CARTESIAN_POINT('Ctrl Pts',(11.1019664729999,15.2,-0.358189274000011));
#189681=CARTESIAN_POINT('Ctrl Pts',(11.1019664729999,11.6,-0.358189274000012));
#189682=CARTESIAN_POINT('Ctrl Pts',(11.0989802999999,15.2,-0.356903228000016));
#189683=CARTESIAN_POINT('Ctrl Pts',(11.0989802999999,11.6,-0.356903228000017));
#189684=CARTESIAN_POINT('Ctrl Pts',(11.0959977499999,15.2,-0.355621573000011));
#189685=CARTESIAN_POINT('Ctrl Pts',(11.0959977499999,11.6,-0.355621573000012));
#189686=CARTESIAN_POINT('Ctrl Pts',(11.0930188349999,15.2,-0.354344304000014));
#189687=CARTESIAN_POINT('Ctrl Pts',(11.0930188349999,11.6,-0.354344304000014));
#189688=CARTESIAN_POINT('Ctrl Pts',(11.0900435649999,15.2,-0.353071421000015));
#189689=CARTESIAN_POINT('Ctrl Pts',(11.0900435649999,11.6,-0.353071421000016));
#189690=CARTESIAN_POINT('Ctrl Pts',(11.0870719499999,15.2,-0.351802918000015));
#189691=CARTESIAN_POINT('Ctrl Pts',(11.0870719499999,11.6,-0.351802918000015));
#189692=CARTESIAN_POINT('Ctrl Pts',(11.0841040009999,15.2,-0.350538795000013));
#189693=CARTESIAN_POINT('Ctrl Pts',(11.0841040009999,11.6,-0.350538795000013));
#189694=CARTESIAN_POINT('Ctrl Pts',(11.0811397299999,15.2,-0.349279047000017));
#189695=CARTESIAN_POINT('Ctrl Pts',(11.0811397299999,11.6,-0.349279047000018));
#189696=CARTESIAN_POINT('Ctrl Pts',(11.0781791459999,15.2,-0.348023671000015));
#189697=CARTESIAN_POINT('Ctrl Pts',(11.0781791459999,11.6,-0.348023671000016));
#189698=CARTESIAN_POINT('Ctrl Pts',(11.0752222619999,15.2,-0.346772665000015));
#189699=CARTESIAN_POINT('Ctrl Pts',(11.0752222619999,11.6,-0.346772665000015));
#189700=CARTESIAN_POINT('Ctrl Pts',(11.0722690859999,15.2,-0.345526025000016));
#189701=CARTESIAN_POINT('Ctrl Pts',(11.0722690859999,11.6,-0.345526025000016));
#189702=CARTESIAN_POINT('Ctrl Pts',(11.0693196309999,15.2,-0.344283750000014));
#189703=CARTESIAN_POINT('Ctrl Pts',(11.0693196309999,11.6,-0.344283750000014));
#189704=CARTESIAN_POINT('Ctrl Pts',(11.0663739069999,15.2,-0.343045834000013));
#189705=CARTESIAN_POINT('Ctrl Pts',(11.0663739069999,11.6,-0.343045834000014));
#189706=CARTESIAN_POINT('Ctrl Pts',(11.0634319249999,15.2,-0.341812275000013));
#189707=CARTESIAN_POINT('Ctrl Pts',(11.0634319249999,11.6,-0.341812275000013));
#189708=CARTESIAN_POINT('Ctrl Pts',(11.0604936949999,15.2,-0.340583072000014));
#189709=CARTESIAN_POINT('Ctrl Pts',(11.0604936949999,11.6,-0.340583072000014));
#189710=CARTESIAN_POINT('Ctrl Pts',(11.0575592289999,15.2,-0.339358220000014));
#189711=CARTESIAN_POINT('Ctrl Pts',(11.0575592289999,11.6,-0.339358220000015));
#189712=CARTESIAN_POINT('Ctrl Pts',(11.0546285369999,15.2,-0.338137715000015));
#189713=CARTESIAN_POINT('Ctrl Pts',(11.0546285369999,11.6,-0.338137715000016));
#189714=CARTESIAN_POINT('Ctrl Pts',(11.0517016309999,15.2,-0.336921557000016));
#189715=CARTESIAN_POINT('Ctrl Pts',(11.0517016309999,11.6,-0.336921557000017));
#189716=CARTESIAN_POINT('Ctrl Pts',(11.0487785209999,15.2,-0.335709740000016));
#189717=CARTESIAN_POINT('Ctrl Pts',(11.0487785209999,11.6,-0.335709740000017));
#189718=CARTESIAN_POINT('Ctrl Pts',(11.0458592189999,15.2,-0.334502262000012));
#189719=CARTESIAN_POINT('Ctrl Pts',(11.0458592189999,11.6,-0.334502262000012));
#189720=CARTESIAN_POINT('Ctrl Pts',(11.0429437349999,15.2,-0.333299120000015));
#189721=CARTESIAN_POINT('Ctrl Pts',(11.0429437349999,11.6,-0.333299120000015));
#189722=CARTESIAN_POINT('Ctrl Pts',(11.0400320799999,15.2,-0.332100311000012));
#189723=CARTESIAN_POINT('Ctrl Pts',(11.0400320799999,11.6,-0.332100311000012));
#189724=CARTESIAN_POINT('Ctrl Pts',(11.0371242659999,15.2,-0.330905831000017));
#189725=CARTESIAN_POINT('Ctrl Pts',(11.0371242659999,11.6,-0.330905831000017));
#189726=CARTESIAN_POINT('Ctrl Pts',(11.0342203029999,15.2,-0.329715677000015));
#189727=CARTESIAN_POINT('Ctrl Pts',(11.0342203029999,11.6,-0.329715677000016));
#189728=CARTESIAN_POINT('Ctrl Pts',(11.0313202029999,15.2,-0.328529847000016));
#189729=CARTESIAN_POINT('Ctrl Pts',(11.0313202029999,11.6,-0.328529847000017));
#189730=CARTESIAN_POINT('Ctrl Pts',(11.0284239769999,15.2,-0.327348336000015));
#189731=CARTESIAN_POINT('Ctrl Pts',(11.0284239769999,11.6,-0.327348336000016));
#189732=CARTESIAN_POINT('Ctrl Pts',(11.0255316349999,15.2,-0.326171141000016));
#189733=CARTESIAN_POINT('Ctrl Pts',(11.0255316349999,11.6,-0.326171141000016));
#189734=CARTESIAN_POINT('Ctrl Pts',(11.0226431889999,15.2,-0.324998260000013));
#189735=CARTESIAN_POINT('Ctrl Pts',(11.0226431889999,11.6,-0.324998260000014));
#189736=CARTESIAN_POINT('Ctrl Pts',(11.0197586499999,15.2,-0.323829688000017));
#189737=CARTESIAN_POINT('Ctrl Pts',(11.0197586499999,11.6,-0.323829688000017));
#189738=CARTESIAN_POINT('Ctrl Pts',(11.0168780289999,15.2,-0.322665425000017));
#189739=CARTESIAN_POINT('Ctrl Pts',(11.0168780289999,11.6,-0.322665425000018));
#189740=CARTESIAN_POINT('Ctrl Pts',(11.0140013379999,15.2,-0.321505464000014));
#189741=CARTESIAN_POINT('Ctrl Pts',(11.0140013379999,11.6,-0.321505464000014));
#189742=CARTESIAN_POINT('Ctrl Pts',(11.0111285869999,15.2,-0.320349803000015));
#189743=CARTESIAN_POINT('Ctrl Pts',(11.0111285869999,11.6,-0.320349803000016));
#189744=CARTESIAN_POINT('Ctrl Pts',(11.0082597879999,15.2,-0.319198439000012));
#189745=CARTESIAN_POINT('Ctrl Pts',(11.0082597879999,11.6,-0.319198439000013));
#189746=CARTESIAN_POINT('Ctrl Pts',(11.0053949529999,15.2,-0.318051369000014));
#189747=CARTESIAN_POINT('Ctrl Pts',(11.0053949529999,11.6,-0.318051369000015));
#189748=CARTESIAN_POINT('Ctrl Pts',(11.0025340919999,15.2,-0.316908589000011));
#189749=CARTESIAN_POINT('Ctrl Pts',(11.0025340919999,11.6,-0.316908589000012));
#189750=CARTESIAN_POINT('Ctrl Pts',(10.9996772159999,15.2,-0.315770095000012));
#189751=CARTESIAN_POINT('Ctrl Pts',(10.9996772159999,11.6,-0.315770095000012));
#189752=CARTESIAN_POINT('Ctrl Pts',(10.9968243389999,15.2,-0.314635885000012));
#189753=CARTESIAN_POINT('Ctrl Pts',(10.9968243389999,11.6,-0.314635885000012));
#189754=CARTESIAN_POINT('Ctrl Pts',(10.9939754689999,15.2,-0.313505954000015));
#189755=CARTESIAN_POINT('Ctrl Pts',(10.9939754689999,11.6,-0.313505954000016));
#189756=CARTESIAN_POINT('Ctrl Pts',(10.9911306189999,15.2,-0.312380300000012));
#189757=CARTESIAN_POINT('Ctrl Pts',(10.9911306189999,11.6,-0.312380300000013));
#189758=CARTESIAN_POINT('Ctrl Pts',(10.9882897999999,15.2,-0.311258919000017));
#189759=CARTESIAN_POINT('Ctrl Pts',(10.9882897999999,11.6,-0.311258919000017));
#189760=CARTESIAN_POINT('Ctrl Pts',(10.9854530239999,15.2,-0.310141807000015));
#189761=CARTESIAN_POINT('Ctrl Pts',(10.9854530239999,11.6,-0.310141807000015));
#189762=CARTESIAN_POINT('Ctrl Pts',(10.9826203019999,15.2,-0.309028962000015));
#189763=CARTESIAN_POINT('Ctrl Pts',(10.9826203019999,11.6,-0.309028962000016));
#189764=CARTESIAN_POINT('Ctrl Pts',(10.9797916459999,15.2,-0.307920379000013));
#189765=CARTESIAN_POINT('Ctrl Pts',(10.9797916459999,11.6,-0.307920379000013));
#189766=CARTESIAN_POINT('Ctrl Pts',(10.9769670669999,15.2,-0.306816055000017));
#189767=CARTESIAN_POINT('Ctrl Pts',(10.9769670669999,11.6,-0.306816055000017));
#189768=CARTESIAN_POINT('Ctrl Pts',(10.9741465759999,15.2,-0.305715987000017));
#189769=CARTESIAN_POINT('Ctrl Pts',(10.9741465759999,11.6,-0.305715987000017));
#189770=CARTESIAN_POINT('Ctrl Pts',(10.9713301849999,15.2,-0.304620170000014));
#189771=CARTESIAN_POINT('Ctrl Pts',(10.9713301849999,11.6,-0.304620170000014));
#189772=CARTESIAN_POINT('Ctrl Pts',(10.9685179069999,15.2,-0.303528602000016));
#189773=CARTESIAN_POINT('Ctrl Pts',(10.9685179069999,11.6,-0.303528602000017));
#189774=CARTESIAN_POINT('Ctrl Pts',(10.9657097509999,15.2,-0.302441280000014));
#189775=CARTESIAN_POINT('Ctrl Pts',(10.9657097509999,11.6,-0.302441280000015));
#189776=CARTESIAN_POINT('Ctrl Pts',(10.9629057309999,15.2,-0.301358197000017));
#189777=CARTESIAN_POINT('Ctrl Pts',(10.9629057309999,11.6,-0.301358197000017));
#189778=CARTESIAN_POINT('Ctrl Pts',(10.9601058569999,15.2,-0.300279353000015));
#189779=CARTESIAN_POINT('Ctrl Pts',(10.9601058569999,11.6,-0.300279353000015));
#189780=CARTESIAN_POINT('Ctrl Pts',(10.9573101409999,15.2,-0.299204743000012));
#189781=CARTESIAN_POINT('Ctrl Pts',(10.9573101409999,11.6,-0.299204743000013));
#189782=CARTESIAN_POINT('Ctrl Pts',(10.9545185949999,15.2,-0.298134363000013));
#189783=CARTESIAN_POINT('Ctrl Pts',(10.9545185949999,11.6,-0.298134363000014));
#189784=CARTESIAN_POINT('Ctrl Pts',(10.9517312309999,15.2,-0.297068209000013));
#189785=CARTESIAN_POINT('Ctrl Pts',(10.9517312309999,11.6,-0.297068209000014));
#189786=CARTESIAN_POINT('Ctrl Pts',(10.9489480589999,15.2,-0.296006279000016));
#189787=CARTESIAN_POINT('Ctrl Pts',(10.9489480589999,11.6,-0.296006279000017));
#189788=CARTESIAN_POINT('Ctrl Pts',(10.9461690929999,15.2,-0.294948568000013));
#189789=CARTESIAN_POINT('Ctrl Pts',(10.9461690929999,11.6,-0.294948568000013));
#189790=CARTESIAN_POINT('Ctrl Pts',(10.9433943439999,15.2,-0.293895072000012));
#189791=CARTESIAN_POINT('Ctrl Pts',(10.9433943439999,11.6,-0.293895072000013));
#189792=CARTESIAN_POINT('Ctrl Pts',(10.9406238229999,15.2,-0.292845788000013));
#189793=CARTESIAN_POINT('Ctrl Pts',(10.9406238229999,11.6,-0.292845788000014));
#189794=CARTESIAN_POINT('Ctrl Pts',(10.9378575429999,15.2,-0.291800712000012));
#189795=CARTESIAN_POINT('Ctrl Pts',(10.9378575429999,11.6,-0.291800712000013));
#189796=CARTESIAN_POINT('Ctrl Pts',(10.9350955149999,15.2,-0.290759841000017));
#189797=CARTESIAN_POINT('Ctrl Pts',(10.9350955149999,11.6,-0.290759841000017));
#189798=CARTESIAN_POINT('Ctrl Pts',(10.9323377509999,15.2,-0.289723170000014));
#189799=CARTESIAN_POINT('Ctrl Pts',(10.9323377509999,11.6,-0.289723170000014));
#189800=CARTESIAN_POINT('Ctrl Pts',(10.9295842629999,15.2,-0.288690696000016));
#189801=CARTESIAN_POINT('Ctrl Pts',(10.9295842629999,11.6,-0.288690696000016));
#189802=CARTESIAN_POINT('Ctrl Pts',(10.9268350629999,15.2,-0.287662415000014));
#189803=CARTESIAN_POINT('Ctrl Pts',(10.9268350629999,11.6,-0.287662415000014));
#189804=CARTESIAN_POINT('Ctrl Pts',(10.9240901629999,15.2,-0.286638322000012));
#189805=CARTESIAN_POINT('Ctrl Pts',(10.9240901629999,11.6,-0.286638322000013));
#189806=CARTESIAN_POINT('Ctrl Pts',(10.9213495759999,15.2,-0.285618415000015));
#189807=CARTESIAN_POINT('Ctrl Pts',(10.9213495759999,11.6,-0.285618415000016));
#189808=CARTESIAN_POINT('Ctrl Pts',(10.9186133109999,15.2,-0.284602689000018));
#189809=CARTESIAN_POINT('Ctrl Pts',(10.9186133109999,11.6,-0.284602689000018));
#189810=CARTESIAN_POINT('Ctrl Pts',(10.9158813839999,15.2,-0.283591141000015));
#189811=CARTESIAN_POINT('Ctrl Pts',(10.9158813839999,11.6,-0.283591141000015));
#189812=CARTESIAN_POINT('Ctrl Pts',(10.9131538029999,15.2,-0.282583766000015));
#189813=CARTESIAN_POINT('Ctrl Pts',(10.9131538029999,11.6,-0.282583766000016));
#189814=CARTESIAN_POINT('Ctrl Pts',(10.9104305819999,15.2,-0.281580561000014));
#189815=CARTESIAN_POINT('Ctrl Pts',(10.9104305819999,11.6,-0.281580561000015));
#189816=CARTESIAN_POINT('Ctrl Pts',(10.9077117349999,15.2,-0.280581520000016));
#189817=CARTESIAN_POINT('Ctrl Pts',(10.9077117349999,11.6,-0.280581520000017));
#189818=CARTESIAN_POINT('Ctrl Pts',(10.9049972699999,15.2,-0.279586642000016));
#189819=CARTESIAN_POINT('Ctrl Pts',(10.9049972699999,11.6,-0.279586642000016));
#189820=CARTESIAN_POINT('Ctrl Pts',(10.9022872019999,15.2,-0.278595921000013));
#189821=CARTESIAN_POINT('Ctrl Pts',(10.9022872019999,11.6,-0.278595921000014));
#189822=CARTESIAN_POINT('Ctrl Pts',(10.8995815439999,15.2,-0.277609354000017));
#189823=CARTESIAN_POINT('Ctrl Pts',(10.8995815439999,11.6,-0.277609354000017));
#189824=CARTESIAN_POINT('Ctrl Pts',(10.8968803049999,15.2,-0.276626936000017));
#189825=CARTESIAN_POINT('Ctrl Pts',(10.8968803049999,11.6,-0.276626936000018));
#189826=CARTESIAN_POINT('Ctrl Pts',(10.8941834999999,15.2,-0.275648665000015));
#189827=CARTESIAN_POINT('Ctrl Pts',(10.8941834999999,11.6,-0.275648665000015));
#189828=CARTESIAN_POINT('Ctrl Pts',(10.8914911399999,15.2,-0.274674534000017));
#189829=CARTESIAN_POINT('Ctrl Pts',(10.8914911399999,11.6,-0.274674534000017));
#189830=CARTESIAN_POINT('Ctrl Pts',(10.8888032369999,15.2,-0.273704541000015));
#189831=CARTESIAN_POINT('Ctrl Pts',(10.8888032369999,11.6,-0.273704541000015));
#189832=CARTESIAN_POINT('Ctrl Pts',(10.8861198049999,15.2,-0.272738682000018));
#189833=CARTESIAN_POINT('Ctrl Pts',(10.8861198049999,11.6,-0.272738682000018));
#189834=CARTESIAN_POINT('Ctrl Pts',(10.8834408539999,15.2,-0.271776950000016));
#189835=CARTESIAN_POINT('Ctrl Pts',(10.8834408539999,11.6,-0.271776950000016));
#189836=CARTESIAN_POINT('Ctrl Pts',(10.8807663989999,15.2,-0.270819345000017));
#189837=CARTESIAN_POINT('Ctrl Pts',(10.8807663989999,11.6,-0.270819345000018));
#189838=CARTESIAN_POINT('Ctrl Pts',(10.8780964489999,15.2,-0.269865861000014));
#189839=CARTESIAN_POINT('Ctrl Pts',(10.8780964489999,11.6,-0.269865861000014));
#189840=CARTESIAN_POINT('Ctrl Pts',(10.8754310189999,15.2,-0.268916493000013));
#189841=CARTESIAN_POINT('Ctrl Pts',(10.8754310189999,11.6,-0.268916493000014));
#189842=CARTESIAN_POINT('Ctrl Pts',(10.8727701199999,15.2,-0.267971237000015));
#189843=CARTESIAN_POINT('Ctrl Pts',(10.8727701199999,11.6,-0.267971237000016));
#189844=CARTESIAN_POINT('Ctrl Pts',(10.8701137659999,15.2,-0.267030089000015));
#189845=CARTESIAN_POINT('Ctrl Pts',(10.8701137659999,11.6,-0.267030089000016));
#189846=CARTESIAN_POINT('Ctrl Pts',(10.8674619699999,15.2,-0.266093046000013));
#189847=CARTESIAN_POINT('Ctrl Pts',(10.8674619699999,11.6,-0.266093046000014));
#189848=CARTESIAN_POINT('Ctrl Pts',(10.8648147409999,15.2,-0.265160103000017));
#189849=CARTESIAN_POINT('Ctrl Pts',(10.8648147409999,11.6,-0.265160103000018));
#189850=CARTESIAN_POINT('Ctrl Pts',(10.8621720949999,15.2,-0.264231254000014));
#189851=CARTESIAN_POINT('Ctrl Pts',(10.8621720949999,11.6,-0.264231254000014));
#189852=CARTESIAN_POINT('Ctrl Pts',(10.8595340429999,15.2,-0.263306498000015));
#189853=CARTESIAN_POINT('Ctrl Pts',(10.8595340429999,11.6,-0.263306498000016));
#189854=CARTESIAN_POINT('Ctrl Pts',(10.8569005969999,15.2,-0.262385828000014));
#189855=CARTESIAN_POINT('Ctrl Pts',(10.8569005969999,11.6,-0.262385828000014));
#189856=CARTESIAN_POINT('Ctrl Pts',(10.8542717719999,15.2,-0.261469241000012));
#189857=CARTESIAN_POINT('Ctrl Pts',(10.8542717719999,11.6,-0.261469241000012));
#189858=CARTESIAN_POINT('Ctrl Pts',(10.8516475779999,15.2,-0.260556732000015));
#189859=CARTESIAN_POINT('Ctrl Pts',(10.8516475779999,11.6,-0.260556732000015));
#189860=CARTESIAN_POINT('Ctrl Pts',(10.8490280299999,15.2,-0.259648296000012));
#189861=CARTESIAN_POINT('Ctrl Pts',(10.8490280299999,11.6,-0.259648296000013));
#189862=CARTESIAN_POINT('Ctrl Pts',(10.8464131379999,15.2,-0.258743931000014));
#189863=CARTESIAN_POINT('Ctrl Pts',(10.8464131379999,11.6,-0.258743931000014));
#189864=CARTESIAN_POINT('Ctrl Pts',(10.8438029179999,15.2,-0.257843630000014));
#189865=CARTESIAN_POINT('Ctrl Pts',(10.8438029179999,11.6,-0.257843630000015));
#189866=CARTESIAN_POINT('Ctrl Pts',(10.8411973799999,15.2,-0.256947389000013));
#189867=CARTESIAN_POINT('Ctrl Pts',(10.8411973799999,11.6,-0.256947389000013));
#189868=CARTESIAN_POINT('Ctrl Pts',(10.8385965389999,15.2,-0.256055205000014));
#189869=CARTESIAN_POINT('Ctrl Pts',(10.8385965389999,11.6,-0.256055205000015));
#189870=CARTESIAN_POINT('Ctrl Pts',(10.8360004059999,15.2,-0.255167073000013));
#189871=CARTESIAN_POINT('Ctrl Pts',(10.8360004059999,11.6,-0.255167073000014));
#189872=CARTESIAN_POINT('Ctrl Pts',(10.8334089939999,15.2,-0.254282987000014));
#189873=CARTESIAN_POINT('Ctrl Pts',(10.8334089939999,11.6,-0.254282987000015));
#189874=CARTESIAN_POINT('Ctrl Pts',(10.8308223169999,15.2,-0.253402945000012));
#189875=CARTESIAN_POINT('Ctrl Pts',(10.8308223169999,11.6,-0.253402945000012));
#189876=CARTESIAN_POINT('Ctrl Pts',(10.8282403869999,15.2,-0.252526940000015));
#189877=CARTESIAN_POINT('Ctrl Pts',(10.8282403869999,11.6,-0.252526940000016));
#189878=CARTESIAN_POINT('Ctrl Pts',(10.8256632179999,15.2,-0.251654969000015));
#189879=CARTESIAN_POINT('Ctrl Pts',(10.8256632179999,11.6,-0.251654969000015));
#189880=CARTESIAN_POINT('Ctrl Pts',(10.8230908219999,15.2,-0.250787027000015));
#189881=CARTESIAN_POINT('Ctrl Pts',(10.8230908219999,11.6,-0.250787027000015));
#189882=CARTESIAN_POINT('Ctrl Pts',(10.8205232129999,15.2,-0.249923108000014));
#189883=CARTESIAN_POINT('Ctrl Pts',(10.8205232129999,11.6,-0.249923108000015));
#189884=CARTESIAN_POINT('Ctrl Pts',(10.8179604029999,15.2,-0.249063210000013));
#189885=CARTESIAN_POINT('Ctrl Pts',(10.8179604029999,11.6,-0.249063210000014));
#189886=CARTESIAN_POINT('Ctrl Pts',(10.8154024049999,15.2,-0.248207327000016));
#189887=CARTESIAN_POINT('Ctrl Pts',(10.8154024049999,11.6,-0.248207327000017));
#189888=CARTESIAN_POINT('Ctrl Pts',(10.8128492319999,15.2,-0.247355454000013));
#189889=CARTESIAN_POINT('Ctrl Pts',(10.8128492319999,11.6,-0.247355454000014));
#189890=CARTESIAN_POINT('Ctrl Pts',(10.8103008979999,15.2,-0.246507587000018));
#189891=CARTESIAN_POINT('Ctrl Pts',(10.8103008979999,11.6,-0.246507587000018));
#189892=CARTESIAN_POINT('Ctrl Pts',(10.8077574159999,15.2,-0.245663720000016));
#189893=CARTESIAN_POINT('Ctrl Pts',(10.8077574159999,11.6,-0.245663720000016));
#189894=CARTESIAN_POINT('Ctrl Pts',(10.8052187989999,15.2,-0.244823851000016));
#189895=CARTESIAN_POINT('Ctrl Pts',(10.8052187989999,11.6,-0.244823851000016));
#189896=CARTESIAN_POINT('Ctrl Pts',(10.8026850599999,15.2,-0.243987972000017));
#189897=CARTESIAN_POINT('Ctrl Pts',(10.8026850599999,11.6,-0.243987972000018));
#189898=CARTESIAN_POINT('Ctrl Pts',(10.8001562119999,15.2,-0.243156081000016));
#189899=CARTESIAN_POINT('Ctrl Pts',(10.8001562119999,11.6,-0.243156081000016));
#189900=CARTESIAN_POINT('Ctrl Pts',(10.7976322689999,15.2,-0.242328170000015));
#189901=CARTESIAN_POINT('Ctrl Pts',(10.7976322689999,11.6,-0.242328170000015));
#189902=CARTESIAN_POINT('Ctrl Pts',(10.7951132439999,15.2,-0.241504237000014));
#189903=CARTESIAN_POINT('Ctrl Pts',(10.7951132439999,11.6,-0.241504237000015));
#189904=CARTESIAN_POINT('Ctrl Pts',(10.7925991499999,15.2,-0.240684278000014));
#189905=CARTESIAN_POINT('Ctrl Pts',(10.7925991499999,11.6,-0.240684278000014));
#189906=CARTESIAN_POINT('Ctrl Pts',(10.7900900009999,15.2,-0.239868284000018));
#189907=CARTESIAN_POINT('Ctrl Pts',(10.7900900009999,11.6,-0.239868284000018));
#189908=CARTESIAN_POINT('Ctrl Pts',(10.7875858089999,15.2,-0.239056253000012));
#189909=CARTESIAN_POINT('Ctrl Pts',(10.7875858089999,11.6,-0.239056253000012));
#189910=CARTESIAN_POINT('Ctrl Pts',(10.7850865899999,15.2,-0.238248181000014));
#189911=CARTESIAN_POINT('Ctrl Pts',(10.7850865899999,11.6,-0.238248181000014));
#189912=CARTESIAN_POINT('Ctrl Pts',(10.7825923549999,15.2,-0.237444060000014));
#189913=CARTESIAN_POINT('Ctrl Pts',(10.7825923549999,11.6,-0.237444060000014));
#189914=CARTESIAN_POINT('Ctrl Pts',(10.7801031189999,15.2,-0.236643887000016));
#189915=CARTESIAN_POINT('Ctrl Pts',(10.7801031189999,11.6,-0.236643887000017));
#189916=CARTESIAN_POINT('Ctrl Pts',(10.7776188939999,15.2,-0.235847657000012));
#189917=CARTESIAN_POINT('Ctrl Pts',(10.7776188939999,11.6,-0.235847657000013));
#189918=CARTESIAN_POINT('Ctrl Pts',(10.7751396949999,15.2,-0.235055365000014));
#189919=CARTESIAN_POINT('Ctrl Pts',(10.7751396949999,11.6,-0.235055365000015));
#189920=CARTESIAN_POINT('Ctrl Pts',(10.7726655359999,15.2,-0.234267005000017));
#189921=CARTESIAN_POINT('Ctrl Pts',(10.7726655359999,11.6,-0.234267005000018));
#189922=CARTESIAN_POINT('Ctrl Pts',(10.7701964279999,15.2,-0.233482574000017));
#189923=CARTESIAN_POINT('Ctrl Pts',(10.7701964279999,11.6,-0.233482574000017));
#189924=CARTESIAN_POINT('Ctrl Pts',(10.7677323879999,15.2,-0.232702063000012));
#189925=CARTESIAN_POINT('Ctrl Pts',(10.7677323879999,11.6,-0.232702063000013));
#189926=CARTESIAN_POINT('Ctrl Pts',(10.7652734269999,15.2,-0.231925472000012));
#189927=CARTESIAN_POINT('Ctrl Pts',(10.7652734269999,11.6,-0.231925472000012));
#189928=CARTESIAN_POINT('Ctrl Pts',(10.7628195609999,15.2,-0.231152792000016));
#189929=CARTESIAN_POINT('Ctrl Pts',(10.7628195609999,11.6,-0.231152792000016));
#189930=CARTESIAN_POINT('Ctrl Pts',(10.7603708009999,15.2,-0.230384019000014));
#189931=CARTESIAN_POINT('Ctrl Pts',(10.7603708009999,11.6,-0.230384019000014));
#189932=CARTESIAN_POINT('Ctrl Pts',(10.7579271629999,15.2,-0.229619149000015));
#189933=CARTESIAN_POINT('Ctrl Pts',(10.7579271629999,11.6,-0.229619149000016));
#189934=CARTESIAN_POINT('Ctrl Pts',(10.7554886599999,15.2,-0.228858176000015));
#189935=CARTESIAN_POINT('Ctrl Pts',(10.7554886599999,11.6,-0.228858176000016));
#189936=CARTESIAN_POINT('Ctrl Pts',(10.7530553059999,15.2,-0.228101094000017));
#189937=CARTESIAN_POINT('Ctrl Pts',(10.7530553059999,11.6,-0.228101094000018));
#189938=CARTESIAN_POINT('Ctrl Pts',(10.7506271149999,15.2,-0.227347899000012));
#189939=CARTESIAN_POINT('Ctrl Pts',(10.7506271149999,11.6,-0.227347899000013));
#189940=CARTESIAN_POINT('Ctrl Pts',(10.7482041009999,15.2,-0.226598584000013));
#189941=CARTESIAN_POINT('Ctrl Pts',(10.7482041009999,11.6,-0.226598584000013));
#189942=CARTESIAN_POINT('Ctrl Pts',(10.7457862769999,15.2,-0.225853146000015));
#189943=CARTESIAN_POINT('Ctrl Pts',(10.7457862769999,11.6,-0.225853146000015));
#189944=CARTESIAN_POINT('Ctrl Pts',(10.7433736579999,15.2,-0.225111577000017));
#189945=CARTESIAN_POINT('Ctrl Pts',(10.7433736579999,11.6,-0.225111577000017));
#189946=CARTESIAN_POINT('Ctrl Pts',(10.7409662579999,15.2,-0.224373875000015));
#189947=CARTESIAN_POINT('Ctrl Pts',(10.7409662579999,11.6,-0.224373875000015));
#189948=CARTESIAN_POINT('Ctrl Pts',(10.7385640919999,15.2,-0.223640032000016));
#189949=CARTESIAN_POINT('Ctrl Pts',(10.7385640919999,11.6,-0.223640032000017));
#189950=CARTESIAN_POINT('Ctrl Pts',(10.7361671709999,15.2,-0.222910044000013));
#189951=CARTESIAN_POINT('Ctrl Pts',(10.7361671709999,11.6,-0.222910044000014));
#189952=CARTESIAN_POINT('Ctrl Pts',(10.7337755109999,15.2,-0.222183905000013));
#189953=CARTESIAN_POINT('Ctrl Pts',(10.7337755109999,11.6,-0.222183905000013));
#189954=CARTESIAN_POINT('Ctrl Pts',(10.7313891279999,15.2,-0.221461609000015));
#189955=CARTESIAN_POINT('Ctrl Pts',(10.7313891279999,11.6,-0.221461609000016));
#189956=CARTESIAN_POINT('Ctrl Pts',(10.7290080319999,15.2,-0.220743152000011));
#189957=CARTESIAN_POINT('Ctrl Pts',(10.7290080319999,11.6,-0.220743152000012));
#189958=CARTESIAN_POINT('Ctrl Pts',(10.7266322409999,15.2,-0.220028527000018));
#189959=CARTESIAN_POINT('Ctrl Pts',(10.7266322409999,11.6,-0.220028527000018));
#189960=CARTESIAN_POINT('Ctrl Pts',(10.7242617679999,15.2,-0.219317729000017));
#189961=CARTESIAN_POINT('Ctrl Pts',(10.7242617679999,11.6,-0.219317729000017));
#189962=CARTESIAN_POINT('Ctrl Pts',(10.7218966269999,15.2,-0.218610753000017));
#189963=CARTESIAN_POINT('Ctrl Pts',(10.7218966269999,11.6,-0.218610753000017));
#189964=CARTESIAN_POINT('Ctrl Pts',(10.7195368329999,15.2,-0.217907593000017));
#189965=CARTESIAN_POINT('Ctrl Pts',(10.7195368329999,11.6,-0.217907593000018));
#189966=CARTESIAN_POINT('Ctrl Pts',(10.7171823989999,15.2,-0.217208244000013));
#189967=CARTESIAN_POINT('Ctrl Pts',(10.7171823989999,11.6,-0.217208244000014));
#189968=CARTESIAN_POINT('Ctrl Pts',(10.7148333409999,15.2,-0.216512699000013));
#189969=CARTESIAN_POINT('Ctrl Pts',(10.7148333409999,11.6,-0.216512699000014));
#189970=CARTESIAN_POINT('Ctrl Pts',(10.7124896719999,15.2,-0.215820955000012));
#189971=CARTESIAN_POINT('Ctrl Pts',(10.7124896719999,11.6,-0.215820955000013));
#189972=CARTESIAN_POINT('Ctrl Pts',(10.7101514079999,15.2,-0.215133003000014));
#189973=CARTESIAN_POINT('Ctrl Pts',(10.7101514079999,11.6,-0.215133003000015));
#189974=CARTESIAN_POINT('Ctrl Pts',(10.7078185619999,15.2,-0.214448839000014));
#189975=CARTESIAN_POINT('Ctrl Pts',(10.7078185619999,11.6,-0.214448839000015));
#189976=CARTESIAN_POINT('Ctrl Pts',(10.7054911499999,15.2,-0.213768458000012));
#189977=CARTESIAN_POINT('Ctrl Pts',(10.7054911499999,11.6,-0.213768458000013));
#189978=CARTESIAN_POINT('Ctrl Pts',(10.7031691859999,15.2,-0.213091853000016));
#189979=CARTESIAN_POINT('Ctrl Pts',(10.7031691859999,11.6,-0.213091853000016));
#189980=CARTESIAN_POINT('Ctrl Pts',(10.7008526839999,15.2,-0.212419018000016));
#189981=CARTESIAN_POINT('Ctrl Pts',(10.7008526839999,11.6,-0.212419018000017));
#189982=CARTESIAN_POINT('Ctrl Pts',(10.6985416599999,15.2,-0.211749949000013));
#189983=CARTESIAN_POINT('Ctrl Pts',(10.6985416599999,11.6,-0.211749949000013));
#189984=CARTESIAN_POINT('Ctrl Pts',(10.6962361279999,15.2,-0.211084638000014));
#189985=CARTESIAN_POINT('Ctrl Pts',(10.6962361279999,11.6,-0.211084638000015));
#189986=CARTESIAN_POINT('Ctrl Pts',(10.6939361019999,15.2,-0.210423081000015));
#189987=CARTESIAN_POINT('Ctrl Pts',(10.6939361019999,11.6,-0.210423081000016));
#189988=CARTESIAN_POINT('Ctrl Pts',(10.6916415969999,15.2,-0.209765271000015));
#189989=CARTESIAN_POINT('Ctrl Pts',(10.6916415969999,11.6,-0.209765271000016));
#189990=CARTESIAN_POINT('Ctrl Pts',(10.6893526289999,15.2,-0.209111203000014));
#189991=CARTESIAN_POINT('Ctrl Pts',(10.6893526289999,11.6,-0.209111203000015));
#189992=CARTESIAN_POINT('Ctrl Pts',(10.6870692119999,15.2,-0.208460870000016));
#189993=CARTESIAN_POINT('Ctrl Pts',(10.6870692119999,11.6,-0.208460870000016));
#189994=CARTESIAN_POINT('Ctrl Pts',(10.6847913619999,15.2,-0.207814266000015));
#189995=CARTESIAN_POINT('Ctrl Pts',(10.6847913619999,11.6,-0.207814266000015));
#189996=CARTESIAN_POINT('Ctrl Pts',(10.6825190919999,15.2,-0.207171387000016));
#189997=CARTESIAN_POINT('Ctrl Pts',(10.6825190919999,11.6,-0.207171387000016));
#189998=CARTESIAN_POINT('Ctrl Pts',(10.6802524189999,15.2,-0.206532225000018));
#189999=CARTESIAN_POINT('Ctrl Pts',(10.6802524189999,11.6,-0.206532225000018));
#190000=CARTESIAN_POINT('Ctrl Pts',(10.6779913559999,15.2,-0.205896774000016));
#190001=CARTESIAN_POINT('Ctrl Pts',(10.6779913559999,11.6,-0.205896774000017));
#190002=CARTESIAN_POINT('Ctrl Pts',(10.6757359199999,15.2,-0.205265028000015));
#190003=CARTESIAN_POINT('Ctrl Pts',(10.6757359199999,11.6,-0.205265028000015));
#190004=CARTESIAN_POINT('Ctrl Pts',(10.6734861239999,15.2,-0.204636983000013));
#190005=CARTESIAN_POINT('Ctrl Pts',(10.6734861239999,11.6,-0.204636983000013));
#190006=CARTESIAN_POINT('Ctrl Pts',(10.6712419859999,15.2,-0.204012630000014));
#190007=CARTESIAN_POINT('Ctrl Pts',(10.6712419859999,11.6,-0.204012630000015));
#190008=CARTESIAN_POINT('Ctrl Pts',(10.6690035179999,15.2,-0.203391965000015));
#190009=CARTESIAN_POINT('Ctrl Pts',(10.6690035179999,11.6,-0.203391965000015));
#190010=CARTESIAN_POINT('Ctrl Pts',(10.6667707369999,15.2,-0.202774980000013));
#190011=CARTESIAN_POINT('Ctrl Pts',(10.6667707369999,11.6,-0.202774980000014));
#190012=CARTESIAN_POINT('Ctrl Pts',(10.6645436589999,15.2,-0.202161669000014));
#190013=CARTESIAN_POINT('Ctrl Pts',(10.6645436589999,11.6,-0.202161669000014));
#190014=CARTESIAN_POINT('Ctrl Pts',(10.6623222969999,15.2,-0.201552028000016));
#190015=CARTESIAN_POINT('Ctrl Pts',(10.6623222969999,11.6,-0.201552028000016));
#190016=CARTESIAN_POINT('Ctrl Pts',(10.6601066689999,15.2,-0.200946048000015));
#190017=CARTESIAN_POINT('Ctrl Pts',(10.6601066689999,11.6,-0.200946048000015));
#190018=CARTESIAN_POINT('Ctrl Pts',(10.6578967889999,15.2,-0.200343724000014));
#190019=CARTESIAN_POINT('Ctrl Pts',(10.6578967889999,11.6,-0.200343724000014));
#190020=CARTESIAN_POINT('Ctrl Pts',(10.6556926709999,15.2,-0.199745050000013));
#190021=CARTESIAN_POINT('Ctrl Pts',(10.6556926709999,11.6,-0.199745050000014));
#190022=CARTESIAN_POINT('Ctrl Pts',(10.6534943329999,15.2,-0.199150020000012));
#190023=CARTESIAN_POINT('Ctrl Pts',(10.6534943329999,11.6,-0.199150020000012));
#190024=CARTESIAN_POINT('Ctrl Pts',(10.6513017899999,15.2,-0.198558626000014));
#190025=CARTESIAN_POINT('Ctrl Pts',(10.6513017899999,11.6,-0.198558626000014));
#190026=CARTESIAN_POINT('Ctrl Pts',(10.6491150549999,15.2,-0.197970862000014));
#190027=CARTESIAN_POINT('Ctrl Pts',(10.6491150549999,11.6,-0.197970862000015));
#190028=CARTESIAN_POINT('Ctrl Pts',(10.6469341469999,15.2,-0.197386722000013));
#190029=CARTESIAN_POINT('Ctrl Pts',(10.6469341469999,11.6,-0.197386722000013));
#190030=CARTESIAN_POINT('Ctrl Pts',(10.6447590809999,15.2,-0.196806200000013));
#190031=CARTESIAN_POINT('Ctrl Pts',(10.6447590809999,11.6,-0.196806200000013));
#190032=CARTESIAN_POINT('Ctrl Pts',(10.6425898709999,15.2,-0.196229289000014));
#190033=CARTESIAN_POINT('Ctrl Pts',(10.6425898709999,11.6,-0.196229289000014));
#190034=CARTESIAN_POINT('Ctrl Pts',(10.6404265339999,15.2,-0.195655982000016));
#190035=CARTESIAN_POINT('Ctrl Pts',(10.6404265339999,11.6,-0.195655982000016));
#190036=CARTESIAN_POINT('Ctrl Pts',(10.6382690849999,15.2,-0.195086273000014));
#190037=CARTESIAN_POINT('Ctrl Pts',(10.6382690849999,11.6,-0.195086273000014));
#190038=CARTESIAN_POINT('Ctrl Pts',(10.6361175409999,15.2,-0.194520155000015));
#190039=CARTESIAN_POINT('Ctrl Pts',(10.6361175409999,11.6,-0.194520155000016));
#190040=CARTESIAN_POINT('Ctrl Pts',(10.6339719169999,15.2,-0.193957622000016));
#190041=CARTESIAN_POINT('Ctrl Pts',(10.6339719169999,11.6,-0.193957622000017));
#190042=CARTESIAN_POINT('Ctrl Pts',(10.6318322289999,15.2,-0.193398667000015));
#190043=CARTESIAN_POINT('Ctrl Pts',(10.6318322289999,11.6,-0.193398667000016));
#190044=CARTESIAN_POINT('Ctrl Pts',(10.6296984919999,15.2,-0.192843283000013));
#190045=CARTESIAN_POINT('Ctrl Pts',(10.6296984919999,11.6,-0.192843283000013));
#190046=CARTESIAN_POINT('Ctrl Pts',(10.6275707239999,15.2,-0.192291464000016));
#190047=CARTESIAN_POINT('Ctrl Pts',(10.6275707239999,11.6,-0.192291464000017));
#190048=CARTESIAN_POINT('Ctrl Pts',(10.6254489389999,15.2,-0.191743203000012));
#190049=CARTESIAN_POINT('Ctrl Pts',(10.6254489389999,11.6,-0.191743203000013));
#190050=CARTESIAN_POINT('Ctrl Pts',(10.6233331559999,15.2,-0.191198492000013));
#190051=CARTESIAN_POINT('Ctrl Pts',(10.6233331559999,11.6,-0.191198492000014));
#190052=CARTESIAN_POINT('Ctrl Pts',(10.6212233869999,15.2,-0.190657326000014));
#190053=CARTESIAN_POINT('Ctrl Pts',(10.6212233869999,11.6,-0.190657326000015));
#190054=CARTESIAN_POINT('Ctrl Pts',(10.6191196519999,15.2,-0.190119697000015));
#190055=CARTESIAN_POINT('Ctrl Pts',(10.6191196519999,11.6,-0.190119697000016));
#190056=CARTESIAN_POINT('Ctrl Pts',(10.6170219649999,15.2,-0.189585598000015));
#190057=CARTESIAN_POINT('Ctrl Pts',(10.6170219649999,11.6,-0.189585598000015));
#190058=CARTESIAN_POINT('Ctrl Pts',(10.6149303439999,15.2,-0.189055023000013));
#190059=CARTESIAN_POINT('Ctrl Pts',(10.6149303439999,11.6,-0.189055023000014));
#190060=CARTESIAN_POINT('Ctrl Pts',(10.6128448019999,15.2,-0.188527965000014));
#190061=CARTESIAN_POINT('Ctrl Pts',(10.6128448019999,11.6,-0.188527965000014));
#190062=CARTESIAN_POINT('Ctrl Pts',(10.6107653599999,15.2,-0.188004416000016));
#190063=CARTESIAN_POINT('Ctrl Pts',(10.6107653599999,11.6,-0.188004416000016));
#190064=CARTESIAN_POINT('Ctrl Pts',(10.6086920309999,15.2,-0.187484371000015));
#190065=CARTESIAN_POINT('Ctrl Pts',(10.6086920309999,11.6,-0.187484371000016));
#190066=CARTESIAN_POINT('Ctrl Pts',(10.6066248309999,15.2,-0.186967820000015));
#190067=CARTESIAN_POINT('Ctrl Pts',(10.6066248309999,11.6,-0.186967820000015));
#190068=CARTESIAN_POINT('Ctrl Pts',(10.6045637799999,15.2,-0.186454758000014));
#190069=CARTESIAN_POINT('Ctrl Pts',(10.6045637799999,11.6,-0.186454758000015));
#190070=CARTESIAN_POINT('Ctrl Pts',(10.6025088909999,15.2,-0.185945177000013));
#190071=CARTESIAN_POINT('Ctrl Pts',(10.6025088909999,11.6,-0.185945177000014));
#190072=CARTESIAN_POINT('Ctrl Pts',(10.6004601839999,15.2,-0.185439072000015));
#190073=CARTESIAN_POINT('Ctrl Pts',(10.6004601839999,11.6,-0.185439072000016));
#190074=CARTESIAN_POINT('Ctrl Pts',(10.5984176719999,15.2,-0.184936432000011));
#190075=CARTESIAN_POINT('Ctrl Pts',(10.5984176719999,11.6,-0.184936432000012));
#190076=CARTESIAN_POINT('Ctrl Pts',(10.5963813739999,15.2,-0.184437252000014));
#190077=CARTESIAN_POINT('Ctrl Pts',(10.5963813739999,11.6,-0.184437252000014));
#190078=CARTESIAN_POINT('Ctrl Pts',(10.5943513069999,15.2,-0.183941526000013));
#190079=CARTESIAN_POINT('Ctrl Pts',(10.5943513069999,11.6,-0.183941526000014));
#190080=CARTESIAN_POINT('Ctrl Pts',(10.5923274859999,15.2,-0.183449245000014));
#190081=CARTESIAN_POINT('Ctrl Pts',(10.5923274859999,11.6,-0.183449245000014));
#190082=CARTESIAN_POINT('Ctrl Pts',(10.5903099289999,15.2,-0.182960401000014));
#190083=CARTESIAN_POINT('Ctrl Pts',(10.5903099289999,11.6,-0.182960401000015));
#190084=CARTESIAN_POINT('Ctrl Pts',(10.5882986539999,15.2,-0.182474988000014));
#190085=CARTESIAN_POINT('Ctrl Pts',(10.5882986539999,11.6,-0.182474988000015));
#190086=CARTESIAN_POINT('Ctrl Pts',(10.5862936749999,15.2,-0.181992998000013));
#190087=CARTESIAN_POINT('Ctrl Pts',(10.5862936749999,11.6,-0.181992998000014));
#190088=CARTESIAN_POINT('Ctrl Pts',(10.5842950119999,15.2,-0.181514425000016));
#190089=CARTESIAN_POINT('Ctrl Pts',(10.5842950119999,11.6,-0.181514425000016));
#190090=CARTESIAN_POINT('Ctrl Pts',(10.5823026799999,15.2,-0.181039259000015));
#190091=CARTESIAN_POINT('Ctrl Pts',(10.5823026799999,11.6,-0.181039259000016));
#190092=CARTESIAN_POINT('Ctrl Pts',(10.5803166979999,15.2,-0.180567496000013));
#190093=CARTESIAN_POINT('Ctrl Pts',(10.5803166979999,11.6,-0.180567496000013));
#190094=CARTESIAN_POINT('Ctrl Pts',(10.5783370809999,15.2,-0.180099124000015));
#190095=CARTESIAN_POINT('Ctrl Pts',(10.5783370809999,11.6,-0.180099124000015));
#190096=CARTESIAN_POINT('Ctrl Pts',(10.5763638469999,15.2,-0.179634139000013));
#190097=CARTESIAN_POINT('Ctrl Pts',(10.5763638469999,11.6,-0.179634139000014));
#190098=CARTESIAN_POINT('Ctrl Pts',(10.5743970139999,15.2,-0.179172532000016));
#190099=CARTESIAN_POINT('Ctrl Pts',(10.5743970139999,11.6,-0.179172532000016));
#190100=CARTESIAN_POINT('Ctrl Pts',(10.5724365989999,15.2,-0.178714295000013));
#190101=CARTESIAN_POINT('Ctrl Pts',(10.5724365989999,11.6,-0.178714295000014));
#190102=CARTESIAN_POINT('Ctrl Pts',(10.5704826189999,15.2,-0.178259423000018));
#190103=CARTESIAN_POINT('Ctrl Pts',(10.5704826189999,11.6,-0.178259423000018));
#190104=CARTESIAN_POINT('Ctrl Pts',(10.5685350909999,15.2,-0.177807905000016));
#190105=CARTESIAN_POINT('Ctrl Pts',(10.5685350909999,11.6,-0.177807905000016));
#190106=CARTESIAN_POINT('Ctrl Pts',(10.5665940339999,15.2,-0.177359733000015));
#190107=CARTESIAN_POINT('Ctrl Pts',(10.5665940339999,11.6,-0.177359733000016));
#190108=CARTESIAN_POINT('Ctrl Pts',(10.5646594639999,15.2,-0.176914903000016));
#190109=CARTESIAN_POINT('Ctrl Pts',(10.5646594639999,11.6,-0.176914903000017));
#190110=CARTESIAN_POINT('Ctrl Pts',(10.5627313999999,15.2,-0.176473403000017));
#190111=CARTESIAN_POINT('Ctrl Pts',(10.5627313999999,11.6,-0.176473403000017));
#190112=CARTESIAN_POINT('Ctrl Pts',(10.5608098579999,15.2,-0.176035228000018));
#190113=CARTESIAN_POINT('Ctrl Pts',(10.5608098579999,11.6,-0.176035228000018));
#190114=CARTESIAN_POINT('Ctrl Pts',(10.5588948559999,15.2,-0.175600368000013));
#190115=CARTESIAN_POINT('Ctrl Pts',(10.5588948559999,11.6,-0.175600368000013));
#190116=CARTESIAN_POINT('Ctrl Pts',(10.5569864129999,15.2,-0.175168818000015));
#190117=CARTESIAN_POINT('Ctrl Pts',(10.5569864129999,11.6,-0.175168818000016));
#190118=CARTESIAN_POINT('Ctrl Pts',(10.5550845449999,15.2,-0.174740567000011));
#190119=CARTESIAN_POINT('Ctrl Pts',(10.5550845449999,11.6,-0.174740567000012));
#190120=CARTESIAN_POINT('Ctrl Pts',(10.5531892719999,15.2,-0.174315609000013));
#190121=CARTESIAN_POINT('Ctrl Pts',(10.5531892719999,11.6,-0.174315609000014));
#190122=CARTESIAN_POINT('Ctrl Pts',(10.5513006109999,15.2,-0.173893935000016));
#190123=CARTESIAN_POINT('Ctrl Pts',(10.5513006109999,11.6,-0.173893935000016));
#190124=CARTESIAN_POINT('Ctrl Pts',(10.5494185789999,15.2,-0.173475536000014));
#190125=CARTESIAN_POINT('Ctrl Pts',(10.5494185789999,11.6,-0.173475536000014));
#190126=CARTESIAN_POINT('Ctrl Pts',(10.5475431949999,15.2,-0.173060406000012));
#190127=CARTESIAN_POINT('Ctrl Pts',(10.5475431949999,11.6,-0.173060406000012));
#190128=CARTESIAN_POINT('Ctrl Pts',(10.5456744759999,15.2,-0.172648535000013));
#190129=CARTESIAN_POINT('Ctrl Pts',(10.5456744759999,11.6,-0.172648535000013));
#190130=CARTESIAN_POINT('Ctrl Pts',(10.5438124429999,15.2,-0.172239916000017));
#190131=CARTESIAN_POINT('Ctrl Pts',(10.5438124429999,11.6,-0.172239916000017));
#190132=CARTESIAN_POINT('Ctrl Pts',(10.5419571109999,15.2,-0.171834540000013));
#190133=CARTESIAN_POINT('Ctrl Pts',(10.5419571109999,11.6,-0.171834540000014));
#190134=CARTESIAN_POINT('Ctrl Pts',(10.5401084989999,15.2,-0.171432400000011));
#190135=CARTESIAN_POINT('Ctrl Pts',(10.5401084989999,11.6,-0.171432400000012));
#190136=CARTESIAN_POINT('Ctrl Pts',(10.5382666269999,15.2,-0.171033486000014));
#190137=CARTESIAN_POINT('Ctrl Pts',(10.5382666269999,11.6,-0.171033486000014));
#190138=CARTESIAN_POINT('Ctrl Pts',(10.5364315109999,15.2,-0.170637790000012));
#190139=CARTESIAN_POINT('Ctrl Pts',(10.5364315109999,11.6,-0.170637790000013));
#190140=CARTESIAN_POINT('Ctrl Pts',(10.5346031709999,15.2,-0.170245304000014));
#190141=CARTESIAN_POINT('Ctrl Pts',(10.5346031709999,11.6,-0.170245304000014));
#190142=CARTESIAN_POINT('Ctrl Pts',(10.5327816249999,15.2,-0.169856021000014));
#190143=CARTESIAN_POINT('Ctrl Pts',(10.5327816249999,11.6,-0.169856021000015));
#190144=CARTESIAN_POINT('Ctrl Pts',(10.5309668919999,15.2,-0.169469929000012));
#190145=CARTESIAN_POINT('Ctrl Pts',(10.5309668919999,11.6,-0.169469929000013));
#190146=CARTESIAN_POINT('Ctrl Pts',(10.5291589899999,15.2,-0.169087023000016));
#190147=CARTESIAN_POINT('Ctrl Pts',(10.5291589899999,11.6,-0.169087023000017));
#190148=CARTESIAN_POINT('Ctrl Pts',(10.5273579379999,15.2,-0.168707293000012));
#190149=CARTESIAN_POINT('Ctrl Pts',(10.5273579379999,11.6,-0.168707293000013));
#190150=CARTESIAN_POINT('Ctrl Pts',(10.5255637549999,15.2,-0.168330729000012));
#190151=CARTESIAN_POINT('Ctrl Pts',(10.5255637549999,11.6,-0.168330729000013));
#190152=CARTESIAN_POINT('Ctrl Pts',(10.5237764589999,15.2,-0.167957324000017));
#190153=CARTESIAN_POINT('Ctrl Pts',(10.5237764589999,11.6,-0.167957324000017));
#190154=CARTESIAN_POINT('Ctrl Pts',(10.5219960679999,15.2,-0.167587069000015));
#190155=CARTESIAN_POINT('Ctrl Pts',(10.5219960679999,11.6,-0.167587069000015));
#190156=CARTESIAN_POINT('Ctrl Pts',(10.5202226039999,15.2,-0.167219956000015));
#190157=CARTESIAN_POINT('Ctrl Pts',(10.5202226039999,11.6,-0.167219956000016));
#190158=CARTESIAN_POINT('Ctrl Pts',(10.5184560839999,15.2,-0.166855975000013));
#190159=CARTESIAN_POINT('Ctrl Pts',(10.5184560839999,11.6,-0.166855975000014));
#190160=CARTESIAN_POINT('Ctrl Pts',(10.5166965259999,15.2,-0.166495117000016));
#190161=CARTESIAN_POINT('Ctrl Pts',(10.5166965259999,11.6,-0.166495117000017));
#190162=CARTESIAN_POINT('Ctrl Pts',(10.5149439519999,15.2,-0.166137374000015));
#190163=CARTESIAN_POINT('Ctrl Pts',(10.5149439519999,11.6,-0.166137374000015));
#190164=CARTESIAN_POINT('Ctrl Pts',(10.5131983789999,15.2,-0.165782737000013));
#190165=CARTESIAN_POINT('Ctrl Pts',(10.5131983789999,11.6,-0.165782737000014));
#190166=CARTESIAN_POINT('Ctrl Pts',(10.5114598269999,15.2,-0.165431197000014));
#190167=CARTESIAN_POINT('Ctrl Pts',(10.5114598269999,11.6,-0.165431197000015));
#190168=CARTESIAN_POINT('Ctrl Pts',(10.5097283139999,15.2,-0.165082745000014));
#190169=CARTESIAN_POINT('Ctrl Pts',(10.5097283139999,11.6,-0.165082745000014));
#190170=CARTESIAN_POINT('Ctrl Pts',(10.5080038619999,15.2,-0.164737371000014));
#190171=CARTESIAN_POINT('Ctrl Pts',(10.5080038619999,11.6,-0.164737371000015));
#190172=CARTESIAN_POINT('Ctrl Pts',(10.5062864879999,15.2,-0.164395067000012));
#190173=CARTESIAN_POINT('Ctrl Pts',(10.5062864879999,11.6,-0.164395067000012));
#190174=CARTESIAN_POINT('Ctrl Pts',(10.5045762119999,15.2,-0.164055824000013));
#190175=CARTESIAN_POINT('Ctrl Pts',(10.5045762119999,11.6,-0.164055824000014));
#190176=CARTESIAN_POINT('Ctrl Pts',(10.5028730549999,15.2,-0.163719632000014));
#190177=CARTESIAN_POINT('Ctrl Pts',(10.5028730549999,11.6,-0.163719632000015));
#190178=CARTESIAN_POINT('Ctrl Pts',(10.5011770349999,15.2,-0.163386483000014));
#190179=CARTESIAN_POINT('Ctrl Pts',(10.5011770349999,11.6,-0.163386483000015));
#190180=CARTESIAN_POINT('Ctrl Pts',(10.4994881719999,15.2,-0.163056366000016));
#190181=CARTESIAN_POINT('Ctrl Pts',(10.4994881719999,11.6,-0.163056366000017));
#190182=CARTESIAN_POINT('Ctrl Pts',(10.4978064869999,15.2,-0.162729273000015));
#190183=CARTESIAN_POINT('Ctrl Pts',(10.4978064869999,11.6,-0.162729273000016));
#190184=CARTESIAN_POINT('Ctrl Pts',(10.4961319979999,15.2,-0.162405194000015));
#190185=CARTESIAN_POINT('Ctrl Pts',(10.4961319979999,11.6,-0.162405194000015));
#190186=CARTESIAN_POINT('Ctrl Pts',(10.4944647269999,15.2,-0.162084120000014));
#190187=CARTESIAN_POINT('Ctrl Pts',(10.4944647269999,11.6,-0.162084120000015));
#190188=CARTESIAN_POINT('Ctrl Pts',(10.4928046919999,15.2,-0.161766042000018));
#190189=CARTESIAN_POINT('Ctrl Pts',(10.4928046919999,11.6,-0.161766042000018));
#190190=CARTESIAN_POINT('Ctrl Pts',(10.4911519139999,15.2,-0.161450949000015));
#190191=CARTESIAN_POINT('Ctrl Pts',(10.4911519139999,11.6,-0.161450949000015));
#190192=CARTESIAN_POINT('Ctrl Pts',(10.4895064129999,15.2,-0.161138832000014));
#190193=CARTESIAN_POINT('Ctrl Pts',(10.4895064129999,11.6,-0.161138832000014));
#190194=CARTESIAN_POINT('Ctrl Pts',(10.4878682099999,15.2,-0.160829682000014));
#190195=CARTESIAN_POINT('Ctrl Pts',(10.4878682099999,11.6,-0.160829682000015));
#190196=CARTESIAN_POINT('Ctrl Pts',(10.4862373239999,15.2,-0.160523489000015));
#190197=CARTESIAN_POINT('Ctrl Pts',(10.4862373239999,11.6,-0.160523489000016));
#190198=CARTESIAN_POINT('Ctrl Pts',(10.4846137759999,15.2,-0.160220244000016));
#190199=CARTESIAN_POINT('Ctrl Pts',(10.4846137759999,11.6,-0.160220244000016));
#190200=CARTESIAN_POINT('Ctrl Pts',(10.4829975859999,15.2,-0.159919936000015));
#190201=CARTESIAN_POINT('Ctrl Pts',(10.4829975859999,11.6,-0.159919936000015));
#190202=CARTESIAN_POINT('Ctrl Pts',(10.4813887749999,15.2,-0.159622556000016));
#190203=CARTESIAN_POINT('Ctrl Pts',(10.4813887749999,11.6,-0.159622556000017));
#190204=CARTESIAN_POINT('Ctrl Pts',(10.4797873629999,15.2,-0.159328093000015));
#190205=CARTESIAN_POINT('Ctrl Pts',(10.4797873629999,11.6,-0.159328093000016));
#190206=CARTESIAN_POINT('Ctrl Pts',(10.4781933699999,15.2,-0.159036540000015));
#190207=CARTESIAN_POINT('Ctrl Pts',(10.4781933699999,11.6,-0.159036540000015));
#190208=CARTESIAN_POINT('Ctrl Pts',(10.4766068189999,15.2,-0.158747884000014));
#190209=CARTESIAN_POINT('Ctrl Pts',(10.4766068189999,11.6,-0.158747884000015));
#190210=CARTESIAN_POINT('Ctrl Pts',(10.4750277289999,15.2,-0.158462116000013));
#190211=CARTESIAN_POINT('Ctrl Pts',(10.4750277289999,11.6,-0.158462116000014));
#190212=CARTESIAN_POINT('Ctrl Pts',(10.4734561209999,15.2,-0.158179227000015));
#190213=CARTESIAN_POINT('Ctrl Pts',(10.4734561209999,11.6,-0.158179227000015));
#190214=CARTESIAN_POINT('Ctrl Pts',(10.4718920149999,15.2,-0.157899205000014));
#190215=CARTESIAN_POINT('Ctrl Pts',(10.4718920149999,11.6,-0.157899205000014));
#190216=CARTESIAN_POINT('Ctrl Pts',(10.4703354349999,15.2,-0.157622040000014));
#190217=CARTESIAN_POINT('Ctrl Pts',(10.4703354349999,11.6,-0.157622040000014));
#190218=CARTESIAN_POINT('Ctrl Pts',(10.4687863999999,15.2,-0.157347725000014));
#190219=CARTESIAN_POINT('Ctrl Pts',(10.4687863999999,11.6,-0.157347725000015));
#190220=CARTESIAN_POINT('Ctrl Pts',(10.4672449309999,15.2,-0.157076245000014));
#190221=CARTESIAN_POINT('Ctrl Pts',(10.4672449309999,11.6,-0.157076245000014));
#190222=CARTESIAN_POINT('Ctrl Pts',(10.4657110499999,15.2,-0.156807593000017));
#190223=CARTESIAN_POINT('Ctrl Pts',(10.4657110499999,11.6,-0.156807593000017));
#190224=CARTESIAN_POINT('Ctrl Pts',(10.4641847769999,15.2,-0.156541758000017));
#190225=CARTESIAN_POINT('Ctrl Pts',(10.4641847769999,11.6,-0.156541758000018));
#190226=CARTESIAN_POINT('Ctrl Pts',(10.4626661349999,15.2,-0.156278729000014));
#190227=CARTESIAN_POINT('Ctrl Pts',(10.4626661349999,11.6,-0.156278729000015));
#190228=CARTESIAN_POINT('Ctrl Pts',(10.4611551459999,15.2,-0.156018496000012));
#190229=CARTESIAN_POINT('Ctrl Pts',(10.4611551459999,11.6,-0.156018496000013));
#190230=CARTESIAN_POINT('Ctrl Pts',(10.4596518279999,15.2,-0.155761048000014));
#190231=CARTESIAN_POINT('Ctrl Pts',(10.4596518279999,11.6,-0.155761048000014));
#190232=CARTESIAN_POINT('Ctrl Pts',(10.4581562069999,15.2,-0.155506375000014));
#190233=CARTESIAN_POINT('Ctrl Pts',(10.4581562069999,11.6,-0.155506375000015));
#190234=CARTESIAN_POINT('Ctrl Pts',(10.4566683019999,15.2,-0.155254466000017));
#190235=CARTESIAN_POINT('Ctrl Pts',(10.4566683019999,11.6,-0.155254466000017));
#190236=CARTESIAN_POINT('Ctrl Pts',(10.4551881359999,15.2,-0.155005310000016));
#190237=CARTESIAN_POINT('Ctrl Pts',(10.4551881359999,11.6,-0.155005310000016));
#190238=CARTESIAN_POINT('Ctrl Pts',(10.4537157299999,15.2,-0.154758897000011));
#190239=CARTESIAN_POINT('Ctrl Pts',(10.4537157299999,11.6,-0.154758897000012));
#190240=CARTESIAN_POINT('Ctrl Pts',(10.4522511059999,15.2,-0.154515216000015));
#190241=CARTESIAN_POINT('Ctrl Pts',(10.4522511059999,11.6,-0.154515216000016));
#190242=CARTESIAN_POINT('Ctrl Pts',(10.4507942869999,15.2,-0.154274256000013));
#190243=CARTESIAN_POINT('Ctrl Pts',(10.4507942869999,11.6,-0.154274256000014));
#190244=CARTESIAN_POINT('Ctrl Pts',(10.4493452949999,15.2,-0.154036006000013));
#190245=CARTESIAN_POINT('Ctrl Pts',(10.4493452949999,11.6,-0.154036006000014));
#190246=CARTESIAN_POINT('Ctrl Pts',(10.4479041509999,15.2,-0.153800456000015));
#190247=CARTESIAN_POINT('Ctrl Pts',(10.4479041509999,11.6,-0.153800456000015));
#190248=CARTESIAN_POINT('Ctrl Pts',(10.4464708799999,15.2,-0.153567592000012));
#190249=CARTESIAN_POINT('Ctrl Pts',(10.4464708799999,11.6,-0.153567592000013));
#190250=CARTESIAN_POINT('Ctrl Pts',(10.4450455009999,15.2,-0.153337407000014));
#190251=CARTESIAN_POINT('Ctrl Pts',(10.4450455009999,11.6,-0.153337407000014));
#190252=CARTESIAN_POINT('Ctrl Pts',(10.4436280379999,15.2,-0.153109887000014));
#190253=CARTESIAN_POINT('Ctrl Pts',(10.4436280379999,11.6,-0.153109887000014));
#190254=CARTESIAN_POINT('Ctrl Pts',(10.4422185139999,15.2,-0.152885022000016));
#190255=CARTESIAN_POINT('Ctrl Pts',(10.4422185139999,11.6,-0.152885022000016));
#190256=CARTESIAN_POINT('Ctrl Pts',(10.4408169509999,15.2,-0.152662801000014));
#190257=CARTESIAN_POINT('Ctrl Pts',(10.4408169509999,11.6,-0.152662801000015));
#190258=CARTESIAN_POINT('Ctrl Pts',(10.4394233719999,15.2,-0.152443211000013));
#190259=CARTESIAN_POINT('Ctrl Pts',(10.4394233719999,11.6,-0.152443211000013));
#190260=CARTESIAN_POINT('Ctrl Pts',(10.4380377999999,15.2,-0.152226243000015));
#190261=CARTESIAN_POINT('Ctrl Pts',(10.4380377999999,11.6,-0.152226243000016));
#190262=CARTESIAN_POINT('Ctrl Pts',(10.4366602579999,15.2,-0.152011884000016));
#190263=CARTESIAN_POINT('Ctrl Pts',(10.4366602579999,11.6,-0.152011884000017));
#190264=CARTESIAN_POINT('Ctrl Pts',(10.4352907679999,15.2,-0.151800122000014));
#190265=CARTESIAN_POINT('Ctrl Pts',(10.4352907679999,11.6,-0.151800122000015));
#190266=CARTESIAN_POINT('Ctrl Pts',(10.4339293549999,15.2,-0.151590947000013));
#190267=CARTESIAN_POINT('Ctrl Pts',(10.4339293549999,11.6,-0.151590947000014));
#190268=CARTESIAN_POINT('Ctrl Pts',(10.4325760399999,15.2,-0.151384346000012));
#190269=CARTESIAN_POINT('Ctrl Pts',(10.4325760399999,11.6,-0.151384346000012));
#190270=CARTESIAN_POINT('Ctrl Pts',(10.4312308479999,15.2,-0.151180309000014));
#190271=CARTESIAN_POINT('Ctrl Pts',(10.4312308479999,11.6,-0.151180309000015));
#190272=CARTESIAN_POINT('Ctrl Pts',(10.4298938009999,15.2,-0.150978823000014));
#190273=CARTESIAN_POINT('Ctrl Pts',(10.4298938009999,11.6,-0.150978823000015));
#190274=CARTESIAN_POINT('Ctrl Pts',(10.4285649239999,15.2,-0.150779877000016));
#190275=CARTESIAN_POINT('Ctrl Pts',(10.4285649239999,11.6,-0.150779877000016));
#190276=CARTESIAN_POINT('Ctrl Pts',(10.4272442399999,15.2,-0.150583457000018));
#190277=CARTESIAN_POINT('Ctrl Pts',(10.4272442399999,11.6,-0.150583457000018));
#190278=CARTESIAN_POINT('Ctrl Pts',(10.4259317729999,15.2,-0.150389553000014));
#190279=CARTESIAN_POINT('Ctrl Pts',(10.4259317729999,11.6,-0.150389553000015));
#190280=CARTESIAN_POINT('Ctrl Pts',(10.4246275449999,15.2,-0.150198153000014));
#190281=CARTESIAN_POINT('Ctrl Pts',(10.4246275449999,11.6,-0.150198153000014));
#190282=CARTESIAN_POINT('Ctrl Pts',(10.4233315819999,15.2,-0.150009245000016));
#190283=CARTESIAN_POINT('Ctrl Pts',(10.4233315819999,11.6,-0.150009245000016));
#190284=CARTESIAN_POINT('Ctrl Pts',(10.4220439069999,15.2,-0.149822817000014));
#190285=CARTESIAN_POINT('Ctrl Pts',(10.4220439069999,11.6,-0.149822817000014));
#190286=CARTESIAN_POINT('Ctrl Pts',(10.4207645439999,15.2,-0.149638856000016));
#190287=CARTESIAN_POINT('Ctrl Pts',(10.4207645439999,11.6,-0.149638856000017));
#190288=CARTESIAN_POINT('Ctrl Pts',(10.4194935179999,15.2,-0.149457349000013));
#190289=CARTESIAN_POINT('Ctrl Pts',(10.4194935179999,11.6,-0.149457349000013));
#190290=CARTESIAN_POINT('Ctrl Pts',(10.4182308519999,15.2,-0.149278285000012));
#190291=CARTESIAN_POINT('Ctrl Pts',(10.4182308519999,11.6,-0.149278285000012));
#190292=CARTESIAN_POINT('Ctrl Pts',(10.4169765709999,15.2,-0.149101653000017));
#190293=CARTESIAN_POINT('Ctrl Pts',(10.4169765709999,11.6,-0.149101653000017));
#190294=CARTESIAN_POINT('Ctrl Pts',(10.4157306989999,15.2,-0.148927436000013));
#190295=CARTESIAN_POINT('Ctrl Pts',(10.4157306989999,11.6,-0.148927436000013));
#190296=CARTESIAN_POINT('Ctrl Pts',(10.4144932619999,15.2,-0.148755626000017));
#190297=CARTESIAN_POINT('Ctrl Pts',(10.4144932619999,11.6,-0.148755626000017));
#190298=CARTESIAN_POINT('Ctrl Pts',(10.4132642839999,15.2,-0.148586210000015));
#190299=CARTESIAN_POINT('Ctrl Pts',(10.4132642839999,11.6,-0.148586210000015));
#190300=CARTESIAN_POINT('Ctrl Pts',(10.4120437889999,15.2,-0.148419172000014));
#190301=CARTESIAN_POINT('Ctrl Pts',(10.4120437889999,11.6,-0.148419172000014));
#190302=CARTESIAN_POINT('Ctrl Pts',(10.4108318009999,15.2,-0.148254502000014));
#190303=CARTESIAN_POINT('Ctrl Pts',(10.4108318009999,11.6,-0.148254502000014));
#190304=CARTESIAN_POINT('Ctrl Pts',(10.4096283479999,15.2,-0.148092188000017));
#190305=CARTESIAN_POINT('Ctrl Pts',(10.4096283479999,11.6,-0.148092188000018));
#190306=CARTESIAN_POINT('Ctrl Pts',(10.4084334529999,15.2,-0.147932214000015));
#190307=CARTESIAN_POINT('Ctrl Pts',(10.4084334529999,11.6,-0.147932214000015));
#190308=CARTESIAN_POINT('Ctrl Pts',(10.4072471419999,15.2,-0.147774569000014));
#190309=CARTESIAN_POINT('Ctrl Pts',(10.4072471419999,11.6,-0.147774569000015));
#190310=CARTESIAN_POINT('Ctrl Pts',(10.4060694389999,15.2,-0.147619240000014));
#190311=CARTESIAN_POINT('Ctrl Pts',(10.4060694389999,11.6,-0.147619240000015));
#190312=CARTESIAN_POINT('Ctrl Pts',(10.4049003719999,15.2,-0.147466214000014));
#190313=CARTESIAN_POINT('Ctrl Pts',(10.4049003719999,11.6,-0.147466214000014));
#190314=CARTESIAN_POINT('Ctrl Pts',(10.4037399639999,15.2,-0.147315477000016));
#190315=CARTESIAN_POINT('Ctrl Pts',(10.4037399639999,11.6,-0.147315477000017));
#190316=CARTESIAN_POINT('Ctrl Pts',(10.4025882419999,15.2,-0.147167016000012));
#190317=CARTESIAN_POINT('Ctrl Pts',(10.4025882419999,11.6,-0.147167016000012));
#190318=CARTESIAN_POINT('Ctrl Pts',(10.4014452309999,15.2,-0.147020819000012));
#190319=CARTESIAN_POINT('Ctrl Pts',(10.4014452309999,11.6,-0.147020819000013));
#190320=CARTESIAN_POINT('Ctrl Pts',(10.4003109569999,15.2,-0.146876871000017));
#190321=CARTESIAN_POINT('Ctrl Pts',(10.4003109569999,11.6,-0.146876871000017));
#190322=CARTESIAN_POINT('Ctrl Pts',(10.3991854459999,15.2,-0.146735160000016));
#190323=CARTESIAN_POINT('Ctrl Pts',(10.3991854459999,11.6,-0.146735160000016));
#190324=CARTESIAN_POINT('Ctrl Pts',(10.3980687249999,15.2,-0.146595671000016));
#190325=CARTESIAN_POINT('Ctrl Pts',(10.3980687249999,11.6,-0.146595671000016));
#190326=CARTESIAN_POINT('Ctrl Pts',(10.3969608199999,15.2,-0.146458391000017));
#190327=CARTESIAN_POINT('Ctrl Pts',(10.3969608199999,11.6,-0.146458391000018));
#190328=CARTESIAN_POINT('Ctrl Pts',(10.3958617559999,15.2,-0.146323307000014));
#190329=CARTESIAN_POINT('Ctrl Pts',(10.3958617559999,11.6,-0.146323307000014));
#190330=CARTESIAN_POINT('Ctrl Pts',(10.3947715609999,15.2,-0.146190403000013));
#190331=CARTESIAN_POINT('Ctrl Pts',(10.3947715609999,11.6,-0.146190403000013));
#190332=CARTESIAN_POINT('Ctrl Pts',(10.3936902589999,15.2,-0.146059668000014));
#190333=CARTESIAN_POINT('Ctrl Pts',(10.3936902589999,11.6,-0.146059668000014));
#190334=CARTESIAN_POINT('Ctrl Pts',(10.3926178809999,15.2,-0.145931087000015));
#190335=CARTESIAN_POINT('Ctrl Pts',(10.3926178809999,11.6,-0.145931087000016));
#190336=CARTESIAN_POINT('Ctrl Pts',(10.3915544509999,15.2,-0.145804646000016));
#190337=CARTESIAN_POINT('Ctrl Pts',(10.3915544509999,11.6,-0.145804646000017));
#190338=CARTESIAN_POINT('Ctrl Pts',(10.3904999949999,15.2,-0.145680330000015));
#190339=CARTESIAN_POINT('Ctrl Pts',(10.3904999949999,11.6,-0.145680330000016));
#190340=CARTESIAN_POINT('Ctrl Pts',(10.3894545419999,15.2,-0.145558126000012));
#190341=CARTESIAN_POINT('Ctrl Pts',(10.3894545419999,11.6,-0.145558126000012));
#190342=CARTESIAN_POINT('Ctrl Pts',(10.3884181189999,15.2,-0.145438019000017));
#190343=CARTESIAN_POINT('Ctrl Pts',(10.3884181189999,11.6,-0.145438019000018));
#190344=CARTESIAN_POINT('Ctrl Pts',(10.3873907519999,15.2,-0.145319997000013));
#190345=CARTESIAN_POINT('Ctrl Pts',(10.3873907519999,11.6,-0.145319997000013));
#190346=CARTESIAN_POINT('Ctrl Pts',(10.3863724699999,15.2,-0.145204042000016));
#190347=CARTESIAN_POINT('Ctrl Pts',(10.3863724699999,11.6,-0.145204042000016));
#190348=CARTESIAN_POINT('Ctrl Pts',(10.3853632999999,15.2,-0.145090141000015));
#190349=CARTESIAN_POINT('Ctrl Pts',(10.3853632999999,11.6,-0.145090141000015));
#190350=CARTESIAN_POINT('Ctrl Pts',(10.3843632689999,15.2,-0.144978281000014));
#190351=CARTESIAN_POINT('Ctrl Pts',(10.3843632689999,11.6,-0.144978281000015));
#190352=CARTESIAN_POINT('Ctrl Pts',(10.3833724059999,15.2,-0.144868445000017));
#190353=CARTESIAN_POINT('Ctrl Pts',(10.3833724059999,11.6,-0.144868445000017));
#190354=CARTESIAN_POINT('Ctrl Pts',(10.3823907369999,15.2,-0.144760620000017));
#190355=CARTESIAN_POINT('Ctrl Pts',(10.3823907369999,11.6,-0.144760620000018));
#190356=CARTESIAN_POINT('Ctrl Pts',(10.3814182929999,15.2,-0.144654790000014));
#190357=CARTESIAN_POINT('Ctrl Pts',(10.3814182929999,11.6,-0.144654790000014));
#190358=CARTESIAN_POINT('Ctrl Pts',(10.3804550999999,15.2,-0.144550941000015));
#190359=CARTESIAN_POINT('Ctrl Pts',(10.3804550999999,11.6,-0.144550941000015));
#190360=CARTESIAN_POINT('Ctrl Pts',(10.3795011859999,15.2,-0.144449057000013));
#190361=CARTESIAN_POINT('Ctrl Pts',(10.3795011859999,11.6,-0.144449057000014));
#190362=CARTESIAN_POINT('Ctrl Pts',(10.3785565819999,15.2,-0.144349124000014));
#190363=CARTESIAN_POINT('Ctrl Pts',(10.3785565819999,11.6,-0.144349124000014));
#190364=CARTESIAN_POINT('Ctrl Pts',(10.3776213129999,15.2,-0.144251127000015));
#190365=CARTESIAN_POINT('Ctrl Pts',(10.3776213129999,11.6,-0.144251127000015));
#190366=CARTESIAN_POINT('Ctrl Pts',(10.3766954109999,15.2,-0.144155050000014));
#190367=CARTESIAN_POINT('Ctrl Pts',(10.3766954109999,11.6,-0.144155050000015));
#190368=CARTESIAN_POINT('Ctrl Pts',(10.3757841819999,15.2,-0.144061420000017));
#190369=CARTESIAN_POINT('Ctrl Pts',(10.3757841819999,11.6,-0.144061420000017));
#190370=CARTESIAN_POINT('Ctrl Pts',(10.3750636849999,15.2,-0.143988114000013));
#190371=CARTESIAN_POINT('Ctrl Pts',(10.3750636849999,11.6,-0.143988114000014));
#190372=CARTESIAN_POINT('Ctrl Pts',(10.3745287909999,15.2,-0.143934095000016));
#190373=CARTESIAN_POINT('Ctrl Pts',(10.3745287909999,11.6,-0.143934095000016));
#190374=CARTESIAN_POINT('Ctrl Pts',(10.3741757629999,15.2,-0.143898619000016));
#190375=CARTESIAN_POINT('Ctrl Pts',(10.3741757629999,11.6,-0.143898619000016));
#190376=CARTESIAN_POINT('Ctrl Pts',(10.3740022749999,15.2,-0.143881227000016));
#190377=CARTESIAN_POINT('Ctrl Pts',(10.3740022749999,11.6,-0.143881227000016));
#190378=CARTESIAN_POINT('',(10.3740022745143,12.2,-0.143881227669191));
#190379=CARTESIAN_POINT('',(10.3740022745143,15.2,-0.143881227669191));
#190380=CARTESIAN_POINT('',(10.3740022739999,12.2,-0.143881228000016));
#190381=CARTESIAN_POINT('Ctrl Pts',(11.4869855309999,12.2,-0.546958306000014));
#190382=CARTESIAN_POINT('Ctrl Pts',(11.4836329088539,12.2,-0.545121269824113));
#190383=CARTESIAN_POINT('Ctrl Pts',(11.4802840213634,12.2,-0.543291206986518));
#190384=CARTESIAN_POINT('Ctrl Pts',(11.4769388591068,12.2,-0.541468106410471));
#190385=CARTESIAN_POINT('Ctrl Pts',(11.4735936968502,12.2,-0.539645005834425));
#190386=CARTESIAN_POINT('Ctrl Pts',(11.4702522623749,12.2,-0.537828869725522));
#190387=CARTESIAN_POINT('Ctrl Pts',(11.4669145744124,12.2,-0.536019697075066));
#190388=CARTESIAN_POINT('Ctrl Pts',(11.4635768864498,12.2,-0.53421052442461));
#190389=CARTESIAN_POINT('Ctrl Pts',(11.4602429461721,12.2,-0.532408315160394));
#190390=CARTESIAN_POINT('Ctrl Pts',(11.4569127942509,12.2,-0.530613060641336));
#190391=CARTESIAN_POINT('Ctrl Pts',(11.4535826417247,12.2,-0.528817805796139));
#190392=CARTESIAN_POINT('Ctrl Pts',(11.4502562798913,12.2,-0.52702950746958));
#190393=CARTESIAN_POINT('Ctrl Pts',(11.4469337572423,12.2,-0.525248154128303));
#190394=CARTESIAN_POINT('Ctrl Pts',(11.4436112351968,12.2,-0.523466801110638));
#190395=CARTESIAN_POINT('Ctrl Pts',(11.4402925523679,12.2,-0.521692394659278));
#190396=CARTESIAN_POINT('Ctrl Pts',(11.4369777481137,12.2,-0.519924928099098));
#190397=CARTESIAN_POINT('Ctrl Pts',(11.4336629438594,12.2,-0.518157461538918));
#190398=CARTESIAN_POINT('Ctrl Pts',(11.4303520166751,12.2,-0.516396934242597));
#190399=CARTESIAN_POINT('Ctrl Pts',(11.4270450034886,12.2,-0.514643339715042));
#190400=CARTESIAN_POINT('Ctrl Pts',(11.4237379903021,12.2,-0.512889745187486));
#190401=CARTESIAN_POINT('Ctrl Pts',(11.4204348911314,12.2,-0.511143084062936));
#190402=CARTESIAN_POINT('Ctrl Pts',(11.4171357470279,12.2,-0.509403348034881));
#190403=CARTESIAN_POINT('Ctrl Pts',(11.4138366029244,12.2,-0.507663612006827));
#190404=CARTESIAN_POINT('Ctrl Pts',(11.4105414141562,12.2,-0.505930801676099));
#190405=CARTESIAN_POINT('Ctrl Pts',(11.4072502226087,12.2,-0.504204908613204));
#190406=CARTESIAN_POINT('Ctrl Pts',(11.4039590310613,12.2,-0.502479015550309));
#190407=CARTESIAN_POINT('Ctrl Pts',(11.4006718374802,12.2,-0.500760040078605));
#190408=CARTESIAN_POINT('Ctrl Pts',(11.3973886809323,12.2,-0.499047974889869));
#190409=CARTESIAN_POINT('Ctrl Pts',(11.394105523788,12.2,-0.497335909390109));
#190410=CARTESIAN_POINT('Ctrl Pts',(11.390826404928,12.2,-0.495630752808958));
#190411=CARTESIAN_POINT('Ctrl Pts',(11.3875513632443,12.2,-0.493932498896419));
#190412=CARTESIAN_POINT('Ctrl Pts',(11.3842763221555,12.2,-0.492234245292397));
#190413=CARTESIAN_POINT('Ctrl Pts',(11.3810053589286,12.2,-0.490542893312953));
#190414=CARTESIAN_POINT('Ctrl Pts',(11.3777385150929,12.2,-0.488858436124135));
#190415=CARTESIAN_POINT('Ctrl Pts',(11.3744716712572,12.2,-0.487173978935316));
#190416=CARTESIAN_POINT('Ctrl Pts',(11.3712089465594,12.2,-0.485496416156678));
#190417=CARTESIAN_POINT('Ctrl Pts',(11.3679503829281,12.2,-0.483825738551309));
#190418=CARTESIAN_POINT('Ctrl Pts',(11.3646918192969,12.2,-0.482155060945941));
#190419=CARTESIAN_POINT('Ctrl Pts',(11.3614374165318,12.2,-0.480491269423095));
#190420=CARTESIAN_POINT('Ctrl Pts',(11.3581872154832,12.2,-0.478834355816627));
#190421=CARTESIAN_POINT('Ctrl Pts',(11.3549370144347,12.2,-0.477177442210161));
#190422=CARTESIAN_POINT('Ctrl Pts',(11.3516910159193,12.2,-0.475527406186752));
#190423=CARTESIAN_POINT('Ctrl Pts',(11.3484492608283,12.2,-0.47388423916252));
#190424=CARTESIAN_POINT('Ctrl Pts',(11.3452075057374,12.2,-0.472241072138288));
#190425=CARTESIAN_POINT('Ctrl Pts',(11.3419699946701,12.2,-0.470604774954951));
#190426=CARTESIAN_POINT('Ctrl Pts',(11.3387367688755,12.2,-0.468975337806958));
#190427=CARTESIAN_POINT('Ctrl Pts',(11.335503543081,12.2,-0.467345900658965));
#190428=CARTESIAN_POINT('Ctrl Pts',(11.3322746022863,12.2,-0.465723324144431));
#190429=CARTESIAN_POINT('Ctrl Pts',(11.3290499901946,12.2,-0.464107599577203));
#190430=CARTESIAN_POINT('Ctrl Pts',(11.325825377517,12.2,-0.46249187471645));
#190431=CARTESIAN_POINT('Ctrl Pts',(11.3226050936823,12.2,-0.460883002232627));
#190432=CARTESIAN_POINT('Ctrl Pts',(11.3193891785489,12.2,-0.459280972375732));
#190433=CARTESIAN_POINT('Ctrl Pts',(11.3161732639996,12.2,-0.457678942809872));
#190434=CARTESIAN_POINT('Ctrl Pts',(11.3129617193168,12.2,-0.45608375716865));
#190435=CARTESIAN_POINT('Ctrl Pts',(11.3097545881421,12.2,-0.454495404601949));
#190436=CARTESIAN_POINT('Ctrl Pts',(11.3065474569673,12.2,-0.452907052035249));
#190437=CARTESIAN_POINT('Ctrl Pts',(11.3033447376004,12.2,-0.451325533326077));
#190438=CARTESIAN_POINT('Ctrl Pts',(11.3001464735082,12.2,-0.44975083971663));
#190439=CARTESIAN_POINT('Ctrl Pts',(11.2969482094161,12.2,-0.448176146107184));
#190440=CARTESIAN_POINT('Ctrl Pts',(11.2937544009988,12.2,-0.44660827731411));
#190441=CARTESIAN_POINT('Ctrl Pts',(11.2905650908643,12.2,-0.445047224161904));
#190442=CARTESIAN_POINT('Ctrl Pts',(11.2873757807298,12.2,-0.443486171009697));
#190443=CARTESIAN_POINT('Ctrl Pts',(11.2841909683758,12.2,-0.441931933054628));
#190444=CARTESIAN_POINT('Ctrl Pts',(11.2810106971653,12.2,-0.440384501782759));
#190445=CARTESIAN_POINT('Ctrl Pts',(11.2778304259548,12.2,-0.43883707051089));
#190446=CARTESIAN_POINT('Ctrl Pts',(11.2746546961933,12.2,-0.437296444696212));
#190447=CARTESIAN_POINT('Ctrl Pts',(11.2714835511412,12.2,-0.435762615084349));
#190448=CARTESIAN_POINT('Ctrl Pts',(11.2683124055131,12.2,-0.434228785193839));
#190449=CARTESIAN_POINT('Ctrl Pts',(11.2651458446695,12.2,-0.432701751788574));
#190450=CARTESIAN_POINT('Ctrl Pts',(11.2619839115856,12.2,-0.431181504901892));
#190451=CARTESIAN_POINT('Ctrl Pts',(11.2588219790761,12.2,-0.429661258291389));
#190452=CARTESIAN_POINT('Ctrl Pts',(11.2556646758581,12.2,-0.42814779848052));
#190453=CARTESIAN_POINT('Ctrl Pts',(11.2525120433897,12.2,-0.42664111532752));
#190454=CARTESIAN_POINT('Ctrl Pts',(11.2493594109213,12.2,-0.425134432174519));
#190455=CARTESIAN_POINT('Ctrl Pts',(11.2462114513304,12.2,-0.42363452516778));
#190456=CARTESIAN_POINT('Ctrl Pts',(11.2430682067637,12.2,-0.42214138496528));
#190457=CARTESIAN_POINT('Ctrl Pts',(11.2388772141984,12.2,-0.420150531452365));
#190458=CARTESIAN_POINT('Ctrl Pts',(11.2346946050503,12.2,-0.418171707756432));
#190459=CARTESIAN_POINT('Ctrl Pts',(11.2305204852241,12.2,-0.416204887804882));
#190460=CARTESIAN_POINT('Ctrl Pts',(11.2273898946434,12.2,-0.414729772506245));
#190461=CARTESIAN_POINT('Ctrl Pts',(11.2242640798725,12.2,-0.413261410576182));
#190462=CARTESIAN_POINT('Ctrl Pts',(11.2211430833362,12.2,-0.411799790198013));
#190463=CARTESIAN_POINT('Ctrl Pts',(11.2169817555662,12.2,-0.409850963469666));
#190464=CARTESIAN_POINT('Ctrl Pts',(11.2128289954728,12.2,-0.407914122531416));
#190465=CARTESIAN_POINT('Ctrl Pts',(11.2086849095888,12.2,-0.405989243632441));
#190466=CARTESIAN_POINT('Ctrl Pts',(11.2055768450346,12.2,-0.404545584392643));
#190467=CARTESIAN_POINT('Ctrl Pts',(11.2024736597755,12.2,-0.403108652330341));
#190468=CARTESIAN_POINT('Ctrl Pts',(11.1993753985661,12.2,-0.401678437560079));
#190469=CARTESIAN_POINT('Ctrl Pts',(11.1962771373566,12.2,-0.400248222789816));
#190470=CARTESIAN_POINT('Ctrl Pts',(11.1931838001617,12.2,-0.398824724941605));
#190471=CARTESIAN_POINT('Ctrl Pts',(11.1900954321482,12.2,-0.397407932825503));
#190472=CARTESIAN_POINT('Ctrl Pts',(11.1870070635737,12.2,-0.395991140452016));
#190473=CARTESIAN_POINT('Ctrl Pts',(11.1839236651589,12.2,-0.394581054313751));
#190474=CARTESIAN_POINT('Ctrl Pts',(11.1808452810872,12.2,-0.393177662444036));
#190475=CARTESIAN_POINT('Ctrl Pts',(11.1777668975747,12.2,-0.39177427082927));
#190476=CARTESIAN_POINT('Ctrl Pts',(11.1746935291703,12.2,-0.390377574464148));
#190477=CARTESIAN_POINT('Ctrl Pts',(11.1716252211572,12.2,-0.388987560390236));
#190478=CARTESIAN_POINT('Ctrl Pts',(11.1685569131441,12.2,-0.387597546316323));
#190479=CARTESIAN_POINT('Ctrl Pts',(11.1654936657999,12.2,-0.386214216388258));
#190480=CARTESIAN_POINT('Ctrl Pts',(11.1624355252305,12.2,-0.384837557765384));
#190481=CARTESIAN_POINT('Ctrl Pts',(11.159377384661,12.2,-0.383460899142509));
#190482=CARTESIAN_POINT('Ctrl Pts',(11.1563243500558,12.2,-0.38209091239123));
#190483=CARTESIAN_POINT('Ctrl Pts',(11.153276468986,12.2,-0.380727584767877));
#190484=CARTESIAN_POINT('Ctrl Pts',(11.1492126271905,12.2,-0.378909814438292));
#190485=CARTESIAN_POINT('Ctrl Pts',(11.1451579450302,12.2,-0.377103884222651));
#190486=CARTESIAN_POINT('Ctrl Pts',(11.1411125345885,12.2,-0.375309765181635));
#190487=CARTESIAN_POINT('Ctrl Pts',(11.1370671246979,12.2,-0.373515646385067));
#190488=CARTESIAN_POINT('Ctrl Pts',(11.1330309860561,12.2,-0.371733339120291));
#190489=CARTESIAN_POINT('Ctrl Pts',(11.1290042288292,12.2,-0.369962813653153));
#190490=CARTESIAN_POINT('Ctrl Pts',(11.1249774710536,12.2,-0.368192287944782));
#190491=CARTESIAN_POINT('Ctrl Pts',(11.1209600942279,12.2,-0.366433545350228));
#190492=CARTESIAN_POINT('Ctrl Pts',(11.1169522116434,12.2,-0.36468655427987));
#190493=CARTESIAN_POINT('Ctrl Pts',(11.112944329605,12.2,-0.36293956344754));
#190494=CARTESIAN_POINT('Ctrl Pts',(11.1089459418451,12.2,-0.361204326048066));
#190495=CARTESIAN_POINT('Ctrl Pts',(11.1049571600594,12.2,-0.359480811132644));
#190496=CARTESIAN_POINT('Ctrl Pts',(11.1009683777303,12.2,-0.357757295982392));
#190497=CARTESIAN_POINT('Ctrl Pts',(11.0969892016968,12.2,-0.356045502069655));
#190498=CARTESIAN_POINT('Ctrl Pts',(11.0930197459255,12.2,-0.354345400311095));
#190499=CARTESIAN_POINT('Ctrl Pts',(11.0890502906951,12.2,-0.352645298784174));
#190500=CARTESIAN_POINT('Ctrl Pts',(11.0850905543428,12.2,-0.350956889810494));
#190501=CARTESIAN_POINT('Ctrl Pts',(11.0811406523565,12.2,-0.349280140251676));
#190502=CARTESIAN_POINT('Ctrl Pts',(11.0771907498319,12.2,-0.3476033904644));
#190503=CARTESIAN_POINT('Ctrl Pts',(11.0732506818173,12.2,-0.345938300848709));
#190504=CARTESIAN_POINT('Ctrl Pts',(11.069320563437,12.2,-0.344284839648241));
#190505=CARTESIAN_POINT('Ctrl Pts',(11.0653904455923,12.2,-0.342631378673058));
#190506=CARTESIAN_POINT('Ctrl Pts',(11.0614702769483,12.2,-0.340989545139982));
#190507=CARTESIAN_POINT('Ctrl Pts',(11.0575601731559,12.2,-0.339359307049856));
#190508=CARTESIAN_POINT('Ctrl Pts',(11.0536500688307,12.2,-0.33772906873761));
#190509=CARTESIAN_POINT('Ctrl Pts',(11.0497500299019,12.2,-0.336110426427056));
#190510=CARTESIAN_POINT('Ctrl Pts',(11.0458601735056,12.2,-0.334503345998876));
#190511=CARTESIAN_POINT('Ctrl Pts',(11.0419703176393,12.2,-0.332896265789661));
#190512=CARTESIAN_POINT('Ctrl Pts',(11.0380906431145,12.2,-0.331300747827863));
#190513=CARTESIAN_POINT('Ctrl Pts',(11.0342212693742,12.2,-0.32971675823396));
#190514=CARTESIAN_POINT('Ctrl Pts',(11.0303518951068,12.2,-0.328132768424238));
#190515=CARTESIAN_POINT('Ctrl Pts',(11.0264928214041,12.2,-0.326560306321151));
#190516=CARTESIAN_POINT('Ctrl Pts',(11.0226441657499,12.2,-0.324999337291632));
#190517=CARTESIAN_POINT('Ctrl Pts',(11.0187955100957,12.2,-0.323438368262112));
#190518=CARTESIAN_POINT('Ctrl Pts',(11.0149572732483,12.2,-0.321888894081161));
#190519=CARTESIAN_POINT('Ctrl Pts',(11.0111295743741,12.2,-0.320350876998509));
#190520=CARTESIAN_POINT('Ctrl Pts',(11.0073018760214,12.2,-0.318812860125413));
#190521=CARTESIAN_POINT('Ctrl Pts',(11.0034847161864,12.2,-0.317286302247945));
#190522=CARTESIAN_POINT('Ctrl Pts',(10.9996782157025,12.2,-0.315771165976002));
#190523=CARTESIAN_POINT('Ctrl Pts',(10.9958717146999,12.2,-0.314256029497622));
#190524=CARTESIAN_POINT('Ctrl Pts',(10.9920758723835,12.2,-0.312752315102815));
#190525=CARTESIAN_POINT('Ctrl Pts',(10.9882908101227,12.2,-0.311259986022648));
#190526=CARTESIAN_POINT('Ctrl Pts',(10.9835594825547,12.2,-0.309394574774104));
#190527=CARTESIAN_POINT('Ctrl Pts',(10.9788450003228,12.2,-0.30754695418688));
#190528=CARTESIAN_POINT('Ctrl Pts',(10.9741476003936,12.2,-0.305717049535556));
#190529=CARTESIAN_POINT('Ctrl Pts',(10.9703896807575,12.2,-0.304253125934172));
#190530=CARTESIAN_POINT('Ctrl Pts',(10.9666426956285,12.2,-0.302800541653595));
#190531=CARTESIAN_POINT('Ctrl Pts',(10.9629067678221,12.2,-0.301359256826237));
#190532=CARTESIAN_POINT('Ctrl Pts',(10.9591708395066,12.2,-0.299917971802503));
#190533=CARTESIAN_POINT('Ctrl Pts',(10.9554459682147,12.2,-0.298487987971941));
#190534=CARTESIAN_POINT('Ctrl Pts',(10.9517322784944,12.2,-0.297069264769167));
#190535=CARTESIAN_POINT('Ctrl Pts',(10.9480185892801,12.2,-0.295650541759694));
#190536=CARTESIAN_POINT('Ctrl Pts',(10.9443160825674,12.2,-0.294243080398028));
#190537=CARTESIAN_POINT('Ctrl Pts',(10.9406248835351,12.2,-0.292846840122553));
#190538=CARTESIAN_POINT('Ctrl Pts',(10.9369336839999,12.2,-0.29145059965684));
#190539=CARTESIAN_POINT('Ctrl Pts',(10.9332537922326,12.2,-0.29006558137024));
#190540=CARTESIAN_POINT('Ctrl Pts',(10.9295853347001,12.2,-0.288691744129432));
#190541=CARTESIAN_POINT('Ctrl Pts',(10.9259168776674,12.2,-0.28731790707581));
#190542=CARTESIAN_POINT('Ctrl Pts',(10.9222598558474,12.2,-0.285955250081925));
#190543=CARTESIAN_POINT('Ctrl Pts',(10.9186143959623,12.2,-0.284603733679482));
#190544=CARTESIAN_POINT('Ctrl Pts',(10.9149689355805,12.2,-0.283252217092895));
#190545=CARTESIAN_POINT('Ctrl Pts',(10.9113350371811,12.2,-0.281911840393686));
#190546=CARTESIAN_POINT('Ctrl Pts',(10.9077128302622,12.2,-0.280582560599743));
#190547=CARTESIAN_POINT('Ctrl Pts',(10.9031850718604,12.2,-0.278920960947872));
#190548=CARTESIAN_POINT('Ctrl Pts',(10.8986755801998,12.2,-0.277276702226101));
#190549=CARTESIAN_POINT('Ctrl Pts',(10.8941846109646,12.2,-0.275649699935338));
#190550=CARTESIAN_POINT('Ctrl Pts',(10.8905918358702,12.2,-0.274348098209133));
#190551=CARTESIAN_POINT('Ctrl Pts',(10.8870109143554,12.2,-0.273057540179318));
#190552=CARTESIAN_POINT('Ctrl Pts',(10.8834419784678,12.2,-0.271777981885708));
#190553=CARTESIAN_POINT('Ctrl Pts',(10.8789808082437,12.2,-0.270178533887939));
#190554=CARTESIAN_POINT('Ctrl Pts',(10.8745383625625,12.2,-0.268596275058888));
#190555=CARTESIAN_POINT('Ctrl Pts',(10.870114905756,12.2,-0.26703111533577));
#190556=CARTESIAN_POINT('Ctrl Pts',(10.8665761401179,12.2,-0.265778987489035));
#190557=CARTESIAN_POINT('Ctrl Pts',(10.8630495249284,12.2,-0.264537804054729));
#190558=CARTESIAN_POINT('Ctrl Pts',(10.8595351942377,12.2,-0.263307519432833));
#190559=CARTESIAN_POINT('Ctrl Pts',(10.8560208640258,12.2,-0.262077234978564));
#190560=CARTESIAN_POINT('Ctrl Pts',(10.8525188196687,12.2,-0.260857848346251));
#190561=CARTESIAN_POINT('Ctrl Pts',(10.8490291945563,12.2,-0.259649313883731));
#190562=CARTESIAN_POINT('Ctrl Pts',(10.8455395689685,12.2,-0.258440779256548));
#190563=CARTESIAN_POINT('Ctrl Pts',(10.8420623639215,12.2,-0.257243095903136));
#190564=CARTESIAN_POINT('Ctrl Pts',(10.8385977157334,12.2,-0.256056217894713));
#190565=CARTESIAN_POINT('Ctrl Pts',(10.8351330680175,12.2,-0.254869340048002));
#190566=CARTESIAN_POINT('Ctrl Pts',(10.8316809754046,12.2,-0.253693266357451));
#190567=CARTESIAN_POINT('Ctrl Pts',(10.8282415777956,12.2,-0.252527948673841));
#190568=CARTESIAN_POINT('Ctrl Pts',(10.8248021797179,12.2,-0.251362630831455));
#190569=CARTESIAN_POINT('Ctrl Pts',(10.8213754767546,12.2,-0.250208068436137));
#190570=CARTESIAN_POINT('Ctrl Pts',(10.8179616059976,12.2,-0.249064213757529));
#190571=CARTESIAN_POINT('Ctrl Pts',(10.8145477357056,12.2,-0.247920359234771));
#190572=CARTESIAN_POINT('Ctrl Pts',(10.8111466970838,12.2,-0.246787210765058));
#190573=CARTESIAN_POINT('Ctrl Pts',(10.8077586328038,12.2,-0.245664719633507));
#190574=CARTESIAN_POINT('Ctrl Pts',(10.8043705680623,12.2,-0.244542228349017));
#190575=CARTESIAN_POINT('Ctrl Pts',(10.8009954759054,12.2,-0.243430394209988));
#190576=CARTESIAN_POINT('Ctrl Pts',(10.7976334984999,12.2,-0.242329164483303));
#190577=CARTESIAN_POINT('Ctrl Pts',(10.7942715210944,12.2,-0.241227934756618));
#190578=CARTESIAN_POINT('Ctrl Pts',(10.7909226576766,12.2,-0.240137311931174));
#190579=CARTESIAN_POINT('Ctrl Pts',(10.7875870516629,12.2,-0.239057242540053));
#190580=CARTESIAN_POINT('Ctrl Pts',(10.7842514461036,12.2,-0.237977173296091));
#190581=CARTESIAN_POINT('Ctrl Pts',(10.7809290979606,12.2,-0.236907656688414));
#190582=CARTESIAN_POINT('Ctrl Pts',(10.7776201504938,12.2,-0.235848641492363));
#190583=CARTESIAN_POINT('Ctrl Pts',(10.7743112025762,12.2,-0.23478962615202));
#190584=CARTESIAN_POINT('Ctrl Pts',(10.7710156565991,12.2,-0.233741111310766));
#190585=CARTESIAN_POINT('Ctrl Pts',(10.767733657255,12.2,-0.232703042755253));
#190586=CARTESIAN_POINT('Ctrl Pts',(10.764451658358,12.2,-0.231664974341178));
#190587=CARTESIAN_POINT('Ctrl Pts',(10.7611832059259,12.2,-0.230637352584084));
#190588=CARTESIAN_POINT('Ctrl Pts',(10.7579284470244,12.2,-0.229620123333231));
#190589=CARTESIAN_POINT('Ctrl Pts',(10.7546736876795,12.2,-0.228602893943781));
#190590=CARTESIAN_POINT('Ctrl Pts',(10.751432622162,12.2,-0.227596055778067));
#190591=CARTESIAN_POINT('Ctrl Pts',(10.7482053980483,12.2,-0.226599553063762));
#190592=CARTESIAN_POINT('Ctrl Pts',(10.7449781743744,12.2,-0.22560305048523));
#190593=CARTESIAN_POINT('Ctrl Pts',(10.7417647931259,12.2,-0.224616883622968));
#190594=CARTESIAN_POINT('Ctrl Pts',(10.7385654035532,12.2,-0.223640995813185));
#190595=CARTESIAN_POINT('Ctrl Pts',(10.7345661662604,12.2,-0.222421135951232));
#190596=CARTESIAN_POINT('Ctrl Pts',(10.7305887888932,12.2,-0.221217337023033));
#190597=CARTESIAN_POINT('Ctrl Pts',(10.726633570767,12.2,-0.220029483827759));
#190598=CARTESIAN_POINT('Ctrl Pts',(10.7226783526409,12.2,-0.218841630632484));
#190599=CARTESIAN_POINT('Ctrl Pts',(10.7187452921143,12.2,-0.217669724205901));
#190600=CARTESIAN_POINT('Ctrl Pts',(10.714834688277,12.2,-0.216513649200605));
#190601=CARTESIAN_POINT('Ctrl Pts',(10.7109240844398,12.2,-0.215357574195309));
#190602=CARTESIAN_POINT('Ctrl Pts',(10.7070359377665,12.2,-0.214217329544415));
#190603=CARTESIAN_POINT('Ctrl Pts',(10.7031705515165,12.2,-0.213092795516639));
#190604=CARTESIAN_POINT('Ctrl Pts',(10.6993051652665,12.2,-0.211968261488863));
#190605=CARTESIAN_POINT('Ctrl Pts',(10.6954625399832,12.2,-0.21085943898331));
#190606=CARTESIAN_POINT('Ctrl Pts',(10.6916429812332,12.2,-0.209766206483308));
#190607=CARTESIAN_POINT('Ctrl Pts',(10.6878234224832,12.2,-0.208672973983305));
#190608=CARTESIAN_POINT('Ctrl Pts',(10.6840269327982,12.2,-0.207595331087518));
#190609=CARTESIAN_POINT('Ctrl Pts',(10.6802538215312,12.2,-0.206533152749401));
#190610=CARTESIAN_POINT('Ctrl Pts',(10.6757260881752,12.2,-0.205258538789973));
#190611=CARTESIAN_POINT('Ctrl Pts',(10.6712320193909,12.2,-0.204006195373377));
#190612=CARTESIAN_POINT('Ctrl Pts',(10.6667721629681,12.2,-0.202775898583787));
#190613=CARTESIAN_POINT('Ctrl Pts',(10.6630556158141,12.2,-0.201750651221878));
#190614=CARTESIAN_POINT('Ctrl Pts',(10.6593628272579,12.2,-0.200740715354806));
#190615=CARTESIAN_POINT('Ctrl Pts',(10.655694116215,12.2,-0.199745961048458));
#190616=CARTESIAN_POINT('Ctrl Pts',(10.6505579206749,12.2,-0.198353304997884));
#190617=CARTESIAN_POINT('Ctrl Pts',(10.6454689197468,12.2,-0.196990401379664));
#190618=CARTESIAN_POINT('Ctrl Pts',(10.6404280057812,12.2,-0.19565688142944));
#190619=CARTESIAN_POINT('Ctrl Pts',(10.6368273530047,12.2,-0.194704367194113));
#190620=CARTESIAN_POINT('Ctrl Pts',(10.6332512359276,12.2,-0.193766844250058));
#190621=CARTESIAN_POINT('Ctrl Pts',(10.6296999839844,12.2,-0.192844174181391));
#190622=CARTESIAN_POINT('Ctrl Pts',(10.6261487320413,12.2,-0.191921504112725));
#190623=CARTESIAN_POINT('Ctrl Pts',(10.6226223465778,12.2,-0.191013687017728));
#190624=CARTESIAN_POINT('Ctrl Pts',(10.6191211636269,12.2,-0.190120579404687));
#190625=CARTESIAN_POINT('Ctrl Pts',(10.6156199806759,12.2,-0.189227471791647));
#190626=CARTESIAN_POINT('Ctrl Pts',(10.6121440011632,12.2,-0.18834907546914));
#190627=CARTESIAN_POINT('Ctrl Pts',(10.6086935628319,12.2,-0.187485244428661));
#190628=CARTESIAN_POINT('Ctrl Pts',(10.6052431245007,12.2,-0.186621413388182));
#190629=CARTESIAN_POINT('Ctrl Pts',(10.6018182308698,12.2,-0.185772147645162));
#190630=CARTESIAN_POINT('Ctrl Pts',(10.5984192250386,12.2,-0.18493729688245));
#190631=CARTESIAN_POINT('Ctrl Pts',(10.5950202195779,12.2,-0.184102446210736));
#190632=CARTESIAN_POINT('Ctrl Pts',(10.5916471040972,12.2,-0.183282013924282));
#190633=CARTESIAN_POINT('Ctrl Pts',(10.5883002284877,12.2,-0.182475843872099));
#190634=CARTESIAN_POINT('Ctrl Pts',(10.5849533525133,12.2,-0.181669673732044));
#190635=CARTESIAN_POINT('Ctrl Pts',(10.5816327171829,12.2,-0.180877769213984));
#190636=CARTESIAN_POINT('Ctrl Pts',(10.5783386771807,12.2,-0.180099970810053));
#190637=CARTESIAN_POINT('Ctrl Pts',(10.5737270211059,12.2,-0.179011053027593));
#190638=CARTESIAN_POINT('Ctrl Pts',(10.5691674934979,12.2,-0.177949788899013));
#190639=CARTESIAN_POINT('Ctrl Pts',(10.5646610904766,12.2,-0.176915735558718));
#190640=CARTESIAN_POINT('Ctrl Pts',(10.560798459516,12.2,-0.176029404170184));
#190641=CARTESIAN_POINT('Ctrl Pts',(10.5569748564442,12.2,-0.175163063562843));
#190642=CARTESIAN_POINT('Ctrl Pts',(10.5531909254123,12.2,-0.174316430092268));
#190643=CARTESIAN_POINT('Ctrl Pts',(10.5494069940368,12.2,-0.173469796544791));
#190644=CARTESIAN_POINT('Ctrl Pts',(10.5456627317846,12.2,-0.172642866396811));
#190645=CARTESIAN_POINT('Ctrl Pts',(10.54195879065,12.2,-0.171835348896911));
#190646=CARTESIAN_POINT('Ctrl Pts',(10.5382548498519,12.2,-0.17102783147036));
#190647=CARTESIAN_POINT('Ctrl Pts',(10.5345912315432,12.2,-0.170239724680368));
#190648=CARTESIAN_POINT('Ctrl Pts',(10.5309685997582,12.2,-0.169470725458311));
#190649=CARTESIAN_POINT('Ctrl Pts',(10.5273459679732,12.2,-0.168701726236254));
#190650=CARTESIAN_POINT('Ctrl Pts',(10.5237643214848,12.2,-0.167951834673472));
#190651=CARTESIAN_POINT('Ctrl Pts',(10.5202243403508,12.2,-0.167220739079087));
#190652=CARTESIAN_POINT('Ctrl Pts',(10.5166843588952,12.2,-0.166489643418294));
#190653=CARTESIAN_POINT('Ctrl Pts',(10.513186040767,12.2,-0.165777341977581));
#190654=CARTESIAN_POINT('Ctrl Pts',(10.5097300788315,12.2,-0.165083514441026));
#190655=CARTESIAN_POINT('Ctrl Pts',(10.50627411721,12.2,-0.164389686967494));
#190656=CARTESIAN_POINT('Ctrl Pts',(10.5028605111161,12.2,-0.163714333462085));
#190657=CARTESIAN_POINT('Ctrl Pts',(10.4994899664733,12.2,-0.163057121983021));
#190658=CARTESIAN_POINT('Ctrl Pts',(10.4961194218306,12.2,-0.162399910503956));
#190659=CARTESIAN_POINT('Ctrl Pts',(10.4927919382116,12.2,-0.16176084233712));
#190660=CARTESIAN_POINT('Ctrl Pts',(10.4895082376623,12.2,-0.161139573775585));
#190661=CARTESIAN_POINT('Ctrl Pts',(10.4862245368148,12.2,-0.160518305157617));
#190662=CARTESIAN_POINT('Ctrl Pts',(10.4829846190144,12.2,-0.15991483808353));
#190663=CARTESIAN_POINT('Ctrl Pts',(10.4797892174266,12.2,-0.159328820386113));
#190664=CARTESIAN_POINT('Ctrl Pts',(10.4765938161291,12.2,-0.158742802741927));
#190665=CARTESIAN_POINT('Ctrl Pts',(10.473442932833,12.2,-0.15817423424883));
#190666=CARTESIAN_POINT('Ctrl Pts',(10.4703373212651,12.2,-0.157622752433069));
#190667=CARTESIAN_POINT('Ctrl Pts',(10.4672317096973,12.2,-0.157071270617307));
#190668=CARTESIAN_POINT('Ctrl Pts',(10.4641713672068,12.2,-0.15653687501852));
#190669=CARTESIAN_POINT('Ctrl Pts',(10.461157063981,12.2,-0.156019192286602));
#190670=CARTESIAN_POINT('Ctrl Pts',(10.4581427604814,12.2,-0.155501509507661));
#190671=CARTESIAN_POINT('Ctrl Pts',(10.4551744963291,12.2,-0.155000539055797));
#190672=CARTESIAN_POINT('Ctrl Pts',(10.4522530569231,12.2,-0.154515896197163));
#190673=CARTESIAN_POINT('Ctrl Pts',(10.4493316177824,12.2,-0.154031253382552));
#190674=CARTESIAN_POINT('Ctrl Pts',(10.4464570057329,12.2,-0.153562937449933));
#190675=CARTESIAN_POINT('Ctrl Pts',(10.4436300225877,12.2,-0.153110550717065));
#190676=CARTESIAN_POINT('Ctrl Pts',(10.4403318754137,12.2,-0.152582766167991));
#190677=CARTESIAN_POINT('Ctrl Pts',(10.4370985574772,12.2,-0.15207666472211));
#190678=CARTESIAN_POINT('Ctrl Pts',(10.4339313792373,12.2,-0.15159159047967));
#190679=CARTESIAN_POINT('Ctrl Pts',(10.4312166551726,12.2,-0.15117581257916));
#190680=CARTESIAN_POINT('Ctrl Pts',(10.4285505235436,12.2,-0.150775484964402));
#190681=CARTESIAN_POINT('Ctrl Pts',(10.4259338326408,12.2,-0.150390178979053));
#190682=CARTESIAN_POINT('Ctrl Pts',(10.423317141738,12.2,-0.150004872993703));
#190683=CARTESIAN_POINT('Ctrl Pts',(10.4207498912063,12.2,-0.149634591290477));
#190684=CARTESIAN_POINT('Ctrl Pts',(10.4182329483789,12.2,-0.149278892969435));
#190685=CARTESIAN_POINT('Ctrl Pts',(10.4157160055515,12.2,-0.148923194648394));
#190686=CARTESIAN_POINT('Ctrl Pts',(10.4132493716372,12.2,-0.148582077324715));
#190687=CARTESIAN_POINT('Ctrl Pts',(10.4108339349715,12.2,-0.148255091002302));
#190688=CARTESIAN_POINT('Ctrl Pts',(10.4084184980864,12.2,-0.147928104650187));
#190689=CARTESIAN_POINT('Ctrl Pts',(10.4060542611478,12.2,-0.147615246091123));
#190690=CARTESIAN_POINT('Ctrl Pts',(10.4037421353574,12.2,-0.147316045992075));
#190691=CARTESIAN_POINT('Ctrl Pts',(10.401430009777,12.2,-0.147016845920205));
#190692=CARTESIAN_POINT('Ctrl Pts',(10.3991699947892,12.2,-0.146731306383157));
#190693=CARTESIAN_POINT('Ctrl Pts',(10.3969630302759,12.2,-0.146458939975118));
#190694=CARTESIAN_POINT('Ctrl Pts',(10.39438823821,12.2,-0.146141179149247));
#190695=CARTESIAN_POINT('Ctrl Pts',(10.3918856495939,12.2,-0.145841349057267));
#190696=CARTESIAN_POINT('Ctrl Pts',(10.3894567993783,12.2,-0.145558650261839));
#190697=CARTESIAN_POINT('Ctrl Pts',(10.3873749278729,12.2,-0.145316337021192));
#190698=CARTESIAN_POINT('Ctrl Pts',(10.3853472317298,12.2,-0.145086611134867));
#190699=CARTESIAN_POINT('Ctrl Pts',(10.3833747045424,12.2,-0.144868947725095));
#190700=CARTESIAN_POINT('Ctrl Pts',(10.3800966258014,12.2,-0.144507219987798));
#190701=CARTESIAN_POINT('Ctrl Pts',(10.3769709056722,12.2,-0.144178829281747));
#190702=CARTESIAN_POINT('Ctrl Pts',(10.3740022749999,12.2,-0.143881227000016));
#190703=CARTESIAN_POINT('Ctrl Pts',(10.3740022749999,15.2,-0.143881227000016));
#190704=CARTESIAN_POINT('Ctrl Pts',(10.3757800241214,15.2,-0.144059444586938));
#190705=CARTESIAN_POINT('Ctrl Pts',(10.3776141114604,15.2,-0.144248693896987));
#190706=CARTESIAN_POINT('Ctrl Pts',(10.3795035132429,15.2,-0.144449544719664));
#190707=CARTESIAN_POINT('Ctrl Pts',(10.3814020266759,15.2,-0.144651364146533));
#190708=CARTESIAN_POINT('Ctrl Pts',(10.3833563884146,15.2,-0.144864887714238));
#190709=CARTESIAN_POINT('Ctrl Pts',(10.385365584961,15.2,-0.14509065123853));
#190710=CARTESIAN_POINT('Ctrl Pts',(10.388044513507,15.2,-0.145391669250414));
#190711=CARTESIAN_POINT('Ctrl Pts',(10.3908209228729,15.2,-0.145714448637587));
#190712=CARTESIAN_POINT('Ctrl Pts',(10.3936924900591,15.2,-0.146060206522512));
#190713=CARTESIAN_POINT('Ctrl Pts',(10.3958461653999,15.2,-0.146319524930317));
#190714=CARTESIAN_POINT('Ctrl Pts',(10.3980533672458,15.2,-0.14659176898398));
#190715=CARTESIAN_POINT('Ctrl Pts',(10.4003131477572,15.2,-0.146877430224863));
#190716=CARTESIAN_POINT('Ctrl Pts',(10.4025729282685,15.2,-0.147163091465747));
#190717=CARTESIAN_POINT('Ctrl Pts',(10.4048852841982,15.2,-0.147462171811529));
#190718=CARTESIAN_POINT('Ctrl Pts',(10.4072492937755,15.2,-0.147775147965879));
#190719=CARTESIAN_POINT('Ctrl Pts',(10.4096133035675,15.2,-0.148088124148657));
#190720=CARTESIAN_POINT('Ctrl Pts',(10.412028965728,15.2,-0.148414996054894));
#190721=CARTESIAN_POINT('Ctrl Pts',(10.4144953769886,15.2,-0.148756224508035));
#190722=CARTESIAN_POINT('Ctrl Pts',(10.4169617880251,15.2,-0.149097452930182));
#190723=CARTESIAN_POINT('Ctrl Pts',(10.4194789511848,15.2,-0.149453042596778));
#190724=CARTESIAN_POINT('Ctrl Pts',(10.4220459850082,15.2,-0.149823433749987));
#190725=CARTESIAN_POINT('Ctrl Pts',(10.4246130188316,15.2,-0.150193824903195));
#190726=CARTESIAN_POINT('Ctrl Pts',(10.4272299231919,15.2,-0.150579023848384));
#190727=CARTESIAN_POINT('Ctrl Pts',(10.4298958432254,15.2,-0.150979457936288));
#190728=CARTESIAN_POINT('Ctrl Pts',(10.4325617635011,15.2,-0.151379892060566));
#190729=CARTESIAN_POINT('Ctrl Pts',(10.4352766973889,15.2,-0.151795566197436));
#190730=CARTESIAN_POINT('Ctrl Pts',(10.4380398077927,15.2,-0.152226895305339));
#190731=CARTESIAN_POINT('Ctrl Pts',(10.4408029179456,15.2,-0.152658224374064));
#190732=CARTESIAN_POINT('Ctrl Pts',(10.4436142067169,15.2,-0.153105210956548));
#190733=CARTESIAN_POINT('Ctrl Pts',(10.4464728530428,15.2,-0.153568261691863));
#190734=CARTESIAN_POINT('Ctrl Pts',(10.4493314993687,15.2,-0.154031312427179));
#190735=CARTESIAN_POINT('Ctrl Pts',(10.4522375075401,15.2,-0.154510424983432));
#190736=CARTESIAN_POINT('Ctrl Pts',(10.4551900758475,15.2,-0.155005995714713));
#190737=CARTESIAN_POINT('Ctrl Pts',(10.458142644423,15.2,-0.15550156649101));
#190738=CARTESIAN_POINT('Ctrl Pts',(10.4611417736544,15.2,-0.156013593785998));
#190739=CARTESIAN_POINT('Ctrl Pts',(10.4641866850734,15.2,-0.156542459565971));
#190740=CARTESIAN_POINT('Ctrl Pts',(10.4672315962159,15.2,-0.157071325297905));
#190741=CARTESIAN_POINT('Ctrl Pts',(10.4703222864829,15.2,-0.157617030983772));
#190742=CARTESIAN_POINT('Ctrl Pts',(10.4734579967043,15.2,-0.158179943797402));
#190743=CARTESIAN_POINT('Ctrl Pts',(10.4765937069257,15.2,-0.158742856611032));
#190744=CARTESIAN_POINT('Ctrl Pts',(10.4797744331017,15.2,-0.159322978306633));
#190745=CARTESIAN_POINT('Ctrl Pts',(10.482999430566,15.2,-0.159920667950818));
#190746=CARTESIAN_POINT('Ctrl Pts',(10.4867619278028,15.2,-0.160617972571893));
#190747=CARTESIAN_POINT('Ctrl Pts',(10.4905846827399,15.2,-0.161339189690789));
#190748=CARTESIAN_POINT('Ctrl Pts',(10.4944665360264,15.2,-0.162084868983609));
#190749=CARTESIAN_POINT('Ctrl Pts',(10.4977938386707,15.2,-0.162724022629994));
#190750=CARTESIAN_POINT('Ctrl Pts',(10.5011645619149,15.2,-0.163381150255252));
#190751=CARTESIAN_POINT('Ctrl Pts',(10.504577991539,15.2,-0.164056586729913));
#190752=CARTESIAN_POINT('Ctrl Pts',(10.5079914214732,15.2,-0.164732023265927));
#190753=CARTESIAN_POINT('Ctrl Pts',(10.511447558546,15.2,-0.165425769037539));
#190754=CARTESIAN_POINT('Ctrl Pts',(10.5149457026562,15.2,-0.166138150577636));
#190755=CARTESIAN_POINT('Ctrl Pts',(10.5184438464486,15.2,-0.166850532053025));
#190756=CARTESIAN_POINT('Ctrl Pts',(10.5219840010736,15.2,-0.16758154846736));
#190757=CARTESIAN_POINT('Ctrl Pts',(10.5255654769452,15.2,-0.168331518774267));
#190758=CARTESIAN_POINT('Ctrl Pts',(10.5309376907527,15.2,-0.169456474234627));
#190759=CARTESIAN_POINT('Ctrl Pts',(10.5364028794528,15.2,-0.170624072757087));
#190760=CARTESIAN_POINT('Ctrl Pts',(10.54195879065,15.2,-0.17183534889691));
#190761=CARTESIAN_POINT('Ctrl Pts',(10.5456627317846,15.2,-0.172642866396808));
#190762=CARTESIAN_POINT('Ctrl Pts',(10.5494069940367,15.2,-0.173469796544786));
#190763=CARTESIAN_POINT('Ctrl Pts',(10.5531909254123,15.2,-0.174316430092267));
#190764=CARTESIAN_POINT('Ctrl Pts',(10.5569748564442,15.2,-0.175163063562845));
#190765=CARTESIAN_POINT('Ctrl Pts',(10.560798459516,15.2,-0.176029404170188));
#190766=CARTESIAN_POINT('Ctrl Pts',(10.5646610904766,15.2,-0.176915735558719));
#190767=CARTESIAN_POINT('Ctrl Pts',(10.5685237214373,15.2,-0.177802066947249));
#190768=CARTESIAN_POINT('Ctrl Pts',(10.5724253830885,15.2,-0.178708390075781));
#190769=CARTESIAN_POINT('Ctrl Pts',(10.576365447027,15.2,-0.179634983457898));
#190770=CARTESIAN_POINT('Ctrl Pts',(10.5796488337617,15.2,-0.180407144637717));
#190771=CARTESIAN_POINT('Ctrl Pts',(10.5829588878388,15.2,-0.181193381887345));
#190772=CARTESIAN_POINT('Ctrl Pts',(10.5862952537402,15.2,-0.181993852164381));
#190773=CARTESIAN_POINT('Ctrl Pts',(10.5902988926764,15.2,-0.182954416461924));
#190774=CARTESIAN_POINT('Ctrl Pts',(10.5943404181894,15.2,-0.183935476003593));
#190775=CARTESIAN_POINT('Ctrl Pts',(10.5984192250386,15.2,-0.184937296882449));
#190776=CARTESIAN_POINT('Ctrl Pts',(10.6018182308698,15.2,-0.185772147645162));
#190777=CARTESIAN_POINT('Ctrl Pts',(10.6052431245007,15.2,-0.186621413388184));
#190778=CARTESIAN_POINT('Ctrl Pts',(10.6086935628319,15.2,-0.187485244428661));
#190779=CARTESIAN_POINT('Ctrl Pts',(10.6121440011631,15.2,-0.188349075469137));
#190780=CARTESIAN_POINT('Ctrl Pts',(10.6156199806759,15.2,-0.189227471791648));
#190781=CARTESIAN_POINT('Ctrl Pts',(10.6191211636269,15.2,-0.190120579404687));
#190782=CARTESIAN_POINT('Ctrl Pts',(10.6226223465778,15.2,-0.191013687017726));
#190783=CARTESIAN_POINT('Ctrl Pts',(10.6261487320413,15.2,-0.191921504112721));
#190784=CARTESIAN_POINT('Ctrl Pts',(10.6296999839844,15.2,-0.192844174181391));
#190785=CARTESIAN_POINT('Ctrl Pts',(10.6332512359276,15.2,-0.193766844250061));
#190786=CARTESIAN_POINT('Ctrl Pts',(10.6368273530047,15.2,-0.194704367194112));
#190787=CARTESIAN_POINT('Ctrl Pts',(10.6404280057812,15.2,-0.19565688142944));
#190788=CARTESIAN_POINT('Ctrl Pts',(10.644748788956,15.2,-0.196799898470305));
#190789=CARTESIAN_POINT('Ctrl Pts',(10.6491049027498,15.2,-0.197964503765251));
#190790=CARTESIAN_POINT('Ctrl Pts',(10.6534957812546,15.2,-0.199150928887326));
#190791=CARTESIAN_POINT('Ctrl Pts',(10.6571548468082,15.2,-0.200139616524977));
#190792=CARTESIAN_POINT('Ctrl Pts',(10.6608380563781,15.2,-0.201143458756819));
#190793=CARTESIAN_POINT('Ctrl Pts',(10.6645450875567,15.2,-0.202162586325013));
#190794=CARTESIAN_POINT('Ctrl Pts',(10.6682521187353,15.2,-0.203181713893206));
#190795=CARTESIAN_POINT('Ctrl Pts',(10.6719829715727,15.2,-0.204216126299005));
#190796=CARTESIAN_POINT('Ctrl Pts',(10.6757373296058,15.2,-0.205265953086495));
#190797=CARTESIAN_POINT('Ctrl Pts',(10.679491687639,15.2,-0.206315779873984));
#190798=CARTESIAN_POINT('Ctrl Pts',(10.6832695496582,15.2,-0.207381020669087));
#190799=CARTESIAN_POINT('Ctrl Pts',(10.6870706034764,15.2,-0.208461802196053));
#190800=CARTESIAN_POINT('Ctrl Pts',(10.6908716572947,15.2,-0.20954258372302));
#190801=CARTESIAN_POINT('Ctrl Pts',(10.6946959046941,15.2,-0.210638904294831));
#190802=CARTESIAN_POINT('Ctrl Pts',(10.6985430327484,15.2,-0.211750888460679));
#190803=CARTESIAN_POINT('Ctrl Pts',(10.7023901608028,15.2,-0.212862872626528));
#190804=CARTESIAN_POINT('Ctrl Pts',(10.7062601726189,15.2,-0.213990519292782));
#190805=CARTESIAN_POINT('Ctrl Pts',(10.7101527622704,15.2,-0.215133949916956));
#190806=CARTESIAN_POINT('Ctrl Pts',(10.7148238696827,15.2,-0.216506066616112));
#190807=CARTESIAN_POINT('Ctrl Pts',(10.719527489083,15.2,-0.217900909473521));
#190808=CARTESIAN_POINT('Ctrl Pts',(10.7242631004921,15.2,-0.219318684337112));
#190809=CARTESIAN_POINT('Ctrl Pts',(10.7282094434763,15.2,-0.220500163433032));
#190810=CARTESIAN_POINT('Ctrl Pts',(10.7321780037853,15.2,-0.221697566092568));
#190811=CARTESIAN_POINT('Ctrl Pts',(10.7361684857279,15.2,-0.222911006091261));
#190812=CARTESIAN_POINT('Ctrl Pts',(10.7401589676706,15.2,-0.224124446089953));
#190813=CARTESIAN_POINT('Ctrl Pts',(10.7441713681261,15.2,-0.22535392473877));
#190814=CARTESIAN_POINT('Ctrl Pts',(10.7482053980483,15.2,-0.226599553063764));
#190815=CARTESIAN_POINT('Ctrl Pts',(10.7530462342189,15.2,-0.228094307135222));
#190816=CARTESIAN_POINT('Ctrl Pts',(10.7579182140567,15.2,-0.229612315165725));
#190817=CARTESIAN_POINT('Ctrl Pts',(10.7628208380759,15.2,-0.231153768917997));
#190818=CARTESIAN_POINT('Ctrl Pts',(10.7660892536435,15.2,-0.232181404612829));
#190819=CARTESIAN_POINT('Ctrl Pts',(10.7693712890231,15.2,-0.233219459200759));
#190820=CARTESIAN_POINT('Ctrl Pts',(10.7726667985306,15.2,-0.234267987114358));
#190821=CARTESIAN_POINT('Ctrl Pts',(10.7776100630164,15.2,-0.235840779056186));
#190822=CARTESIAN_POINT('Ctrl Pts',(10.7825836430967,15.2,-0.237437138600533));
#190823=CARTESIAN_POINT('Ctrl Pts',(10.7875870516629,15.2,-0.239057242540053));
#190824=CARTESIAN_POINT('Ctrl Pts',(10.7909226576766,15.2,-0.240137311931172));
#190825=CARTESIAN_POINT('Ctrl Pts',(10.7942715210944,15.2,-0.241227934756618));
#190826=CARTESIAN_POINT('Ctrl Pts',(10.7976334984999,15.2,-0.242329164483303));
#190827=CARTESIAN_POINT('Ctrl Pts',(10.8009954759054,15.2,-0.243430394209989));
#190828=CARTESIAN_POINT('Ctrl Pts',(10.8043705680623,15.2,-0.244542228349019));
#190829=CARTESIAN_POINT('Ctrl Pts',(10.8077586328038,15.2,-0.245664719633506));
#190830=CARTESIAN_POINT('Ctrl Pts',(10.8119937130383,15.2,-0.247067833509706));
#190831=CARTESIAN_POINT('Ctrl Pts',(10.8162490652361,15.2,-0.248487598464472));
#190832=CARTESIAN_POINT('Ctrl Pts',(10.820524412199,15.2,-0.249924113028749));
#190833=CARTESIAN_POINT('Ctrl Pts',(10.8239446903286,15.2,-0.251073324868067));
#190834=CARTESIAN_POINT('Ctrl Pts',(10.8273777670232,15.2,-0.252233255663941));
#190835=CARTESIAN_POINT('Ctrl Pts',(10.8308235037666,15.2,-0.2534039542833));
#190836=CARTESIAN_POINT('Ctrl Pts',(10.8342692405099,15.2,-0.25457465290266));
#190837=CARTESIAN_POINT('Ctrl Pts',(10.8377276367047,15.2,-0.255756119584384));
#190838=CARTESIAN_POINT('Ctrl Pts',(10.8411985547841,15.2,-0.256948403428247));
#190839=CARTESIAN_POINT('Ctrl Pts',(10.8446694723905,15.2,-0.258140687109662));
#190840=CARTESIAN_POINT('Ctrl Pts',(10.8481529131147,15.2,-0.25934378664569));
#190841=CARTESIAN_POINT('Ctrl Pts',(10.8516487394559,15.2,-0.260557750274145));
#190842=CARTESIAN_POINT('Ctrl Pts',(10.8551445662733,15.2,-0.261771714068003));
#190843=CARTESIAN_POINT('Ctrl Pts',(10.8586527798352,15.2,-0.262996540222445));
#190844=CARTESIAN_POINT('Ctrl Pts',(10.8621732440838,15.2,-0.26423227740202));
#190845=CARTESIAN_POINT('Ctrl Pts',(10.8665738241548,15.2,-0.265776948792305));
#190846=CARTESIAN_POINT('Ctrl Pts',(10.87099354659,15.2,-0.267338667316199));
#190847=CARTESIAN_POINT('Ctrl Pts',(10.8754321523555,15.2,-0.26891752120649));
#190848=CARTESIAN_POINT('Ctrl Pts',(10.8798707576371,15.2,-0.270496374924684));
#190849=CARTESIAN_POINT('Ctrl Pts',(10.8843282437872,15.2,-0.272092363677334));
#190850=CARTESIAN_POINT('Ctrl Pts',(10.8888043541311,15.2,-0.273705574263971));
#190851=CARTESIAN_POINT('Ctrl Pts',(10.8932804649629,15.2,-0.275318785026448));
#190852=CARTESIAN_POINT('Ctrl Pts',(10.8977752004055,15.2,-0.276949218713644));
#190853=CARTESIAN_POINT('Ctrl Pts',(10.9022883038763,15.2,-0.278596959267787));
#190854=CARTESIAN_POINT('Ctrl Pts',(10.9058987868496,15.2,-0.279915151782942));
#190855=CARTESIAN_POINT('Ctrl Pts',(10.9095210263433,15.2,-0.281244421230046));
#190856=CARTESIAN_POINT('Ctrl Pts',(10.9131548930024,15.2,-0.282584808475887));
#190857=CARTESIAN_POINT('Ctrl Pts',(10.9167887591663,15.2,-0.2839251955391));
#190858=CARTESIAN_POINT('Ctrl Pts',(10.9204342508077,15.2,-0.285276701309163));
#190859=CARTESIAN_POINT('Ctrl Pts',(10.9240912406187,15.2,-0.28663936825218));
#190860=CARTESIAN_POINT('Ctrl Pts',(10.9286624782561,15.2,-0.288342702070198));
#190861=CARTESIAN_POINT('Ctrl Pts',(10.933251683671,15.2,-0.290063473285158));
#190862=CARTESIAN_POINT('Ctrl Pts',(10.9378586054057,15.2,-0.291801763005941));
#190863=CARTESIAN_POINT('Ctrl Pts',(10.9415441429942,15.2,-0.293192394858356));
#190864=CARTESIAN_POINT('Ctrl Pts',(10.9452410196473,15.2,-0.294594239175797));
#190865=CARTESIAN_POINT('Ctrl Pts',(10.9489491104774,15.2,-0.296007333759269));
#190866=CARTESIAN_POINT('Ctrl Pts',(10.9526572008023,15.2,-0.297420428150207));
#190867=CARTESIAN_POINT('Ctrl Pts',(10.9563765041961,15.2,-0.298844774892099));
#190868=CARTESIAN_POINT('Ctrl Pts',(10.96010689589,15.2,-0.300280411273583));
#190869=CARTESIAN_POINT('Ctrl Pts',(10.9638372880922,15.2,-0.301716047850672));
#190870=CARTESIAN_POINT('Ctrl Pts',(10.9675787682343,15.2,-0.303162975217712));
#190871=CARTESIAN_POINT('Ctrl Pts',(10.9713312132166,15.2,-0.304621232241633));
#190872=CARTESIAN_POINT('Ctrl Pts',(10.9750836581989,15.2,-0.306079489265555));
#190873=CARTESIAN_POINT('Ctrl Pts',(10.9788470681798,15.2,-0.307549075232504));
#190874=CARTESIAN_POINT('Ctrl Pts',(10.9826213191086,15.2,-0.309030027758749));
#190875=CARTESIAN_POINT('Ctrl Pts',(10.9863955695232,15.2,-0.310510980083215));
#190876=CARTESIAN_POINT('Ctrl Pts',(10.990180661984,15.2,-0.312003299567486));
#190877=CARTESIAN_POINT('Ctrl Pts',(10.993976473673,15.2,-0.313507023110482));
#190878=CARTESIAN_POINT('Ctrl Pts',(10.9977722858792,15.2,-0.315010746858359));
#190879=CARTESIAN_POINT('Ctrl Pts',(11.0015788171625,15.2,-0.316525874449976));
#190880=CARTESIAN_POINT('Ctrl Pts',(11.0053959470622,15.2,-0.318052441721547));
#190881=CARTESIAN_POINT('Ctrl Pts',(11.0120759236065,15.2,-0.320723934134804));
#190882=CARTESIAN_POINT('Ctrl Pts',(11.0187883583528,15.2,-0.323430463377752));
#190883=CARTESIAN_POINT('Ctrl Pts',(11.0255326083615,15.2,-0.326172219218818));
#190884=CARTESIAN_POINT('Ctrl Pts',(11.0322768588952,15.2,-0.328913975273349));
#190885=CARTESIAN_POINT('Ctrl Pts',(11.039052925077,15.2,-0.331690955359036));
#190886=CARTESIAN_POINT('Ctrl Pts',(11.0458601735056,15.2,-0.334503345998875));
#190887=CARTESIAN_POINT('Ctrl Pts',(11.0497500299019,15.2,-0.33611042642706));
#190888=CARTESIAN_POINT('Ctrl Pts',(11.0536500688306,15.2,-0.337729068737601));
#190889=CARTESIAN_POINT('Ctrl Pts',(11.0575601731559,15.2,-0.339359307049852));
#190890=CARTESIAN_POINT('Ctrl Pts',(11.0644028549259,15.2,-0.342212223763112));
#190891=CARTESIAN_POINT('Ctrl Pts',(11.0712763598475,15.2,-0.345100650362057));
#190892=CARTESIAN_POINT('Ctrl Pts',(11.0781800703859,15.2,-0.348024763240908));
#190893=CARTESIAN_POINT('Ctrl Pts',(11.0821250482971,15.2,-0.349695685081105));
#190894=CARTESIAN_POINT('Ctrl Pts',(11.0860798900324,15.2,-0.351378258428816));
#190895=CARTESIAN_POINT('Ctrl Pts',(11.0900444790824,15.2,-0.353072516188583));
#190896=CARTESIAN_POINT('Ctrl Pts',(11.0940090675923,15.2,-0.354766773717508));
#190897=CARTESIAN_POINT('Ctrl Pts',(11.0979834043697,15.2,-0.356472715607979));
#190898=CARTESIAN_POINT('Ctrl Pts',(11.1019673755985,15.2,-0.358190371744137));
#190899=CARTESIAN_POINT('Ctrl Pts',(11.1059513473702,15.2,-0.359908028114326));
#190900=CARTESIAN_POINT('Ctrl Pts',(11.1099449541246,15.2,-0.361637398078874));
#190901=CARTESIAN_POINT('Ctrl Pts',(11.1139480825276,15.2,-0.363378514459489));
#190902=CARTESIAN_POINT('Ctrl Pts',(11.1179512103853,15.2,-0.365119630602876));
#190903=CARTESIAN_POINT('Ctrl Pts',(11.1219638605776,15.2,-0.366872491570809));
#190904=CARTESIAN_POINT('Ctrl Pts',(11.125985920359,15.2,-0.368637127703124));
#190905=CARTESIAN_POINT('Ctrl Pts',(11.1300079806883,15.2,-0.37040176407587));
#190906=CARTESIAN_POINT('Ctrl Pts',(11.1340394499741,15.2,-0.372178175419171));
#190907=CARTESIAN_POINT('Ctrl Pts',(11.1380802177499,15.2,-0.373966390516629));
#190908=CARTESIAN_POINT('Ctrl Pts',(11.144141368863,15.2,-0.376648712919171));
#190909=CARTESIAN_POINT('Ctrl Pts',(11.150223442411,15.2,-0.379357595624685));
#190910=CARTESIAN_POINT('Ctrl Pts',(11.1563260656596,15.2,-0.382093132243738));
#190911=CARTESIAN_POINT('Ctrl Pts',(11.1593773772839,15.2,-0.383460900553265));
#190912=CARTESIAN_POINT('Ctrl Pts',(11.1624338258278,15.2,-0.384835332933315));
#190913=CARTESIAN_POINT('Ctrl Pts',(11.1654953658408,15.2,-0.386216440215559));
#190914=CARTESIAN_POINT('Ctrl Pts',(11.1685569064101,15.2,-0.387597547748704));
#190915=CARTESIAN_POINT('Ctrl Pts',(11.1716235383224,15.2,-0.388985332300396));
#190916=CARTESIAN_POINT('Ctrl Pts',(11.1746952154362,15.2,-0.390379802795634));
#190917=CARTESIAN_POINT('Ctrl Pts',(11.1777668919919,15.2,-0.391774273037542));
#190918=CARTESIAN_POINT('Ctrl Pts',(11.1808436140308,15.2,-0.393175430720772));
#190919=CARTESIAN_POINT('Ctrl Pts',(11.1839253355859,15.2,-0.394583286420206));
#190920=CARTESIAN_POINT('Ctrl Pts',(11.187007057141,15.2,-0.395991142119639));
#190921=CARTESIAN_POINT('Ctrl Pts',(11.1900937785343,15.2,-0.397405696546413));
#190922=CARTESIAN_POINT('Ctrl Pts',(11.1931854545194,15.2,-0.398826960251261));
#190923=CARTESIAN_POINT('Ctrl Pts',(11.1962771305045,15.2,-0.400248223956108));
#190924=CARTESIAN_POINT('Ctrl Pts',(11.1993737599957,15.2,-0.401676197327638));
#190925=CARTESIAN_POINT('Ctrl Pts',(11.2024752990221,15.2,-0.403110891448664));
#190926=CARTESIAN_POINT('Ctrl Pts',(11.2076445309205,15.2,-0.405502048403918));
#190927=CARTESIAN_POINT('Ctrl Pts',(11.2128273990221,15.2,-0.407911872788857));
#190928=CARTESIAN_POINT('Ctrl Pts',(11.2180236959666,15.2,-0.410340417233299));
#190929=CARTESIAN_POINT('Ctrl Pts',(11.2221807337487,15.2,-0.412283252894736));
#190930=CARTESIAN_POINT('Ctrl Pts',(11.226346364829,15.2,-0.414238067585351));
#190931=CARTESIAN_POINT('Ctrl Pts',(11.2305204852241,15.2,-0.416204887804882));
#190932=CARTESIAN_POINT('Ctrl Pts',(11.2346946050503,15.2,-0.418171707756433));
#190933=CARTESIAN_POINT('Ctrl Pts',(11.2388772141984,15.2,-0.420150531452363));
#190934=CARTESIAN_POINT('Ctrl Pts',(11.2430682067637,15.2,-0.422141384965282));
#190935=CARTESIAN_POINT('Ctrl Pts',(11.2472591999,15.2,-0.424132238749455));
#190936=CARTESIAN_POINT('Ctrl Pts',(11.2514585765911,15.2,-0.426135121996156));
#190937=CARTESIAN_POINT('Ctrl Pts',(11.2556662324879,15.2,-0.428150058329414));
#190938=CARTESIAN_POINT('Ctrl Pts',(11.2588219741238,15.2,-0.42966126044209));
#190939=CARTESIAN_POINT('Ctrl Pts',(11.2619823732762,15.2,-0.431179242571089));
#190940=CARTESIAN_POINT('Ctrl Pts',(11.2651473863283,15.2,-0.432704014682948));
#190941=CARTESIAN_POINT('Ctrl Pts',(11.2683123993804,15.2,-0.434228786794806));
#190942=CARTESIAN_POINT('Ctrl Pts',(11.2714820257037,15.2,-0.43576034866691));
#190943=CARTESIAN_POINT('Ctrl Pts',(11.2746562223111,15.2,-0.437298710243033));
#190944=CARTESIAN_POINT('Ctrl Pts',(11.2778304189186,15.2,-0.438837071819156));
#190945=CARTESIAN_POINT('Ctrl Pts',(11.2810091860649,15.2,-0.440382231914597));
#190946=CARTESIAN_POINT('Ctrl Pts',(11.2841924797137,15.2,-0.441934201990225));
#190947=CARTESIAN_POINT('Ctrl Pts',(11.2884368716309,15.2,-0.444003495612356));
#190948=CARTESIAN_POINT('Ctrl Pts',(11.2926893109079,15.2,-0.44608489472415));
#190949=CARTESIAN_POINT('Ctrl Pts',(11.2969496966965,15.2,-0.448178421117267));
#190950=CARTESIAN_POINT('Ctrl Pts',(11.3001449857477,15.2,-0.449748565769483));
#190951=CARTESIAN_POINT('Ctrl Pts',(11.303344744782,15.2,-0.451325532279665));
#190952=CARTESIAN_POINT('Ctrl Pts',(11.3065489298742,15.2,-0.452909329889383));
#190953=CARTESIAN_POINT('Ctrl Pts',(11.3097531149665,15.2,-0.454493127499101));
#190954=CARTESIAN_POINT('Ctrl Pts',(11.3129617262,15.2,-0.456083755857998));
#190955=CARTESIAN_POINT('Ctrl Pts',(11.3161747227499,15.2,-0.457681224008297));
#190956=CARTESIAN_POINT('Ctrl Pts',(11.3193877192999,15.2,-0.459278692158597));
#190957=CARTESIAN_POINT('Ctrl Pts',(11.3226050997162,15.2,-0.4608830011336));
#190958=CARTESIAN_POINT('Ctrl Pts',(11.3258268213905,15.2,-0.462494158324467));
#190959=CARTESIAN_POINT('Ctrl Pts',(11.3301224506797,15.2,-0.464642368107419));
#190960=CARTESIAN_POINT('Ctrl Pts',(11.3344258007579,15.2,-0.466802754745619));
#190961=CARTESIAN_POINT('Ctrl Pts',(11.3387367688755,15.2,-0.468975337806954));
#190962=CARTESIAN_POINT('Ctrl Pts',(11.3419699946701,15.2,-0.470604774954949));
#190963=CARTESIAN_POINT('Ctrl Pts',(11.3452075057374,15.2,-0.472241072138293));
#190964=CARTESIAN_POINT('Ctrl Pts',(11.3484492608283,15.2,-0.47388423916252));
#190965=CARTESIAN_POINT('Ctrl Pts',(11.3516910159192,15.2,-0.475527406186747));
#190966=CARTESIAN_POINT('Ctrl Pts',(11.3549370144347,15.2,-0.477177442210163));
#190967=CARTESIAN_POINT('Ctrl Pts',(11.3581872154832,15.2,-0.478834355816626));
#190968=CARTESIAN_POINT('Ctrl Pts',(11.3614374165318,15.2,-0.480491269423089));
#190969=CARTESIAN_POINT('Ctrl Pts',(11.3646918192969,15.2,-0.482155060945944));
#190970=CARTESIAN_POINT('Ctrl Pts',(11.3679503829281,15.2,-0.483825738551313));
#190971=CARTESIAN_POINT('Ctrl Pts',(11.3712089465594,15.2,-0.485496416156681));
#190972=CARTESIAN_POINT('Ctrl Pts',(11.3744716712572,15.2,-0.487173978935321));
#190973=CARTESIAN_POINT('Ctrl Pts',(11.3777385150929,15.2,-0.488858436124135));
#190974=CARTESIAN_POINT('Ctrl Pts',(11.3810053589286,15.2,-0.490542893312949));
#190975=CARTESIAN_POINT('Ctrl Pts',(11.3842763221555,15.2,-0.492234245292398));
#190976=CARTESIAN_POINT('Ctrl Pts',(11.3875513632443,15.2,-0.49393249889642));
#190977=CARTESIAN_POINT('Ctrl Pts',(11.390826404928,15.2,-0.495630752808959));
#190978=CARTESIAN_POINT('Ctrl Pts',(11.394105523788,15.2,-0.497335909390109));
#190979=CARTESIAN_POINT('Ctrl Pts',(11.3973886809323,15.2,-0.499047974889869));
#190980=CARTESIAN_POINT('Ctrl Pts',(11.4017662227974,15.2,-0.501330728371175));
#190981=CARTESIAN_POINT('Ctrl Pts',(11.4061509424338,15.2,-0.503625766992553));
#190982=CARTESIAN_POINT('Ctrl Pts',(11.4105427444076,15.2,-0.505933107636456));
#190983=CARTESIAN_POINT('Ctrl Pts',(11.4160324973237,15.2,-0.508817283677116));
#190984=CARTESIAN_POINT('Ctrl Pts',(11.4215333146442,15.2,-0.51172068206293));
#190985=CARTESIAN_POINT('Ctrl Pts',(11.4270450034886,15.2,-0.514643339715044));
#190986=CARTESIAN_POINT('Ctrl Pts',(11.4303520166751,15.2,-0.516396934242598));
#190987=CARTESIAN_POINT('Ctrl Pts',(11.4336629438595,15.2,-0.518157461538919));
#190988=CARTESIAN_POINT('Ctrl Pts',(11.4369777481137,15.2,-0.519924928099095));
#190989=CARTESIAN_POINT('Ctrl Pts',(11.4402925523679,15.2,-0.521692394659271));
#190990=CARTESIAN_POINT('Ctrl Pts',(11.4436112351968,15.2,-0.523466801110638));
#190991=CARTESIAN_POINT('Ctrl Pts',(11.4469337572423,15.2,-0.525248154128306));
#190992=CARTESIAN_POINT('Ctrl Pts',(11.4502562798913,15.2,-0.527029507469586));
#190993=CARTESIAN_POINT('Ctrl Pts',(11.4535826417247,15.2,-0.528817805796141));
#190994=CARTESIAN_POINT('Ctrl Pts',(11.4569127942509,15.2,-0.530613060641335));
#190995=CARTESIAN_POINT('Ctrl Pts',(11.4624630470496,15.2,-0.533605151289005));
#190996=CARTESIAN_POINT('Ctrl Pts',(11.4680238153293,15.2,-0.536616564596594));
#190997=CARTESIAN_POINT('Ctrl Pts',(11.4735949393046,15.2,-0.539647326903549));
#190998=CARTESIAN_POINT('Ctrl Pts',(11.4780518392134,15.2,-0.542071937145537));
#190999=CARTESIAN_POINT('Ctrl Pts',(11.4825153677325,15.2,-0.54450892420966));
#191000=CARTESIAN_POINT('Ctrl Pts',(11.4869855309999,15.2,-0.546958306000014));
#191001=CARTESIAN_POINT('Origin',(-5.66257110645729E-14,15.2,-1.77635683940025E-14));
#191002=CARTESIAN_POINT('',(10.3708900234023,15.2,0.29200192900193));
#191003=CARTESIAN_POINT('',(10.3708900234023,12.2,0.292001929001926));
#191004=CARTESIAN_POINT('',(10.3708900229999,15.2,0.292001928999985));
#191005=CARTESIAN_POINT('Origin',(-5.66257110645729E-14,12.2,-1.77635683940025E-14));
#191006=CARTESIAN_POINT('Origin',(-5.66257110645729E-14,15.2,-1.77635683940025E-14));
#191007=CARTESIAN_POINT('Origin',(-5.66257110645729E-14,15.2,-1.77635683940025E-14));
#191008=CARTESIAN_POINT('',(11.4780040719999,15.2,0.710930734999984));
#191009=CARTESIAN_POINT('',(11.4479048649999,15.2,1.09337742899998));
#191010=CARTESIAN_POINT('Origin',(-5.66257110645729E-14,15.2,-1.77635683940025E-14));
#191011=CARTESIAN_POINT('',(11.4479048649999,12.2,1.09337742899998));
#191012=CARTESIAN_POINT('',(11.4479048649999,15.2,1.09337742899998));
#191013=CARTESIAN_POINT('',(11.4780040719999,12.2,0.710930734999984));
#191014=CARTESIAN_POINT('Origin',(-5.66257110645729E-14,12.2,-1.77635683940025E-14));
#191015=CARTESIAN_POINT('',(11.4780040719999,15.2,0.710930734999984));
#191016=CARTESIAN_POINT('Ctrl Pts',(11.4479048649999,15.2,1.09337742899998));
#191017=CARTESIAN_POINT('Ctrl Pts',(11.4479048649999,11.6,1.09337742899998));
#191018=CARTESIAN_POINT('Ctrl Pts',(11.4471888789999,15.2,1.09364567099998));
#191019=CARTESIAN_POINT('Ctrl Pts',(11.4471888789999,11.6,1.09364567099998));
#191020=CARTESIAN_POINT('Ctrl Pts',(11.4457572179999,15.2,1.09418172899999));
#191021=CARTESIAN_POINT('Ctrl Pts',(11.4457572179999,11.6,1.09418172899999));
#191022=CARTESIAN_POINT('Ctrl Pts',(11.4436106639999,15.2,1.09498454299999));
#191023=CARTESIAN_POINT('Ctrl Pts',(11.4436106639999,11.6,1.09498454299999));
#191024=CARTESIAN_POINT('Ctrl Pts',(11.4407504639999,15.2,1.09605241699999));
#191025=CARTESIAN_POINT('Ctrl Pts',(11.4407504639999,11.6,1.09605241699999));
#191026=CARTESIAN_POINT('Ctrl Pts',(11.4371783349999,15.2,1.09738301699998));
#191027=CARTESIAN_POINT('Ctrl Pts',(11.4371783349999,11.6,1.09738301699998));
#191028=CARTESIAN_POINT('Ctrl Pts',(11.4336093279999,15.2,1.09870937299998));
#191029=CARTESIAN_POINT('Ctrl Pts',(11.4336093279999,11.6,1.09870937299998));
#191030=CARTESIAN_POINT('Ctrl Pts',(11.4300434449999,15.2,1.10003148899999));
#191031=CARTESIAN_POINT('Ctrl Pts',(11.4300434449999,11.6,1.10003148899999));
#191032=CARTESIAN_POINT('Ctrl Pts',(11.4264806909999,15.2,1.10134936399998));
#191033=CARTESIAN_POINT('Ctrl Pts',(11.4264806909999,11.6,1.10134936399998));
#191034=CARTESIAN_POINT('Ctrl Pts',(11.4229210689999,15.2,1.10266299899999));
#191035=CARTESIAN_POINT('Ctrl Pts',(11.4229210689999,11.6,1.10266299899999));
#191036=CARTESIAN_POINT('Ctrl Pts',(11.4193645909999,15.2,1.10397239899998));
#191037=CARTESIAN_POINT('Ctrl Pts',(11.4193645909999,11.6,1.10397239899998));
#191038=CARTESIAN_POINT('Ctrl Pts',(11.4158112619999,15.2,1.10527756499998));
#191039=CARTESIAN_POINT('Ctrl Pts',(11.4158112619999,11.6,1.10527756499998));
#191040=CARTESIAN_POINT('Ctrl Pts',(11.4122610939999,15.2,1.10657849999999));
#191041=CARTESIAN_POINT('Ctrl Pts',(11.4122610939999,11.6,1.10657849999999));
#191042=CARTESIAN_POINT('Ctrl Pts',(11.4087140989999,15.2,1.10787520999999));
#191043=CARTESIAN_POINT('Ctrl Pts',(11.4087140989999,11.6,1.10787520999999));
#191044=CARTESIAN_POINT('Ctrl Pts',(11.4051702859999,15.2,1.10916769599998));
#191045=CARTESIAN_POINT('Ctrl Pts',(11.4051702859999,11.6,1.10916769599998));
#191046=CARTESIAN_POINT('Ctrl Pts',(11.4016296639999,15.2,1.11045596299999));
#191047=CARTESIAN_POINT('Ctrl Pts',(11.4016296639999,11.6,1.11045596299999));
#191048=CARTESIAN_POINT('Ctrl Pts',(11.3980922449999,15.2,1.11174001299998));
#191049=CARTESIAN_POINT('Ctrl Pts',(11.3980922449999,11.6,1.11174001299998));
#191050=CARTESIAN_POINT('Ctrl Pts',(11.3945580339999,15.2,1.11301984899999));
#191051=CARTESIAN_POINT('Ctrl Pts',(11.3945580339999,11.6,1.11301984899998));
#191052=CARTESIAN_POINT('Ctrl Pts',(11.3910270409999,15.2,1.11429547399998));
#191053=CARTESIAN_POINT('Ctrl Pts',(11.3910270409999,11.6,1.11429547399998));
#191054=CARTESIAN_POINT('Ctrl Pts',(11.3874992709999,15.2,1.11556689099999));
#191055=CARTESIAN_POINT('Ctrl Pts',(11.3874992709999,11.6,1.11556689099999));
#191056=CARTESIAN_POINT('Ctrl Pts',(11.3839747349999,15.2,1.11683410099999));
#191057=CARTESIAN_POINT('Ctrl Pts',(11.3839747349999,11.6,1.11683410099999));
#191058=CARTESIAN_POINT('Ctrl Pts',(11.3804534399999,15.2,1.11809710599998));
#191059=CARTESIAN_POINT('Ctrl Pts',(11.3804534399999,11.6,1.11809710599998));
#191060=CARTESIAN_POINT('Ctrl Pts',(11.3769353939999,15.2,1.11935591199999));
#191061=CARTESIAN_POINT('Ctrl Pts',(11.3769353939999,11.6,1.11935591199999));
#191062=CARTESIAN_POINT('Ctrl Pts',(11.3734206059999,15.2,1.12061051999999));
#191063=CARTESIAN_POINT('Ctrl Pts',(11.3734206059999,11.6,1.12061051999999));
#191064=CARTESIAN_POINT('Ctrl Pts',(11.3699090849999,15.2,1.12186093299998));
#191065=CARTESIAN_POINT('Ctrl Pts',(11.3699090849999,11.6,1.12186093299998));
#191066=CARTESIAN_POINT('Ctrl Pts',(11.3664008399999,15.2,1.12310715499999));
#191067=CARTESIAN_POINT('Ctrl Pts',(11.3664008399999,11.6,1.12310715499999));
#191068=CARTESIAN_POINT('Ctrl Pts',(11.3628958789999,15.2,1.12434918799998));
#191069=CARTESIAN_POINT('Ctrl Pts',(11.3628958789999,11.6,1.12434918799998));
#191070=CARTESIAN_POINT('Ctrl Pts',(11.3593942139999,15.2,1.12558703499999));
#191071=CARTESIAN_POINT('Ctrl Pts',(11.3593942139999,11.6,1.12558703499999));
#191072=CARTESIAN_POINT('Ctrl Pts',(11.3558958509999,15.2,1.12682069999999));
#191073=CARTESIAN_POINT('Ctrl Pts',(11.3558958509999,11.6,1.12682069999999));
#191074=CARTESIAN_POINT('Ctrl Pts',(11.3524007989999,15.2,1.12805018499999));
#191075=CARTESIAN_POINT('Ctrl Pts',(11.3524007989999,11.6,1.12805018499999));
#191076=CARTESIAN_POINT('Ctrl Pts',(11.3489090669999,15.2,1.12927549499998));
#191077=CARTESIAN_POINT('Ctrl Pts',(11.3489090669999,11.6,1.12927549499998));
#191078=CARTESIAN_POINT('Ctrl Pts',(11.3454206639999,15.2,1.13049662999999));
#191079=CARTESIAN_POINT('Ctrl Pts',(11.3454206639999,11.6,1.13049662999999));
#191080=CARTESIAN_POINT('Ctrl Pts',(11.3419355979999,15.2,1.13171359399999));
#191081=CARTESIAN_POINT('Ctrl Pts',(11.3419355979999,11.6,1.13171359399999));
#191082=CARTESIAN_POINT('Ctrl Pts',(11.3384538779999,15.2,1.13292639099999));
#191083=CARTESIAN_POINT('Ctrl Pts',(11.3384538779999,11.6,1.13292639099999));
#191084=CARTESIAN_POINT('Ctrl Pts',(11.3349755119999,15.2,1.13413502399998));
#191085=CARTESIAN_POINT('Ctrl Pts',(11.3349755119999,11.6,1.13413502399998));
#191086=CARTESIAN_POINT('Ctrl Pts',(11.3315005099999,15.2,1.13533949399999));
#191087=CARTESIAN_POINT('Ctrl Pts',(11.3315005099999,11.6,1.13533949399998));
#191088=CARTESIAN_POINT('Ctrl Pts',(11.3280288789999,15.2,1.13653980499999));
#191089=CARTESIAN_POINT('Ctrl Pts',(11.3280288789999,11.6,1.13653980499999));
#191090=CARTESIAN_POINT('Ctrl Pts',(11.3245606299999,15.2,1.13773596199998));
#191091=CARTESIAN_POINT('Ctrl Pts',(11.3245606299999,11.6,1.13773596199998));
#191092=CARTESIAN_POINT('Ctrl Pts',(11.3210957719999,15.2,1.13892796799998));
#191093=CARTESIAN_POINT('Ctrl Pts',(11.3210957719999,11.6,1.13892796799998));
#191094=CARTESIAN_POINT('Ctrl Pts',(11.3176343119999,15.2,1.14011582299999));
#191095=CARTESIAN_POINT('Ctrl Pts',(11.3176343119999,11.6,1.14011582299998));
#191096=CARTESIAN_POINT('Ctrl Pts',(11.3141762599999,15.2,1.14129953199999));
#191097=CARTESIAN_POINT('Ctrl Pts',(11.3141762599999,11.6,1.14129953199999));
#191098=CARTESIAN_POINT('Ctrl Pts',(11.3107216239999,15.2,1.14247909899999));
#191099=CARTESIAN_POINT('Ctrl Pts',(11.3107216239999,11.6,1.14247909899999));
#191100=CARTESIAN_POINT('Ctrl Pts',(11.3072704139999,15.2,1.14365452599999));
#191101=CARTESIAN_POINT('Ctrl Pts',(11.3072704139999,11.6,1.14365452599999));
#191102=CARTESIAN_POINT('Ctrl Pts',(11.3038226389999,15.2,1.14482581599999));
#191103=CARTESIAN_POINT('Ctrl Pts',(11.3038226389999,11.6,1.14482581599999));
#191104=CARTESIAN_POINT('Ctrl Pts',(11.3003783059999,15.2,1.14599297299999));
#191105=CARTESIAN_POINT('Ctrl Pts',(11.3003783059999,11.6,1.14599297299998));
#191106=CARTESIAN_POINT('Ctrl Pts',(11.2969374249999,15.2,1.14715599999998));
#191107=CARTESIAN_POINT('Ctrl Pts',(11.2969374249999,11.6,1.14715599999998));
#191108=CARTESIAN_POINT('Ctrl Pts',(11.2935000059999,15.2,1.14831489899998));
#191109=CARTESIAN_POINT('Ctrl Pts',(11.2935000059999,11.6,1.14831489899998));
#191110=CARTESIAN_POINT('Ctrl Pts',(11.2900660559999,15.2,1.14946967499999));
#191111=CARTESIAN_POINT('Ctrl Pts',(11.2900660559999,11.6,1.14946967499999));
#191112=CARTESIAN_POINT('Ctrl Pts',(11.2866355859999,15.2,1.15062032999999));
#191113=CARTESIAN_POINT('Ctrl Pts',(11.2866355859999,11.6,1.15062032999999));
#191114=CARTESIAN_POINT('Ctrl Pts',(11.2832086039999,15.2,1.15176686799999));
#191115=CARTESIAN_POINT('Ctrl Pts',(11.2832086039999,11.6,1.15176686799999));
#191116=CARTESIAN_POINT('Ctrl Pts',(11.2797851169999,15.2,1.15290929199999));
#191117=CARTESIAN_POINT('Ctrl Pts',(11.2797851169999,11.6,1.15290929199999));
#191118=CARTESIAN_POINT('Ctrl Pts',(11.2763651379999,15.2,1.15404760499999));
#191119=CARTESIAN_POINT('Ctrl Pts',(11.2763651379999,11.6,1.15404760499999));
#191120=CARTESIAN_POINT('Ctrl Pts',(11.2729486729999,15.2,1.15518180999999));
#191121=CARTESIAN_POINT('Ctrl Pts',(11.2729486729999,11.6,1.15518180999999));
#191122=CARTESIAN_POINT('Ctrl Pts',(11.2695357319999,15.2,1.15631191099999));
#191123=CARTESIAN_POINT('Ctrl Pts',(11.2695357319999,11.6,1.15631191099998));
#191124=CARTESIAN_POINT('Ctrl Pts',(11.2661263239999,15.2,1.15743791099999));
#191125=CARTESIAN_POINT('Ctrl Pts',(11.2661263239999,11.6,1.15743791099999));
#191126=CARTESIAN_POINT('Ctrl Pts',(11.2627204589999,15.2,1.15855981299998));
#191127=CARTESIAN_POINT('Ctrl Pts',(11.2627204589999,11.6,1.15855981299998));
#191128=CARTESIAN_POINT('Ctrl Pts',(11.2593181439999,15.2,1.15967762199999));
#191129=CARTESIAN_POINT('Ctrl Pts',(11.2593181439999,11.6,1.15967762199999));
#191130=CARTESIAN_POINT('Ctrl Pts',(11.2559193889999,15.2,1.16079133899999));
#191131=CARTESIAN_POINT('Ctrl Pts',(11.2559193889999,11.6,1.16079133899999));
#191132=CARTESIAN_POINT('Ctrl Pts',(11.2525242039999,15.2,1.16190096799999));
#191133=CARTESIAN_POINT('Ctrl Pts',(11.2525242039999,11.6,1.16190096799999));
#191134=CARTESIAN_POINT('Ctrl Pts',(11.2491325969999,15.2,1.16300651299999));
#191135=CARTESIAN_POINT('Ctrl Pts',(11.2491325969999,11.6,1.16300651299999));
#191136=CARTESIAN_POINT('Ctrl Pts',(11.2457445769999,15.2,1.16410797799999));
#191137=CARTESIAN_POINT('Ctrl Pts',(11.2457445769999,11.6,1.16410797799999));
#191138=CARTESIAN_POINT('Ctrl Pts',(11.2423601539999,15.2,1.16520536499999));
#191139=CARTESIAN_POINT('Ctrl Pts',(11.2423601539999,11.6,1.16520536499999));
#191140=CARTESIAN_POINT('Ctrl Pts',(11.2389793369999,15.2,1.16629867799999));
#191141=CARTESIAN_POINT('Ctrl Pts',(11.2389793369999,11.6,1.16629867799999));
#191142=CARTESIAN_POINT('Ctrl Pts',(11.2356021349999,15.2,1.16738791999999));
#191143=CARTESIAN_POINT('Ctrl Pts',(11.2356021349999,11.6,1.16738791999999));
#191144=CARTESIAN_POINT('Ctrl Pts',(11.2322285569999,15.2,1.16847309399999));
#191145=CARTESIAN_POINT('Ctrl Pts',(11.2322285569999,11.6,1.16847309399999));
#191146=CARTESIAN_POINT('Ctrl Pts',(11.2288586119999,15.2,1.16955420599998));
#191147=CARTESIAN_POINT('Ctrl Pts',(11.2288586119999,11.6,1.16955420599998));
#191148=CARTESIAN_POINT('Ctrl Pts',(11.2254923089999,15.2,1.17063125699998));
#191149=CARTESIAN_POINT('Ctrl Pts',(11.2254923089999,11.6,1.17063125699998));
#191150=CARTESIAN_POINT('Ctrl Pts',(11.2221296589999,15.2,1.17170425099999));
#191151=CARTESIAN_POINT('Ctrl Pts',(11.2221296589999,11.6,1.17170425099998));
#191152=CARTESIAN_POINT('Ctrl Pts',(11.2187706689999,15.2,1.17277319199999));
#191153=CARTESIAN_POINT('Ctrl Pts',(11.2187706689999,11.6,1.17277319199998));
#191154=CARTESIAN_POINT('Ctrl Pts',(11.2154153489999,15.2,1.17383808299998));
#191155=CARTESIAN_POINT('Ctrl Pts',(11.2154153489999,11.6,1.17383808299998));
#191156=CARTESIAN_POINT('Ctrl Pts',(11.2120637079999,15.2,1.17489892799998));
#191157=CARTESIAN_POINT('Ctrl Pts',(11.2120637079999,11.6,1.17489892799998));
#191158=CARTESIAN_POINT('Ctrl Pts',(11.2087157559999,15.2,1.17595572999999));
#191159=CARTESIAN_POINT('Ctrl Pts',(11.2087157559999,11.6,1.17595572999999));
#191160=CARTESIAN_POINT('Ctrl Pts',(11.2053715019999,15.2,1.17700849199998));
#191161=CARTESIAN_POINT('Ctrl Pts',(11.2053715019999,11.6,1.17700849199998));
#191162=CARTESIAN_POINT('Ctrl Pts',(11.2020309559999,15.2,1.17805721999999));
#191163=CARTESIAN_POINT('Ctrl Pts',(11.2020309559999,11.6,1.17805721999999));
#191164=CARTESIAN_POINT('Ctrl Pts',(11.1986941249999,15.2,1.17910191499998));
#191165=CARTESIAN_POINT('Ctrl Pts',(11.1986941249999,11.6,1.17910191499998));
#191166=CARTESIAN_POINT('Ctrl Pts',(11.1953610209999,15.2,1.18014258099999));
#191167=CARTESIAN_POINT('Ctrl Pts',(11.1953610209999,11.6,1.18014258099999));
#191168=CARTESIAN_POINT('Ctrl Pts',(11.1920316519999,15.2,1.18117922199998));
#191169=CARTESIAN_POINT('Ctrl Pts',(11.1920316519999,11.6,1.18117922199998));
#191170=CARTESIAN_POINT('Ctrl Pts',(11.1887060269999,15.2,1.18221184299999));
#191171=CARTESIAN_POINT('Ctrl Pts',(11.1887060269999,11.6,1.18221184299998));
#191172=CARTESIAN_POINT('Ctrl Pts',(11.1853841569999,15.2,1.18324044599999));
#191173=CARTESIAN_POINT('Ctrl Pts',(11.1853841569999,11.6,1.18324044599999));
#191174=CARTESIAN_POINT('Ctrl Pts',(11.1820660499999,15.2,1.18426503499999));
#191175=CARTESIAN_POINT('Ctrl Pts',(11.1820660499999,11.6,1.18426503499998));
#191176=CARTESIAN_POINT('Ctrl Pts',(11.1787517149999,15.2,1.18528561399998));
#191177=CARTESIAN_POINT('Ctrl Pts',(11.1787517149999,11.6,1.18528561399998));
#191178=CARTESIAN_POINT('Ctrl Pts',(11.1754411629999,15.2,1.18630218499999));
#191179=CARTESIAN_POINT('Ctrl Pts',(11.1754411629999,11.6,1.18630218499999));
#191180=CARTESIAN_POINT('Ctrl Pts',(11.1721344009999,15.2,1.18731475499999));
#191181=CARTESIAN_POINT('Ctrl Pts',(11.1721344009999,11.6,1.18731475499999));
#191182=CARTESIAN_POINT('Ctrl Pts',(11.1688314409999,15.2,1.18832332399998));
#191183=CARTESIAN_POINT('Ctrl Pts',(11.1688314409999,11.6,1.18832332399998));
#191184=CARTESIAN_POINT('Ctrl Pts',(11.1655322919999,15.2,1.18932789899999));
#191185=CARTESIAN_POINT('Ctrl Pts',(11.1655322919999,11.6,1.18932789899999));
#191186=CARTESIAN_POINT('Ctrl Pts',(11.1622369629999,15.2,1.19032848099998));
#191187=CARTESIAN_POINT('Ctrl Pts',(11.1622369629999,11.6,1.19032848099998));
#191188=CARTESIAN_POINT('Ctrl Pts',(11.1589454619999,15.2,1.19132507599998));
#191189=CARTESIAN_POINT('Ctrl Pts',(11.1589454619999,11.6,1.19132507599998));
#191190=CARTESIAN_POINT('Ctrl Pts',(11.1556577999999,15.2,1.19231768599999));
#191191=CARTESIAN_POINT('Ctrl Pts',(11.1556577999999,11.6,1.19231768599999));
#191192=CARTESIAN_POINT('Ctrl Pts',(11.1523739879999,15.2,1.19330631599999));
#191193=CARTESIAN_POINT('Ctrl Pts',(11.1523739879999,11.6,1.19330631599999));
#191194=CARTESIAN_POINT('Ctrl Pts',(11.1490940329999,15.2,1.19429096899998));
#191195=CARTESIAN_POINT('Ctrl Pts',(11.1490940329999,11.6,1.19429096899998));
#191196=CARTESIAN_POINT('Ctrl Pts',(11.1458179459999,15.2,1.19527164899999));
#191197=CARTESIAN_POINT('Ctrl Pts',(11.1458179459999,11.6,1.19527164899999));
#191198=CARTESIAN_POINT('Ctrl Pts',(11.1425457349999,15.2,1.19624835999999));
#191199=CARTESIAN_POINT('Ctrl Pts',(11.1425457349999,11.6,1.19624835999998));
#191200=CARTESIAN_POINT('Ctrl Pts',(11.1392774109999,15.2,1.19722110599998));
#191201=CARTESIAN_POINT('Ctrl Pts',(11.1392774109999,11.6,1.19722110599998));
#191202=CARTESIAN_POINT('Ctrl Pts',(11.1360129839999,15.2,1.19818988999999));
#191203=CARTESIAN_POINT('Ctrl Pts',(11.1360129839999,11.6,1.19818988999999));
#191204=CARTESIAN_POINT('Ctrl Pts',(11.1327524619999,15.2,1.19915471699999));
#191205=CARTESIAN_POINT('Ctrl Pts',(11.1327524619999,11.6,1.19915471699999));
#191206=CARTESIAN_POINT('Ctrl Pts',(11.1294958549999,15.2,1.20011559099999));
#191207=CARTESIAN_POINT('Ctrl Pts',(11.1294958549999,11.6,1.20011559099999));
#191208=CARTESIAN_POINT('Ctrl Pts',(11.1262431739999,15.2,1.20107251499999));
#191209=CARTESIAN_POINT('Ctrl Pts',(11.1262431739999,11.6,1.20107251499999));
#191210=CARTESIAN_POINT('Ctrl Pts',(11.1229944269999,15.2,1.20202549299998));
#191211=CARTESIAN_POINT('Ctrl Pts',(11.1229944269999,11.6,1.20202549299998));
#191212=CARTESIAN_POINT('Ctrl Pts',(11.1197496249999,15.2,1.20297452899999));
#191213=CARTESIAN_POINT('Ctrl Pts',(11.1197496249999,11.6,1.20297452899999));
#191214=CARTESIAN_POINT('Ctrl Pts',(11.1165087779999,15.2,1.20391962699999));
#191215=CARTESIAN_POINT('Ctrl Pts',(11.1165087779999,11.6,1.20391962699998));
#191216=CARTESIAN_POINT('Ctrl Pts',(11.1132718939999,15.2,1.20486079099999));
#191217=CARTESIAN_POINT('Ctrl Pts',(11.1132718939999,11.6,1.20486079099999));
#191218=CARTESIAN_POINT('Ctrl Pts',(11.1100389819999,15.2,1.20579802499998));
#191219=CARTESIAN_POINT('Ctrl Pts',(11.1100389819999,11.6,1.20579802499998));
#191220=CARTESIAN_POINT('Ctrl Pts',(11.1068100549999,15.2,1.20673133399999));
#191221=CARTESIAN_POINT('Ctrl Pts',(11.1068100549999,11.6,1.20673133399999));
#191222=CARTESIAN_POINT('Ctrl Pts',(11.1035851209999,15.2,1.20766071999999));
#191223=CARTESIAN_POINT('Ctrl Pts',(11.1035851209999,11.6,1.20766071999999));
#191224=CARTESIAN_POINT('Ctrl Pts',(11.1003641889999,15.2,1.20858618799998));
#191225=CARTESIAN_POINT('Ctrl Pts',(11.1003641889999,11.6,1.20858618799998));
#191226=CARTESIAN_POINT('Ctrl Pts',(11.0971472699999,15.2,1.20950774199999));
#191227=CARTESIAN_POINT('Ctrl Pts',(11.0971472699999,11.6,1.20950774199999));
#191228=CARTESIAN_POINT('Ctrl Pts',(11.0939343729999,15.2,1.21042538699998));
#191229=CARTESIAN_POINT('Ctrl Pts',(11.0939343729999,11.6,1.21042538699998));
#191230=CARTESIAN_POINT('Ctrl Pts',(11.0907255089999,15.2,1.21133912599999));
#191231=CARTESIAN_POINT('Ctrl Pts',(11.0907255089999,11.6,1.21133912599999));
#191232=CARTESIAN_POINT('Ctrl Pts',(11.0875206859999,15.2,1.21224896199998));
#191233=CARTESIAN_POINT('Ctrl Pts',(11.0875206859999,11.6,1.21224896199998));
#191234=CARTESIAN_POINT('Ctrl Pts',(11.0843199139999,15.2,1.21315490199999));
#191235=CARTESIAN_POINT('Ctrl Pts',(11.0843199139999,11.6,1.21315490199999));
#191236=CARTESIAN_POINT('Ctrl Pts',(11.0811232049999,15.2,1.21405694799999));
#191237=CARTESIAN_POINT('Ctrl Pts',(11.0811232049999,11.6,1.21405694799999));
#191238=CARTESIAN_POINT('Ctrl Pts',(11.0779305669999,15.2,1.21495510399999));
#191239=CARTESIAN_POINT('Ctrl Pts',(11.0779305669999,11.6,1.21495510399999));
#191240=CARTESIAN_POINT('Ctrl Pts',(11.0747420099999,15.2,1.21584937499998));
#191241=CARTESIAN_POINT('Ctrl Pts',(11.0747420099999,11.6,1.21584937499998));
#191242=CARTESIAN_POINT('Ctrl Pts',(11.0715575449999,15.2,1.21673976599999));
#191243=CARTESIAN_POINT('Ctrl Pts',(11.0715575449999,11.6,1.21673976599999));
#191244=CARTESIAN_POINT('Ctrl Pts',(11.0683771819999,15.2,1.21762627999999));
#191245=CARTESIAN_POINT('Ctrl Pts',(11.0683771819999,11.6,1.21762627999999));
#191246=CARTESIAN_POINT('Ctrl Pts',(11.0652009289999,15.2,1.21850892099999));
#191247=CARTESIAN_POINT('Ctrl Pts',(11.0652009289999,11.6,1.21850892099999));
#191248=CARTESIAN_POINT('Ctrl Pts',(11.0620287979999,15.2,1.21938769199998));
#191249=CARTESIAN_POINT('Ctrl Pts',(11.0620287979999,11.6,1.21938769199998));
#191250=CARTESIAN_POINT('Ctrl Pts',(11.0588607969999,15.2,1.22026260099998));
#191251=CARTESIAN_POINT('Ctrl Pts',(11.0588607969999,11.6,1.22026260099998));
#191252=CARTESIAN_POINT('Ctrl Pts',(11.0556969379999,15.2,1.22113364899999));
#191253=CARTESIAN_POINT('Ctrl Pts',(11.0556969379999,11.6,1.22113364899999));
#191254=CARTESIAN_POINT('Ctrl Pts',(11.0525372299999,15.2,1.22200084099998));
#191255=CARTESIAN_POINT('Ctrl Pts',(11.0525372299999,11.6,1.22200084099998));
#191256=CARTESIAN_POINT('Ctrl Pts',(11.0493816829999,15.2,1.22286418199999));
#191257=CARTESIAN_POINT('Ctrl Pts',(11.0493816829999,11.6,1.22286418199998));
#191258=CARTESIAN_POINT('Ctrl Pts',(11.0462303079999,15.2,1.22372367599999));
#191259=CARTESIAN_POINT('Ctrl Pts',(11.0462303079999,11.6,1.22372367599999));
#191260=CARTESIAN_POINT('Ctrl Pts',(11.0430831139999,15.2,1.22457932799998));
#191261=CARTESIAN_POINT('Ctrl Pts',(11.0430831139999,11.6,1.22457932799998));
#191262=CARTESIAN_POINT('Ctrl Pts',(11.0399401109999,15.2,1.22543113999999));
#191263=CARTESIAN_POINT('Ctrl Pts',(11.0399401109999,11.6,1.22543113999999));
#191264=CARTESIAN_POINT('Ctrl Pts',(11.0368013089999,15.2,1.22627911899999));
#191265=CARTESIAN_POINT('Ctrl Pts',(11.0368013089999,11.6,1.22627911899999));
#191266=CARTESIAN_POINT('Ctrl Pts',(11.0336667189999,15.2,1.22712326699999));
#191267=CARTESIAN_POINT('Ctrl Pts',(11.0336667189999,11.6,1.22712326699998));
#191268=CARTESIAN_POINT('Ctrl Pts',(11.0305363499999,15.2,1.22796359099999));
#191269=CARTESIAN_POINT('Ctrl Pts',(11.0305363499999,11.6,1.22796359099999));
#191270=CARTESIAN_POINT('Ctrl Pts',(11.0274102129999,15.2,1.22880009299998));
#191271=CARTESIAN_POINT('Ctrl Pts',(11.0274102129999,11.6,1.22880009299998));
#191272=CARTESIAN_POINT('Ctrl Pts',(11.0242883189999,15.2,1.22963277999999));
#191273=CARTESIAN_POINT('Ctrl Pts',(11.0242883189999,11.6,1.22963277999998));
#191274=CARTESIAN_POINT('Ctrl Pts',(11.0211706759999,15.2,1.23046165299999));
#191275=CARTESIAN_POINT('Ctrl Pts',(11.0211706759999,11.6,1.23046165299999));
#191276=CARTESIAN_POINT('Ctrl Pts',(11.0180572959999,15.2,1.23128671899998));
#191277=CARTESIAN_POINT('Ctrl Pts',(11.0180572959999,11.6,1.23128671899998));
#191278=CARTESIAN_POINT('Ctrl Pts',(11.0149481889999,15.2,1.23210798199999));
#191279=CARTESIAN_POINT('Ctrl Pts',(11.0149481889999,11.6,1.23210798199999));
#191280=CARTESIAN_POINT('Ctrl Pts',(11.0118433639999,15.2,1.23292544599999));
#191281=CARTESIAN_POINT('Ctrl Pts',(11.0118433639999,11.6,1.23292544599999));
#191282=CARTESIAN_POINT('Ctrl Pts',(11.0087428319999,15.2,1.23373911599999));
#191283=CARTESIAN_POINT('Ctrl Pts',(11.0087428319999,11.6,1.23373911599999));
#191284=CARTESIAN_POINT('Ctrl Pts',(11.0056466049999,15.2,1.23454899599999));
#191285=CARTESIAN_POINT('Ctrl Pts',(11.0056466049999,11.6,1.23454899599999));
#191286=CARTESIAN_POINT('Ctrl Pts',(11.0025546899999,15.2,1.23535509099999));
#191287=CARTESIAN_POINT('Ctrl Pts',(11.0025546899999,11.6,1.23535509099999));
#191288=CARTESIAN_POINT('Ctrl Pts',(10.9994670979999,15.2,1.23615740499998));
#191289=CARTESIAN_POINT('Ctrl Pts',(10.9994670979999,11.6,1.23615740499998));
#191290=CARTESIAN_POINT('Ctrl Pts',(10.9963838419999,15.2,1.23695594399999));
#191291=CARTESIAN_POINT('Ctrl Pts',(10.9963838419999,11.6,1.23695594399999));
#191292=CARTESIAN_POINT('Ctrl Pts',(10.9933049299999,15.2,1.23775071099999));
#191293=CARTESIAN_POINT('Ctrl Pts',(10.9933049299999,11.6,1.23775071099998));
#191294=CARTESIAN_POINT('Ctrl Pts',(10.9902303719999,15.2,1.23854171099998));
#191295=CARTESIAN_POINT('Ctrl Pts',(10.9902303719999,11.6,1.23854171099998));
#191296=CARTESIAN_POINT('Ctrl Pts',(10.9871601809999,15.2,1.23932894899998));
#191297=CARTESIAN_POINT('Ctrl Pts',(10.9871601809999,11.6,1.23932894899998));
#191298=CARTESIAN_POINT('Ctrl Pts',(10.9840943639999,15.2,1.24011242999998));
#191299=CARTESIAN_POINT('Ctrl Pts',(10.9840943639999,11.6,1.24011242999998));
#191300=CARTESIAN_POINT('Ctrl Pts',(10.9810329339999,15.2,1.24089215599998));
#191301=CARTESIAN_POINT('Ctrl Pts',(10.9810329339999,11.6,1.24089215599998));
#191302=CARTESIAN_POINT('Ctrl Pts',(10.9779759009999,15.2,1.24166813599999));
#191303=CARTESIAN_POINT('Ctrl Pts',(10.9779759009999,11.6,1.24166813599999));
#191304=CARTESIAN_POINT('Ctrl Pts',(10.9749232749999,15.2,1.24244037199999));
#191305=CARTESIAN_POINT('Ctrl Pts',(10.9749232749999,11.6,1.24244037199999));
#191306=CARTESIAN_POINT('Ctrl Pts',(10.9718750649999,15.2,1.24320886799998));
#191307=CARTESIAN_POINT('Ctrl Pts',(10.9718750649999,11.6,1.24320886799998));
#191308=CARTESIAN_POINT('Ctrl Pts',(10.9688312839999,15.2,1.24397363099999));
#191309=CARTESIAN_POINT('Ctrl Pts',(10.9688312839999,11.6,1.24397363099999));
#191310=CARTESIAN_POINT('Ctrl Pts',(10.9657919419999,15.2,1.24473466399999));
#191311=CARTESIAN_POINT('Ctrl Pts',(10.9657919419999,11.6,1.24473466399999));
#191312=CARTESIAN_POINT('Ctrl Pts',(10.9627570469999,15.2,1.24549197299999));
#191313=CARTESIAN_POINT('Ctrl Pts',(10.9627570469999,11.6,1.24549197299999));
#191314=CARTESIAN_POINT('Ctrl Pts',(10.9597266129999,15.2,1.24624556199999));
#191315=CARTESIAN_POINT('Ctrl Pts',(10.9597266129999,11.6,1.24624556199999));
#191316=CARTESIAN_POINT('Ctrl Pts',(10.9567006489999,15.2,1.24699543599998));
#191317=CARTESIAN_POINT('Ctrl Pts',(10.9567006489999,11.6,1.24699543599998));
#191318=CARTESIAN_POINT('Ctrl Pts',(10.9536791659999,15.2,1.24774160099999));
#191319=CARTESIAN_POINT('Ctrl Pts',(10.9536791659999,11.6,1.24774160099998));
#191320=CARTESIAN_POINT('Ctrl Pts',(10.9506621729999,15.2,1.24848405899999));
#191321=CARTESIAN_POINT('Ctrl Pts',(10.9506621729999,11.6,1.24848405899999));
#191322=CARTESIAN_POINT('Ctrl Pts',(10.9476496829999,15.2,1.24922281699998));
#191323=CARTESIAN_POINT('Ctrl Pts',(10.9476496829999,11.6,1.24922281699998));
#191324=CARTESIAN_POINT('Ctrl Pts',(10.9446417049999,15.2,1.24995787999998));
#191325=CARTESIAN_POINT('Ctrl Pts',(10.9446417049999,11.6,1.24995787999998));
#191326=CARTESIAN_POINT('Ctrl Pts',(10.9416382509999,15.2,1.25068925199999));
#191327=CARTESIAN_POINT('Ctrl Pts',(10.9416382509999,11.6,1.25068925199999));
#191328=CARTESIAN_POINT('Ctrl Pts',(10.9386393289999,15.2,1.25141693899999));
#191329=CARTESIAN_POINT('Ctrl Pts',(10.9386393289999,11.6,1.25141693899998));
#191330=CARTESIAN_POINT('Ctrl Pts',(10.9356449539999,15.2,1.25214094399999));
#191331=CARTESIAN_POINT('Ctrl Pts',(10.9356449539999,11.6,1.25214094399999));
#191332=CARTESIAN_POINT('Ctrl Pts',(10.9326551319999,15.2,1.25286127399999));
#191333=CARTESIAN_POINT('Ctrl Pts',(10.9326551319999,11.6,1.25286127399999));
#191334=CARTESIAN_POINT('Ctrl Pts',(10.9296698779999,15.2,1.25357793199999));
#191335=CARTESIAN_POINT('Ctrl Pts',(10.9296698779999,11.6,1.25357793199999));
#191336=CARTESIAN_POINT('Ctrl Pts',(10.9266891999999,15.2,1.25429092499999));
#191337=CARTESIAN_POINT('Ctrl Pts',(10.9266891999999,11.6,1.25429092499999));
#191338=CARTESIAN_POINT('Ctrl Pts',(10.9237131089999,15.2,1.25500025699999));
#191339=CARTESIAN_POINT('Ctrl Pts',(10.9237131089999,11.6,1.25500025699999));
#191340=CARTESIAN_POINT('Ctrl Pts',(10.9207416159999,15.2,1.25570593399999));
#191341=CARTESIAN_POINT('Ctrl Pts',(10.9207416159999,11.6,1.25570593399999));
#191342=CARTESIAN_POINT('Ctrl Pts',(10.9177747329999,15.2,1.25640795999999));
#191343=CARTESIAN_POINT('Ctrl Pts',(10.9177747329999,11.6,1.25640795999999));
#191344=CARTESIAN_POINT('Ctrl Pts',(10.9148124699999,15.2,1.25710633999998));
#191345=CARTESIAN_POINT('Ctrl Pts',(10.9148124699999,11.6,1.25710633999998));
#191346=CARTESIAN_POINT('Ctrl Pts',(10.9118548369999,15.2,1.25780107899998));
#191347=CARTESIAN_POINT('Ctrl Pts',(10.9118548369999,11.6,1.25780107899998));
#191348=CARTESIAN_POINT('Ctrl Pts',(10.9089018469999,15.2,1.25849218299999));
#191349=CARTESIAN_POINT('Ctrl Pts',(10.9089018469999,11.6,1.25849218299999));
#191350=CARTESIAN_POINT('Ctrl Pts',(10.9059535079999,15.2,1.25917965599998));
#191351=CARTESIAN_POINT('Ctrl Pts',(10.9059535079999,11.6,1.25917965599998));
#191352=CARTESIAN_POINT('Ctrl Pts',(10.9030098339999,15.2,1.25986350499999));
#191353=CARTESIAN_POINT('Ctrl Pts',(10.9030098339999,11.6,1.25986350499998));
#191354=CARTESIAN_POINT('Ctrl Pts',(10.9000708339999,15.2,1.26054373299999));
#191355=CARTESIAN_POINT('Ctrl Pts',(10.9000708339999,11.6,1.26054373299999));
#191356=CARTESIAN_POINT('Ctrl Pts',(10.8971365199999,15.2,1.26122034599998));
#191357=CARTESIAN_POINT('Ctrl Pts',(10.8971365199999,11.6,1.26122034599998));
#191358=CARTESIAN_POINT('Ctrl Pts',(10.8942069009999,15.2,1.26189335099999));
#191359=CARTESIAN_POINT('Ctrl Pts',(10.8942069009999,11.6,1.26189335099998));
#191360=CARTESIAN_POINT('Ctrl Pts',(10.8912819899999,15.2,1.26256274999998));
#191361=CARTESIAN_POINT('Ctrl Pts',(10.8912819899999,11.6,1.26256274999998));
#191362=CARTESIAN_POINT('Ctrl Pts',(10.8883617979999,15.2,1.26322854999998));
#191363=CARTESIAN_POINT('Ctrl Pts',(10.8883617979999,11.6,1.26322854999998));
#191364=CARTESIAN_POINT('Ctrl Pts',(10.8854463339999,15.2,1.26389075699999));
#191365=CARTESIAN_POINT('Ctrl Pts',(10.8854463339999,11.6,1.26389075699999));
#191366=CARTESIAN_POINT('Ctrl Pts',(10.8825356119999,15.2,1.26454937599998));
#191367=CARTESIAN_POINT('Ctrl Pts',(10.8825356119999,11.6,1.26454937599998));
#191368=CARTESIAN_POINT('Ctrl Pts',(10.8796296409999,15.2,1.26520441099998));
#191369=CARTESIAN_POINT('Ctrl Pts',(10.8796296409999,11.6,1.26520441099998));
#191370=CARTESIAN_POINT('Ctrl Pts',(10.8767284329999,15.2,1.26585586799999));
#191371=CARTESIAN_POINT('Ctrl Pts',(10.8767284329999,11.6,1.26585586799999));
#191372=CARTESIAN_POINT('Ctrl Pts',(10.8738319979999,15.2,1.26650375199999));
#191373=CARTESIAN_POINT('Ctrl Pts',(10.8738319979999,11.6,1.26650375199999));
#191374=CARTESIAN_POINT('Ctrl Pts',(10.8709403489999,15.2,1.26714806999999));
#191375=CARTESIAN_POINT('Ctrl Pts',(10.8709403489999,11.6,1.26714806999999));
#191376=CARTESIAN_POINT('Ctrl Pts',(10.8680534959999,15.2,1.26778882499998));
#191377=CARTESIAN_POINT('Ctrl Pts',(10.8680534959999,11.6,1.26778882499998));
#191378=CARTESIAN_POINT('Ctrl Pts',(10.8651714489999,15.2,1.26842602399998));
#191379=CARTESIAN_POINT('Ctrl Pts',(10.8651714489999,11.6,1.26842602399998));
#191380=CARTESIAN_POINT('Ctrl Pts',(10.8622942209999,15.2,1.26905967299999));
#191381=CARTESIAN_POINT('Ctrl Pts',(10.8622942209999,11.6,1.26905967299999));
#191382=CARTESIAN_POINT('Ctrl Pts',(10.8594218239999,15.2,1.26968977599998));
#191383=CARTESIAN_POINT('Ctrl Pts',(10.8594218239999,11.6,1.26968977599998));
#191384=CARTESIAN_POINT('Ctrl Pts',(10.8565542679999,15.2,1.27031633899998));
#191385=CARTESIAN_POINT('Ctrl Pts',(10.8565542679999,11.6,1.27031633899998));
#191386=CARTESIAN_POINT('Ctrl Pts',(10.8536915629999,15.2,1.27093936699998));
#191387=CARTESIAN_POINT('Ctrl Pts',(10.8536915629999,11.6,1.27093936699998));
#191388=CARTESIAN_POINT('Ctrl Pts',(10.8508337229999,15.2,1.27155886699999));
#191389=CARTESIAN_POINT('Ctrl Pts',(10.8508337229999,11.6,1.27155886699999));
#191390=CARTESIAN_POINT('Ctrl Pts',(10.8479807569999,15.2,1.27217484299999));
#191391=CARTESIAN_POINT('Ctrl Pts',(10.8479807569999,11.6,1.27217484299999));
#191392=CARTESIAN_POINT('Ctrl Pts',(10.8451326779999,15.2,1.27278730199999));
#191393=CARTESIAN_POINT('Ctrl Pts',(10.8451326779999,11.6,1.27278730199999));
#191394=CARTESIAN_POINT('Ctrl Pts',(10.8422894959999,15.2,1.27339624799998));
#191395=CARTESIAN_POINT('Ctrl Pts',(10.8422894959999,11.6,1.27339624799998));
#191396=CARTESIAN_POINT('Ctrl Pts',(10.8394512219999,15.2,1.27400168799999));
#191397=CARTESIAN_POINT('Ctrl Pts',(10.8394512219999,11.6,1.27400168799999));
#191398=CARTESIAN_POINT('Ctrl Pts',(10.8366178699999,15.2,1.27460362699999));
#191399=CARTESIAN_POINT('Ctrl Pts',(10.8366178699999,11.6,1.27460362699999));
#191400=CARTESIAN_POINT('Ctrl Pts',(10.8337894499999,15.2,1.27520206999999));
#191401=CARTESIAN_POINT('Ctrl Pts',(10.8337894499999,11.6,1.27520206999999));
#191402=CARTESIAN_POINT('Ctrl Pts',(10.8309659719999,15.2,1.27579702399998));
#191403=CARTESIAN_POINT('Ctrl Pts',(10.8309659719999,11.6,1.27579702399998));
#191404=CARTESIAN_POINT('Ctrl Pts',(10.8281474499999,15.2,1.27638849299998));
#191405=CARTESIAN_POINT('Ctrl Pts',(10.8281474499999,11.6,1.27638849299998));
#191406=CARTESIAN_POINT('Ctrl Pts',(10.8253338939999,15.2,1.27697648499999));
#191407=CARTESIAN_POINT('Ctrl Pts',(10.8253338939999,11.6,1.27697648499998));
#191408=CARTESIAN_POINT('Ctrl Pts',(10.8225253159999,15.2,1.27756100399999));
#191409=CARTESIAN_POINT('Ctrl Pts',(10.8225253159999,11.6,1.27756100399999));
#191410=CARTESIAN_POINT('Ctrl Pts',(10.8197217269999,15.2,1.27814205699998));
#191411=CARTESIAN_POINT('Ctrl Pts',(10.8197217269999,11.6,1.27814205699998));
#191412=CARTESIAN_POINT('Ctrl Pts',(10.8169231379999,15.2,1.27871964799999));
#191413=CARTESIAN_POINT('Ctrl Pts',(10.8169231379999,11.6,1.27871964799999));
#191414=CARTESIAN_POINT('Ctrl Pts',(10.8141295629999,15.2,1.27929378499998));
#191415=CARTESIAN_POINT('Ctrl Pts',(10.8141295629999,11.6,1.27929378499998));
#191416=CARTESIAN_POINT('Ctrl Pts',(10.8113410119999,15.2,1.27986447199998));
#191417=CARTESIAN_POINT('Ctrl Pts',(10.8113410119999,11.6,1.27986447199998));
#191418=CARTESIAN_POINT('Ctrl Pts',(10.8085574969999,15.2,1.28043171599999));
#191419=CARTESIAN_POINT('Ctrl Pts',(10.8085574969999,11.6,1.28043171599999));
#191420=CARTESIAN_POINT('Ctrl Pts',(10.8057790279999,15.2,1.28099552199998));
#191421=CARTESIAN_POINT('Ctrl Pts',(10.8057790279999,11.6,1.28099552199998));
#191422=CARTESIAN_POINT('Ctrl Pts',(10.8030056189999,15.2,1.28155589599999));
#191423=CARTESIAN_POINT('Ctrl Pts',(10.8030056189999,11.6,1.28155589599999));
#191424=CARTESIAN_POINT('Ctrl Pts',(10.8002372809999,15.2,1.28211284599999));
#191425=CARTESIAN_POINT('Ctrl Pts',(10.8002372809999,11.6,1.28211284599998));
#191426=CARTESIAN_POINT('Ctrl Pts',(10.7974740259999,15.2,1.28266637499999));
#191427=CARTESIAN_POINT('Ctrl Pts',(10.7974740259999,11.6,1.28266637499999));
#191428=CARTESIAN_POINT('Ctrl Pts',(10.7947158649999,15.2,1.28321648999998));
#191429=CARTESIAN_POINT('Ctrl Pts',(10.7947158649999,11.6,1.28321648999998));
#191430=CARTESIAN_POINT('Ctrl Pts',(10.7919628099999,15.2,1.28376319699999));
#191431=CARTESIAN_POINT('Ctrl Pts',(10.7919628099999,11.6,1.28376319699999));
#191432=CARTESIAN_POINT('Ctrl Pts',(10.7892148729999,15.2,1.28430650299999));
#191433=CARTESIAN_POINT('Ctrl Pts',(10.7892148729999,11.6,1.28430650299999));
#191434=CARTESIAN_POINT('Ctrl Pts',(10.7864720659999,15.2,1.28484641299998));
#191435=CARTESIAN_POINT('Ctrl Pts',(10.7864720659999,11.6,1.28484641299998));
#191436=CARTESIAN_POINT('Ctrl Pts',(10.7837344009999,15.2,1.28538293399998));
#191437=CARTESIAN_POINT('Ctrl Pts',(10.7837344009999,11.6,1.28538293399998));
#191438=CARTESIAN_POINT('Ctrl Pts',(10.7810018879999,15.2,1.28591607099999));
#191439=CARTESIAN_POINT('Ctrl Pts',(10.7810018879999,11.6,1.28591607099999));
#191440=CARTESIAN_POINT('Ctrl Pts',(10.7782745419999,15.2,1.28644583099998));
#191441=CARTESIAN_POINT('Ctrl Pts',(10.7782745419999,11.6,1.28644583099998));
#191442=CARTESIAN_POINT('Ctrl Pts',(10.7755523729999,15.2,1.28697221799999));
#191443=CARTESIAN_POINT('Ctrl Pts',(10.7755523729999,11.6,1.28697221799999));
#191444=CARTESIAN_POINT('Ctrl Pts',(10.7728353919999,15.2,1.28749524099999));
#191445=CARTESIAN_POINT('Ctrl Pts',(10.7728353919999,11.6,1.28749524099998));
#191446=CARTESIAN_POINT('Ctrl Pts',(10.7701236149999,15.2,1.28801490499999));
#191447=CARTESIAN_POINT('Ctrl Pts',(10.7701236149999,11.6,1.28801490499999));
#191448=CARTESIAN_POINT('Ctrl Pts',(10.7674170489999,15.2,1.28853121599999));
#191449=CARTESIAN_POINT('Ctrl Pts',(10.7674170489999,11.6,1.28853121599999));
#191450=CARTESIAN_POINT('Ctrl Pts',(10.7647157089999,15.2,1.28904418099999));
#191451=CARTESIAN_POINT('Ctrl Pts',(10.7647157089999,11.6,1.28904418099998));
#191452=CARTESIAN_POINT('Ctrl Pts',(10.7620196059999,15.2,1.28955380499999));
#191453=CARTESIAN_POINT('Ctrl Pts',(10.7620196059999,11.6,1.28955380499999));
#191454=CARTESIAN_POINT('Ctrl Pts',(10.7593287539999,15.2,1.29006009499999));
#191455=CARTESIAN_POINT('Ctrl Pts',(10.7593287539999,11.6,1.29006009499998));
#191456=CARTESIAN_POINT('Ctrl Pts',(10.7566431619999,15.2,1.29056305799998));
#191457=CARTESIAN_POINT('Ctrl Pts',(10.7566431619999,11.6,1.29056305799998));
#191458=CARTESIAN_POINT('Ctrl Pts',(10.7539628449999,15.2,1.29106269999999));
#191459=CARTESIAN_POINT('Ctrl Pts',(10.7539628449999,11.6,1.29106269999998));
#191460=CARTESIAN_POINT('Ctrl Pts',(10.7512878129999,15.2,1.29155902599999));
#191461=CARTESIAN_POINT('Ctrl Pts',(10.7512878129999,11.6,1.29155902599999));
#191462=CARTESIAN_POINT('Ctrl Pts',(10.7486180789999,15.2,1.29205204399998));
#191463=CARTESIAN_POINT('Ctrl Pts',(10.7486180789999,11.6,1.29205204399998));
#191464=CARTESIAN_POINT('Ctrl Pts',(10.7459536549999,15.2,1.29254175999999));
#191465=CARTESIAN_POINT('Ctrl Pts',(10.7459536549999,11.6,1.29254175999999));
#191466=CARTESIAN_POINT('Ctrl Pts',(10.7432945539999,15.2,1.29302817899998));
#191467=CARTESIAN_POINT('Ctrl Pts',(10.7432945539999,11.6,1.29302817899998));
#191468=CARTESIAN_POINT('Ctrl Pts',(10.7406407879999,15.2,1.29351130999999));
#191469=CARTESIAN_POINT('Ctrl Pts',(10.7406407879999,11.6,1.29351130999999));
#191470=CARTESIAN_POINT('Ctrl Pts',(10.7379923689999,15.2,1.29399115799998));
#191471=CARTESIAN_POINT('Ctrl Pts',(10.7379923689999,11.6,1.29399115799998));
#191472=CARTESIAN_POINT('Ctrl Pts',(10.7353493089999,15.2,1.29446772899998));
#191473=CARTESIAN_POINT('Ctrl Pts',(10.7353493089999,11.6,1.29446772899998));
#191474=CARTESIAN_POINT('Ctrl Pts',(10.7327116219999,15.2,1.29494102999999));
#191475=CARTESIAN_POINT('Ctrl Pts',(10.7327116219999,11.6,1.29494102999998));
#191476=CARTESIAN_POINT('Ctrl Pts',(10.7300793179999,15.2,1.29541106899998));
#191477=CARTESIAN_POINT('Ctrl Pts',(10.7300793179999,11.6,1.29541106899998));
#191478=CARTESIAN_POINT('Ctrl Pts',(10.7274524109999,15.2,1.29587785099998));
#191479=CARTESIAN_POINT('Ctrl Pts',(10.7274524109999,11.6,1.29587785099998));
#191480=CARTESIAN_POINT('Ctrl Pts',(10.7248309119999,15.2,1.29634138299998));
#191481=CARTESIAN_POINT('Ctrl Pts',(10.7248309119999,11.6,1.29634138299998));
#191482=CARTESIAN_POINT('Ctrl Pts',(10.7222148359999,15.2,1.29680166999998));
#191483=CARTESIAN_POINT('Ctrl Pts',(10.7222148359999,11.6,1.29680166999998));
#191484=CARTESIAN_POINT('Ctrl Pts',(10.7196041929999,15.2,1.29725872299999));
#191485=CARTESIAN_POINT('Ctrl Pts',(10.7196041929999,11.6,1.29725872299999));
#191486=CARTESIAN_POINT('Ctrl Pts',(10.7169989959999,15.2,1.29771254499999));
#191487=CARTESIAN_POINT('Ctrl Pts',(10.7169989959999,11.6,1.29771254499999));
#191488=CARTESIAN_POINT('Ctrl Pts',(10.7143992589999,15.2,1.29816314299998));
#191489=CARTESIAN_POINT('Ctrl Pts',(10.7143992589999,11.6,1.29816314299998));
#191490=CARTESIAN_POINT('Ctrl Pts',(10.7118049929999,15.2,1.29861052499999));
#191491=CARTESIAN_POINT('Ctrl Pts',(10.7118049929999,11.6,1.29861052499999));
#191492=CARTESIAN_POINT('Ctrl Pts',(10.7092162099999,15.2,1.29905469699999));
#191493=CARTESIAN_POINT('Ctrl Pts',(10.7092162099999,11.6,1.29905469699999));
#191494=CARTESIAN_POINT('Ctrl Pts',(10.7066329249999,15.2,1.29949566599999));
#191495=CARTESIAN_POINT('Ctrl Pts',(10.7066329249999,11.6,1.29949566599999));
#191496=CARTESIAN_POINT('Ctrl Pts',(10.7040551489999,15.2,1.29993343899999));
#191497=CARTESIAN_POINT('Ctrl Pts',(10.7040551489999,11.6,1.29993343899998));
#191498=CARTESIAN_POINT('Ctrl Pts',(10.7014828959999,15.2,1.30036802199998));
#191499=CARTESIAN_POINT('Ctrl Pts',(10.7014828959999,11.6,1.30036802199998));
#191500=CARTESIAN_POINT('Ctrl Pts',(10.6989161759999,15.2,1.30079942299998));
#191501=CARTESIAN_POINT('Ctrl Pts',(10.6989161759999,11.6,1.30079942299998));
#191502=CARTESIAN_POINT('Ctrl Pts',(10.6963550049999,15.2,1.30122764799999));
#191503=CARTESIAN_POINT('Ctrl Pts',(10.6963550049999,11.6,1.30122764799998));
#191504=CARTESIAN_POINT('Ctrl Pts',(10.6937993929999,15.2,1.30165270599999));
#191505=CARTESIAN_POINT('Ctrl Pts',(10.6937993929999,11.6,1.30165270599999));
#191506=CARTESIAN_POINT('Ctrl Pts',(10.6912493539999,15.2,1.30207460099999));
#191507=CARTESIAN_POINT('Ctrl Pts',(10.6912493539999,11.6,1.30207460099998));
#191508=CARTESIAN_POINT('Ctrl Pts',(10.6887049019999,15.2,1.30249334199998));
#191509=CARTESIAN_POINT('Ctrl Pts',(10.6887049019999,11.6,1.30249334199998));
#191510=CARTESIAN_POINT('Ctrl Pts',(10.6861660479999,15.2,1.30290893499998));
#191511=CARTESIAN_POINT('Ctrl Pts',(10.6861660479999,11.6,1.30290893499998));
#191512=CARTESIAN_POINT('Ctrl Pts',(10.6836328059999,15.2,1.30332138799998));
#191513=CARTESIAN_POINT('Ctrl Pts',(10.6836328059999,11.6,1.30332138799998));
#191514=CARTESIAN_POINT('Ctrl Pts',(10.6811051889999,15.2,1.30373070699998));
#191515=CARTESIAN_POINT('Ctrl Pts',(10.6811051889999,11.6,1.30373070699998));
#191516=CARTESIAN_POINT('Ctrl Pts',(10.6785832079999,15.2,1.30413689899999));
#191517=CARTESIAN_POINT('Ctrl Pts',(10.6785832079999,11.6,1.30413689899999));
#191518=CARTESIAN_POINT('Ctrl Pts',(10.6760668779999,15.2,1.30453997299998));
#191519=CARTESIAN_POINT('Ctrl Pts',(10.6760668779999,11.6,1.30453997299998));
#191520=CARTESIAN_POINT('Ctrl Pts',(10.6735562119999,15.2,1.30493993399998));
#191521=CARTESIAN_POINT('Ctrl Pts',(10.6735562119999,11.6,1.30493993399998));
#191522=CARTESIAN_POINT('Ctrl Pts',(10.6710512209999,15.2,1.30533679099999));
#191523=CARTESIAN_POINT('Ctrl Pts',(10.6710512209999,11.6,1.30533679099999));
#191524=CARTESIAN_POINT('Ctrl Pts',(10.6685519209999,15.2,1.30573054999998));
#191525=CARTESIAN_POINT('Ctrl Pts',(10.6685519209999,11.6,1.30573054999998));
#191526=CARTESIAN_POINT('Ctrl Pts',(10.6660583229999,15.2,1.30612121799999));
#191527=CARTESIAN_POINT('Ctrl Pts',(10.6660583229999,11.6,1.30612121799999));
#191528=CARTESIAN_POINT('Ctrl Pts',(10.6635704409999,15.2,1.30650880399998));
#191529=CARTESIAN_POINT('Ctrl Pts',(10.6635704409999,11.6,1.30650880399998));
#191530=CARTESIAN_POINT('Ctrl Pts',(10.6610882879999,15.2,1.30689331299998));
#191531=CARTESIAN_POINT('Ctrl Pts',(10.6610882879999,11.6,1.30689331299998));
#191532=CARTESIAN_POINT('Ctrl Pts',(10.6586118759999,15.2,1.30727475299999));
#191533=CARTESIAN_POINT('Ctrl Pts',(10.6586118759999,11.6,1.30727475299999));
#191534=CARTESIAN_POINT('Ctrl Pts',(10.6561412199999,15.2,1.30765313299999));
#191535=CARTESIAN_POINT('Ctrl Pts',(10.6561412199999,11.6,1.30765313299999));
#191536=CARTESIAN_POINT('Ctrl Pts',(10.6536763329999,15.2,1.30802845899999));
#191537=CARTESIAN_POINT('Ctrl Pts',(10.6536763329999,11.6,1.30802845899999));
#191538=CARTESIAN_POINT('Ctrl Pts',(10.6512172259999,15.2,1.30840073799999));
#191539=CARTESIAN_POINT('Ctrl Pts',(10.6512172259999,11.6,1.30840073799999));
#191540=CARTESIAN_POINT('Ctrl Pts',(10.6487639159999,15.2,1.30876997899998));
#191541=CARTESIAN_POINT('Ctrl Pts',(10.6487639159999,11.6,1.30876997899998));
#191542=CARTESIAN_POINT('Ctrl Pts',(10.6463164129999,15.2,1.30913618899998));
#191543=CARTESIAN_POINT('Ctrl Pts',(10.6463164129999,11.6,1.30913618899998));
#191544=CARTESIAN_POINT('Ctrl Pts',(10.6438747329999,15.2,1.30949937399999));
#191545=CARTESIAN_POINT('Ctrl Pts',(10.6438747329999,11.6,1.30949937399999));
#191546=CARTESIAN_POINT('Ctrl Pts',(10.6414388879999,15.2,1.30985954199998));
#191547=CARTESIAN_POINT('Ctrl Pts',(10.6414388879999,11.6,1.30985954199998));
#191548=CARTESIAN_POINT('Ctrl Pts',(10.6390088909999,15.2,1.31021670299999));
#191549=CARTESIAN_POINT('Ctrl Pts',(10.6390088909999,11.6,1.31021670299999));
#191550=CARTESIAN_POINT('Ctrl Pts',(10.6365847569999,15.2,1.31057086099998));
#191551=CARTESIAN_POINT('Ctrl Pts',(10.6365847569999,11.6,1.31057086099998));
#191552=CARTESIAN_POINT('Ctrl Pts',(10.6341664979999,15.2,1.31092202699998));
#191553=CARTESIAN_POINT('Ctrl Pts',(10.6341664979999,11.6,1.31092202699998));
#191554=CARTESIAN_POINT('Ctrl Pts',(10.6317541279999,15.2,1.31127020699998));
#191555=CARTESIAN_POINT('Ctrl Pts',(10.6317541279999,11.6,1.31127020699998));
#191556=CARTESIAN_POINT('Ctrl Pts',(10.6293476599999,15.2,1.31161540699999));
#191557=CARTESIAN_POINT('Ctrl Pts',(10.6293476599999,11.6,1.31161540699999));
#191558=CARTESIAN_POINT('Ctrl Pts',(10.6269471099999,15.2,1.31195763899999));
#191559=CARTESIAN_POINT('Ctrl Pts',(10.6269471099999,11.6,1.31195763899999));
#191560=CARTESIAN_POINT('Ctrl Pts',(10.6245524889999,15.2,1.31229690699998));
#191561=CARTESIAN_POINT('Ctrl Pts',(10.6245524889999,11.6,1.31229690699998));
#191562=CARTESIAN_POINT('Ctrl Pts',(10.6221638119999,15.2,1.31263321999999));
#191563=CARTESIAN_POINT('Ctrl Pts',(10.6221638119999,11.6,1.31263321999999));
#191564=CARTESIAN_POINT('Ctrl Pts',(10.6197810909999,15.2,1.31296658599998));
#191565=CARTESIAN_POINT('Ctrl Pts',(10.6197810909999,11.6,1.31296658599998));
#191566=CARTESIAN_POINT('Ctrl Pts',(10.6174043419999,15.2,1.31329701299999));
#191567=CARTESIAN_POINT('Ctrl Pts',(10.6174043419999,11.6,1.31329701299999));
#191568=CARTESIAN_POINT('Ctrl Pts',(10.6150335779999,15.2,1.31362450999998));
#191569=CARTESIAN_POINT('Ctrl Pts',(10.6150335779999,11.6,1.31362450999998));
#191570=CARTESIAN_POINT('Ctrl Pts',(10.6126688119999,15.2,1.31394908099999));
#191571=CARTESIAN_POINT('Ctrl Pts',(10.6126688119999,11.6,1.31394908099998));
#191572=CARTESIAN_POINT('Ctrl Pts',(10.6103100589999,15.2,1.31427073799999));
#191573=CARTESIAN_POINT('Ctrl Pts',(10.6103100589999,11.6,1.31427073799998));
#191574=CARTESIAN_POINT('Ctrl Pts',(10.6079573329999,15.2,1.31458948699999));
#191575=CARTESIAN_POINT('Ctrl Pts',(10.6079573329999,11.6,1.31458948699999));
#191576=CARTESIAN_POINT('Ctrl Pts',(10.6056106459999,15.2,1.31490533699999));
#191577=CARTESIAN_POINT('Ctrl Pts',(10.6056106459999,11.6,1.31490533699999));
#191578=CARTESIAN_POINT('Ctrl Pts',(10.6032700129999,15.2,1.31521829699999));
#191579=CARTESIAN_POINT('Ctrl Pts',(10.6032700129999,11.6,1.31521829699999));
#191580=CARTESIAN_POINT('Ctrl Pts',(10.6009354489999,15.2,1.31552837099999));
#191581=CARTESIAN_POINT('Ctrl Pts',(10.6009354489999,11.6,1.31552837099999));
#191582=CARTESIAN_POINT('Ctrl Pts',(10.5986069669999,15.2,1.31583557099999));
#191583=CARTESIAN_POINT('Ctrl Pts',(10.5986069669999,11.6,1.31583557099999));
#191584=CARTESIAN_POINT('Ctrl Pts',(10.5962845809999,15.2,1.31613990499998));
#191585=CARTESIAN_POINT('Ctrl Pts',(10.5962845809999,11.6,1.31613990499998));
#191586=CARTESIAN_POINT('Ctrl Pts',(10.5939683049999,15.2,1.31644137899999));
#191587=CARTESIAN_POINT('Ctrl Pts',(10.5939683049999,11.6,1.31644137899999));
#191588=CARTESIAN_POINT('Ctrl Pts',(10.5916581539999,15.2,1.31674000199999));
#191589=CARTESIAN_POINT('Ctrl Pts',(10.5916581539999,11.6,1.31674000199998));
#191590=CARTESIAN_POINT('Ctrl Pts',(10.5893541409999,15.2,1.31703578299998));
#191591=CARTESIAN_POINT('Ctrl Pts',(10.5893541409999,11.6,1.31703578299998));
#191592=CARTESIAN_POINT('Ctrl Pts',(10.5870562799999,15.2,1.31732872999998));
#191593=CARTESIAN_POINT('Ctrl Pts',(10.5870562799999,11.6,1.31732872999998));
#191594=CARTESIAN_POINT('Ctrl Pts',(10.5847645859999,15.2,1.31761885099999));
#191595=CARTESIAN_POINT('Ctrl Pts',(10.5847645859999,11.6,1.31761885099999));
#191596=CARTESIAN_POINT('Ctrl Pts',(10.5824790749999,15.2,1.31790615499999));
#191597=CARTESIAN_POINT('Ctrl Pts',(10.5824790749999,11.6,1.31790615499999));
#191598=CARTESIAN_POINT('Ctrl Pts',(10.5801997579999,15.2,1.31819064899998));
#191599=CARTESIAN_POINT('Ctrl Pts',(10.5801997579999,11.6,1.31819064899998));
#191600=CARTESIAN_POINT('Ctrl Pts',(10.5779266509999,15.2,1.31847234299999));
#191601=CARTESIAN_POINT('Ctrl Pts',(10.5779266509999,11.6,1.31847234299999));
#191602=CARTESIAN_POINT('Ctrl Pts',(10.5756597679999,15.2,1.31875124499999));
#191603=CARTESIAN_POINT('Ctrl Pts',(10.5756597679999,11.6,1.31875124499999));
#191604=CARTESIAN_POINT('Ctrl Pts',(10.5733991249999,15.2,1.31902736299998));
#191605=CARTESIAN_POINT('Ctrl Pts',(10.5733991249999,11.6,1.31902736299998));
#191606=CARTESIAN_POINT('Ctrl Pts',(10.5711447329999,15.2,1.31930070599998));
#191607=CARTESIAN_POINT('Ctrl Pts',(10.5711447329999,11.6,1.31930070599998));
#191608=CARTESIAN_POINT('Ctrl Pts',(10.5688966099999,15.2,1.31957128299999));
#191609=CARTESIAN_POINT('Ctrl Pts',(10.5688966099999,11.6,1.31957128299998));
#191610=CARTESIAN_POINT('Ctrl Pts',(10.5666547689999,15.2,1.31983910099999));
#191611=CARTESIAN_POINT('Ctrl Pts',(10.5666547689999,11.6,1.31983910099999));
#191612=CARTESIAN_POINT('Ctrl Pts',(10.5644192249999,15.2,1.32010417099998));
#191613=CARTESIAN_POINT('Ctrl Pts',(10.5644192249999,11.6,1.32010417099998));
#191614=CARTESIAN_POINT('Ctrl Pts',(10.5621899909999,15.2,1.32036649799999));
#191615=CARTESIAN_POINT('Ctrl Pts',(10.5621899909999,11.6,1.32036649799998));
#191616=CARTESIAN_POINT('Ctrl Pts',(10.5599670829999,15.2,1.32062609399998));
#191617=CARTESIAN_POINT('Ctrl Pts',(10.5599670829999,11.6,1.32062609399998));
#191618=CARTESIAN_POINT('Ctrl Pts',(10.5577505169999,15.2,1.32088296799999));
#191619=CARTESIAN_POINT('Ctrl Pts',(10.5577505169999,11.6,1.32088296799999));
#191620=CARTESIAN_POINT('Ctrl Pts',(10.5555403039999,15.2,1.32113712699998));
#191621=CARTESIAN_POINT('Ctrl Pts',(10.5555403039999,11.6,1.32113712699998));
#191622=CARTESIAN_POINT('Ctrl Pts',(10.5533364629999,15.2,1.32138857999998));
#191623=CARTESIAN_POINT('Ctrl Pts',(10.5533364629999,11.6,1.32138857999998));
#191624=CARTESIAN_POINT('Ctrl Pts',(10.5511390059999,15.2,1.32163733699999));
#191625=CARTESIAN_POINT('Ctrl Pts',(10.5511390059999,11.6,1.32163733699999));
#191626=CARTESIAN_POINT('Ctrl Pts',(10.5489479479999,15.2,1.32188340599999));
#191627=CARTESIAN_POINT('Ctrl Pts',(10.5489479479999,11.6,1.32188340599999));
#191628=CARTESIAN_POINT('Ctrl Pts',(10.5467633059999,15.2,1.32212679499998));
#191629=CARTESIAN_POINT('Ctrl Pts',(10.5467633059999,11.6,1.32212679499998));
#191630=CARTESIAN_POINT('Ctrl Pts',(10.5445850929999,15.2,1.32236751399998));
#191631=CARTESIAN_POINT('Ctrl Pts',(10.5445850929999,11.6,1.32236751399998));
#191632=CARTESIAN_POINT('Ctrl Pts',(10.5424133229999,15.2,1.32260557299999));
#191633=CARTESIAN_POINT('Ctrl Pts',(10.5424133229999,11.6,1.32260557299999));
#191634=CARTESIAN_POINT('Ctrl Pts',(10.5402480139999,15.2,1.32284097999999));
#191635=CARTESIAN_POINT('Ctrl Pts',(10.5402480139999,11.6,1.32284097999999));
#191636=CARTESIAN_POINT('Ctrl Pts',(10.5380891789999,15.2,1.32307374399999));
#191637=CARTESIAN_POINT('Ctrl Pts',(10.5380891789999,11.6,1.32307374399998));
#191638=CARTESIAN_POINT('Ctrl Pts',(10.5359368329999,15.2,1.32330387399998));
#191639=CARTESIAN_POINT('Ctrl Pts',(10.5359368329999,11.6,1.32330387399998));
#191640=CARTESIAN_POINT('Ctrl Pts',(10.5337909929999,15.2,1.32353137899999));
#191641=CARTESIAN_POINT('Ctrl Pts',(10.5337909929999,11.6,1.32353137899999));
#191642=CARTESIAN_POINT('Ctrl Pts',(10.5316516719999,15.2,1.32375626999998));
#191643=CARTESIAN_POINT('Ctrl Pts',(10.5316516719999,11.6,1.32375626999998));
#191644=CARTESIAN_POINT('Ctrl Pts',(10.5295188859999,15.2,1.32397855399998));
#191645=CARTESIAN_POINT('Ctrl Pts',(10.5295188859999,11.6,1.32397855399998));
#191646=CARTESIAN_POINT('Ctrl Pts',(10.5273926489999,15.2,1.32419824099999));
#191647=CARTESIAN_POINT('Ctrl Pts',(10.5273926489999,11.6,1.32419824099998));
#191648=CARTESIAN_POINT('Ctrl Pts',(10.5252729789999,15.2,1.32441534099998));
#191649=CARTESIAN_POINT('Ctrl Pts',(10.5252729789999,11.6,1.32441534099998));
#191650=CARTESIAN_POINT('Ctrl Pts',(10.5231598899999,15.2,1.32462986199998));
#191651=CARTESIAN_POINT('Ctrl Pts',(10.5231598899999,11.6,1.32462986199998));
#191652=CARTESIAN_POINT('Ctrl Pts',(10.5210533959999,15.2,1.32484181499999));
#191653=CARTESIAN_POINT('Ctrl Pts',(10.5210533959999,11.6,1.32484181499999));
#191654=CARTESIAN_POINT('Ctrl Pts',(10.5189535149999,15.2,1.32505120799999));
#191655=CARTESIAN_POINT('Ctrl Pts',(10.5189535149999,11.6,1.32505120799998));
#191656=CARTESIAN_POINT('Ctrl Pts',(10.5168602599999,15.2,1.32525805099998));
#191657=CARTESIAN_POINT('Ctrl Pts',(10.5168602599999,11.6,1.32525805099998));
#191658=CARTESIAN_POINT('Ctrl Pts',(10.5147736479999,15.2,1.32546235499999));
#191659=CARTESIAN_POINT('Ctrl Pts',(10.5147736479999,11.6,1.32546235499999));
#191660=CARTESIAN_POINT('Ctrl Pts',(10.5126936939999,15.2,1.32566412699999));
#191661=CARTESIAN_POINT('Ctrl Pts',(10.5126936939999,11.6,1.32566412699999));
#191662=CARTESIAN_POINT('Ctrl Pts',(10.5106204149999,15.2,1.32586337799999));
#191663=CARTESIAN_POINT('Ctrl Pts',(10.5106204149999,11.6,1.32586337799998));
#191664=CARTESIAN_POINT('Ctrl Pts',(10.5085538239999,15.2,1.32606011699998));
#191665=CARTESIAN_POINT('Ctrl Pts',(10.5085538239999,11.6,1.32606011699998));
#191666=CARTESIAN_POINT('Ctrl Pts',(10.5064939389999,15.2,1.32625435499999));
#191667=CARTESIAN_POINT('Ctrl Pts',(10.5064939389999,11.6,1.32625435499999));
#191668=CARTESIAN_POINT('Ctrl Pts',(10.5044407749999,15.2,1.32644610099999));
#191669=CARTESIAN_POINT('Ctrl Pts',(10.5044407749999,11.6,1.32644610099998));
#191670=CARTESIAN_POINT('Ctrl Pts',(10.5023943459999,15.2,1.32663536299999));
#191671=CARTESIAN_POINT('Ctrl Pts',(10.5023943459999,11.6,1.32663536299999));
#191672=CARTESIAN_POINT('Ctrl Pts',(10.5003546709999,15.2,1.32682215399999));
#191673=CARTESIAN_POINT('Ctrl Pts',(10.5003546709999,11.6,1.32682215399999));
#191674=CARTESIAN_POINT('Ctrl Pts',(10.4983217629999,15.2,1.32700648099998));
#191675=CARTESIAN_POINT('Ctrl Pts',(10.4983217629999,11.6,1.32700648099998));
#191676=CARTESIAN_POINT('Ctrl Pts',(10.4962956399999,15.2,1.32718835599999));
#191677=CARTESIAN_POINT('Ctrl Pts',(10.4962956399999,11.6,1.32718835599999));
#191678=CARTESIAN_POINT('Ctrl Pts',(10.4942763159999,15.2,1.32736778799998));
#191679=CARTESIAN_POINT('Ctrl Pts',(10.4942763159999,11.6,1.32736778799998));
#191680=CARTESIAN_POINT('Ctrl Pts',(10.4922638099999,15.2,1.32754478599999));
#191681=CARTESIAN_POINT('Ctrl Pts',(10.4922638099999,11.6,1.32754478599999));
#191682=CARTESIAN_POINT('Ctrl Pts',(10.4902581349999,15.2,1.32771936199998));
#191683=CARTESIAN_POINT('Ctrl Pts',(10.4902581349999,11.6,1.32771936199998));
#191684=CARTESIAN_POINT('Ctrl Pts',(10.4882593079999,15.2,1.32789152599999));
#191685=CARTESIAN_POINT('Ctrl Pts',(10.4882593079999,11.6,1.32789152599999));
#191686=CARTESIAN_POINT('Ctrl Pts',(10.4862673459999,15.2,1.32806128699999));
#191687=CARTESIAN_POINT('Ctrl Pts',(10.4862673459999,11.6,1.32806128699999));
#191688=CARTESIAN_POINT('Ctrl Pts',(10.4842822649999,15.2,1.32822865399998));
#191689=CARTESIAN_POINT('Ctrl Pts',(10.4842822649999,11.6,1.32822865399998));
#191690=CARTESIAN_POINT('Ctrl Pts',(10.4823040789999,15.2,1.32839363899999));
#191691=CARTESIAN_POINT('Ctrl Pts',(10.4823040789999,11.6,1.32839363899999));
#191692=CARTESIAN_POINT('Ctrl Pts',(10.4803328079999,15.2,1.32855625199999));
#191693=CARTESIAN_POINT('Ctrl Pts',(10.4803328079999,11.6,1.32855625199999));
#191694=CARTESIAN_POINT('Ctrl Pts',(10.4783684649999,15.2,1.32871650399998));
#191695=CARTESIAN_POINT('Ctrl Pts',(10.4783684649999,11.6,1.32871650399998));
#191696=CARTESIAN_POINT('Ctrl Pts',(10.4764110689999,15.2,1.32887440299998));
#191697=CARTESIAN_POINT('Ctrl Pts',(10.4764110689999,11.6,1.32887440299998));
#191698=CARTESIAN_POINT('Ctrl Pts',(10.4744606349999,15.2,1.32902996199999));
#191699=CARTESIAN_POINT('Ctrl Pts',(10.4744606349999,11.6,1.32902996199999));
#191700=CARTESIAN_POINT('Ctrl Pts',(10.4725171799999,15.2,1.32918318999999));
#191701=CARTESIAN_POINT('Ctrl Pts',(10.4725171799999,11.6,1.32918318999998));
#191702=CARTESIAN_POINT('Ctrl Pts',(10.4705807189999,15.2,1.32933409699998));
#191703=CARTESIAN_POINT('Ctrl Pts',(10.4705807189999,11.6,1.32933409699998));
#191704=CARTESIAN_POINT('Ctrl Pts',(10.4686512709999,15.2,1.32948269499999));
#191705=CARTESIAN_POINT('Ctrl Pts',(10.4686512709999,11.6,1.32948269499999));
#191706=CARTESIAN_POINT('Ctrl Pts',(10.4667288519999,15.2,1.32962899399999));
#191707=CARTESIAN_POINT('Ctrl Pts',(10.4667288519999,11.6,1.32962899399998));
#191708=CARTESIAN_POINT('Ctrl Pts',(10.4648134769999,15.2,1.32977300399999));
#191709=CARTESIAN_POINT('Ctrl Pts',(10.4648134769999,11.6,1.32977300399999));
#191710=CARTESIAN_POINT('Ctrl Pts',(10.4629051649999,15.2,1.32991473599999));
#191711=CARTESIAN_POINT('Ctrl Pts',(10.4629051649999,11.6,1.32991473599999));
#191712=CARTESIAN_POINT('Ctrl Pts',(10.4610039309999,15.2,1.33005419999999));
#191713=CARTESIAN_POINT('Ctrl Pts',(10.4610039309999,11.6,1.33005419999999));
#191714=CARTESIAN_POINT('Ctrl Pts',(10.4591097919999,15.2,1.33019140799998));
#191715=CARTESIAN_POINT('Ctrl Pts',(10.4591097919999,11.6,1.33019140799998));
#191716=CARTESIAN_POINT('Ctrl Pts',(10.4572227669999,15.2,1.33032637099999));
#191717=CARTESIAN_POINT('Ctrl Pts',(10.4572227669999,11.6,1.33032637099999));
#191718=CARTESIAN_POINT('Ctrl Pts',(10.4553428709999,15.2,1.33045909899999));
#191719=CARTESIAN_POINT('Ctrl Pts',(10.4553428709999,11.6,1.33045909899998));
#191720=CARTESIAN_POINT('Ctrl Pts',(10.4534701199999,15.2,1.33058960299998));
#191721=CARTESIAN_POINT('Ctrl Pts',(10.4534701199999,11.6,1.33058960299998));
#191722=CARTESIAN_POINT('Ctrl Pts',(10.4516045329999,15.2,1.33071789399999));
#191723=CARTESIAN_POINT('Ctrl Pts',(10.4516045329999,11.6,1.33071789399999));
#191724=CARTESIAN_POINT('Ctrl Pts',(10.4497461279999,15.2,1.33084398299999));
#191725=CARTESIAN_POINT('Ctrl Pts',(10.4497461279999,11.6,1.33084398299998));
#191726=CARTESIAN_POINT('Ctrl Pts',(10.4478949189999,15.2,1.33096787999999));
#191727=CARTESIAN_POINT('Ctrl Pts',(10.4478949189999,11.6,1.33096787999999));
#191728=CARTESIAN_POINT('Ctrl Pts',(10.4460509249999,15.2,1.33108959799999));
#191729=CARTESIAN_POINT('Ctrl Pts',(10.4460509249999,11.6,1.33108959799999));
#191730=CARTESIAN_POINT('Ctrl Pts',(10.4442141639999,15.2,1.33120914799999));
#191731=CARTESIAN_POINT('Ctrl Pts',(10.4442141639999,11.6,1.33120914799999));
#191732=CARTESIAN_POINT('Ctrl Pts',(10.4423846519999,15.2,1.33132653899999));
#191733=CARTESIAN_POINT('Ctrl Pts',(10.4423846519999,11.6,1.33132653899999));
#191734=CARTESIAN_POINT('Ctrl Pts',(10.4405624069999,15.2,1.33144178399998));
#191735=CARTESIAN_POINT('Ctrl Pts',(10.4405624069999,11.6,1.33144178399998));
#191736=CARTESIAN_POINT('Ctrl Pts',(10.4387474469999,15.2,1.33155489399998));
#191737=CARTESIAN_POINT('Ctrl Pts',(10.4387474469999,11.6,1.33155489399998));
#191738=CARTESIAN_POINT('Ctrl Pts',(10.4369397879999,15.2,1.33166588099999));
#191739=CARTESIAN_POINT('Ctrl Pts',(10.4369397879999,11.6,1.33166588099999));
#191740=CARTESIAN_POINT('Ctrl Pts',(10.4351394479999,15.2,1.33177475499998));
#191741=CARTESIAN_POINT('Ctrl Pts',(10.4351394479999,11.6,1.33177475499998));
#191742=CARTESIAN_POINT('Ctrl Pts',(10.4333464449999,15.2,1.33188152799999));
#191743=CARTESIAN_POINT('Ctrl Pts',(10.4333464449999,11.6,1.33188152799998));
#191744=CARTESIAN_POINT('Ctrl Pts',(10.4315607969999,15.2,1.33198621299998));
#191745=CARTESIAN_POINT('Ctrl Pts',(10.4315607969999,11.6,1.33198621299998));
#191746=CARTESIAN_POINT('Ctrl Pts',(10.4297825219999,15.2,1.33208881899999));
#191747=CARTESIAN_POINT('Ctrl Pts',(10.4297825219999,11.6,1.33208881899999));
#191748=CARTESIAN_POINT('Ctrl Pts',(10.4280116349999,15.2,1.33218935899999));
#191749=CARTESIAN_POINT('Ctrl Pts',(10.4280116349999,11.6,1.33218935899999));
#191750=CARTESIAN_POINT('Ctrl Pts',(10.4262481579999,15.2,1.33228784499998));
#191751=CARTESIAN_POINT('Ctrl Pts',(10.4262481579999,11.6,1.33228784499998));
#191752=CARTESIAN_POINT('Ctrl Pts',(10.4244921049999,15.2,1.33238428799999));
#191753=CARTESIAN_POINT('Ctrl Pts',(10.4244921049999,11.6,1.33238428799999));
#191754=CARTESIAN_POINT('Ctrl Pts',(10.4227434979999,15.2,1.33247869999999));
#191755=CARTESIAN_POINT('Ctrl Pts',(10.4227434979999,11.6,1.33247869999999));
#191756=CARTESIAN_POINT('Ctrl Pts',(10.4210023509999,15.2,1.33257109199999));
#191757=CARTESIAN_POINT('Ctrl Pts',(10.4210023509999,11.6,1.33257109199999));
#191758=CARTESIAN_POINT('Ctrl Pts',(10.4192686839999,15.2,1.33266147799999));
#191759=CARTESIAN_POINT('Ctrl Pts',(10.4192686839999,11.6,1.33266147799999));
#191760=CARTESIAN_POINT('Ctrl Pts',(10.4175425149999,15.2,1.33274986699998));
#191761=CARTESIAN_POINT('Ctrl Pts',(10.4175425149999,11.6,1.33274986699998));
#191762=CARTESIAN_POINT('Ctrl Pts',(10.4158238619999,15.2,1.33283627399999));
#191763=CARTESIAN_POINT('Ctrl Pts',(10.4158238619999,11.6,1.33283627399999));
#191764=CARTESIAN_POINT('Ctrl Pts',(10.4141127429999,15.2,1.33292070899998));
#191765=CARTESIAN_POINT('Ctrl Pts',(10.4141127429999,11.6,1.33292070899998));
#191766=CARTESIAN_POINT('Ctrl Pts',(10.4124091789999,15.2,1.33300318499999));
#191767=CARTESIAN_POINT('Ctrl Pts',(10.4124091789999,11.6,1.33300318499999));
#191768=CARTESIAN_POINT('Ctrl Pts',(10.4107131829999,15.2,1.33308371299998));
#191769=CARTESIAN_POINT('Ctrl Pts',(10.4107131829999,11.6,1.33308371299998));
#191770=CARTESIAN_POINT('Ctrl Pts',(10.4090247779999,15.2,1.33316230699998));
#191771=CARTESIAN_POINT('Ctrl Pts',(10.4090247779999,11.6,1.33316230699998));
#191772=CARTESIAN_POINT('Ctrl Pts',(10.4073439809999,15.2,1.33323897699999));
#191773=CARTESIAN_POINT('Ctrl Pts',(10.4073439809999,11.6,1.33323897699999));
#191774=CARTESIAN_POINT('Ctrl Pts',(10.4056708099999,15.2,1.33331373699999));
#191775=CARTESIAN_POINT('Ctrl Pts',(10.4056708099999,11.6,1.33331373699999));
#191776=CARTESIAN_POINT('Ctrl Pts',(10.4040052849999,15.2,1.33338659999998));
#191777=CARTESIAN_POINT('Ctrl Pts',(10.4040052849999,11.6,1.33338659999998));
#191778=CARTESIAN_POINT('Ctrl Pts',(10.4023474229999,15.2,1.33345757799999));
#191779=CARTESIAN_POINT('Ctrl Pts',(10.4023474229999,11.6,1.33345757799999));
#191780=CARTESIAN_POINT('Ctrl Pts',(10.4006972429999,15.2,1.33352668099999));
#191781=CARTESIAN_POINT('Ctrl Pts',(10.4006972429999,11.6,1.33352668099999));
#191782=CARTESIAN_POINT('Ctrl Pts',(10.3990547659999,15.2,1.33359392399999));
#191783=CARTESIAN_POINT('Ctrl Pts',(10.3990547659999,11.6,1.33359392399999));
#191784=CARTESIAN_POINT('Ctrl Pts',(10.3974200079999,15.2,1.33365931999998));
#191785=CARTESIAN_POINT('Ctrl Pts',(10.3974200079999,11.6,1.33365931999998));
#191786=CARTESIAN_POINT('Ctrl Pts',(10.3957929889999,15.2,1.33372287999999));
#191787=CARTESIAN_POINT('Ctrl Pts',(10.3957929889999,11.6,1.33372287999999));
#191788=CARTESIAN_POINT('Ctrl Pts',(10.3941737289999,15.2,1.33378461799999));
#191789=CARTESIAN_POINT('Ctrl Pts',(10.3941737289999,11.6,1.33378461799999));
#191790=CARTESIAN_POINT('Ctrl Pts',(10.3925622469999,15.2,1.33384454499998));
#191791=CARTESIAN_POINT('Ctrl Pts',(10.3925622469999,11.6,1.33384454499998));
#191792=CARTESIAN_POINT('Ctrl Pts',(10.3909585599999,15.2,1.33390267699999));
#191793=CARTESIAN_POINT('Ctrl Pts',(10.3909585599999,11.6,1.33390267699998));
#191794=CARTESIAN_POINT('Ctrl Pts',(10.3893626899999,15.2,1.33395902399998));
#191795=CARTESIAN_POINT('Ctrl Pts',(10.3893626899999,11.6,1.33395902399998));
#191796=CARTESIAN_POINT('Ctrl Pts',(10.3877746539999,15.2,1.33401360099999));
#191797=CARTESIAN_POINT('Ctrl Pts',(10.3877746539999,11.6,1.33401360099999));
#191798=CARTESIAN_POINT('Ctrl Pts',(10.3861944729999,15.2,1.33406641899999));
#191799=CARTESIAN_POINT('Ctrl Pts',(10.3861944729999,11.6,1.33406641899999));
#191800=CARTESIAN_POINT('Ctrl Pts',(10.3846221649999,15.2,1.33411749199999));
#191801=CARTESIAN_POINT('Ctrl Pts',(10.3846221649999,11.6,1.33411749199999));
#191802=CARTESIAN_POINT('Ctrl Pts',(10.3830577499999,15.2,1.33416683399998));
#191803=CARTESIAN_POINT('Ctrl Pts',(10.3830577499999,11.6,1.33416683399998));
#191804=CARTESIAN_POINT('Ctrl Pts',(10.3815012489999,15.2,1.33421445799998));
#191805=CARTESIAN_POINT('Ctrl Pts',(10.3815012489999,11.6,1.33421445799998));
#191806=CARTESIAN_POINT('Ctrl Pts',(10.3799526789999,15.2,1.33426037599999));
#191807=CARTESIAN_POINT('Ctrl Pts',(10.3799526789999,11.6,1.33426037599999));
#191808=CARTESIAN_POINT('Ctrl Pts',(10.3784120619999,15.2,1.33430460199999));
#191809=CARTESIAN_POINT('Ctrl Pts',(10.3784120619999,11.6,1.33430460199999));
#191810=CARTESIAN_POINT('Ctrl Pts',(10.3768794159999,15.2,1.33434714999999));
#191811=CARTESIAN_POINT('Ctrl Pts',(10.3768794159999,11.6,1.33434714999999));
#191812=CARTESIAN_POINT('Ctrl Pts',(10.3753547629999,15.2,1.33438803399998));
#191813=CARTESIAN_POINT('Ctrl Pts',(10.3753547629999,11.6,1.33438803399998));
#191814=CARTESIAN_POINT('Ctrl Pts',(10.3738381209999,15.2,1.33442726599998));
#191815=CARTESIAN_POINT('Ctrl Pts',(10.3738381209999,11.6,1.33442726599998));
#191816=CARTESIAN_POINT('Ctrl Pts',(10.3723295099999,15.2,1.33446485899999));
#191817=CARTESIAN_POINT('Ctrl Pts',(10.3723295099999,11.6,1.33446485899999));
#191818=CARTESIAN_POINT('Ctrl Pts',(10.3708289509999,15.2,1.33450082899999));
#191819=CARTESIAN_POINT('Ctrl Pts',(10.3708289509999,11.6,1.33450082899999));
#191820=CARTESIAN_POINT('Ctrl Pts',(10.3693364639999,15.2,1.33453518899998));
#191821=CARTESIAN_POINT('Ctrl Pts',(10.3693364639999,11.6,1.33453518899998));
#191822=CARTESIAN_POINT('Ctrl Pts',(10.3678520689999,15.2,1.33456795199999));
#191823=CARTESIAN_POINT('Ctrl Pts',(10.3678520689999,11.6,1.33456795199998));
#191824=CARTESIAN_POINT('Ctrl Pts',(10.3663757859999,15.2,1.33459913299999));
#191825=CARTESIAN_POINT('Ctrl Pts',(10.3663757859999,11.6,1.33459913299998));
#191826=CARTESIAN_POINT('Ctrl Pts',(10.3649076359999,15.2,1.33462874399998));
#191827=CARTESIAN_POINT('Ctrl Pts',(10.3649076359999,11.6,1.33462874399998));
#191828=CARTESIAN_POINT('Ctrl Pts',(10.3634476389999,15.2,1.33465680099999));
#191829=CARTESIAN_POINT('Ctrl Pts',(10.3634476389999,11.6,1.33465680099999));
#191830=CARTESIAN_POINT('Ctrl Pts',(10.3619958159999,15.2,1.33468331699999));
#191831=CARTESIAN_POINT('Ctrl Pts',(10.3619958159999,11.6,1.33468331699999));
#191832=CARTESIAN_POINT('Ctrl Pts',(10.3605521859999,15.2,1.33470830799999));
#191833=CARTESIAN_POINT('Ctrl Pts',(10.3605521859999,11.6,1.33470830799999));
#191834=CARTESIAN_POINT('Ctrl Pts',(10.3591167719999,15.2,1.33473178499999));
#191835=CARTESIAN_POINT('Ctrl Pts',(10.3591167719999,11.6,1.33473178499999));
#191836=CARTESIAN_POINT('Ctrl Pts',(10.3576895929999,15.2,1.33475376599999));
#191837=CARTESIAN_POINT('Ctrl Pts',(10.3576895929999,11.6,1.33475376599998));
#191838=CARTESIAN_POINT('Ctrl Pts',(10.3562706699999,15.2,1.33477426199998));
#191839=CARTESIAN_POINT('Ctrl Pts',(10.3562706699999,11.6,1.33477426199998));
#191840=CARTESIAN_POINT('Ctrl Pts',(10.3548600249999,15.2,1.33479328899998));
#191841=CARTESIAN_POINT('Ctrl Pts',(10.3548600249999,11.6,1.33479328899998));
#191842=CARTESIAN_POINT('Ctrl Pts',(10.3534576789999,15.2,1.33481086299998));
#191843=CARTESIAN_POINT('Ctrl Pts',(10.3534576789999,11.6,1.33481086299998));
#191844=CARTESIAN_POINT('Ctrl Pts',(10.3520636509999,15.2,1.33482699499998));
#191845=CARTESIAN_POINT('Ctrl Pts',(10.3520636509999,11.6,1.33482699499998));
#191846=CARTESIAN_POINT('Ctrl Pts',(10.3506779649999,15.2,1.33484170199999));
#191847=CARTESIAN_POINT('Ctrl Pts',(10.3506779649999,11.6,1.33484170199999));
#191848=CARTESIAN_POINT('Ctrl Pts',(10.3493006389999,15.2,1.33485499899999));
#191849=CARTESIAN_POINT('Ctrl Pts',(10.3493006389999,11.6,1.33485499899999));
#191850=CARTESIAN_POINT('Ctrl Pts',(10.3479316969999,15.2,1.33486689999998));
#191851=CARTESIAN_POINT('Ctrl Pts',(10.3479316969999,11.6,1.33486689999998));
#191852=CARTESIAN_POINT('Ctrl Pts',(10.3465711599999,15.2,1.33487741899998));
#191853=CARTESIAN_POINT('Ctrl Pts',(10.3465711599999,11.6,1.33487741899998));
#191854=CARTESIAN_POINT('Ctrl Pts',(10.3452190479999,15.2,1.33488657399999));
#191855=CARTESIAN_POINT('Ctrl Pts',(10.3452190479999,11.6,1.33488657399999));
#191856=CARTESIAN_POINT('Ctrl Pts',(10.3438753839999,15.2,1.33489437599998));
#191857=CARTESIAN_POINT('Ctrl Pts',(10.3438753839999,11.6,1.33489437599998));
#191858=CARTESIAN_POINT('Ctrl Pts',(10.3425401889999,15.2,1.33490084399998));
#191859=CARTESIAN_POINT('Ctrl Pts',(10.3425401889999,11.6,1.33490084399998));
#191860=CARTESIAN_POINT('Ctrl Pts',(10.3412134849999,15.2,1.33490598999999));
#191861=CARTESIAN_POINT('Ctrl Pts',(10.3412134849999,11.6,1.33490598999999));
#191862=CARTESIAN_POINT('Ctrl Pts',(10.3398952939999,15.2,1.33490982999998));
#191863=CARTESIAN_POINT('Ctrl Pts',(10.3398952939999,11.6,1.33490982999998));
#191864=CARTESIAN_POINT('Ctrl Pts',(10.3385856379999,15.2,1.33491238099999));
#191865=CARTESIAN_POINT('Ctrl Pts',(10.3385856379999,11.6,1.33491238099999));
#191866=CARTESIAN_POINT('Ctrl Pts',(10.3372845369999,15.2,1.33491365699999));
#191867=CARTESIAN_POINT('Ctrl Pts',(10.3372845369999,11.6,1.33491365699998));
#191868=CARTESIAN_POINT('Ctrl Pts',(10.3359920159999,15.2,1.33491367299999));
#191869=CARTESIAN_POINT('Ctrl Pts',(10.3359920159999,11.6,1.33491367299999));
#191870=CARTESIAN_POINT('Ctrl Pts',(10.3347080959999,15.2,1.33491244599998));
#191871=CARTESIAN_POINT('Ctrl Pts',(10.3347080959999,11.6,1.33491244599998));
#191872=CARTESIAN_POINT('Ctrl Pts',(10.3334327989999,15.2,1.33490999099998));
#191873=CARTESIAN_POINT('Ctrl Pts',(10.3334327989999,11.6,1.33490999099998));
#191874=CARTESIAN_POINT('Ctrl Pts',(10.3321661469999,15.2,1.33490632399999));
#191875=CARTESIAN_POINT('Ctrl Pts',(10.3321661469999,11.6,1.33490632399999));
#191876=CARTESIAN_POINT('Ctrl Pts',(10.3309081639999,15.2,1.33490145999998));
#191877=CARTESIAN_POINT('Ctrl Pts',(10.3309081639999,11.6,1.33490145999998));
#191878=CARTESIAN_POINT('Ctrl Pts',(10.3296588699999,15.2,1.33489541599999));
#191879=CARTESIAN_POINT('Ctrl Pts',(10.3296588699999,11.6,1.33489541599999));
#191880=CARTESIAN_POINT('Ctrl Pts',(10.3284182899999,15.2,1.33488820699998));
#191881=CARTESIAN_POINT('Ctrl Pts',(10.3284182899999,11.6,1.33488820699998));
#191882=CARTESIAN_POINT('Ctrl Pts',(10.3271864459999,15.2,1.33487984899999));
#191883=CARTESIAN_POINT('Ctrl Pts',(10.3271864459999,11.6,1.33487984899999));
#191884=CARTESIAN_POINT('Ctrl Pts',(10.3259633609999,15.2,1.33487035899998));
#191885=CARTESIAN_POINT('Ctrl Pts',(10.3259633609999,11.6,1.33487035899998));
#191886=CARTESIAN_POINT('Ctrl Pts',(10.3247490569999,15.2,1.33485975299998));
#191887=CARTESIAN_POINT('Ctrl Pts',(10.3247490569999,11.6,1.33485975299998));
#191888=CARTESIAN_POINT('Ctrl Pts',(10.3235435579999,15.2,1.33484804699998));
#191889=CARTESIAN_POINT('Ctrl Pts',(10.3235435579999,11.6,1.33484804699998));
#191890=CARTESIAN_POINT('Ctrl Pts',(10.3223468859999,15.2,1.33483525699999));
#191891=CARTESIAN_POINT('Ctrl Pts',(10.3223468859999,11.6,1.33483525699999));
#191892=CARTESIAN_POINT('Ctrl Pts',(10.3211590649999,15.2,1.33482139999999));
#191893=CARTESIAN_POINT('Ctrl Pts',(10.3211590649999,11.6,1.33482139999999));
#191894=CARTESIAN_POINT('Ctrl Pts',(10.3199801189999,15.2,1.33480649299999));
#191895=CARTESIAN_POINT('Ctrl Pts',(10.3199801189999,11.6,1.33480649299999));
#191896=CARTESIAN_POINT('Ctrl Pts',(10.3188100709999,15.2,1.33479055299999));
#191897=CARTESIAN_POINT('Ctrl Pts',(10.3188100709999,11.6,1.33479055299999));
#191898=CARTESIAN_POINT('Ctrl Pts',(10.3176489429999,15.2,1.33477359499999));
#191899=CARTESIAN_POINT('Ctrl Pts',(10.3176489429999,11.6,1.33477359499999));
#191900=CARTESIAN_POINT('Ctrl Pts',(10.3164967599999,15.2,1.33475563599998));
#191901=CARTESIAN_POINT('Ctrl Pts',(10.3164967599999,11.6,1.33475563599998));
#191902=CARTESIAN_POINT('Ctrl Pts',(10.3153535459999,15.2,1.33473669599999));
#191903=CARTESIAN_POINT('Ctrl Pts',(10.3153535459999,11.6,1.33473669599998));
#191904=CARTESIAN_POINT('Ctrl Pts',(10.3142193239999,15.2,1.33471678699999));
#191905=CARTESIAN_POINT('Ctrl Pts',(10.3142193239999,11.6,1.33471678699998));
#191906=CARTESIAN_POINT('Ctrl Pts',(10.3130941179999,15.2,1.33469593099999));
#191907=CARTESIAN_POINT('Ctrl Pts',(10.3130941179999,11.6,1.33469593099999));
#191908=CARTESIAN_POINT('Ctrl Pts',(10.3119779519999,15.2,1.33467414199998));
#191909=CARTESIAN_POINT('Ctrl Pts',(10.3119779519999,11.6,1.33467414199998));
#191910=CARTESIAN_POINT('Ctrl Pts',(10.3108708509999,15.2,1.33465143799999));
#191911=CARTESIAN_POINT('Ctrl Pts',(10.3108708509999,11.6,1.33465143799999));
#191912=CARTESIAN_POINT('Ctrl Pts',(10.3097728379999,15.2,1.33462783699999));
#191913=CARTESIAN_POINT('Ctrl Pts',(10.3097728379999,11.6,1.33462783699999));
#191914=CARTESIAN_POINT('Ctrl Pts',(10.3086839379999,15.2,1.33460335699999));
#191915=CARTESIAN_POINT('Ctrl Pts',(10.3086839379999,11.6,1.33460335699999));
#191916=CARTESIAN_POINT('Ctrl Pts',(10.3076041749999,15.2,1.33457801399999));
#191917=CARTESIAN_POINT('Ctrl Pts',(10.3076041749999,11.6,1.33457801399999));
#191918=CARTESIAN_POINT('Ctrl Pts',(10.3065335739999,15.2,1.33455182699999));
#191919=CARTESIAN_POINT('Ctrl Pts',(10.3065335739999,11.6,1.33455182699999));
#191920=CARTESIAN_POINT('Ctrl Pts',(10.3054721599999,15.2,1.33452481299999));
#191921=CARTESIAN_POINT('Ctrl Pts',(10.3054721599999,11.6,1.33452481299999));
#191922=CARTESIAN_POINT('Ctrl Pts',(10.3044199559999,15.2,1.33449698899998));
#191923=CARTESIAN_POINT('Ctrl Pts',(10.3044199559999,11.6,1.33449698899998));
#191924=CARTESIAN_POINT('Ctrl Pts',(10.3033769899999,15.2,1.33446837399998));
#191925=CARTESIAN_POINT('Ctrl Pts',(10.3033769899999,11.6,1.33446837399998));
#191926=CARTESIAN_POINT('Ctrl Pts',(10.3023432839999,15.2,1.33443898699999));
#191927=CARTESIAN_POINT('Ctrl Pts',(10.3023432839999,11.6,1.33443898699999));
#191928=CARTESIAN_POINT('Ctrl Pts',(10.3013188639999,15.2,1.33440884399999));
#191929=CARTESIAN_POINT('Ctrl Pts',(10.3013188639999,11.6,1.33440884399999));
#191930=CARTESIAN_POINT('Ctrl Pts',(10.3003037569999,15.2,1.33437796599999));
#191931=CARTESIAN_POINT('Ctrl Pts',(10.3003037569999,11.6,1.33437796599999));
#191932=CARTESIAN_POINT('Ctrl Pts',(10.2992979849999,15.2,1.33434636899999));
#191933=CARTESIAN_POINT('Ctrl Pts',(10.2992979849999,11.6,1.33434636899999));
#191934=CARTESIAN_POINT('Ctrl Pts',(10.2983015759999,15.2,1.33431407099998));
#191935=CARTESIAN_POINT('Ctrl Pts',(10.2983015759999,11.6,1.33431407099998));
#191936=CARTESIAN_POINT('Ctrl Pts',(10.2973145539999,15.2,1.33428109299999));
#191937=CARTESIAN_POINT('Ctrl Pts',(10.2973145539999,11.6,1.33428109299999));
#191938=CARTESIAN_POINT('Ctrl Pts',(10.2963369469999,15.2,1.33424745299998));
#191939=CARTESIAN_POINT('Ctrl Pts',(10.2963369469999,11.6,1.33424745299998));
#191940=CARTESIAN_POINT('Ctrl Pts',(10.2953687779999,15.2,1.33421316799998));
#191941=CARTESIAN_POINT('Ctrl Pts',(10.2953687779999,11.6,1.33421316799998));
#191942=CARTESIAN_POINT('Ctrl Pts',(10.2944100739999,15.2,1.33417825799999));
#191943=CARTESIAN_POINT('Ctrl Pts',(10.2944100739999,11.6,1.33417825799999));
#191944=CARTESIAN_POINT('Ctrl Pts',(10.2934608629999,15.2,1.33414274199998));
#191945=CARTESIAN_POINT('Ctrl Pts',(10.2934608629999,11.6,1.33414274199998));
#191946=CARTESIAN_POINT('Ctrl Pts',(10.2925211679999,15.2,1.33410663999999));
#191947=CARTESIAN_POINT('Ctrl Pts',(10.2925211679999,11.6,1.33410663999999));
#191948=CARTESIAN_POINT('Ctrl Pts',(10.2915910169999,15.2,1.33406996999998));
#191949=CARTESIAN_POINT('Ctrl Pts',(10.2915910169999,11.6,1.33406996999998));
#191950=CARTESIAN_POINT('Ctrl Pts',(10.2906757369999,15.2,1.33403296599999));
#191951=CARTESIAN_POINT('Ctrl Pts',(10.2906757369999,11.6,1.33403296599999));
#191952=CARTESIAN_POINT('Ctrl Pts',(10.2899521419999,15.2,1.33400298799998));
#191953=CARTESIAN_POINT('Ctrl Pts',(10.2899521419999,11.6,1.33400298799998));
#191954=CARTESIAN_POINT('Ctrl Pts',(10.2894150039999,15.2,1.33398033399999));
#191955=CARTESIAN_POINT('Ctrl Pts',(10.2894150039999,11.6,1.33398033399999));
#191956=CARTESIAN_POINT('Ctrl Pts',(10.2890605209999,15.2,1.33396520799999));
#191957=CARTESIAN_POINT('Ctrl Pts',(10.2890605209999,11.6,1.33396520799998));
#191958=CARTESIAN_POINT('Ctrl Pts',(10.2888863229999,15.2,1.33395773199998));
#191959=CARTESIAN_POINT('Ctrl Pts',(10.2888863229999,11.6,1.33395773199998));
#191960=CARTESIAN_POINT('',(10.2888863229999,12.2,1.33395773199998));
#191961=CARTESIAN_POINT('',(10.2888863229999,15.2,1.33395773199998));
#191962=CARTESIAN_POINT('',(10.2888863229999,12.2,1.33395773199998));
#191963=CARTESIAN_POINT('Ctrl Pts',(11.4479048649999,12.2,1.09337742899998));
#191964=CARTESIAN_POINT('Ctrl Pts',(11.4471888789999,12.2,1.09364567099998));
#191965=CARTESIAN_POINT('Ctrl Pts',(11.4457572179999,12.2,1.09418172899999));
#191966=CARTESIAN_POINT('Ctrl Pts',(11.4436106639999,12.2,1.09498454299999));
#191967=CARTESIAN_POINT('Ctrl Pts',(11.4407504639999,12.2,1.09605241699999));
#191968=CARTESIAN_POINT('Ctrl Pts',(11.4371783349999,12.2,1.09738301699998));
#191969=CARTESIAN_POINT('Ctrl Pts',(11.4336093279999,12.2,1.09870937299998));
#191970=CARTESIAN_POINT('Ctrl Pts',(11.4300434449999,12.2,1.10003148899999));
#191971=CARTESIAN_POINT('Ctrl Pts',(11.4264806909999,12.2,1.10134936399998));
#191972=CARTESIAN_POINT('Ctrl Pts',(11.4229210689999,12.2,1.10266299899999));
#191973=CARTESIAN_POINT('Ctrl Pts',(11.4193645909999,12.2,1.10397239899998));
#191974=CARTESIAN_POINT('Ctrl Pts',(11.4158112619999,12.2,1.10527756499998));
#191975=CARTESIAN_POINT('Ctrl Pts',(11.4122610939999,12.2,1.10657849999999));
#191976=CARTESIAN_POINT('Ctrl Pts',(11.4087140989999,12.2,1.10787520999999));
#191977=CARTESIAN_POINT('Ctrl Pts',(11.4051702859999,12.2,1.10916769599998));
#191978=CARTESIAN_POINT('Ctrl Pts',(11.4016296639999,12.2,1.11045596299999));
#191979=CARTESIAN_POINT('Ctrl Pts',(11.3980922449999,12.2,1.11174001299998));
#191980=CARTESIAN_POINT('Ctrl Pts',(11.3945580339999,12.2,1.11301984899999));
#191981=CARTESIAN_POINT('Ctrl Pts',(11.3910270409999,12.2,1.11429547399998));
#191982=CARTESIAN_POINT('Ctrl Pts',(11.3874992709999,12.2,1.11556689099999));
#191983=CARTESIAN_POINT('Ctrl Pts',(11.3839747349999,12.2,1.11683410099999));
#191984=CARTESIAN_POINT('Ctrl Pts',(11.3804534399999,12.2,1.11809710599998));
#191985=CARTESIAN_POINT('Ctrl Pts',(11.3769353939999,12.2,1.11935591199999));
#191986=CARTESIAN_POINT('Ctrl Pts',(11.3734206059999,12.2,1.12061051999999));
#191987=CARTESIAN_POINT('Ctrl Pts',(11.3699090849999,12.2,1.12186093299998));
#191988=CARTESIAN_POINT('Ctrl Pts',(11.3664008399999,12.2,1.12310715499999));
#191989=CARTESIAN_POINT('Ctrl Pts',(11.3628958789999,12.2,1.12434918799998));
#191990=CARTESIAN_POINT('Ctrl Pts',(11.3593942139999,12.2,1.12558703499999));
#191991=CARTESIAN_POINT('Ctrl Pts',(11.3558958509999,12.2,1.12682069999999));
#191992=CARTESIAN_POINT('Ctrl Pts',(11.3524007989999,12.2,1.12805018499999));
#191993=CARTESIAN_POINT('Ctrl Pts',(11.3489090669999,12.2,1.12927549499998));
#191994=CARTESIAN_POINT('Ctrl Pts',(11.3454206639999,12.2,1.13049662999999));
#191995=CARTESIAN_POINT('Ctrl Pts',(11.3419355979999,12.2,1.13171359399999));
#191996=CARTESIAN_POINT('Ctrl Pts',(11.3384538779999,12.2,1.13292639099999));
#191997=CARTESIAN_POINT('Ctrl Pts',(11.3349755119999,12.2,1.13413502399998));
#191998=CARTESIAN_POINT('Ctrl Pts',(11.3315005099999,12.2,1.13533949399999));
#191999=CARTESIAN_POINT('Ctrl Pts',(11.3280288789999,12.2,1.13653980499999));
#192000=CARTESIAN_POINT('Ctrl Pts',(11.3245606299999,12.2,1.13773596199998));
#192001=CARTESIAN_POINT('Ctrl Pts',(11.3210957719999,12.2,1.13892796799998));
#192002=CARTESIAN_POINT('Ctrl Pts',(11.3176343119999,12.2,1.14011582299999));
#192003=CARTESIAN_POINT('Ctrl Pts',(11.3141762599999,12.2,1.14129953199999));
#192004=CARTESIAN_POINT('Ctrl Pts',(11.3107216239999,12.2,1.14247909899999));
#192005=CARTESIAN_POINT('Ctrl Pts',(11.3072704139999,12.2,1.14365452599999));
#192006=CARTESIAN_POINT('Ctrl Pts',(11.3038226389999,12.2,1.14482581599999));
#192007=CARTESIAN_POINT('Ctrl Pts',(11.3003783059999,12.2,1.14599297299999));
#192008=CARTESIAN_POINT('Ctrl Pts',(11.2969374249999,12.2,1.14715599999998));
#192009=CARTESIAN_POINT('Ctrl Pts',(11.2935000059999,12.2,1.14831489899998));
#192010=CARTESIAN_POINT('Ctrl Pts',(11.2900660559999,12.2,1.14946967499999));
#192011=CARTESIAN_POINT('Ctrl Pts',(11.2866355859999,12.2,1.15062032999999));
#192012=CARTESIAN_POINT('Ctrl Pts',(11.2832086039999,12.2,1.15176686799999));
#192013=CARTESIAN_POINT('Ctrl Pts',(11.2797851169999,12.2,1.15290929199999));
#192014=CARTESIAN_POINT('Ctrl Pts',(11.2763651379999,12.2,1.15404760499999));
#192015=CARTESIAN_POINT('Ctrl Pts',(11.2729486729999,12.2,1.15518180999999));
#192016=CARTESIAN_POINT('Ctrl Pts',(11.2695357319999,12.2,1.15631191099999));
#192017=CARTESIAN_POINT('Ctrl Pts',(11.2661263239999,12.2,1.15743791099999));
#192018=CARTESIAN_POINT('Ctrl Pts',(11.2627204589999,12.2,1.15855981299998));
#192019=CARTESIAN_POINT('Ctrl Pts',(11.2593181439999,12.2,1.15967762199999));
#192020=CARTESIAN_POINT('Ctrl Pts',(11.2559193889999,12.2,1.16079133899999));
#192021=CARTESIAN_POINT('Ctrl Pts',(11.2525242039999,12.2,1.16190096799999));
#192022=CARTESIAN_POINT('Ctrl Pts',(11.2491325969999,12.2,1.16300651299999));
#192023=CARTESIAN_POINT('Ctrl Pts',(11.2457445769999,12.2,1.16410797799999));
#192024=CARTESIAN_POINT('Ctrl Pts',(11.2423601539999,12.2,1.16520536499999));
#192025=CARTESIAN_POINT('Ctrl Pts',(11.2389793369999,12.2,1.16629867799999));
#192026=CARTESIAN_POINT('Ctrl Pts',(11.2356021349999,12.2,1.16738791999999));
#192027=CARTESIAN_POINT('Ctrl Pts',(11.2322285569999,12.2,1.16847309399999));
#192028=CARTESIAN_POINT('Ctrl Pts',(11.2288586119999,12.2,1.16955420599998));
#192029=CARTESIAN_POINT('Ctrl Pts',(11.2254923089999,12.2,1.17063125699998));
#192030=CARTESIAN_POINT('Ctrl Pts',(11.2221296589999,12.2,1.17170425099999));
#192031=CARTESIAN_POINT('Ctrl Pts',(11.2187706689999,12.2,1.17277319199999));
#192032=CARTESIAN_POINT('Ctrl Pts',(11.2154153489999,12.2,1.17383808299998));
#192033=CARTESIAN_POINT('Ctrl Pts',(11.2120637079999,12.2,1.17489892799998));
#192034=CARTESIAN_POINT('Ctrl Pts',(11.2087157559999,12.2,1.17595572999999));
#192035=CARTESIAN_POINT('Ctrl Pts',(11.2053715019999,12.2,1.17700849199998));
#192036=CARTESIAN_POINT('Ctrl Pts',(11.2020309559999,12.2,1.17805721999999));
#192037=CARTESIAN_POINT('Ctrl Pts',(11.1986941249999,12.2,1.17910191499998));
#192038=CARTESIAN_POINT('Ctrl Pts',(11.1953610209999,12.2,1.18014258099999));
#192039=CARTESIAN_POINT('Ctrl Pts',(11.1920316519999,12.2,1.18117922199998));
#192040=CARTESIAN_POINT('Ctrl Pts',(11.1887060269999,12.2,1.18221184299999));
#192041=CARTESIAN_POINT('Ctrl Pts',(11.1853841569999,12.2,1.18324044599999));
#192042=CARTESIAN_POINT('Ctrl Pts',(11.1820660499999,12.2,1.18426503499999));
#192043=CARTESIAN_POINT('Ctrl Pts',(11.1787517149999,12.2,1.18528561399998));
#192044=CARTESIAN_POINT('Ctrl Pts',(11.1754411629999,12.2,1.18630218499999));
#192045=CARTESIAN_POINT('Ctrl Pts',(11.1721344009999,12.2,1.18731475499999));
#192046=CARTESIAN_POINT('Ctrl Pts',(11.1688314409999,12.2,1.18832332399998));
#192047=CARTESIAN_POINT('Ctrl Pts',(11.1655322919999,12.2,1.18932789899999));
#192048=CARTESIAN_POINT('Ctrl Pts',(11.1622369629999,12.2,1.19032848099998));
#192049=CARTESIAN_POINT('Ctrl Pts',(11.1589454619999,12.2,1.19132507599998));
#192050=CARTESIAN_POINT('Ctrl Pts',(11.1556577999999,12.2,1.19231768599999));
#192051=CARTESIAN_POINT('Ctrl Pts',(11.1523739879999,12.2,1.19330631599999));
#192052=CARTESIAN_POINT('Ctrl Pts',(11.1490940329999,12.2,1.19429096899998));
#192053=CARTESIAN_POINT('Ctrl Pts',(11.1458179459999,12.2,1.19527164899999));
#192054=CARTESIAN_POINT('Ctrl Pts',(11.1425457349999,12.2,1.19624835999999));
#192055=CARTESIAN_POINT('Ctrl Pts',(11.1392774109999,12.2,1.19722110599998));
#192056=CARTESIAN_POINT('Ctrl Pts',(11.1360129839999,12.2,1.19818988999999));
#192057=CARTESIAN_POINT('Ctrl Pts',(11.1327524619999,12.2,1.19915471699999));
#192058=CARTESIAN_POINT('Ctrl Pts',(11.1294958549999,12.2,1.20011559099999));
#192059=CARTESIAN_POINT('Ctrl Pts',(11.1262431739999,12.2,1.20107251499999));
#192060=CARTESIAN_POINT('Ctrl Pts',(11.1229944269999,12.2,1.20202549299998));
#192061=CARTESIAN_POINT('Ctrl Pts',(11.1197496249999,12.2,1.20297452899999));
#192062=CARTESIAN_POINT('Ctrl Pts',(11.1165087779999,12.2,1.20391962699999));
#192063=CARTESIAN_POINT('Ctrl Pts',(11.1132718939999,12.2,1.20486079099999));
#192064=CARTESIAN_POINT('Ctrl Pts',(11.1100389819999,12.2,1.20579802499998));
#192065=CARTESIAN_POINT('Ctrl Pts',(11.1068100549999,12.2,1.20673133399999));
#192066=CARTESIAN_POINT('Ctrl Pts',(11.1035851209999,12.2,1.20766071999999));
#192067=CARTESIAN_POINT('Ctrl Pts',(11.1003641889999,12.2,1.20858618799998));
#192068=CARTESIAN_POINT('Ctrl Pts',(11.0971472699999,12.2,1.20950774199999));
#192069=CARTESIAN_POINT('Ctrl Pts',(11.0939343729999,12.2,1.21042538699998));
#192070=CARTESIAN_POINT('Ctrl Pts',(11.0907255089999,12.2,1.21133912599999));
#192071=CARTESIAN_POINT('Ctrl Pts',(11.0875206859999,12.2,1.21224896199998));
#192072=CARTESIAN_POINT('Ctrl Pts',(11.0843199139999,12.2,1.21315490199999));
#192073=CARTESIAN_POINT('Ctrl Pts',(11.0811232049999,12.2,1.21405694799999));
#192074=CARTESIAN_POINT('Ctrl Pts',(11.0779305669999,12.2,1.21495510399999));
#192075=CARTESIAN_POINT('Ctrl Pts',(11.0747420099999,12.2,1.21584937499998));
#192076=CARTESIAN_POINT('Ctrl Pts',(11.0715575449999,12.2,1.21673976599999));
#192077=CARTESIAN_POINT('Ctrl Pts',(11.0683771819999,12.2,1.21762627999999));
#192078=CARTESIAN_POINT('Ctrl Pts',(11.0652009289999,12.2,1.21850892099999));
#192079=CARTESIAN_POINT('Ctrl Pts',(11.0620287979999,12.2,1.21938769199998));
#192080=CARTESIAN_POINT('Ctrl Pts',(11.0588607969999,12.2,1.22026260099998));
#192081=CARTESIAN_POINT('Ctrl Pts',(11.0556969379999,12.2,1.22113364899999));
#192082=CARTESIAN_POINT('Ctrl Pts',(11.0525372299999,12.2,1.22200084099998));
#192083=CARTESIAN_POINT('Ctrl Pts',(11.0493816829999,12.2,1.22286418199999));
#192084=CARTESIAN_POINT('Ctrl Pts',(11.0462303079999,12.2,1.22372367599999));
#192085=CARTESIAN_POINT('Ctrl Pts',(11.0430831139999,12.2,1.22457932799998));
#192086=CARTESIAN_POINT('Ctrl Pts',(11.0399401109999,12.2,1.22543113999999));
#192087=CARTESIAN_POINT('Ctrl Pts',(11.0368013089999,12.2,1.22627911899999));
#192088=CARTESIAN_POINT('Ctrl Pts',(11.0336667189999,12.2,1.22712326699999));
#192089=CARTESIAN_POINT('Ctrl Pts',(11.0305363499999,12.2,1.22796359099999));
#192090=CARTESIAN_POINT('Ctrl Pts',(11.0274102129999,12.2,1.22880009299998));
#192091=CARTESIAN_POINT('Ctrl Pts',(11.0242883189999,12.2,1.22963277999999));
#192092=CARTESIAN_POINT('Ctrl Pts',(11.0211706759999,12.2,1.23046165299999));
#192093=CARTESIAN_POINT('Ctrl Pts',(11.0180572959999,12.2,1.23128671899998));
#192094=CARTESIAN_POINT('Ctrl Pts',(11.0149481889999,12.2,1.23210798199999));
#192095=CARTESIAN_POINT('Ctrl Pts',(11.0118433639999,12.2,1.23292544599999));
#192096=CARTESIAN_POINT('Ctrl Pts',(11.0087428319999,12.2,1.23373911599999));
#192097=CARTESIAN_POINT('Ctrl Pts',(11.0056466049999,12.2,1.23454899599999));
#192098=CARTESIAN_POINT('Ctrl Pts',(11.0025546899999,12.2,1.23535509099999));
#192099=CARTESIAN_POINT('Ctrl Pts',(10.9994670979999,12.2,1.23615740499998));
#192100=CARTESIAN_POINT('Ctrl Pts',(10.9963838419999,12.2,1.23695594399999));
#192101=CARTESIAN_POINT('Ctrl Pts',(10.9933049299999,12.2,1.23775071099999));
#192102=CARTESIAN_POINT('Ctrl Pts',(10.9902303719999,12.2,1.23854171099998));
#192103=CARTESIAN_POINT('Ctrl Pts',(10.9871601809999,12.2,1.23932894899998));
#192104=CARTESIAN_POINT('Ctrl Pts',(10.9840943639999,12.2,1.24011242999998));
#192105=CARTESIAN_POINT('Ctrl Pts',(10.9810329339999,12.2,1.24089215599998));
#192106=CARTESIAN_POINT('Ctrl Pts',(10.9779759009999,12.2,1.24166813599999));
#192107=CARTESIAN_POINT('Ctrl Pts',(10.9749232749999,12.2,1.24244037199999));
#192108=CARTESIAN_POINT('Ctrl Pts',(10.9718750649999,12.2,1.24320886799998));
#192109=CARTESIAN_POINT('Ctrl Pts',(10.9688312839999,12.2,1.24397363099999));
#192110=CARTESIAN_POINT('Ctrl Pts',(10.9657919419999,12.2,1.24473466399999));
#192111=CARTESIAN_POINT('Ctrl Pts',(10.9627570469999,12.2,1.24549197299999));
#192112=CARTESIAN_POINT('Ctrl Pts',(10.9597266129999,12.2,1.24624556199999));
#192113=CARTESIAN_POINT('Ctrl Pts',(10.9567006489999,12.2,1.24699543599998));
#192114=CARTESIAN_POINT('Ctrl Pts',(10.9536791659999,12.2,1.24774160099999));
#192115=CARTESIAN_POINT('Ctrl Pts',(10.9506621729999,12.2,1.24848405899999));
#192116=CARTESIAN_POINT('Ctrl Pts',(10.9476496829999,12.2,1.24922281699998));
#192117=CARTESIAN_POINT('Ctrl Pts',(10.9446417049999,12.2,1.24995787999998));
#192118=CARTESIAN_POINT('Ctrl Pts',(10.9416382509999,12.2,1.25068925199999));
#192119=CARTESIAN_POINT('Ctrl Pts',(10.9386393289999,12.2,1.25141693899999));
#192120=CARTESIAN_POINT('Ctrl Pts',(10.9356449539999,12.2,1.25214094399999));
#192121=CARTESIAN_POINT('Ctrl Pts',(10.9326551319999,12.2,1.25286127399999));
#192122=CARTESIAN_POINT('Ctrl Pts',(10.9296698779999,12.2,1.25357793199999));
#192123=CARTESIAN_POINT('Ctrl Pts',(10.9266891999999,12.2,1.25429092499999));
#192124=CARTESIAN_POINT('Ctrl Pts',(10.9237131089999,12.2,1.25500025699999));
#192125=CARTESIAN_POINT('Ctrl Pts',(10.9207416159999,12.2,1.25570593399999));
#192126=CARTESIAN_POINT('Ctrl Pts',(10.9177747329999,12.2,1.25640795999999));
#192127=CARTESIAN_POINT('Ctrl Pts',(10.9148124699999,12.2,1.25710633999998));
#192128=CARTESIAN_POINT('Ctrl Pts',(10.9118548369999,12.2,1.25780107899998));
#192129=CARTESIAN_POINT('Ctrl Pts',(10.9089018469999,12.2,1.25849218299999));
#192130=CARTESIAN_POINT('Ctrl Pts',(10.9059535079999,12.2,1.25917965599998));
#192131=CARTESIAN_POINT('Ctrl Pts',(10.9030098339999,12.2,1.25986350499999));
#192132=CARTESIAN_POINT('Ctrl Pts',(10.9000708339999,12.2,1.26054373299999));
#192133=CARTESIAN_POINT('Ctrl Pts',(10.8971365199999,12.2,1.26122034599998));
#192134=CARTESIAN_POINT('Ctrl Pts',(10.8942069009999,12.2,1.26189335099999));
#192135=CARTESIAN_POINT('Ctrl Pts',(10.8912819899999,12.2,1.26256274999998));
#192136=CARTESIAN_POINT('Ctrl Pts',(10.8883617979999,12.2,1.26322854999998));
#192137=CARTESIAN_POINT('Ctrl Pts',(10.8854463339999,12.2,1.26389075699999));
#192138=CARTESIAN_POINT('Ctrl Pts',(10.8825356119999,12.2,1.26454937599998));
#192139=CARTESIAN_POINT('Ctrl Pts',(10.8796296409999,12.2,1.26520441099998));
#192140=CARTESIAN_POINT('Ctrl Pts',(10.8767284329999,12.2,1.26585586799999));
#192141=CARTESIAN_POINT('Ctrl Pts',(10.8738319979999,12.2,1.26650375199999));
#192142=CARTESIAN_POINT('Ctrl Pts',(10.8709403489999,12.2,1.26714806999999));
#192143=CARTESIAN_POINT('Ctrl Pts',(10.8680534959999,12.2,1.26778882499998));
#192144=CARTESIAN_POINT('Ctrl Pts',(10.8651714489999,12.2,1.26842602399998));
#192145=CARTESIAN_POINT('Ctrl Pts',(10.8622942209999,12.2,1.26905967299999));
#192146=CARTESIAN_POINT('Ctrl Pts',(10.8594218239999,12.2,1.26968977599998));
#192147=CARTESIAN_POINT('Ctrl Pts',(10.8565542679999,12.2,1.27031633899998));
#192148=CARTESIAN_POINT('Ctrl Pts',(10.8536915629999,12.2,1.27093936699998));
#192149=CARTESIAN_POINT('Ctrl Pts',(10.8508337229999,12.2,1.27155886699999));
#192150=CARTESIAN_POINT('Ctrl Pts',(10.8479807569999,12.2,1.27217484299999));
#192151=CARTESIAN_POINT('Ctrl Pts',(10.8451326779999,12.2,1.27278730199999));
#192152=CARTESIAN_POINT('Ctrl Pts',(10.8422894959999,12.2,1.27339624799998));
#192153=CARTESIAN_POINT('Ctrl Pts',(10.8394512219999,12.2,1.27400168799999));
#192154=CARTESIAN_POINT('Ctrl Pts',(10.8366178699999,12.2,1.27460362699999));
#192155=CARTESIAN_POINT('Ctrl Pts',(10.8337894499999,12.2,1.27520206999999));
#192156=CARTESIAN_POINT('Ctrl Pts',(10.8309659719999,12.2,1.27579702399998));
#192157=CARTESIAN_POINT('Ctrl Pts',(10.8281474499999,12.2,1.27638849299998));
#192158=CARTESIAN_POINT('Ctrl Pts',(10.8253338939999,12.2,1.27697648499999));
#192159=CARTESIAN_POINT('Ctrl Pts',(10.8225253159999,12.2,1.27756100399999));
#192160=CARTESIAN_POINT('Ctrl Pts',(10.8197217269999,12.2,1.27814205699998));
#192161=CARTESIAN_POINT('Ctrl Pts',(10.8169231379999,12.2,1.27871964799999));
#192162=CARTESIAN_POINT('Ctrl Pts',(10.8141295629999,12.2,1.27929378499998));
#192163=CARTESIAN_POINT('Ctrl Pts',(10.8113410119999,12.2,1.27986447199998));
#192164=CARTESIAN_POINT('Ctrl Pts',(10.8085574969999,12.2,1.28043171599999));
#192165=CARTESIAN_POINT('Ctrl Pts',(10.8057790279999,12.2,1.28099552199998));
#192166=CARTESIAN_POINT('Ctrl Pts',(10.8030056189999,12.2,1.28155589599999));
#192167=CARTESIAN_POINT('Ctrl Pts',(10.8002372809999,12.2,1.28211284599999));
#192168=CARTESIAN_POINT('Ctrl Pts',(10.7974740259999,12.2,1.28266637499999));
#192169=CARTESIAN_POINT('Ctrl Pts',(10.7947158649999,12.2,1.28321648999998));
#192170=CARTESIAN_POINT('Ctrl Pts',(10.7919628099999,12.2,1.28376319699999));
#192171=CARTESIAN_POINT('Ctrl Pts',(10.7892148729999,12.2,1.28430650299999));
#192172=CARTESIAN_POINT('Ctrl Pts',(10.7864720659999,12.2,1.28484641299998));
#192173=CARTESIAN_POINT('Ctrl Pts',(10.7837344009999,12.2,1.28538293399998));
#192174=CARTESIAN_POINT('Ctrl Pts',(10.7810018879999,12.2,1.28591607099999));
#192175=CARTESIAN_POINT('Ctrl Pts',(10.7782745419999,12.2,1.28644583099998));
#192176=CARTESIAN_POINT('Ctrl Pts',(10.7755523729999,12.2,1.28697221799999));
#192177=CARTESIAN_POINT('Ctrl Pts',(10.7728353919999,12.2,1.28749524099999));
#192178=CARTESIAN_POINT('Ctrl Pts',(10.7701236149999,12.2,1.28801490499999));
#192179=CARTESIAN_POINT('Ctrl Pts',(10.7674170489999,12.2,1.28853121599999));
#192180=CARTESIAN_POINT('Ctrl Pts',(10.7647157089999,12.2,1.28904418099999));
#192181=CARTESIAN_POINT('Ctrl Pts',(10.7620196059999,12.2,1.28955380499999));
#192182=CARTESIAN_POINT('Ctrl Pts',(10.7593287539999,12.2,1.29006009499999));
#192183=CARTESIAN_POINT('Ctrl Pts',(10.7566431619999,12.2,1.29056305799998));
#192184=CARTESIAN_POINT('Ctrl Pts',(10.7539628449999,12.2,1.29106269999999));
#192185=CARTESIAN_POINT('Ctrl Pts',(10.7512878129999,12.2,1.29155902599999));
#192186=CARTESIAN_POINT('Ctrl Pts',(10.7486180789999,12.2,1.29205204399998));
#192187=CARTESIAN_POINT('Ctrl Pts',(10.7459536549999,12.2,1.29254175999999));
#192188=CARTESIAN_POINT('Ctrl Pts',(10.7432945539999,12.2,1.29302817899998));
#192189=CARTESIAN_POINT('Ctrl Pts',(10.7406407879999,12.2,1.29351130999999));
#192190=CARTESIAN_POINT('Ctrl Pts',(10.7379923689999,12.2,1.29399115799998));
#192191=CARTESIAN_POINT('Ctrl Pts',(10.7353493089999,12.2,1.29446772899998));
#192192=CARTESIAN_POINT('Ctrl Pts',(10.7327116219999,12.2,1.29494102999999));
#192193=CARTESIAN_POINT('Ctrl Pts',(10.7300793179999,12.2,1.29541106899998));
#192194=CARTESIAN_POINT('Ctrl Pts',(10.7274524109999,12.2,1.29587785099998));
#192195=CARTESIAN_POINT('Ctrl Pts',(10.7248309119999,12.2,1.29634138299998));
#192196=CARTESIAN_POINT('Ctrl Pts',(10.7222148359999,12.2,1.29680166999998));
#192197=CARTESIAN_POINT('Ctrl Pts',(10.7196041929999,12.2,1.29725872299999));
#192198=CARTESIAN_POINT('Ctrl Pts',(10.7169989959999,12.2,1.29771254499999));
#192199=CARTESIAN_POINT('Ctrl Pts',(10.7143992589999,12.2,1.29816314299998));
#192200=CARTESIAN_POINT('Ctrl Pts',(10.7118049929999,12.2,1.29861052499999));
#192201=CARTESIAN_POINT('Ctrl Pts',(10.7092162099999,12.2,1.29905469699999));
#192202=CARTESIAN_POINT('Ctrl Pts',(10.7066329249999,12.2,1.29949566599999));
#192203=CARTESIAN_POINT('Ctrl Pts',(10.7040551489999,12.2,1.29993343899999));
#192204=CARTESIAN_POINT('Ctrl Pts',(10.7014828959999,12.2,1.30036802199998));
#192205=CARTESIAN_POINT('Ctrl Pts',(10.6989161759999,12.2,1.30079942299998));
#192206=CARTESIAN_POINT('Ctrl Pts',(10.6963550049999,12.2,1.30122764799999));
#192207=CARTESIAN_POINT('Ctrl Pts',(10.6937993929999,12.2,1.30165270599999));
#192208=CARTESIAN_POINT('Ctrl Pts',(10.6912493539999,12.2,1.30207460099999));
#192209=CARTESIAN_POINT('Ctrl Pts',(10.6887049019999,12.2,1.30249334199998));
#192210=CARTESIAN_POINT('Ctrl Pts',(10.6861660479999,12.2,1.30290893499998));
#192211=CARTESIAN_POINT('Ctrl Pts',(10.6836328059999,12.2,1.30332138799998));
#192212=CARTESIAN_POINT('Ctrl Pts',(10.6811051889999,12.2,1.30373070699998));
#192213=CARTESIAN_POINT('Ctrl Pts',(10.6785832079999,12.2,1.30413689899999));
#192214=CARTESIAN_POINT('Ctrl Pts',(10.6760668779999,12.2,1.30453997299998));
#192215=CARTESIAN_POINT('Ctrl Pts',(10.6735562119999,12.2,1.30493993399998));
#192216=CARTESIAN_POINT('Ctrl Pts',(10.6710512209999,12.2,1.30533679099999));
#192217=CARTESIAN_POINT('Ctrl Pts',(10.6685519209999,12.2,1.30573054999998));
#192218=CARTESIAN_POINT('Ctrl Pts',(10.6660583229999,12.2,1.30612121799999));
#192219=CARTESIAN_POINT('Ctrl Pts',(10.6635704409999,12.2,1.30650880399998));
#192220=CARTESIAN_POINT('Ctrl Pts',(10.6610882879999,12.2,1.30689331299998));
#192221=CARTESIAN_POINT('Ctrl Pts',(10.6586118759999,12.2,1.30727475299999));
#192222=CARTESIAN_POINT('Ctrl Pts',(10.6561412199999,12.2,1.30765313299999));
#192223=CARTESIAN_POINT('Ctrl Pts',(10.6536763329999,12.2,1.30802845899999));
#192224=CARTESIAN_POINT('Ctrl Pts',(10.6512172259999,12.2,1.30840073799999));
#192225=CARTESIAN_POINT('Ctrl Pts',(10.6487639159999,12.2,1.30876997899998));
#192226=CARTESIAN_POINT('Ctrl Pts',(10.6463164129999,12.2,1.30913618899998));
#192227=CARTESIAN_POINT('Ctrl Pts',(10.6438747329999,12.2,1.30949937399999));
#192228=CARTESIAN_POINT('Ctrl Pts',(10.6414388879999,12.2,1.30985954199998));
#192229=CARTESIAN_POINT('Ctrl Pts',(10.6390088909999,12.2,1.31021670299999));
#192230=CARTESIAN_POINT('Ctrl Pts',(10.6365847569999,12.2,1.31057086099998));
#192231=CARTESIAN_POINT('Ctrl Pts',(10.6341664979999,12.2,1.31092202699998));
#192232=CARTESIAN_POINT('Ctrl Pts',(10.6317541279999,12.2,1.31127020699998));
#192233=CARTESIAN_POINT('Ctrl Pts',(10.6293476599999,12.2,1.31161540699999));
#192234=CARTESIAN_POINT('Ctrl Pts',(10.6269471099999,12.2,1.31195763899999));
#192235=CARTESIAN_POINT('Ctrl Pts',(10.6245524889999,12.2,1.31229690699998));
#192236=CARTESIAN_POINT('Ctrl Pts',(10.6221638119999,12.2,1.31263321999999));
#192237=CARTESIAN_POINT('Ctrl Pts',(10.6197810909999,12.2,1.31296658599998));
#192238=CARTESIAN_POINT('Ctrl Pts',(10.6174043419999,12.2,1.31329701299999));
#192239=CARTESIAN_POINT('Ctrl Pts',(10.6150335779999,12.2,1.31362450999998));
#192240=CARTESIAN_POINT('Ctrl Pts',(10.6126688119999,12.2,1.31394908099999));
#192241=CARTESIAN_POINT('Ctrl Pts',(10.6103100589999,12.2,1.31427073799999));
#192242=CARTESIAN_POINT('Ctrl Pts',(10.6079573329999,12.2,1.31458948699999));
#192243=CARTESIAN_POINT('Ctrl Pts',(10.6056106459999,12.2,1.31490533699999));
#192244=CARTESIAN_POINT('Ctrl Pts',(10.6032700129999,12.2,1.31521829699999));
#192245=CARTESIAN_POINT('Ctrl Pts',(10.6009354489999,12.2,1.31552837099999));
#192246=CARTESIAN_POINT('Ctrl Pts',(10.5986069669999,12.2,1.31583557099999));
#192247=CARTESIAN_POINT('Ctrl Pts',(10.5962845809999,12.2,1.31613990499998));
#192248=CARTESIAN_POINT('Ctrl Pts',(10.5935050499009,12.2,1.31650167378684));
#192249=CARTESIAN_POINT('Ctrl Pts',(10.5907347060494,12.2,1.31685916610655));
#192250=CARTESIAN_POINT('Ctrl Pts',(10.5879735759504,12.2,1.31721239989341));
#192251=CARTESIAN_POINT('Ctrl Pts',(10.5852216883489,12.2,1.31756139018143));
#192252=CARTESIAN_POINT('Ctrl Pts',(10.5824790749999,12.2,1.31790615499999));
#192253=CARTESIAN_POINT('Ctrl Pts',(10.5801997579999,12.2,1.31819064899998));
#192254=CARTESIAN_POINT('Ctrl Pts',(10.5779266509999,12.2,1.31847234299999));
#192255=CARTESIAN_POINT('Ctrl Pts',(10.5756597679999,12.2,1.31875124499999));
#192256=CARTESIAN_POINT('Ctrl Pts',(10.5733991249999,12.2,1.31902736299998));
#192257=CARTESIAN_POINT('Ctrl Pts',(10.5711447329999,12.2,1.31930070599998));
#192258=CARTESIAN_POINT('Ctrl Pts',(10.5688966099999,12.2,1.31957128299999));
#192259=CARTESIAN_POINT('Ctrl Pts',(10.5666547689999,12.2,1.31983910099999));
#192260=CARTESIAN_POINT('Ctrl Pts',(10.5644192249999,12.2,1.32010417099998));
#192261=CARTESIAN_POINT('Ctrl Pts',(10.5621899909999,12.2,1.32036649799999));
#192262=CARTESIAN_POINT('Ctrl Pts',(10.5599670829999,12.2,1.32062609399998));
#192263=CARTESIAN_POINT('Ctrl Pts',(10.5577505169999,12.2,1.32088296799999));
#192264=CARTESIAN_POINT('Ctrl Pts',(10.5555403039999,12.2,1.32113712699998));
#192265=CARTESIAN_POINT('Ctrl Pts',(10.5533364629999,12.2,1.32138857999998));
#192266=CARTESIAN_POINT('Ctrl Pts',(10.5511390059999,12.2,1.32163733699999));
#192267=CARTESIAN_POINT('Ctrl Pts',(10.5489479479999,12.2,1.32188340599999));
#192268=CARTESIAN_POINT('Ctrl Pts',(10.5467633059999,12.2,1.32212679499998));
#192269=CARTESIAN_POINT('Ctrl Pts',(10.5445850929999,12.2,1.32236751399998));
#192270=CARTESIAN_POINT('Ctrl Pts',(10.5424133229999,12.2,1.32260557299999));
#192271=CARTESIAN_POINT('Ctrl Pts',(10.5402480139999,12.2,1.32284097999999));
#192272=CARTESIAN_POINT('Ctrl Pts',(10.5380891789999,12.2,1.32307374399999));
#192273=CARTESIAN_POINT('Ctrl Pts',(10.5359368329999,12.2,1.32330387399998));
#192274=CARTESIAN_POINT('Ctrl Pts',(10.5337909929999,12.2,1.32353137899999));
#192275=CARTESIAN_POINT('Ctrl Pts',(10.5316516719999,12.2,1.32375626999998));
#192276=CARTESIAN_POINT('Ctrl Pts',(10.5295188859999,12.2,1.32397855399998));
#192277=CARTESIAN_POINT('Ctrl Pts',(10.5273926489999,12.2,1.32419824099999));
#192278=CARTESIAN_POINT('Ctrl Pts',(10.5252729789999,12.2,1.32441534099998));
#192279=CARTESIAN_POINT('Ctrl Pts',(10.5231598899999,12.2,1.32462986199998));
#192280=CARTESIAN_POINT('Ctrl Pts',(10.5210533959999,12.2,1.32484181499999));
#192281=CARTESIAN_POINT('Ctrl Pts',(10.5189535149999,12.2,1.32505120799999));
#192282=CARTESIAN_POINT('Ctrl Pts',(10.5168602599999,12.2,1.32525805099998));
#192283=CARTESIAN_POINT('Ctrl Pts',(10.5147736479999,12.2,1.32546235499999));
#192284=CARTESIAN_POINT('Ctrl Pts',(10.5126936939999,12.2,1.32566412699999));
#192285=CARTESIAN_POINT('Ctrl Pts',(10.5106204149999,12.2,1.32586337799999));
#192286=CARTESIAN_POINT('Ctrl Pts',(10.5085538239999,12.2,1.32606011699998));
#192287=CARTESIAN_POINT('Ctrl Pts',(10.5064939389999,12.2,1.32625435499999));
#192288=CARTESIAN_POINT('Ctrl Pts',(10.5044407749999,12.2,1.32644610099999));
#192289=CARTESIAN_POINT('Ctrl Pts',(10.5023943459999,12.2,1.32663536299999));
#192290=CARTESIAN_POINT('Ctrl Pts',(10.5003546709999,12.2,1.32682215399999));
#192291=CARTESIAN_POINT('Ctrl Pts',(10.4983217629999,12.2,1.32700648099998));
#192292=CARTESIAN_POINT('Ctrl Pts',(10.4962956399999,12.2,1.32718835599999));
#192293=CARTESIAN_POINT('Ctrl Pts',(10.4942763159999,12.2,1.32736778799998));
#192294=CARTESIAN_POINT('Ctrl Pts',(10.4922638099999,12.2,1.32754478599999));
#192295=CARTESIAN_POINT('Ctrl Pts',(10.4902581349999,12.2,1.32771936199998));
#192296=CARTESIAN_POINT('Ctrl Pts',(10.4882593079999,12.2,1.32789152599999));
#192297=CARTESIAN_POINT('Ctrl Pts',(10.4862673459999,12.2,1.32806128699999));
#192298=CARTESIAN_POINT('Ctrl Pts',(10.4842822649999,12.2,1.32822865399998));
#192299=CARTESIAN_POINT('Ctrl Pts',(10.4823040789999,12.2,1.32839363899999));
#192300=CARTESIAN_POINT('Ctrl Pts',(10.4803328079999,12.2,1.32855625199999));
#192301=CARTESIAN_POINT('Ctrl Pts',(10.4783684649999,12.2,1.32871650399998));
#192302=CARTESIAN_POINT('Ctrl Pts',(10.4764110689999,12.2,1.32887440299998));
#192303=CARTESIAN_POINT('Ctrl Pts',(10.4744606349999,12.2,1.32902996199999));
#192304=CARTESIAN_POINT('Ctrl Pts',(10.4725171799999,12.2,1.32918318999999));
#192305=CARTESIAN_POINT('Ctrl Pts',(10.4705807189999,12.2,1.32933409699998));
#192306=CARTESIAN_POINT('Ctrl Pts',(10.4686512709999,12.2,1.32948269499999));
#192307=CARTESIAN_POINT('Ctrl Pts',(10.4667288519999,12.2,1.32962899399999));
#192308=CARTESIAN_POINT('Ctrl Pts',(10.4648134769999,12.2,1.32977300399999));
#192309=CARTESIAN_POINT('Ctrl Pts',(10.4629051649999,12.2,1.32991473599999));
#192310=CARTESIAN_POINT('Ctrl Pts',(10.4610039309999,12.2,1.33005419999999));
#192311=CARTESIAN_POINT('Ctrl Pts',(10.4591097919999,12.2,1.33019140799998));
#192312=CARTESIAN_POINT('Ctrl Pts',(10.4572227669999,12.2,1.33032637099999));
#192313=CARTESIAN_POINT('Ctrl Pts',(10.4553428709999,12.2,1.33045909899999));
#192314=CARTESIAN_POINT('Ctrl Pts',(10.4534701199999,12.2,1.33058960299998));
#192315=CARTESIAN_POINT('Ctrl Pts',(10.4516045329999,12.2,1.33071789399999));
#192316=CARTESIAN_POINT('Ctrl Pts',(10.4497461279999,12.2,1.33084398299999));
#192317=CARTESIAN_POINT('Ctrl Pts',(10.4478949189999,12.2,1.33096787999999));
#192318=CARTESIAN_POINT('Ctrl Pts',(10.4460509249999,12.2,1.33108959799999));
#192319=CARTESIAN_POINT('Ctrl Pts',(10.4442141639999,12.2,1.33120914799999));
#192320=CARTESIAN_POINT('Ctrl Pts',(10.4423846519999,12.2,1.33132653899999));
#192321=CARTESIAN_POINT('Ctrl Pts',(10.4405624069999,12.2,1.33144178399998));
#192322=CARTESIAN_POINT('Ctrl Pts',(10.4387474469999,12.2,1.33155489399998));
#192323=CARTESIAN_POINT('Ctrl Pts',(10.4369397879999,12.2,1.33166588099999));
#192324=CARTESIAN_POINT('Ctrl Pts',(10.4351394479999,12.2,1.33177475499998));
#192325=CARTESIAN_POINT('Ctrl Pts',(10.4333464449999,12.2,1.33188152799999));
#192326=CARTESIAN_POINT('Ctrl Pts',(10.4315607969999,12.2,1.33198621299998));
#192327=CARTESIAN_POINT('Ctrl Pts',(10.4297825219999,12.2,1.33208881899999));
#192328=CARTESIAN_POINT('Ctrl Pts',(10.4280116349999,12.2,1.33218935899999));
#192329=CARTESIAN_POINT('Ctrl Pts',(10.4262481579999,12.2,1.33228784499998));
#192330=CARTESIAN_POINT('Ctrl Pts',(10.4244921049999,12.2,1.33238428799999));
#192331=CARTESIAN_POINT('Ctrl Pts',(10.4227434979999,12.2,1.33247869999999));
#192332=CARTESIAN_POINT('Ctrl Pts',(10.4210023509999,12.2,1.33257109199999));
#192333=CARTESIAN_POINT('Ctrl Pts',(10.4192686839999,12.2,1.33266147799999));
#192334=CARTESIAN_POINT('Ctrl Pts',(10.4175425149999,12.2,1.33274986699998));
#192335=CARTESIAN_POINT('Ctrl Pts',(10.4158238619999,12.2,1.33283627399999));
#192336=CARTESIAN_POINT('Ctrl Pts',(10.4141127429999,12.2,1.33292070899998));
#192337=CARTESIAN_POINT('Ctrl Pts',(10.4124091789999,12.2,1.33300318499999));
#192338=CARTESIAN_POINT('Ctrl Pts',(10.4107131829999,12.2,1.33308371299998));
#192339=CARTESIAN_POINT('Ctrl Pts',(10.4090247779999,12.2,1.33316230699998));
#192340=CARTESIAN_POINT('Ctrl Pts',(10.4073439809999,12.2,1.33323897699999));
#192341=CARTESIAN_POINT('Ctrl Pts',(10.4056708099999,12.2,1.33331373699999));
#192342=CARTESIAN_POINT('Ctrl Pts',(10.4040052849999,12.2,1.33338659999998));
#192343=CARTESIAN_POINT('Ctrl Pts',(10.4023474229999,12.2,1.33345757799999));
#192344=CARTESIAN_POINT('Ctrl Pts',(10.4006972429999,12.2,1.33352668099999));
#192345=CARTESIAN_POINT('Ctrl Pts',(10.3990547659999,12.2,1.33359392399999));
#192346=CARTESIAN_POINT('Ctrl Pts',(10.3974200079999,12.2,1.33365931999998));
#192347=CARTESIAN_POINT('Ctrl Pts',(10.3957929889999,12.2,1.33372287999999));
#192348=CARTESIAN_POINT('Ctrl Pts',(10.3941737289999,12.2,1.33378461799999));
#192349=CARTESIAN_POINT('Ctrl Pts',(10.3925622469999,12.2,1.33384454499998));
#192350=CARTESIAN_POINT('Ctrl Pts',(10.3909585599999,12.2,1.33390267699999));
#192351=CARTESIAN_POINT('Ctrl Pts',(10.3893626899999,12.2,1.33395902399998));
#192352=CARTESIAN_POINT('Ctrl Pts',(10.3877746539999,12.2,1.33401360099999));
#192353=CARTESIAN_POINT('Ctrl Pts',(10.3861944729999,12.2,1.33406641899999));
#192354=CARTESIAN_POINT('Ctrl Pts',(10.3846221649999,12.2,1.33411749199999));
#192355=CARTESIAN_POINT('Ctrl Pts',(10.3830577499999,12.2,1.33416683399998));
#192356=CARTESIAN_POINT('Ctrl Pts',(10.3815012489999,12.2,1.33421445799998));
#192357=CARTESIAN_POINT('Ctrl Pts',(10.3799526789999,12.2,1.33426037599999));
#192358=CARTESIAN_POINT('Ctrl Pts',(10.3784120619999,12.2,1.33430460199999));
#192359=CARTESIAN_POINT('Ctrl Pts',(10.3768794159999,12.2,1.33434714999999));
#192360=CARTESIAN_POINT('Ctrl Pts',(10.3753547629999,12.2,1.33438803399998));
#192361=CARTESIAN_POINT('Ctrl Pts',(10.3738381209999,12.2,1.33442726599998));
#192362=CARTESIAN_POINT('Ctrl Pts',(10.3723295099999,12.2,1.33446485899999));
#192363=CARTESIAN_POINT('Ctrl Pts',(10.3708289509999,12.2,1.33450082899999));
#192364=CARTESIAN_POINT('Ctrl Pts',(10.3693364639999,12.2,1.33453518899998));
#192365=CARTESIAN_POINT('Ctrl Pts',(10.3678520689999,12.2,1.33456795199999));
#192366=CARTESIAN_POINT('Ctrl Pts',(10.3663757859999,12.2,1.33459913299999));
#192367=CARTESIAN_POINT('Ctrl Pts',(10.3649076359999,12.2,1.33462874399998));
#192368=CARTESIAN_POINT('Ctrl Pts',(10.3634476389999,12.2,1.33465680099999));
#192369=CARTESIAN_POINT('Ctrl Pts',(10.3619958159999,12.2,1.33468331699999));
#192370=CARTESIAN_POINT('Ctrl Pts',(10.3605521859999,12.2,1.33470830799999));
#192371=CARTESIAN_POINT('Ctrl Pts',(10.3591167719999,12.2,1.33473178499999));
#192372=CARTESIAN_POINT('Ctrl Pts',(10.3576895929999,12.2,1.33475376599999));
#192373=CARTESIAN_POINT('Ctrl Pts',(10.3562706699999,12.2,1.33477426199998));
#192374=CARTESIAN_POINT('Ctrl Pts',(10.3548600249999,12.2,1.33479328899998));
#192375=CARTESIAN_POINT('Ctrl Pts',(10.3534576789999,12.2,1.33481086299998));
#192376=CARTESIAN_POINT('Ctrl Pts',(10.3520636509999,12.2,1.33482699499998));
#192377=CARTESIAN_POINT('Ctrl Pts',(10.3506779649999,12.2,1.33484170199999));
#192378=CARTESIAN_POINT('Ctrl Pts',(10.3493006389999,12.2,1.33485499899999));
#192379=CARTESIAN_POINT('Ctrl Pts',(10.3479316969999,12.2,1.33486689999998));
#192380=CARTESIAN_POINT('Ctrl Pts',(10.3465711599999,12.2,1.33487741899998));
#192381=CARTESIAN_POINT('Ctrl Pts',(10.3452190479999,12.2,1.33488657399999));
#192382=CARTESIAN_POINT('Ctrl Pts',(10.3438753839999,12.2,1.33489437599998));
#192383=CARTESIAN_POINT('Ctrl Pts',(10.3425401889999,12.2,1.33490084399998));
#192384=CARTESIAN_POINT('Ctrl Pts',(10.3412134849999,12.2,1.33490598999999));
#192385=CARTESIAN_POINT('Ctrl Pts',(10.3398952939999,12.2,1.33490982999998));
#192386=CARTESIAN_POINT('Ctrl Pts',(10.3385856379999,12.2,1.33491238099999));
#192387=CARTESIAN_POINT('Ctrl Pts',(10.3372845369999,12.2,1.33491365699999));
#192388=CARTESIAN_POINT('Ctrl Pts',(10.3359920159999,12.2,1.33491367299999));
#192389=CARTESIAN_POINT('Ctrl Pts',(10.3347080959999,12.2,1.33491244599998));
#192390=CARTESIAN_POINT('Ctrl Pts',(10.3334327989999,12.2,1.33490999099998));
#192391=CARTESIAN_POINT('Ctrl Pts',(10.3321661469999,12.2,1.33490632399999));
#192392=CARTESIAN_POINT('Ctrl Pts',(10.3309081639999,12.2,1.33490145999998));
#192393=CARTESIAN_POINT('Ctrl Pts',(10.3296588699999,12.2,1.33489541599999));
#192394=CARTESIAN_POINT('Ctrl Pts',(10.3284182899999,12.2,1.33488820699998));
#192395=CARTESIAN_POINT('Ctrl Pts',(10.3271864459999,12.2,1.33487984899999));
#192396=CARTESIAN_POINT('Ctrl Pts',(10.3259633609999,12.2,1.33487035899998));
#192397=CARTESIAN_POINT('Ctrl Pts',(10.3247490569999,12.2,1.33485975299998));
#192398=CARTESIAN_POINT('Ctrl Pts',(10.3235435579999,12.2,1.33484804699998));
#192399=CARTESIAN_POINT('Ctrl Pts',(10.3223468859999,12.2,1.33483525699999));
#192400=CARTESIAN_POINT('Ctrl Pts',(10.3211590649999,12.2,1.33482139999999));
#192401=CARTESIAN_POINT('Ctrl Pts',(10.3199801189999,12.2,1.33480649299999));
#192402=CARTESIAN_POINT('Ctrl Pts',(10.3188100709999,12.2,1.33479055299999));
#192403=CARTESIAN_POINT('Ctrl Pts',(10.3176489429999,12.2,1.33477359499999));
#192404=CARTESIAN_POINT('Ctrl Pts',(10.3164967599999,12.2,1.33475563599998));
#192405=CARTESIAN_POINT('Ctrl Pts',(10.3153535459999,12.2,1.33473669599999));
#192406=CARTESIAN_POINT('Ctrl Pts',(10.3142193239999,12.2,1.33471678699999));
#192407=CARTESIAN_POINT('Ctrl Pts',(10.3130941179999,12.2,1.33469593099999));
#192408=CARTESIAN_POINT('Ctrl Pts',(10.3119779519999,12.2,1.33467414199998));
#192409=CARTESIAN_POINT('Ctrl Pts',(10.3108708509999,12.2,1.33465143799999));
#192410=CARTESIAN_POINT('Ctrl Pts',(10.3097728379999,12.2,1.33462783699999));
#192411=CARTESIAN_POINT('Ctrl Pts',(10.3086839379999,12.2,1.33460335699999));
#192412=CARTESIAN_POINT('Ctrl Pts',(10.3076041749999,12.2,1.33457801399999));
#192413=CARTESIAN_POINT('Ctrl Pts',(10.3065335739999,12.2,1.33455182699999));
#192414=CARTESIAN_POINT('Ctrl Pts',(10.3054721599999,12.2,1.33452481299999));
#192415=CARTESIAN_POINT('Ctrl Pts',(10.3044199559999,12.2,1.33449698899998));
#192416=CARTESIAN_POINT('Ctrl Pts',(10.3033769899999,12.2,1.33446837399998));
#192417=CARTESIAN_POINT('Ctrl Pts',(10.3023432839999,12.2,1.33443898699999));
#192418=CARTESIAN_POINT('Ctrl Pts',(10.3013188639999,12.2,1.33440884399999));
#192419=CARTESIAN_POINT('Ctrl Pts',(10.3003037569999,12.2,1.33437796599999));
#192420=CARTESIAN_POINT('Ctrl Pts',(10.2992979849999,12.2,1.33434636899999));
#192421=CARTESIAN_POINT('Ctrl Pts',(10.2983015759999,12.2,1.33431407099998));
#192422=CARTESIAN_POINT('Ctrl Pts',(10.2973145539999,12.2,1.33428109299999));
#192423=CARTESIAN_POINT('Ctrl Pts',(10.2963369469999,12.2,1.33424745299998));
#192424=CARTESIAN_POINT('Ctrl Pts',(10.2953687779999,12.2,1.33421316799998));
#192425=CARTESIAN_POINT('Ctrl Pts',(10.2944100739999,12.2,1.33417825799999));
#192426=CARTESIAN_POINT('Ctrl Pts',(10.2934608629999,12.2,1.33414274199998));
#192427=CARTESIAN_POINT('Ctrl Pts',(10.2925211679999,12.2,1.33410663999999));
#192428=CARTESIAN_POINT('Ctrl Pts',(10.2915910169999,12.2,1.33406996999998));
#192429=CARTESIAN_POINT('Ctrl Pts',(10.2906757369999,12.2,1.33403296599999));
#192430=CARTESIAN_POINT('Ctrl Pts',(10.2899521419999,12.2,1.33400298799998));
#192431=CARTESIAN_POINT('Ctrl Pts',(10.2894150039999,12.2,1.33398033399999));
#192432=CARTESIAN_POINT('Ctrl Pts',(10.2890605199999,12.2,1.33396520799999));
#192433=CARTESIAN_POINT('Ctrl Pts',(10.2888863229999,12.2,1.33395773199998));
#192434=CARTESIAN_POINT('Ctrl Pts',(10.2888863229999,15.2,1.33395773199998));
#192435=CARTESIAN_POINT('Ctrl Pts',(10.2890605199999,15.2,1.33396520799999));
#192436=CARTESIAN_POINT('Ctrl Pts',(10.2894150039999,15.2,1.33398033399999));
#192437=CARTESIAN_POINT('Ctrl Pts',(10.2899521419999,15.2,1.33400298799998));
#192438=CARTESIAN_POINT('Ctrl Pts',(10.2906757369999,15.2,1.33403296599999));
#192439=CARTESIAN_POINT('Ctrl Pts',(10.2915910169999,15.2,1.33406996999998));
#192440=CARTESIAN_POINT('Ctrl Pts',(10.2925211679999,15.2,1.33410663999999));
#192441=CARTESIAN_POINT('Ctrl Pts',(10.2934608629999,15.2,1.33414274199998));
#192442=CARTESIAN_POINT('Ctrl Pts',(10.2944100739999,15.2,1.33417825799999));
#192443=CARTESIAN_POINT('Ctrl Pts',(10.2953687779999,15.2,1.33421316799998));
#192444=CARTESIAN_POINT('Ctrl Pts',(10.2963369469999,15.2,1.33424745299998));
#192445=CARTESIAN_POINT('Ctrl Pts',(10.2973145539999,15.2,1.33428109299999));
#192446=CARTESIAN_POINT('Ctrl Pts',(10.2983015759999,15.2,1.33431407099998));
#192447=CARTESIAN_POINT('Ctrl Pts',(10.2992979849999,15.2,1.33434636899999));
#192448=CARTESIAN_POINT('Ctrl Pts',(10.3003037569999,15.2,1.33437796599999));
#192449=CARTESIAN_POINT('Ctrl Pts',(10.3013188639999,15.2,1.33440884399999));
#192450=CARTESIAN_POINT('Ctrl Pts',(10.3023432839999,15.2,1.33443898699999));
#192451=CARTESIAN_POINT('Ctrl Pts',(10.3033769899999,15.2,1.33446837399998));
#192452=CARTESIAN_POINT('Ctrl Pts',(10.3044199559999,15.2,1.33449698899998));
#192453=CARTESIAN_POINT('Ctrl Pts',(10.3054721599999,15.2,1.33452481299999));
#192454=CARTESIAN_POINT('Ctrl Pts',(10.3065335739999,15.2,1.33455182699999));
#192455=CARTESIAN_POINT('Ctrl Pts',(10.3076041749999,15.2,1.33457801399999));
#192456=CARTESIAN_POINT('Ctrl Pts',(10.3086839379999,15.2,1.33460335699999));
#192457=CARTESIAN_POINT('Ctrl Pts',(10.3097728379999,15.2,1.33462783699999));
#192458=CARTESIAN_POINT('Ctrl Pts',(10.3108708509999,15.2,1.33465143799999));
#192459=CARTESIAN_POINT('Ctrl Pts',(10.3119779519999,15.2,1.33467414199998));
#192460=CARTESIAN_POINT('Ctrl Pts',(10.3130941179999,15.2,1.33469593099999));
#192461=CARTESIAN_POINT('Ctrl Pts',(10.3142193239999,15.2,1.33471678699999));
#192462=CARTESIAN_POINT('Ctrl Pts',(10.3153535459999,15.2,1.33473669599999));
#192463=CARTESIAN_POINT('Ctrl Pts',(10.3164967599999,15.2,1.33475563599998));
#192464=CARTESIAN_POINT('Ctrl Pts',(10.3176489429999,15.2,1.33477359499999));
#192465=CARTESIAN_POINT('Ctrl Pts',(10.3188100709999,15.2,1.33479055299999));
#192466=CARTESIAN_POINT('Ctrl Pts',(10.3199801189999,15.2,1.33480649299999));
#192467=CARTESIAN_POINT('Ctrl Pts',(10.3211590649999,15.2,1.33482139999999));
#192468=CARTESIAN_POINT('Ctrl Pts',(10.3223468859999,15.2,1.33483525699999));
#192469=CARTESIAN_POINT('Ctrl Pts',(10.3235435579999,15.2,1.33484804699998));
#192470=CARTESIAN_POINT('Ctrl Pts',(10.3247490569999,15.2,1.33485975299998));
#192471=CARTESIAN_POINT('Ctrl Pts',(10.3259633609999,15.2,1.33487035899998));
#192472=CARTESIAN_POINT('Ctrl Pts',(10.3271864459999,15.2,1.33487984899999));
#192473=CARTESIAN_POINT('Ctrl Pts',(10.3284182899999,15.2,1.33488820699998));
#192474=CARTESIAN_POINT('Ctrl Pts',(10.3296588699999,15.2,1.33489541599999));
#192475=CARTESIAN_POINT('Ctrl Pts',(10.3309081639999,15.2,1.33490145999998));
#192476=CARTESIAN_POINT('Ctrl Pts',(10.3321661469999,15.2,1.33490632399999));
#192477=CARTESIAN_POINT('Ctrl Pts',(10.3334327989999,15.2,1.33490999099998));
#192478=CARTESIAN_POINT('Ctrl Pts',(10.3347080959999,15.2,1.33491244599998));
#192479=CARTESIAN_POINT('Ctrl Pts',(10.3359920159999,15.2,1.33491367299999));
#192480=CARTESIAN_POINT('Ctrl Pts',(10.3372845369999,15.2,1.33491365699999));
#192481=CARTESIAN_POINT('Ctrl Pts',(10.3385856379999,15.2,1.33491238099999));
#192482=CARTESIAN_POINT('Ctrl Pts',(10.3398952939999,15.2,1.33490982999998));
#192483=CARTESIAN_POINT('Ctrl Pts',(10.3412134849999,15.2,1.33490598999999));
#192484=CARTESIAN_POINT('Ctrl Pts',(10.3425401889999,15.2,1.33490084399998));
#192485=CARTESIAN_POINT('Ctrl Pts',(10.3438753839999,15.2,1.33489437599998));
#192486=CARTESIAN_POINT('Ctrl Pts',(10.3452190479999,15.2,1.33488657399999));
#192487=CARTESIAN_POINT('Ctrl Pts',(10.3465711599999,15.2,1.33487741899998));
#192488=CARTESIAN_POINT('Ctrl Pts',(10.3479316969999,15.2,1.33486689999998));
#192489=CARTESIAN_POINT('Ctrl Pts',(10.3493006389999,15.2,1.33485499899999));
#192490=CARTESIAN_POINT('Ctrl Pts',(10.3506779649999,15.2,1.33484170199999));
#192491=CARTESIAN_POINT('Ctrl Pts',(10.3520636509999,15.2,1.33482699499998));
#192492=CARTESIAN_POINT('Ctrl Pts',(10.3534576789999,15.2,1.33481086299998));
#192493=CARTESIAN_POINT('Ctrl Pts',(10.3548600249999,15.2,1.33479328899998));
#192494=CARTESIAN_POINT('Ctrl Pts',(10.3562706699999,15.2,1.33477426199998));
#192495=CARTESIAN_POINT('Ctrl Pts',(10.3576895929999,15.2,1.33475376599999));
#192496=CARTESIAN_POINT('Ctrl Pts',(10.3591167719999,15.2,1.33473178499999));
#192497=CARTESIAN_POINT('Ctrl Pts',(10.3605521859999,15.2,1.33470830799999));
#192498=CARTESIAN_POINT('Ctrl Pts',(10.3619958159999,15.2,1.33468331699999));
#192499=CARTESIAN_POINT('Ctrl Pts',(10.3634476389999,15.2,1.33465680099999));
#192500=CARTESIAN_POINT('Ctrl Pts',(10.3649076359999,15.2,1.33462874399998));
#192501=CARTESIAN_POINT('Ctrl Pts',(10.3663757859999,15.2,1.33459913299999));
#192502=CARTESIAN_POINT('Ctrl Pts',(10.3678520689999,15.2,1.33456795199999));
#192503=CARTESIAN_POINT('Ctrl Pts',(10.3693364639999,15.2,1.33453518899998));
#192504=CARTESIAN_POINT('Ctrl Pts',(10.3708289509999,15.2,1.33450082899999));
#192505=CARTESIAN_POINT('Ctrl Pts',(10.3723295099999,15.2,1.33446485899999));
#192506=CARTESIAN_POINT('Ctrl Pts',(10.3738381209999,15.2,1.33442726599998));
#192507=CARTESIAN_POINT('Ctrl Pts',(10.3753547629999,15.2,1.33438803399998));
#192508=CARTESIAN_POINT('Ctrl Pts',(10.3768794159999,15.2,1.33434714999999));
#192509=CARTESIAN_POINT('Ctrl Pts',(10.3784120619999,15.2,1.33430460199999));
#192510=CARTESIAN_POINT('Ctrl Pts',(10.3799526789999,15.2,1.33426037599999));
#192511=CARTESIAN_POINT('Ctrl Pts',(10.3815012489999,15.2,1.33421445799998));
#192512=CARTESIAN_POINT('Ctrl Pts',(10.3830577499999,15.2,1.33416683399998));
#192513=CARTESIAN_POINT('Ctrl Pts',(10.3846221649999,15.2,1.33411749199999));
#192514=CARTESIAN_POINT('Ctrl Pts',(10.3861944729999,15.2,1.33406641899999));
#192515=CARTESIAN_POINT('Ctrl Pts',(10.3877746539999,15.2,1.33401360099999));
#192516=CARTESIAN_POINT('Ctrl Pts',(10.3893626899999,15.2,1.33395902399998));
#192517=CARTESIAN_POINT('Ctrl Pts',(10.3909585599999,15.2,1.33390267699999));
#192518=CARTESIAN_POINT('Ctrl Pts',(10.3925622469999,15.2,1.33384454499998));
#192519=CARTESIAN_POINT('Ctrl Pts',(10.3941737289999,15.2,1.33378461799999));
#192520=CARTESIAN_POINT('Ctrl Pts',(10.3957929889999,15.2,1.33372287999999));
#192521=CARTESIAN_POINT('Ctrl Pts',(10.3974200079999,15.2,1.33365931999998));
#192522=CARTESIAN_POINT('Ctrl Pts',(10.3990547659999,15.2,1.33359392399999));
#192523=CARTESIAN_POINT('Ctrl Pts',(10.4006972429999,15.2,1.33352668099999));
#192524=CARTESIAN_POINT('Ctrl Pts',(10.4023474229999,15.2,1.33345757799999));
#192525=CARTESIAN_POINT('Ctrl Pts',(10.4040052849999,15.2,1.33338659999998));
#192526=CARTESIAN_POINT('Ctrl Pts',(10.4056708099999,15.2,1.33331373699999));
#192527=CARTESIAN_POINT('Ctrl Pts',(10.4073439809999,15.2,1.33323897699999));
#192528=CARTESIAN_POINT('Ctrl Pts',(10.4090247779999,15.2,1.33316230699998));
#192529=CARTESIAN_POINT('Ctrl Pts',(10.4107131829999,15.2,1.33308371299998));
#192530=CARTESIAN_POINT('Ctrl Pts',(10.4124091789999,15.2,1.33300318499999));
#192531=CARTESIAN_POINT('Ctrl Pts',(10.4141127429999,15.2,1.33292070899998));
#192532=CARTESIAN_POINT('Ctrl Pts',(10.4158238619999,15.2,1.33283627399999));
#192533=CARTESIAN_POINT('Ctrl Pts',(10.4175425149999,15.2,1.33274986699998));
#192534=CARTESIAN_POINT('Ctrl Pts',(10.4192686839999,15.2,1.33266147799999));
#192535=CARTESIAN_POINT('Ctrl Pts',(10.4210023509999,15.2,1.33257109199999));
#192536=CARTESIAN_POINT('Ctrl Pts',(10.4227434979999,15.2,1.33247869999999));
#192537=CARTESIAN_POINT('Ctrl Pts',(10.4244921049999,15.2,1.33238428799999));
#192538=CARTESIAN_POINT('Ctrl Pts',(10.4262481579999,15.2,1.33228784499998));
#192539=CARTESIAN_POINT('Ctrl Pts',(10.4280116349999,15.2,1.33218935899999));
#192540=CARTESIAN_POINT('Ctrl Pts',(10.4297825219999,15.2,1.33208881899999));
#192541=CARTESIAN_POINT('Ctrl Pts',(10.4315607969999,15.2,1.33198621299998));
#192542=CARTESIAN_POINT('Ctrl Pts',(10.4333464449999,15.2,1.33188152799999));
#192543=CARTESIAN_POINT('Ctrl Pts',(10.4351394479999,15.2,1.33177475499998));
#192544=CARTESIAN_POINT('Ctrl Pts',(10.4369397879999,15.2,1.33166588099999));
#192545=CARTESIAN_POINT('Ctrl Pts',(10.4387474469999,15.2,1.33155489399998));
#192546=CARTESIAN_POINT('Ctrl Pts',(10.4405624069999,15.2,1.33144178399998));
#192547=CARTESIAN_POINT('Ctrl Pts',(10.4423846519999,15.2,1.33132653899999));
#192548=CARTESIAN_POINT('Ctrl Pts',(10.4442141639999,15.2,1.33120914799999));
#192549=CARTESIAN_POINT('Ctrl Pts',(10.4460509249999,15.2,1.33108959799999));
#192550=CARTESIAN_POINT('Ctrl Pts',(10.4478949189999,15.2,1.33096787999999));
#192551=CARTESIAN_POINT('Ctrl Pts',(10.4497461279999,15.2,1.33084398299999));
#192552=CARTESIAN_POINT('Ctrl Pts',(10.4516045329999,15.2,1.33071789399999));
#192553=CARTESIAN_POINT('Ctrl Pts',(10.4534701199999,15.2,1.33058960299998));
#192554=CARTESIAN_POINT('Ctrl Pts',(10.4553428709999,15.2,1.33045909899999));
#192555=CARTESIAN_POINT('Ctrl Pts',(10.4572227669999,15.2,1.33032637099999));
#192556=CARTESIAN_POINT('Ctrl Pts',(10.4591097919999,15.2,1.33019140799998));
#192557=CARTESIAN_POINT('Ctrl Pts',(10.4610039309999,15.2,1.33005419999999));
#192558=CARTESIAN_POINT('Ctrl Pts',(10.4629051649999,15.2,1.32991473599999));
#192559=CARTESIAN_POINT('Ctrl Pts',(10.4648134769999,15.2,1.32977300399999));
#192560=CARTESIAN_POINT('Ctrl Pts',(10.4667288519999,15.2,1.32962899399999));
#192561=CARTESIAN_POINT('Ctrl Pts',(10.4686512709999,15.2,1.32948269499999));
#192562=CARTESIAN_POINT('Ctrl Pts',(10.4705807189999,15.2,1.32933409699998));
#192563=CARTESIAN_POINT('Ctrl Pts',(10.4725171799999,15.2,1.32918318999999));
#192564=CARTESIAN_POINT('Ctrl Pts',(10.4744606349999,15.2,1.32902996199999));
#192565=CARTESIAN_POINT('Ctrl Pts',(10.4764110689999,15.2,1.32887440299998));
#192566=CARTESIAN_POINT('Ctrl Pts',(10.4783684649999,15.2,1.32871650399998));
#192567=CARTESIAN_POINT('Ctrl Pts',(10.4803328079999,15.2,1.32855625199999));
#192568=CARTESIAN_POINT('Ctrl Pts',(10.4823040789999,15.2,1.32839363899999));
#192569=CARTESIAN_POINT('Ctrl Pts',(10.4842822649999,15.2,1.32822865399998));
#192570=CARTESIAN_POINT('Ctrl Pts',(10.4862673459999,15.2,1.32806128699999));
#192571=CARTESIAN_POINT('Ctrl Pts',(10.4882593079999,15.2,1.32789152599999));
#192572=CARTESIAN_POINT('Ctrl Pts',(10.4902581349999,15.2,1.32771936199998));
#192573=CARTESIAN_POINT('Ctrl Pts',(10.4922638099999,15.2,1.32754478599999));
#192574=CARTESIAN_POINT('Ctrl Pts',(10.4942763159999,15.2,1.32736778799998));
#192575=CARTESIAN_POINT('Ctrl Pts',(10.4962956399999,15.2,1.32718835599999));
#192576=CARTESIAN_POINT('Ctrl Pts',(10.4983217629999,15.2,1.32700648099998));
#192577=CARTESIAN_POINT('Ctrl Pts',(10.5003546709999,15.2,1.32682215399999));
#192578=CARTESIAN_POINT('Ctrl Pts',(10.5023943459999,15.2,1.32663536299999));
#192579=CARTESIAN_POINT('Ctrl Pts',(10.5044407749999,15.2,1.32644610099999));
#192580=CARTESIAN_POINT('Ctrl Pts',(10.5064939389999,15.2,1.32625435499999));
#192581=CARTESIAN_POINT('Ctrl Pts',(10.5085538239999,15.2,1.32606011699998));
#192582=CARTESIAN_POINT('Ctrl Pts',(10.5106204149999,15.2,1.32586337799999));
#192583=CARTESIAN_POINT('Ctrl Pts',(10.5126936939999,15.2,1.32566412699999));
#192584=CARTESIAN_POINT('Ctrl Pts',(10.5147736479999,15.2,1.32546235499999));
#192585=CARTESIAN_POINT('Ctrl Pts',(10.5168602599999,15.2,1.32525805099998));
#192586=CARTESIAN_POINT('Ctrl Pts',(10.5189535149999,15.2,1.32505120799999));
#192587=CARTESIAN_POINT('Ctrl Pts',(10.5210533959999,15.2,1.32484181499999));
#192588=CARTESIAN_POINT('Ctrl Pts',(10.5231598899999,15.2,1.32462986199998));
#192589=CARTESIAN_POINT('Ctrl Pts',(10.5252729789999,15.2,1.32441534099998));
#192590=CARTESIAN_POINT('Ctrl Pts',(10.5273926489999,15.2,1.32419824099999));
#192591=CARTESIAN_POINT('Ctrl Pts',(10.5295188859999,15.2,1.32397855399998));
#192592=CARTESIAN_POINT('Ctrl Pts',(10.5316516719999,15.2,1.32375626999998));
#192593=CARTESIAN_POINT('Ctrl Pts',(10.5337909929999,15.2,1.32353137899999));
#192594=CARTESIAN_POINT('Ctrl Pts',(10.5359368329999,15.2,1.32330387399998));
#192595=CARTESIAN_POINT('Ctrl Pts',(10.5380891789999,15.2,1.32307374399999));
#192596=CARTESIAN_POINT('Ctrl Pts',(10.5402480139999,15.2,1.32284097999999));
#192597=CARTESIAN_POINT('Ctrl Pts',(10.5424133229999,15.2,1.32260557299999));
#192598=CARTESIAN_POINT('Ctrl Pts',(10.5445850929999,15.2,1.32236751399998));
#192599=CARTESIAN_POINT('Ctrl Pts',(10.5467633059999,15.2,1.32212679499998));
#192600=CARTESIAN_POINT('Ctrl Pts',(10.5489479479999,15.2,1.32188340599999));
#192601=CARTESIAN_POINT('Ctrl Pts',(10.5511390059999,15.2,1.32163733699999));
#192602=CARTESIAN_POINT('Ctrl Pts',(10.5533364629999,15.2,1.32138857999998));
#192603=CARTESIAN_POINT('Ctrl Pts',(10.5555403039999,15.2,1.32113712699998));
#192604=CARTESIAN_POINT('Ctrl Pts',(10.5577505169999,15.2,1.32088296799999));
#192605=CARTESIAN_POINT('Ctrl Pts',(10.5599670829999,15.2,1.32062609399998));
#192606=CARTESIAN_POINT('Ctrl Pts',(10.5621899909999,15.2,1.32036649799999));
#192607=CARTESIAN_POINT('Ctrl Pts',(10.5644192249999,15.2,1.32010417099998));
#192608=CARTESIAN_POINT('Ctrl Pts',(10.5666547689999,15.2,1.31983910099999));
#192609=CARTESIAN_POINT('Ctrl Pts',(10.5688966099999,15.2,1.31957128299999));
#192610=CARTESIAN_POINT('Ctrl Pts',(10.5711447329999,15.2,1.31930070599998));
#192611=CARTESIAN_POINT('Ctrl Pts',(10.5733991249999,15.2,1.31902736299998));
#192612=CARTESIAN_POINT('Ctrl Pts',(10.5756597679999,15.2,1.31875124499999));
#192613=CARTESIAN_POINT('Ctrl Pts',(10.5779266509999,15.2,1.31847234299999));
#192614=CARTESIAN_POINT('Ctrl Pts',(10.5801997579999,15.2,1.31819064899998));
#192615=CARTESIAN_POINT('Ctrl Pts',(10.5824790749999,15.2,1.31790615499999));
#192616=CARTESIAN_POINT('Ctrl Pts',(10.5852216883494,15.2,1.3175613901812));
#192617=CARTESIAN_POINT('Ctrl Pts',(10.5879735759502,15.2,1.31721239989353));
#192618=CARTESIAN_POINT('Ctrl Pts',(10.5907347060497,15.2,1.31685916610644));
#192619=CARTESIAN_POINT('Ctrl Pts',(10.5935050499004,15.2,1.31650167378707));
#192620=CARTESIAN_POINT('Ctrl Pts',(10.5962845809999,15.2,1.31613990499998));
#192621=CARTESIAN_POINT('Ctrl Pts',(10.5986069669999,15.2,1.31583557099999));
#192622=CARTESIAN_POINT('Ctrl Pts',(10.6009354489999,15.2,1.31552837099999));
#192623=CARTESIAN_POINT('Ctrl Pts',(10.6032700129999,15.2,1.31521829699999));
#192624=CARTESIAN_POINT('Ctrl Pts',(10.6056106459999,15.2,1.31490533699999));
#192625=CARTESIAN_POINT('Ctrl Pts',(10.6079573329999,15.2,1.31458948699999));
#192626=CARTESIAN_POINT('Ctrl Pts',(10.6103100589999,15.2,1.31427073799999));
#192627=CARTESIAN_POINT('Ctrl Pts',(10.6126688119999,15.2,1.31394908099999));
#192628=CARTESIAN_POINT('Ctrl Pts',(10.6150335779999,15.2,1.31362450999998));
#192629=CARTESIAN_POINT('Ctrl Pts',(10.6174043419999,15.2,1.31329701299999));
#192630=CARTESIAN_POINT('Ctrl Pts',(10.6197810909999,15.2,1.31296658599998));
#192631=CARTESIAN_POINT('Ctrl Pts',(10.6221638119999,15.2,1.31263321999999));
#192632=CARTESIAN_POINT('Ctrl Pts',(10.6245524889999,15.2,1.31229690699998));
#192633=CARTESIAN_POINT('Ctrl Pts',(10.6269471099999,15.2,1.31195763899999));
#192634=CARTESIAN_POINT('Ctrl Pts',(10.6293476599999,15.2,1.31161540699999));
#192635=CARTESIAN_POINT('Ctrl Pts',(10.6317541279999,15.2,1.31127020699998));
#192636=CARTESIAN_POINT('Ctrl Pts',(10.6341664979999,15.2,1.31092202699998));
#192637=CARTESIAN_POINT('Ctrl Pts',(10.6365847569999,15.2,1.31057086099998));
#192638=CARTESIAN_POINT('Ctrl Pts',(10.6390088909999,15.2,1.31021670299999));
#192639=CARTESIAN_POINT('Ctrl Pts',(10.6414388879999,15.2,1.30985954199998));
#192640=CARTESIAN_POINT('Ctrl Pts',(10.6438747329999,15.2,1.30949937399999));
#192641=CARTESIAN_POINT('Ctrl Pts',(10.6463164129999,15.2,1.30913618899998));
#192642=CARTESIAN_POINT('Ctrl Pts',(10.6487639159999,15.2,1.30876997899998));
#192643=CARTESIAN_POINT('Ctrl Pts',(10.6512172259999,15.2,1.30840073799999));
#192644=CARTESIAN_POINT('Ctrl Pts',(10.6536763329999,15.2,1.30802845899999));
#192645=CARTESIAN_POINT('Ctrl Pts',(10.6561412199999,15.2,1.30765313299999));
#192646=CARTESIAN_POINT('Ctrl Pts',(10.6586118759999,15.2,1.30727475299999));
#192647=CARTESIAN_POINT('Ctrl Pts',(10.6610882879999,15.2,1.30689331299998));
#192648=CARTESIAN_POINT('Ctrl Pts',(10.6635704409999,15.2,1.30650880399998));
#192649=CARTESIAN_POINT('Ctrl Pts',(10.6660583229999,15.2,1.30612121799999));
#192650=CARTESIAN_POINT('Ctrl Pts',(10.6685519209999,15.2,1.30573054999998));
#192651=CARTESIAN_POINT('Ctrl Pts',(10.6710512209999,15.2,1.30533679099999));
#192652=CARTESIAN_POINT('Ctrl Pts',(10.6735562119999,15.2,1.30493993399998));
#192653=CARTESIAN_POINT('Ctrl Pts',(10.6760668779999,15.2,1.30453997299998));
#192654=CARTESIAN_POINT('Ctrl Pts',(10.6785832079999,15.2,1.30413689899999));
#192655=CARTESIAN_POINT('Ctrl Pts',(10.6811051889999,15.2,1.30373070699998));
#192656=CARTESIAN_POINT('Ctrl Pts',(10.6836328059999,15.2,1.30332138799998));
#192657=CARTESIAN_POINT('Ctrl Pts',(10.6861660479999,15.2,1.30290893499998));
#192658=CARTESIAN_POINT('Ctrl Pts',(10.6887049019999,15.2,1.30249334199998));
#192659=CARTESIAN_POINT('Ctrl Pts',(10.6912493539999,15.2,1.30207460099999));
#192660=CARTESIAN_POINT('Ctrl Pts',(10.6937993929999,15.2,1.30165270599999));
#192661=CARTESIAN_POINT('Ctrl Pts',(10.6963550049999,15.2,1.30122764799999));
#192662=CARTESIAN_POINT('Ctrl Pts',(10.6989161759999,15.2,1.30079942299998));
#192663=CARTESIAN_POINT('Ctrl Pts',(10.7014828959999,15.2,1.30036802199998));
#192664=CARTESIAN_POINT('Ctrl Pts',(10.7040551489999,15.2,1.29993343899999));
#192665=CARTESIAN_POINT('Ctrl Pts',(10.7066329249999,15.2,1.29949566599999));
#192666=CARTESIAN_POINT('Ctrl Pts',(10.7092162099999,15.2,1.29905469699999));
#192667=CARTESIAN_POINT('Ctrl Pts',(10.7118049929999,15.2,1.29861052499999));
#192668=CARTESIAN_POINT('Ctrl Pts',(10.7143992589999,15.2,1.29816314299998));
#192669=CARTESIAN_POINT('Ctrl Pts',(10.7169989959999,15.2,1.29771254499999));
#192670=CARTESIAN_POINT('Ctrl Pts',(10.7196041929999,15.2,1.29725872299999));
#192671=CARTESIAN_POINT('Ctrl Pts',(10.7222148359999,15.2,1.29680166999998));
#192672=CARTESIAN_POINT('Ctrl Pts',(10.7248309119999,15.2,1.29634138299998));
#192673=CARTESIAN_POINT('Ctrl Pts',(10.7274524109999,15.2,1.29587785099998));
#192674=CARTESIAN_POINT('Ctrl Pts',(10.7300793179999,15.2,1.29541106899998));
#192675=CARTESIAN_POINT('Ctrl Pts',(10.7327116219999,15.2,1.29494102999999));
#192676=CARTESIAN_POINT('Ctrl Pts',(10.7353493089999,15.2,1.29446772899998));
#192677=CARTESIAN_POINT('Ctrl Pts',(10.7379923689999,15.2,1.29399115799998));
#192678=CARTESIAN_POINT('Ctrl Pts',(10.7406407879999,15.2,1.29351130999999));
#192679=CARTESIAN_POINT('Ctrl Pts',(10.7432945539999,15.2,1.29302817899998));
#192680=CARTESIAN_POINT('Ctrl Pts',(10.7459536549999,15.2,1.29254175999999));
#192681=CARTESIAN_POINT('Ctrl Pts',(10.7486180789999,15.2,1.29205204399998));
#192682=CARTESIAN_POINT('Ctrl Pts',(10.7512878129999,15.2,1.29155902599999));
#192683=CARTESIAN_POINT('Ctrl Pts',(10.7539628449999,15.2,1.29106269999999));
#192684=CARTESIAN_POINT('Ctrl Pts',(10.7566431619999,15.2,1.29056305799998));
#192685=CARTESIAN_POINT('Ctrl Pts',(10.7593287539999,15.2,1.29006009499999));
#192686=CARTESIAN_POINT('Ctrl Pts',(10.7620196059999,15.2,1.28955380499999));
#192687=CARTESIAN_POINT('Ctrl Pts',(10.7647157089999,15.2,1.28904418099999));
#192688=CARTESIAN_POINT('Ctrl Pts',(10.7674170489999,15.2,1.28853121599999));
#192689=CARTESIAN_POINT('Ctrl Pts',(10.7701236149999,15.2,1.28801490499999));
#192690=CARTESIAN_POINT('Ctrl Pts',(10.7728353919999,15.2,1.28749524099999));
#192691=CARTESIAN_POINT('Ctrl Pts',(10.7755523729999,15.2,1.28697221799999));
#192692=CARTESIAN_POINT('Ctrl Pts',(10.7782745419999,15.2,1.28644583099998));
#192693=CARTESIAN_POINT('Ctrl Pts',(10.7810018879999,15.2,1.28591607099999));
#192694=CARTESIAN_POINT('Ctrl Pts',(10.7837344009999,15.2,1.28538293399998));
#192695=CARTESIAN_POINT('Ctrl Pts',(10.7864720659999,15.2,1.28484641299998));
#192696=CARTESIAN_POINT('Ctrl Pts',(10.7892148729999,15.2,1.28430650299999));
#192697=CARTESIAN_POINT('Ctrl Pts',(10.7919628099999,15.2,1.28376319699999));
#192698=CARTESIAN_POINT('Ctrl Pts',(10.7947158649999,15.2,1.28321648999998));
#192699=CARTESIAN_POINT('Ctrl Pts',(10.7974740259999,15.2,1.28266637499999));
#192700=CARTESIAN_POINT('Ctrl Pts',(10.8002372809999,15.2,1.28211284599999));
#192701=CARTESIAN_POINT('Ctrl Pts',(10.8030056189999,15.2,1.28155589599999));
#192702=CARTESIAN_POINT('Ctrl Pts',(10.8057790279999,15.2,1.28099552199998));
#192703=CARTESIAN_POINT('Ctrl Pts',(10.8085574969999,15.2,1.28043171599999));
#192704=CARTESIAN_POINT('Ctrl Pts',(10.8113410119999,15.2,1.27986447199998));
#192705=CARTESIAN_POINT('Ctrl Pts',(10.8141295629999,15.2,1.27929378499998));
#192706=CARTESIAN_POINT('Ctrl Pts',(10.8169231379999,15.2,1.27871964799999));
#192707=CARTESIAN_POINT('Ctrl Pts',(10.8197217269999,15.2,1.27814205699998));
#192708=CARTESIAN_POINT('Ctrl Pts',(10.8225253159999,15.2,1.27756100399999));
#192709=CARTESIAN_POINT('Ctrl Pts',(10.8253338939999,15.2,1.27697648499999));
#192710=CARTESIAN_POINT('Ctrl Pts',(10.8281474499999,15.2,1.27638849299998));
#192711=CARTESIAN_POINT('Ctrl Pts',(10.8309659719999,15.2,1.27579702399998));
#192712=CARTESIAN_POINT('Ctrl Pts',(10.8337894499999,15.2,1.27520206999999));
#192713=CARTESIAN_POINT('Ctrl Pts',(10.8366178699999,15.2,1.27460362699999));
#192714=CARTESIAN_POINT('Ctrl Pts',(10.8394512219999,15.2,1.27400168799999));
#192715=CARTESIAN_POINT('Ctrl Pts',(10.8422894959999,15.2,1.27339624799998));
#192716=CARTESIAN_POINT('Ctrl Pts',(10.8451326779999,15.2,1.27278730199999));
#192717=CARTESIAN_POINT('Ctrl Pts',(10.8479807569999,15.2,1.27217484299999));
#192718=CARTESIAN_POINT('Ctrl Pts',(10.8508337229999,15.2,1.27155886699999));
#192719=CARTESIAN_POINT('Ctrl Pts',(10.8536915629999,15.2,1.27093936699998));
#192720=CARTESIAN_POINT('Ctrl Pts',(10.8565542679999,15.2,1.27031633899998));
#192721=CARTESIAN_POINT('Ctrl Pts',(10.8594218239999,15.2,1.26968977599998));
#192722=CARTESIAN_POINT('Ctrl Pts',(10.8622942209999,15.2,1.26905967299999));
#192723=CARTESIAN_POINT('Ctrl Pts',(10.8651714489999,15.2,1.26842602399998));
#192724=CARTESIAN_POINT('Ctrl Pts',(10.8680534959999,15.2,1.26778882499998));
#192725=CARTESIAN_POINT('Ctrl Pts',(10.8709403489999,15.2,1.26714806999999));
#192726=CARTESIAN_POINT('Ctrl Pts',(10.8738319979999,15.2,1.26650375199999));
#192727=CARTESIAN_POINT('Ctrl Pts',(10.8767284329999,15.2,1.26585586799999));
#192728=CARTESIAN_POINT('Ctrl Pts',(10.8796296409999,15.2,1.26520441099998));
#192729=CARTESIAN_POINT('Ctrl Pts',(10.8825356119999,15.2,1.26454937599998));
#192730=CARTESIAN_POINT('Ctrl Pts',(10.8854463339999,15.2,1.26389075699999));
#192731=CARTESIAN_POINT('Ctrl Pts',(10.8883617979999,15.2,1.26322854999998));
#192732=CARTESIAN_POINT('Ctrl Pts',(10.8912819899999,15.2,1.26256274999998));
#192733=CARTESIAN_POINT('Ctrl Pts',(10.8942069009999,15.2,1.26189335099999));
#192734=CARTESIAN_POINT('Ctrl Pts',(10.8971365199999,15.2,1.26122034599998));
#192735=CARTESIAN_POINT('Ctrl Pts',(10.9000708339999,15.2,1.26054373299999));
#192736=CARTESIAN_POINT('Ctrl Pts',(10.9030098339999,15.2,1.25986350499999));
#192737=CARTESIAN_POINT('Ctrl Pts',(10.9059535079999,15.2,1.25917965599998));
#192738=CARTESIAN_POINT('Ctrl Pts',(10.9089018469999,15.2,1.25849218299999));
#192739=CARTESIAN_POINT('Ctrl Pts',(10.9118548369999,15.2,1.25780107899998));
#192740=CARTESIAN_POINT('Ctrl Pts',(10.9148124699999,15.2,1.25710633999998));
#192741=CARTESIAN_POINT('Ctrl Pts',(10.9177747329999,15.2,1.25640795999999));
#192742=CARTESIAN_POINT('Ctrl Pts',(10.9207416159999,15.2,1.25570593399999));
#192743=CARTESIAN_POINT('Ctrl Pts',(10.9237131089999,15.2,1.25500025699999));
#192744=CARTESIAN_POINT('Ctrl Pts',(10.9266891999999,15.2,1.25429092499999));
#192745=CARTESIAN_POINT('Ctrl Pts',(10.9296698779999,15.2,1.25357793199999));
#192746=CARTESIAN_POINT('Ctrl Pts',(10.9326551319999,15.2,1.25286127399999));
#192747=CARTESIAN_POINT('Ctrl Pts',(10.9356449539999,15.2,1.25214094399999));
#192748=CARTESIAN_POINT('Ctrl Pts',(10.9386393289999,15.2,1.25141693899999));
#192749=CARTESIAN_POINT('Ctrl Pts',(10.9416382509999,15.2,1.25068925199999));
#192750=CARTESIAN_POINT('Ctrl Pts',(10.9446417049999,15.2,1.24995787999998));
#192751=CARTESIAN_POINT('Ctrl Pts',(10.9476496829999,15.2,1.24922281699998));
#192752=CARTESIAN_POINT('Ctrl Pts',(10.9506621729999,15.2,1.24848405899999));
#192753=CARTESIAN_POINT('Ctrl Pts',(10.9536791659999,15.2,1.24774160099999));
#192754=CARTESIAN_POINT('Ctrl Pts',(10.9567006489999,15.2,1.24699543599998));
#192755=CARTESIAN_POINT('Ctrl Pts',(10.9597266129999,15.2,1.24624556199999));
#192756=CARTESIAN_POINT('Ctrl Pts',(10.9627570469999,15.2,1.24549197299999));
#192757=CARTESIAN_POINT('Ctrl Pts',(10.9657919419999,15.2,1.24473466399999));
#192758=CARTESIAN_POINT('Ctrl Pts',(10.9688312839999,15.2,1.24397363099999));
#192759=CARTESIAN_POINT('Ctrl Pts',(10.9718750649999,15.2,1.24320886799998));
#192760=CARTESIAN_POINT('Ctrl Pts',(10.9749232749999,15.2,1.24244037199999));
#192761=CARTESIAN_POINT('Ctrl Pts',(10.9779759009999,15.2,1.24166813599999));
#192762=CARTESIAN_POINT('Ctrl Pts',(10.9810329339999,15.2,1.24089215599998));
#192763=CARTESIAN_POINT('Ctrl Pts',(10.9840943639999,15.2,1.24011242999998));
#192764=CARTESIAN_POINT('Ctrl Pts',(10.9871601809999,15.2,1.23932894899998));
#192765=CARTESIAN_POINT('Ctrl Pts',(10.9902303719999,15.2,1.23854171099998));
#192766=CARTESIAN_POINT('Ctrl Pts',(10.9933049299999,15.2,1.23775071099999));
#192767=CARTESIAN_POINT('Ctrl Pts',(10.9963838419999,15.2,1.23695594399999));
#192768=CARTESIAN_POINT('Ctrl Pts',(10.9994670979999,15.2,1.23615740499998));
#192769=CARTESIAN_POINT('Ctrl Pts',(11.0025546899999,15.2,1.23535509099999));
#192770=CARTESIAN_POINT('Ctrl Pts',(11.0056466049999,15.2,1.23454899599999));
#192771=CARTESIAN_POINT('Ctrl Pts',(11.0087428319999,15.2,1.23373911599999));
#192772=CARTESIAN_POINT('Ctrl Pts',(11.0118433639999,15.2,1.23292544599999));
#192773=CARTESIAN_POINT('Ctrl Pts',(11.0149481889999,15.2,1.23210798199999));
#192774=CARTESIAN_POINT('Ctrl Pts',(11.0180572959999,15.2,1.23128671899998));
#192775=CARTESIAN_POINT('Ctrl Pts',(11.0211706759999,15.2,1.23046165299999));
#192776=CARTESIAN_POINT('Ctrl Pts',(11.0242883189999,15.2,1.22963277999999));
#192777=CARTESIAN_POINT('Ctrl Pts',(11.0274102129999,15.2,1.22880009299998));
#192778=CARTESIAN_POINT('Ctrl Pts',(11.0305363499999,15.2,1.22796359099999));
#192779=CARTESIAN_POINT('Ctrl Pts',(11.0336667189999,15.2,1.22712326699999));
#192780=CARTESIAN_POINT('Ctrl Pts',(11.0368013089999,15.2,1.22627911899999));
#192781=CARTESIAN_POINT('Ctrl Pts',(11.0399401109999,15.2,1.22543113999999));
#192782=CARTESIAN_POINT('Ctrl Pts',(11.0430831139999,15.2,1.22457932799998));
#192783=CARTESIAN_POINT('Ctrl Pts',(11.0462303079999,15.2,1.22372367599999));
#192784=CARTESIAN_POINT('Ctrl Pts',(11.0493816829999,15.2,1.22286418199999));
#192785=CARTESIAN_POINT('Ctrl Pts',(11.0525372299999,15.2,1.22200084099998));
#192786=CARTESIAN_POINT('Ctrl Pts',(11.0556969379999,15.2,1.22113364899999));
#192787=CARTESIAN_POINT('Ctrl Pts',(11.0588607969999,15.2,1.22026260099998));
#192788=CARTESIAN_POINT('Ctrl Pts',(11.0620287979999,15.2,1.21938769199998));
#192789=CARTESIAN_POINT('Ctrl Pts',(11.0652009289999,15.2,1.21850892099999));
#192790=CARTESIAN_POINT('Ctrl Pts',(11.0683771819999,15.2,1.21762627999999));
#192791=CARTESIAN_POINT('Ctrl Pts',(11.0715575449999,15.2,1.21673976599999));
#192792=CARTESIAN_POINT('Ctrl Pts',(11.0747420099999,15.2,1.21584937499998));
#192793=CARTESIAN_POINT('Ctrl Pts',(11.0779305669999,15.2,1.21495510399999));
#192794=CARTESIAN_POINT('Ctrl Pts',(11.0811232049999,15.2,1.21405694799999));
#192795=CARTESIAN_POINT('Ctrl Pts',(11.0843199139999,15.2,1.21315490199999));
#192796=CARTESIAN_POINT('Ctrl Pts',(11.0875206859999,15.2,1.21224896199998));
#192797=CARTESIAN_POINT('Ctrl Pts',(11.0907255089999,15.2,1.21133912599999));
#192798=CARTESIAN_POINT('Ctrl Pts',(11.0939343729999,15.2,1.21042538699998));
#192799=CARTESIAN_POINT('Ctrl Pts',(11.0971472699999,15.2,1.20950774199999));
#192800=CARTESIAN_POINT('Ctrl Pts',(11.1003641889999,15.2,1.20858618799998));
#192801=CARTESIAN_POINT('Ctrl Pts',(11.1035851209999,15.2,1.20766071999999));
#192802=CARTESIAN_POINT('Ctrl Pts',(11.1068100549999,15.2,1.20673133399999));
#192803=CARTESIAN_POINT('Ctrl Pts',(11.1100389819999,15.2,1.20579802499998));
#192804=CARTESIAN_POINT('Ctrl Pts',(11.1132718939999,15.2,1.20486079099999));
#192805=CARTESIAN_POINT('Ctrl Pts',(11.1165087779999,15.2,1.20391962699999));
#192806=CARTESIAN_POINT('Ctrl Pts',(11.1197496249999,15.2,1.20297452899999));
#192807=CARTESIAN_POINT('Ctrl Pts',(11.1229944269999,15.2,1.20202549299998));
#192808=CARTESIAN_POINT('Ctrl Pts',(11.1262431739999,15.2,1.20107251499999));
#192809=CARTESIAN_POINT('Ctrl Pts',(11.1294958549999,15.2,1.20011559099999));
#192810=CARTESIAN_POINT('Ctrl Pts',(11.1327524619999,15.2,1.19915471699999));
#192811=CARTESIAN_POINT('Ctrl Pts',(11.1360129839999,15.2,1.19818988999999));
#192812=CARTESIAN_POINT('Ctrl Pts',(11.1392774109999,15.2,1.19722110599998));
#192813=CARTESIAN_POINT('Ctrl Pts',(11.1425457349999,15.2,1.19624835999999));
#192814=CARTESIAN_POINT('Ctrl Pts',(11.1458179459999,15.2,1.19527164899999));
#192815=CARTESIAN_POINT('Ctrl Pts',(11.1490940329999,15.2,1.19429096899998));
#192816=CARTESIAN_POINT('Ctrl Pts',(11.1523739879999,15.2,1.19330631599999));
#192817=CARTESIAN_POINT('Ctrl Pts',(11.1556577999999,15.2,1.19231768599999));
#192818=CARTESIAN_POINT('Ctrl Pts',(11.1589454619999,15.2,1.19132507599998));
#192819=CARTESIAN_POINT('Ctrl Pts',(11.1622369629999,15.2,1.19032848099998));
#192820=CARTESIAN_POINT('Ctrl Pts',(11.1655322919999,15.2,1.18932789899999));
#192821=CARTESIAN_POINT('Ctrl Pts',(11.1688314409999,15.2,1.18832332399998));
#192822=CARTESIAN_POINT('Ctrl Pts',(11.1721344009999,15.2,1.18731475499999));
#192823=CARTESIAN_POINT('Ctrl Pts',(11.1754411629999,15.2,1.18630218499999));
#192824=CARTESIAN_POINT('Ctrl Pts',(11.1787517149999,15.2,1.18528561399998));
#192825=CARTESIAN_POINT('Ctrl Pts',(11.1820660499999,15.2,1.18426503499999));
#192826=CARTESIAN_POINT('Ctrl Pts',(11.1853841569999,15.2,1.18324044599999));
#192827=CARTESIAN_POINT('Ctrl Pts',(11.1887060269999,15.2,1.18221184299999));
#192828=CARTESIAN_POINT('Ctrl Pts',(11.1920316519999,15.2,1.18117922199998));
#192829=CARTESIAN_POINT('Ctrl Pts',(11.1953610209999,15.2,1.18014258099999));
#192830=CARTESIAN_POINT('Ctrl Pts',(11.1986941249999,15.2,1.17910191499998));
#192831=CARTESIAN_POINT('Ctrl Pts',(11.2020309559999,15.2,1.17805721999999));
#192832=CARTESIAN_POINT('Ctrl Pts',(11.2053715019999,15.2,1.17700849199998));
#192833=CARTESIAN_POINT('Ctrl Pts',(11.2087157559999,15.2,1.17595572999999));
#192834=CARTESIAN_POINT('Ctrl Pts',(11.2120637079999,15.2,1.17489892799998));
#192835=CARTESIAN_POINT('Ctrl Pts',(11.2154153489999,15.2,1.17383808299998));
#192836=CARTESIAN_POINT('Ctrl Pts',(11.2187706689999,15.2,1.17277319199999));
#192837=CARTESIAN_POINT('Ctrl Pts',(11.2221296589999,15.2,1.17170425099999));
#192838=CARTESIAN_POINT('Ctrl Pts',(11.2254923089999,15.2,1.17063125699998));
#192839=CARTESIAN_POINT('Ctrl Pts',(11.2288586119999,15.2,1.16955420599998));
#192840=CARTESIAN_POINT('Ctrl Pts',(11.2322285569999,15.2,1.16847309399999));
#192841=CARTESIAN_POINT('Ctrl Pts',(11.2356021349999,15.2,1.16738791999999));
#192842=CARTESIAN_POINT('Ctrl Pts',(11.2389793369999,15.2,1.16629867799999));
#192843=CARTESIAN_POINT('Ctrl Pts',(11.2423601539999,15.2,1.16520536499999));
#192844=CARTESIAN_POINT('Ctrl Pts',(11.2457445769999,15.2,1.16410797799999));
#192845=CARTESIAN_POINT('Ctrl Pts',(11.2491325969999,15.2,1.16300651299999));
#192846=CARTESIAN_POINT('Ctrl Pts',(11.2525242039999,15.2,1.16190096799999));
#192847=CARTESIAN_POINT('Ctrl Pts',(11.2559193889999,15.2,1.16079133899999));
#192848=CARTESIAN_POINT('Ctrl Pts',(11.2593181439999,15.2,1.15967762199999));
#192849=CARTESIAN_POINT('Ctrl Pts',(11.2627204589999,15.2,1.15855981299998));
#192850=CARTESIAN_POINT('Ctrl Pts',(11.2661263239999,15.2,1.15743791099999));
#192851=CARTESIAN_POINT('Ctrl Pts',(11.2695357319999,15.2,1.15631191099999));
#192852=CARTESIAN_POINT('Ctrl Pts',(11.2729486729999,15.2,1.15518180999999));
#192853=CARTESIAN_POINT('Ctrl Pts',(11.2763651379999,15.2,1.15404760499999));
#192854=CARTESIAN_POINT('Ctrl Pts',(11.2797851169999,15.2,1.15290929199999));
#192855=CARTESIAN_POINT('Ctrl Pts',(11.2832086039999,15.2,1.15176686799999));
#192856=CARTESIAN_POINT('Ctrl Pts',(11.2866355859999,15.2,1.15062032999999));
#192857=CARTESIAN_POINT('Ctrl Pts',(11.2900660559999,15.2,1.14946967499999));
#192858=CARTESIAN_POINT('Ctrl Pts',(11.2935000059999,15.2,1.14831489899998));
#192859=CARTESIAN_POINT('Ctrl Pts',(11.2969374249999,15.2,1.14715599999998));
#192860=CARTESIAN_POINT('Ctrl Pts',(11.3003783059999,15.2,1.14599297299999));
#192861=CARTESIAN_POINT('Ctrl Pts',(11.3038226389999,15.2,1.14482581599999));
#192862=CARTESIAN_POINT('Ctrl Pts',(11.3072704139999,15.2,1.14365452599999));
#192863=CARTESIAN_POINT('Ctrl Pts',(11.3107216239999,15.2,1.14247909899999));
#192864=CARTESIAN_POINT('Ctrl Pts',(11.3141762599999,15.2,1.14129953199999));
#192865=CARTESIAN_POINT('Ctrl Pts',(11.3176343119999,15.2,1.14011582299999));
#192866=CARTESIAN_POINT('Ctrl Pts',(11.3210957719999,15.2,1.13892796799998));
#192867=CARTESIAN_POINT('Ctrl Pts',(11.3245606299999,15.2,1.13773596199998));
#192868=CARTESIAN_POINT('Ctrl Pts',(11.3280288789999,15.2,1.13653980499999));
#192869=CARTESIAN_POINT('Ctrl Pts',(11.3315005099999,15.2,1.13533949399999));
#192870=CARTESIAN_POINT('Ctrl Pts',(11.3349755119999,15.2,1.13413502399998));
#192871=CARTESIAN_POINT('Ctrl Pts',(11.3384538779999,15.2,1.13292639099999));
#192872=CARTESIAN_POINT('Ctrl Pts',(11.3419355979999,15.2,1.13171359399999));
#192873=CARTESIAN_POINT('Ctrl Pts',(11.3454206639999,15.2,1.13049662999999));
#192874=CARTESIAN_POINT('Ctrl Pts',(11.3489090669999,15.2,1.12927549499998));
#192875=CARTESIAN_POINT('Ctrl Pts',(11.3524007989999,15.2,1.12805018499999));
#192876=CARTESIAN_POINT('Ctrl Pts',(11.3558958509999,15.2,1.12682069999999));
#192877=CARTESIAN_POINT('Ctrl Pts',(11.3593942139999,15.2,1.12558703499999));
#192878=CARTESIAN_POINT('Ctrl Pts',(11.3628958789999,15.2,1.12434918799998));
#192879=CARTESIAN_POINT('Ctrl Pts',(11.3664008399999,15.2,1.12310715499999));
#192880=CARTESIAN_POINT('Ctrl Pts',(11.3699090849999,15.2,1.12186093299998));
#192881=CARTESIAN_POINT('Ctrl Pts',(11.3734206059999,15.2,1.12061051999999));
#192882=CARTESIAN_POINT('Ctrl Pts',(11.3769353939999,15.2,1.11935591199999));
#192883=CARTESIAN_POINT('Ctrl Pts',(11.3804534399999,15.2,1.11809710599998));
#192884=CARTESIAN_POINT('Ctrl Pts',(11.3839747349999,15.2,1.11683410099999));
#192885=CARTESIAN_POINT('Ctrl Pts',(11.3874992709999,15.2,1.11556689099999));
#192886=CARTESIAN_POINT('Ctrl Pts',(11.3910270409999,15.2,1.11429547399998));
#192887=CARTESIAN_POINT('Ctrl Pts',(11.3945580339999,15.2,1.11301984899999));
#192888=CARTESIAN_POINT('Ctrl Pts',(11.3980922449999,15.2,1.11174001299998));
#192889=CARTESIAN_POINT('Ctrl Pts',(11.4016296639999,15.2,1.11045596299999));
#192890=CARTESIAN_POINT('Ctrl Pts',(11.4051702859999,15.2,1.10916769599998));
#192891=CARTESIAN_POINT('Ctrl Pts',(11.4087140989999,15.2,1.10787520999999));
#192892=CARTESIAN_POINT('Ctrl Pts',(11.4122610939999,15.2,1.10657849999999));
#192893=CARTESIAN_POINT('Ctrl Pts',(11.4158112619999,15.2,1.10527756499998));
#192894=CARTESIAN_POINT('Ctrl Pts',(11.4193645909999,15.2,1.10397239899998));
#192895=CARTESIAN_POINT('Ctrl Pts',(11.4229210689999,15.2,1.10266299899999));
#192896=CARTESIAN_POINT('Ctrl Pts',(11.4264806909999,15.2,1.10134936399998));
#192897=CARTESIAN_POINT('Ctrl Pts',(11.4300434449999,15.2,1.10003148899999));
#192898=CARTESIAN_POINT('Ctrl Pts',(11.4336093279999,15.2,1.09870937299998));
#192899=CARTESIAN_POINT('Ctrl Pts',(11.4371783349999,15.2,1.09738301699998));
#192900=CARTESIAN_POINT('Ctrl Pts',(11.4407504639999,15.2,1.09605241699999));
#192901=CARTESIAN_POINT('Ctrl Pts',(11.4436106639999,15.2,1.09498454299999));
#192902=CARTESIAN_POINT('Ctrl Pts',(11.4457572179999,15.2,1.09418172899999));
#192903=CARTESIAN_POINT('Ctrl Pts',(11.4471888789999,15.2,1.09364567099998));
#192904=CARTESIAN_POINT('Ctrl Pts',(11.4479048649999,15.2,1.09337742899998));
#192905=CARTESIAN_POINT('Ctrl Pts',(10.3708900239999,15.2,0.292001928999985));
#192906=CARTESIAN_POINT('Ctrl Pts',(10.3708900239999,11.6,0.292001928999985));
#192907=CARTESIAN_POINT('Ctrl Pts',(10.3710632449999,15.2,0.292021795999986));
#192908=CARTESIAN_POINT('Ctrl Pts',(10.3710632449999,11.6,0.292021795999986));
#192909=CARTESIAN_POINT('Ctrl Pts',(10.3714157299999,15.2,0.292062309999985));
#192910=CARTESIAN_POINT('Ctrl Pts',(10.3714157299999,11.6,0.292062309999985));
#192911=CARTESIAN_POINT('Ctrl Pts',(10.3719497989999,15.2,0.292123961999984));
#192912=CARTESIAN_POINT('Ctrl Pts',(10.3719497989999,11.6,0.292123961999983));
#192913=CARTESIAN_POINT('Ctrl Pts',(10.3726691759999,15.2,0.292207547999985));
#192914=CARTESIAN_POINT('Ctrl Pts',(10.3726691759999,11.6,0.292207547999985));
#192915=CARTESIAN_POINT('Ctrl Pts',(10.3735789749999,15.2,0.292314179999984));
#192916=CARTESIAN_POINT('Ctrl Pts',(10.3735789749999,11.6,0.292314179999984));
#192917=CARTESIAN_POINT('Ctrl Pts',(10.3745034109999,15.2,0.292423468999985));
#192918=CARTESIAN_POINT('Ctrl Pts',(10.3745034109999,11.6,0.292423468999985));
#192919=CARTESIAN_POINT('Ctrl Pts',(10.3754371839999,15.2,0.292534811999987));
#192920=CARTESIAN_POINT('Ctrl Pts',(10.3754371839999,11.6,0.292534811999987));
#192921=CARTESIAN_POINT('Ctrl Pts',(10.3763802659999,15.2,0.292648223999983));
#192922=CARTESIAN_POINT('Ctrl Pts',(10.3763802659999,11.6,0.292648223999982));
#192923=CARTESIAN_POINT('Ctrl Pts',(10.3773326269999,15.2,0.292763717999982));
#192924=CARTESIAN_POINT('Ctrl Pts',(10.3773326269999,11.6,0.292763717999982));
#192925=CARTESIAN_POINT('Ctrl Pts',(10.3782942399999,15.2,0.292881309999986));
#192926=CARTESIAN_POINT('Ctrl Pts',(10.3782942399999,11.6,0.292881309999986));
#192927=CARTESIAN_POINT('Ctrl Pts',(10.3792650739999,15.2,0.293001014999987));
#192928=CARTESIAN_POINT('Ctrl Pts',(10.3792650739999,11.6,0.293001014999987));
#192929=CARTESIAN_POINT('Ctrl Pts',(10.3802451029999,15.2,0.293122846999987));
#192930=CARTESIAN_POINT('Ctrl Pts',(10.3802451029999,11.6,0.293122846999986));
#192931=CARTESIAN_POINT('Ctrl Pts',(10.3812342959999,15.2,0.293246819999986));
#192932=CARTESIAN_POINT('Ctrl Pts',(10.3812342959999,11.6,0.293246819999986));
#192933=CARTESIAN_POINT('Ctrl Pts',(10.3822326279999,15.2,0.293372949999986));
#192934=CARTESIAN_POINT('Ctrl Pts',(10.3822326279999,11.6,0.293372949999986));
#192935=CARTESIAN_POINT('Ctrl Pts',(10.3832400689999,15.2,0.293501248999988));
#192936=CARTESIAN_POINT('Ctrl Pts',(10.3832400689999,11.6,0.293501248999987));
#192937=CARTESIAN_POINT('Ctrl Pts',(10.3842565909999,15.2,0.293631731999984));
#192938=CARTESIAN_POINT('Ctrl Pts',(10.3842565909999,11.6,0.293631731999983));
#192939=CARTESIAN_POINT('Ctrl Pts',(10.3852821679999,15.2,0.293764413999984));
#192940=CARTESIAN_POINT('Ctrl Pts',(10.3852821679999,11.6,0.293764413999984));
#192941=CARTESIAN_POINT('Ctrl Pts',(10.3863167709999,15.2,0.293899307999985));
#192942=CARTESIAN_POINT('Ctrl Pts',(10.3863167709999,11.6,0.293899307999985));
#192943=CARTESIAN_POINT('Ctrl Pts',(10.3873603719999,15.2,0.294036427999984));
#192944=CARTESIAN_POINT('Ctrl Pts',(10.3873603719999,11.6,0.294036427999984));
#192945=CARTESIAN_POINT('Ctrl Pts',(10.3884129439999,15.2,0.294175786999986));
#192946=CARTESIAN_POINT('Ctrl Pts',(10.3884129439999,11.6,0.294175786999986));
#192947=CARTESIAN_POINT('Ctrl Pts',(10.3894744609999,15.2,0.294317400999984));
#192948=CARTESIAN_POINT('Ctrl Pts',(10.3894744609999,11.6,0.294317400999983));
#192949=CARTESIAN_POINT('Ctrl Pts',(10.3905448939999,15.2,0.294461282999983));
#192950=CARTESIAN_POINT('Ctrl Pts',(10.3905448939999,11.6,0.294461282999982));
#192951=CARTESIAN_POINT('Ctrl Pts',(10.3916242179999,15.2,0.294607444999984));
#192952=CARTESIAN_POINT('Ctrl Pts',(10.3916242179999,11.6,0.294607444999983));
#192953=CARTESIAN_POINT('Ctrl Pts',(10.3927124039999,15.2,0.294755900999988));
#192954=CARTESIAN_POINT('Ctrl Pts',(10.3927124039999,11.6,0.294755900999987));
#192955=CARTESIAN_POINT('Ctrl Pts',(10.3938094269999,15.2,0.294906666999988));
#192956=CARTESIAN_POINT('Ctrl Pts',(10.3938094269999,11.6,0.294906666999987));
#192957=CARTESIAN_POINT('Ctrl Pts',(10.3949152589999,15.2,0.295059752999984));
#192958=CARTESIAN_POINT('Ctrl Pts',(10.3949152589999,11.6,0.295059752999984));
#192959=CARTESIAN_POINT('Ctrl Pts',(10.3960298749999,15.2,0.295215173999988));
#192960=CARTESIAN_POINT('Ctrl Pts',(10.3960298749999,11.6,0.295215173999987));
#192961=CARTESIAN_POINT('Ctrl Pts',(10.3971532469999,15.2,0.295372941999985));
#192962=CARTESIAN_POINT('Ctrl Pts',(10.3971532469999,11.6,0.295372941999985));
#192963=CARTESIAN_POINT('Ctrl Pts',(10.3982853499999,15.2,0.295533071999987));
#192964=CARTESIAN_POINT('Ctrl Pts',(10.3982853499999,11.6,0.295533071999987));
#192965=CARTESIAN_POINT('Ctrl Pts',(10.3994261559999,15.2,0.295695575999986));
#192966=CARTESIAN_POINT('Ctrl Pts',(10.3994261559999,11.6,0.295695575999985));
#192967=CARTESIAN_POINT('Ctrl Pts',(10.4005756419999,15.2,0.295860467999987));
#192968=CARTESIAN_POINT('Ctrl Pts',(10.4005756419999,11.6,0.295860467999986));
#192969=CARTESIAN_POINT('Ctrl Pts',(10.4017337789999,15.2,0.296027758999986));
#192970=CARTESIAN_POINT('Ctrl Pts',(10.4017337789999,11.6,0.296027758999986));
#192971=CARTESIAN_POINT('Ctrl Pts',(10.4029005419999,15.2,0.296197463999985));
#192972=CARTESIAN_POINT('Ctrl Pts',(10.4029005419999,11.6,0.296197463999985));
#192973=CARTESIAN_POINT('Ctrl Pts',(10.4040759059999,15.2,0.296369593999986));
#192974=CARTESIAN_POINT('Ctrl Pts',(10.4040759059999,11.6,0.296369593999985));
#192975=CARTESIAN_POINT('Ctrl Pts',(10.4052598449999,15.2,0.296544161999983));
#192976=CARTESIAN_POINT('Ctrl Pts',(10.4052598449999,11.6,0.296544161999983));
#192977=CARTESIAN_POINT('Ctrl Pts',(10.4064523339999,15.2,0.296721180999988));
#192978=CARTESIAN_POINT('Ctrl Pts',(10.4064523339999,11.6,0.296721180999988));
#192979=CARTESIAN_POINT('Ctrl Pts',(10.4076533469999,15.2,0.296900664999988));
#192980=CARTESIAN_POINT('Ctrl Pts',(10.4076533469999,11.6,0.296900664999988));
#192981=CARTESIAN_POINT('Ctrl Pts',(10.4088628589999,15.2,0.297082624999985));
#192982=CARTESIAN_POINT('Ctrl Pts',(10.4088628589999,11.6,0.297082624999984));
#192983=CARTESIAN_POINT('Ctrl Pts',(10.4100808439999,15.2,0.297267072999983));
#192984=CARTESIAN_POINT('Ctrl Pts',(10.4100808439999,11.6,0.297267072999982));
#192985=CARTESIAN_POINT('Ctrl Pts',(10.4113072789999,15.2,0.297454021999983));
#192986=CARTESIAN_POINT('Ctrl Pts',(10.4113072789999,11.6,0.297454021999983));
#192987=CARTESIAN_POINT('Ctrl Pts',(10.4125421359999,15.2,0.297643483999988));
#192988=CARTESIAN_POINT('Ctrl Pts',(10.4125421359999,11.6,0.297643483999987));
#192989=CARTESIAN_POINT('Ctrl Pts',(10.4137853929999,15.2,0.297835471999988));
#192990=CARTESIAN_POINT('Ctrl Pts',(10.4137853929999,11.6,0.297835471999987));
#192991=CARTESIAN_POINT('Ctrl Pts',(10.4150370239999,15.2,0.298029997999985));
#192992=CARTESIAN_POINT('Ctrl Pts',(10.4150370239999,11.6,0.298029997999984));
#192993=CARTESIAN_POINT('Ctrl Pts',(10.4162970039999,15.2,0.298227073999984));
#192994=CARTESIAN_POINT('Ctrl Pts',(10.4162970039999,11.6,0.298227073999983));
#192995=CARTESIAN_POINT('Ctrl Pts',(10.4175653089999,15.2,0.298426710999986));
#192996=CARTESIAN_POINT('Ctrl Pts',(10.4175653089999,11.6,0.298426710999986));
#192997=CARTESIAN_POINT('Ctrl Pts',(10.4188419149999,15.2,0.298628921999988));
#192998=CARTESIAN_POINT('Ctrl Pts',(10.4188419149999,11.6,0.298628921999988));
#192999=CARTESIAN_POINT('Ctrl Pts',(10.4201267969999,15.2,0.298833718999987));
#193000=CARTESIAN_POINT('Ctrl Pts',(10.4201267969999,11.6,0.298833718999986));
#193001=CARTESIAN_POINT('Ctrl Pts',(10.4214199299999,15.2,0.299041113999987));
#193002=CARTESIAN_POINT('Ctrl Pts',(10.4214199299999,11.6,0.299041113999987));
#193003=CARTESIAN_POINT('Ctrl Pts',(10.4227212909999,15.2,0.299251117999986));
#193004=CARTESIAN_POINT('Ctrl Pts',(10.4227212909999,11.6,0.299251117999985));
#193005=CARTESIAN_POINT('Ctrl Pts',(10.4240308559999,15.2,0.299463742999984));
#193006=CARTESIAN_POINT('Ctrl Pts',(10.4240308559999,11.6,0.299463742999983));
#193007=CARTESIAN_POINT('Ctrl Pts',(10.4253486009999,15.2,0.299679001999986));
#193008=CARTESIAN_POINT('Ctrl Pts',(10.4253486009999,11.6,0.299679001999986));
#193009=CARTESIAN_POINT('Ctrl Pts',(10.4266745019999,15.2,0.299896902999985));
#193010=CARTESIAN_POINT('Ctrl Pts',(10.4266745019999,11.6,0.299896902999985));
#193011=CARTESIAN_POINT('Ctrl Pts',(10.4280085349999,15.2,0.300117460999987));
#193012=CARTESIAN_POINT('Ctrl Pts',(10.4280085349999,11.6,0.300117460999986));
#193013=CARTESIAN_POINT('Ctrl Pts',(10.4293506769999,15.2,0.300340685999987));
#193014=CARTESIAN_POINT('Ctrl Pts',(10.4293506769999,11.6,0.300340685999986));
#193015=CARTESIAN_POINT('Ctrl Pts',(10.4307009019999,15.2,0.300566589999987));
#193016=CARTESIAN_POINT('Ctrl Pts',(10.4307009019999,11.6,0.300566589999986));
#193017=CARTESIAN_POINT('Ctrl Pts',(10.4320591909999,15.2,0.300795183999987));
#193018=CARTESIAN_POINT('Ctrl Pts',(10.4320591909999,11.6,0.300795183999986));
#193019=CARTESIAN_POINT('Ctrl Pts',(10.4334255159999,15.2,0.301026479999984));
#193020=CARTESIAN_POINT('Ctrl Pts',(10.4334255159999,11.6,0.301026479999984));
#193021=CARTESIAN_POINT('Ctrl Pts',(10.4347998569999,15.2,0.301260487999984));
#193022=CARTESIAN_POINT('Ctrl Pts',(10.4347998569999,11.6,0.301260487999983));
#193023=CARTESIAN_POINT('Ctrl Pts',(10.4361821889999,15.2,0.301497219999987));
#193024=CARTESIAN_POINT('Ctrl Pts',(10.4361821889999,11.6,0.301497219999986));
#193025=CARTESIAN_POINT('Ctrl Pts',(10.4375724899999,15.2,0.301736685999985));
#193026=CARTESIAN_POINT('Ctrl Pts',(10.4375724899999,11.6,0.301736685999984));
#193027=CARTESIAN_POINT('Ctrl Pts',(10.4389707379999,15.2,0.301978897999984));
#193028=CARTESIAN_POINT('Ctrl Pts',(10.4389707379999,11.6,0.301978897999983));
#193029=CARTESIAN_POINT('Ctrl Pts',(10.4403769079999,15.2,0.302223867999984));
#193030=CARTESIAN_POINT('Ctrl Pts',(10.4403769079999,11.6,0.302223867999984));
#193031=CARTESIAN_POINT('Ctrl Pts',(10.4417909759999,15.2,0.302471604999983));
#193032=CARTESIAN_POINT('Ctrl Pts',(10.4417909759999,11.6,0.302471604999983));
#193033=CARTESIAN_POINT('Ctrl Pts',(10.4432129229999,15.2,0.302722120999985));
#193034=CARTESIAN_POINT('Ctrl Pts',(10.4432129229999,11.6,0.302722120999985));
#193035=CARTESIAN_POINT('Ctrl Pts',(10.4446427239999,15.2,0.302975425999983));
#193036=CARTESIAN_POINT('Ctrl Pts',(10.4446427239999,11.6,0.302975425999982));
#193037=CARTESIAN_POINT('Ctrl Pts',(10.4460803579999,15.2,0.303231530999986));
#193038=CARTESIAN_POINT('Ctrl Pts',(10.4460803579999,11.6,0.303231530999985));
#193039=CARTESIAN_POINT('Ctrl Pts',(10.4475257999999,15.2,0.303490447999986));
#193040=CARTESIAN_POINT('Ctrl Pts',(10.4475257999999,11.6,0.303490447999985));
#193041=CARTESIAN_POINT('Ctrl Pts',(10.4489790289999,15.2,0.303752186999984));
#193042=CARTESIAN_POINT('Ctrl Pts',(10.4489790289999,11.6,0.303752186999983));
#193043=CARTESIAN_POINT('Ctrl Pts',(10.4504400239999,15.2,0.304016756999985));
#193044=CARTESIAN_POINT('Ctrl Pts',(10.4504400239999,11.6,0.304016756999985));
#193045=CARTESIAN_POINT('Ctrl Pts',(10.4519087609999,15.2,0.304284169999987));
#193046=CARTESIAN_POINT('Ctrl Pts',(10.4519087609999,11.6,0.304284169999986));
#193047=CARTESIAN_POINT('Ctrl Pts',(10.4533852189999,15.2,0.304554435999984));
#193048=CARTESIAN_POINT('Ctrl Pts',(10.4533852189999,11.6,0.304554435999984));
#193049=CARTESIAN_POINT('Ctrl Pts',(10.4548693739999,15.2,0.304827565999983));
#193050=CARTESIAN_POINT('Ctrl Pts',(10.4548693739999,11.6,0.304827565999983));
#193051=CARTESIAN_POINT('Ctrl Pts',(10.4563612069999,15.2,0.305103569999985));
#193052=CARTESIAN_POINT('Ctrl Pts',(10.4563612069999,11.6,0.305103569999984));
#193053=CARTESIAN_POINT('Ctrl Pts',(10.4578606949999,15.2,0.305382457999985));
#193054=CARTESIAN_POINT('Ctrl Pts',(10.4578606949999,11.6,0.305382457999985));
#193055=CARTESIAN_POINT('Ctrl Pts',(10.4593678149999,15.2,0.305664240999985));
#193056=CARTESIAN_POINT('Ctrl Pts',(10.4593678149999,11.6,0.305664240999985));
#193057=CARTESIAN_POINT('Ctrl Pts',(10.4608825449999,15.2,0.305948927999986));
#193058=CARTESIAN_POINT('Ctrl Pts',(10.4608825449999,11.6,0.305948927999986));
#193059=CARTESIAN_POINT('Ctrl Pts',(10.4624048659999,15.2,0.306236530999984));
#193060=CARTESIAN_POINT('Ctrl Pts',(10.4624048659999,11.6,0.306236530999983));
#193061=CARTESIAN_POINT('Ctrl Pts',(10.4639347549999,15.2,0.306527058999984));
#193062=CARTESIAN_POINT('Ctrl Pts',(10.4639347549999,11.6,0.306527058999983));
#193063=CARTESIAN_POINT('Ctrl Pts',(10.4654721899999,15.2,0.306820520999986));
#193064=CARTESIAN_POINT('Ctrl Pts',(10.4654721899999,11.6,0.306820520999986));
#193065=CARTESIAN_POINT('Ctrl Pts',(10.4670171509999,15.2,0.307116928999989));
#193066=CARTESIAN_POINT('Ctrl Pts',(10.4670171509999,11.6,0.307116928999988));
#193067=CARTESIAN_POINT('Ctrl Pts',(10.4685696139999,15.2,0.307416291999987));
#193068=CARTESIAN_POINT('Ctrl Pts',(10.4685696139999,11.6,0.307416291999986));
#193069=CARTESIAN_POINT('Ctrl Pts',(10.4701295609999,15.2,0.307718619999986));
#193070=CARTESIAN_POINT('Ctrl Pts',(10.4701295609999,11.6,0.307718619999986));
#193071=CARTESIAN_POINT('Ctrl Pts',(10.4716969689999,15.2,0.308023921999983));
#193072=CARTESIAN_POINT('Ctrl Pts',(10.4716969689999,11.6,0.308023921999982));
#193073=CARTESIAN_POINT('Ctrl Pts',(10.4732718189999,15.2,0.308332208999986));
#193074=CARTESIAN_POINT('Ctrl Pts',(10.4732718189999,11.6,0.308332208999986));
#193075=CARTESIAN_POINT('Ctrl Pts',(10.4748540859999,15.2,0.308643490999985));
#193076=CARTESIAN_POINT('Ctrl Pts',(10.4748540859999,11.6,0.308643490999984));
#193077=CARTESIAN_POINT('Ctrl Pts',(10.4764437519999,15.2,0.308957776999983));
#193078=CARTESIAN_POINT('Ctrl Pts',(10.4764437519999,11.6,0.308957776999983));
#193079=CARTESIAN_POINT('Ctrl Pts',(10.4780407969999,15.2,0.309275076999986));
#193080=CARTESIAN_POINT('Ctrl Pts',(10.4780407969999,11.6,0.309275076999986));
#193081=CARTESIAN_POINT('Ctrl Pts',(10.4796451969999,15.2,0.309595398999987));
#193082=CARTESIAN_POINT('Ctrl Pts',(10.4796451969999,11.6,0.309595398999986));
#193083=CARTESIAN_POINT('Ctrl Pts',(10.4812569339999,15.2,0.309918754999985));
#193084=CARTESIAN_POINT('Ctrl Pts',(10.4812569339999,11.6,0.309918754999984));
#193085=CARTESIAN_POINT('Ctrl Pts',(10.4828759869999,15.2,0.310245152999986));
#193086=CARTESIAN_POINT('Ctrl Pts',(10.4828759869999,11.6,0.310245152999986));
#193087=CARTESIAN_POINT('Ctrl Pts',(10.4845023339999,15.2,0.310574602999987));
#193088=CARTESIAN_POINT('Ctrl Pts',(10.4845023339999,11.6,0.310574602999986));
#193089=CARTESIAN_POINT('Ctrl Pts',(10.4861359559999,15.2,0.310907112999987));
#193090=CARTESIAN_POINT('Ctrl Pts',(10.4861359559999,11.6,0.310907112999987));
#193091=CARTESIAN_POINT('Ctrl Pts',(10.4877768319999,15.2,0.311242694999985));
#193092=CARTESIAN_POINT('Ctrl Pts',(10.4877768319999,11.6,0.311242694999984));
#193093=CARTESIAN_POINT('Ctrl Pts',(10.4894249419999,15.2,0.311581356999984));
#193094=CARTESIAN_POINT('Ctrl Pts',(10.4894249419999,11.6,0.311581356999983));
#193095=CARTESIAN_POINT('Ctrl Pts',(10.4910802659999,15.2,0.311923107999985));
#193096=CARTESIAN_POINT('Ctrl Pts',(10.4910802659999,11.6,0.311923107999985));
#193097=CARTESIAN_POINT('Ctrl Pts',(10.4927427829999,15.2,0.312267955999985));
#193098=CARTESIAN_POINT('Ctrl Pts',(10.4927427829999,11.6,0.312267955999985));
#193099=CARTESIAN_POINT('Ctrl Pts',(10.4944124729999,15.2,0.312615912999985));
#193100=CARTESIAN_POINT('Ctrl Pts',(10.4944124729999,11.6,0.312615912999985));
#193101=CARTESIAN_POINT('Ctrl Pts',(10.4960893159999,15.2,0.312966985999985));
#193102=CARTESIAN_POINT('Ctrl Pts',(10.4960893159999,11.6,0.312966985999985));
#193103=CARTESIAN_POINT('Ctrl Pts',(10.4977732919999,15.2,0.313321184999986));
#193104=CARTESIAN_POINT('Ctrl Pts',(10.4977732919999,11.6,0.313321184999986));
#193105=CARTESIAN_POINT('Ctrl Pts',(10.4994643819999,15.2,0.313678519999985));
#193106=CARTESIAN_POINT('Ctrl Pts',(10.4994643819999,11.6,0.313678519999984));
#193107=CARTESIAN_POINT('Ctrl Pts',(10.5011625649999,15.2,0.314038996999986));
#193108=CARTESIAN_POINT('Ctrl Pts',(10.5011625649999,11.6,0.314038996999985));
#193109=CARTESIAN_POINT('Ctrl Pts',(10.5028678219999,15.2,0.314402627999986));
#193110=CARTESIAN_POINT('Ctrl Pts',(10.5028678219999,11.6,0.314402627999985));
#193111=CARTESIAN_POINT('Ctrl Pts',(10.5045801319999,15.2,0.314769419999985));
#193112=CARTESIAN_POINT('Ctrl Pts',(10.5045801319999,11.6,0.314769419999985));
#193113=CARTESIAN_POINT('Ctrl Pts',(10.5062994779999,15.2,0.315139381999985));
#193114=CARTESIAN_POINT('Ctrl Pts',(10.5062994779999,11.6,0.315139381999984));
#193115=CARTESIAN_POINT('Ctrl Pts',(10.5080258379999,15.2,0.315512523999986));
#193116=CARTESIAN_POINT('Ctrl Pts',(10.5080258379999,11.6,0.315512523999985));
#193117=CARTESIAN_POINT('Ctrl Pts',(10.5097591929999,15.2,0.315888853999984));
#193118=CARTESIAN_POINT('Ctrl Pts',(10.5097591929999,11.6,0.315888853999983));
#193119=CARTESIAN_POINT('Ctrl Pts',(10.5114995239999,15.2,0.316268379999984));
#193120=CARTESIAN_POINT('Ctrl Pts',(10.5114995239999,11.6,0.316268379999984));
#193121=CARTESIAN_POINT('Ctrl Pts',(10.5132468119999,15.2,0.316651112999988));
#193122=CARTESIAN_POINT('Ctrl Pts',(10.5132468119999,11.6,0.316651112999988));
#193123=CARTESIAN_POINT('Ctrl Pts',(10.5150010359999,15.2,0.317037058999983));
#193124=CARTESIAN_POINT('Ctrl Pts',(10.5150010359999,11.6,0.317037058999982));
#193125=CARTESIAN_POINT('Ctrl Pts',(10.5167621799999,15.2,0.317426227999986));
#193126=CARTESIAN_POINT('Ctrl Pts',(10.5167621799999,11.6,0.317426227999986));
#193127=CARTESIAN_POINT('Ctrl Pts',(10.5185302209999,15.2,0.317818628999986));
#193128=CARTESIAN_POINT('Ctrl Pts',(10.5185302209999,11.6,0.317818628999986));
#193129=CARTESIAN_POINT('Ctrl Pts',(10.5203051419999,15.2,0.318214267999988));
#193130=CARTESIAN_POINT('Ctrl Pts',(10.5203051419999,11.6,0.318214267999987));
#193131=CARTESIAN_POINT('Ctrl Pts',(10.5220869239999,15.2,0.318613156999987));
#193132=CARTESIAN_POINT('Ctrl Pts',(10.5220869239999,11.6,0.318613156999987));
#193133=CARTESIAN_POINT('Ctrl Pts',(10.5238755469999,15.2,0.319015301999985));
#193134=CARTESIAN_POINT('Ctrl Pts',(10.5238755469999,11.6,0.319015301999985));
#193135=CARTESIAN_POINT('Ctrl Pts',(10.5256709929999,15.2,0.319420711999987));
#193136=CARTESIAN_POINT('Ctrl Pts',(10.5256709929999,11.6,0.319420711999987));
#193137=CARTESIAN_POINT('Ctrl Pts',(10.5274732429999,15.2,0.319829395999989));
#193138=CARTESIAN_POINT('Ctrl Pts',(10.5274732429999,11.6,0.319829395999988));
#193139=CARTESIAN_POINT('Ctrl Pts',(10.5292822789999,15.2,0.320241360999987));
#193140=CARTESIAN_POINT('Ctrl Pts',(10.5292822789999,11.6,0.320241360999986));
#193141=CARTESIAN_POINT('Ctrl Pts',(10.5310980799999,15.2,0.320656615999986));
#193142=CARTESIAN_POINT('Ctrl Pts',(10.5310980799999,11.6,0.320656615999985));
#193143=CARTESIAN_POINT('Ctrl Pts',(10.5329206289999,15.2,0.321075169999983));
#193144=CARTESIAN_POINT('Ctrl Pts',(10.5329206289999,11.6,0.321075169999982));
#193145=CARTESIAN_POINT('Ctrl Pts',(10.5347499079999,15.2,0.321497028999986));
#193146=CARTESIAN_POINT('Ctrl Pts',(10.5347499079999,11.6,0.321497028999986));
#193147=CARTESIAN_POINT('Ctrl Pts',(10.5365858959999,15.2,0.321922202999985));
#193148=CARTESIAN_POINT('Ctrl Pts',(10.5365858959999,11.6,0.321922202999984));
#193149=CARTESIAN_POINT('Ctrl Pts',(10.5384285769999,15.2,0.322350700999987));
#193150=CARTESIAN_POINT('Ctrl Pts',(10.5384285769999,11.6,0.322350700999987));
#193151=CARTESIAN_POINT('Ctrl Pts',(10.5402779309999,15.2,0.322782526999985));
#193152=CARTESIAN_POINT('Ctrl Pts',(10.5402779309999,11.6,0.322782526999985));
#193153=CARTESIAN_POINT('Ctrl Pts',(10.5421339399999,15.2,0.323217693999984));
#193154=CARTESIAN_POINT('Ctrl Pts',(10.5421339399999,11.6,0.323217693999984));
#193155=CARTESIAN_POINT('Ctrl Pts',(10.5439965859999,15.2,0.323656206999985));
#193156=CARTESIAN_POINT('Ctrl Pts',(10.5439965859999,11.6,0.323656206999984));
#193157=CARTESIAN_POINT('Ctrl Pts',(10.5458658509999,15.2,0.324098074999988));
#193158=CARTESIAN_POINT('Ctrl Pts',(10.5458658509999,11.6,0.324098074999987));
#193159=CARTESIAN_POINT('Ctrl Pts',(10.5477417169999,15.2,0.324543303999985));
#193160=CARTESIAN_POINT('Ctrl Pts',(10.5477417169999,11.6,0.324543303999984));
#193161=CARTESIAN_POINT('Ctrl Pts',(10.5496241639999,15.2,0.324991904999985));
#193162=CARTESIAN_POINT('Ctrl Pts',(10.5496241639999,11.6,0.324991904999985));
#193163=CARTESIAN_POINT('Ctrl Pts',(10.5515131759999,15.2,0.325443883999985));
#193164=CARTESIAN_POINT('Ctrl Pts',(10.5515131759999,11.6,0.325443883999985));
#193165=CARTESIAN_POINT('Ctrl Pts',(10.5534087349999,15.2,0.325899248999986));
#193166=CARTESIAN_POINT('Ctrl Pts',(10.5534087349999,11.6,0.325899248999985));
#193167=CARTESIAN_POINT('Ctrl Pts',(10.5553108209999,15.2,0.326358006999987));
#193168=CARTESIAN_POINT('Ctrl Pts',(10.5553108209999,11.6,0.326358006999987));
#193169=CARTESIAN_POINT('Ctrl Pts',(10.5572194179999,15.2,0.326820166999986));
#193170=CARTESIAN_POINT('Ctrl Pts',(10.5572194179999,11.6,0.326820166999986));
#193171=CARTESIAN_POINT('Ctrl Pts',(10.5591345069999,15.2,0.327285735999983));
#193172=CARTESIAN_POINT('Ctrl Pts',(10.5591345069999,11.6,0.327285735999982));
#193173=CARTESIAN_POINT('Ctrl Pts',(10.5610560699999,15.2,0.327754721999987));
#193174=CARTESIAN_POINT('Ctrl Pts',(10.5610560699999,11.6,0.327754721999986));
#193175=CARTESIAN_POINT('Ctrl Pts',(10.5629840909999,15.2,0.328227131999985));
#193176=CARTESIAN_POINT('Ctrl Pts',(10.5629840909999,11.6,0.328227131999985));
#193177=CARTESIAN_POINT('Ctrl Pts',(10.5649185509999,15.2,0.328702973999988));
#193178=CARTESIAN_POINT('Ctrl Pts',(10.5649185509999,11.6,0.328702973999988));
#193179=CARTESIAN_POINT('Ctrl Pts',(10.5668594319999,15.2,0.329182255999987));
#193180=CARTESIAN_POINT('Ctrl Pts',(10.5668594319999,11.6,0.329182255999986));
#193181=CARTESIAN_POINT('Ctrl Pts',(10.5688067179999,15.2,0.329664984999987));
#193182=CARTESIAN_POINT('Ctrl Pts',(10.5688067179999,11.6,0.329664984999986));
#193183=CARTESIAN_POINT('Ctrl Pts',(10.5707603889999,15.2,0.330151168999984));
#193184=CARTESIAN_POINT('Ctrl Pts',(10.5707603889999,11.6,0.330151168999983));
#193185=CARTESIAN_POINT('Ctrl Pts',(10.5727204309999,15.2,0.330640813999987));
#193186=CARTESIAN_POINT('Ctrl Pts',(10.5727204309999,11.6,0.330640813999987));
#193187=CARTESIAN_POINT('Ctrl Pts',(10.5746868229999,15.2,0.331133928999985));
#193188=CARTESIAN_POINT('Ctrl Pts',(10.5746868229999,11.6,0.331133928999984));
#193189=CARTESIAN_POINT('Ctrl Pts',(10.5766595509999,15.2,0.331630518999986));
#193190=CARTESIAN_POINT('Ctrl Pts',(10.5766595509999,11.6,0.331630518999985));
#193191=CARTESIAN_POINT('Ctrl Pts',(10.5786385939999,15.2,0.332130593999986));
#193192=CARTESIAN_POINT('Ctrl Pts',(10.5786385939999,11.6,0.332130593999986));
#193193=CARTESIAN_POINT('Ctrl Pts',(10.5806239379999,15.2,0.332634160999987));
#193194=CARTESIAN_POINT('Ctrl Pts',(10.5806239379999,11.6,0.332634160999987));
#193195=CARTESIAN_POINT('Ctrl Pts',(10.5826155629999,15.2,0.333141224999984));
#193196=CARTESIAN_POINT('Ctrl Pts',(10.5826155629999,11.6,0.333141224999984));
#193197=CARTESIAN_POINT('Ctrl Pts',(10.5846134539999,15.2,0.333651795999987));
#193198=CARTESIAN_POINT('Ctrl Pts',(10.5846134539999,11.6,0.333651795999987));
#193199=CARTESIAN_POINT('Ctrl Pts',(10.5866175939999,15.2,0.334165879999984));
#193200=CARTESIAN_POINT('Ctrl Pts',(10.5866175939999,11.6,0.334165879999983));
#193201=CARTESIAN_POINT('Ctrl Pts',(10.5886279639999,15.2,0.334683481999987));
#193202=CARTESIAN_POINT('Ctrl Pts',(10.5886279639999,11.6,0.334683481999986));
#193203=CARTESIAN_POINT('Ctrl Pts',(10.5906445489999,15.2,0.335204612999984));
#193204=CARTESIAN_POINT('Ctrl Pts',(10.5906445489999,11.6,0.335204612999984));
#193205=CARTESIAN_POINT('Ctrl Pts',(10.5926673309999,15.2,0.335729276999985));
#193206=CARTESIAN_POINT('Ctrl Pts',(10.5926673309999,11.6,0.335729276999985));
#193207=CARTESIAN_POINT('Ctrl Pts',(10.5946962929999,15.2,0.336257483999987));
#193208=CARTESIAN_POINT('Ctrl Pts',(10.5946962929999,11.6,0.336257483999986));
#193209=CARTESIAN_POINT('Ctrl Pts',(10.5967314189999,15.2,0.336789236999984));
#193210=CARTESIAN_POINT('Ctrl Pts',(10.5967314189999,11.6,0.336789236999983));
#193211=CARTESIAN_POINT('Ctrl Pts',(10.5987726909999,15.2,0.337324546999986));
#193212=CARTESIAN_POINT('Ctrl Pts',(10.5987726909999,11.6,0.337324546999986));
#193213=CARTESIAN_POINT('Ctrl Pts',(10.6008200939999,15.2,0.337863417999986));
#193214=CARTESIAN_POINT('Ctrl Pts',(10.6008200939999,11.6,0.337863417999986));
#193215=CARTESIAN_POINT('Ctrl Pts',(10.6028736079999,15.2,0.338405857999984));
#193216=CARTESIAN_POINT('Ctrl Pts',(10.6028736079999,11.6,0.338405857999983));
#193217=CARTESIAN_POINT('Ctrl Pts',(10.6049332199999,15.2,0.338951874999989));
#193218=CARTESIAN_POINT('Ctrl Pts',(10.6049332199999,11.6,0.338951874999988));
#193219=CARTESIAN_POINT('Ctrl Pts',(10.6069989119999,15.2,0.339501473999988));
#193220=CARTESIAN_POINT('Ctrl Pts',(10.6069989119999,11.6,0.339501473999988));
#193221=CARTESIAN_POINT('Ctrl Pts',(10.6090706669999,15.2,0.340054661999982));
#193222=CARTESIAN_POINT('Ctrl Pts',(10.6090706669999,11.6,0.340054661999982));
#193223=CARTESIAN_POINT('Ctrl Pts',(10.6111484689999,15.2,0.340611447999986));
#193224=CARTESIAN_POINT('Ctrl Pts',(10.6111484689999,11.6,0.340611447999985));
#193225=CARTESIAN_POINT('Ctrl Pts',(10.6132323019999,15.2,0.341171835999985));
#193226=CARTESIAN_POINT('Ctrl Pts',(10.6132323019999,11.6,0.341171835999984));
#193227=CARTESIAN_POINT('Ctrl Pts',(10.6153221469999,15.2,0.341735832999985));
#193228=CARTESIAN_POINT('Ctrl Pts',(10.6153221469999,11.6,0.341735832999985));
#193229=CARTESIAN_POINT('Ctrl Pts',(10.6174179919999,15.2,0.342303447999988));
#193230=CARTESIAN_POINT('Ctrl Pts',(10.6174179919999,11.6,0.342303447999987));
#193231=CARTESIAN_POINT('Ctrl Pts',(10.6195198169999,15.2,0.342874684999988));
#193232=CARTESIAN_POINT('Ctrl Pts',(10.6195198169999,11.6,0.342874684999987));
#193233=CARTESIAN_POINT('Ctrl Pts',(10.6216276069999,15.2,0.343449551999986));
#193234=CARTESIAN_POINT('Ctrl Pts',(10.6216276069999,11.6,0.343449551999985));
#193235=CARTESIAN_POINT('Ctrl Pts',(10.6237413459999,15.2,0.344028055999988));
#193236=CARTESIAN_POINT('Ctrl Pts',(10.6237413459999,11.6,0.344028055999987));
#193237=CARTESIAN_POINT('Ctrl Pts',(10.6258610179999,15.2,0.344610201999984));
#193238=CARTESIAN_POINT('Ctrl Pts',(10.6258610179999,11.6,0.344610201999984));
#193239=CARTESIAN_POINT('Ctrl Pts',(10.6279866059999,15.2,0.345195998999985));
#193240=CARTESIAN_POINT('Ctrl Pts',(10.6279866059999,11.6,0.345195998999985));
#193241=CARTESIAN_POINT('Ctrl Pts',(10.6301180949999,15.2,0.345785449999987));
#193242=CARTESIAN_POINT('Ctrl Pts',(10.6301180949999,11.6,0.345785449999986));
#193243=CARTESIAN_POINT('Ctrl Pts',(10.6322554669999,15.2,0.346378564999985));
#193244=CARTESIAN_POINT('Ctrl Pts',(10.6322554669999,11.6,0.346378564999985));
#193245=CARTESIAN_POINT('Ctrl Pts',(10.6343987089999,15.2,0.346975346999985));
#193246=CARTESIAN_POINT('Ctrl Pts',(10.6343987089999,11.6,0.346975346999984));
#193247=CARTESIAN_POINT('Ctrl Pts',(10.6365478019999,15.2,0.347575804999987));
#193248=CARTESIAN_POINT('Ctrl Pts',(10.6365478019999,11.6,0.347575804999986));
#193249=CARTESIAN_POINT('Ctrl Pts',(10.6387027319999,15.2,0.348179944999987));
#193250=CARTESIAN_POINT('Ctrl Pts',(10.6387027319999,11.6,0.348179944999986));
#193251=CARTESIAN_POINT('Ctrl Pts',(10.6408634829999,15.2,0.348787772999986));
#193252=CARTESIAN_POINT('Ctrl Pts',(10.6408634829999,11.6,0.348787772999985));
#193253=CARTESIAN_POINT('Ctrl Pts',(10.6430300389999,15.2,0.349399293999983));
#193254=CARTESIAN_POINT('Ctrl Pts',(10.6430300389999,11.6,0.349399293999983));
#193255=CARTESIAN_POINT('Ctrl Pts',(10.6452023819999,15.2,0.350014516999986));
#193256=CARTESIAN_POINT('Ctrl Pts',(10.6452023819999,11.6,0.350014516999985));
#193257=CARTESIAN_POINT('Ctrl Pts',(10.6473805009999,15.2,0.350633446999984));
#193258=CARTESIAN_POINT('Ctrl Pts',(10.6473805009999,11.6,0.350633446999983));
#193259=CARTESIAN_POINT('Ctrl Pts',(10.6495643749999,15.2,0.351256088999987));
#193260=CARTESIAN_POINT('Ctrl Pts',(10.6495643749999,11.6,0.351256088999987));
#193261=CARTESIAN_POINT('Ctrl Pts',(10.6517539929999,15.2,0.351882449999987));
#193262=CARTESIAN_POINT('Ctrl Pts',(10.6517539929999,11.6,0.351882449999987));
#193263=CARTESIAN_POINT('Ctrl Pts',(10.6539493359999,15.2,0.352512536999985));
#193264=CARTESIAN_POINT('Ctrl Pts',(10.6539493359999,11.6,0.352512536999984));
#193265=CARTESIAN_POINT('Ctrl Pts',(10.6561503909999,15.2,0.353146354999985));
#193266=CARTESIAN_POINT('Ctrl Pts',(10.6561503909999,11.6,0.353146354999984));
#193267=CARTESIAN_POINT('Ctrl Pts',(10.6583571409999,15.2,0.353783909999983));
#193268=CARTESIAN_POINT('Ctrl Pts',(10.6583571409999,11.6,0.353783909999982));
#193269=CARTESIAN_POINT('Ctrl Pts',(10.6605695709999,15.2,0.354425208999984));
#193270=CARTESIAN_POINT('Ctrl Pts',(10.6605695709999,11.6,0.354425208999984));
#193271=CARTESIAN_POINT('Ctrl Pts',(10.6627876639999,15.2,0.355070257999985));
#193272=CARTESIAN_POINT('Ctrl Pts',(10.6627876639999,11.6,0.355070257999985));
#193273=CARTESIAN_POINT('Ctrl Pts',(10.6650114069999,15.2,0.355719062999986));
#193274=CARTESIAN_POINT('Ctrl Pts',(10.6650114069999,11.6,0.355719062999986));
#193275=CARTESIAN_POINT('Ctrl Pts',(10.6672407829999,15.2,0.356371629999988));
#193276=CARTESIAN_POINT('Ctrl Pts',(10.6672407829999,11.6,0.356371629999987));
#193277=CARTESIAN_POINT('Ctrl Pts',(10.6694757779999,15.2,0.357027963999985));
#193278=CARTESIAN_POINT('Ctrl Pts',(10.6694757779999,11.6,0.357027963999985));
#193279=CARTESIAN_POINT('Ctrl Pts',(10.6717163759999,15.2,0.357688071999984));
#193280=CARTESIAN_POINT('Ctrl Pts',(10.6717163759999,11.6,0.357688071999984));
#193281=CARTESIAN_POINT('Ctrl Pts',(10.6739625609999,15.2,0.358351958999985));
#193282=CARTESIAN_POINT('Ctrl Pts',(10.6739625609999,11.6,0.358351958999985));
#193283=CARTESIAN_POINT('Ctrl Pts',(10.6762143189999,15.2,0.359019631999988));
#193284=CARTESIAN_POINT('Ctrl Pts',(10.6762143189999,11.6,0.359019631999988));
#193285=CARTESIAN_POINT('Ctrl Pts',(10.6784716349999,15.2,0.359691095999985));
#193286=CARTESIAN_POINT('Ctrl Pts',(10.6784716349999,11.6,0.359691095999985));
#193287=CARTESIAN_POINT('Ctrl Pts',(10.6807344929999,15.2,0.360366356999986));
#193288=CARTESIAN_POINT('Ctrl Pts',(10.6807344929999,11.6,0.360366356999986));
#193289=CARTESIAN_POINT('Ctrl Pts',(10.6830028779999,15.2,0.361045420999986));
#193290=CARTESIAN_POINT('Ctrl Pts',(10.6830028779999,11.6,0.361045420999985));
#193291=CARTESIAN_POINT('Ctrl Pts',(10.6852767759999,15.2,0.361728292999985));
#193292=CARTESIAN_POINT('Ctrl Pts',(10.6852767759999,11.6,0.361728292999985));
#193293=CARTESIAN_POINT('Ctrl Pts',(10.6875561699999,15.2,0.362414979999985));
#193294=CARTESIAN_POINT('Ctrl Pts',(10.6875561699999,11.6,0.362414979999985));
#193295=CARTESIAN_POINT('Ctrl Pts',(10.6898410479999,15.2,0.363105487999986));
#193296=CARTESIAN_POINT('Ctrl Pts',(10.6898410479999,11.6,0.363105487999986));
#193297=CARTESIAN_POINT('Ctrl Pts',(10.6921313919999,15.2,0.363799819999984));
#193298=CARTESIAN_POINT('Ctrl Pts',(10.6921313919999,11.6,0.363799819999983));
#193299=CARTESIAN_POINT('Ctrl Pts',(10.6944271889999,15.2,0.364497984999983));
#193300=CARTESIAN_POINT('Ctrl Pts',(10.6944271889999,11.6,0.364497984999983));
#193301=CARTESIAN_POINT('Ctrl Pts',(10.6967284239999,15.2,0.365199985999984));
#193302=CARTESIAN_POINT('Ctrl Pts',(10.6967284239999,11.6,0.365199985999984));
#193303=CARTESIAN_POINT('Ctrl Pts',(10.6990350819999,15.2,0.365905829999988));
#193304=CARTESIAN_POINT('Ctrl Pts',(10.6990350819999,11.6,0.365905829999988));
#193305=CARTESIAN_POINT('Ctrl Pts',(10.7013471479999,15.2,0.366615522999982));
#193306=CARTESIAN_POINT('Ctrl Pts',(10.7013471479999,11.6,0.366615522999982));
#193307=CARTESIAN_POINT('Ctrl Pts',(10.7036646069999,15.2,0.367329069999984));
#193308=CARTESIAN_POINT('Ctrl Pts',(10.7036646069999,11.6,0.367329069999984));
#193309=CARTESIAN_POINT('Ctrl Pts',(10.7059874449999,15.2,0.368046474999986));
#193310=CARTESIAN_POINT('Ctrl Pts',(10.7059874449999,11.6,0.368046474999985));
#193311=CARTESIAN_POINT('Ctrl Pts',(10.7083156469999,15.2,0.368767745999987));
#193312=CARTESIAN_POINT('Ctrl Pts',(10.7083156469999,11.6,0.368767745999987));
#193313=CARTESIAN_POINT('Ctrl Pts',(10.7106491999999,15.2,0.369492886999985));
#193314=CARTESIAN_POINT('Ctrl Pts',(10.7106491999999,11.6,0.369492886999984));
#193315=CARTESIAN_POINT('Ctrl Pts',(10.7129880859999,15.2,0.370221903999983));
#193316=CARTESIAN_POINT('Ctrl Pts',(10.7129880859999,11.6,0.370221903999983));
#193317=CARTESIAN_POINT('Ctrl Pts',(10.7153322929999,15.2,0.370954801999983));
#193318=CARTESIAN_POINT('Ctrl Pts',(10.7153322929999,11.6,0.370954801999983));
#193319=CARTESIAN_POINT('Ctrl Pts',(10.7176818059999,15.2,0.371691585999985));
#193320=CARTESIAN_POINT('Ctrl Pts',(10.7176818059999,11.6,0.371691585999984));
#193321=CARTESIAN_POINT('Ctrl Pts',(10.7200366109999,15.2,0.372432262999984));
#193322=CARTESIAN_POINT('Ctrl Pts',(10.7200366109999,11.6,0.372432262999984));
#193323=CARTESIAN_POINT('Ctrl Pts',(10.7223966929999,15.2,0.373176837999987));
#193324=CARTESIAN_POINT('Ctrl Pts',(10.7223966929999,11.6,0.373176837999986));
#193325=CARTESIAN_POINT('Ctrl Pts',(10.7247620369999,15.2,0.373925313999983));
#193326=CARTESIAN_POINT('Ctrl Pts',(10.7247620369999,11.6,0.373925313999983));
#193327=CARTESIAN_POINT('Ctrl Pts',(10.7271326309999,15.2,0.374677699999988));
#193328=CARTESIAN_POINT('Ctrl Pts',(10.7271326309999,11.6,0.374677699999987));
#193329=CARTESIAN_POINT('Ctrl Pts',(10.7295084569999,15.2,0.375433997999988));
#193330=CARTESIAN_POINT('Ctrl Pts',(10.7295084569999,11.6,0.375433997999987));
#193331=CARTESIAN_POINT('Ctrl Pts',(10.7318895039999,15.2,0.376194214999988));
#193332=CARTESIAN_POINT('Ctrl Pts',(10.7318895039999,11.6,0.376194214999987));
#193333=CARTESIAN_POINT('Ctrl Pts',(10.7342757559999,15.2,0.376958354999988));
#193334=CARTESIAN_POINT('Ctrl Pts',(10.7342757559999,11.6,0.376958354999987));
#193335=CARTESIAN_POINT('Ctrl Pts',(10.7366671989999,15.2,0.377726424999985));
#193336=CARTESIAN_POINT('Ctrl Pts',(10.7366671989999,11.6,0.377726424999984));
#193337=CARTESIAN_POINT('Ctrl Pts',(10.7390638199999,15.2,0.378498429999983));
#193338=CARTESIAN_POINT('Ctrl Pts',(10.7390638199999,11.6,0.378498429999982));
#193339=CARTESIAN_POINT('Ctrl Pts',(10.7414656029999,15.2,0.379274372999987));
#193340=CARTESIAN_POINT('Ctrl Pts',(10.7414656029999,11.6,0.379274372999987));
#193341=CARTESIAN_POINT('Ctrl Pts',(10.7438725369999,15.2,0.380054260999985));
#193342=CARTESIAN_POINT('Ctrl Pts',(10.7438725369999,11.6,0.380054260999984));
#193343=CARTESIAN_POINT('Ctrl Pts',(10.7462846039999,15.2,0.380838097999985));
#193344=CARTESIAN_POINT('Ctrl Pts',(10.7462846039999,11.6,0.380838097999984));
#193345=CARTESIAN_POINT('Ctrl Pts',(10.7487017909999,15.2,0.381625889999988));
#193346=CARTESIAN_POINT('Ctrl Pts',(10.7487017909999,11.6,0.381625889999988));
#193347=CARTESIAN_POINT('Ctrl Pts',(10.7511240869999,15.2,0.382417640999986));
#193348=CARTESIAN_POINT('Ctrl Pts',(10.7511240869999,11.6,0.382417640999985));
#193349=CARTESIAN_POINT('Ctrl Pts',(10.7535514749999,15.2,0.383213357999987));
#193350=CARTESIAN_POINT('Ctrl Pts',(10.7535514749999,11.6,0.383213357999987));
#193351=CARTESIAN_POINT('Ctrl Pts',(10.7559839419999,15.2,0.384013043999989));
#193352=CARTESIAN_POINT('Ctrl Pts',(10.7559839419999,11.6,0.384013043999988));
#193353=CARTESIAN_POINT('Ctrl Pts',(10.7584214739999,15.2,0.384816704999986));
#193354=CARTESIAN_POINT('Ctrl Pts',(10.7584214739999,11.6,0.384816704999986));
#193355=CARTESIAN_POINT('Ctrl Pts',(10.7608640569999,15.2,0.385624345999984));
#193356=CARTESIAN_POINT('Ctrl Pts',(10.7608640569999,11.6,0.385624345999984));
#193357=CARTESIAN_POINT('Ctrl Pts',(10.7633116769999,15.2,0.386435971999983));
#193358=CARTESIAN_POINT('Ctrl Pts',(10.7633116769999,11.6,0.386435971999983));
#193359=CARTESIAN_POINT('Ctrl Pts',(10.7657643219999,15.2,0.387251585999984));
#193360=CARTESIAN_POINT('Ctrl Pts',(10.7657643219999,11.6,0.387251585999983));
#193361=CARTESIAN_POINT('Ctrl Pts',(10.7682219759999,15.2,0.388071195999986));
#193362=CARTESIAN_POINT('Ctrl Pts',(10.7682219759999,11.6,0.388071195999986));
#193363=CARTESIAN_POINT('Ctrl Pts',(10.7706846259999,15.2,0.388894804999986));
#193364=CARTESIAN_POINT('Ctrl Pts',(10.7706846259999,11.6,0.388894804999986));
#193365=CARTESIAN_POINT('Ctrl Pts',(10.7731522589999,15.2,0.389722418999985));
#193366=CARTESIAN_POINT('Ctrl Pts',(10.7731522589999,11.6,0.389722418999984));
#193367=CARTESIAN_POINT('Ctrl Pts',(10.7756248599999,15.2,0.390554039999986));
#193368=CARTESIAN_POINT('Ctrl Pts',(10.7756248599999,11.6,0.390554039999986));
#193369=CARTESIAN_POINT('Ctrl Pts',(10.7781024159999,15.2,0.391389675999987));
#193370=CARTESIAN_POINT('Ctrl Pts',(10.7781024159999,11.6,0.391389675999986));
#193371=CARTESIAN_POINT('Ctrl Pts',(10.7805849149999,15.2,0.392229330999987));
#193372=CARTESIAN_POINT('Ctrl Pts',(10.7805849149999,11.6,0.392229330999986));
#193373=CARTESIAN_POINT('Ctrl Pts',(10.7830723399999,15.2,0.393073009999987));
#193374=CARTESIAN_POINT('Ctrl Pts',(10.7830723399999,11.6,0.393073009999986));
#193375=CARTESIAN_POINT('Ctrl Pts',(10.7855646809999,15.2,0.393920716999983));
#193376=CARTESIAN_POINT('Ctrl Pts',(10.7855646809999,11.6,0.393920716999982));
#193377=CARTESIAN_POINT('Ctrl Pts',(10.7880619219999,15.2,0.394772455999988));
#193378=CARTESIAN_POINT('Ctrl Pts',(10.7880619219999,11.6,0.394772455999987));
#193379=CARTESIAN_POINT('Ctrl Pts',(10.7905640509999,15.2,0.395628232999985));
#193380=CARTESIAN_POINT('Ctrl Pts',(10.7905640509999,11.6,0.395628232999985));
#193381=CARTESIAN_POINT('Ctrl Pts',(10.7930710549999,15.2,0.396488051999988));
#193382=CARTESIAN_POINT('Ctrl Pts',(10.7930710549999,11.6,0.396488051999988));
#193383=CARTESIAN_POINT('Ctrl Pts',(10.7955829179999,15.2,0.397351917999984));
#193384=CARTESIAN_POINT('Ctrl Pts',(10.7955829179999,11.6,0.397351917999984));
#193385=CARTESIAN_POINT('Ctrl Pts',(10.7980996289999,15.2,0.398219834999987));
#193386=CARTESIAN_POINT('Ctrl Pts',(10.7980996289999,11.6,0.398219834999986));
#193387=CARTESIAN_POINT('Ctrl Pts',(10.8006211739999,15.2,0.399091808999987));
#193388=CARTESIAN_POINT('Ctrl Pts',(10.8006211739999,11.6,0.399091808999987));
#193389=CARTESIAN_POINT('Ctrl Pts',(10.8031475389999,15.2,0.399967843999987));
#193390=CARTESIAN_POINT('Ctrl Pts',(10.8031475389999,11.6,0.399967843999986));
#193391=CARTESIAN_POINT('Ctrl Pts',(10.8056787119999,15.2,0.400847942999984));
#193392=CARTESIAN_POINT('Ctrl Pts',(10.8056787119999,11.6,0.400847942999984));
#193393=CARTESIAN_POINT('Ctrl Pts',(10.8082146789999,15.2,0.401732112999986));
#193394=CARTESIAN_POINT('Ctrl Pts',(10.8082146789999,11.6,0.401732112999986));
#193395=CARTESIAN_POINT('Ctrl Pts',(10.8107554269999,15.2,0.402620356999983));
#193396=CARTESIAN_POINT('Ctrl Pts',(10.8107554269999,11.6,0.402620356999983));
#193397=CARTESIAN_POINT('Ctrl Pts',(10.8133009429999,15.2,0.403512679999984));
#193398=CARTESIAN_POINT('Ctrl Pts',(10.8133009429999,11.6,0.403512679999984));
#193399=CARTESIAN_POINT('Ctrl Pts',(10.8158512129999,15.2,0.404409085999986));
#193400=CARTESIAN_POINT('Ctrl Pts',(10.8158512129999,11.6,0.404409085999986));
#193401=CARTESIAN_POINT('Ctrl Pts',(10.8184062239999,15.2,0.405309579999984));
#193402=CARTESIAN_POINT('Ctrl Pts',(10.8184062239999,11.6,0.405309579999984));
#193403=CARTESIAN_POINT('Ctrl Pts',(10.8209659639999,15.2,0.406214165999987));
#193404=CARTESIAN_POINT('Ctrl Pts',(10.8209659639999,11.6,0.406214165999987));
#193405=CARTESIAN_POINT('Ctrl Pts',(10.8235304189999,15.2,0.407122848999983));
#193406=CARTESIAN_POINT('Ctrl Pts',(10.8235304189999,11.6,0.407122848999983));
#193407=CARTESIAN_POINT('Ctrl Pts',(10.8260995769999,15.2,0.408035632999986));
#193408=CARTESIAN_POINT('Ctrl Pts',(10.8260995769999,11.6,0.408035632999985));
#193409=CARTESIAN_POINT('Ctrl Pts',(10.8286734229999,15.2,0.408952522999986));
#193410=CARTESIAN_POINT('Ctrl Pts',(10.8286734229999,11.6,0.408952522999985));
#193411=CARTESIAN_POINT('Ctrl Pts',(10.8312519469999,15.2,0.409873522999984));
#193412=CARTESIAN_POINT('Ctrl Pts',(10.8312519469999,11.6,0.409873522999983));
#193413=CARTESIAN_POINT('Ctrl Pts',(10.8338351319999,15.2,0.410798634999985));
#193414=CARTESIAN_POINT('Ctrl Pts',(10.8338351319999,11.6,0.410798634999984));
#193415=CARTESIAN_POINT('Ctrl Pts',(10.8364229689999,15.2,0.411727866999985));
#193416=CARTESIAN_POINT('Ctrl Pts',(10.8364229689999,11.6,0.411727866999984));
#193417=CARTESIAN_POINT('Ctrl Pts',(10.8390154429999,15.2,0.412661221999984));
#193418=CARTESIAN_POINT('Ctrl Pts',(10.8390154429999,11.6,0.412661221999983));
#193419=CARTESIAN_POINT('Ctrl Pts',(10.8416125419999,15.2,0.413598703999987));
#193420=CARTESIAN_POINT('Ctrl Pts',(10.8416125419999,11.6,0.413598703999986));
#193421=CARTESIAN_POINT('Ctrl Pts',(10.8442142529999,15.2,0.414540315999985));
#193422=CARTESIAN_POINT('Ctrl Pts',(10.8442142529999,11.6,0.414540315999985));
#193423=CARTESIAN_POINT('Ctrl Pts',(10.8468205619999,15.2,0.415486064999988));
#193424=CARTESIAN_POINT('Ctrl Pts',(10.8468205619999,11.6,0.415486064999988));
#193425=CARTESIAN_POINT('Ctrl Pts',(10.8494314579999,15.2,0.416435953999983));
#193426=CARTESIAN_POINT('Ctrl Pts',(10.8494314579999,11.6,0.416435953999982));
#193427=CARTESIAN_POINT('Ctrl Pts',(10.8520469269999,15.2,0.417389984999983));
#193428=CARTESIAN_POINT('Ctrl Pts',(10.8520469269999,11.6,0.417389984999982));
#193429=CARTESIAN_POINT('Ctrl Pts',(10.8546669569999,15.2,0.418348164999984));
#193430=CARTESIAN_POINT('Ctrl Pts',(10.8546669569999,11.6,0.418348164999984));
#193431=CARTESIAN_POINT('Ctrl Pts',(10.8572915349999,15.2,0.419310497999987));
#193432=CARTESIAN_POINT('Ctrl Pts',(10.8572915349999,11.6,0.419310497999987));
#193433=CARTESIAN_POINT('Ctrl Pts',(10.8599206479999,15.2,0.420276986999983));
#193434=CARTESIAN_POINT('Ctrl Pts',(10.8599206479999,11.6,0.420276986999983));
#193435=CARTESIAN_POINT('Ctrl Pts',(10.8625542849999,15.2,0.421247635999986));
#193436=CARTESIAN_POINT('Ctrl Pts',(10.8625542849999,11.6,0.421247635999986));
#193437=CARTESIAN_POINT('Ctrl Pts',(10.8651924309999,15.2,0.422222449999987));
#193438=CARTESIAN_POINT('Ctrl Pts',(10.8651924309999,11.6,0.422222449999987));
#193439=CARTESIAN_POINT('Ctrl Pts',(10.8678350749999,15.2,0.423201432999987));
#193440=CARTESIAN_POINT('Ctrl Pts',(10.8678350749999,11.6,0.423201432999986));
#193441=CARTESIAN_POINT('Ctrl Pts',(10.8704822049999,15.2,0.424184587999985));
#193442=CARTESIAN_POINT('Ctrl Pts',(10.8704822049999,11.6,0.424184587999985));
#193443=CARTESIAN_POINT('Ctrl Pts',(10.8731338059999,15.2,0.425171920999983));
#193444=CARTESIAN_POINT('Ctrl Pts',(10.8731338059999,11.6,0.425171920999982));
#193445=CARTESIAN_POINT('Ctrl Pts',(10.8757898679999,15.2,0.426163433999989));
#193446=CARTESIAN_POINT('Ctrl Pts',(10.8757898679999,11.6,0.426163433999988));
#193447=CARTESIAN_POINT('Ctrl Pts',(10.8784503779999,15.2,0.427159131999986));
#193448=CARTESIAN_POINT('Ctrl Pts',(10.8784503779999,11.6,0.427159131999985));
#193449=CARTESIAN_POINT('Ctrl Pts',(10.8811153219999,15.2,0.428159017999987));
#193450=CARTESIAN_POINT('Ctrl Pts',(10.8811153219999,11.6,0.428159017999987));
#193451=CARTESIAN_POINT('Ctrl Pts',(10.8837846889999,15.2,0.429163097999985));
#193452=CARTESIAN_POINT('Ctrl Pts',(10.8837846889999,11.6,0.429163097999985));
#193453=CARTESIAN_POINT('Ctrl Pts',(10.8864584659999,15.2,0.430171373999984));
#193454=CARTESIAN_POINT('Ctrl Pts',(10.8864584659999,11.6,0.430171373999983));
#193455=CARTESIAN_POINT('Ctrl Pts',(10.8891366429999,15.2,0.431183849999983));
#193456=CARTESIAN_POINT('Ctrl Pts',(10.8891366429999,11.6,0.431183849999983));
#193457=CARTESIAN_POINT('Ctrl Pts',(10.8918192029999,15.2,0.432200530999989));
#193458=CARTESIAN_POINT('Ctrl Pts',(10.8918192029999,11.6,0.432200530999988));
#193459=CARTESIAN_POINT('Ctrl Pts',(10.8945061379999,15.2,0.433221420999987));
#193460=CARTESIAN_POINT('Ctrl Pts',(10.8945061379999,11.6,0.433221420999987));
#193461=CARTESIAN_POINT('Ctrl Pts',(10.8971974329999,15.2,0.434246522999988));
#193462=CARTESIAN_POINT('Ctrl Pts',(10.8971974329999,11.6,0.434246522999988));
#193463=CARTESIAN_POINT('Ctrl Pts',(10.8998930779999,15.2,0.435275839999987));
#193464=CARTESIAN_POINT('Ctrl Pts',(10.8998930779999,11.6,0.435275839999986));
#193465=CARTESIAN_POINT('Ctrl Pts',(10.9025930589999,15.2,0.436309378999984));
#193466=CARTESIAN_POINT('Ctrl Pts',(10.9025930589999,11.6,0.436309378999983));
#193467=CARTESIAN_POINT('Ctrl Pts',(10.9052973639999,15.2,0.437347140999984));
#193468=CARTESIAN_POINT('Ctrl Pts',(10.9052973639999,11.6,0.437347140999984));
#193469=CARTESIAN_POINT('Ctrl Pts',(10.9080059809999,15.2,0.438389129999983));
#193470=CARTESIAN_POINT('Ctrl Pts',(10.9080059809999,11.6,0.438389129999983));
#193471=CARTESIAN_POINT('Ctrl Pts',(10.9107188979999,15.2,0.439435350999986));
#193472=CARTESIAN_POINT('Ctrl Pts',(10.9107188979999,11.6,0.439435350999986));
#193473=CARTESIAN_POINT('Ctrl Pts',(10.9134361039999,15.2,0.440485805999984));
#193474=CARTESIAN_POINT('Ctrl Pts',(10.9134361039999,11.6,0.440485805999983));
#193475=CARTESIAN_POINT('Ctrl Pts',(10.9161575839999,15.2,0.441540500999986));
#193476=CARTESIAN_POINT('Ctrl Pts',(10.9161575839999,11.6,0.441540500999986));
#193477=CARTESIAN_POINT('Ctrl Pts',(10.9188833299999,15.2,0.442599438999984));
#193478=CARTESIAN_POINT('Ctrl Pts',(10.9188833299999,11.6,0.442599438999984));
#193479=CARTESIAN_POINT('Ctrl Pts',(10.9216133259999,15.2,0.443662621999987));
#193480=CARTESIAN_POINT('Ctrl Pts',(10.9216133259999,11.6,0.443662621999987));
#193481=CARTESIAN_POINT('Ctrl Pts',(10.9243475619999,15.2,0.444730056999987));
#193482=CARTESIAN_POINT('Ctrl Pts',(10.9243475619999,11.6,0.444730056999986));
#193483=CARTESIAN_POINT('Ctrl Pts',(10.9270860269999,15.2,0.445801742999983));
#193484=CARTESIAN_POINT('Ctrl Pts',(10.9270860269999,11.6,0.445801742999982));
#193485=CARTESIAN_POINT('Ctrl Pts',(10.9298287059999,15.2,0.446877687999985));
#193486=CARTESIAN_POINT('Ctrl Pts',(10.9298287059999,11.6,0.446877687999984));
#193487=CARTESIAN_POINT('Ctrl Pts',(10.9325755889999,15.2,0.447957893999984));
#193488=CARTESIAN_POINT('Ctrl Pts',(10.9325755889999,11.6,0.447957893999984));
#193489=CARTESIAN_POINT('Ctrl Pts',(10.9353266639999,15.2,0.449042364999985));
#193490=CARTESIAN_POINT('Ctrl Pts',(10.9353266639999,11.6,0.449042364999985));
#193491=CARTESIAN_POINT('Ctrl Pts',(10.9380819189999,15.2,0.450131101999984));
#193492=CARTESIAN_POINT('Ctrl Pts',(10.9380819189999,11.6,0.450131101999984));
#193493=CARTESIAN_POINT('Ctrl Pts',(10.9408413419999,15.2,0.451224112999986));
#193494=CARTESIAN_POINT('Ctrl Pts',(10.9408413419999,11.6,0.451224112999986));
#193495=CARTESIAN_POINT('Ctrl Pts',(10.9436049209999,15.2,0.452321397999986));
#193496=CARTESIAN_POINT('Ctrl Pts',(10.9436049209999,11.6,0.452321397999986));
#193497=CARTESIAN_POINT('Ctrl Pts',(10.9463726449999,15.2,0.453422962999985));
#193498=CARTESIAN_POINT('Ctrl Pts',(10.9463726449999,11.6,0.453422962999985));
#193499=CARTESIAN_POINT('Ctrl Pts',(10.9491445009999,15.2,0.454528808999988));
#193500=CARTESIAN_POINT('Ctrl Pts',(10.9491445009999,11.6,0.454528808999987));
#193501=CARTESIAN_POINT('Ctrl Pts',(10.9519204779999,15.2,0.455638941999985));
#193502=CARTESIAN_POINT('Ctrl Pts',(10.9519204779999,11.6,0.455638941999985));
#193503=CARTESIAN_POINT('Ctrl Pts',(10.9547005639999,15.2,0.456753363999987));
#193504=CARTESIAN_POINT('Ctrl Pts',(10.9547005639999,11.6,0.456753363999986));
#193505=CARTESIAN_POINT('Ctrl Pts',(10.9574847479999,15.2,0.457872078999984));
#193506=CARTESIAN_POINT('Ctrl Pts',(10.9574847479999,11.6,0.457872078999983));
#193507=CARTESIAN_POINT('Ctrl Pts',(10.9602730159999,15.2,0.458995089999985));
#193508=CARTESIAN_POINT('Ctrl Pts',(10.9602730159999,11.6,0.458995089999985));
#193509=CARTESIAN_POINT('Ctrl Pts',(10.9630653589999,15.2,0.460122401999987));
#193510=CARTESIAN_POINT('Ctrl Pts',(10.9630653589999,11.6,0.460122401999987));
#193511=CARTESIAN_POINT('Ctrl Pts',(10.9658617639999,15.2,0.461254016999986));
#193512=CARTESIAN_POINT('Ctrl Pts',(10.9658617639999,11.6,0.461254016999985));
#193513=CARTESIAN_POINT('Ctrl Pts',(10.9686622189999,15.2,0.462389937999985));
#193514=CARTESIAN_POINT('Ctrl Pts',(10.9686622189999,11.6,0.462389937999985));
#193515=CARTESIAN_POINT('Ctrl Pts',(10.9714667139999,15.2,0.463530168999986));
#193516=CARTESIAN_POINT('Ctrl Pts',(10.9714667139999,11.6,0.463530168999986));
#193517=CARTESIAN_POINT('Ctrl Pts',(10.9742752359999,15.2,0.464674713999984));
#193518=CARTESIAN_POINT('Ctrl Pts',(10.9742752359999,11.6,0.464674713999984));
#193519=CARTESIAN_POINT('Ctrl Pts',(10.9770877739999,15.2,0.465823574999984));
#193520=CARTESIAN_POINT('Ctrl Pts',(10.9770877739999,11.6,0.465823574999984));
#193521=CARTESIAN_POINT('Ctrl Pts',(10.9799043159999,15.2,0.466976757999986));
#193522=CARTESIAN_POINT('Ctrl Pts',(10.9799043159999,11.6,0.466976757999986));
#193523=CARTESIAN_POINT('Ctrl Pts',(10.9827248519999,15.2,0.468134262999986));
#193524=CARTESIAN_POINT('Ctrl Pts',(10.9827248519999,11.6,0.468134262999986));
#193525=CARTESIAN_POINT('Ctrl Pts',(10.9855493679999,15.2,0.469296094999985));
#193526=CARTESIAN_POINT('Ctrl Pts',(10.9855493679999,11.6,0.469296094999984));
#193527=CARTESIAN_POINT('Ctrl Pts',(10.9883778529999,15.2,0.470462257999986));
#193528=CARTESIAN_POINT('Ctrl Pts',(10.9883778529999,11.6,0.470462257999986));
#193529=CARTESIAN_POINT('Ctrl Pts',(10.9912102979999,15.2,0.471632752999986));
#193530=CARTESIAN_POINT('Ctrl Pts',(10.9912102979999,11.6,0.471632752999986));
#193531=CARTESIAN_POINT('Ctrl Pts',(10.9940466899999,15.2,0.472807584999986));
#193532=CARTESIAN_POINT('Ctrl Pts',(10.9940466899999,11.6,0.472807584999985));
#193533=CARTESIAN_POINT('Ctrl Pts',(10.9968870169999,15.2,0.473986756999984));
#193534=CARTESIAN_POINT('Ctrl Pts',(10.9968870169999,11.6,0.473986756999984));
#193535=CARTESIAN_POINT('Ctrl Pts',(10.9997312679999,15.2,0.475170272999983));
#193536=CARTESIAN_POINT('Ctrl Pts',(10.9997312679999,11.6,0.475170272999982));
#193537=CARTESIAN_POINT('Ctrl Pts',(11.0025794309999,15.2,0.476358134999986));
#193538=CARTESIAN_POINT('Ctrl Pts',(11.0025794309999,11.6,0.476358134999985));
#193539=CARTESIAN_POINT('Ctrl Pts',(11.0054314969999,15.2,0.477550345999984));
#193540=CARTESIAN_POINT('Ctrl Pts',(11.0054314969999,11.6,0.477550345999984));
#193541=CARTESIAN_POINT('Ctrl Pts',(11.0082874519999,15.2,0.478746909999987));
#193542=CARTESIAN_POINT('Ctrl Pts',(11.0082874519999,11.6,0.478746909999987));
#193543=CARTESIAN_POINT('Ctrl Pts',(11.0111472859999,15.2,0.479947829999983));
#193544=CARTESIAN_POINT('Ctrl Pts',(11.0111472859999,11.6,0.479947829999982));
#193545=CARTESIAN_POINT('Ctrl Pts',(11.0140109889999,15.2,0.481153109999983));
#193546=CARTESIAN_POINT('Ctrl Pts',(11.0140109889999,11.6,0.481153109999983));
#193547=CARTESIAN_POINT('Ctrl Pts',(11.0168785469999,15.2,0.482362750999985));
#193548=CARTESIAN_POINT('Ctrl Pts',(11.0168785469999,11.6,0.482362750999985));
#193549=CARTESIAN_POINT('Ctrl Pts',(11.0197499499999,15.2,0.483576758999984));
#193550=CARTESIAN_POINT('Ctrl Pts',(11.0197499499999,11.6,0.483576758999984));
#193551=CARTESIAN_POINT('Ctrl Pts',(11.0226251869999,15.2,0.484795133999985));
#193552=CARTESIAN_POINT('Ctrl Pts',(11.0226251869999,11.6,0.484795133999984));
#193553=CARTESIAN_POINT('Ctrl Pts',(11.0255042469999,15.2,0.486017880999987));
#193554=CARTESIAN_POINT('Ctrl Pts',(11.0255042469999,11.6,0.486017880999987));
#193555=CARTESIAN_POINT('Ctrl Pts',(11.0283871179999,15.2,0.487245001999987));
#193556=CARTESIAN_POINT('Ctrl Pts',(11.0283871179999,11.6,0.487245001999987));
#193557=CARTESIAN_POINT('Ctrl Pts',(11.0312737899999,15.2,0.488476501999986));
#193558=CARTESIAN_POINT('Ctrl Pts',(11.0312737899999,11.6,0.488476501999985));
#193559=CARTESIAN_POINT('Ctrl Pts',(11.0341642509999,15.2,0.489712382999983));
#193560=CARTESIAN_POINT('Ctrl Pts',(11.0341642509999,11.6,0.489712382999982));
#193561=CARTESIAN_POINT('Ctrl Pts',(11.0370584909999,15.2,0.490952646999983));
#193562=CARTESIAN_POINT('Ctrl Pts',(11.0370584909999,11.6,0.490952646999982));
#193563=CARTESIAN_POINT('Ctrl Pts',(11.0399564969999,15.2,0.492197297999986));
#193564=CARTESIAN_POINT('Ctrl Pts',(11.0399564969999,11.6,0.492197297999985));
#193565=CARTESIAN_POINT('Ctrl Pts',(11.0428582599999,15.2,0.493446338999988));
#193566=CARTESIAN_POINT('Ctrl Pts',(11.0428582599999,11.6,0.493446338999987));
#193567=CARTESIAN_POINT('Ctrl Pts',(11.0457637679999,15.2,0.494699771999985));
#193568=CARTESIAN_POINT('Ctrl Pts',(11.0457637679999,11.6,0.494699771999984));
#193569=CARTESIAN_POINT('Ctrl Pts',(11.0486730089999,15.2,0.495957601999986));
#193570=CARTESIAN_POINT('Ctrl Pts',(11.0486730089999,11.6,0.495957601999985));
#193571=CARTESIAN_POINT('Ctrl Pts',(11.0515859739999,15.2,0.497219829999986));
#193572=CARTESIAN_POINT('Ctrl Pts',(11.0515859739999,11.6,0.497219829999986));
#193573=CARTESIAN_POINT('Ctrl Pts',(11.0545026509999,15.2,0.498486459999987));
#193574=CARTESIAN_POINT('Ctrl Pts',(11.0545026509999,11.6,0.498486459999987));
#193575=CARTESIAN_POINT('Ctrl Pts',(11.0574230279999,15.2,0.499757494999984));
#193576=CARTESIAN_POINT('Ctrl Pts',(11.0574230279999,11.6,0.499757494999983));
#193577=CARTESIAN_POINT('Ctrl Pts',(11.0603470969999,15.2,0.501032936999986));
#193578=CARTESIAN_POINT('Ctrl Pts',(11.0603470969999,11.6,0.501032936999985));
#193579=CARTESIAN_POINT('Ctrl Pts',(11.0632748429999,15.2,0.502312789999984));
#193580=CARTESIAN_POINT('Ctrl Pts',(11.0632748429999,11.6,0.502312789999983));
#193581=CARTESIAN_POINT('Ctrl Pts',(11.0662062589999,15.2,0.503597055999983));
#193582=CARTESIAN_POINT('Ctrl Pts',(11.0662062589999,11.6,0.503597055999982));
#193583=CARTESIAN_POINT('Ctrl Pts',(11.0691413309999,15.2,0.504885737999987));
#193584=CARTESIAN_POINT('Ctrl Pts',(11.0691413309999,11.6,0.504885737999987));
#193585=CARTESIAN_POINT('Ctrl Pts',(11.0720800509999,15.2,0.506178839999984));
#193586=CARTESIAN_POINT('Ctrl Pts',(11.0720800509999,11.6,0.506178839999984));
#193587=CARTESIAN_POINT('Ctrl Pts',(11.0750224069999,15.2,0.507476362999988));
#193588=CARTESIAN_POINT('Ctrl Pts',(11.0750224069999,11.6,0.507476362999987));
#193589=CARTESIAN_POINT('Ctrl Pts',(11.0779683879999,15.2,0.508778310999984));
#193590=CARTESIAN_POINT('Ctrl Pts',(11.0779683879999,11.6,0.508778310999984));
#193591=CARTESIAN_POINT('Ctrl Pts',(11.0809179819999,15.2,0.510084686999988));
#193592=CARTESIAN_POINT('Ctrl Pts',(11.0809179819999,11.6,0.510084686999987));
#193593=CARTESIAN_POINT('Ctrl Pts',(11.0838711809999,15.2,0.511395492999984));
#193594=CARTESIAN_POINT('Ctrl Pts',(11.0838711809999,11.6,0.511395492999984));
#193595=CARTESIAN_POINT('Ctrl Pts',(11.0868279709999,15.2,0.512710731999988));
#193596=CARTESIAN_POINT('Ctrl Pts',(11.0868279709999,11.6,0.512710731999988));
#193597=CARTESIAN_POINT('Ctrl Pts',(11.0897883439999,15.2,0.514030406999986));
#193598=CARTESIAN_POINT('Ctrl Pts',(11.0897883439999,11.6,0.514030406999985));
#193599=CARTESIAN_POINT('Ctrl Pts',(11.0927522879999,15.2,0.515354519999986));
#193600=CARTESIAN_POINT('Ctrl Pts',(11.0927522879999,11.6,0.515354519999986));
#193601=CARTESIAN_POINT('Ctrl Pts',(11.0957197919999,15.2,0.516683075999986));
#193602=CARTESIAN_POINT('Ctrl Pts',(11.0957197919999,11.6,0.516683075999986));
#193603=CARTESIAN_POINT('Ctrl Pts',(11.0986908469999,15.2,0.518016075999985));
#193604=CARTESIAN_POINT('Ctrl Pts',(11.0986908469999,11.6,0.518016075999985));
#193605=CARTESIAN_POINT('Ctrl Pts',(11.1016654419999,15.2,0.519353521999988));
#193606=CARTESIAN_POINT('Ctrl Pts',(11.1016654419999,11.6,0.519353521999987));
#193607=CARTESIAN_POINT('Ctrl Pts',(11.1046435639999,15.2,0.520695417999986));
#193608=CARTESIAN_POINT('Ctrl Pts',(11.1046435639999,11.6,0.520695417999985));
#193609=CARTESIAN_POINT('Ctrl Pts',(11.1076252049999,15.2,0.522041765999983));
#193610=CARTESIAN_POINT('Ctrl Pts',(11.1076252049999,11.6,0.522041765999983));
#193611=CARTESIAN_POINT('Ctrl Pts',(11.1106103519999,15.2,0.523392568999985));
#193612=CARTESIAN_POINT('Ctrl Pts',(11.1106103519999,11.6,0.523392568999985));
#193613=CARTESIAN_POINT('Ctrl Pts',(11.1135989969999,15.2,0.524747829999987));
#193614=CARTESIAN_POINT('Ctrl Pts',(11.1135989969999,11.6,0.524747829999987));
#193615=CARTESIAN_POINT('Ctrl Pts',(11.1165911289999,15.2,0.526107550999986));
#193616=CARTESIAN_POINT('Ctrl Pts',(11.1165911289999,11.6,0.526107550999985));
#193617=CARTESIAN_POINT('Ctrl Pts',(11.1195867359999,15.2,0.527471733999985));
#193618=CARTESIAN_POINT('Ctrl Pts',(11.1195867359999,11.6,0.527471733999984));
#193619=CARTESIAN_POINT('Ctrl Pts',(11.1225858069999,15.2,0.528840383999984));
#193620=CARTESIAN_POINT('Ctrl Pts',(11.1225858069999,11.6,0.528840383999984));
#193621=CARTESIAN_POINT('Ctrl Pts',(11.1255883349999,15.2,0.530213501999985));
#193622=CARTESIAN_POINT('Ctrl Pts',(11.1255883349999,11.6,0.530213501999985));
#193623=CARTESIAN_POINT('Ctrl Pts',(11.1285943059999,15.2,0.531591089999988));
#193624=CARTESIAN_POINT('Ctrl Pts',(11.1285943059999,11.6,0.531591089999987));
#193625=CARTESIAN_POINT('Ctrl Pts',(11.1316037109999,15.2,0.532973150999982));
#193626=CARTESIAN_POINT('Ctrl Pts',(11.1316037109999,11.6,0.532973150999982));
#193627=CARTESIAN_POINT('Ctrl Pts',(11.1346165399999,15.2,0.534359688999988));
#193628=CARTESIAN_POINT('Ctrl Pts',(11.1346165399999,11.6,0.534359688999988));
#193629=CARTESIAN_POINT('Ctrl Pts',(11.1376327809999,15.2,0.535750703999986));
#193630=CARTESIAN_POINT('Ctrl Pts',(11.1376327809999,11.6,0.535750703999986));
#193631=CARTESIAN_POINT('Ctrl Pts',(11.1406524249999,15.2,0.537146200999987));
#193632=CARTESIAN_POINT('Ctrl Pts',(11.1406524249999,11.6,0.537146200999987));
#193633=CARTESIAN_POINT('Ctrl Pts',(11.1436754609999,15.2,0.538546180999986));
#193634=CARTESIAN_POINT('Ctrl Pts',(11.1436754609999,11.6,0.538546180999985));
#193635=CARTESIAN_POINT('Ctrl Pts',(11.1467018789999,15.2,0.539950646999987));
#193636=CARTESIAN_POINT('Ctrl Pts',(11.1467018789999,11.6,0.539950646999987));
#193637=CARTESIAN_POINT('Ctrl Pts',(11.1497316689999,15.2,0.541359601999982));
#193638=CARTESIAN_POINT('Ctrl Pts',(11.1497316689999,11.6,0.541359601999982));
#193639=CARTESIAN_POINT('Ctrl Pts',(11.1527648199999,15.2,0.542773047999985));
#193640=CARTESIAN_POINT('Ctrl Pts',(11.1527648199999,11.6,0.542773047999984));
#193641=CARTESIAN_POINT('Ctrl Pts',(11.1558013209999,15.2,0.544190986999986));
#193642=CARTESIAN_POINT('Ctrl Pts',(11.1558013209999,11.6,0.544190986999986));
#193643=CARTESIAN_POINT('Ctrl Pts',(11.1588411629999,15.2,0.545613420999986));
#193644=CARTESIAN_POINT('Ctrl Pts',(11.1588411629999,11.6,0.545613420999986));
#193645=CARTESIAN_POINT('Ctrl Pts',(11.1618843359999,15.2,0.547040353999986));
#193646=CARTESIAN_POINT('Ctrl Pts',(11.1618843359999,11.6,0.547040353999985));
#193647=CARTESIAN_POINT('Ctrl Pts',(11.1649308279999,15.2,0.548471788999985));
#193648=CARTESIAN_POINT('Ctrl Pts',(11.1649308279999,11.6,0.548471788999984));
#193649=CARTESIAN_POINT('Ctrl Pts',(11.1679806309999,15.2,0.549907724999983));
#193650=CARTESIAN_POINT('Ctrl Pts',(11.1679806309999,11.6,0.549907724999982));
#193651=CARTESIAN_POINT('Ctrl Pts',(11.1710337319999,15.2,0.551348167999985));
#193652=CARTESIAN_POINT('Ctrl Pts',(11.1710337319999,11.6,0.551348167999985));
#193653=CARTESIAN_POINT('Ctrl Pts',(11.1740901229999,15.2,0.552793118999984));
#193654=CARTESIAN_POINT('Ctrl Pts',(11.1740901229999,11.6,0.552793118999983));
#193655=CARTESIAN_POINT('Ctrl Pts',(11.1771497949999,15.2,0.554242579999986));
#193656=CARTESIAN_POINT('Ctrl Pts',(11.1771497949999,11.6,0.554242579999986));
#193657=CARTESIAN_POINT('Ctrl Pts',(11.1802127339999,15.2,0.555696553999985));
#193658=CARTESIAN_POINT('Ctrl Pts',(11.1802127339999,11.6,0.555696553999984));
#193659=CARTESIAN_POINT('Ctrl Pts',(11.1832789319999,15.2,0.557155042999984));
#193660=CARTESIAN_POINT('Ctrl Pts',(11.1832789319999,11.6,0.557155042999983));
#193661=CARTESIAN_POINT('Ctrl Pts',(11.1863483789999,15.2,0.558618048999988));
#193662=CARTESIAN_POINT('Ctrl Pts',(11.1863483789999,11.6,0.558618048999988));
#193663=CARTESIAN_POINT('Ctrl Pts',(11.1894210649999,15.2,0.560085574999984));
#193664=CARTESIAN_POINT('Ctrl Pts',(11.1894210649999,11.6,0.560085574999984));
#193665=CARTESIAN_POINT('Ctrl Pts',(11.1924969799999,15.2,0.561557623999986));
#193666=CARTESIAN_POINT('Ctrl Pts',(11.1924969799999,11.6,0.561557623999986));
#193667=CARTESIAN_POINT('Ctrl Pts',(11.1955761109999,15.2,0.563034195999985));
#193668=CARTESIAN_POINT('Ctrl Pts',(11.1955761109999,11.6,0.563034195999985));
#193669=CARTESIAN_POINT('Ctrl Pts',(11.1986584539999,15.2,0.564515295999986));
#193670=CARTESIAN_POINT('Ctrl Pts',(11.1986584539999,11.6,0.564515295999985));
#193671=CARTESIAN_POINT('Ctrl Pts',(11.2017439929999,15.2,0.566000923999983));
#193672=CARTESIAN_POINT('Ctrl Pts',(11.2017439929999,11.6,0.566000923999983));
#193673=CARTESIAN_POINT('Ctrl Pts',(11.2048327209999,15.2,0.567491083999982));
#193674=CARTESIAN_POINT('Ctrl Pts',(11.2048327209999,11.6,0.567491083999982));
#193675=CARTESIAN_POINT('Ctrl Pts',(11.2079246269999,15.2,0.568985776999984));
#193676=CARTESIAN_POINT('Ctrl Pts',(11.2079246269999,11.6,0.568985776999984));
#193677=CARTESIAN_POINT('Ctrl Pts',(11.2110197019999,15.2,0.570485004999988));
#193678=CARTESIAN_POINT('Ctrl Pts',(11.2110197019999,11.6,0.570485004999987));
#193679=CARTESIAN_POINT('Ctrl Pts',(11.2141179349999,15.2,0.571988772999985));
#193680=CARTESIAN_POINT('Ctrl Pts',(11.2141179349999,11.6,0.571988772999985));
#193681=CARTESIAN_POINT('Ctrl Pts',(11.2172193169999,15.2,0.573497079999985));
#193682=CARTESIAN_POINT('Ctrl Pts',(11.2172193169999,11.6,0.573497079999985));
#193683=CARTESIAN_POINT('Ctrl Pts',(11.2203238359999,15.2,0.575009928999983));
#193684=CARTESIAN_POINT('Ctrl Pts',(11.2203238359999,11.6,0.575009928999983));
#193685=CARTESIAN_POINT('Ctrl Pts',(11.2234314849999,15.2,0.576527321999984));
#193686=CARTESIAN_POINT('Ctrl Pts',(11.2234314849999,11.6,0.576527321999984));
#193687=CARTESIAN_POINT('Ctrl Pts',(11.2265422519999,15.2,0.578049263999985));
#193688=CARTESIAN_POINT('Ctrl Pts',(11.2265422519999,11.6,0.578049263999984));
#193689=CARTESIAN_POINT('Ctrl Pts',(11.2296561279999,15.2,0.579575753999984));
#193690=CARTESIAN_POINT('Ctrl Pts',(11.2296561279999,11.6,0.579575753999983));
#193691=CARTESIAN_POINT('Ctrl Pts',(11.2327731029999,15.2,0.581106793999986));
#193692=CARTESIAN_POINT('Ctrl Pts',(11.2327731029999,11.6,0.581106793999985));
#193693=CARTESIAN_POINT('Ctrl Pts',(11.2358931669999,15.2,0.582642387999983));
#193694=CARTESIAN_POINT('Ctrl Pts',(11.2358931669999,11.6,0.582642387999983));
#193695=CARTESIAN_POINT('Ctrl Pts',(11.2390163099999,15.2,0.584182537999984));
#193696=CARTESIAN_POINT('Ctrl Pts',(11.2390163099999,11.6,0.584182537999984));
#193697=CARTESIAN_POINT('Ctrl Pts',(11.2421425229999,15.2,0.585727244999985));
#193698=CARTESIAN_POINT('Ctrl Pts',(11.2421425229999,11.6,0.585727244999985));
#193699=CARTESIAN_POINT('Ctrl Pts',(11.2452717949999,15.2,0.587276511999986));
#193700=CARTESIAN_POINT('Ctrl Pts',(11.2452717949999,11.6,0.587276511999985));
#193701=CARTESIAN_POINT('Ctrl Pts',(11.2484041159999,15.2,0.588830339999986));
#193702=CARTESIAN_POINT('Ctrl Pts',(11.2484041159999,11.6,0.588830339999986));
#193703=CARTESIAN_POINT('Ctrl Pts',(11.2515394779999,15.2,0.590388731999987));
#193704=CARTESIAN_POINT('Ctrl Pts',(11.2515394779999,11.6,0.590388731999986));
#193705=CARTESIAN_POINT('Ctrl Pts',(11.2546778709999,15.2,0.591951689999988));
#193706=CARTESIAN_POINT('Ctrl Pts',(11.2546778709999,11.6,0.591951689999987));
#193707=CARTESIAN_POINT('Ctrl Pts',(11.2578192829999,15.2,0.593519215999985));
#193708=CARTESIAN_POINT('Ctrl Pts',(11.2578192829999,11.6,0.593519215999984));
#193709=CARTESIAN_POINT('Ctrl Pts',(11.2609637079999,15.2,0.595091311999987));
#193710=CARTESIAN_POINT('Ctrl Pts',(11.2609637079999,11.6,0.595091311999986));
#193711=CARTESIAN_POINT('Ctrl Pts',(11.2641111319999,15.2,0.596667980999985));
#193712=CARTESIAN_POINT('Ctrl Pts',(11.2641111319999,11.6,0.596667980999985));
#193713=CARTESIAN_POINT('Ctrl Pts',(11.2672615479999,15.2,0.598249222999985));
#193714=CARTESIAN_POINT('Ctrl Pts',(11.2672615479999,11.6,0.598249222999984));
#193715=CARTESIAN_POINT('Ctrl Pts',(11.2704149449999,15.2,0.599835040999985));
#193716=CARTESIAN_POINT('Ctrl Pts',(11.2704149449999,11.6,0.599835040999985));
#193717=CARTESIAN_POINT('Ctrl Pts',(11.2735713159999,15.2,0.601425437999983));
#193718=CARTESIAN_POINT('Ctrl Pts',(11.2735713159999,11.6,0.601425437999982));
#193719=CARTESIAN_POINT('Ctrl Pts',(11.2767306479999,15.2,0.603020413999986));
#193720=CARTESIAN_POINT('Ctrl Pts',(11.2767306479999,11.6,0.603020413999986));
#193721=CARTESIAN_POINT('Ctrl Pts',(11.2798929329999,15.2,0.604619971999987));
#193722=CARTESIAN_POINT('Ctrl Pts',(11.2798929329999,11.6,0.604619971999986));
#193723=CARTESIAN_POINT('Ctrl Pts',(11.2830581619999,15.2,0.606224114999985));
#193724=CARTESIAN_POINT('Ctrl Pts',(11.2830581619999,11.6,0.606224114999984));
#193725=CARTESIAN_POINT('Ctrl Pts',(11.2862263229999,15.2,0.607832843999985));
#193726=CARTESIAN_POINT('Ctrl Pts',(11.2862263229999,11.6,0.607832843999984));
#193727=CARTESIAN_POINT('Ctrl Pts',(11.2893974099999,15.2,0.609446159999987));
#193728=CARTESIAN_POINT('Ctrl Pts',(11.2893974099999,11.6,0.609446159999986));
#193729=CARTESIAN_POINT('Ctrl Pts',(11.2925714099999,15.2,0.611064066999987));
#193730=CARTESIAN_POINT('Ctrl Pts',(11.2925714099999,11.6,0.611064066999986));
#193731=CARTESIAN_POINT('Ctrl Pts',(11.2957483149999,15.2,0.612686564999985));
#193732=CARTESIAN_POINT('Ctrl Pts',(11.2957483149999,11.6,0.612686564999984));
#193733=CARTESIAN_POINT('Ctrl Pts',(11.2989281149999,15.2,0.614313657999985));
#193734=CARTESIAN_POINT('Ctrl Pts',(11.2989281149999,11.6,0.614313657999985));
#193735=CARTESIAN_POINT('Ctrl Pts',(11.3021108019999,15.2,0.615945344999984));
#193736=CARTESIAN_POINT('Ctrl Pts',(11.3021108019999,11.6,0.615945344999984));
#193737=CARTESIAN_POINT('Ctrl Pts',(11.3052963649999,15.2,0.617581629999986));
#193738=CARTESIAN_POINT('Ctrl Pts',(11.3052963649999,11.6,0.617581629999985));
#193739=CARTESIAN_POINT('Ctrl Pts',(11.3084847949999,15.2,0.619222514999986));
#193740=CARTESIAN_POINT('Ctrl Pts',(11.3084847949999,11.6,0.619222514999986));
#193741=CARTESIAN_POINT('Ctrl Pts',(11.3116760819999,15.2,0.620868000999986));
#193742=CARTESIAN_POINT('Ctrl Pts',(11.3116760819999,11.6,0.620868000999985));
#193743=CARTESIAN_POINT('Ctrl Pts',(11.3148702169999,15.2,0.622518089999984));
#193744=CARTESIAN_POINT('Ctrl Pts',(11.3148702169999,11.6,0.622518089999983));
#193745=CARTESIAN_POINT('Ctrl Pts',(11.3180671909999,15.2,0.624172784999986));
#193746=CARTESIAN_POINT('Ctrl Pts',(11.3180671909999,11.6,0.624172784999985));
#193747=CARTESIAN_POINT('Ctrl Pts',(11.3212669929999,15.2,0.625832085999987));
#193748=CARTESIAN_POINT('Ctrl Pts',(11.3212669929999,11.6,0.625832085999986));
#193749=CARTESIAN_POINT('Ctrl Pts',(11.3244696159999,15.2,0.627495995999983));
#193750=CARTESIAN_POINT('Ctrl Pts',(11.3244696159999,11.6,0.627495995999982));
#193751=CARTESIAN_POINT('Ctrl Pts',(11.3276750489999,15.2,0.629164515999987));
#193752=CARTESIAN_POINT('Ctrl Pts',(11.3276750489999,11.6,0.629164515999987));
#193753=CARTESIAN_POINT('Ctrl Pts',(11.3308832819999,15.2,0.630837647999982));
#193754=CARTESIAN_POINT('Ctrl Pts',(11.3308832819999,11.6,0.630837647999982));
#193755=CARTESIAN_POINT('Ctrl Pts',(11.3340943069999,15.2,0.632515394999986));
#193756=CARTESIAN_POINT('Ctrl Pts',(11.3340943069999,11.6,0.632515394999986));
#193757=CARTESIAN_POINT('Ctrl Pts',(11.3373081149999,15.2,0.634197756999986));
#193758=CARTESIAN_POINT('Ctrl Pts',(11.3373081149999,11.6,0.634197756999985));
#193759=CARTESIAN_POINT('Ctrl Pts',(11.3405246939999,15.2,0.635884737999985));
#193760=CARTESIAN_POINT('Ctrl Pts',(11.3405246939999,11.6,0.635884737999985));
#193761=CARTESIAN_POINT('Ctrl Pts',(11.3437440379999,15.2,0.637576336999985));
#193762=CARTESIAN_POINT('Ctrl Pts',(11.3437440379999,11.6,0.637576336999985));
#193763=CARTESIAN_POINT('Ctrl Pts',(11.3469661359999,15.2,0.639272557999986));
#193764=CARTESIAN_POINT('Ctrl Pts',(11.3469661359999,11.6,0.639272557999985));
#193765=CARTESIAN_POINT('Ctrl Pts',(11.3501909789999,15.2,0.640973401999982));
#193766=CARTESIAN_POINT('Ctrl Pts',(11.3501909789999,11.6,0.640973401999982));
#193767=CARTESIAN_POINT('Ctrl Pts',(11.3534185569999,15.2,0.642678869999984));
#193768=CARTESIAN_POINT('Ctrl Pts',(11.3534185569999,11.6,0.642678869999984));
#193769=CARTESIAN_POINT('Ctrl Pts',(11.3566488609999,15.2,0.644388963999987));
#193770=CARTESIAN_POINT('Ctrl Pts',(11.3566488609999,11.6,0.644388963999986));
#193771=CARTESIAN_POINT('Ctrl Pts',(11.3598818839999,15.2,0.646103686999986));
#193772=CARTESIAN_POINT('Ctrl Pts',(11.3598818839999,11.6,0.646103686999985));
#193773=CARTESIAN_POINT('Ctrl Pts',(11.3631176139999,15.2,0.647823038999986));
#193774=CARTESIAN_POINT('Ctrl Pts',(11.3631176139999,11.6,0.647823038999986));
#193775=CARTESIAN_POINT('Ctrl Pts',(11.3663560419999,15.2,0.649547022999983));
#193776=CARTESIAN_POINT('Ctrl Pts',(11.3663560419999,11.6,0.649547022999983));
#193777=CARTESIAN_POINT('Ctrl Pts',(11.3695971609999,15.2,0.651275639999986));
#193778=CARTESIAN_POINT('Ctrl Pts',(11.3695971609999,11.6,0.651275639999986));
#193779=CARTESIAN_POINT('Ctrl Pts',(11.3728409599999,15.2,0.653008890999986));
#193780=CARTESIAN_POINT('Ctrl Pts',(11.3728409599999,11.6,0.653008890999986));
#193781=CARTESIAN_POINT('Ctrl Pts',(11.3760874289999,15.2,0.654746779999984));
#193782=CARTESIAN_POINT('Ctrl Pts',(11.3760874289999,11.6,0.654746779999984));
#193783=CARTESIAN_POINT('Ctrl Pts',(11.3793365599999,15.2,0.656489305999983));
#193784=CARTESIAN_POINT('Ctrl Pts',(11.3793365599999,11.6,0.656489305999983));
#193785=CARTESIAN_POINT('Ctrl Pts',(11.3825883449999,15.2,0.658236471999984));
#193786=CARTESIAN_POINT('Ctrl Pts',(11.3825883449999,11.6,0.658236471999984));
#193787=CARTESIAN_POINT('Ctrl Pts',(11.3858427729999,15.2,0.659988279999983));
#193788=CARTESIAN_POINT('Ctrl Pts',(11.3858427729999,11.6,0.659988279999983));
#193789=CARTESIAN_POINT('Ctrl Pts',(11.3890998339999,15.2,0.661744729999985));
#193790=CARTESIAN_POINT('Ctrl Pts',(11.3890998339999,11.6,0.661744729999984));
#193791=CARTESIAN_POINT('Ctrl Pts',(11.3923595219999,15.2,0.663505825999984));
#193792=CARTESIAN_POINT('Ctrl Pts',(11.3923595219999,11.6,0.663505825999983));
#193793=CARTESIAN_POINT('Ctrl Pts',(11.3956218269999,15.2,0.665271566999985));
#193794=CARTESIAN_POINT('Ctrl Pts',(11.3956218269999,11.6,0.665271566999985));
#193795=CARTESIAN_POINT('Ctrl Pts',(11.3988867389999,15.2,0.667041954999985));
#193796=CARTESIAN_POINT('Ctrl Pts',(11.3988867389999,11.6,0.667041954999985));
#193797=CARTESIAN_POINT('Ctrl Pts',(11.4021542499999,15.2,0.668816992999983));
#193798=CARTESIAN_POINT('Ctrl Pts',(11.4021542499999,11.6,0.668816992999983));
#193799=CARTESIAN_POINT('Ctrl Pts',(11.4054243509999,15.2,0.670596681999989));
#193800=CARTESIAN_POINT('Ctrl Pts',(11.4054243509999,11.6,0.670596681999988));
#193801=CARTESIAN_POINT('Ctrl Pts',(11.4086970319999,15.2,0.672381023999984));
#193802=CARTESIAN_POINT('Ctrl Pts',(11.4086970319999,11.6,0.672381023999983));
#193803=CARTESIAN_POINT('Ctrl Pts',(11.4119722829999,15.2,0.674170018999987));
#193804=CARTESIAN_POINT('Ctrl Pts',(11.4119722829999,11.6,0.674170018999986));
#193805=CARTESIAN_POINT('Ctrl Pts',(11.4152500959999,15.2,0.675963670999984));
#193806=CARTESIAN_POINT('Ctrl Pts',(11.4152500959999,11.6,0.675963670999983));
#193807=CARTESIAN_POINT('Ctrl Pts',(11.4185304599999,15.2,0.677761978999989));
#193808=CARTESIAN_POINT('Ctrl Pts',(11.4185304599999,11.6,0.677761978999988));
#193809=CARTESIAN_POINT('Ctrl Pts',(11.4218133689999,15.2,0.679564945999989));
#193810=CARTESIAN_POINT('Ctrl Pts',(11.4218133689999,11.6,0.679564945999988));
#193811=CARTESIAN_POINT('Ctrl Pts',(11.4250988109999,15.2,0.681372573999983));
#193812=CARTESIAN_POINT('Ctrl Pts',(11.4250988109999,11.6,0.681372573999983));
#193813=CARTESIAN_POINT('Ctrl Pts',(11.4283867809999,15.2,0.683184862999986));
#193814=CARTESIAN_POINT('Ctrl Pts',(11.4283867809999,11.6,0.683184862999985));
#193815=CARTESIAN_POINT('Ctrl Pts',(11.4316772699999,15.2,0.685001813999988));
#193816=CARTESIAN_POINT('Ctrl Pts',(11.4316772699999,11.6,0.685001813999988));
#193817=CARTESIAN_POINT('Ctrl Pts',(11.4349702679999,15.2,0.686823429999985));
#193818=CARTESIAN_POINT('Ctrl Pts',(11.4349702679999,11.6,0.686823429999985));
#193819=CARTESIAN_POINT('Ctrl Pts',(11.4382657689999,15.2,0.688649711999982));
#193820=CARTESIAN_POINT('Ctrl Pts',(11.4382657689999,11.6,0.688649711999982));
#193821=CARTESIAN_POINT('Ctrl Pts',(11.4415637619999,15.2,0.690480658999988));
#193822=CARTESIAN_POINT('Ctrl Pts',(11.4415637619999,11.6,0.690480658999987));
#193823=CARTESIAN_POINT('Ctrl Pts',(11.4448642379999,15.2,0.692316276999985));
#193824=CARTESIAN_POINT('Ctrl Pts',(11.4448642379999,11.6,0.692316276999984));
#193825=CARTESIAN_POINT('Ctrl Pts',(11.4481671859999,15.2,0.694156563999986));
#193826=CARTESIAN_POINT('Ctrl Pts',(11.4481671859999,11.6,0.694156563999985));
#193827=CARTESIAN_POINT('Ctrl Pts',(11.4514725939999,15.2,0.696001523999983));
#193828=CARTESIAN_POINT('Ctrl Pts',(11.4514725939999,11.6,0.696001523999982));
#193829=CARTESIAN_POINT('Ctrl Pts',(11.4547804519999,15.2,0.697851158999985));
#193830=CARTESIAN_POINT('Ctrl Pts',(11.4547804519999,11.6,0.697851158999984));
#193831=CARTESIAN_POINT('Ctrl Pts',(11.4580907499999,15.2,0.699705468999987));
#193832=CARTESIAN_POINT('Ctrl Pts',(11.4580907499999,11.6,0.699705468999987));
#193833=CARTESIAN_POINT('Ctrl Pts',(11.4614034809999,15.2,0.701564455999986));
#193834=CARTESIAN_POINT('Ctrl Pts',(11.4614034809999,11.6,0.701564455999985));
#193835=CARTESIAN_POINT('Ctrl Pts',(11.4647186369999,15.2,0.703428121999985));
#193836=CARTESIAN_POINT('Ctrl Pts',(11.4647186369999,11.6,0.703428121999985));
#193837=CARTESIAN_POINT('Ctrl Pts',(11.4680362159999,15.2,0.705296463999985));
#193838=CARTESIAN_POINT('Ctrl Pts',(11.4680362159999,11.6,0.705296463999984));
#193839=CARTESIAN_POINT('Ctrl Pts',(11.4713562149999,15.2,0.707169484999985));
#193840=CARTESIAN_POINT('Ctrl Pts',(11.4713562149999,11.6,0.707169484999985));
#193841=CARTESIAN_POINT('Ctrl Pts',(11.4740141479999,15.2,0.708671645999988));
#193842=CARTESIAN_POINT('Ctrl Pts',(11.4740141479999,11.6,0.708671645999987));
#193843=CARTESIAN_POINT('Ctrl Pts',(11.4760086869999,15.2,0.709800371999982));
#193844=CARTESIAN_POINT('Ctrl Pts',(11.4760086869999,11.6,0.709800371999982));
#193845=CARTESIAN_POINT('Ctrl Pts',(11.4773388639999,15.2,0.710553791999988));
#193846=CARTESIAN_POINT('Ctrl Pts',(11.4773388639999,11.6,0.710553791999988));
#193847=CARTESIAN_POINT('Ctrl Pts',(11.4780040719999,15.2,0.710930734999984));
#193848=CARTESIAN_POINT('Ctrl Pts',(11.4780040719999,11.6,0.710930734999983));
#193849=CARTESIAN_POINT('Ctrl Pts',(10.3708900239999,15.2,0.292001928999985));
#193850=CARTESIAN_POINT('Ctrl Pts',(10.3726650375455,15.2,0.29220550820869));
#193851=CARTESIAN_POINT('Ctrl Pts',(10.3744962441107,15.2,0.292420934685804));
#193852=CARTESIAN_POINT('Ctrl Pts',(10.3763825855683,15.2,0.292648744500014));
#193853=CARTESIAN_POINT('Ctrl Pts',(10.3782780239178,15.2,0.2928776529283));
#193854=CARTESIAN_POINT('Ctrl Pts',(10.3802291370813,15.2,0.293119061022276));
#193855=CARTESIAN_POINT('Ctrl Pts',(10.3822349054607,15.2,0.293373492299609));
#193856=CARTESIAN_POINT('Ctrl Pts',(10.3845749682966,15.2,0.293670328755164));
#193857=CARTESIAN_POINT('Ctrl Pts',(10.38698942021,15.2,0.29398488688512));
#193858=CARTESIAN_POINT('Ctrl Pts',(10.3894766898008,15.2,0.294317967960511));
#193859=CARTESIAN_POINT('Ctrl Pts',(10.3916086354134,15.2,0.294603466058474));
#193860=CARTESIAN_POINT('Ctrl Pts',(10.3937940804213,15.2,0.294902569521762));
#193861=CARTESIAN_POINT('Ctrl Pts',(10.3960320642415,15.2,0.295215760805294));
#193862=CARTESIAN_POINT('Ctrl Pts',(10.39864304506,15.2,0.295581150593409));
#193863=CARTESIAN_POINT('Ctrl Pts',(10.4013255344682,15.2,0.295965719960752));
#193864=CARTESIAN_POINT('Ctrl Pts',(10.404078049501,15.2,0.296370203462173));
#193865=CARTESIAN_POINT('Ctrl Pts',(10.4064373483761,15.2,0.296716903646738));
#193866=CARTESIAN_POINT('Ctrl Pts',(10.4088480966947,15.2,0.297078237171211));
#193867=CARTESIAN_POINT('Ctrl Pts',(10.4113093847881,15.2,0.297454650294742));
#193868=CARTESIAN_POINT('Ctrl Pts',(10.4137706726579,15.2,0.297831063384081));
#193869=CARTESIAN_POINT('Ctrl Pts',(10.4162825002596,15.2,0.298222558514745));
#193870=CARTESIAN_POINT('Ctrl Pts',(10.4188439839998,15.2,0.298629568499958));
#193871=CARTESIAN_POINT('Ctrl Pts',(10.4214054677401,15.2,0.299036578485171));
#193872=CARTESIAN_POINT('Ctrl Pts',(10.4240166046342,15.2,0.299459106077529));
#193873=CARTESIAN_POINT('Ctrl Pts',(10.426676534751,15.2,0.299897567165915));
#193874=CARTESIAN_POINT('Ctrl Pts',(10.4293364651094,15.2,0.300336028294128));
#193875=CARTESIAN_POINT('Ctrl Pts',(10.4320451858385,15.2,0.3007904271745));
#193876=CARTESIAN_POINT('Ctrl Pts',(10.4348018550753,15.2,0.301261169034604));
#193877=CARTESIAN_POINT('Ctrl Pts',(10.4375585240618,15.2,0.301731910851949));
#193878=CARTESIAN_POINT('Ctrl Pts',(10.4403631424584,15.2,0.302218995524499));
#193879=CARTESIAN_POINT('Ctrl Pts',(10.4432148865345,15.2,0.302722818258519));
#193880=CARTESIAN_POINT('Ctrl Pts',(10.4460666306106,15.2,0.303226640992539));
#193881=CARTESIAN_POINT('Ctrl Pts',(10.4489654999236,15.2,0.303747202499338));
#193882=CARTESIAN_POINT('Ctrl Pts',(10.4519106910645,15.2,0.304284883229058));
#193883=CARTESIAN_POINT('Ctrl Pts',(10.454855882473,15.2,0.304822564007616));
#193884=CARTESIAN_POINT('Ctrl Pts',(10.457847395379,15.2,0.30537736525496));
#193885=CARTESIAN_POINT('Ctrl Pts',(10.4608844430476,15.2,0.305949657037339));
#193886=CARTESIAN_POINT('Ctrl Pts',(10.4639214904403,15.2,0.306521948767735));
#193887=CARTESIAN_POINT('Ctrl Pts',(10.4670040750655,15.2,0.307111731904449));
#193888=CARTESIAN_POINT('Ctrl Pts',(10.4701314264538,15.2,0.307719363549812));
#193889=CARTESIAN_POINT('Ctrl Pts',(10.4732587778421,15.2,0.308326995195175));
#193890=CARTESIAN_POINT('Ctrl Pts',(10.4764308974185,15.2,0.30895247778913));
#193891=CARTESIAN_POINT('Ctrl Pts',(10.4796470310498,15.2,0.309596157431617));
#193892=CARTESIAN_POINT('Ctrl Pts',(10.4828631649731,15.2,0.310239837132572));
#193893=CARTESIAN_POINT('Ctrl Pts',(10.4861233150853,15.2,0.310901714860778));
#193894=CARTESIAN_POINT('Ctrl Pts',(10.4894267458516,15.2,0.311582129315788));
#193895=CARTESIAN_POINT('Ctrl Pts',(10.4927301763179,15.2,0.312262543708994));
#193896=CARTESIAN_POINT('Ctrl Pts',(10.4960768859061,15.2,0.312961492114412));
#193897=CARTESIAN_POINT('Ctrl Pts',(10.4994661554514,15.2,0.313679305589152));
#193898=CARTESIAN_POINT('Ctrl Pts',(10.5045500597695,15.2,0.314756025801263));
#193899=CARTESIAN_POINT('Ctrl Pts',(10.5097297184083,15.2,0.315875189777522));
#193900=CARTESIAN_POINT('Ctrl Pts',(10.5150027656016,15.2,0.317037864666682));
#193901=CARTESIAN_POINT('Ctrl Pts',(10.5185181307164,15.2,0.317812981329863));
#193902=CARTESIAN_POINT('Ctrl Pts',(10.5220750012849,15.2,0.318607435192985));
#193903=CARTESIAN_POINT('Ctrl Pts',(10.5256726944004,15.2,0.319421530572026));
#193904=CARTESIAN_POINT('Ctrl Pts',(10.5292703871891,15.2,0.320235625877121));
#193905=CARTESIAN_POINT('Ctrl Pts',(10.5329089033351,15.2,0.321069360902435));
#193906=CARTESIAN_POINT('Ctrl Pts',(10.5365875692182,15.2,0.321923033958673));
#193907=CARTESIAN_POINT('Ctrl Pts',(10.5408793463046,15.2,0.322918985909312));
#193908=CARTESIAN_POINT('Ctrl Pts',(10.5452257733782,15.2,0.32394207156903));
#193909=CARTESIAN_POINT('Ctrl Pts',(10.5496258056443,15.2,0.324992749614784));
#193910=CARTESIAN_POINT('Ctrl Pts',(10.5533972616766,15.2,0.325893330750115));
#193911=CARTESIAN_POINT('Ctrl Pts',(10.5572081035156,15.2,0.326814180788589));
#193912=CARTESIAN_POINT('Ctrl Pts',(10.5610576844766,15.2,0.327755578008712));
#193913=CARTESIAN_POINT('Ctrl Pts',(10.5649072654377,15.2,0.328696975228835));
#193914=CARTESIAN_POINT('Ctrl Pts',(10.5687955874054,15.2,0.32965892028309));
#193915=CARTESIAN_POINT('Ctrl Pts',(10.5727220183444,15.2,0.330641681413143));
#193916=CARTESIAN_POINT('Ctrl Pts',(10.57664844964,15.2,0.331624442632464));
#193917=CARTESIAN_POINT('Ctrl Pts',(10.5806129884488,15.2,0.332628018379362));
#193918=CARTESIAN_POINT('Ctrl Pts',(10.5846150166694,15.2,0.333652674353308));
#193919=CARTESIAN_POINT('Ctrl Pts',(10.5879500396414,15.2,0.334506554191987));
#193920=CARTESIAN_POINT('Ctrl Pts',(10.5913110962726,15.2,0.335375069576351));
#193921=CARTESIAN_POINT('Ctrl Pts',(10.5946978335402,15.2,0.336258370451084));
#193922=CARTESIAN_POINT('Ctrl Pts',(10.598084571177,15.2,0.337141671422097));
#193923=CARTESIAN_POINT('Ctrl Pts',(10.6014969886578,15.2,0.33803975623175));
#193924=CARTESIAN_POINT('Ctrl Pts',(10.6049347395586,15.2,0.338952770397199));
#193925=CARTESIAN_POINT('Ctrl Pts',(10.6083724904593,15.2,0.339865784562648));
#193926=CARTESIAN_POINT('Ctrl Pts',(10.6118355735781,15.2,0.340793726400022));
#193927=CARTESIAN_POINT('Ctrl Pts',(10.6153236465284,15.2,0.341736737348865));
#193928=CARTESIAN_POINT('Ctrl Pts',(10.6195093342969,15.2,0.34286835054915));
#193929=CARTESIAN_POINT('Ctrl Pts',(10.6237310072045,15.2,0.344021663537506));
#193930=CARTESIAN_POINT('Ctrl Pts',(10.6279880816889,15.2,0.345196912686388));
#193931=CARTESIAN_POINT('Ctrl Pts',(10.6329546680074,15.2,0.34656803653329));
#193932=CARTESIAN_POINT('Ctrl Pts',(10.6379694394394,15.2,0.347969016672691));
#193933=CARTESIAN_POINT('Ctrl Pts',(10.6430314853886,15.2,0.349400219347995));
#193934=CARTESIAN_POINT('Ctrl Pts',(10.6466472327203,15.2,0.350422507036886));
#193935=CARTESIAN_POINT('Ctrl Pts',(10.6502871008117,15.2,0.351460214759748));
#193936=CARTESIAN_POINT('Ctrl Pts',(10.6539507637271,15.2,0.35251346968949));
#193937=CARTESIAN_POINT('Ctrl Pts',(10.6576144266425,15.2,0.353566724619232));
#193938=CARTESIAN_POINT('Ctrl Pts',(10.6613018846863,15.2,0.354635525991042));
#193939=CARTESIAN_POINT('Ctrl Pts',(10.6650128150323,15.2,0.355720003420784));
#193940=CARTESIAN_POINT('Ctrl Pts',(10.670950303505,15.2,0.35745516728473));
#193941=CARTESIAN_POINT('Ctrl Pts',(10.676947882173,15.2,0.359230456968549));
#193942=CARTESIAN_POINT('Ctrl Pts',(10.6830042559775,15.2,0.361046372942483));
#193943=CARTESIAN_POINT('Ctrl Pts',(10.6867894896568,15.2,0.362181320441656));
#193944=CARTESIAN_POINT('Ctrl Pts',(10.690597690334,15.2,0.363332138263453));
#193945=CARTESIAN_POINT('Ctrl Pts',(10.6944285482495,15.2,0.364498943957065));
#193946=CARTESIAN_POINT('Ctrl Pts',(10.6990255779986,15.2,0.365899110865708));
#193947=CARTESIAN_POINT('Ctrl Pts',(10.7036552325434,15.2,0.367322300760531));
#193948=CARTESIAN_POINT('Ctrl Pts',(10.7083169852164,15.2,0.368768713674277));
#193949=CARTESIAN_POINT('Ctrl Pts',(10.7122017784753,15.2,0.369974057571991));
#193950=CARTESIAN_POINT('Ctrl Pts',(10.7161088597494,15.2,0.37119552690207));
#193951=CARTESIAN_POINT('Ctrl Pts',(10.720037929736,15.2,0.37243323732139));
#193952=CARTESIAN_POINT('Ctrl Pts',(10.7239670001508,15.2,0.37367094787562));
#193953=CARTESIAN_POINT('Ctrl Pts',(10.7279180576654,15.2,0.374924897346244));
#193954=CARTESIAN_POINT('Ctrl Pts',(10.7318908047469,15.2,0.376195195608797));
#193955=CARTESIAN_POINT('Ctrl Pts',(10.7350690025854,15.2,0.377211434274224));
#193956=CARTESIAN_POINT('Ctrl Pts',(10.7382610807822,15.2,0.378238137886603));
#193957=CARTESIAN_POINT('Ctrl Pts',(10.7414668906937,15.2,0.379275359225652));
#193958=CARTESIAN_POINT('Ctrl Pts',(10.7462756051243,15.2,0.380831191092906));
#193959=CARTESIAN_POINT('Ctrl Pts',(10.7511152114962,15.2,0.382410689796956));
#193960=CARTESIAN_POINT('Ctrl Pts',(10.7559852079846,15.2,0.384014037654331));
#193961=CARTESIAN_POINT('Ctrl Pts',(10.7592318726051,15.2,0.385082936323006));
#193962=CARTESIAN_POINT('Ctrl Pts',(10.7624920433078,15.2,0.38616243504294));
#193963=CARTESIAN_POINT('Ctrl Pts',(10.7657655745426,15.2,0.387252585047496));
#193964=CARTESIAN_POINT('Ctrl Pts',(10.7690391053314,15.2,0.38834273490352));
#193965=CARTESIAN_POINT('Ctrl Pts',(10.7723259951077,15.2,0.389443538258318));
#193966=CARTESIAN_POINT('Ctrl Pts',(10.7756260982794,15.2,0.390555043555383));
#193967=CARTESIAN_POINT('Ctrl Pts',(10.7789262019008,15.2,0.391666549003891));
#193968=CARTESIAN_POINT('Ctrl Pts',(10.7822395196787,15.2,0.392788760491325));
#193969=CARTESIAN_POINT('Ctrl Pts',(10.7855659063053,15.2,0.393921725109331));
#193970=CARTESIAN_POINT('Ctrl Pts',(10.7888922924786,15.2,0.395054689572969));
#193971=CARTESIAN_POINT('Ctrl Pts',(10.7922317484244,15.2,0.396198408117783));
#193972=CARTESIAN_POINT('Ctrl Pts',(10.7955841294268,15.2,0.397352930577851));
#193973=CARTESIAN_POINT('Ctrl Pts',(10.798936510886,15.2,0.398507453195223));
#193974=CARTESIAN_POINT('Ctrl Pts',(10.8023018184777,15.2,0.399672780759046));
#193975=CARTESIAN_POINT('Ctrl Pts',(10.8056799105105,15.2,0.400848960717413));
#193976=CARTESIAN_POINT('Ctrl Pts',(10.8099025253214,15.2,0.402319185585244));
#193977=CARTESIAN_POINT('Ctrl Pts',(10.8141451158166,15.2,0.403806369147529));
#193978=CARTESIAN_POINT('Ctrl Pts',(10.8184074065121,15.2,0.405310603106756));
#193979=CARTESIAN_POINT('Ctrl Pts',(10.8218172387897,15.2,0.406513990175762));
#193980=CARTESIAN_POINT('Ctrl Pts',(10.8252396803287,15.2,0.407728290050905));
#193981=CARTESIAN_POINT('Ctrl Pts',(10.82867459188,15.2,0.40895355028295));
#193982=CARTESIAN_POINT('Ctrl Pts',(10.8321095038992,15.2,0.410178810681938));
#193983=CARTESIAN_POINT('Ctrl Pts',(10.8355568850952,15.2,0.411415028613229));
#193984=CARTESIAN_POINT('Ctrl Pts',(10.8390165992439,15.2,0.412662253742459));
#193985=CARTESIAN_POINT('Ctrl Pts',(10.8424763129213,15.2,0.413909478701755));
#193986=CARTESIAN_POINT('Ctrl Pts',(10.8459483590941,15.2,0.415167708938981));
#193987=CARTESIAN_POINT('Ctrl Pts',(10.8494326006969,15.2,0.416436989334086));
#193988=CARTESIAN_POINT('Ctrl Pts',(10.8529168427744,15.2,0.41770626990213));
#193989=CARTESIAN_POINT('Ctrl Pts',(10.8564132802198,15.2,0.418986601104559));
#193990=CARTESIAN_POINT('Ctrl Pts',(10.8599217789666,15.2,0.42027802700827));
#193991=CARTESIAN_POINT('Ctrl Pts',(10.8634302777133,15.2,0.421569452911981));
#193992=CARTESIAN_POINT('Ctrl Pts',(10.8669508372309,15.2,0.422871973497555));
#193993=CARTESIAN_POINT('Ctrl Pts',(10.8704833233691,15.2,0.424185632681398));
#193994=CARTESIAN_POINT('Ctrl Pts',(10.8748989303199,15.2,0.425827706392724));
#193995=CARTESIAN_POINT('Ctrl Pts',(10.8793331730265,15.2,0.427487183231485));
#193996=CARTESIAN_POINT('Ctrl Pts',(10.8837857909425,15.2,0.429164146797266));
#193997=CARTESIAN_POINT('Ctrl Pts',(10.8873478858576,15.2,0.430505717869237));
#193998=CARTESIAN_POINT('Ctrl Pts',(10.8909217425684,15.2,0.431858478925605));
#193999=CARTESIAN_POINT('Ctrl Pts',(10.8945072280416,15.2,0.433222473999939));
#194000=CARTESIAN_POINT('Ctrl Pts',(10.8980927135147,15.2,0.434586469074274));
#194001=CARTESIAN_POINT('Ctrl Pts',(10.9016898290587,15.2,0.435961696741592));
#194002=CARTESIAN_POINT('Ctrl Pts',(10.9052984425899,15.2,0.437348197984971));
#194003=CARTESIAN_POINT('Ctrl Pts',(10.9098092087663,15.2,0.43908132425583));
#194004=CARTESIAN_POINT('Ctrl Pts',(10.9143379425911,15.2,0.44083206546284));
#194005=CARTESIAN_POINT('Ctrl Pts',(10.9188843919552,15.2,0.442600500060302));
#194006=CARTESIAN_POINT('Ctrl Pts',(10.9225215520412,15.2,0.444015247969582));
#194007=CARTESIAN_POINT('Ctrl Pts',(10.926170050006,15.2,0.445441318854928));
#194008=CARTESIAN_POINT('Ctrl Pts',(10.9298297569832,15.2,0.446878753266602));
#194009=CARTESIAN_POINT('Ctrl Pts',(10.9334894639605,15.2,0.448316187678278));
#194010=CARTESIAN_POINT('Ctrl Pts',(10.9371603813529,15.2,0.449764984041275));
#194011=CARTESIAN_POINT('Ctrl Pts',(10.9408423816103,15.2,0.45122518178869));
#194012=CARTESIAN_POINT('Ctrl Pts',(10.9454448811794,15.2,0.45305042867453));
#194013=CARTESIAN_POINT('Ctrl Pts',(10.9500646984447,15.2,0.454893489216396));
#194014=CARTESIAN_POINT('Ctrl Pts',(10.9547015878684,15.2,0.456754436998201));
#194015=CARTESIAN_POINT('Ctrl Pts',(10.9584111000139,15.2,0.458243195467058));
#194016=CARTESIAN_POINT('Ctrl Pts',(10.9621315375354,15.2,0.45974340237033));
#194017=CARTESIAN_POINT('Ctrl Pts',(10.9658627765166,15.2,0.46125509350827));
#194018=CARTESIAN_POINT('Ctrl Pts',(10.9695940154977,15.2,0.462766784646209));
#194019=CARTESIAN_POINT('Ctrl Pts',(10.9733360566467,15.2,0.464289959282709));
#194020=CARTESIAN_POINT('Ctrl Pts',(10.9770887756301,15.2,0.465824655700869));
#194021=CARTESIAN_POINT('Ctrl Pts',(10.9817796741037,15.2,0.467743026119018));
#194022=CARTESIAN_POINT('Ctrl Pts',(10.9864872562776,15.2,0.469679397765223));
#194023=CARTESIAN_POINT('Ctrl Pts',(10.9912112853761,15.2,0.471633837488921));
#194024=CARTESIAN_POINT('Ctrl Pts',(10.994990508346,15.2,0.473197389140058));
#194025=CARTESIAN_POINT('Ctrl Pts',(10.9987802556102,15.2,0.474772506657516));
#194026=CARTESIAN_POINT('Ctrl Pts',(11.0025804067057,15.2,0.476359222257194));
#194027=CARTESIAN_POINT('Ctrl Pts',(11.0063805583189,15.2,0.477945938073063));
#194028=CARTESIAN_POINT('Ctrl Pts',(11.0101911138653,15.2,0.479544252743684));
#194029=CARTESIAN_POINT('Ctrl Pts',(11.014011953408,15.2,0.481154200554837));
#194030=CARTESIAN_POINT('Ctrl Pts',(11.0187880025759,15.2,0.483166635209101));
#194031=CARTESIAN_POINT('Ctrl Pts',(11.0235801178886,15.2,0.485197245672002));
#194032=CARTESIAN_POINT('Ctrl Pts',(11.0283880688621,15.2,0.487246096992937));
#194033=CARTESIAN_POINT('Ctrl Pts',(11.0331960193116,15.2,0.489294948090548));
#194034=CARTESIAN_POINT('Ctrl Pts',(11.0380198053124,15.2,0.491362041494871));
#194035=CARTESIAN_POINT('Ctrl Pts',(11.0428591956169,15.2,0.493447436752176));
#194036=CARTESIAN_POINT('Ctrl Pts',(11.047698586449,15.2,0.495532832236788));
#194037=CARTESIAN_POINT('Ctrl Pts',(11.0525535802363,15.2,0.497636531907216));
#194038=CARTESIAN_POINT('Ctrl Pts',(11.0574239503045,15.2,0.499758596489045));
#194039=CARTESIAN_POINT('Ctrl Pts',(11.0613202465714,15.2,0.50145624824703));
#194040=CARTESIAN_POINT('Ctrl Pts',(11.0652263825158,15.2,0.503165653263345));
#194041=CARTESIAN_POINT('Ctrl Pts',(11.0691422429692,15.2,0.504886842976115));
#194042=CARTESIAN_POINT('Ctrl Pts',(11.0730581028892,15.2,0.506608032454372));
#194043=CARTESIAN_POINT('Ctrl Pts',(11.0769836887681,15.2,0.508341006089075));
#194044=CARTESIAN_POINT('Ctrl Pts',(11.0809188825565,15.2,0.510085794223005));
#194045=CARTESIAN_POINT('Ctrl Pts',(11.0848540768811,15.2,0.511830582594661));
#194046=CARTESIAN_POINT('Ctrl Pts',(11.0887988802455,15.2,0.513587184286891));
#194047=CARTESIAN_POINT('Ctrl Pts',(11.0927531780166,15.2,0.515355630716602));
#194048=CARTESIAN_POINT('Ctrl Pts',(11.097696049961,15.2,0.517566188633265));
#194049=CARTESIAN_POINT('Ctrl Pts',(11.1026537596467,15.2,0.519795253490901));
#194050=CARTESIAN_POINT('Ctrl Pts',(11.1076260815443,15.2,0.522042879751165));
#194051=CARTESIAN_POINT('Ctrl Pts',(11.1135928676047,15.2,0.524740031165488));
#194052=CARTESIAN_POINT('Ctrl Pts',(11.1195806986001,15.2,0.527463913042928));
#194053=CARTESIAN_POINT('Ctrl Pts',(11.1255891954642,15.2,0.530214619358469));
#194054=CARTESIAN_POINT('Ctrl Pts',(11.1295948604041,15.2,0.5320484237354));
#194055=CARTESIAN_POINT('Ctrl Pts',(11.1336097096201,15.2,0.533894149516556));
#194056=CARTESIAN_POINT('Ctrl Pts',(11.1376336320623,15.2,0.535751824618584));
#194057=CARTESIAN_POINT('Ctrl Pts',(11.1426635348408,15.2,0.538073918369565));
#194058=CARTESIAN_POINT('Ctrl Pts',(11.1477076159057,15.2,0.540414683626949));
#194059=CARTESIAN_POINT('Ctrl Pts',(11.1527656581038,15.2,0.542774171523905));
#194060=CARTESIAN_POINT('Ctrl Pts',(11.1568120915315,15.2,0.544661761687159));
#194061=CARTESIAN_POINT('Ctrl Pts',(11.1608674602089,15.2,0.54656133336473));
#194062=CARTESIAN_POINT('Ctrl Pts',(11.1649316553761,15.2,0.548472914152112));
#194063=CARTESIAN_POINT('Ctrl Pts',(11.168995851097,15.2,0.550384495199946));
#194064=CARTESIAN_POINT('Ctrl Pts',(11.1730688724662,15.2,0.55230808468256));
#194065=CARTESIAN_POINT('Ctrl Pts',(11.1771506121337,15.2,0.554243708399956));
#194066=CARTESIAN_POINT('Ctrl Pts',(11.1822527864399,15.2,0.556663237914836));
#194067=CARTESIAN_POINT('Ctrl Pts',(11.1873685805938,15.2,0.559101570438957));
#194068=CARTESIAN_POINT('Ctrl Pts',(11.1924977846704,15.2,0.561558755076914));
#194069=CARTESIAN_POINT('Ctrl Pts',(11.1955753070045,15.2,0.563033065806122));
#194070=CARTESIAN_POINT('Ctrl Pts',(11.1986576579149,15.2,0.564514162982364));
#194071=CARTESIAN_POINT('Ctrl Pts',(11.2017447905532,15.2,0.566002057137232));
#194072=CARTESIAN_POINT('Ctrl Pts',(11.2058609672172,15.2,0.56798591592029));
#194073=CARTESIAN_POINT('Ctrl Pts',(11.2099856463879,15.2,0.569981857509243));
#194074=CARTESIAN_POINT('Ctrl Pts',(11.2141187215492,15.2,0.571989907454961));
#194075=CARTESIAN_POINT('Ctrl Pts',(11.2182517972736,15.2,0.573997957674276));
#194076=CARTESIAN_POINT('Ctrl Pts',(11.2223932680549,15.2,0.576018112850739));
#194077=CARTESIAN_POINT('Ctrl Pts',(11.2265430292444,15.2,0.578050401026323));
#194078=CARTESIAN_POINT('Ctrl Pts',(11.2296553498538,15.2,0.579574617019562));
#194079=CARTESIAN_POINT('Ctrl Pts',(11.2327723341463,15.2,0.581105654914132));
#194080=CARTESIAN_POINT('Ctrl Pts',(11.2358939367554,15.2,0.582643526990209));
#194081=CARTESIAN_POINT('Ctrl Pts',(11.2390155393645,15.2,0.584181399066286));
#194082=CARTESIAN_POINT('Ctrl Pts',(11.2421417612895,15.2,0.585726104487905));
#194083=CARTESIAN_POINT('Ctrl Pts',(11.2452725569254,15.2,0.587277652097601));
#194084=CARTESIAN_POINT('Ctrl Pts',(11.2494469514857,15.2,0.589346382431773));
#194085=CARTESIAN_POINT('Ctrl Pts',(11.2536294794081,15.2,0.591427276953513));
#194086=CARTESIAN_POINT('Ctrl Pts',(11.2578200365259,15.2,0.593520358679495));
#194087=CARTESIAN_POINT('Ctrl Pts',(11.2609629540788,15.2,0.59509016983139));
#194088=CARTESIAN_POINT('Ctrl Pts',(11.2641103876363,15.2,0.59666683680169));
#194089=CARTESIAN_POINT('Ctrl Pts',(11.2672622932861,15.2,0.598250367001377));
#194090=CARTESIAN_POINT('Ctrl Pts',(11.2714648339617,15.2,0.60036174050507));
#194091=CARTESIAN_POINT('Ctrl Pts',(11.2756753271309,15.2,0.602485317171043));
#194092=CARTESIAN_POINT('Ctrl Pts',(11.2798936682852,15.2,0.604621117884072));
#194093=CARTESIAN_POINT('Ctrl Pts',(11.2830574248694,15.2,0.606222968782597));
#194094=CARTESIAN_POINT('Ctrl Pts',(11.2862255958965,15.2,0.607831696166409));
#194095=CARTESIAN_POINT('Ctrl Pts',(11.2893981389832,15.2,0.609447308068814));
#194096=CARTESIAN_POINT('Ctrl Pts',(11.2925706814935,15.2,0.611062919677716));
#194097=CARTESIAN_POINT('Ctrl Pts',(11.2957475944786,15.2,0.612685416652924));
#194098=CARTESIAN_POINT('Ctrl Pts',(11.2989288370717,15.2,0.614314806719324));
#194099=CARTESIAN_POINT('Ctrl Pts',(11.3031704936699,15.2,0.616487326709188));
#194100=CARTESIAN_POINT('Ctrl Pts',(11.3074198466527,15.2,0.618672101302142));
#194101=CARTESIAN_POINT('Ctrl Pts',(11.3116767933039,15.2,0.62086915139906));
#194102=CARTESIAN_POINT('Ctrl Pts',(11.3148695040173,15.2,0.622516939345932));
#194103=CARTESIAN_POINT('Ctrl Pts',(11.3180664866986,15.2,0.624171632686409));
#194104=CARTESIAN_POINT('Ctrl Pts',(11.3212676989145,15.2,0.625833238595509));
#194105=CARTESIAN_POINT('Ctrl Pts',(11.3244689105487,15.2,0.62749484420275));
#194106=CARTESIAN_POINT('Ctrl Pts',(11.3276743522767,15.2,0.62916336240053));
#194107=CARTESIAN_POINT('Ctrl Pts',(11.3308839806126,15.2,0.63083880204916));
#194108=CARTESIAN_POINT('Ctrl Pts',(11.3340936089485,15.2,0.632514241697791));
#194109=CARTESIAN_POINT('Ctrl Pts',(11.337307424884,15.2,0.634196602661629));
#194110=CARTESIAN_POINT('Ctrl Pts',(11.3405253855591,15.2,0.635885892725854));
#194111=CARTESIAN_POINT('Ctrl Pts',(11.3448159995977,15.2,0.638138279375857));
#194112=CARTESIAN_POINT('Ctrl Pts',(11.3491139843876,15.2,0.640402984712273));
#194113=CARTESIAN_POINT('Ctrl Pts',(11.3534192378127,15.2,0.642680026135979));
#194114=CARTESIAN_POINT('Ctrl Pts',(11.3566481786147,15.2,0.644387807591567));
#194115=CARTESIAN_POINT('Ctrl Pts',(11.3598812104179,15.2,0.646102528940771));
#194116=CARTESIAN_POINT('Ctrl Pts',(11.3631182892223,15.2,0.647824197358602));
#194117=CARTESIAN_POINT('Ctrl Pts',(11.3685134191907,15.2,0.650693643991859));
#194118=CARTESIAN_POINT('Ctrl Pts',(11.3739197946772,15.2,0.653582388915906));
#194119=CARTESIAN_POINT('Ctrl Pts',(11.3793372227663,15.2,0.65649046561123));
#194120=CARTESIAN_POINT('Ctrl Pts',(11.3825876804465,15.2,0.658235312072198));
#194121=CARTESIAN_POINT('Ctrl Pts',(11.3858421171195,15.2,0.659987118460131));
#194122=CARTESIAN_POINT('Ctrl Pts',(11.3891004914269,15.2,0.661745891841689));
#194123=CARTESIAN_POINT('Ctrl Pts',(11.3945311144834,15.2,0.664677180384938));
#194124=CARTESIAN_POINT('Ctrl Pts',(11.3999726797678,15.2,0.667627819647947));
#194125=CARTESIAN_POINT('Ctrl Pts',(11.4054249967131,15.2,0.670597845621758));
#194126=CARTESIAN_POINT('Ctrl Pts',(11.4086963867614,15.2,0.672379861141297));
#194127=CARTESIAN_POINT('Ctrl Pts',(11.4119716465893,15.2,0.674168855272206));
#194128=CARTESIAN_POINT('Ctrl Pts',(11.415250734426,15.2,0.67596483538082));
#194129=CARTESIAN_POINT('Ctrl Pts',(11.4185298222628,15.2,0.677760815489433));
#194130=CARTESIAN_POINT('Ctrl Pts',(11.4218127380273,15.2,0.679563780979161));
#194131=CARTESIAN_POINT('Ctrl Pts',(11.4250994433249,15.2,0.681373739455673));
#194132=CARTESIAN_POINT('Ctrl Pts',(11.4283861486225,15.2,0.683183697932186));
#194133=CARTESIAN_POINT('Ctrl Pts',(11.4316766450363,15.2,0.685000647549539));
#194134=CARTESIAN_POINT('Ctrl Pts',(11.4349708937083,15.2,0.686824596483266));
#194135=CARTESIAN_POINT('Ctrl Pts',(11.4382651423802,15.2,0.688648545416993));
#194136=CARTESIAN_POINT('Ctrl Pts',(11.4415631447104,15.2,0.690479491583784));
#194137=CARTESIAN_POINT('Ctrl Pts',(11.4448648556318,15.2,0.692317444099715));
#194138=CARTESIAN_POINT('Ctrl Pts',(11.4481665665531,15.2,0.694155396615647));
#194139=CARTESIAN_POINT('Ctrl Pts',(11.4514719840484,15.2,0.696000354800605));
#194140=CARTESIAN_POINT('Ctrl Pts',(11.4547810613847,15.2,0.697852327408362));
#194141=CARTESIAN_POINT('Ctrl Pts',(11.4580901387211,15.2,0.69970430001612));
#194142=CARTESIAN_POINT('Ctrl Pts',(11.4614028748479,15.2,0.701563286711907));
#194143=CARTESIAN_POINT('Ctrl Pts',(11.4647192420186,15.2,0.703429290643153));
#194144=CARTESIAN_POINT('Ctrl Pts',(11.4691410653145,15.2,0.705917296110807));
#194145=CARTESIAN_POINT('Ctrl Pts',(11.4735693507915,15.2,0.7084177809819));
#194146=CARTESIAN_POINT('Ctrl Pts',(11.4780040719999,15.2,0.710930734999984));
#194147=CARTESIAN_POINT('Ctrl Pts',(10.3708900239999,12.2,0.292001928999985));
#194148=CARTESIAN_POINT('Ctrl Pts',(10.3726650375455,12.2,0.29220550820869));
#194149=CARTESIAN_POINT('Ctrl Pts',(10.3744962441107,12.2,0.292420934685804));
#194150=CARTESIAN_POINT('Ctrl Pts',(10.3763825855683,12.2,0.292648744500013));
#194151=CARTESIAN_POINT('Ctrl Pts',(10.3782780239178,12.2,0.2928776529283));
#194152=CARTESIAN_POINT('Ctrl Pts',(10.3802291370813,12.2,0.293119061022275));
#194153=CARTESIAN_POINT('Ctrl Pts',(10.3822349054607,12.2,0.293373492299608));
#194154=CARTESIAN_POINT('Ctrl Pts',(10.3845749682966,12.2,0.293670328755164));
#194155=CARTESIAN_POINT('Ctrl Pts',(10.38698942021,12.2,0.29398488688512));
#194156=CARTESIAN_POINT('Ctrl Pts',(10.3894766898008,12.2,0.29431796796051));
#194157=CARTESIAN_POINT('Ctrl Pts',(10.3916086354134,12.2,0.294603466058474));
#194158=CARTESIAN_POINT('Ctrl Pts',(10.3937940804213,12.2,0.294902569521762));
#194159=CARTESIAN_POINT('Ctrl Pts',(10.3960320642415,12.2,0.295215760805293));
#194160=CARTESIAN_POINT('Ctrl Pts',(10.39864304506,12.2,0.295581150593408));
#194161=CARTESIAN_POINT('Ctrl Pts',(10.4013255344682,12.2,0.295965719960751));
#194162=CARTESIAN_POINT('Ctrl Pts',(10.404078049501,12.2,0.296370203462172));
#194163=CARTESIAN_POINT('Ctrl Pts',(10.4064373483761,12.2,0.296716903646737));
#194164=CARTESIAN_POINT('Ctrl Pts',(10.4088480966947,12.2,0.29707823717121));
#194165=CARTESIAN_POINT('Ctrl Pts',(10.4113093847881,12.2,0.297454650294741));
#194166=CARTESIAN_POINT('Ctrl Pts',(10.4137706726579,12.2,0.297831063384081));
#194167=CARTESIAN_POINT('Ctrl Pts',(10.4162825002596,12.2,0.298222558514745));
#194168=CARTESIAN_POINT('Ctrl Pts',(10.4188439839998,12.2,0.298629568499958));
#194169=CARTESIAN_POINT('Ctrl Pts',(10.4214054677401,12.2,0.299036578485171));
#194170=CARTESIAN_POINT('Ctrl Pts',(10.4240166046342,12.2,0.299459106077528));
#194171=CARTESIAN_POINT('Ctrl Pts',(10.426676534751,12.2,0.299897567165915));
#194172=CARTESIAN_POINT('Ctrl Pts',(10.429779786715,12.2,0.300409105128917));
#194173=CARTESIAN_POINT('Ctrl Pts',(10.4329494469773,12.2,0.300942337035746));
#194174=CARTESIAN_POINT('Ctrl Pts',(10.4361841812499,12.2,0.301497903516621));
#194175=CARTESIAN_POINT('Ctrl Pts',(10.4389568104824,12.2,0.301974103332653));
#194176=CARTESIAN_POINT('Ctrl Pts',(10.4417772507362,12.2,0.302466714036415));
#194177=CARTESIAN_POINT('Ctrl Pts',(10.4446446819393,12.2,0.30297612595905));
#194178=CARTESIAN_POINT('Ctrl Pts',(10.4475121134028,12.2,0.303485537927957));
#194179=CARTESIAN_POINT('Ctrl Pts',(10.4504265340331,12.2,0.304011754270072));
#194180=CARTESIAN_POINT('Ctrl Pts',(10.4533871436142,12.2,0.304555152050855));
#194181=CARTESIAN_POINT('Ctrl Pts',(10.4563477529265,12.2,0.305098549782279));
#194182=CARTESIAN_POINT('Ctrl Pts',(10.4593545518565,12.2,0.30565912976856));
#194183=CARTESIAN_POINT('Ctrl Pts',(10.4624067580096,12.2,0.306237262250217));
#194184=CARTESIAN_POINT('Ctrl Pts',(10.4654589641627,12.2,0.306815394731874));
#194185=CARTESIAN_POINT('Ctrl Pts',(10.4685565750616,12.2,0.307411077481327));
#194186=CARTESIAN_POINT('Ctrl Pts',(10.4716988292788,12.2,0.308024668208254));
#194187=CARTESIAN_POINT('Ctrl Pts',(10.4748410837814,12.2,0.308638258990916));
#194188=CARTESIAN_POINT('Ctrl Pts',(10.478027976748,12.2,0.309269760050793));
#194189=CARTESIAN_POINT('Ctrl Pts',(10.4812587633437,12.2,0.309919515587448));
#194190=CARTESIAN_POINT('Ctrl Pts',(10.484489549646,12.2,0.310569271065084));
#194191=CARTESIAN_POINT('Ctrl Pts',(10.4877642267818,12.2,0.311237281638716));
#194192=CARTESIAN_POINT('Ctrl Pts',(10.4910820642597,12.2,0.311923882283599));
#194193=CARTESIAN_POINT('Ctrl Pts',(10.4943999017377,12.2,0.312610482928481));
#194194=CARTESIAN_POINT('Ctrl Pts',(10.4977608967567,12.2,0.3133156758627));
#194195=CARTESIAN_POINT('Ctrl Pts',(10.5011643332979,12.2,0.314039785418901));
#194196=CARTESIAN_POINT('Ctrl Pts',(10.5045677701482,12.2,0.314763895040875));
#194197=CARTESIAN_POINT('Ctrl Pts',(10.5080136477538,12.2,0.315506921331853));
#194198=CARTESIAN_POINT('Ctrl Pts',(10.5115012636134,12.2,0.316269181791375));
#194199=CARTESIAN_POINT('Ctrl Pts',(10.5149888791561,12.2,0.31703144218166));
#194200=CARTESIAN_POINT('Ctrl Pts',(10.5185182327559,12.2,0.317812935846945));
#194201=CARTESIAN_POINT('Ctrl Pts',(10.5220886344613,12.2,0.318613971068692));
#194202=CARTESIAN_POINT('Ctrl Pts',(10.5256590361667,12.2,0.319415006290438));
#194203=CARTESIAN_POINT('Ctrl Pts',(10.5292704866605,12.2,0.320235581935627));
#194204=CARTESIAN_POINT('Ctrl Pts',(10.532922311276,12.2,0.321075996237563));
#194205=CARTESIAN_POINT('Ctrl Pts',(10.5365741358916,12.2,0.321916410539499));
#194206=CARTESIAN_POINT('Ctrl Pts',(10.5402663324814,12.2,0.32277666341235));
#194207=CARTESIAN_POINT('Ctrl Pts',(10.5439982403431,12.2,0.323657045628992));
#194208=CARTESIAN_POINT('Ctrl Pts',(10.5477301485438,12.2,0.324537427925602));
#194209=CARTESIAN_POINT('Ctrl Pts',(10.55150176864,12.2,0.325437938149148));
#194210=CARTESIAN_POINT('Ctrl Pts',(10.5553124489327,12.2,0.32635885753356));
#194211=CARTESIAN_POINT('Ctrl Pts',(10.5597582420884,12.2,0.327433263356567));
#194212=CARTESIAN_POINT('Ctrl Pts',(10.5642572009667,12.2,0.328535448838623));
#194213=CARTESIAN_POINT('Ctrl Pts',(10.5688083138747,12.2,0.329665848627676));
#194214=CARTESIAN_POINT('Ctrl Pts',(10.5720591090114,12.2,0.330473277098718));
#194215=CARTESIAN_POINT('Ctrl Pts',(10.5753365152977,12.2,0.33129509770841));
#194216=CARTESIAN_POINT('Ctrl Pts',(10.5786401687678,12.2,0.332131466873889));
#194217=CARTESIAN_POINT('Ctrl Pts',(10.5819438222378,12.2,0.332967836039368));
#194218=CARTESIAN_POINT('Ctrl Pts',(10.5852737236279,12.2,0.333818752173959));
#194219=CARTESIAN_POINT('Ctrl Pts',(10.5886295173354,12.2,0.334684364091183));
#194220=CARTESIAN_POINT('Ctrl Pts',(10.5919853110429,12.2,0.335549976008407));
#194221=CARTESIAN_POINT('Ctrl Pts',(10.5953669967508,12.2,0.336430285558935));
#194222=CARTESIAN_POINT('Ctrl Pts',(10.5987742234855,12.2,0.337325437224829));
#194223=CARTESIAN_POINT('Ctrl Pts',(10.6021814502203,12.2,0.338220588890723));
#194224=CARTESIAN_POINT('Ctrl Pts',(10.6056142165808,12.2,0.339130582162553));
#194225=CARTESIAN_POINT('Ctrl Pts',(10.6090721785239,12.2,0.340055561397878));
#194226=CARTESIAN_POINT('Ctrl Pts',(10.612530140467,12.2,0.340980540633203));
#194227=CARTESIAN_POINT('Ctrl Pts',(10.6160132978765,12.2,0.341920504778467));
#194228=CARTESIAN_POINT('Ctrl Pts',(10.6195213082396,12.2,0.342875592491096));
#194229=CARTESIAN_POINT('Ctrl Pts',(10.6230293186027,12.2,0.343830680203724));
#194230=CARTESIAN_POINT('Ctrl Pts',(10.6265621837777,12.2,0.344800893372168));
#194231=CARTESIAN_POINT('Ctrl Pts',(10.6301195657916,12.2,0.345786365941613));
#194232=CARTESIAN_POINT('Ctrl Pts',(10.6336769478055,12.2,0.346771838511057));
#194233=CARTESIAN_POINT('Ctrl Pts',(10.6372588474132,12.2,0.347772571140291));
#194234=CARTESIAN_POINT('Ctrl Pts',(10.6408649342352,12.2,0.348788696283835));
#194235=CARTESIAN_POINT('Ctrl Pts',(10.6444710210572,12.2,0.349804821427379));
#194236=CARTESIAN_POINT('Ctrl Pts',(10.6481012925933,12.2,0.35083634071771));
#194237=CARTESIAN_POINT('Ctrl Pts',(10.651755424539,12.2,0.351883381551851));
#194238=CARTESIAN_POINT('Ctrl Pts',(10.6561403827145,12.2,0.353139830507171));
#194239=CARTESIAN_POINT('Ctrl Pts',(10.6605596987789,12.2,0.354418630552376));
#194240=CARTESIAN_POINT('Ctrl Pts',(10.6650128150323,12.2,0.355720003420783));
#194241=CARTESIAN_POINT('Ctrl Pts',(10.6702081175976,12.2,0.357238271846064));
#194242=CARTESIAN_POINT('Ctrl Pts',(10.6754494275741,12.2,0.35878726088698));
#194243=CARTESIAN_POINT('Ctrl Pts',(10.6807358750053,12.2,0.360367307815519));
#194244=CARTESIAN_POINT('Ctrl Pts',(10.684511908826,12.2,0.361495912746902));
#194245=CARTESIAN_POINT('Ctrl Pts',(10.6883109732599,12.2,0.3626403632751));
#194246=CARTESIAN_POINT('Ctrl Pts',(10.6921327554833,12.2,0.363800778275934));
#194247=CARTESIAN_POINT('Ctrl Pts',(10.6959545377067,12.2,0.364961193276767));
#194248=CARTESIAN_POINT('Ctrl Pts',(10.6997990398407,12.2,0.366137573777189));
#194249=CARTESIAN_POINT('Ctrl Pts',(10.7036659519946,12.2,0.367330034611361));
#194250=CARTESIAN_POINT('Ctrl Pts',(10.7075328641485,12.2,0.368522495445535));
#194251=CARTESIAN_POINT('Ctrl Pts',(10.711422188446,12.2,0.369731037763199));
#194252=CARTESIAN_POINT('Ctrl Pts',(10.7153336199624,12.2,0.37095577365884));
#194253=CARTESIAN_POINT('Ctrl Pts',(10.7192450514787,12.2,0.372180509554481));
#194254=CARTESIAN_POINT('Ctrl Pts',(10.7231785915877,12.2,0.373421440913062));
#194255=CARTESIAN_POINT('Ctrl Pts',(10.7271339395756,12.2,0.374678678206065));
#194256=CARTESIAN_POINT('Ctrl Pts',(10.7302982177072,12.2,0.375684467958244));
#194257=CARTESIAN_POINT('Ctrl Pts',(10.7334764524204,12.2,0.376700691622952));
#194258=CARTESIAN_POINT('Ctrl Pts',(10.7366684932141,12.2,0.377727408649442));
#194259=CARTESIAN_POINT('Ctrl Pts',(10.7398605344427,12.2,0.378754125815822));
#194260=CARTESIAN_POINT('Ctrl Pts',(10.743066382813,12.2,0.379791333552787));
#194261=CARTESIAN_POINT('Ctrl Pts',(10.7462858844838,12.2,0.380839086885371));
#194262=CARTESIAN_POINT('Ctrl Pts',(10.749505385716,12.2,0.381886840075198));
#194263=CARTESIAN_POINT('Ctrl Pts',(10.7527385438064,12.2,0.382945139131294));
#194264=CARTESIAN_POINT('Ctrl Pts',(10.7559852079846,12.2,0.384014037654331));
#194265=CARTESIAN_POINT('Ctrl Pts',(10.7592318726051,12.2,0.385082936323006));
#194266=CARTESIAN_POINT('Ctrl Pts',(10.7624920433078,12.2,0.38616243504294));
#194267=CARTESIAN_POINT('Ctrl Pts',(10.7657655745426,12.2,0.387252585047496));
#194268=CARTESIAN_POINT('Ctrl Pts',(10.7690391053314,12.2,0.388342734903519));
#194269=CARTESIAN_POINT('Ctrl Pts',(10.7723259951077,12.2,0.389443538258318));
#194270=CARTESIAN_POINT('Ctrl Pts',(10.7756260982794,12.2,0.390555043555382));
#194271=CARTESIAN_POINT('Ctrl Pts',(10.7789262019008,12.2,0.39166654900389));
#194272=CARTESIAN_POINT('Ctrl Pts',(10.7822395196787,12.2,0.392788760491324));
#194273=CARTESIAN_POINT('Ctrl Pts',(10.7855659063053,12.2,0.39392172510933));
#194274=CARTESIAN_POINT('Ctrl Pts',(10.7888922924786,12.2,0.395054689572968));
#194275=CARTESIAN_POINT('Ctrl Pts',(10.7922317484244,12.2,0.396198408117784));
#194276=CARTESIAN_POINT('Ctrl Pts',(10.7955841294268,12.2,0.397352930577852));
#194277=CARTESIAN_POINT('Ctrl Pts',(10.798936510886,12.2,0.398507453195224));
#194278=CARTESIAN_POINT('Ctrl Pts',(10.8023018184777,12.2,0.399672780759045));
#194279=CARTESIAN_POINT('Ctrl Pts',(10.8056799105105,12.2,0.400848960717412));
#194280=CARTESIAN_POINT('Ctrl Pts',(10.8090580020831,12.2,0.402025140515525));
#194281=CARTESIAN_POINT('Ctrl Pts',(10.8124488787035,12.2,0.403212174061467));
#194282=CARTESIAN_POINT('Ctrl Pts',(10.8158523977018,12.2,0.404410107795754));
#194283=CARTESIAN_POINT('Ctrl Pts',(10.8192559171637,12.2,0.405608041693259));
#194284=CARTESIAN_POINT('Ctrl Pts',(10.8226720809103,12.2,0.406816876258458));
#194285=CARTESIAN_POINT('Ctrl Pts',(10.8261007490416,12.2,0.408036659491605));
#194286=CARTESIAN_POINT('Ctrl Pts',(10.8295294171729,12.2,0.409256442724752));
#194287=CARTESIAN_POINT('Ctrl Pts',(10.8329705894834,12.2,0.410487172836951));
#194288=CARTESIAN_POINT('Ctrl Pts',(10.8364241288396,12.2,0.411728897961302));
#194289=CARTESIAN_POINT('Ctrl Pts',(10.8398776677252,12.2,0.412970622916468));
#194290=CARTESIAN_POINT('Ctrl Pts',(10.8433435737133,12.2,0.414223341143917));
#194291=CARTESIAN_POINT('Ctrl Pts',(10.8468217087225,12.2,0.41548709999075));
#194292=CARTESIAN_POINT('Ctrl Pts',(10.8502998442056,12.2,0.41675085900977));
#194293=CARTESIAN_POINT('Ctrl Pts',(10.8537902098138,12.2,0.418025655425087));
#194294=CARTESIAN_POINT('Ctrl Pts',(10.8572926693392,12.2,0.419311537218523));
#194295=CARTESIAN_POINT('Ctrl Pts',(10.8607951283875,12.2,0.420597418836759));
#194296=CARTESIAN_POINT('Ctrl Pts',(10.8643096819758,12.2,0.42189438352578));
#194297=CARTESIAN_POINT('Ctrl Pts',(10.8678361961867,12.2,0.423202475918111));
#194298=CARTESIAN_POINT('Ctrl Pts',(10.8713627108781,12.2,0.424510568488671));
#194299=CARTESIAN_POINT('Ctrl Pts',(10.8749011853905,12.2,0.425829789244775));
#194300=CARTESIAN_POINT('Ctrl Pts',(10.8784514870401,12.2,0.427160179218054));
#194301=CARTESIAN_POINT('Ctrl Pts',(10.8820017882061,12.2,0.428490569010066));
#194302=CARTESIAN_POINT('Ctrl Pts',(10.885563915548,12.2,0.429832129409109));
#194303=CARTESIAN_POINT('Ctrl Pts',(10.8891377385328,12.2,0.431184901131124));
#194304=CARTESIAN_POINT('Ctrl Pts',(10.8927115620046,12.2,0.432537673037453));
#194305=CARTESIAN_POINT('Ctrl Pts',(10.8962970795584,12.2,0.433901657709012));
#194306=CARTESIAN_POINT('Ctrl Pts',(10.8998941623107,12.2,0.435276895562474));
#194307=CARTESIAN_POINT('Ctrl Pts',(10.903491244573,12.2,0.436652133228559));
#194308=CARTESIAN_POINT('Ctrl Pts',(10.9070998892519,12.2,0.438038624931487));
#194309=CARTESIAN_POINT('Ctrl Pts',(10.9107199696913,12.2,0.439436409330509));
#194310=CARTESIAN_POINT('Ctrl Pts',(10.9152450706106,12.2,0.441183639972123));
#194311=CARTESIAN_POINT('Ctrl Pts',(10.9197880365582,12.2,0.442948518389949));
#194312=CARTESIAN_POINT('Ctrl Pts',(10.9243486189184,12.2,0.444731119708467));
#194313=CARTESIAN_POINT('Ctrl Pts',(10.9279970850054,12.2,0.446157200841003));
#194314=CARTESIAN_POINT('Ctrl Pts',(10.931656823766,12.2,0.447594625763789));
#194315=CARTESIAN_POINT('Ctrl Pts',(10.9353277093001,12.2,0.449043431676821));
#194316=CARTESIAN_POINT('Ctrl Pts',(10.938998594334,12.2,0.450492237392454));
#194317=CARTESIAN_POINT('Ctrl Pts',(10.9426806255991,12.2,0.451952425403687));
#194318=CARTESIAN_POINT('Ctrl Pts',(10.9463736774807,12.2,0.453424033078131));
#194319=CARTESIAN_POINT('Ctrl Pts',(10.9500667298655,12.2,0.454895640953082));
#194320=CARTESIAN_POINT('Ctrl Pts',(10.95377080242,12.2,0.456378668612243));
#194321=CARTESIAN_POINT('Ctrl Pts',(10.9574857693454,12.2,0.45787315313889));
#194322=CARTESIAN_POINT('Ctrl Pts',(10.9612007357646,12.2,0.459367637461913));
#194323=CARTESIAN_POINT('Ctrl Pts',(10.964926596615,12.2,0.460873580265958));
#194324=CARTESIAN_POINT('Ctrl Pts',(10.968663228364,12.2,0.462391015251845));
#194325=CARTESIAN_POINT('Ctrl Pts',(10.9723998606221,12.2,0.463908450444482));
#194326=CARTESIAN_POINT('Ctrl Pts',(10.9761472635951,12.2,0.465437379513202));
#194327=CARTESIAN_POINT('Ctrl Pts',(10.9799053144666,12.2,0.466977838541603));
#194328=CARTESIAN_POINT('Ctrl Pts',(10.9836633653381,12.2,0.468518297570005));
#194329=CARTESIAN_POINT('Ctrl Pts',(10.9874320618913,12.2,0.470070285624747));
#194330=CARTESIAN_POINT('Ctrl Pts',(10.9912112853761,12.2,0.471633837488919));
#194331=CARTESIAN_POINT('Ctrl Pts',(10.994990508346,12.2,0.473197389140057));
#194332=CARTESIAN_POINT('Ctrl Pts',(10.9987802556102,12.2,0.474772506657516));
#194333=CARTESIAN_POINT('Ctrl Pts',(11.0025804067057,12.2,0.476359222257194));
#194334=CARTESIAN_POINT('Ctrl Pts',(11.0063805583189,12.2,0.477945938073062));
#194335=CARTESIAN_POINT('Ctrl Pts',(11.0101911138653,12.2,0.479544252743683));
#194336=CARTESIAN_POINT('Ctrl Pts',(11.014011953408,12.2,0.481154200554837));
#194337=CARTESIAN_POINT('Ctrl Pts',(11.0187880025759,12.2,0.483166635209101));
#194338=CARTESIAN_POINT('Ctrl Pts',(11.0235801178886,12.2,0.485197245672001));
#194339=CARTESIAN_POINT('Ctrl Pts',(11.0283880688621,12.2,0.487246096992937));
#194340=CARTESIAN_POINT('Ctrl Pts',(11.0322344293265,12.2,0.48888517791569));
#194341=CARTESIAN_POINT('Ctrl Pts',(11.0360909250208,12.2,0.490535934007757));
#194342=CARTESIAN_POINT('Ctrl Pts',(11.0399574362223,12.2,0.492198395490474));
#194343=CARTESIAN_POINT('Ctrl Pts',(11.0438239479505,12.2,0.493860857199702));
#194344=CARTESIAN_POINT('Ctrl Pts',(11.0477004757558,12.2,0.495535024951953));
#194345=CARTESIAN_POINT('Ctrl Pts',(11.0515869026353,12.2,0.497220930767254));
#194346=CARTESIAN_POINT('Ctrl Pts',(11.0554733289853,12.2,0.49890683635285));
#194347=CARTESIAN_POINT('Ctrl Pts',(11.059369653609,12.2,0.500604480314707));
#194348=CARTESIAN_POINT('Ctrl Pts',(11.0632757601223,12.2,0.502313893118637));
#194349=CARTESIAN_POINT('Ctrl Pts',(11.0671818671679,12.2,0.504023306155474));
#194350=CARTESIAN_POINT('Ctrl Pts',(11.0710977566781,12.2,0.505744488255535));
#194351=CARTESIAN_POINT('Ctrl Pts',(11.0750233138113,12.2,0.507477469493138));
#194352=CARTESIAN_POINT('Ctrl Pts',(11.0789488704095,12.2,0.509210450494623));
#194353=CARTESIAN_POINT('Ctrl Pts',(11.0828840924951,12.2,0.510955231381379));
#194354=CARTESIAN_POINT('Ctrl Pts',(11.0868288663942,12.2,0.512711840848114));
#194355=CARTESIAN_POINT('Ctrl Pts',(11.0907736408308,12.2,0.514468450554187));
#194356=CARTESIAN_POINT('Ctrl Pts',(11.0947279667574,12.2,0.516236889897792));
#194357=CARTESIAN_POINT('Ctrl Pts',(11.0986917323074,12.2,0.518017187662257));
#194358=CARTESIAN_POINT('Ctrl Pts',(11.1026554973173,12.2,0.519797485184156));
#194359=CARTESIAN_POINT('Ctrl Pts',(11.10662869908,12.2,0.521589640343834));
#194360=CARTESIAN_POINT('Ctrl Pts',(11.1106112258971,12.2,0.523393683229892));
#194361=CARTESIAN_POINT('Ctrl Pts',(11.1145937532567,12.2,0.525197726361749));
#194362=CARTESIAN_POINT('Ctrl Pts',(11.1185856064668,12.2,0.527013655557412));
#194363=CARTESIAN_POINT('Ctrl Pts',(11.1225866715188,12.2,0.528841501157811));
#194364=CARTESIAN_POINT('Ctrl Pts',(11.1265877360256,12.2,0.530669346509165));
#194365=CARTESIAN_POINT('Ctrl Pts',(11.1305980138639,12.2,0.532509105863678));
#194366=CARTESIAN_POINT('Ctrl Pts',(11.1346173923677,12.2,0.534360807988857));
#194367=CARTESIAN_POINT('Ctrl Pts',(11.1386367714192,12.2,0.536212510366331));
#194368=CARTESIAN_POINT('Ctrl Pts',(11.1426652509226,12.2,0.538076154854329));
#194369=CARTESIAN_POINT('Ctrl Pts',(11.1467027219943,12.2,0.539951769242885));
#194370=CARTESIAN_POINT('Ctrl Pts',(11.1497308250231,12.2,0.541358479906526));
#194371=CARTESIAN_POINT('Ctrl Pts',(11.1527639856271,12.2,0.542771924060498));
#194372=CARTESIAN_POINT('Ctrl Pts',(11.1558021562388,12.2,0.544192110765316));
#194373=CARTESIAN_POINT('Ctrl Pts',(11.1588403268505,12.2,0.545612297470135));
#194374=CARTESIAN_POINT('Ctrl Pts',(11.1618835088623,12.2,0.547039228496462));
#194375=CARTESIAN_POINT('Ctrl Pts',(11.1649316553761,12.2,0.548472914152111));
#194376=CARTESIAN_POINT('Ctrl Pts',(11.1679798018899,12.2,0.54990659980776));
#194377=CARTESIAN_POINT('Ctrl Pts',(11.1710329121117,12.2,0.551347040037955));
#194378=CARTESIAN_POINT('Ctrl Pts',(11.1740909425416,12.2,0.552794246192785));
#194379=CARTESIAN_POINT('Ctrl Pts',(11.177148973527,12.2,0.554241452610524));
#194380=CARTESIAN_POINT('Ctrl Pts',(11.1802119228055,12.2,0.555695424655167));
#194381=CARTESIAN_POINT('Ctrl Pts',(11.1832797449187,12.2,0.557156172576721));
#194382=CARTESIAN_POINT('Ctrl Pts',(11.1863475664746,12.2,0.558616920232907));
#194383=CARTESIAN_POINT('Ctrl Pts',(11.1894202623362,12.2,0.560084444347706));
#194384=CARTESIAN_POINT('Ctrl Pts',(11.1924977846704,12.2,0.561558755076913));
#194385=CARTESIAN_POINT('Ctrl Pts',(11.1955753070045,12.2,0.563033065806121));
#194386=CARTESIAN_POINT('Ctrl Pts',(11.1986576579149,12.2,0.564514162982363));
#194387=CARTESIAN_POINT('Ctrl Pts',(11.2017447905532,12.2,0.566002057137232));
#194388=CARTESIAN_POINT('Ctrl Pts',(11.2058609672172,12.2,0.567985915920289));
#194389=CARTESIAN_POINT('Ctrl Pts',(11.2099856463879,12.2,0.569981857509243));
#194390=CARTESIAN_POINT('Ctrl Pts',(11.2141187215492,12.2,0.571989907454961));
#194391=CARTESIAN_POINT('Ctrl Pts',(11.217218528624,12.2,0.573495945256245));
#194392=CARTESIAN_POINT('Ctrl Pts',(11.2203230576252,12.2,0.575008791642777));
#194393=CARTESIAN_POINT('Ctrl Pts',(11.2234322652027,12.2,0.576528459531231));
#194394=CARTESIAN_POINT('Ctrl Pts',(11.2265414722154,12.2,0.578048127143612));
#194395=CARTESIAN_POINT('Ctrl Pts',(11.2296553571436,12.2,0.579574615508317));
#194396=CARTESIAN_POINT('Ctrl Pts',(11.2327738758533,12.2,0.581107932780002));
#194397=CARTESIAN_POINT('Ctrl Pts',(11.235892394563,12.2,0.582641250051688));
#194398=CARTESIAN_POINT('Ctrl Pts',(11.2390155465875,12.2,0.584181398040953));
#194399=CARTESIAN_POINT('Ctrl Pts',(11.2421432880992,12.2,0.585728385152007));
#194400=CARTESIAN_POINT('Ctrl Pts',(11.245271029611,12.2,0.587275372263061));
#194401=CARTESIAN_POINT('Ctrl Pts',(11.2484033592639,12.2,0.588829198389968));
#194402=CARTESIAN_POINT('Ctrl Pts',(11.2515402357332,12.2,0.590389873499935));
#194403=CARTESIAN_POINT('Ctrl Pts',(11.2546771122026,12.2,0.591950548609903));
#194404=CARTESIAN_POINT('Ctrl Pts',(11.2578185339551,12.2,0.593518072486248));
#194405=CARTESIAN_POINT('Ctrl Pts',(11.2609644574654,12.2,0.595092455053444));
#194406=CARTESIAN_POINT('Ctrl Pts',(11.2641103809757,12.2,0.59666683762064));
#194407=CARTESIAN_POINT('Ctrl Pts',(11.2672608046304,12.2,0.598248077771908));
#194408=CARTESIAN_POINT('Ctrl Pts',(11.2704156878396,12.2,0.599836185417745));
#194409=CARTESIAN_POINT('Ctrl Pts',(11.2735705710487,12.2,0.601424293063581));
#194410=CARTESIAN_POINT('Ctrl Pts',(11.2767299122758,12.2,0.603019267276549));
#194411=CARTESIAN_POINT('Ctrl Pts',(11.2798936682852,12.2,0.604621117884072));
#194412=CARTESIAN_POINT('Ctrl Pts',(11.2830574248694,12.2,0.606222968782597));
#194413=CARTESIAN_POINT('Ctrl Pts',(11.2862255958965,12.2,0.607831696166409));
#194414=CARTESIAN_POINT('Ctrl Pts',(11.2893981389832,12.2,0.609447308068814));
#194415=CARTESIAN_POINT('Ctrl Pts',(11.2936281954715,12.2,0.611601456782849));
#194416=CARTESIAN_POINT('Ctrl Pts',(11.2978660221283,12.2,0.613767846150855));
#194417=CARTESIAN_POINT('Ctrl Pts',(11.3021115206696,12.2,0.615946494305279));
#194418=CARTESIAN_POINT('Ctrl Pts',(11.3052956447202,12.2,0.617580480495307));
#194419=CARTESIAN_POINT('Ctrl Pts',(11.3084840831705,12.2,0.619221363751534));
#194420=CARTESIAN_POINT('Ctrl Pts',(11.3116767933039,12.2,0.62086915139906));
#194421=CARTESIAN_POINT('Ctrl Pts',(11.3148695040173,12.2,0.622516939345933));
#194422=CARTESIAN_POINT('Ctrl Pts',(11.3180664866986,12.2,0.624171632686409));
#194423=CARTESIAN_POINT('Ctrl Pts',(11.3212676989145,12.2,0.625833238595508));
#194424=CARTESIAN_POINT('Ctrl Pts',(11.3244689105487,12.2,0.627494844202749));
#194425=CARTESIAN_POINT('Ctrl Pts',(11.3276743522767,12.2,0.629163362400529));
#194426=CARTESIAN_POINT('Ctrl Pts',(11.3308839806126,12.2,0.63083880204916));
#194427=CARTESIAN_POINT('Ctrl Pts',(11.3340936089485,12.2,0.632514241697791));
#194428=CARTESIAN_POINT('Ctrl Pts',(11.337307424884,12.2,0.634196602661628));
#194429=CARTESIAN_POINT('Ctrl Pts',(11.3405253855591,12.2,0.635885892725853));
#194430=CARTESIAN_POINT('Ctrl Pts',(11.3437433462342,12.2,0.637575182790078));
#194431=CARTESIAN_POINT('Ctrl Pts',(11.3469654531671,12.2,0.639271401945137));
#194432=CARTESIAN_POINT('Ctrl Pts',(11.3501916627582,12.2,0.640974558008262));
#194433=CARTESIAN_POINT('Ctrl Pts',(11.3534178723494,12.2,0.642677714071387));
#194434=CARTESIAN_POINT('Ctrl Pts',(11.3566481849153,12.2,0.644387806525886));
#194435=CARTESIAN_POINT('Ctrl Pts',(11.3598825604224,12.2,0.646104844087896));
#194436=CARTESIAN_POINT('Ctrl Pts',(11.3631169359296,12.2,0.647821881649906));
#194437=CARTESIAN_POINT('Ctrl Pts',(11.3663553722123,12.2,0.649545863958999));
#194438=CARTESIAN_POINT('Ctrl Pts',(11.369597830381,12.2,0.651276798190114));
#194439=CARTESIAN_POINT('Ctrl Pts',(11.3728402885497,12.2,0.653007732421228));
#194440=CARTESIAN_POINT('Ctrl Pts',(11.3760867656766,12.2,0.654745619467243));
#194441=CARTESIAN_POINT('Ctrl Pts',(11.3793372227663,12.2,0.65649046561123));
#194442=CARTESIAN_POINT('Ctrl Pts',(11.3825876804465,12.2,0.658235312072197));
#194443=CARTESIAN_POINT('Ctrl Pts',(11.3858421171195,12.2,0.659987118460131));
#194444=CARTESIAN_POINT('Ctrl Pts',(11.3891004914269,12.2,0.661745891841688));
#194445=CARTESIAN_POINT('Ctrl Pts',(11.3934449895169,12.2,0.664090922484581));
#194446=CARTESIAN_POINT('Ctrl Pts',(11.3977964905477,12.2,0.666448337592532));
#194447=CARTESIAN_POINT('Ctrl Pts',(11.4021548971354,12.2,0.668818155564653));
#194448=CARTESIAN_POINT('Ctrl Pts',(11.4054237022246,12.2,0.670595519124467));
#194449=CARTESIAN_POINT('Ctrl Pts',(11.4086963915885,12.2,0.672379859213161));
#194450=CARTESIAN_POINT('Ctrl Pts',(11.411972922841,12.2,0.674171182861762));
#194451=CARTESIAN_POINT('Ctrl Pts',(11.4152494540936,12.2,0.675962506510362));
#194452=CARTESIAN_POINT('Ctrl Pts',(11.4185298269205,12.2,0.67776081332294));
#194453=CARTESIAN_POINT('Ctrl Pts',(11.4218140015923,12.2,0.679566110839722));
#194454=CARTESIAN_POINT('Ctrl Pts',(11.4261929015525,12.2,0.681973174414073));
#194455=CARTESIAN_POINT('Ctrl Pts',(11.4305785617466,12.2,0.684392664350729));
#194456=CARTESIAN_POINT('Ctrl Pts',(11.4349708937083,12.2,0.686824596483265));
#194457=CARTESIAN_POINT('Ctrl Pts',(11.4382651423802,12.2,0.688648545416993));
#194458=CARTESIAN_POINT('Ctrl Pts',(11.4415631447104,12.2,0.690479491583783));
#194459=CARTESIAN_POINT('Ctrl Pts',(11.4448648556318,12.2,0.692317444099715));
#194460=CARTESIAN_POINT('Ctrl Pts',(11.4481665665531,12.2,0.694155396615647));
#194461=CARTESIAN_POINT('Ctrl Pts',(11.4514719840484,12.2,0.696000354800609));
#194462=CARTESIAN_POINT('Ctrl Pts',(11.4547810613847,12.2,0.697852327408367));
#194463=CARTESIAN_POINT('Ctrl Pts',(11.4580901387211,12.2,0.699704300016125));
#194464=CARTESIAN_POINT('Ctrl Pts',(11.4614028748479,12.2,0.701563286711908));
#194465=CARTESIAN_POINT('Ctrl Pts',(11.4647192420186,12.2,0.703429290643153));
#194466=CARTESIAN_POINT('Ctrl Pts',(11.4691410653145,12.2,0.705917296110806));
#194467=CARTESIAN_POINT('Ctrl Pts',(11.4735693507915,12.2,0.7084177809819));
#194468=CARTESIAN_POINT('Ctrl Pts',(11.4780040719999,12.2,0.710930734999983));
#194469=CARTESIAN_POINT('Origin',(-5.66257110645729E-14,15.2,-1.77635683940025E-14));
#194470=CARTESIAN_POINT('',(10.2237731090076,15.2,1.76496130733463));
#194471=CARTESIAN_POINT('',(10.2237731090076,12.2,1.76496130733463));
#194472=CARTESIAN_POINT('',(10.2237731089999,15.2,1.76496130699999));
#194473=CARTESIAN_POINT('Origin',(-5.66257110645729E-14,12.2,-1.77635683940025E-14));
#194474=CARTESIAN_POINT('Origin',(-5.66257110645729E-14,15.2,-1.77635683940025E-14));
#194475=CARTESIAN_POINT('Origin',(-5.66257110645729E-14,15.2,-1.77635683940025E-14));
#194476=CARTESIAN_POINT('',(11.2599985479999,15.2,2.33718477899998));
#194477=CARTESIAN_POINT('',(11.1757778679999,15.2,2.71145515299998));
#194478=CARTESIAN_POINT('Origin',(-5.66257110645729E-14,15.2,-1.77635683940025E-14));
#194479=CARTESIAN_POINT('',(11.1757778679999,12.2,2.71145515299998));
#194480=CARTESIAN_POINT('',(11.1757778679999,15.2,2.71145515299998));
#194481=CARTESIAN_POINT('',(11.2599985479999,12.2,2.33718477899998));
#194482=CARTESIAN_POINT('Origin',(-5.66257110645729E-14,12.2,-1.77635683940025E-14));
#194483=CARTESIAN_POINT('',(11.2599985479999,15.2,2.33718477899998));
#194484=CARTESIAN_POINT('Ctrl Pts',(10.2237731089999,15.2,1.76496130799999));
#194485=CARTESIAN_POINT('Ctrl Pts',(10.2237731089999,11.6,1.76496130799999));
#194486=CARTESIAN_POINT('Ctrl Pts',(10.2239417409999,15.2,1.76500562399998));
#194487=CARTESIAN_POINT('Ctrl Pts',(10.2239417409999,11.6,1.76500562399998));
#194488=CARTESIAN_POINT('Ctrl Pts',(10.2242848729999,15.2,1.76509588899998));
#194489=CARTESIAN_POINT('Ctrl Pts',(10.2242848729999,11.6,1.76509588899998));
#194490=CARTESIAN_POINT('Ctrl Pts',(10.2248047309999,15.2,1.76523291899999));
#194491=CARTESIAN_POINT('Ctrl Pts',(10.2248047309999,11.6,1.76523291899999));
#194492=CARTESIAN_POINT('Ctrl Pts',(10.2255048889999,15.2,1.76541803299999));
#194493=CARTESIAN_POINT('Ctrl Pts',(10.2255048889999,11.6,1.76541803299999));
#194494=CARTESIAN_POINT('Ctrl Pts',(10.2263902529999,15.2,1.76565305799999));
#194495=CARTESIAN_POINT('Ctrl Pts',(10.2263902529999,11.6,1.76565305799999));
#194496=CARTESIAN_POINT('Ctrl Pts',(10.2272897259999,15.2,1.76589279499999));
#194497=CARTESIAN_POINT('Ctrl Pts',(10.2272897259999,11.6,1.76589279499999));
#194498=CARTESIAN_POINT('Ctrl Pts',(10.2281981499999,15.2,1.76613589499999));
#194499=CARTESIAN_POINT('Ctrl Pts',(10.2281981499999,11.6,1.76613589499999));
#194500=CARTESIAN_POINT('Ctrl Pts',(10.2291154919999,15.2,1.76638236599999));
#194501=CARTESIAN_POINT('Ctrl Pts',(10.2291154919999,11.6,1.76638236599999));
#194502=CARTESIAN_POINT('Ctrl Pts',(10.2300417219999,15.2,1.76663221999998));
#194503=CARTESIAN_POINT('Ctrl Pts',(10.2300417219999,11.6,1.76663221999998));
#194504=CARTESIAN_POINT('Ctrl Pts',(10.2309768119999,15.2,1.76688546699999));
#194505=CARTESIAN_POINT('Ctrl Pts',(10.2309768119999,11.6,1.76688546699999));
#194506=CARTESIAN_POINT('Ctrl Pts',(10.2319207289999,15.2,1.76714211799998));
#194507=CARTESIAN_POINT('Ctrl Pts',(10.2319207289999,11.6,1.76714211799998));
#194508=CARTESIAN_POINT('Ctrl Pts',(10.2328734439999,15.2,1.76740218199999));
#194509=CARTESIAN_POINT('Ctrl Pts',(10.2328734439999,11.6,1.76740218199999));
#194510=CARTESIAN_POINT('Ctrl Pts',(10.2338349259999,15.2,1.76766566999999));
#194511=CARTESIAN_POINT('Ctrl Pts',(10.2338349259999,11.6,1.76766566999999));
#194512=CARTESIAN_POINT('Ctrl Pts',(10.2348051459999,15.2,1.76793259399998));
#194513=CARTESIAN_POINT('Ctrl Pts',(10.2348051459999,11.6,1.76793259399998));
#194514=CARTESIAN_POINT('Ctrl Pts',(10.2357840739999,15.2,1.76820296099998));
#194515=CARTESIAN_POINT('Ctrl Pts',(10.2357840739999,11.6,1.76820296099998));
#194516=CARTESIAN_POINT('Ctrl Pts',(10.2367716789999,15.2,1.76847678099998));
#194517=CARTESIAN_POINT('Ctrl Pts',(10.2367716789999,11.6,1.76847678099998));
#194518=CARTESIAN_POINT('Ctrl Pts',(10.2377679339999,15.2,1.76875406799998));
#194519=CARTESIAN_POINT('Ctrl Pts',(10.2377679339999,11.6,1.76875406799998));
#194520=CARTESIAN_POINT('Ctrl Pts',(10.2387728089999,15.2,1.76903482699998));
#194521=CARTESIAN_POINT('Ctrl Pts',(10.2387728089999,11.6,1.76903482699998));
#194522=CARTESIAN_POINT('Ctrl Pts',(10.2397862729999,15.2,1.76931907099998));
#194523=CARTESIAN_POINT('Ctrl Pts',(10.2397862729999,11.6,1.76931907099998));
#194524=CARTESIAN_POINT('Ctrl Pts',(10.2408082999999,15.2,1.76960680999999));
#194525=CARTESIAN_POINT('Ctrl Pts',(10.2408082999999,11.6,1.76960680999999));
#194526=CARTESIAN_POINT('Ctrl Pts',(10.2418388579999,15.2,1.76989805099999));
#194527=CARTESIAN_POINT('Ctrl Pts',(10.2418388579999,11.6,1.76989805099998));
#194528=CARTESIAN_POINT('Ctrl Pts',(10.2428779189999,15.2,1.77019280699998));
#194529=CARTESIAN_POINT('Ctrl Pts',(10.2428779189999,11.6,1.77019280699998));
#194530=CARTESIAN_POINT('Ctrl Pts',(10.2439254559999,15.2,1.77049108599999));
#194531=CARTESIAN_POINT('Ctrl Pts',(10.2439254559999,11.6,1.77049108599999));
#194532=CARTESIAN_POINT('Ctrl Pts',(10.2449814379999,15.2,1.77079289599999));
#194533=CARTESIAN_POINT('Ctrl Pts',(10.2449814379999,11.6,1.77079289599999));
#194534=CARTESIAN_POINT('Ctrl Pts',(10.2460458399999,15.2,1.77109824999999));
#194535=CARTESIAN_POINT('Ctrl Pts',(10.2460458399999,11.6,1.77109824999999));
#194536=CARTESIAN_POINT('Ctrl Pts',(10.2471186289999,15.2,1.77140715399998));
#194537=CARTESIAN_POINT('Ctrl Pts',(10.2471186289999,11.6,1.77140715399998));
#194538=CARTESIAN_POINT('Ctrl Pts',(10.2481997809999,15.2,1.77171961899999));
#194539=CARTESIAN_POINT('Ctrl Pts',(10.2481997809999,11.6,1.77171961899999));
#194540=CARTESIAN_POINT('Ctrl Pts',(10.2492892659999,15.2,1.77203565399998));
#194541=CARTESIAN_POINT('Ctrl Pts',(10.2492892659999,11.6,1.77203565399998));
#194542=CARTESIAN_POINT('Ctrl Pts',(10.2503870569999,15.2,1.77235526999999));
#194543=CARTESIAN_POINT('Ctrl Pts',(10.2503870569999,11.6,1.77235526999999));
#194544=CARTESIAN_POINT('Ctrl Pts',(10.2514931249999,15.2,1.77267847299999));
#194545=CARTESIAN_POINT('Ctrl Pts',(10.2514931249999,11.6,1.77267847299999));
#194546=CARTESIAN_POINT('Ctrl Pts',(10.2526074429999,15.2,1.77300527499999));
#194547=CARTESIAN_POINT('Ctrl Pts',(10.2526074429999,11.6,1.77300527499999));
#194548=CARTESIAN_POINT('Ctrl Pts',(10.2537299839999,15.2,1.77333568399999));
#194549=CARTESIAN_POINT('Ctrl Pts',(10.2537299839999,11.6,1.77333568399999));
#194550=CARTESIAN_POINT('Ctrl Pts',(10.2548607199999,15.2,1.77366970799998));
#194551=CARTESIAN_POINT('Ctrl Pts',(10.2548607199999,11.6,1.77366970799998));
#194552=CARTESIAN_POINT('Ctrl Pts',(10.2559996249999,15.2,1.77400735799999));
#194553=CARTESIAN_POINT('Ctrl Pts',(10.2559996249999,11.6,1.77400735799999));
#194554=CARTESIAN_POINT('Ctrl Pts',(10.2571466689999,15.2,1.77434864199999));
#194555=CARTESIAN_POINT('Ctrl Pts',(10.2571466689999,11.6,1.77434864199998));
#194556=CARTESIAN_POINT('Ctrl Pts',(10.2583018279999,15.2,1.77469356899998));
#194557=CARTESIAN_POINT('Ctrl Pts',(10.2583018279999,11.6,1.77469356899998));
#194558=CARTESIAN_POINT('Ctrl Pts',(10.2594650729999,15.2,1.77504214699999));
#194559=CARTESIAN_POINT('Ctrl Pts',(10.2594650729999,11.6,1.77504214699999));
#194560=CARTESIAN_POINT('Ctrl Pts',(10.2606363769999,15.2,1.77539438599998));
#194561=CARTESIAN_POINT('Ctrl Pts',(10.2606363769999,11.6,1.77539438599998));
#194562=CARTESIAN_POINT('Ctrl Pts',(10.2618157169999,15.2,1.77575029399998));
#194563=CARTESIAN_POINT('Ctrl Pts',(10.2618157169999,11.6,1.77575029399998));
#194564=CARTESIAN_POINT('Ctrl Pts',(10.2630030619999,15.2,1.77610988099998));
#194565=CARTESIAN_POINT('Ctrl Pts',(10.2630030619999,11.6,1.77610988099998));
#194566=CARTESIAN_POINT('Ctrl Pts',(10.2641983869999,15.2,1.77647315299998));
#194567=CARTESIAN_POINT('Ctrl Pts',(10.2641983869999,11.6,1.77647315299998));
#194568=CARTESIAN_POINT('Ctrl Pts',(10.2654016659999,15.2,1.77684012099999));
#194569=CARTESIAN_POINT('Ctrl Pts',(10.2654016659999,11.6,1.77684012099998));
#194570=CARTESIAN_POINT('Ctrl Pts',(10.2666128729999,15.2,1.77721079199999));
#194571=CARTESIAN_POINT('Ctrl Pts',(10.2666128729999,11.6,1.77721079199999));
#194572=CARTESIAN_POINT('Ctrl Pts',(10.2678319819999,15.2,1.77758517599999));
#194573=CARTESIAN_POINT('Ctrl Pts',(10.2678319819999,11.6,1.77758517599999));
#194574=CARTESIAN_POINT('Ctrl Pts',(10.2690589659999,15.2,1.77796327999999));
#194575=CARTESIAN_POINT('Ctrl Pts',(10.2690589659999,11.6,1.77796327999999));
#194576=CARTESIAN_POINT('Ctrl Pts',(10.2702937999999,15.2,1.77834511299999));
#194577=CARTESIAN_POINT('Ctrl Pts',(10.2702937999999,11.6,1.77834511299999));
#194578=CARTESIAN_POINT('Ctrl Pts',(10.2715364579999,15.2,1.77873068299998));
#194579=CARTESIAN_POINT('Ctrl Pts',(10.2715364579999,11.6,1.77873068299998));
#194580=CARTESIAN_POINT('Ctrl Pts',(10.2727869139999,15.2,1.77911999899999));
#194581=CARTESIAN_POINT('Ctrl Pts',(10.2727869139999,11.6,1.77911999899999));
#194582=CARTESIAN_POINT('Ctrl Pts',(10.2740451429999,15.2,1.77951306799998));
#194583=CARTESIAN_POINT('Ctrl Pts',(10.2740451429999,11.6,1.77951306799998));
#194584=CARTESIAN_POINT('Ctrl Pts',(10.2753111179999,15.2,1.77990989899998));
#194585=CARTESIAN_POINT('Ctrl Pts',(10.2753111179999,11.6,1.77990989899998));
#194586=CARTESIAN_POINT('Ctrl Pts',(10.2765848159999,15.2,1.78031050099999));
#194587=CARTESIAN_POINT('Ctrl Pts',(10.2765848159999,11.6,1.78031050099999));
#194588=CARTESIAN_POINT('Ctrl Pts',(10.2778662099999,15.2,1.78071487999999));
#194589=CARTESIAN_POINT('Ctrl Pts',(10.2778662099999,11.6,1.78071487999999));
#194590=CARTESIAN_POINT('Ctrl Pts',(10.2791552759999,15.2,1.78112304599999));
#194591=CARTESIAN_POINT('Ctrl Pts',(10.2791552759999,11.6,1.78112304599999));
#194592=CARTESIAN_POINT('Ctrl Pts',(10.2804519869999,15.2,1.78153500599999));
#194593=CARTESIAN_POINT('Ctrl Pts',(10.2804519869999,11.6,1.78153500599999));
#194594=CARTESIAN_POINT('Ctrl Pts',(10.2817563209999,15.2,1.78195076799998));
#194595=CARTESIAN_POINT('Ctrl Pts',(10.2817563209999,11.6,1.78195076799998));
#194596=CARTESIAN_POINT('Ctrl Pts',(10.2830682509999,15.2,1.78237033999999));
#194597=CARTESIAN_POINT('Ctrl Pts',(10.2830682509999,11.6,1.78237033999999));
#194598=CARTESIAN_POINT('Ctrl Pts',(10.2843877529999,15.2,1.78279372899999));
#194599=CARTESIAN_POINT('Ctrl Pts',(10.2843877529999,11.6,1.78279372899999));
#194600=CARTESIAN_POINT('Ctrl Pts',(10.2857148029999,15.2,1.78322094399999));
#194601=CARTESIAN_POINT('Ctrl Pts',(10.2857148029999,11.6,1.78322094399999));
#194602=CARTESIAN_POINT('Ctrl Pts',(10.2870493749999,15.2,1.78365199299999));
#194603=CARTESIAN_POINT('Ctrl Pts',(10.2870493749999,11.6,1.78365199299999));
#194604=CARTESIAN_POINT('Ctrl Pts',(10.2883914449999,15.2,1.78408688299998));
#194605=CARTESIAN_POINT('Ctrl Pts',(10.2883914449999,11.6,1.78408688299998));
#194606=CARTESIAN_POINT('Ctrl Pts',(10.2897409889999,15.2,1.78452562099999));
#194607=CARTESIAN_POINT('Ctrl Pts',(10.2897409889999,11.6,1.78452562099999));
#194608=CARTESIAN_POINT('Ctrl Pts',(10.2910979839999,15.2,1.78496821599999));
#194609=CARTESIAN_POINT('Ctrl Pts',(10.2910979839999,11.6,1.78496821599999));
#194610=CARTESIAN_POINT('Ctrl Pts',(10.2924624019999,15.2,1.78541467399999));
#194611=CARTESIAN_POINT('Ctrl Pts',(10.2924624019999,11.6,1.78541467399999));
#194612=CARTESIAN_POINT('Ctrl Pts',(10.2938342229999,15.2,1.78586500399998));
#194613=CARTESIAN_POINT('Ctrl Pts',(10.2938342229999,11.6,1.78586500399998));
#194614=CARTESIAN_POINT('Ctrl Pts',(10.2952134229999,15.2,1.78631921299999));
#194615=CARTESIAN_POINT('Ctrl Pts',(10.2952134229999,11.6,1.78631921299999));
#194616=CARTESIAN_POINT('Ctrl Pts',(10.2965999749999,15.2,1.78677730799999));
#194617=CARTESIAN_POINT('Ctrl Pts',(10.2965999749999,11.6,1.78677730799999));
#194618=CARTESIAN_POINT('Ctrl Pts',(10.2979938569999,15.2,1.78723929699999));
#194619=CARTESIAN_POINT('Ctrl Pts',(10.2979938569999,11.6,1.78723929699998));
#194620=CARTESIAN_POINT('Ctrl Pts',(10.2993950459999,15.2,1.78770518799999));
#194621=CARTESIAN_POINT('Ctrl Pts',(10.2993950459999,11.6,1.78770518799999));
#194622=CARTESIAN_POINT('Ctrl Pts',(10.3008035169999,15.2,1.78817498699999));
#194623=CARTESIAN_POINT('Ctrl Pts',(10.3008035169999,11.6,1.78817498699999));
#194624=CARTESIAN_POINT('Ctrl Pts',(10.3022192479999,15.2,1.78864870099999));
#194625=CARTESIAN_POINT('Ctrl Pts',(10.3022192479999,11.6,1.78864870099999));
#194626=CARTESIAN_POINT('Ctrl Pts',(10.3036422139999,15.2,1.78912633799999));
#194627=CARTESIAN_POINT('Ctrl Pts',(10.3036422139999,11.6,1.78912633799999));
#194628=CARTESIAN_POINT('Ctrl Pts',(10.3050723929999,15.2,1.78960790499998));
#194629=CARTESIAN_POINT('Ctrl Pts',(10.3050723929999,11.6,1.78960790499998));
#194630=CARTESIAN_POINT('Ctrl Pts',(10.3065097609999,15.2,1.79009340899999));
#194631=CARTESIAN_POINT('Ctrl Pts',(10.3065097609999,11.6,1.79009340899999));
#194632=CARTESIAN_POINT('Ctrl Pts',(10.3079542959999,15.2,1.79058285899998));
#194633=CARTESIAN_POINT('Ctrl Pts',(10.3079542959999,11.6,1.79058285899998));
#194634=CARTESIAN_POINT('Ctrl Pts',(10.3094059739999,15.2,1.79107625799999));
#194635=CARTESIAN_POINT('Ctrl Pts',(10.3094059739999,11.6,1.79107625799999));
#194636=CARTESIAN_POINT('Ctrl Pts',(10.3108647719999,15.2,1.79157361699998));
#194637=CARTESIAN_POINT('Ctrl Pts',(10.3108647719999,11.6,1.79157361699998));
#194638=CARTESIAN_POINT('Ctrl Pts',(10.3123306679999,15.2,1.79207494199999));
#194639=CARTESIAN_POINT('Ctrl Pts',(10.3123306679999,11.6,1.79207494199999));
#194640=CARTESIAN_POINT('Ctrl Pts',(10.3138036379999,15.2,1.79258023699999));
#194641=CARTESIAN_POINT('Ctrl Pts',(10.3138036379999,11.6,1.79258023699999));
#194642=CARTESIAN_POINT('Ctrl Pts',(10.3152836599999,15.2,1.79308951299999));
#194643=CARTESIAN_POINT('Ctrl Pts',(10.3152836599999,11.6,1.79308951299999));
#194644=CARTESIAN_POINT('Ctrl Pts',(10.3167707109999,15.2,1.79360277499998));
#194645=CARTESIAN_POINT('Ctrl Pts',(10.3167707109999,11.6,1.79360277499998));
#194646=CARTESIAN_POINT('Ctrl Pts',(10.3182647709999,15.2,1.79412002899999));
#194647=CARTESIAN_POINT('Ctrl Pts',(10.3182647709999,11.6,1.79412002899999));
#194648=CARTESIAN_POINT('Ctrl Pts',(10.3197658129999,15.2,1.79464128299998));
#194649=CARTESIAN_POINT('Ctrl Pts',(10.3197658129999,11.6,1.79464128299998));
#194650=CARTESIAN_POINT('Ctrl Pts',(10.3212738189999,15.2,1.79516654399999));
#194651=CARTESIAN_POINT('Ctrl Pts',(10.3212738189999,11.6,1.79516654399999));
#194652=CARTESIAN_POINT('Ctrl Pts',(10.3227887639999,15.2,1.79569581799999));
#194653=CARTESIAN_POINT('Ctrl Pts',(10.3227887639999,11.6,1.79569581799999));
#194654=CARTESIAN_POINT('Ctrl Pts',(10.3243106259999,15.2,1.79622911099999));
#194655=CARTESIAN_POINT('Ctrl Pts',(10.3243106259999,11.6,1.79622911099999));
#194656=CARTESIAN_POINT('Ctrl Pts',(10.3258393839999,15.2,1.79676642999999));
#194657=CARTESIAN_POINT('Ctrl Pts',(10.3258393839999,11.6,1.79676642999999));
#194658=CARTESIAN_POINT('Ctrl Pts',(10.3273750169999,15.2,1.79730778399998));
#194659=CARTESIAN_POINT('Ctrl Pts',(10.3273750169999,11.6,1.79730778399998));
#194660=CARTESIAN_POINT('Ctrl Pts',(10.3289175009999,15.2,1.79785317599999));
#194661=CARTESIAN_POINT('Ctrl Pts',(10.3289175009999,11.6,1.79785317599999));
#194662=CARTESIAN_POINT('Ctrl Pts',(10.3304668139999,15.2,1.79840261399999));
#194663=CARTESIAN_POINT('Ctrl Pts',(10.3304668139999,11.6,1.79840261399998));
#194664=CARTESIAN_POINT('Ctrl Pts',(10.3320229349999,15.2,1.79895610499999));
#194665=CARTESIAN_POINT('Ctrl Pts',(10.3320229349999,11.6,1.79895610499999));
#194666=CARTESIAN_POINT('Ctrl Pts',(10.3335858439999,15.2,1.79951365499999));
#194667=CARTESIAN_POINT('Ctrl Pts',(10.3335858439999,11.6,1.79951365499999));
#194668=CARTESIAN_POINT('Ctrl Pts',(10.3351555169999,15.2,1.80007527099999));
#194669=CARTESIAN_POINT('Ctrl Pts',(10.3351555169999,11.6,1.80007527099999));
#194670=CARTESIAN_POINT('Ctrl Pts',(10.3367319329999,15.2,1.80064095699999));
#194671=CARTESIAN_POINT('Ctrl Pts',(10.3367319329999,11.6,1.80064095699999));
#194672=CARTESIAN_POINT('Ctrl Pts',(10.3383150709999,15.2,1.80121072199999));
#194673=CARTESIAN_POINT('Ctrl Pts',(10.3383150709999,11.6,1.80121072199999));
#194674=CARTESIAN_POINT('Ctrl Pts',(10.3399049089999,15.2,1.80178457099998));
#194675=CARTESIAN_POINT('Ctrl Pts',(10.3399049089999,11.6,1.80178457099998));
#194676=CARTESIAN_POINT('Ctrl Pts',(10.3415014269999,15.2,1.80236251099998));
#194677=CARTESIAN_POINT('Ctrl Pts',(10.3415014269999,11.6,1.80236251099998));
#194678=CARTESIAN_POINT('Ctrl Pts',(10.3431046029999,15.2,1.80294454799999));
#194679=CARTESIAN_POINT('Ctrl Pts',(10.3431046029999,11.6,1.80294454799998));
#194680=CARTESIAN_POINT('Ctrl Pts',(10.3447144149999,15.2,1.80353068699999));
#194681=CARTESIAN_POINT('Ctrl Pts',(10.3447144149999,11.6,1.80353068699999));
#194682=CARTESIAN_POINT('Ctrl Pts',(10.3463308429999,15.2,1.80412093599998));
#194683=CARTESIAN_POINT('Ctrl Pts',(10.3463308429999,11.6,1.80412093599998));
#194684=CARTESIAN_POINT('Ctrl Pts',(10.3479538659999,15.2,1.80471529999998));
#194685=CARTESIAN_POINT('Ctrl Pts',(10.3479538659999,11.6,1.80471529999998));
#194686=CARTESIAN_POINT('Ctrl Pts',(10.3495834629999,15.2,1.80531378499999));
#194687=CARTESIAN_POINT('Ctrl Pts',(10.3495834629999,11.6,1.80531378499999));
#194688=CARTESIAN_POINT('Ctrl Pts',(10.3512196119999,15.2,1.80591639799998));
#194689=CARTESIAN_POINT('Ctrl Pts',(10.3512196119999,11.6,1.80591639799998));
#194690=CARTESIAN_POINT('Ctrl Pts',(10.3528622949999,15.2,1.80652314399998));
#194691=CARTESIAN_POINT('Ctrl Pts',(10.3528622949999,11.6,1.80652314399998));
#194692=CARTESIAN_POINT('Ctrl Pts',(10.3545114879999,15.2,1.80713402899999));
#194693=CARTESIAN_POINT('Ctrl Pts',(10.3545114879999,11.6,1.80713402899999));
#194694=CARTESIAN_POINT('Ctrl Pts',(10.3561671729999,15.2,1.80774905899999));
#194695=CARTESIAN_POINT('Ctrl Pts',(10.3561671729999,11.6,1.80774905899999));
#194696=CARTESIAN_POINT('Ctrl Pts',(10.3578293269999,15.2,1.80836824099998));
#194697=CARTESIAN_POINT('Ctrl Pts',(10.3578293269999,11.6,1.80836824099998));
#194698=CARTESIAN_POINT('Ctrl Pts',(10.3594979319999,15.2,1.80899157899999));
#194699=CARTESIAN_POINT('Ctrl Pts',(10.3594979319999,11.6,1.80899157899999));
#194700=CARTESIAN_POINT('Ctrl Pts',(10.3611729669999,15.2,1.80961908099999));
#194701=CARTESIAN_POINT('Ctrl Pts',(10.3611729669999,11.6,1.80961908099999));
#194702=CARTESIAN_POINT('Ctrl Pts',(10.3628544089999,15.2,1.81025075099999));
#194703=CARTESIAN_POINT('Ctrl Pts',(10.3628544089999,11.6,1.81025075099999));
#194704=CARTESIAN_POINT('Ctrl Pts',(10.3645422419999,15.2,1.81088659599999));
#194705=CARTESIAN_POINT('Ctrl Pts',(10.3645422419999,11.6,1.81088659599998));
#194706=CARTESIAN_POINT('Ctrl Pts',(10.3662364429999,15.2,1.81152661999999));
#194707=CARTESIAN_POINT('Ctrl Pts',(10.3662364429999,11.6,1.81152661999999));
#194708=CARTESIAN_POINT('Ctrl Pts',(10.3679369919999,15.2,1.81217083099999));
#194709=CARTESIAN_POINT('Ctrl Pts',(10.3679369919999,11.6,1.81217083099999));
#194710=CARTESIAN_POINT('Ctrl Pts',(10.3696438709999,15.2,1.81281923299998));
#194711=CARTESIAN_POINT('Ctrl Pts',(10.3696438709999,11.6,1.81281923299998));
#194712=CARTESIAN_POINT('Ctrl Pts',(10.3713570579999,15.2,1.81347183299998));
#194713=CARTESIAN_POINT('Ctrl Pts',(10.3713570579999,11.6,1.81347183299998));
#194714=CARTESIAN_POINT('Ctrl Pts',(10.3730765319999,15.2,1.81412863499999));
#194715=CARTESIAN_POINT('Ctrl Pts',(10.3730765319999,11.6,1.81412863499998));
#194716=CARTESIAN_POINT('Ctrl Pts',(10.3748022759999,15.2,1.81478964499998));
#194717=CARTESIAN_POINT('Ctrl Pts',(10.3748022759999,11.6,1.81478964499998));
#194718=CARTESIAN_POINT('Ctrl Pts',(10.3765342689999,15.2,1.81545486999998));
#194719=CARTESIAN_POINT('Ctrl Pts',(10.3765342689999,11.6,1.81545486999998));
#194720=CARTESIAN_POINT('Ctrl Pts',(10.3782724909999,15.2,1.81612431399999));
#194721=CARTESIAN_POINT('Ctrl Pts',(10.3782724909999,11.6,1.81612431399999));
#194722=CARTESIAN_POINT('Ctrl Pts',(10.3800169229999,15.2,1.81679798299998));
#194723=CARTESIAN_POINT('Ctrl Pts',(10.3800169229999,11.6,1.81679798299998));
#194724=CARTESIAN_POINT('Ctrl Pts',(10.3817675449999,15.2,1.81747588299999));
#194725=CARTESIAN_POINT('Ctrl Pts',(10.3817675449999,11.6,1.81747588299999));
#194726=CARTESIAN_POINT('Ctrl Pts',(10.3835243379999,15.2,1.81815801799999));
#194727=CARTESIAN_POINT('Ctrl Pts',(10.3835243379999,11.6,1.81815801799999));
#194728=CARTESIAN_POINT('Ctrl Pts',(10.3852872809999,15.2,1.81884439299999));
#194729=CARTESIAN_POINT('Ctrl Pts',(10.3852872809999,11.6,1.81884439299999));
#194730=CARTESIAN_POINT('Ctrl Pts',(10.3870563549999,15.2,1.81953501599999));
#194731=CARTESIAN_POINT('Ctrl Pts',(10.3870563549999,11.6,1.81953501599999));
#194732=CARTESIAN_POINT('Ctrl Pts',(10.3888315429999,15.2,1.82022989099998));
#194733=CARTESIAN_POINT('Ctrl Pts',(10.3888315429999,11.6,1.82022989099998));
#194734=CARTESIAN_POINT('Ctrl Pts',(10.3906128229999,15.2,1.82092902299999));
#194735=CARTESIAN_POINT('Ctrl Pts',(10.3906128229999,11.6,1.82092902299999));
#194736=CARTESIAN_POINT('Ctrl Pts',(10.3924001779999,15.2,1.82163241699998));
#194737=CARTESIAN_POINT('Ctrl Pts',(10.3924001779999,11.6,1.82163241699998));
#194738=CARTESIAN_POINT('Ctrl Pts',(10.3941935869999,15.2,1.82234007799998));
#194739=CARTESIAN_POINT('Ctrl Pts',(10.3941935869999,11.6,1.82234007799998));
#194740=CARTESIAN_POINT('Ctrl Pts',(10.3959930309999,15.2,1.82305201299998));
#194741=CARTESIAN_POINT('Ctrl Pts',(10.3959930309999,11.6,1.82305201299998));
#194742=CARTESIAN_POINT('Ctrl Pts',(10.3977984929999,15.2,1.82376822499998));
#194743=CARTESIAN_POINT('Ctrl Pts',(10.3977984929999,11.6,1.82376822499998));
#194744=CARTESIAN_POINT('Ctrl Pts',(10.3996099509999,15.2,1.82448872199998));
#194745=CARTESIAN_POINT('Ctrl Pts',(10.3996099509999,11.6,1.82448872199998));
#194746=CARTESIAN_POINT('Ctrl Pts',(10.4014273889999,15.2,1.82521350599998));
#194747=CARTESIAN_POINT('Ctrl Pts',(10.4014273889999,11.6,1.82521350599998));
#194748=CARTESIAN_POINT('Ctrl Pts',(10.4032507859999,15.2,1.82594258299998));
#194749=CARTESIAN_POINT('Ctrl Pts',(10.4032507859999,11.6,1.82594258299998));
#194750=CARTESIAN_POINT('Ctrl Pts',(10.4050801249999,15.2,1.82667595899999));
#194751=CARTESIAN_POINT('Ctrl Pts',(10.4050801249999,11.6,1.82667595899999));
#194752=CARTESIAN_POINT('Ctrl Pts',(10.4069153869999,15.2,1.82741363799999));
#194753=CARTESIAN_POINT('Ctrl Pts',(10.4069153869999,11.6,1.82741363799999));
#194754=CARTESIAN_POINT('Ctrl Pts',(10.4087565519999,15.2,1.82815562599998));
#194755=CARTESIAN_POINT('Ctrl Pts',(10.4087565519999,11.6,1.82815562599998));
#194756=CARTESIAN_POINT('Ctrl Pts',(10.4106036029999,15.2,1.82890192799999));
#194757=CARTESIAN_POINT('Ctrl Pts',(10.4106036029999,11.6,1.82890192799999));
#194758=CARTESIAN_POINT('Ctrl Pts',(10.4124565199999,15.2,1.82965254699999));
#194759=CARTESIAN_POINT('Ctrl Pts',(10.4124565199999,11.6,1.82965254699999));
#194760=CARTESIAN_POINT('Ctrl Pts',(10.4143152849999,15.2,1.83040748999999));
#194761=CARTESIAN_POINT('Ctrl Pts',(10.4143152849999,11.6,1.83040748999999));
#194762=CARTESIAN_POINT('Ctrl Pts',(10.4161798809999,15.2,1.83116676099999));
#194763=CARTESIAN_POINT('Ctrl Pts',(10.4161798809999,11.6,1.83116676099999));
#194764=CARTESIAN_POINT('Ctrl Pts',(10.4180502869999,15.2,1.83193036499999));
#194765=CARTESIAN_POINT('Ctrl Pts',(10.4180502869999,11.6,1.83193036499999));
#194766=CARTESIAN_POINT('Ctrl Pts',(10.4199264869999,15.2,1.83269830799999));
#194767=CARTESIAN_POINT('Ctrl Pts',(10.4199264869999,11.6,1.83269830799999));
#194768=CARTESIAN_POINT('Ctrl Pts',(10.4218084619999,15.2,1.83347059299999));
#194769=CARTESIAN_POINT('Ctrl Pts',(10.4218084619999,11.6,1.83347059299999));
#194770=CARTESIAN_POINT('Ctrl Pts',(10.4236961939999,15.2,1.83424722499999));
#194771=CARTESIAN_POINT('Ctrl Pts',(10.4236961939999,11.6,1.83424722499998));
#194772=CARTESIAN_POINT('Ctrl Pts',(10.4255896649999,15.2,1.83502820899998));
#194773=CARTESIAN_POINT('Ctrl Pts',(10.4255896649999,11.6,1.83502820899998));
#194774=CARTESIAN_POINT('Ctrl Pts',(10.4274888559999,15.2,1.83581354999999));
#194775=CARTESIAN_POINT('Ctrl Pts',(10.4274888559999,11.6,1.83581354999998));
#194776=CARTESIAN_POINT('Ctrl Pts',(10.4293937499999,15.2,1.83660325299998));
#194777=CARTESIAN_POINT('Ctrl Pts',(10.4293937499999,11.6,1.83660325299998));
#194778=CARTESIAN_POINT('Ctrl Pts',(10.4313043289999,15.2,1.83739732299999));
#194779=CARTESIAN_POINT('Ctrl Pts',(10.4313043289999,11.6,1.83739732299998));
#194780=CARTESIAN_POINT('Ctrl Pts',(10.4332205739999,15.2,1.83819576399999));
#194781=CARTESIAN_POINT('Ctrl Pts',(10.4332205739999,11.6,1.83819576399999));
#194782=CARTESIAN_POINT('Ctrl Pts',(10.4351424679999,15.2,1.83899857999998));
#194783=CARTESIAN_POINT('Ctrl Pts',(10.4351424679999,11.6,1.83899857999998));
#194784=CARTESIAN_POINT('Ctrl Pts',(10.4370699929999,15.2,1.83980577599999));
#194785=CARTESIAN_POINT('Ctrl Pts',(10.4370699929999,11.6,1.83980577599998));
#194786=CARTESIAN_POINT('Ctrl Pts',(10.4390031319999,15.2,1.84061735699999));
#194787=CARTESIAN_POINT('Ctrl Pts',(10.4390031319999,11.6,1.84061735699998));
#194788=CARTESIAN_POINT('Ctrl Pts',(10.4409418659999,15.2,1.84143332699998));
#194789=CARTESIAN_POINT('Ctrl Pts',(10.4409418659999,11.6,1.84143332699998));
#194790=CARTESIAN_POINT('Ctrl Pts',(10.4428861799999,15.2,1.84225368999998));
#194791=CARTESIAN_POINT('Ctrl Pts',(10.4428861799999,11.6,1.84225368999998));
#194792=CARTESIAN_POINT('Ctrl Pts',(10.4448360519999,15.2,1.84307845199998));
#194793=CARTESIAN_POINT('Ctrl Pts',(10.4448360519999,11.6,1.84307845199998));
#194794=CARTESIAN_POINT('Ctrl Pts',(10.4467914679999,15.2,1.84390761799999));
#194795=CARTESIAN_POINT('Ctrl Pts',(10.4467914679999,11.6,1.84390761799999));
#194796=CARTESIAN_POINT('Ctrl Pts',(10.4487524099999,15.2,1.84474118999999));
#194797=CARTESIAN_POINT('Ctrl Pts',(10.4487524099999,11.6,1.84474118999999));
#194798=CARTESIAN_POINT('Ctrl Pts',(10.4507188599999,15.2,1.84557917299998));
#194799=CARTESIAN_POINT('Ctrl Pts',(10.4507188599999,11.6,1.84557917299998));
#194800=CARTESIAN_POINT('Ctrl Pts',(10.4526908009999,15.2,1.84642157199999));
#194801=CARTESIAN_POINT('Ctrl Pts',(10.4526908009999,11.6,1.84642157199999));
#194802=CARTESIAN_POINT('Ctrl Pts',(10.4546682149999,15.2,1.84726839199998));
#194803=CARTESIAN_POINT('Ctrl Pts',(10.4546682149999,11.6,1.84726839199998));
#194804=CARTESIAN_POINT('Ctrl Pts',(10.4566510849999,15.2,1.84811963699998));
#194805=CARTESIAN_POINT('Ctrl Pts',(10.4566510849999,11.6,1.84811963699998));
#194806=CARTESIAN_POINT('Ctrl Pts',(10.4586393939999,15.2,1.84897530999999));
#194807=CARTESIAN_POINT('Ctrl Pts',(10.4586393939999,11.6,1.84897530999998));
#194808=CARTESIAN_POINT('Ctrl Pts',(10.4606331249999,15.2,1.84983541599999));
#194809=CARTESIAN_POINT('Ctrl Pts',(10.4606331249999,11.6,1.84983541599998));
#194810=CARTESIAN_POINT('Ctrl Pts',(10.4626322619999,15.2,1.85069995999998));
#194811=CARTESIAN_POINT('Ctrl Pts',(10.4626322619999,11.6,1.85069995999998));
#194812=CARTESIAN_POINT('Ctrl Pts',(10.4646367859999,15.2,1.85156894599999));
#194813=CARTESIAN_POINT('Ctrl Pts',(10.4646367859999,11.6,1.85156894599999));
#194814=CARTESIAN_POINT('Ctrl Pts',(10.4666466809999,15.2,1.85244237799999));
#194815=CARTESIAN_POINT('Ctrl Pts',(10.4666466809999,11.6,1.85244237799999));
#194816=CARTESIAN_POINT('Ctrl Pts',(10.4686619289999,15.2,1.85332025999998));
#194817=CARTESIAN_POINT('Ctrl Pts',(10.4686619289999,11.6,1.85332025999998));
#194818=CARTESIAN_POINT('Ctrl Pts',(10.4706825139999,15.2,1.85420259599999));
#194819=CARTESIAN_POINT('Ctrl Pts',(10.4706825139999,11.6,1.85420259599998));
#194820=CARTESIAN_POINT('Ctrl Pts',(10.4727084189999,15.2,1.85508938999998));
#194821=CARTESIAN_POINT('Ctrl Pts',(10.4727084189999,11.6,1.85508938999998));
#194822=CARTESIAN_POINT('Ctrl Pts',(10.4747396279999,15.2,1.85598064699999));
#194823=CARTESIAN_POINT('Ctrl Pts',(10.4747396279999,11.6,1.85598064699999));
#194824=CARTESIAN_POINT('Ctrl Pts',(10.4767761229999,15.2,1.85687637099999));
#194825=CARTESIAN_POINT('Ctrl Pts',(10.4767761229999,11.6,1.85687637099999));
#194826=CARTESIAN_POINT('Ctrl Pts',(10.4788178879999,15.2,1.85777656499999));
#194827=CARTESIAN_POINT('Ctrl Pts',(10.4788178879999,11.6,1.85777656499999));
#194828=CARTESIAN_POINT('Ctrl Pts',(10.4808649049999,15.2,1.85868123499999));
#194829=CARTESIAN_POINT('Ctrl Pts',(10.4808649049999,11.6,1.85868123499999));
#194830=CARTESIAN_POINT('Ctrl Pts',(10.4829171589999,15.2,1.85959038199998));
#194831=CARTESIAN_POINT('Ctrl Pts',(10.4829171589999,11.6,1.85959038199998));
#194832=CARTESIAN_POINT('Ctrl Pts',(10.4849746339999,15.2,1.86050401299998));
#194833=CARTESIAN_POINT('Ctrl Pts',(10.4849746339999,11.6,1.86050401299998));
#194834=CARTESIAN_POINT('Ctrl Pts',(10.4870373119999,15.2,1.86142212899998));
#194835=CARTESIAN_POINT('Ctrl Pts',(10.4870373119999,11.6,1.86142212899998));
#194836=CARTESIAN_POINT('Ctrl Pts',(10.4891051769999,15.2,1.86234473799999));
#194837=CARTESIAN_POINT('Ctrl Pts',(10.4891051769999,11.6,1.86234473799999));
#194838=CARTESIAN_POINT('Ctrl Pts',(10.4911782119999,15.2,1.86327183999999));
#194839=CARTESIAN_POINT('Ctrl Pts',(10.4911782119999,11.6,1.86327183999999));
#194840=CARTESIAN_POINT('Ctrl Pts',(10.4932564019999,15.2,1.86420344099998));
#194841=CARTESIAN_POINT('Ctrl Pts',(10.4932564019999,11.6,1.86420344099998));
#194842=CARTESIAN_POINT('Ctrl Pts',(10.4953397299999,15.2,1.86513954399999));
#194843=CARTESIAN_POINT('Ctrl Pts',(10.4953397299999,11.6,1.86513954399999));
#194844=CARTESIAN_POINT('Ctrl Pts',(10.4974281779999,15.2,1.86608015299999));
#194845=CARTESIAN_POINT('Ctrl Pts',(10.4974281779999,11.6,1.86608015299999));
#194846=CARTESIAN_POINT('Ctrl Pts',(10.4995217329999,15.2,1.86702527299999));
#194847=CARTESIAN_POINT('Ctrl Pts',(10.4995217329999,11.6,1.86702527299999));
#194848=CARTESIAN_POINT('Ctrl Pts',(10.5016203769999,15.2,1.86797490599998));
#194849=CARTESIAN_POINT('Ctrl Pts',(10.5016203769999,11.6,1.86797490599998));
#194850=CARTESIAN_POINT('Ctrl Pts',(10.5037240939999,15.2,1.86892905699999));
#194851=CARTESIAN_POINT('Ctrl Pts',(10.5037240939999,11.6,1.86892905699999));
#194852=CARTESIAN_POINT('Ctrl Pts',(10.5058328669999,15.2,1.86988772999999));
#194853=CARTESIAN_POINT('Ctrl Pts',(10.5058328669999,11.6,1.86988772999999));
#194854=CARTESIAN_POINT('Ctrl Pts',(10.5079466819999,15.2,1.87085092699999));
#194855=CARTESIAN_POINT('Ctrl Pts',(10.5079466819999,11.6,1.87085092699998));
#194856=CARTESIAN_POINT('Ctrl Pts',(10.5100655219999,15.2,1.87181865399999));
#194857=CARTESIAN_POINT('Ctrl Pts',(10.5100655219999,11.6,1.87181865399999));
#194858=CARTESIAN_POINT('Ctrl Pts',(10.5121893699999,15.2,1.87279091299999));
#194859=CARTESIAN_POINT('Ctrl Pts',(10.5121893699999,11.6,1.87279091299999));
#194860=CARTESIAN_POINT('Ctrl Pts',(10.5143182119999,15.2,1.87376770899998));
#194861=CARTESIAN_POINT('Ctrl Pts',(10.5143182119999,11.6,1.87376770899998));
#194862=CARTESIAN_POINT('Ctrl Pts',(10.5164520309999,15.2,1.87474904399998));
#194863=CARTESIAN_POINT('Ctrl Pts',(10.5164520309999,11.6,1.87474904399998));
#194864=CARTESIAN_POINT('Ctrl Pts',(10.5185908099999,15.2,1.87573492299999));
#194865=CARTESIAN_POINT('Ctrl Pts',(10.5185908099999,11.6,1.87573492299998));
#194866=CARTESIAN_POINT('Ctrl Pts',(10.5207345359999,15.2,1.87672534899999));
#194867=CARTESIAN_POINT('Ctrl Pts',(10.5207345359999,11.6,1.87672534899999));
#194868=CARTESIAN_POINT('Ctrl Pts',(10.5228831919999,15.2,1.87772032599999));
#194869=CARTESIAN_POINT('Ctrl Pts',(10.5228831919999,11.6,1.87772032599998));
#194870=CARTESIAN_POINT('Ctrl Pts',(10.5250367609999,15.2,1.87871985699998));
#194871=CARTESIAN_POINT('Ctrl Pts',(10.5250367609999,11.6,1.87871985699998));
#194872=CARTESIAN_POINT('Ctrl Pts',(10.5271952289999,15.2,1.87972394599999));
#194873=CARTESIAN_POINT('Ctrl Pts',(10.5271952289999,11.6,1.87972394599999));
#194874=CARTESIAN_POINT('Ctrl Pts',(10.5293585799999,15.2,1.88073259699999));
#194875=CARTESIAN_POINT('Ctrl Pts',(10.5293585799999,11.6,1.88073259699999));
#194876=CARTESIAN_POINT('Ctrl Pts',(10.5315267989999,15.2,1.88174581299998));
#194877=CARTESIAN_POINT('Ctrl Pts',(10.5315267989999,11.6,1.88174581299998));
#194878=CARTESIAN_POINT('Ctrl Pts',(10.5336998689999,15.2,1.88276359699998));
#194879=CARTESIAN_POINT('Ctrl Pts',(10.5336998689999,11.6,1.88276359699998));
#194880=CARTESIAN_POINT('Ctrl Pts',(10.5358777749999,15.2,1.88378595299998));
#194881=CARTESIAN_POINT('Ctrl Pts',(10.5358777749999,11.6,1.88378595299998));
#194882=CARTESIAN_POINT('Ctrl Pts',(10.5380605019999,15.2,1.88481288399998));
#194883=CARTESIAN_POINT('Ctrl Pts',(10.5380605019999,11.6,1.88481288399998));
#194884=CARTESIAN_POINT('Ctrl Pts',(10.5402480349999,15.2,1.88584439399999));
#194885=CARTESIAN_POINT('Ctrl Pts',(10.5402480349999,11.6,1.88584439399999));
#194886=CARTESIAN_POINT('Ctrl Pts',(10.5424403579999,15.2,1.88688048699999));
#194887=CARTESIAN_POINT('Ctrl Pts',(10.5424403579999,11.6,1.88688048699999));
#194888=CARTESIAN_POINT('Ctrl Pts',(10.5446374549999,15.2,1.88792116499998));
#194889=CARTESIAN_POINT('Ctrl Pts',(10.5446374549999,11.6,1.88792116499998));
#194890=CARTESIAN_POINT('Ctrl Pts',(10.5468393119999,15.2,1.88896643199998));
#194891=CARTESIAN_POINT('Ctrl Pts',(10.5468393119999,11.6,1.88896643199998));
#194892=CARTESIAN_POINT('Ctrl Pts',(10.5490459129999,15.2,1.89001629099999));
#194893=CARTESIAN_POINT('Ctrl Pts',(10.5490459129999,11.6,1.89001629099998));
#194894=CARTESIAN_POINT('Ctrl Pts',(10.5512572439999,15.2,1.89107074599999));
#194895=CARTESIAN_POINT('Ctrl Pts',(10.5512572439999,11.6,1.89107074599998));
#194896=CARTESIAN_POINT('Ctrl Pts',(10.5534732879999,15.2,1.89212979899999));
#194897=CARTESIAN_POINT('Ctrl Pts',(10.5534732879999,11.6,1.89212979899999));
#194898=CARTESIAN_POINT('Ctrl Pts',(10.5556940319999,15.2,1.89319345599999));
#194899=CARTESIAN_POINT('Ctrl Pts',(10.5556940319999,11.6,1.89319345599999));
#194900=CARTESIAN_POINT('Ctrl Pts',(10.5579194589999,15.2,1.89426171699999));
#194901=CARTESIAN_POINT('Ctrl Pts',(10.5579194589999,11.6,1.89426171699999));
#194902=CARTESIAN_POINT('Ctrl Pts',(10.5601495539999,15.2,1.89533458699998));
#194903=CARTESIAN_POINT('Ctrl Pts',(10.5601495539999,11.6,1.89533458699998));
#194904=CARTESIAN_POINT('Ctrl Pts',(10.5623843029999,15.2,1.89641206899998));
#194905=CARTESIAN_POINT('Ctrl Pts',(10.5623843029999,11.6,1.89641206899998));
#194906=CARTESIAN_POINT('Ctrl Pts',(10.5646236909999,15.2,1.89749416699998));
#194907=CARTESIAN_POINT('Ctrl Pts',(10.5646236909999,11.6,1.89749416699998));
#194908=CARTESIAN_POINT('Ctrl Pts',(10.5668677029999,15.2,1.89858088199998));
#194909=CARTESIAN_POINT('Ctrl Pts',(10.5668677029999,11.6,1.89858088199998));
#194910=CARTESIAN_POINT('Ctrl Pts',(10.5691163239999,15.2,1.89967221899999));
#194911=CARTESIAN_POINT('Ctrl Pts',(10.5691163239999,11.6,1.89967221899999));
#194912=CARTESIAN_POINT('Ctrl Pts',(10.5713695389999,15.2,1.90076818199998));
#194913=CARTESIAN_POINT('Ctrl Pts',(10.5713695389999,11.6,1.90076818199998));
#194914=CARTESIAN_POINT('Ctrl Pts',(10.5736273329999,15.2,1.90186877199999));
#194915=CARTESIAN_POINT('Ctrl Pts',(10.5736273329999,11.6,1.90186877199999));
#194916=CARTESIAN_POINT('Ctrl Pts',(10.5758896919999,15.2,1.90297399199999));
#194917=CARTESIAN_POINT('Ctrl Pts',(10.5758896919999,11.6,1.90297399199999));
#194918=CARTESIAN_POINT('Ctrl Pts',(10.5781565999999,15.2,1.90408384699999));
#194919=CARTESIAN_POINT('Ctrl Pts',(10.5781565999999,11.6,1.90408384699999));
#194920=CARTESIAN_POINT('Ctrl Pts',(10.5804280449999,15.2,1.90519833799998));
#194921=CARTESIAN_POINT('Ctrl Pts',(10.5804280449999,11.6,1.90519833799998));
#194922=CARTESIAN_POINT('Ctrl Pts',(10.5827040089999,15.2,1.90631746999999));
#194923=CARTESIAN_POINT('Ctrl Pts',(10.5827040089999,11.6,1.90631746999998));
#194924=CARTESIAN_POINT('Ctrl Pts',(10.5849844789999,15.2,1.90744124499998));
#194925=CARTESIAN_POINT('Ctrl Pts',(10.5849844789999,11.6,1.90744124499998));
#194926=CARTESIAN_POINT('Ctrl Pts',(10.5872694409999,15.2,1.90856966699998));
#194927=CARTESIAN_POINT('Ctrl Pts',(10.5872694409999,11.6,1.90856966699998));
#194928=CARTESIAN_POINT('Ctrl Pts',(10.5895588789999,15.2,1.90970273699998));
#194929=CARTESIAN_POINT('Ctrl Pts',(10.5895588789999,11.6,1.90970273699998));
#194930=CARTESIAN_POINT('Ctrl Pts',(10.5918527799999,15.2,1.91084046099999));
#194931=CARTESIAN_POINT('Ctrl Pts',(10.5918527799999,11.6,1.91084046099998));
#194932=CARTESIAN_POINT('Ctrl Pts',(10.5941511279999,15.2,1.91198283799999));
#194933=CARTESIAN_POINT('Ctrl Pts',(10.5941511279999,11.6,1.91198283799999));
#194934=CARTESIAN_POINT('Ctrl Pts',(10.5964539099999,15.2,1.91312987399999));
#194935=CARTESIAN_POINT('Ctrl Pts',(10.5964539099999,11.6,1.91312987399999));
#194936=CARTESIAN_POINT('Ctrl Pts',(10.5987611109999,15.2,1.91428157099998));
#194937=CARTESIAN_POINT('Ctrl Pts',(10.5987611109999,11.6,1.91428157099998));
#194938=CARTESIAN_POINT('Ctrl Pts',(10.6010727169999,15.2,1.91543793199999));
#194939=CARTESIAN_POINT('Ctrl Pts',(10.6010727169999,11.6,1.91543793199999));
#194940=CARTESIAN_POINT('Ctrl Pts',(10.6033887129999,15.2,1.91659895999999));
#194941=CARTESIAN_POINT('Ctrl Pts',(10.6033887129999,11.6,1.91659895999999));
#194942=CARTESIAN_POINT('Ctrl Pts',(10.6057090859999,15.2,1.91776465699999));
#194943=CARTESIAN_POINT('Ctrl Pts',(10.6057090859999,11.6,1.91776465699998));
#194944=CARTESIAN_POINT('Ctrl Pts',(10.6080338189999,15.2,1.91893502699998));
#194945=CARTESIAN_POINT('Ctrl Pts',(10.6080338189999,11.6,1.91893502699998));
#194946=CARTESIAN_POINT('Ctrl Pts',(10.6103629009999,15.2,1.92011007299998));
#194947=CARTESIAN_POINT('Ctrl Pts',(10.6103629009999,11.6,1.92011007299998));
#194948=CARTESIAN_POINT('Ctrl Pts',(10.6126963159999,15.2,1.92128979699998));
#194949=CARTESIAN_POINT('Ctrl Pts',(10.6126963159999,11.6,1.92128979699998));
#194950=CARTESIAN_POINT('Ctrl Pts',(10.6150340509999,15.2,1.92247420199998));
#194951=CARTESIAN_POINT('Ctrl Pts',(10.6150340509999,11.6,1.92247420199998));
#194952=CARTESIAN_POINT('Ctrl Pts',(10.6173760899999,15.2,1.92366328999999));
#194953=CARTESIAN_POINT('Ctrl Pts',(10.6173760899999,11.6,1.92366328999999));
#194954=CARTESIAN_POINT('Ctrl Pts',(10.6197224209999,15.2,1.92485706499999));
#194955=CARTESIAN_POINT('Ctrl Pts',(10.6197224209999,11.6,1.92485706499998));
#194956=CARTESIAN_POINT('Ctrl Pts',(10.6220730289999,15.2,1.92605552899999));
#194957=CARTESIAN_POINT('Ctrl Pts',(10.6220730289999,11.6,1.92605552899999));
#194958=CARTESIAN_POINT('Ctrl Pts',(10.6244279009999,15.2,1.92725868499998));
#194959=CARTESIAN_POINT('Ctrl Pts',(10.6244279009999,11.6,1.92725868499998));
#194960=CARTESIAN_POINT('Ctrl Pts',(10.6267870199999,15.2,1.92846653699998));
#194961=CARTESIAN_POINT('Ctrl Pts',(10.6267870199999,11.6,1.92846653699998));
#194962=CARTESIAN_POINT('Ctrl Pts',(10.6291503759999,15.2,1.92967908499998));
#194963=CARTESIAN_POINT('Ctrl Pts',(10.6291503759999,11.6,1.92967908499998));
#194964=CARTESIAN_POINT('Ctrl Pts',(10.6315179529999,15.2,1.93089633399998));
#194965=CARTESIAN_POINT('Ctrl Pts',(10.6315179529999,11.6,1.93089633399998));
#194966=CARTESIAN_POINT('Ctrl Pts',(10.6338897369999,15.2,1.93211828599999));
#194967=CARTESIAN_POINT('Ctrl Pts',(10.6338897369999,11.6,1.93211828599999));
#194968=CARTESIAN_POINT('Ctrl Pts',(10.6362657159999,15.2,1.93334494299998));
#194969=CARTESIAN_POINT('Ctrl Pts',(10.6362657159999,11.6,1.93334494299998));
#194970=CARTESIAN_POINT('Ctrl Pts',(10.6386458729999,15.2,1.93457630799998));
#194971=CARTESIAN_POINT('Ctrl Pts',(10.6386458729999,11.6,1.93457630799998));
#194972=CARTESIAN_POINT('Ctrl Pts',(10.6410301979999,15.2,1.93581238299998));
#194973=CARTESIAN_POINT('Ctrl Pts',(10.6410301979999,11.6,1.93581238299998));
#194974=CARTESIAN_POINT('Ctrl Pts',(10.6434186729999,15.2,1.93705317299999));
#194975=CARTESIAN_POINT('Ctrl Pts',(10.6434186729999,11.6,1.93705317299999));
#194976=CARTESIAN_POINT('Ctrl Pts',(10.6458112889999,15.2,1.93829867799999));
#194977=CARTESIAN_POINT('Ctrl Pts',(10.6458112889999,11.6,1.93829867799999));
#194978=CARTESIAN_POINT('Ctrl Pts',(10.6482080289999,15.2,1.93954890099999));
#194979=CARTESIAN_POINT('Ctrl Pts',(10.6482080289999,11.6,1.93954890099999));
#194980=CARTESIAN_POINT('Ctrl Pts',(10.6506088799999,15.2,1.94080384499999));
#194981=CARTESIAN_POINT('Ctrl Pts',(10.6506088799999,11.6,1.94080384499998));
#194982=CARTESIAN_POINT('Ctrl Pts',(10.6530138299999,15.2,1.94206351299998));
#194983=CARTESIAN_POINT('Ctrl Pts',(10.6530138299999,11.6,1.94206351299998));
#194984=CARTESIAN_POINT('Ctrl Pts',(10.6554228629999,15.2,1.94332790599999));
#194985=CARTESIAN_POINT('Ctrl Pts',(10.6554228629999,11.6,1.94332790599998));
#194986=CARTESIAN_POINT('Ctrl Pts',(10.6578359679999,15.2,1.94459702899998));
#194987=CARTESIAN_POINT('Ctrl Pts',(10.6578359679999,11.6,1.94459702899998));
#194988=CARTESIAN_POINT('Ctrl Pts',(10.6602531299999,15.2,1.94587088299999));
#194989=CARTESIAN_POINT('Ctrl Pts',(10.6602531299999,11.6,1.94587088299999));
#194990=CARTESIAN_POINT('Ctrl Pts',(10.6626743349999,15.2,1.94714946999999));
#194991=CARTESIAN_POINT('Ctrl Pts',(10.6626743349999,11.6,1.94714946999999));
#194992=CARTESIAN_POINT('Ctrl Pts',(10.6650995699999,15.2,1.94843279199999));
#194993=CARTESIAN_POINT('Ctrl Pts',(10.6650995699999,11.6,1.94843279199999));
#194994=CARTESIAN_POINT('Ctrl Pts',(10.6675288229999,15.2,1.94972085299999));
#194995=CARTESIAN_POINT('Ctrl Pts',(10.6675288229999,11.6,1.94972085299998));
#194996=CARTESIAN_POINT('Ctrl Pts',(10.6699620789999,15.2,1.95101365499998));
#194997=CARTESIAN_POINT('Ctrl Pts',(10.6699620789999,11.6,1.95101365499998));
#194998=CARTESIAN_POINT('Ctrl Pts',(10.6723993259999,15.2,1.95231119999999));
#194999=CARTESIAN_POINT('Ctrl Pts',(10.6723993259999,11.6,1.95231119999998));
#195000=CARTESIAN_POINT('Ctrl Pts',(10.6748405499999,15.2,1.95361349199999));
#195001=CARTESIAN_POINT('Ctrl Pts',(10.6748405499999,11.6,1.95361349199999));
#195002=CARTESIAN_POINT('Ctrl Pts',(10.6772857359999,15.2,1.95492052999999));
#195003=CARTESIAN_POINT('Ctrl Pts',(10.6772857359999,11.6,1.95492052999999));
#195004=CARTESIAN_POINT('Ctrl Pts',(10.6797348739999,15.2,1.95623231899999));
#195005=CARTESIAN_POINT('Ctrl Pts',(10.6797348739999,11.6,1.95623231899999));
#195006=CARTESIAN_POINT('Ctrl Pts',(10.6821879489999,15.2,1.95754885999999));
#195007=CARTESIAN_POINT('Ctrl Pts',(10.6821879489999,11.6,1.95754885999999));
#195008=CARTESIAN_POINT('Ctrl Pts',(10.6846449469999,15.2,1.95887015699999));
#195009=CARTESIAN_POINT('Ctrl Pts',(10.6846449469999,11.6,1.95887015699999));
#195010=CARTESIAN_POINT('Ctrl Pts',(10.6871058569999,15.2,1.96019620999999));
#195011=CARTESIAN_POINT('Ctrl Pts',(10.6871058569999,11.6,1.96019620999999));
#195012=CARTESIAN_POINT('Ctrl Pts',(10.6895706639999,15.2,1.96152702399999));
#195013=CARTESIAN_POINT('Ctrl Pts',(10.6895706639999,11.6,1.96152702399999));
#195014=CARTESIAN_POINT('Ctrl Pts',(10.6920393549999,15.2,1.96286259899999));
#195015=CARTESIAN_POINT('Ctrl Pts',(10.6920393549999,11.6,1.96286259899999));
#195016=CARTESIAN_POINT('Ctrl Pts',(10.6945119189999,15.2,1.96420293799999));
#195017=CARTESIAN_POINT('Ctrl Pts',(10.6945119189999,11.6,1.96420293799999));
#195018=CARTESIAN_POINT('Ctrl Pts',(10.6969883409999,15.2,1.96554804299998));
#195019=CARTESIAN_POINT('Ctrl Pts',(10.6969883409999,11.6,1.96554804299998));
#195020=CARTESIAN_POINT('Ctrl Pts',(10.6994686089999,15.2,1.96689791799999));
#195021=CARTESIAN_POINT('Ctrl Pts',(10.6994686089999,11.6,1.96689791799999));
#195022=CARTESIAN_POINT('Ctrl Pts',(10.7019527089999,15.2,1.96825256199999));
#195023=CARTESIAN_POINT('Ctrl Pts',(10.7019527089999,11.6,1.96825256199999));
#195024=CARTESIAN_POINT('Ctrl Pts',(10.7044406279999,15.2,1.96961197999999));
#195025=CARTESIAN_POINT('Ctrl Pts',(10.7044406279999,11.6,1.96961197999999));
#195026=CARTESIAN_POINT('Ctrl Pts',(10.7069323549999,15.2,1.97097617399999));
#195027=CARTESIAN_POINT('Ctrl Pts',(10.7069323549999,11.6,1.97097617399998));
#195028=CARTESIAN_POINT('Ctrl Pts',(10.7094278759999,15.2,1.97234514399999));
#195029=CARTESIAN_POINT('Ctrl Pts',(10.7094278759999,11.6,1.97234514399998));
#195030=CARTESIAN_POINT('Ctrl Pts',(10.7119271769999,15.2,1.97371889399999));
#195031=CARTESIAN_POINT('Ctrl Pts',(10.7119271769999,11.6,1.97371889399998));
#195032=CARTESIAN_POINT('Ctrl Pts',(10.7144302479999,15.2,1.97509742499999));
#195033=CARTESIAN_POINT('Ctrl Pts',(10.7144302479999,11.6,1.97509742499998));
#195034=CARTESIAN_POINT('Ctrl Pts',(10.7169370719999,15.2,1.97648073999999));
#195035=CARTESIAN_POINT('Ctrl Pts',(10.7169370719999,11.6,1.97648073999999));
#195036=CARTESIAN_POINT('Ctrl Pts',(10.7194476399999,15.2,1.97786884199999));
#195037=CARTESIAN_POINT('Ctrl Pts',(10.7194476399999,11.6,1.97786884199999));
#195038=CARTESIAN_POINT('Ctrl Pts',(10.7219619379999,15.2,1.97926173099999));
#195039=CARTESIAN_POINT('Ctrl Pts',(10.7219619379999,11.6,1.97926173099999));
#195040=CARTESIAN_POINT('Ctrl Pts',(10.7244799519999,15.2,1.98065940999999));
#195041=CARTESIAN_POINT('Ctrl Pts',(10.7244799519999,11.6,1.98065940999998));
#195042=CARTESIAN_POINT('Ctrl Pts',(10.7270016709999,15.2,1.98206188099999));
#195043=CARTESIAN_POINT('Ctrl Pts',(10.7270016709999,11.6,1.98206188099999));
#195044=CARTESIAN_POINT('Ctrl Pts',(10.7295270829999,15.2,1.98346914599998));
#195045=CARTESIAN_POINT('Ctrl Pts',(10.7295270829999,11.6,1.98346914599998));
#195046=CARTESIAN_POINT('Ctrl Pts',(10.7320561729999,15.2,1.98488120799999));
#195047=CARTESIAN_POINT('Ctrl Pts',(10.7320561729999,11.6,1.98488120799999));
#195048=CARTESIAN_POINT('Ctrl Pts',(10.7345889299999,15.2,1.98629806799998));
#195049=CARTESIAN_POINT('Ctrl Pts',(10.7345889299999,11.6,1.98629806799998));
#195050=CARTESIAN_POINT('Ctrl Pts',(10.7371253409999,15.2,1.98771972799999));
#195051=CARTESIAN_POINT('Ctrl Pts',(10.7371253409999,11.6,1.98771972799999));
#195052=CARTESIAN_POINT('Ctrl Pts',(10.7396653929999,15.2,1.98914618999999));
#195053=CARTESIAN_POINT('Ctrl Pts',(10.7396653929999,11.6,1.98914618999999));
#195054=CARTESIAN_POINT('Ctrl Pts',(10.7422090749999,15.2,1.99057745699998));
#195055=CARTESIAN_POINT('Ctrl Pts',(10.7422090749999,11.6,1.99057745699998));
#195056=CARTESIAN_POINT('Ctrl Pts',(10.7447563729999,15.2,1.99201352999999));
#195057=CARTESIAN_POINT('Ctrl Pts',(10.7447563729999,11.6,1.99201352999998));
#195058=CARTESIAN_POINT('Ctrl Pts',(10.7473072759999,15.2,1.99345441099998));
#195059=CARTESIAN_POINT('Ctrl Pts',(10.7473072759999,11.6,1.99345441099998));
#195060=CARTESIAN_POINT('Ctrl Pts',(10.7498617699999,15.2,1.99490010199999));
#195061=CARTESIAN_POINT('Ctrl Pts',(10.7498617699999,11.6,1.99490010199999));
#195062=CARTESIAN_POINT('Ctrl Pts',(10.7524198429999,15.2,1.99635060499999));
#195063=CARTESIAN_POINT('Ctrl Pts',(10.7524198429999,11.6,1.99635060499999));
#195064=CARTESIAN_POINT('Ctrl Pts',(10.7549814829999,15.2,1.99780592199998));
#195065=CARTESIAN_POINT('Ctrl Pts',(10.7549814829999,11.6,1.99780592199998));
#195066=CARTESIAN_POINT('Ctrl Pts',(10.7575466779999,15.2,1.99926605499999));
#195067=CARTESIAN_POINT('Ctrl Pts',(10.7575466779999,11.6,1.99926605499999));
#195068=CARTESIAN_POINT('Ctrl Pts',(10.7601154139999,15.2,2.00073100599999));
#195069=CARTESIAN_POINT('Ctrl Pts',(10.7601154139999,11.6,2.00073100599999));
#195070=CARTESIAN_POINT('Ctrl Pts',(10.7626876819999,15.2,2.00220077599999));
#195071=CARTESIAN_POINT('Ctrl Pts',(10.7626876819999,11.6,2.00220077599999));
#195072=CARTESIAN_POINT('Ctrl Pts',(10.7652634659999,15.2,2.00367536799999));
#195073=CARTESIAN_POINT('Ctrl Pts',(10.7652634659999,11.6,2.00367536799999));
#195074=CARTESIAN_POINT('Ctrl Pts',(10.7678427559999,15.2,2.00515478299998));
#195075=CARTESIAN_POINT('Ctrl Pts',(10.7678427559999,11.6,2.00515478299998));
#195076=CARTESIAN_POINT('Ctrl Pts',(10.7704255389999,15.2,2.00663902299999));
#195077=CARTESIAN_POINT('Ctrl Pts',(10.7704255389999,11.6,2.00663902299999));
#195078=CARTESIAN_POINT('Ctrl Pts',(10.7730118039999,15.2,2.00812809099999));
#195079=CARTESIAN_POINT('Ctrl Pts',(10.7730118039999,11.6,2.00812809099999));
#195080=CARTESIAN_POINT('Ctrl Pts',(10.7756015359999,15.2,2.00962198699999));
#195081=CARTESIAN_POINT('Ctrl Pts',(10.7756015359999,11.6,2.00962198699999));
#195082=CARTESIAN_POINT('Ctrl Pts',(10.7781947259999,15.2,2.01112071299999));
#195083=CARTESIAN_POINT('Ctrl Pts',(10.7781947259999,11.6,2.01112071299998));
#195084=CARTESIAN_POINT('Ctrl Pts',(10.7807913609999,15.2,2.01262427099998));
#195085=CARTESIAN_POINT('Ctrl Pts',(10.7807913609999,11.6,2.01262427099998));
#195086=CARTESIAN_POINT('Ctrl Pts',(10.7833914279999,15.2,2.01413266499999));
#195087=CARTESIAN_POINT('Ctrl Pts',(10.7833914279999,11.6,2.01413266499999));
#195088=CARTESIAN_POINT('Ctrl Pts',(10.7859949149999,15.2,2.01564589299998));
#195089=CARTESIAN_POINT('Ctrl Pts',(10.7859949149999,11.6,2.01564589299998));
#195090=CARTESIAN_POINT('Ctrl Pts',(10.7886018119999,15.2,2.01716395899998));
#195091=CARTESIAN_POINT('Ctrl Pts',(10.7886018119999,11.6,2.01716395899998));
#195092=CARTESIAN_POINT('Ctrl Pts',(10.7912121039999,15.2,2.01868686499999));
#195093=CARTESIAN_POINT('Ctrl Pts',(10.7912121039999,11.6,2.01868686499999));
#195094=CARTESIAN_POINT('Ctrl Pts',(10.7938257809999,15.2,2.02021461199998));
#195095=CARTESIAN_POINT('Ctrl Pts',(10.7938257809999,11.6,2.02021461199998));
#195096=CARTESIAN_POINT('Ctrl Pts',(10.7964428309999,15.2,2.02174720099999));
#195097=CARTESIAN_POINT('Ctrl Pts',(10.7964428309999,11.6,2.02174720099999));
#195098=CARTESIAN_POINT('Ctrl Pts',(10.7990632409999,15.2,2.02328463499999));
#195099=CARTESIAN_POINT('Ctrl Pts',(10.7990632409999,11.6,2.02328463499999));
#195100=CARTESIAN_POINT('Ctrl Pts',(10.8016870009999,15.2,2.02482691399998));
#195101=CARTESIAN_POINT('Ctrl Pts',(10.8016870009999,11.6,2.02482691399998));
#195102=CARTESIAN_POINT('Ctrl Pts',(10.8043140959999,15.2,2.02637404199999));
#195103=CARTESIAN_POINT('Ctrl Pts',(10.8043140959999,11.6,2.02637404199998));
#195104=CARTESIAN_POINT('Ctrl Pts',(10.8069445179999,15.2,2.02792601899999));
#195105=CARTESIAN_POINT('Ctrl Pts',(10.8069445179999,11.6,2.02792601899999));
#195106=CARTESIAN_POINT('Ctrl Pts',(10.8095782509999,15.2,2.02948284699998));
#195107=CARTESIAN_POINT('Ctrl Pts',(10.8095782509999,11.6,2.02948284699998));
#195108=CARTESIAN_POINT('Ctrl Pts',(10.8122152859999,15.2,2.03104452799999));
#195109=CARTESIAN_POINT('Ctrl Pts',(10.8122152859999,11.6,2.03104452799999));
#195110=CARTESIAN_POINT('Ctrl Pts',(10.8148556109999,15.2,2.03261106299998));
#195111=CARTESIAN_POINT('Ctrl Pts',(10.8148556109999,11.6,2.03261106299998));
#195112=CARTESIAN_POINT('Ctrl Pts',(10.8174992139999,15.2,2.03418245299999));
#195113=CARTESIAN_POINT('Ctrl Pts',(10.8174992139999,11.6,2.03418245299999));
#195114=CARTESIAN_POINT('Ctrl Pts',(10.8201460829999,15.2,2.03575870199999));
#195115=CARTESIAN_POINT('Ctrl Pts',(10.8201460829999,11.6,2.03575870199999));
#195116=CARTESIAN_POINT('Ctrl Pts',(10.8227962069999,15.2,2.03733980899999));
#195117=CARTESIAN_POINT('Ctrl Pts',(10.8227962069999,11.6,2.03733980899999));
#195118=CARTESIAN_POINT('Ctrl Pts',(10.8254495719999,15.2,2.03892577599999));
#195119=CARTESIAN_POINT('Ctrl Pts',(10.8254495719999,11.6,2.03892577599999));
#195120=CARTESIAN_POINT('Ctrl Pts',(10.8281061699999,15.2,2.04051660499998));
#195121=CARTESIAN_POINT('Ctrl Pts',(10.8281061699999,11.6,2.04051660499998));
#195122=CARTESIAN_POINT('Ctrl Pts',(10.8307659859999,15.2,2.04211229899999));
#195123=CARTESIAN_POINT('Ctrl Pts',(10.8307659859999,11.6,2.04211229899998));
#195124=CARTESIAN_POINT('Ctrl Pts',(10.8334290109999,15.2,2.04371285799999));
#195125=CARTESIAN_POINT('Ctrl Pts',(10.8334290109999,11.6,2.04371285799999));
#195126=CARTESIAN_POINT('Ctrl Pts',(10.8360952309999,15.2,2.04531828299999));
#195127=CARTESIAN_POINT('Ctrl Pts',(10.8360952309999,11.6,2.04531828299999));
#195128=CARTESIAN_POINT('Ctrl Pts',(10.8387646369999,15.2,2.04692857699999));
#195129=CARTESIAN_POINT('Ctrl Pts',(10.8387646369999,11.6,2.04692857699999));
#195130=CARTESIAN_POINT('Ctrl Pts',(10.8414372149999,15.2,2.04854373999999));
#195131=CARTESIAN_POINT('Ctrl Pts',(10.8414372149999,11.6,2.04854373999999));
#195132=CARTESIAN_POINT('Ctrl Pts',(10.8441129549999,15.2,2.05016377399998));
#195133=CARTESIAN_POINT('Ctrl Pts',(10.8441129549999,11.6,2.05016377399998));
#195134=CARTESIAN_POINT('Ctrl Pts',(10.8467918459999,15.2,2.05178867999999));
#195135=CARTESIAN_POINT('Ctrl Pts',(10.8467918459999,11.6,2.05178867999999));
#195136=CARTESIAN_POINT('Ctrl Pts',(10.8494738749999,15.2,2.05341846099998));
#195137=CARTESIAN_POINT('Ctrl Pts',(10.8494738749999,11.6,2.05341846099998));
#195138=CARTESIAN_POINT('Ctrl Pts',(10.8521590309999,15.2,2.05505311699998));
#195139=CARTESIAN_POINT('Ctrl Pts',(10.8521590309999,11.6,2.05505311699998));
#195140=CARTESIAN_POINT('Ctrl Pts',(10.8548473029999,15.2,2.05669265099999));
#195141=CARTESIAN_POINT('Ctrl Pts',(10.8548473029999,11.6,2.05669265099999));
#195142=CARTESIAN_POINT('Ctrl Pts',(10.8575386799999,15.2,2.05833706299998));
#195143=CARTESIAN_POINT('Ctrl Pts',(10.8575386799999,11.6,2.05833706299998));
#195144=CARTESIAN_POINT('Ctrl Pts',(10.8602331499999,15.2,2.05998635399999));
#195145=CARTESIAN_POINT('Ctrl Pts',(10.8602331499999,11.6,2.05998635399998));
#195146=CARTESIAN_POINT('Ctrl Pts',(10.8629307009999,15.2,2.06164052599998));
#195147=CARTESIAN_POINT('Ctrl Pts',(10.8629307009999,11.6,2.06164052599998));
#195148=CARTESIAN_POINT('Ctrl Pts',(10.8656313229999,15.2,2.06329958099999));
#195149=CARTESIAN_POINT('Ctrl Pts',(10.8656313229999,11.6,2.06329958099999));
#195150=CARTESIAN_POINT('Ctrl Pts',(10.8683350049999,15.2,2.06496351899998));
#195151=CARTESIAN_POINT('Ctrl Pts',(10.8683350049999,11.6,2.06496351899998));
#195152=CARTESIAN_POINT('Ctrl Pts',(10.8710417329999,15.2,2.06663234299999));
#195153=CARTESIAN_POINT('Ctrl Pts',(10.8710417329999,11.6,2.06663234299999));
#195154=CARTESIAN_POINT('Ctrl Pts',(10.8737514979999,15.2,2.06830605399999));
#195155=CARTESIAN_POINT('Ctrl Pts',(10.8737514979999,11.6,2.06830605399999));
#195156=CARTESIAN_POINT('Ctrl Pts',(10.8764642889999,15.2,2.06998465199999));
#195157=CARTESIAN_POINT('Ctrl Pts',(10.8764642889999,11.6,2.06998465199998));
#195158=CARTESIAN_POINT('Ctrl Pts',(10.8791800939999,15.2,2.07166813999998));
#195159=CARTESIAN_POINT('Ctrl Pts',(10.8791800939999,11.6,2.07166813999998));
#195160=CARTESIAN_POINT('Ctrl Pts',(10.8818989019999,15.2,2.07335651799998));
#195161=CARTESIAN_POINT('Ctrl Pts',(10.8818989019999,11.6,2.07335651799998));
#195162=CARTESIAN_POINT('Ctrl Pts',(10.8846207019999,15.2,2.07504978699999));
#195163=CARTESIAN_POINT('Ctrl Pts',(10.8846207019999,11.6,2.07504978699998));
#195164=CARTESIAN_POINT('Ctrl Pts',(10.8873454819999,15.2,2.07674795099999));
#195165=CARTESIAN_POINT('Ctrl Pts',(10.8873454819999,11.6,2.07674795099999));
#195166=CARTESIAN_POINT('Ctrl Pts',(10.8900732309999,15.2,2.07845100799998));
#195167=CARTESIAN_POINT('Ctrl Pts',(10.8900732309999,11.6,2.07845100799998));
#195168=CARTESIAN_POINT('Ctrl Pts',(10.8928039389999,15.2,2.08015895999999));
#195169=CARTESIAN_POINT('Ctrl Pts',(10.8928039389999,11.6,2.08015895999999));
#195170=CARTESIAN_POINT('Ctrl Pts',(10.8955375949999,15.2,2.08187180999999));
#195171=CARTESIAN_POINT('Ctrl Pts',(10.8955375949999,11.6,2.08187180999999));
#195172=CARTESIAN_POINT('Ctrl Pts',(10.8982741869999,15.2,2.08358955799998));
#195173=CARTESIAN_POINT('Ctrl Pts',(10.8982741869999,11.6,2.08358955799998));
#195174=CARTESIAN_POINT('Ctrl Pts',(10.9010137039999,15.2,2.08531220599999));
#195175=CARTESIAN_POINT('Ctrl Pts',(10.9010137039999,11.6,2.08531220599998));
#195176=CARTESIAN_POINT('Ctrl Pts',(10.9037561339999,15.2,2.08703975299999));
#195177=CARTESIAN_POINT('Ctrl Pts',(10.9037561339999,11.6,2.08703975299999));
#195178=CARTESIAN_POINT('Ctrl Pts',(10.9065014689999,15.2,2.08877220199998));
#195179=CARTESIAN_POINT('Ctrl Pts',(10.9065014689999,11.6,2.08877220199998));
#195180=CARTESIAN_POINT('Ctrl Pts',(10.9092496959999,15.2,2.09050955499999));
#195181=CARTESIAN_POINT('Ctrl Pts',(10.9092496959999,11.6,2.09050955499999));
#195182=CARTESIAN_POINT('Ctrl Pts',(10.9120008039999,15.2,2.09225181199999));
#195183=CARTESIAN_POINT('Ctrl Pts',(10.9120008039999,11.6,2.09225181199999));
#195184=CARTESIAN_POINT('Ctrl Pts',(10.9147547819999,15.2,2.09399897299999));
#195185=CARTESIAN_POINT('Ctrl Pts',(10.9147547819999,11.6,2.09399897299999));
#195186=CARTESIAN_POINT('Ctrl Pts',(10.9175116189999,15.2,2.09575104199998));
#195187=CARTESIAN_POINT('Ctrl Pts',(10.9175116189999,11.6,2.09575104199998));
#195188=CARTESIAN_POINT('Ctrl Pts',(10.9202713059999,15.2,2.09750801799998));
#195189=CARTESIAN_POINT('Ctrl Pts',(10.9202713059999,11.6,2.09750801799998));
#195190=CARTESIAN_POINT('Ctrl Pts',(10.9230338299999,15.2,2.09926990299998));
#195191=CARTESIAN_POINT('Ctrl Pts',(10.9230338299999,11.6,2.09926990299998));
#195192=CARTESIAN_POINT('Ctrl Pts',(10.9257991809999,15.2,2.10103669699999));
#195193=CARTESIAN_POINT('Ctrl Pts',(10.9257991809999,11.6,2.10103669699999));
#195194=CARTESIAN_POINT('Ctrl Pts',(10.9285673489999,15.2,2.10280840299998));
#195195=CARTESIAN_POINT('Ctrl Pts',(10.9285673489999,11.6,2.10280840299998));
#195196=CARTESIAN_POINT('Ctrl Pts',(10.9313383209999,15.2,2.10458502099999));
#195197=CARTESIAN_POINT('Ctrl Pts',(10.9313383209999,11.6,2.10458502099998));
#195198=CARTESIAN_POINT('Ctrl Pts',(10.9341120879999,15.2,2.10636655199998));
#195199=CARTESIAN_POINT('Ctrl Pts',(10.9341120879999,11.6,2.10636655199998));
#195200=CARTESIAN_POINT('Ctrl Pts',(10.9368886379999,15.2,2.10815299699998));
#195201=CARTESIAN_POINT('Ctrl Pts',(10.9368886379999,11.6,2.10815299699998));
#195202=CARTESIAN_POINT('Ctrl Pts',(10.9396679609999,15.2,2.10994435799998));
#195203=CARTESIAN_POINT('Ctrl Pts',(10.9396679609999,11.6,2.10994435799998));
#195204=CARTESIAN_POINT('Ctrl Pts',(10.9424500479999,15.2,2.11174063499998));
#195205=CARTESIAN_POINT('Ctrl Pts',(10.9424500479999,11.6,2.11174063499998));
#195206=CARTESIAN_POINT('Ctrl Pts',(10.9452348849999,15.2,2.11354182899999));
#195207=CARTESIAN_POINT('Ctrl Pts',(10.9452348849999,11.6,2.11354182899999));
#195208=CARTESIAN_POINT('Ctrl Pts',(10.9480224639999,15.2,2.11534794299999));
#195209=CARTESIAN_POINT('Ctrl Pts',(10.9480224639999,11.6,2.11534794299999));
#195210=CARTESIAN_POINT('Ctrl Pts',(10.9508127719999,15.2,2.11715897599999));
#195211=CARTESIAN_POINT('Ctrl Pts',(10.9508127719999,11.6,2.11715897599999));
#195212=CARTESIAN_POINT('Ctrl Pts',(10.9536057999999,15.2,2.11897492899999));
#195213=CARTESIAN_POINT('Ctrl Pts',(10.9536057999999,11.6,2.11897492899999));
#195214=CARTESIAN_POINT('Ctrl Pts',(10.9564015379999,15.2,2.12079580299998));
#195215=CARTESIAN_POINT('Ctrl Pts',(10.9564015379999,11.6,2.12079580299998));
#195216=CARTESIAN_POINT('Ctrl Pts',(10.9591999729999,15.2,2.12262160099999));
#195217=CARTESIAN_POINT('Ctrl Pts',(10.9591999729999,11.6,2.12262160099998));
#195218=CARTESIAN_POINT('Ctrl Pts',(10.9620010959999,15.2,2.12445232199999));
#195219=CARTESIAN_POINT('Ctrl Pts',(10.9620010959999,11.6,2.12445232199999));
#195220=CARTESIAN_POINT('Ctrl Pts',(10.9648048959999,15.2,2.12628796699999));
#195221=CARTESIAN_POINT('Ctrl Pts',(10.9648048959999,11.6,2.12628796699999));
#195222=CARTESIAN_POINT('Ctrl Pts',(10.9676113639999,15.2,2.12812853899999));
#195223=CARTESIAN_POINT('Ctrl Pts',(10.9676113639999,11.6,2.12812853899999));
#195224=CARTESIAN_POINT('Ctrl Pts',(10.9704204879999,15.2,2.12997403599998));
#195225=CARTESIAN_POINT('Ctrl Pts',(10.9704204879999,11.6,2.12997403599998));
#195226=CARTESIAN_POINT('Ctrl Pts',(10.9732322569999,15.2,2.13182446099998));
#195227=CARTESIAN_POINT('Ctrl Pts',(10.9732322569999,11.6,2.13182446099998));
#195228=CARTESIAN_POINT('Ctrl Pts',(10.9760466609999,15.2,2.13367981399998));
#195229=CARTESIAN_POINT('Ctrl Pts',(10.9760466609999,11.6,2.13367981399998));
#195230=CARTESIAN_POINT('Ctrl Pts',(10.9788636899999,15.2,2.13554009799998));
#195231=CARTESIAN_POINT('Ctrl Pts',(10.9788636899999,11.6,2.13554009799998));
#195232=CARTESIAN_POINT('Ctrl Pts',(10.9816833339999,15.2,2.13740531099999));
#195233=CARTESIAN_POINT('Ctrl Pts',(10.9816833339999,11.6,2.13740531099999));
#195234=CARTESIAN_POINT('Ctrl Pts',(10.9845055819999,15.2,2.13927545499998));
#195235=CARTESIAN_POINT('Ctrl Pts',(10.9845055819999,11.6,2.13927545499998));
#195236=CARTESIAN_POINT('Ctrl Pts',(10.9873304239999,15.2,2.14115053199999));
#195237=CARTESIAN_POINT('Ctrl Pts',(10.9873304239999,11.6,2.14115053199999));
#195238=CARTESIAN_POINT('Ctrl Pts',(10.9901578469999,15.2,2.14303053999998));
#195239=CARTESIAN_POINT('Ctrl Pts',(10.9901578469999,11.6,2.14303053999998));
#195240=CARTESIAN_POINT('Ctrl Pts',(10.9929878449999,15.2,2.14491548299999));
#195241=CARTESIAN_POINT('Ctrl Pts',(10.9929878449999,11.6,2.14491548299998));
#195242=CARTESIAN_POINT('Ctrl Pts',(10.9958204049999,15.2,2.14680536099999));
#195243=CARTESIAN_POINT('Ctrl Pts',(10.9958204049999,11.6,2.14680536099999));
#195244=CARTESIAN_POINT('Ctrl Pts',(10.9986555149999,15.2,2.14870017399999));
#195245=CARTESIAN_POINT('Ctrl Pts',(10.9986555149999,11.6,2.14870017399999));
#195246=CARTESIAN_POINT('Ctrl Pts',(11.0014931689999,15.2,2.15059992399999));
#195247=CARTESIAN_POINT('Ctrl Pts',(11.0014931689999,11.6,2.15059992399999));
#195248=CARTESIAN_POINT('Ctrl Pts',(11.0043333539999,15.2,2.15250460999998));
#195249=CARTESIAN_POINT('Ctrl Pts',(11.0043333539999,11.6,2.15250460999998));
#195250=CARTESIAN_POINT('Ctrl Pts',(11.0071760609999,15.2,2.15441423599998));
#195251=CARTESIAN_POINT('Ctrl Pts',(11.0071760609999,11.6,2.15441423599998));
#195252=CARTESIAN_POINT('Ctrl Pts',(11.0100212779999,15.2,2.15632879999998));
#195253=CARTESIAN_POINT('Ctrl Pts',(11.0100212779999,11.6,2.15632879999998));
#195254=CARTESIAN_POINT('Ctrl Pts',(11.0128689959999,15.2,2.15824830299999));
#195255=CARTESIAN_POINT('Ctrl Pts',(11.0128689959999,11.6,2.15824830299999));
#195256=CARTESIAN_POINT('Ctrl Pts',(11.0157192049999,15.2,2.16017274699999));
#195257=CARTESIAN_POINT('Ctrl Pts',(11.0157192049999,11.6,2.16017274699999));
#195258=CARTESIAN_POINT('Ctrl Pts',(11.0185718939999,15.2,2.16210213199998));
#195259=CARTESIAN_POINT('Ctrl Pts',(11.0185718939999,11.6,2.16210213199998));
#195260=CARTESIAN_POINT('Ctrl Pts',(11.0214270539999,15.2,2.16403645899998));
#195261=CARTESIAN_POINT('Ctrl Pts',(11.0214270539999,11.6,2.16403645899998));
#195262=CARTESIAN_POINT('Ctrl Pts',(11.0242846729999,15.2,2.16597572899999));
#195263=CARTESIAN_POINT('Ctrl Pts',(11.0242846729999,11.6,2.16597572899999));
#195264=CARTESIAN_POINT('Ctrl Pts',(11.0271447429999,15.2,2.16791994299999));
#195265=CARTESIAN_POINT('Ctrl Pts',(11.0271447429999,11.6,2.16791994299998));
#195266=CARTESIAN_POINT('Ctrl Pts',(11.0300072519999,15.2,2.16986909999999));
#195267=CARTESIAN_POINT('Ctrl Pts',(11.0300072519999,11.6,2.16986909999999));
#195268=CARTESIAN_POINT('Ctrl Pts',(11.0328721909999,15.2,2.17182320299999));
#195269=CARTESIAN_POINT('Ctrl Pts',(11.0328721909999,11.6,2.17182320299999));
#195270=CARTESIAN_POINT('Ctrl Pts',(11.0357395489999,15.2,2.17378225199999));
#195271=CARTESIAN_POINT('Ctrl Pts',(11.0357395489999,11.6,2.17378225199999));
#195272=CARTESIAN_POINT('Ctrl Pts',(11.0386093189999,15.2,2.17574624799999));
#195273=CARTESIAN_POINT('Ctrl Pts',(11.0386093189999,11.6,2.17574624799999));
#195274=CARTESIAN_POINT('Ctrl Pts',(11.0414814859999,15.2,2.17771519099998));
#195275=CARTESIAN_POINT('Ctrl Pts',(11.0414814859999,11.6,2.17771519099998));
#195276=CARTESIAN_POINT('Ctrl Pts',(11.0443560429999,15.2,2.17968908099999));
#195277=CARTESIAN_POINT('Ctrl Pts',(11.0443560429999,11.6,2.17968908099999));
#195278=CARTESIAN_POINT('Ctrl Pts',(11.0472329809999,15.2,2.18166791999999));
#195279=CARTESIAN_POINT('Ctrl Pts',(11.0472329809999,11.6,2.18166791999999));
#195280=CARTESIAN_POINT('Ctrl Pts',(11.0501122879999,15.2,2.18365170899999));
#195281=CARTESIAN_POINT('Ctrl Pts',(11.0501122879999,11.6,2.18365170899998));
#195282=CARTESIAN_POINT('Ctrl Pts',(11.0529939539999,15.2,2.18564044699999));
#195283=CARTESIAN_POINT('Ctrl Pts',(11.0529939539999,11.6,2.18564044699999));
#195284=CARTESIAN_POINT('Ctrl Pts',(11.0558779689999,15.2,2.18763413699998));
#195285=CARTESIAN_POINT('Ctrl Pts',(11.0558779689999,11.6,2.18763413699998));
#195286=CARTESIAN_POINT('Ctrl Pts',(11.0587643239999,15.2,2.18963277699999));
#195287=CARTESIAN_POINT('Ctrl Pts',(11.0587643239999,11.6,2.18963277699999));
#195288=CARTESIAN_POINT('Ctrl Pts',(11.0616530089999,15.2,2.19163636999999));
#195289=CARTESIAN_POINT('Ctrl Pts',(11.0616530089999,11.6,2.19163636999998));
#195290=CARTESIAN_POINT('Ctrl Pts',(11.0645440139999,15.2,2.19364491499999));
#195291=CARTESIAN_POINT('Ctrl Pts',(11.0645440139999,11.6,2.19364491499999));
#195292=CARTESIAN_POINT('Ctrl Pts',(11.0674373299999,15.2,2.19565841299998));
#195293=CARTESIAN_POINT('Ctrl Pts',(11.0674373299999,11.6,2.19565841299998));
#195294=CARTESIAN_POINT('Ctrl Pts',(11.0703329449999,15.2,2.19767686499999));
#195295=CARTESIAN_POINT('Ctrl Pts',(11.0703329449999,11.6,2.19767686499999));
#195296=CARTESIAN_POINT('Ctrl Pts',(11.0732308509999,15.2,2.19970027199999));
#195297=CARTESIAN_POINT('Ctrl Pts',(11.0732308509999,11.6,2.19970027199999));
#195298=CARTESIAN_POINT('Ctrl Pts',(11.0761310369999,15.2,2.20172863399998));
#195299=CARTESIAN_POINT('Ctrl Pts',(11.0761310369999,11.6,2.20172863399998));
#195300=CARTESIAN_POINT('Ctrl Pts',(11.0790334939999,15.2,2.20376195199998));
#195301=CARTESIAN_POINT('Ctrl Pts',(11.0790334939999,11.6,2.20376195199998));
#195302=CARTESIAN_POINT('Ctrl Pts',(11.0819382109999,15.2,2.20580022499998));
#195303=CARTESIAN_POINT('Ctrl Pts',(11.0819382109999,11.6,2.20580022499998));
#195304=CARTESIAN_POINT('Ctrl Pts',(11.0848451789999,15.2,2.20784345599998));
#195305=CARTESIAN_POINT('Ctrl Pts',(11.0848451789999,11.6,2.20784345599998));
#195306=CARTESIAN_POINT('Ctrl Pts',(11.0877543899999,15.2,2.20989164299999));
#195307=CARTESIAN_POINT('Ctrl Pts',(11.0877543899999,11.6,2.20989164299999));
#195308=CARTESIAN_POINT('Ctrl Pts',(11.0906658309999,15.2,2.21194478999998));
#195309=CARTESIAN_POINT('Ctrl Pts',(11.0906658309999,11.6,2.21194478999998));
#195310=CARTESIAN_POINT('Ctrl Pts',(11.0935794949999,15.2,2.21400289499998));
#195311=CARTESIAN_POINT('Ctrl Pts',(11.0935794949999,11.6,2.21400289499998));
#195312=CARTESIAN_POINT('Ctrl Pts',(11.0964953709999,15.2,2.21606595799999));
#195313=CARTESIAN_POINT('Ctrl Pts',(11.0964953709999,11.6,2.21606595799999));
#195314=CARTESIAN_POINT('Ctrl Pts',(11.0994134489999,15.2,2.21813398099998));
#195315=CARTESIAN_POINT('Ctrl Pts',(11.0994134489999,11.6,2.21813398099998));
#195316=CARTESIAN_POINT('Ctrl Pts',(11.1023337189999,15.2,2.22020696299999));
#195317=CARTESIAN_POINT('Ctrl Pts',(11.1023337189999,11.6,2.22020696299999));
#195318=CARTESIAN_POINT('Ctrl Pts',(11.1052561719999,15.2,2.22228490799999));
#195319=CARTESIAN_POINT('Ctrl Pts',(11.1052561719999,11.6,2.22228490799999));
#195320=CARTESIAN_POINT('Ctrl Pts',(11.1081808009999,15.2,2.22436781199999));
#195321=CARTESIAN_POINT('Ctrl Pts',(11.1081808009999,11.6,2.22436781199999));
#195322=CARTESIAN_POINT('Ctrl Pts',(11.1111075909999,15.2,2.22645567899999));
#195323=CARTESIAN_POINT('Ctrl Pts',(11.1111075909999,11.6,2.22645567899999));
#195324=CARTESIAN_POINT('Ctrl Pts',(11.1140365369999,15.2,2.22854850799999));
#195325=CARTESIAN_POINT('Ctrl Pts',(11.1140365369999,11.6,2.22854850799999));
#195326=CARTESIAN_POINT('Ctrl Pts',(11.1169676269999,15.2,2.23064629899998));
#195327=CARTESIAN_POINT('Ctrl Pts',(11.1169676269999,11.6,2.23064629899998));
#195328=CARTESIAN_POINT('Ctrl Pts',(11.1199008519999,15.2,2.23274905299998));
#195329=CARTESIAN_POINT('Ctrl Pts',(11.1199008519999,11.6,2.23274905299998));
#195330=CARTESIAN_POINT('Ctrl Pts',(11.1228362039999,15.2,2.23485677099998));
#195331=CARTESIAN_POINT('Ctrl Pts',(11.1228362039999,11.6,2.23485677099998));
#195332=CARTESIAN_POINT('Ctrl Pts',(11.1257736699999,15.2,2.23696945299999));
#195333=CARTESIAN_POINT('Ctrl Pts',(11.1257736699999,11.6,2.23696945299999));
#195334=CARTESIAN_POINT('Ctrl Pts',(11.1287132429999,15.2,2.23908709899999));
#195335=CARTESIAN_POINT('Ctrl Pts',(11.1287132429999,11.6,2.23908709899999));
#195336=CARTESIAN_POINT('Ctrl Pts',(11.1316549139999,15.2,2.24120970899999));
#195337=CARTESIAN_POINT('Ctrl Pts',(11.1316549139999,11.6,2.24120970899999));
#195338=CARTESIAN_POINT('Ctrl Pts',(11.1345986719999,15.2,2.24333728499999));
#195339=CARTESIAN_POINT('Ctrl Pts',(11.1345986719999,11.6,2.24333728499999));
#195340=CARTESIAN_POINT('Ctrl Pts',(11.1375445069999,15.2,2.24546982699998));
#195341=CARTESIAN_POINT('Ctrl Pts',(11.1375445069999,11.6,2.24546982699998));
#195342=CARTESIAN_POINT('Ctrl Pts',(11.1404924099999,15.2,2.24760733499998));
#195343=CARTESIAN_POINT('Ctrl Pts',(11.1404924099999,11.6,2.24760733499998));
#195344=CARTESIAN_POINT('Ctrl Pts',(11.1434423739999,15.2,2.24974980999999));
#195345=CARTESIAN_POINT('Ctrl Pts',(11.1434423739999,11.6,2.24974980999999));
#195346=CARTESIAN_POINT('Ctrl Pts',(11.1463943869999,15.2,2.25189725099999));
#195347=CARTESIAN_POINT('Ctrl Pts',(11.1463943869999,11.6,2.25189725099999));
#195348=CARTESIAN_POINT('Ctrl Pts',(11.1493484399999,15.2,2.25404965899999));
#195349=CARTESIAN_POINT('Ctrl Pts',(11.1493484399999,11.6,2.25404965899999));
#195350=CARTESIAN_POINT('Ctrl Pts',(11.1523045239999,15.2,2.25620703599999));
#195351=CARTESIAN_POINT('Ctrl Pts',(11.1523045239999,11.6,2.25620703599999));
#195352=CARTESIAN_POINT('Ctrl Pts',(11.1552626289999,15.2,2.25836937999999));
#195353=CARTESIAN_POINT('Ctrl Pts',(11.1552626289999,11.6,2.25836937999999));
#195354=CARTESIAN_POINT('Ctrl Pts',(11.1582227479999,15.2,2.26053669299999));
#195355=CARTESIAN_POINT('Ctrl Pts',(11.1582227479999,11.6,2.26053669299999));
#195356=CARTESIAN_POINT('Ctrl Pts',(11.1611848689999,15.2,2.26270897399999));
#195357=CARTESIAN_POINT('Ctrl Pts',(11.1611848689999,11.6,2.26270897399999));
#195358=CARTESIAN_POINT('Ctrl Pts',(11.1641489819999,15.2,2.26488622499998));
#195359=CARTESIAN_POINT('Ctrl Pts',(11.1641489819999,11.6,2.26488622499998));
#195360=CARTESIAN_POINT('Ctrl Pts',(11.1671150809999,15.2,2.26706844399999));
#195361=CARTESIAN_POINT('Ctrl Pts',(11.1671150809999,11.6,2.26706844399999));
#195362=CARTESIAN_POINT('Ctrl Pts',(11.1700831519999,15.2,2.26925563399998));
#195363=CARTESIAN_POINT('Ctrl Pts',(11.1700831519999,11.6,2.26925563399998));
#195364=CARTESIAN_POINT('Ctrl Pts',(11.1730531909999,15.2,2.27144779399998));
#195365=CARTESIAN_POINT('Ctrl Pts',(11.1730531909999,11.6,2.27144779399998));
#195366=CARTESIAN_POINT('Ctrl Pts',(11.1760251839999,15.2,2.27364492299999));
#195367=CARTESIAN_POINT('Ctrl Pts',(11.1760251839999,11.6,2.27364492299999));
#195368=CARTESIAN_POINT('Ctrl Pts',(11.1789991259999,15.2,2.27584702399998));
#195369=CARTESIAN_POINT('Ctrl Pts',(11.1789991259999,11.6,2.27584702399998));
#195370=CARTESIAN_POINT('Ctrl Pts',(11.1819750049999,15.2,2.27805409499998));
#195371=CARTESIAN_POINT('Ctrl Pts',(11.1819750049999,11.6,2.27805409499998));
#195372=CARTESIAN_POINT('Ctrl Pts',(11.1849528119999,15.2,2.28026613799999));
#195373=CARTESIAN_POINT('Ctrl Pts',(11.1849528119999,11.6,2.28026613799999));
#195374=CARTESIAN_POINT('Ctrl Pts',(11.1879325399999,15.2,2.28248315199998));
#195375=CARTESIAN_POINT('Ctrl Pts',(11.1879325399999,11.6,2.28248315199998));
#195376=CARTESIAN_POINT('Ctrl Pts',(11.1909141789999,15.2,2.28470513899998));
#195377=CARTESIAN_POINT('Ctrl Pts',(11.1909141789999,11.6,2.28470513899998));
#195378=CARTESIAN_POINT('Ctrl Pts',(11.1938977179999,15.2,2.28693209699999));
#195379=CARTESIAN_POINT('Ctrl Pts',(11.1938977179999,11.6,2.28693209699998));
#195380=CARTESIAN_POINT('Ctrl Pts',(11.1968831489999,15.2,2.28916402699999));
#195381=CARTESIAN_POINT('Ctrl Pts',(11.1968831489999,11.6,2.28916402699999));
#195382=CARTESIAN_POINT('Ctrl Pts',(11.1998704629999,15.2,2.29140092999998));
#195383=CARTESIAN_POINT('Ctrl Pts',(11.1998704629999,11.6,2.29140092999998));
#195384=CARTESIAN_POINT('Ctrl Pts',(11.2028596489999,15.2,2.29364280599999));
#195385=CARTESIAN_POINT('Ctrl Pts',(11.2028596489999,11.6,2.29364280599999));
#195386=CARTESIAN_POINT('Ctrl Pts',(11.2058506979999,15.2,2.29588965499998));
#195387=CARTESIAN_POINT('Ctrl Pts',(11.2058506979999,11.6,2.29588965499998));
#195388=CARTESIAN_POINT('Ctrl Pts',(11.2088436019999,15.2,2.29814147699999));
#195389=CARTESIAN_POINT('Ctrl Pts',(11.2088436019999,11.6,2.29814147699999));
#195390=CARTESIAN_POINT('Ctrl Pts',(11.2118383509999,15.2,2.30039827199999));
#195391=CARTESIAN_POINT('Ctrl Pts',(11.2118383509999,11.6,2.30039827199999));
#195392=CARTESIAN_POINT('Ctrl Pts',(11.2148349389999,15.2,2.30266004199999));
#195393=CARTESIAN_POINT('Ctrl Pts',(11.2148349389999,11.6,2.30266004199999));
#195394=CARTESIAN_POINT('Ctrl Pts',(11.2178333559999,15.2,2.30492678499999));
#195395=CARTESIAN_POINT('Ctrl Pts',(11.2178333559999,11.6,2.30492678499999));
#195396=CARTESIAN_POINT('Ctrl Pts',(11.2208335929999,15.2,2.30719850199999));
#195397=CARTESIAN_POINT('Ctrl Pts',(11.2208335929999,11.6,2.30719850199998));
#195398=CARTESIAN_POINT('Ctrl Pts',(11.2238356439999,15.2,2.30947519299999));
#195399=CARTESIAN_POINT('Ctrl Pts',(11.2238356439999,11.6,2.30947519299999));
#195400=CARTESIAN_POINT('Ctrl Pts',(11.2268394979999,15.2,2.31175685899998));
#195401=CARTESIAN_POINT('Ctrl Pts',(11.2268394979999,11.6,2.31175685899998));
#195402=CARTESIAN_POINT('Ctrl Pts',(11.2298451429999,15.2,2.31404349899998));
#195403=CARTESIAN_POINT('Ctrl Pts',(11.2298451429999,11.6,2.31404349899998));
#195404=CARTESIAN_POINT('Ctrl Pts',(11.2328525719999,15.2,2.31633511299998));
#195405=CARTESIAN_POINT('Ctrl Pts',(11.2328525719999,11.6,2.31633511299998));
#195406=CARTESIAN_POINT('Ctrl Pts',(11.2358617709999,15.2,2.31863170299999));
#195407=CARTESIAN_POINT('Ctrl Pts',(11.2358617709999,11.6,2.31863170299999));
#195408=CARTESIAN_POINT('Ctrl Pts',(11.2388727289999,15.2,2.32093326799999));
#195409=CARTESIAN_POINT('Ctrl Pts',(11.2388727289999,11.6,2.32093326799998));
#195410=CARTESIAN_POINT('Ctrl Pts',(11.2418854369999,15.2,2.32323980799999));
#195411=CARTESIAN_POINT('Ctrl Pts',(11.2418854369999,11.6,2.32323980799999));
#195412=CARTESIAN_POINT('Ctrl Pts',(11.2448998869999,15.2,2.32555132399999));
#195413=CARTESIAN_POINT('Ctrl Pts',(11.2448998869999,11.6,2.32555132399999));
#195414=CARTESIAN_POINT('Ctrl Pts',(11.2479160729999,15.2,2.32786781599998));
#195415=CARTESIAN_POINT('Ctrl Pts',(11.2479160729999,11.6,2.32786781599998));
#195416=CARTESIAN_POINT('Ctrl Pts',(11.2509339899999,15.2,2.33018928199999));
#195417=CARTESIAN_POINT('Ctrl Pts',(11.2509339899999,11.6,2.33018928199999));
#195418=CARTESIAN_POINT('Ctrl Pts',(11.2539536379999,15.2,2.33251572499999));
#195419=CARTESIAN_POINT('Ctrl Pts',(11.2539536379999,11.6,2.33251572499999));
#195420=CARTESIAN_POINT('Ctrl Pts',(11.2563707379999,15.2,2.33438085799999));
#195421=CARTESIAN_POINT('Ctrl Pts',(11.2563707379999,11.6,2.33438085799999));
#195422=CARTESIAN_POINT('Ctrl Pts',(11.2581843409999,15.2,2.33578194799998));
#195423=CARTESIAN_POINT('Ctrl Pts',(11.2581843409999,11.6,2.33578194799998));
#195424=CARTESIAN_POINT('Ctrl Pts',(11.2593937549999,15.2,2.33671700299999));
#195425=CARTESIAN_POINT('Ctrl Pts',(11.2593937549999,11.6,2.33671700299999));
#195426=CARTESIAN_POINT('Ctrl Pts',(11.2599985479999,15.2,2.33718477899998));
#195427=CARTESIAN_POINT('Ctrl Pts',(11.2599985479999,11.6,2.33718477899998));
#195428=CARTESIAN_POINT('Ctrl Pts',(10.2237731089999,15.2,1.76496130799999));
#195429=CARTESIAN_POINT('Ctrl Pts',(10.2255010835344,15.2,1.76541541469069));
#195430=CARTESIAN_POINT('Ctrl Pts',(10.227282994496,15.2,1.76588926687173));
#195431=CARTESIAN_POINT('Ctrl Pts',(10.2291177138156,15.2,1.76638321167919));
#195432=CARTESIAN_POINT('Ctrl Pts',(10.2309612810791,15.2,1.76687953853818));
#195433=CARTESIAN_POINT('Ctrl Pts',(10.2328581800569,15.2,1.76739616235299));
#195434=CARTESIAN_POINT('Ctrl Pts',(10.2348073231802,15.2,1.76793345482698));
#195435=CARTESIAN_POINT('Ctrl Pts',(10.2367564661265,15.2,1.76847074725216));
#195436=CARTESIAN_POINT('Ctrl Pts',(10.2387578528578,15.2,1.76902870390431));
#195437=CARTESIAN_POINT('Ctrl Pts',(10.2408104327832,15.2,1.76960768554995));
#195438=CARTESIAN_POINT('Ctrl Pts',(10.2428630127086,15.2,1.77018666719558));
#195439=CARTESIAN_POINT('Ctrl Pts',(10.2449667829652,15.2,1.77078667349933));
#195440=CARTESIAN_POINT('Ctrl Pts',(10.2471207194916,15.2,1.77140804417322));
#195441=CARTESIAN_POINT('Ctrl Pts',(10.2492746562137,15.2,1.77202941490356));
#195442=CARTESIAN_POINT('Ctrl Pts',(10.251478760386,15.2,1.77267215322636));
#195443=CARTESIAN_POINT('Ctrl Pts',(10.2537320330121,15.2,1.77333658784738));
#195444=CARTESIAN_POINT('Ctrl Pts',(10.256360850769,15.2,1.77411176148137));
#195445=CARTESIAN_POINT('Ctrl Pts',(10.2590565910528,15.2,1.77491646793701));
#195446=CARTESIAN_POINT('Ctrl Pts',(10.261817718071,15.2,1.77575121364745));
#195447=CARTESIAN_POINT('Ctrl Pts',(10.2641843986488,15.2,1.77646671005425));
#195448=CARTESIAN_POINT('Ctrl Pts',(10.2665991148725,15.2,1.77720427386484));
#195449=CARTESIAN_POINT('Ctrl Pts',(10.2690609287599,15.2,1.77796421232445));
#195450=CARTESIAN_POINT('Ctrl Pts',(10.2715227424237,15.2,1.77872415071503));
#195451=CARTESIAN_POINT('Ctrl Pts',(10.2740316523571,15.2,1.77950646297585));
#195452=CARTESIAN_POINT('Ctrl Pts',(10.276586740026,15.2,1.78031144528365));
#195453=CARTESIAN_POINT('Ctrl Pts',(10.2791418276949,15.2,1.78111642759145));
#195454=CARTESIAN_POINT('Ctrl Pts',(10.281743092104,15.2,1.78194408006059));
#195455=CARTESIAN_POINT('Ctrl Pts',(10.2843896398392,15.2,1.78279468544535));
#195456=CARTESIAN_POINT('Ctrl Pts',(10.2870361878147,15.2,1.78364529090738));
#195457=CARTESIAN_POINT('Ctrl Pts',(10.2897280175293,15.2,1.78451885269724));
#195458=CARTESIAN_POINT('Ctrl Pts',(10.2924642530148,15.2,1.78541564208104));
#195459=CARTESIAN_POINT('Ctrl Pts',(10.2952004882518,15.2,1.78631243138337));
#195460=CARTESIAN_POINT('Ctrl Pts',(10.2979811341463,15.2,1.78723245159305));
#195461=CARTESIAN_POINT('Ctrl Pts',(10.300805332129,15.2,1.7881759658098));
#195462=CARTESIAN_POINT('Ctrl Pts',(10.3036295301116,15.2,1.78911948002654));
#195463=CARTESIAN_POINT('Ctrl Pts',(10.3064972817074,15.2,1.79008648852474));
#195464=CARTESIAN_POINT('Ctrl Pts',(10.3094077538498,15.2,1.79107724790438));
#195465=CARTESIAN_POINT('Ctrl Pts',(10.3123182259922,15.2,1.79206800728402));
#195466=CARTESIAN_POINT('Ctrl Pts',(10.3152714181101,15.2,1.79308251966779));
#195467=CARTESIAN_POINT('Ctrl Pts',(10.3182665162484,15.2,1.79412102887842));
#195468=CARTESIAN_POINT('Ctrl Pts',(10.3212616146588,15.2,1.79515953818338));
#195469=CARTESIAN_POINT('Ctrl Pts',(10.3242986165983,15.2,1.79622204662399));
#195470=CARTESIAN_POINT('Ctrl Pts',(10.3273767299345,15.2,1.79730879360094));
#195471=CARTESIAN_POINT('Ctrl Pts',(10.3304548429911,15.2,1.79839554047917));
#195472=CARTESIAN_POINT('Ctrl Pts',(10.3335740630194,15.2,1.79950652453049));
#195473=CARTESIAN_POINT('Ctrl Pts',(10.3367336133195,15.2,1.80064197665483));
#195474=CARTESIAN_POINT('Ctrl Pts',(10.3398931636196,15.2,1.80177742877918));
#195475=CARTESIAN_POINT('Ctrl Pts',(10.3430930440172,15.2,1.80293735075722));
#195476=CARTESIAN_POINT('Ctrl Pts',(10.3463324913968,15.2,1.80412196462916));
#195477=CARTESIAN_POINT('Ctrl Pts',(10.3495719390707,15.2,1.8053065786087));
#195478=CARTESIAN_POINT('Ctrl Pts',(10.3528509547067,15.2,1.8065158840573));
#195479=CARTESIAN_POINT('Ctrl Pts',(10.3561687904725,15.2,1.80775009704231));
#195480=CARTESIAN_POINT('Ctrl Pts',(10.359486625937,15.2,1.80898430991522));
#195481=CARTESIAN_POINT('Ctrl Pts',(10.3628432832897,15.2,1.81024343075692));
#195482=CARTESIAN_POINT('Ctrl Pts',(10.366238030015,15.2,1.81152766671603));
#195483=CARTESIAN_POINT('Ctrl Pts',(10.3696327767403,15.2,1.81281190267514));
#195484=CARTESIAN_POINT('Ctrl Pts',(10.3730656142586,15.2,1.81412125483802));
#195485=CARTESIAN_POINT('Ctrl Pts',(10.37653582588,15.2,1.81545592462113));
#195486=CARTESIAN_POINT('Ctrl Pts',(10.3800060378165,15.2,1.81679059452548));
#195487=CARTESIAN_POINT('Ctrl Pts',(10.3835136246788,15.2,1.81815058024617));
#195488=CARTESIAN_POINT('Ctrl Pts',(10.3870578838012,15.2,1.81953607914237));
#195489=CARTESIAN_POINT('Ctrl Pts',(10.3906021426016,15.2,1.82092157791272));
#195490=CARTESIAN_POINT('Ctrl Pts',(10.3941830753479,15.2,1.8223325864188));
#195491=CARTESIAN_POINT('Ctrl Pts',(10.3977999920499,15.2,1.82376929619994));
#195492=CARTESIAN_POINT('Ctrl Pts',(10.4014169087518,15.2,1.82520600598107));
#195493=CARTESIAN_POINT('Ctrl Pts',(10.4050698101533,15.2,1.82666841365391));
#195494=CARTESIAN_POINT('Ctrl Pts',(10.4087580231182,15.2,1.82815670433936));
#195495=CARTESIAN_POINT('Ctrl Pts',(10.4124462364181,15.2,1.82964499516));
#195496=CARTESIAN_POINT('Ctrl Pts',(10.416169759044,15.2,1.83115916493211));
#195497=CARTESIAN_POINT('Ctrl Pts',(10.4199279311679,15.2,1.8326993936845));
#195498=CARTESIAN_POINT('Ctrl Pts',(10.4230597411004,15.2,1.83398291757487));
#195499=CARTESIAN_POINT('Ctrl Pts',(10.4262156133916,15.2,1.83528453345442));
#195500=CARTESIAN_POINT('Ctrl Pts',(10.4293951716574,15.2,1.83660434491424));
#195501=CARTESIAN_POINT('Ctrl Pts',(10.4325747295767,15.2,1.8379241562302));
#195502=CARTESIAN_POINT('Ctrl Pts',(10.4357779722426,15.2,1.83926216116631));
#195503=CARTESIAN_POINT('Ctrl Pts',(10.4390045303612,15.2,1.84061845407254));
#195504=CARTESIAN_POINT('Ctrl Pts',(10.4422310888315,15.2,1.8419747471266));
#195505=CARTESIAN_POINT('Ctrl Pts',(10.4454809623459,15.2,1.8433493293748));
#195506=CARTESIAN_POINT('Ctrl Pts',(10.4487537865801,15.2,1.84474229256775));
#195507=CARTESIAN_POINT('Ctrl Pts',(10.4520266108144,15.2,1.84613525576069));
#195508=CARTESIAN_POINT('Ctrl Pts',(10.4553223845839,15.2,1.8475466014861));
#195509=CARTESIAN_POINT('Ctrl Pts',(10.4586407491231,15.2,1.84897641808402));
#195510=CARTESIAN_POINT('Ctrl Pts',(10.4619591136623,15.2,1.85040623468195));
#195511=CARTESIAN_POINT('Ctrl Pts',(10.4653000711479,15.2,1.8518545245162));
#195512=CARTESIAN_POINT('Ctrl Pts',(10.4686632630217,15.2,1.85332137340412));
#195513=CARTESIAN_POINT('Ctrl Pts',(10.4720264548956,15.2,1.85478822229204));
#195514=CARTESIAN_POINT('Ctrl Pts',(10.4754118847616,15.2,1.85627363004155));
#195515=CARTESIAN_POINT('Ctrl Pts',(10.4788192008022,15.2,1.85777768386002));
#195516=CARTESIAN_POINT('Ctrl Pts',(10.4835894433332,15.2,1.85988335923867));
#195517=CARTESIAN_POINT('Ctrl Pts',(10.4884025857108,15.2,1.86202557789432));
#195518=CARTESIAN_POINT('Ctrl Pts',(10.4932576867185,15.2,1.86420456661017));
#195519=CARTESIAN_POINT('Ctrl Pts',(10.4974192016519,15.2,1.86607227112682));
#195520=CARTESIAN_POINT('Ctrl Pts',(10.5016115419829,15.2,1.86796699033299));
#195521=CARTESIAN_POINT('Ctrl Pts',(10.5058341272449,15.2,1.86988886092864));
#195522=CARTESIAN_POINT('Ctrl Pts',(10.5093529484243,15.2,1.87149041981655));
#195523=CARTESIAN_POINT('Ctrl Pts',(10.5128927747652,15.2,1.87311083441943));
#195524=CARTESIAN_POINT('Ctrl Pts',(10.5164532710313,15.2,1.87475017998238));
#195525=CARTESIAN_POINT('Ctrl Pts',(10.5207258663954,15.2,1.87671739458644));
#195526=CARTESIAN_POINT('Ctrl Pts',(10.5250282293371,15.2,1.87871187060489));
#195527=CARTESIAN_POINT('Ctrl Pts',(10.5293597965111,15.2,1.88073373802956));
#195528=CARTESIAN_POINT('Ctrl Pts',(10.5329694359539,15.2,1.88241862761134));
#195529=CARTESIAN_POINT('Ctrl Pts',(10.5365993542464,15.2,1.88412253659281));
#195530=CARTESIAN_POINT('Ctrl Pts',(10.5402492320225,15.2,1.88584553950791));
#195531=CARTESIAN_POINT('Ctrl Pts',(10.5438991097986,15.2,1.887568542423));
#195532=CARTESIAN_POINT('Ctrl Pts',(10.5475689445887,15.2,1.88931063802));
#195533=CARTESIAN_POINT('Ctrl Pts',(10.551258421855,15.2,1.89107189532888));
#195534=CARTESIAN_POINT('Ctrl Pts',(10.5549478991213,15.2,1.89283315263777));
#195535=CARTESIAN_POINT('Ctrl Pts',(10.5586570170905,15.2,1.89461357251113));
#195536=CARTESIAN_POINT('Ctrl Pts',(10.5623854625062,15.2,1.89641322285736));
#195537=CARTESIAN_POINT('Ctrl Pts',(10.5661139079218,15.2,1.89821287320358));
#195538=CARTESIAN_POINT('Ctrl Pts',(10.5698616819046,15.2,1.90003175384195));
#195539=CARTESIAN_POINT('Ctrl Pts',(10.573628473987,15.2,1.9018699293965));
#195540=CARTESIAN_POINT('Ctrl Pts',(10.5766419078171,15.2,1.90334046992029));
#195541=CARTESIAN_POINT('Ctrl Pts',(10.5796675144474,15.2,1.90482335915971));
#195542=CARTESIAN_POINT('Ctrl Pts',(10.5827051359324,15.2,1.90631863098364));
#195543=CARTESIAN_POINT('Ctrl Pts',(10.5865021625817,15.2,1.9081877206617));
#195544=CARTESIAN_POINT('Ctrl Pts',(10.5903179639277,15.2,1.91007615824236));
#195545=CARTESIAN_POINT('Ctrl Pts',(10.5941522369848,15.2,1.91198400296616));
#195546=CARTESIAN_POINT('Ctrl Pts',(10.5972196551796,15.2,1.91351027862042));
#195547=CARTESIAN_POINT('Ctrl Pts',(10.6002988962174,15.2,1.9150489769342));
#195548=CARTESIAN_POINT('Ctrl Pts',(10.603389806964,15.2,1.91660012713992));
#195549=CARTESIAN_POINT('Ctrl Pts',(10.6064807181317,15.2,1.91815127755698));
#195550=CARTESIAN_POINT('Ctrl Pts',(10.6095832977116,15.2,1.91971488102687));
#195551=CARTESIAN_POINT('Ctrl Pts',(10.6126973964268,15.2,1.92129096747037));
#195552=CARTESIAN_POINT('Ctrl Pts',(10.6158114947177,15.2,1.92286705369913));
#195553=CARTESIAN_POINT('Ctrl Pts',(10.6189371099674,15.2,1.92445562162032));
#195554=CARTESIAN_POINT('Ctrl Pts',(10.6220740947102,15.2,1.9260567018775));
#195555=CARTESIAN_POINT('Ctrl Pts',(10.6267795724656,15.2,1.9284583225905));
#195556=CARTESIAN_POINT('Ctrl Pts',(10.6315106270658,15.2,1.93088809770698));
#195557=CARTESIAN_POINT('Ctrl Pts',(10.6362667610767,15.2,1.93334612025953));
#195558=CARTESIAN_POINT('Ctrl Pts',(10.6402302054377,15.2,1.93539447205175));
#195559=CARTESIAN_POINT('Ctrl Pts',(10.6442110659086,15.2,1.9374624416227));
#195560=CARTESIAN_POINT('Ctrl Pts',(10.6482090562353,15.2,1.93955008097688));
#195561=CARTESIAN_POINT('Ctrl Pts',(10.6514074490196,15.2,1.94122019273328));
#195562=CARTESIAN_POINT('Ctrl Pts',(10.6546168056938,15.2,1.9429028934992));
#195563=CARTESIAN_POINT('Ctrl Pts',(10.6578369822582,15.2,1.94459821175827));
#195564=CARTESIAN_POINT('Ctrl Pts',(10.6610571588226,15.2,1.94629353001733));
#195565=CARTESIAN_POINT('Ctrl Pts',(10.6642881529605,15.2,1.94800146288064));
#195566=CARTESIAN_POINT('Ctrl Pts',(10.6675298243049,15.2,1.94972203853126));
#195567=CARTESIAN_POINT('Ctrl Pts',(10.6715819128229,15.2,1.95187275774288));
#195568=CARTESIAN_POINT('Ctrl Pts',(10.6756506826844,15.2,1.9540432316316));
#195569=CARTESIAN_POINT('Ctrl Pts',(10.6797358577239,15.2,1.95623350673846));
#195570=CARTESIAN_POINT('Ctrl Pts',(10.6830039982898,15.2,1.95798572711043));
#195571=CARTESIAN_POINT('Ctrl Pts',(10.686282637504,15.2,1.95975062134473));
#195572=CARTESIAN_POINT('Ctrl Pts',(10.6895716350166,15.2,1.96152821427493));
#195573=CARTESIAN_POINT('Ctrl Pts',(10.6928606325291,15.2,1.96330580720514));
#195574=CARTESIAN_POINT('Ctrl Pts',(10.6961599902013,15.2,1.96509609760628));
#195575=CARTESIAN_POINT('Ctrl Pts',(10.6994695675494,15.2,1.96689911059474));
#195576=CARTESIAN_POINT('Ctrl Pts',(10.7036065385581,15.2,1.96915287646182));
#195577=CARTESIAN_POINT('Ctrl Pts',(10.7077594778936,15.2,1.97142652144045));
#195578=CARTESIAN_POINT('Ctrl Pts',(10.7119281188963,15.2,1.97372008896661));
#195579=CARTESIAN_POINT('Ctrl Pts',(10.7152630322437,15.2,1.97555494328754));
#195580=CARTESIAN_POINT('Ctrl Pts',(10.7186079935643,15.2,1.97740254944576));
#195581=CARTESIAN_POINT('Ctrl Pts',(10.7219628670249,15.2,1.9792629284916));
#195582=CARTESIAN_POINT('Ctrl Pts',(10.7253177404855,15.2,1.98112330753744));
#195583=CARTESIAN_POINT('Ctrl Pts',(10.7286825267667,15.2,1.98299645954587));
#195584=CARTESIAN_POINT('Ctrl Pts',(10.732057090285,15.2,1.98488240781663));
#195585=CARTESIAN_POINT('Ctrl Pts',(10.7362752939931,15.2,1.98723984276964));
#195586=CARTESIAN_POINT('Ctrl Pts',(10.7405087750363,15.2,1.98961727000487));
#195587=CARTESIAN_POINT('Ctrl Pts',(10.7447572736692,15.2,1.99201473168635));
#195588=CARTESIAN_POINT('Ctrl Pts',(10.7481560731312,15.2,1.99393270134512));
#195589=CARTESIAN_POINT('Ctrl Pts',(10.7515644829914,15.2,1.99586349233844));
#195590=CARTESIAN_POINT('Ctrl Pts',(10.7549823717332,15.2,1.99780712599993));
#195591=CARTESIAN_POINT('Ctrl Pts',(10.7584002604751,15.2,1.99975075966142));
#195592=CARTESIAN_POINT('Ctrl Pts',(10.7618276281264,15.2,2.00170723580496));
#195593=CARTESIAN_POINT('Ctrl Pts',(10.7652643430368,15.2,2.00367657408026));
#195594=CARTESIAN_POINT('Ctrl Pts',(10.768701057479,15.2,2.00564591208724));
#195595=CARTESIAN_POINT('Ctrl Pts',(10.7721471206199,15.2,2.0076281130971));
#195596=CARTESIAN_POINT('Ctrl Pts',(10.7756024004642,15.2,2.00962319449858));
#195597=CARTESIAN_POINT('Ctrl Pts',(10.7790576807793,15.2,2.01161827617189));
#195598=CARTESIAN_POINT('Ctrl Pts',(10.7825221798915,15.2,2.01362623970223));
#195599=CARTESIAN_POINT('Ctrl Pts',(10.7859957680262,15.2,2.01564710281369));
#195600=CARTESIAN_POINT('Ctrl Pts',(10.7903377529579,15.2,2.01817318156534));
#195601=CARTESIAN_POINT('Ctrl Pts',(10.7946939390982,15.2,2.02071941883954));
#195602=CARTESIAN_POINT('Ctrl Pts',(10.7990640790299,15.2,2.02328584661897));
#195603=CARTESIAN_POINT('Ctrl Pts',(10.8043082467573,15.2,2.02636555984238));
#195604=CARTESIAN_POINT('Ctrl Pts',(10.8095725046703,15.2,2.02947435145939));
#195605=CARTESIAN_POINT('Ctrl Pts',(10.8148564305023,15.2,2.03261227677636));
#195606=CARTESIAN_POINT('Ctrl Pts',(10.8183790475637,15.2,2.03470422689267));
#195607=CARTESIAN_POINT('Ctrl Pts',(10.8219104058475,15.2,2.03680912705869));
#195608=CARTESIAN_POINT('Ctrl Pts',(10.8254503796128,15.2,2.03892699116201));
#195609=CARTESIAN_POINT('Ctrl Pts',(10.8289903538604,15.2,2.04104485555388));
#195610=CARTESIAN_POINT('Ctrl Pts',(10.8325389445422,15.2,2.04317568727476));
#195611=CARTESIAN_POINT('Ctrl Pts',(10.8360960274582,15.2,2.04531950022493));
#195612=CARTESIAN_POINT('Ctrl Pts',(10.8396531103743,15.2,2.0474633131751));
#195613=CARTESIAN_POINT('Ctrl Pts',(10.843218685572,15.2,2.04962010746013));
#195614=CARTESIAN_POINT('Ctrl Pts',(10.8467926311009,15.2,2.0517898990797));
#195615=CARTESIAN_POINT('Ctrl Pts',(10.8512600622817,15.2,2.05450213816072));
#195616=CARTESIAN_POINT('Ctrl Pts',(10.8557405708641,15.2,2.05723468808047));
#195617=CARTESIAN_POINT('Ctrl Pts',(10.8602339196788,15.2,2.05998757388986));
#195618=CARTESIAN_POINT('Ctrl Pts',(10.8638285993184,15.2,2.06218988289744));
#195619=CARTESIAN_POINT('Ctrl Pts',(10.8674314978142,15.2,2.06440520789794));
#195620=CARTESIAN_POINT('Ctrl Pts',(10.8710424922332,15.2,2.0666335647416));
#195621=CARTESIAN_POINT('Ctrl Pts',(10.8746534866523,15.2,2.06886192158526));
#195622=CARTESIAN_POINT('Ctrl Pts',(10.8782725796639,15.2,2.07110330940823));
#195623=CARTESIAN_POINT('Ctrl Pts',(10.8818996505846,15.2,2.07335774114354));
#195624=CARTESIAN_POINT('Ctrl Pts',(10.8873402564715,15.2,2.07673938843934));
#195625=CARTESIAN_POINT('Ctrl Pts',(10.8927988116549,15.2,2.08015038720294));
#195626=CARTESIAN_POINT('Ctrl Pts',(10.8982749185401,15.2,2.08359078316256));
#195627=CARTESIAN_POINT('Ctrl Pts',(10.9019256562977,15.2,2.0858843803648));
#195628=CARTESIAN_POINT('Ctrl Pts',(10.9055841938399,15.2,2.08819104081164));
#195629=CARTESIAN_POINT('Ctrl Pts',(10.9092504156505,15.2,2.09051078062066));
#195630=CARTESIAN_POINT('Ctrl Pts',(10.9147497491157,15.2,2.0939903908083));
#195631=CARTESIAN_POINT('Ctrl Pts',(10.9202663680979,15.2,2.09749942469599));
#195632=CARTESIAN_POINT('Ctrl Pts',(10.9257998857603,15.2,2.10103792531731));
#195633=CARTESIAN_POINT('Ctrl Pts',(10.9294888970325,15.2,2.10339692541012));
#195634=CARTESIAN_POINT('Ctrl Pts',(10.933185416981,15.2,2.10576902187315));
#195635=CARTESIAN_POINT('Ctrl Pts',(10.9368893309555,15.2,2.1081542257884));
#195636=CARTESIAN_POINT('Ctrl Pts',(10.9405932454347,15.2,2.11053943002863));
#195637=CARTESIAN_POINT('Ctrl Pts',(10.9443045562731,15.2,2.11293774149825));
#195638=CARTESIAN_POINT('Ctrl Pts',(10.9480231465873,15.2,2.11534917296386));
#195639=CARTESIAN_POINT('Ctrl Pts',(10.9526713842268,15.2,2.11836346213159));
#195640=CARTESIAN_POINT('Ctrl Pts',(10.9573309977969,15.2,2.12139824793951));
#195641=CARTESIAN_POINT('Ctrl Pts',(10.9620017658088,15.2,2.12445355337135));
#195642=CARTESIAN_POINT('Ctrl Pts',(10.9666725338207,15.2,2.12750885880319));
#195643=CARTESIAN_POINT('Ctrl Pts',(10.9713544584184,15.2,2.13058468287549));
#195644=CARTESIAN_POINT('Ctrl Pts',(10.9760473178638,15.2,2.13368104711328));
#195645=CARTESIAN_POINT('Ctrl Pts',(10.9798016051131,15.2,2.13615813830101));
#195646=CARTESIAN_POINT('Ctrl Pts',(10.9835628936977,15.2,2.13864837468981));
#195647=CARTESIAN_POINT('Ctrl Pts',(10.9873310690003,15.2,2.14115176459541));
#195648=CARTESIAN_POINT('Ctrl Pts',(10.9901572006056,15.2,2.14302930710988));
#195649=CARTESIAN_POINT('Ctrl Pts',(10.9929872077135,15.2,2.14491424879229));
#195650=CARTESIAN_POINT('Ctrl Pts',(10.9958210420017,15.2,2.14680659440055));
#195651=CARTESIAN_POINT('Ctrl Pts',(10.9986548762898,15.2,2.14869894000881));
#195652=CARTESIAN_POINT('Ctrl Pts',(11.0014925388342,15.2,2.15059868852115));
#195653=CARTESIAN_POINT('Ctrl Pts',(11.0043339838555,15.2,2.15250584453418));
#195654=CARTESIAN_POINT('Ctrl Pts',(11.0071754293929,15.2,2.15441300089368));
#195655=CARTESIAN_POINT('Ctrl Pts',(11.0100206563231,15.2,2.1563275647886));
#195656=CARTESIAN_POINT('Ctrl Pts',(11.0128696193627,15.2,2.15824953865226));
#195657=CARTESIAN_POINT('Ctrl Pts',(11.0166682358861,15.2,2.16081216988856));
#195658=CARTESIAN_POINT('Ctrl Pts',(11.0204734941615,15.2,2.16338797565092));
#195659=CARTESIAN_POINT('Ctrl Pts',(11.024285285405,15.2,2.16597696477174));
#195660=CARTESIAN_POINT('Ctrl Pts',(11.0271441289675,15.2,2.16791870670055));
#195661=CARTESIAN_POINT('Ctrl Pts',(11.0300066474401,15.2,2.16986786306232));
#195662=CARTESIAN_POINT('Ctrl Pts',(11.0328727952288,15.2,2.17182443912979));
#195663=CARTESIAN_POINT('Ctrl Pts',(11.0357389430174,15.2,2.17378101519726));
#195664=CARTESIAN_POINT('Ctrl Pts',(11.0386087216284,15.2,2.17574501082614));
#195665=CARTESIAN_POINT('Ctrl Pts',(11.0414820828569,15.2,2.17771642733684));
#195666=CARTESIAN_POINT('Ctrl Pts',(11.0453132315094,15.2,2.18034498292319));
#195667=CARTESIAN_POINT('Ctrl Pts',(11.049150754771,15.2,2.18298673275803));
#195668=CARTESIAN_POINT('Ctrl Pts',(11.0529945412583,15.2,2.18564168495826));
#195669=CARTESIAN_POINT('Ctrl Pts',(11.0558773808618,15.2,2.18763289892758));
#195670=CARTESIAN_POINT('Ctrl Pts',(11.0587637445903,15.2,2.1896315388716));
#195671=CARTESIAN_POINT('Ctrl Pts',(11.0616535886933,15.2,2.19163760779806));
#195672=CARTESIAN_POINT('Ctrl Pts',(11.0645434327964,15.2,2.19364367672452));
#195673=CARTESIAN_POINT('Ctrl Pts',(11.0674367574171,15.2,2.19565717378234));
#195674=CARTESIAN_POINT('Ctrl Pts',(11.0703335171645,15.2,2.19767810335068));
#195675=CARTESIAN_POINT('Ctrl Pts',(11.0732302769119,15.2,2.19969903291901));
#195676=CARTESIAN_POINT('Ctrl Pts',(11.0761304723229,15.2,2.20172739483113));
#195677=CARTESIAN_POINT('Ctrl Pts',(11.0790340583836,15.2,2.20376319033947));
#195678=CARTESIAN_POINT('Ctrl Pts',(11.0819376449718,15.2,2.20579898621764));
#195679=CARTESIAN_POINT('Ctrl Pts',(11.0848446225943,15.2,2.20784221601461));
#195680=CARTESIAN_POINT('Ctrl Pts',(11.0877549481844,15.2,2.20989288339699));
#195681=CARTESIAN_POINT('Ctrl Pts',(11.0926054901296,15.2,2.2133106618709));
#195682=CARTESIAN_POINT('Ctrl Pts',(11.0974653306805,15.2,2.21674909830068));
#195683=CARTESIAN_POINT('Ctrl Pts',(11.1023342654034,15.2,2.22020820413573));
#195684=CARTESIAN_POINT('Ctrl Pts',(11.1052556261311,15.2,2.22228366756135));
#195685=CARTESIAN_POINT('Ctrl Pts',(11.1081802630752,15.2,2.22436657185321));
#195686=CARTESIAN_POINT('Ctrl Pts',(11.1111081302608,15.2,2.22645691973624));
#195687=CARTESIAN_POINT('Ctrl Pts',(11.1140359974464,15.2,2.22854726761927));
#195688=CARTESIAN_POINT('Ctrl Pts',(11.1169670961792,15.2,2.23064505801875));
#195689=CARTESIAN_POINT('Ctrl Pts',(11.1199013837109,15.2,2.23275029399352));
#195690=CARTESIAN_POINT('Ctrl Pts',(11.1228356712426,15.2,2.23485552996828));
#195691=CARTESIAN_POINT('Ctrl Pts',(11.1257731464074,15.2,2.23696821199878));
#195692=CARTESIAN_POINT('Ctrl Pts',(11.1287137674806,15.2,2.23908834001468));
#195693=CARTESIAN_POINT('Ctrl Pts',(11.1316543885538,15.2,2.24120846803057));
#195694=CARTESIAN_POINT('Ctrl Pts',(11.1345981554694,15.2,2.24333604331223));
#195695=CARTESIAN_POINT('Ctrl Pts',(11.1375450236954,15.2,2.24547106827567));
#195696=CARTESIAN_POINT('Ctrl Pts',(11.1404918919214,15.2,2.24760609323912));
#195697=CARTESIAN_POINT('Ctrl Pts',(11.1434418642139,15.2,2.24974856774373));
#195698=CARTESIAN_POINT('Ctrl Pts',(11.1463948963562,15.2,2.25189849228959));
#195699=CARTESIAN_POINT('Ctrl Pts',(11.1503322729035,15.2,2.25476505861112));
#195700=CARTESIAN_POINT('Ctrl Pts',(11.1542750895084,15.2,2.25764487213383));
#195701=CARTESIAN_POINT('Ctrl Pts',(11.1582232485193,15.2,2.26053793502691));
#195702=CARTESIAN_POINT('Ctrl Pts',(11.1611843675085,15.2,2.26270773199963));
#195703=CARTESIAN_POINT('Ctrl Pts',(11.1641484899249,15.2,2.26488498220077));
#195704=CARTESIAN_POINT('Ctrl Pts',(11.1671155740806,15.2,2.26706968671462));
#195705=CARTESIAN_POINT('Ctrl Pts',(11.1700826582362,15.2,2.26925439122848));
#195706=CARTESIAN_POINT('Ctrl Pts',(11.1730527041842,15.2,2.27144655075754));
#195707=CARTESIAN_POINT('Ctrl Pts',(11.1760256708676,15.2,2.27364616571863));
#195708=CARTESIAN_POINT('Ctrl Pts',(11.178998637551,15.2,2.27584578067973));
#195709=CARTESIAN_POINT('Ctrl Pts',(11.1819745248925,15.2,2.278052851832));
#195710=CARTESIAN_POINT('Ctrl Pts',(11.1849532915756,15.2,2.28026738029217));
#195711=CARTESIAN_POINT('Ctrl Pts',(11.188924980847,15.2,2.28322008517394));
#195712=CARTESIAN_POINT('Ctrl Pts',(11.192901790612,15.2,2.28618604801213));
#195713=CARTESIAN_POINT('Ctrl Pts',(11.196883619736,15.2,2.28916527024364));
#195714=CARTESIAN_POINT('Ctrl Pts',(11.1998699913077,15.2,2.29139968671431));
#195715=CARTESIAN_POINT('Ctrl Pts',(11.2028591860757,15.2,2.29364156281944));
#195716=CARTESIAN_POINT('Ctrl Pts',(11.2058511617305,15.2,2.29589089824789));
#195717=CARTESIAN_POINT('Ctrl Pts',(11.2088431373854,15.2,2.29814023367635));
#195718=CARTESIAN_POINT('Ctrl Pts',(11.2118378943324,15.2,2.30039702865285));
#195719=CARTESIAN_POINT('Ctrl Pts',(11.2148353959316,15.2,2.30266128502826));
#195720=CARTESIAN_POINT('Ctrl Pts',(11.2178328975308,15.2,2.30492554140367));
#195721=CARTESIAN_POINT('Ctrl Pts',(11.2208331426548,15.2,2.30719725782024));
#195722=CARTESIAN_POINT('Ctrl Pts',(11.223836094087,15.2,2.30947643623641));
#195723=CARTESIAN_POINT('Ctrl Pts',(11.2268390460647,15.2,2.31175561506664));
#195724=CARTESIAN_POINT('Ctrl Pts',(11.2298447017849,15.2,2.31404225509897));
#195725=CARTESIAN_POINT('Ctrl Pts',(11.2328530151807,15.2,2.31633635747505));
#195726=CARTESIAN_POINT('Ctrl Pts',(11.2358613280301,15.2,2.31863045943438));
#195727=CARTESIAN_POINT('Ctrl Pts',(11.2388722946416,15.2,2.32093202436442));
#195728=CARTESIAN_POINT('Ctrl Pts',(11.2418858730997,15.2,2.32324105243841));
#195729=CARTESIAN_POINT('Ctrl Pts',(11.2448994515577,15.2,2.32555008051241));
#195730=CARTESIAN_POINT('Ctrl Pts',(11.2479156408273,15.2,2.32786657206639));
#195731=CARTESIAN_POINT('Ctrl Pts',(11.2509344230443,15.2,2.33019052644606));
#195732=CARTESIAN_POINT('Ctrl Pts',(11.2539532052613,15.2,2.33251448082574));
#195733=CARTESIAN_POINT('Ctrl Pts',(11.2569745824506,15.2,2.3348458985751));
#195734=CARTESIAN_POINT('Ctrl Pts',(11.2599985479999,15.2,2.33718477899998));
#195735=CARTESIAN_POINT('Ctrl Pts',(10.2237731089999,12.2,1.76496130799999));
#195736=CARTESIAN_POINT('Ctrl Pts',(10.2255010835344,12.2,1.76541541469069));
#195737=CARTESIAN_POINT('Ctrl Pts',(10.227282994496,12.2,1.76588926687173));
#195738=CARTESIAN_POINT('Ctrl Pts',(10.2291177138156,12.2,1.76638321167919));
#195739=CARTESIAN_POINT('Ctrl Pts',(10.2309612810791,12.2,1.76687953853818));
#195740=CARTESIAN_POINT('Ctrl Pts',(10.2328581800569,12.2,1.76739616235299));
#195741=CARTESIAN_POINT('Ctrl Pts',(10.2348073231802,12.2,1.76793345482698));
#195742=CARTESIAN_POINT('Ctrl Pts',(10.2367564661264,12.2,1.76847074725216));
#195743=CARTESIAN_POINT('Ctrl Pts',(10.2387578528578,12.2,1.76902870390432));
#195744=CARTESIAN_POINT('Ctrl Pts',(10.2408104327832,12.2,1.76960768554995));
#195745=CARTESIAN_POINT('Ctrl Pts',(10.2428630127086,12.2,1.77018666719558));
#195746=CARTESIAN_POINT('Ctrl Pts',(10.2449667829652,12.2,1.77078667349933));
#195747=CARTESIAN_POINT('Ctrl Pts',(10.2471207194916,12.2,1.77140804417322));
#195748=CARTESIAN_POINT('Ctrl Pts',(10.2492746562137,12.2,1.77202941490356));
#195749=CARTESIAN_POINT('Ctrl Pts',(10.251478760386,12.2,1.77267215322635));
#195750=CARTESIAN_POINT('Ctrl Pts',(10.2537320330121,12.2,1.77333658784738));
#195751=CARTESIAN_POINT('Ctrl Pts',(10.256360850769,12.2,1.77411176148137));
#195752=CARTESIAN_POINT('Ctrl Pts',(10.2590565910528,12.2,1.77491646793701));
#195753=CARTESIAN_POINT('Ctrl Pts',(10.261817718071,12.2,1.77575121364745));
#195754=CARTESIAN_POINT('Ctrl Pts',(10.2641843986488,12.2,1.77646671005425));
#195755=CARTESIAN_POINT('Ctrl Pts',(10.2665991148725,12.2,1.77720427386484));
#195756=CARTESIAN_POINT('Ctrl Pts',(10.2690609287599,12.2,1.77796421232445));
#195757=CARTESIAN_POINT('Ctrl Pts',(10.2715227424237,12.2,1.77872415071503));
#195758=CARTESIAN_POINT('Ctrl Pts',(10.2740316523571,12.2,1.77950646297585));
#195759=CARTESIAN_POINT('Ctrl Pts',(10.276586740026,12.2,1.78031144528364));
#195760=CARTESIAN_POINT('Ctrl Pts',(10.2791418276949,12.2,1.78111642759144));
#195761=CARTESIAN_POINT('Ctrl Pts',(10.281743092104,12.2,1.78194408006059));
#195762=CARTESIAN_POINT('Ctrl Pts',(10.2843896398392,12.2,1.78279468544535));
#195763=CARTESIAN_POINT('Ctrl Pts',(10.2870361878147,12.2,1.78364529090738));
#195764=CARTESIAN_POINT('Ctrl Pts',(10.2897280175293,12.2,1.78451885269724));
#195765=CARTESIAN_POINT('Ctrl Pts',(10.2924642530148,12.2,1.78541564208103));
#195766=CARTESIAN_POINT('Ctrl Pts',(10.2952004882518,12.2,1.78631243138337));
#195767=CARTESIAN_POINT('Ctrl Pts',(10.2979811341463,12.2,1.78723245159305));
#195768=CARTESIAN_POINT('Ctrl Pts',(10.300805332129,12.2,1.7881759658098));
#195769=CARTESIAN_POINT('Ctrl Pts',(10.3036295301116,12.2,1.78911948002654));
#195770=CARTESIAN_POINT('Ctrl Pts',(10.3064972817074,12.2,1.79008648852474));
#195771=CARTESIAN_POINT('Ctrl Pts',(10.3094077538498,12.2,1.79107724790438));
#195772=CARTESIAN_POINT('Ctrl Pts',(10.3128033048588,12.2,1.79223313390729));
#195773=CARTESIAN_POINT('Ctrl Pts',(10.3162570022295,12.2,1.79342134934796));
#195774=CARTESIAN_POINT('Ctrl Pts',(10.3197675541057,12.2,1.79464228479875));
#195775=CARTESIAN_POINT('Ctrl Pts',(10.3227765984149,12.2,1.7956888008451));
#195776=CARTESIAN_POINT('Ctrl Pts',(10.3258274147873,12.2,1.79675935622287));
#195777=CARTESIAN_POINT('Ctrl Pts',(10.3289192080899,12.2,1.79785418743204));
#195778=CARTESIAN_POINT('Ctrl Pts',(10.3320110016733,12.2,1.79894901874066));
#195779=CARTESIAN_POINT('Ctrl Pts',(10.3351437736867,12.2,1.80006812807728));
#195780=CARTESIAN_POINT('Ctrl Pts',(10.3383167463624,12.2,1.80121174314127));
#195781=CARTESIAN_POINT('Ctrl Pts',(10.3414897187499,12.2,1.80235535810139));
#195782=CARTESIAN_POINT('Ctrl Pts',(10.3447028933688,12.2,1.80352348028232));
#195783=CARTESIAN_POINT('Ctrl Pts',(10.347955509669,12.2,1.80471633032339));
#195784=CARTESIAN_POINT('Ctrl Pts',(10.3512081259692,12.2,1.80590918036446));
#195785=CARTESIAN_POINT('Ctrl Pts',(10.3545001839163,12.2,1.8071267590119));
#195786=CARTESIAN_POINT('Ctrl Pts',(10.3578309395435,12.2,1.80836927996566));
#195787=CARTESIAN_POINT('Ctrl Pts',(10.3611616951708,12.2,1.80961180091942));
#195788=CARTESIAN_POINT('Ctrl Pts',(10.3645311495549,12.2,1.81087926476607));
#195789=CARTESIAN_POINT('Ctrl Pts',(10.3679385740951,12.2,1.81217187863405));
#195790=CARTESIAN_POINT('Ctrl Pts',(10.3713459989449,12.2,1.81346449261945));
#195791=CARTESIAN_POINT('Ctrl Pts',(10.3747913927401,12.2,1.81478225624894));
#195792=CARTESIAN_POINT('Ctrl Pts',(10.3782740436815,12.2,1.81612537032325));
#195793=CARTESIAN_POINT('Ctrl Pts',(10.3817566943066,12.2,1.81746848427556));
#195794=CARTESIAN_POINT('Ctrl Pts',(10.3852766014031,12.2,1.81883694746036));
#195795=CARTESIAN_POINT('Ctrl Pts',(10.3888330660399,12.2,1.82023095524931));
#195796=CARTESIAN_POINT('Ctrl Pts',(10.3923895306768,12.2,1.82162496303826));
#195797=CARTESIAN_POINT('Ctrl Pts',(10.3959825527803,12.2,1.82304451201334));
#195798=CARTESIAN_POINT('Ctrl Pts',(10.3996114455627,12.2,1.82448979362574));
#195799=CARTESIAN_POINT('Ctrl Pts',(10.4032403386747,12.2,1.82593507536942));
#195800=CARTESIAN_POINT('Ctrl Pts',(10.4069051046527,12.2,1.82740608543694));
#195801=CARTESIAN_POINT('Ctrl Pts',(10.4106050698746,12.2,1.82890300742815));
#195802=CARTESIAN_POINT('Ctrl Pts',(10.4136883740581,12.2,1.83015044235283));
#195803=CARTESIAN_POINT('Ctrl Pts',(10.4167961212353,12.2,1.83141586979413));
#195804=CARTESIAN_POINT('Ctrl Pts',(10.4199279311679,12.2,1.8326993936845));
#195805=CARTESIAN_POINT('Ctrl Pts',(10.4230597411004,12.2,1.83398291757487));
#195806=CARTESIAN_POINT('Ctrl Pts',(10.4262156133916,12.2,1.83528453345442));
#195807=CARTESIAN_POINT('Ctrl Pts',(10.4293951716574,12.2,1.83660434491424));
#195808=CARTESIAN_POINT('Ctrl Pts',(10.4325747295767,12.2,1.8379241562302));
#195809=CARTESIAN_POINT('Ctrl Pts',(10.4357779722426,12.2,1.83926216116631));
#195810=CARTESIAN_POINT('Ctrl Pts',(10.4390045303612,12.2,1.84061845407254));
#195811=CARTESIAN_POINT('Ctrl Pts',(10.4422310888315,12.2,1.8419747471266));
#195812=CARTESIAN_POINT('Ctrl Pts',(10.4454809623459,12.2,1.8433493293748));
#195813=CARTESIAN_POINT('Ctrl Pts',(10.4487537865801,12.2,1.84474229256775));
#195814=CARTESIAN_POINT('Ctrl Pts',(10.4520266108144,12.2,1.84613525576069));
#195815=CARTESIAN_POINT('Ctrl Pts',(10.4553223845839,12.2,1.8475466014861));
#195816=CARTESIAN_POINT('Ctrl Pts',(10.4586407491231,12.2,1.84897641808402));
#195817=CARTESIAN_POINT('Ctrl Pts',(10.4619591136623,12.2,1.85040623468195));
#195818=CARTESIAN_POINT('Ctrl Pts',(10.4653000711479,12.2,1.8518545245162));
#195819=CARTESIAN_POINT('Ctrl Pts',(10.4686632630217,12.2,1.85332137340412));
#195820=CARTESIAN_POINT('Ctrl Pts',(10.4720264548956,12.2,1.85478822229204));
#195821=CARTESIAN_POINT('Ctrl Pts',(10.4754118847616,12.2,1.85627363004155));
#195822=CARTESIAN_POINT('Ctrl Pts',(10.4788192008022,12.2,1.85777768386002));
#195823=CARTESIAN_POINT('Ctrl Pts',(10.4829079799022,12.2,1.85958254837661));
#195824=CARTESIAN_POINT('Ctrl Pts',(10.4870282781004,12.2,1.86141426084172));
#195825=CARTESIAN_POINT('Ctrl Pts',(10.4911795002807,12.2,1.86327296452234));
#195826=CARTESIAN_POINT('Ctrl Pts',(10.4946388522234,12.2,1.86482188431247));
#195827=CARTESIAN_POINT('Ctrl Pts',(10.4981196795769,12.2,1.86638954799397));
#195828=CARTESIAN_POINT('Ctrl Pts',(10.5016216447835,12.2,1.8679760352841));
#195829=CARTESIAN_POINT('Ctrl Pts',(10.5051236099901,12.2,1.86956252257423));
#195830=CARTESIAN_POINT('Ctrl Pts',(10.5086467117074,12.2,1.87116783397052));
#195831=CARTESIAN_POINT('Ctrl Pts',(10.5121906180636,12.2,1.87279204703646));
#195832=CARTESIAN_POINT('Ctrl Pts',(10.5157345244197,12.2,1.87441626010239));
#195833=CARTESIAN_POINT('Ctrl Pts',(10.5192992346944,12.2,1.87605937391457));
#195834=CARTESIAN_POINT('Ctrl Pts',(10.5228844200405,12.2,1.87772146439968));
#195835=CARTESIAN_POINT('Ctrl Pts',(10.5264696053867,12.2,1.8793835548848));
#195836=CARTESIAN_POINT('Ctrl Pts',(10.5300752665139,12.2,1.88106462272875));
#195837=CARTESIAN_POINT('Ctrl Pts',(10.5337010777629,12.2,1.88276473988053));
#195838=CARTESIAN_POINT('Ctrl Pts',(10.5373268890118,12.2,1.88446485703231));
#195839=CARTESIAN_POINT('Ctrl Pts',(10.540972851828,12.2,1.88618402414291));
#195840=CARTESIAN_POINT('Ctrl Pts',(10.5446386447436,12.2,1.88792231212803));
#195841=CARTESIAN_POINT('Ctrl Pts',(10.5483044376593,12.2,1.88966060011315));
#195842=CARTESIAN_POINT('Ctrl Pts',(10.55199006247,12.2,1.89141800835207));
#195843=CARTESIAN_POINT('Ctrl Pts',(10.5556952027645,12.2,1.89319460704064));
#195844=CARTESIAN_POINT('Ctrl Pts',(10.5594003430591,12.2,1.89497120572921));
#195845=CARTESIAN_POINT('Ctrl Pts',(10.5631249964999,12.2,1.89676699353326));
#195846=CARTESIAN_POINT('Ctrl Pts',(10.5668688552499,12.2,1.8985820374916));
#195847=CARTESIAN_POINT('Ctrl Pts',(10.5698639424131,12.2,1.9000340727374));
#195848=CARTESIAN_POINT('Ctrl Pts',(10.5728713198333,12.2,1.90149843387631));
#195849=CARTESIAN_POINT('Ctrl Pts',(10.5758908297769,12.2,1.90297515095805));
#195850=CARTESIAN_POINT('Ctrl Pts',(10.5796652165893,12.2,1.90482104700843));
#195851=CARTESIAN_POINT('Ctrl Pts',(10.5834585619572,12.2,1.90668625184932));
#195852=CARTESIAN_POINT('Ctrl Pts',(10.5872705595263,12.2,1.9085708287951));
#195853=CARTESIAN_POINT('Ctrl Pts',(10.5903201580802,12.2,1.91007849059822));
#195854=CARTESIAN_POINT('Ctrl Pts',(10.5933816942018,12.2,1.9115985502303));
#195855=CARTESIAN_POINT('Ctrl Pts',(10.5964550147582,12.2,1.91313103925827));
#195856=CARTESIAN_POINT('Ctrl Pts',(10.6002966652444,12.2,1.91504665043883));
#195857=CARTESIAN_POINT('Ctrl Pts',(10.604156728901,12.2,1.91698168230319));
#195858=CARTESIAN_POINT('Ctrl Pts',(10.6080349062104,12.2,1.91893619599267));
#195859=CARTESIAN_POINT('Ctrl Pts',(10.6111374478042,12.2,1.92049980681643));
#195860=CARTESIAN_POINT('Ctrl Pts',(10.6142515842205,12.2,1.92207588593802));
#195861=CARTESIAN_POINT('Ctrl Pts',(10.6173771624639,12.2,1.92366446147354));
#195862=CARTESIAN_POINT('Ctrl Pts',(10.620502741133,12.2,1.92525303722551));
#195863=CARTESIAN_POINT('Ctrl Pts',(10.6236397638061,12.2,1.92685411067588));
#195864=CARTESIAN_POINT('Ctrl Pts',(10.6267880791999,12.2,1.9284677110416));
#195865=CARTESIAN_POINT('Ctrl Pts',(10.6299363945937,12.2,1.93008131140732));
#195866=CARTESIAN_POINT('Ctrl Pts',(10.6330960050694,12.2,1.93170743855783));
#195867=CARTESIAN_POINT('Ctrl Pts',(10.6362667610767,12.2,1.93334612025953));
#195868=CARTESIAN_POINT('Ctrl Pts',(10.6402302054377,12.2,1.93539447205175));
#195869=CARTESIAN_POINT('Ctrl Pts',(10.6442110659086,12.2,1.93746244162271));
#195870=CARTESIAN_POINT('Ctrl Pts',(10.6482090562353,12.2,1.93955008097688));
#195871=CARTESIAN_POINT('Ctrl Pts',(10.6514074490196,12.2,1.94122019273328));
#195872=CARTESIAN_POINT('Ctrl Pts',(10.6546168056938,12.2,1.9429028934992));
#195873=CARTESIAN_POINT('Ctrl Pts',(10.6578369822582,12.2,1.94459821175826));
#195874=CARTESIAN_POINT('Ctrl Pts',(10.6610571588226,12.2,1.94629353001733));
#195875=CARTESIAN_POINT('Ctrl Pts',(10.6642881529605,12.2,1.94800146288064));
#195876=CARTESIAN_POINT('Ctrl Pts',(10.6675298243049,12.2,1.94972203853126));
#195877=CARTESIAN_POINT('Ctrl Pts',(10.6707714952077,12.2,1.95144261394744));
#195878=CARTESIAN_POINT('Ctrl Pts',(10.6740238429302,12.2,1.95317583285026));
#195879=CARTESIAN_POINT('Ctrl Pts',(10.677286723956,12.2,1.95492171771542));
#195880=CARTESIAN_POINT('Ctrl Pts',(10.6805496054264,12.2,1.95666760281846));
#195881=CARTESIAN_POINT('Ctrl Pts',(10.6838230218457,12.2,1.95842615545561));
#195882=CARTESIAN_POINT('Ctrl Pts',(10.6871068318035,12.2,1.96019740049788));
#195883=CARTESIAN_POINT('Ctrl Pts',(10.6903906413139,12.2,1.96196864529881));
#195884=CARTESIAN_POINT('Ctrl Pts',(10.6936848439284,12.2,1.96375258195922));
#195885=CARTESIAN_POINT('Ctrl Pts',(10.6969893022132,12.2,1.96554923531151));
#195886=CARTESIAN_POINT('Ctrl Pts',(10.7002937609482,12.2,1.9673458889086));
#195887=CARTESIAN_POINT('Ctrl Pts',(10.7036084731898,12.2,1.96915525855073));
#195888=CARTESIAN_POINT('Ctrl Pts',(10.7069333039824,12.2,1.97097736829774));
#195889=CARTESIAN_POINT('Ctrl Pts',(10.710258134322,12.2,1.97279947779648));
#195890=CARTESIAN_POINT('Ctrl Pts',(10.7135930812368,12.2,1.9746343252259));
#195891=CARTESIAN_POINT('Ctrl Pts',(10.7169380076849,12.2,1.97648193657401));
#195892=CARTESIAN_POINT('Ctrl Pts',(10.7202829345887,12.2,1.97832954817386));
#195893=CARTESIAN_POINT('Ctrl Pts',(10.723637841816,12.2,1.98018992194748));
#195894=CARTESIAN_POINT('Ctrl Pts',(10.7270025945001,12.2,1.98206307966152));
#195895=CARTESIAN_POINT('Ctrl Pts',(10.7303673467257,12.2,1.98393623712034));
#195896=CARTESIAN_POINT('Ctrl Pts',(10.7337419435507,12.2,1.98582218001653));
#195897=CARTESIAN_POINT('Ctrl Pts',(10.7371262507755,12.2,1.98772092823282));
#195898=CARTESIAN_POINT('Ctrl Pts',(10.7422027123046,12.2,1.99056905094533));
#195899=CARTESIAN_POINT('Ctrl Pts',(10.7473010240275,12.2,1.993445988323));
#195900=CARTESIAN_POINT('Ctrl Pts',(10.752420735308,12.2,1.99635180881668));
#195901=CARTESIAN_POINT('Ctrl Pts',(10.7558338756966,12.2,1.99828902221519));
#195902=CARTESIAN_POINT('Ctrl Pts',(10.7592565278284,12.2,2.00023907326201));
#195903=CARTESIAN_POINT('Ctrl Pts',(10.7626885607694,12.2,2.00220198132292));
#195904=CARTESIAN_POINT('Ctrl Pts',(10.7661205941781,12.2,2.00416488965128));
#195905=CARTESIAN_POINT('Ctrl Pts',(10.7695620076061,12.2,2.00614065531861));
#195906=CARTESIAN_POINT('Ctrl Pts',(10.7730126713007,12.2,2.00812929830524));
#195907=CARTESIAN_POINT('Ctrl Pts',(10.7764633345251,12.2,2.01011794102092));
#195908=CARTESIAN_POINT('Ctrl Pts',(10.7799232482395,12.2,2.01211945877313));
#195909=CARTESIAN_POINT('Ctrl Pts',(10.7833922827331,12.2,2.01413387338538));
#195910=CARTESIAN_POINT('Ctrl Pts',(10.7877285762045,12.2,2.01665189185654));
#195911=CARTESIAN_POINT('Ctrl Pts',(10.7920791223375,12.2,2.01919005935047));
#195912=CARTESIAN_POINT('Ctrl Pts',(10.7964436707396,12.2,2.02174841205774));
#195913=CARTESIAN_POINT('Ctrl Pts',(10.7999353096515,12.2,2.0237950943351));
#195914=CARTESIAN_POINT('Ctrl Pts',(10.8034359106256,12.2,2.0258546949168));
#195915=CARTESIAN_POINT('Ctrl Pts',(10.8069453460952,12.2,2.02792723191949));
#195916=CARTESIAN_POINT('Ctrl Pts',(10.8104547810867,12.2,2.0299997686398));
#195917=CARTESIAN_POINT('Ctrl Pts',(10.8139730500538,12.2,2.03208524130502));
#195918=CARTESIAN_POINT('Ctrl Pts',(10.8175000299965,12.2,2.03418366740384));
#195919=CARTESIAN_POINT('Ctrl Pts',(10.8210270104197,12.2,2.03628209378858));
#195920=CARTESIAN_POINT('Ctrl Pts',(10.8245626999794,12.2,2.03839347244877));
#195921=CARTESIAN_POINT('Ctrl Pts',(10.8281069748397,12.2,2.04051782139872));
#195922=CARTESIAN_POINT('Ctrl Pts',(10.8316512492172,12.2,2.04264217005924));
#195923=CARTESIAN_POINT('Ctrl Pts',(10.8352041084096,12.2,2.04477948931438));
#195924=CARTESIAN_POINT('Ctrl Pts',(10.838765429451,12.2,2.04692979391504));
#195925=CARTESIAN_POINT('Ctrl Pts',(10.8423267509775,12.2,2.04908009880867));
#195926=CARTESIAN_POINT('Ctrl Pts',(10.8458965344299,12.2,2.05124338814788));
#195927=CARTESIAN_POINT('Ctrl Pts',(10.8494746567524,12.2,2.05341967977642));
#195928=CARTESIAN_POINT('Ctrl Pts',(10.8530527785872,12.2,2.05559597110844));
#195929=CARTESIAN_POINT('Ctrl Pts',(10.8566392405291,12.2,2.05778526518234));
#195930=CARTESIAN_POINT('Ctrl Pts',(10.8602339196788,12.2,2.05998757388986));
#195931=CARTESIAN_POINT('Ctrl Pts',(10.8638285993184,12.2,2.06218988289744));
#195932=CARTESIAN_POINT('Ctrl Pts',(10.8674314978142,12.2,2.06440520789793));
#195933=CARTESIAN_POINT('Ctrl Pts',(10.8710424922332,12.2,2.06663356474159));
#195934=CARTESIAN_POINT('Ctrl Pts',(10.8746534866523,12.2,2.06886192158525));
#195935=CARTESIAN_POINT('Ctrl Pts',(10.8782725796639,12.2,2.07110330940823));
#195936=CARTESIAN_POINT('Ctrl Pts',(10.8818996505846,12.2,2.07335774114354));
#195937=CARTESIAN_POINT('Ctrl Pts',(10.8873402564715,12.2,2.07673938843934));
#195938=CARTESIAN_POINT('Ctrl Pts',(10.8927988116549,12.2,2.08015038720294));
#195939=CARTESIAN_POINT('Ctrl Pts',(10.8982749185401,12.2,2.08359078316256));
#195940=CARTESIAN_POINT('Ctrl Pts',(10.9019256562977,12.2,2.0858843803648));
#195941=CARTESIAN_POINT('Ctrl Pts',(10.9055841938399,12.2,2.08819104081164));
#195942=CARTESIAN_POINT('Ctrl Pts',(10.9092504156505,12.2,2.09051078062066));
#195943=CARTESIAN_POINT('Ctrl Pts',(10.9129166379606,12.2,2.09283052074575));
#195944=CARTESIAN_POINT('Ctrl Pts',(10.9165905423378,12.2,2.09516333765187));
#195945=CARTESIAN_POINT('Ctrl Pts',(10.9202720152774,12.2,2.09750924523487));
#195946=CARTESIAN_POINT('Ctrl Pts',(10.9239534877154,12.2,2.09985515249824));
#195947=CARTESIAN_POINT('Ctrl Pts',(10.9276425279235,12.2,2.10221414961292));
#195948=CARTESIAN_POINT('Ctrl Pts',(10.9313390191205,12.2,2.1045862488621));
#195949=CARTESIAN_POINT('Ctrl Pts',(10.9350355108212,12.2,2.10695834843448));
#195950=CARTESIAN_POINT('Ctrl Pts',(10.9387394539032,12.2,2.10934354991367));
#195951=CARTESIAN_POINT('Ctrl Pts',(10.9424507355499,12.2,2.11174186426659));
#195952=CARTESIAN_POINT('Ctrl Pts',(10.9461620171966,12.2,2.11414017861952));
#195953=CARTESIAN_POINT('Ctrl Pts',(10.9498806351581,12.2,2.116551607974));
#195954=CARTESIAN_POINT('Ctrl Pts',(10.9536064780841,12.2,2.11897615966302));
#195955=CARTESIAN_POINT('Ctrl Pts',(10.9564008600248,12.2,2.12079457326461));
#195956=CARTESIAN_POINT('Ctrl Pts',(10.9591993051035,12.2,2.12262037017885));
#195957=CARTESIAN_POINT('Ctrl Pts',(10.9620017658088,12.2,2.12445355337135));
#195958=CARTESIAN_POINT('Ctrl Pts',(10.9657383799129,12.2,2.12689779751701));
#195959=CARTESIAN_POINT('Ctrl Pts',(10.9694821348616,12.2,2.12935517419258));
#195960=CARTESIAN_POINT('Ctrl Pts',(10.9732329154434,12.2,2.13182569282309));
#195961=CARTESIAN_POINT('Ctrl Pts',(10.9760460010075,12.2,2.13367858188013));
#195962=CARTESIAN_POINT('Ctrl Pts',(10.9788630393713,12.2,2.13553886474498));
#195963=CARTESIAN_POINT('Ctrl Pts',(10.9816839843933,12.2,2.13740654334279));
#195964=CARTESIAN_POINT('Ctrl Pts',(10.9845049299278,12.2,2.13927422227989));
#195965=CARTESIAN_POINT('Ctrl Pts',(10.9873297811883,12.2,2.14114929818572));
#195966=CARTESIAN_POINT('Ctrl Pts',(10.9901584913082,12.2,2.14303177412699));
#195967=CARTESIAN_POINT('Ctrl Pts',(10.9939301039451,12.2,2.1455417414787));
#195968=CARTESIAN_POINT('Ctrl Pts',(10.9977085772952,12.2,2.14806486740242));
#195969=CARTESIAN_POINT('Ctrl Pts',(11.0014938017807,12.2,2.15060115803988));
#195970=CARTESIAN_POINT('Ctrl Pts',(11.0043327202737,12.2,2.15250337610436));
#195971=CARTESIAN_POINT('Ctrl Pts',(11.0071754363268,12.2,2.15441300099473));
#195972=CARTESIAN_POINT('Ctrl Pts',(11.0100219029314,12.2,2.15633003454943));
#195973=CARTESIAN_POINT('Ctrl Pts',(11.012868369536,12.2,2.15824706810413));
#195974=CARTESIAN_POINT('Ctrl Pts',(11.015718587582,12.2,2.16017151106667));
#195975=CARTESIAN_POINT('Ctrl Pts',(11.0185725111028,12.2,2.16210336707879));
#195976=CARTESIAN_POINT('Ctrl Pts',(11.021426435142,12.2,2.16403522344187));
#195977=CARTESIAN_POINT('Ctrl Pts',(11.0242840643573,12.2,2.16597449334039));
#195978=CARTESIAN_POINT('Ctrl Pts',(11.0271453533987,12.2,2.16792117920765));
#195979=CARTESIAN_POINT('Ctrl Pts',(11.0300066419202,12.2,2.16986786472126));
#195980=CARTESIAN_POINT('Ctrl Pts',(11.0328715893654,12.2,2.17182196655192));
#195981=CARTESIAN_POINT('Ctrl Pts',(11.0357401524883,12.2,2.17378348912119));
#195982=CARTESIAN_POINT('Ctrl Pts',(11.0386087156111,12.2,2.17574501169045));
#195983=CARTESIAN_POINT('Ctrl Pts',(11.0414808920176,12.2,2.17771395390331));
#195984=CARTESIAN_POINT('Ctrl Pts',(11.0443566385384,12.2,2.17969031845715));
#195985=CARTESIAN_POINT('Ctrl Pts',(11.0472323850593,12.2,2.18166668301098));
#195986=CARTESIAN_POINT('Ctrl Pts',(11.0501117016547,12.2,2.18365047098895));
#195987=CARTESIAN_POINT('Ctrl Pts',(11.0529945412583,12.2,2.18564168495826));
#195988=CARTESIAN_POINT('Ctrl Pts',(11.0558773808618,12.2,2.18763289892758));
#195989=CARTESIAN_POINT('Ctrl Pts',(11.0587637445903,12.2,2.1896315388716));
#195990=CARTESIAN_POINT('Ctrl Pts',(11.0616535886933,12.2,2.19163760779806));
#195991=CARTESIAN_POINT('Ctrl Pts',(11.0645434327964,12.2,2.19364367672452));
#195992=CARTESIAN_POINT('Ctrl Pts',(11.0674367574171,12.2,2.19565717378234));
#195993=CARTESIAN_POINT('Ctrl Pts',(11.0703335171645,12.2,2.19767810335068));
#195994=CARTESIAN_POINT('Ctrl Pts',(11.0732302769119,12.2,2.19969903291901));
#195995=CARTESIAN_POINT('Ctrl Pts',(11.0761304723229,12.2,2.20172739483113));
#195996=CARTESIAN_POINT('Ctrl Pts',(11.0790340583836,12.2,2.20376319033947));
#195997=CARTESIAN_POINT('Ctrl Pts',(11.0819376449718,12.2,2.20579898621764));
#195998=CARTESIAN_POINT('Ctrl Pts',(11.0848446225943,12.2,2.20784221601461));
#195999=CARTESIAN_POINT('Ctrl Pts',(11.0877549481844,12.2,2.20989288339698));
#196000=CARTESIAN_POINT('Ctrl Pts',(11.0916353814233,12.2,2.21262710595259));
#196001=CARTESIAN_POINT('Ctrl Pts',(11.0955217660643,12.2,2.21537455062593));
#196002=CARTESIAN_POINT('Ctrl Pts',(11.0994139966901,12.2,2.21813522056604));
#196003=CARTESIAN_POINT('Ctrl Pts',(11.1023331697921,12.2,2.22020572311515));
#196004=CARTESIAN_POINT('Ctrl Pts',(11.1052556321355,12.2,2.22228366670545));
#196005=CARTESIAN_POINT('Ctrl Pts',(11.1081813406955,12.2,2.22436905225366));
#196006=CARTESIAN_POINT('Ctrl Pts',(11.1111070497869,12.2,2.22645443818071));
#196007=CARTESIAN_POINT('Ctrl Pts',(11.1140360041792,12.2,2.22854726731821));
#196008=CARTESIAN_POINT('Ctrl Pts',(11.1169681613975,12.2,2.2306475402078));
#196009=CARTESIAN_POINT('Ctrl Pts',(11.119900318083,12.2,2.23274781271583));
#196010=CARTESIAN_POINT('Ctrl Pts',(11.1228356784281,12.2,2.23485553037956));
#196011=CARTESIAN_POINT('Ctrl Pts',(11.1257741973018,12.2,2.23697069440924));
#196012=CARTESIAN_POINT('Ctrl Pts',(11.1296922222889,12.2,2.2397909129874));
#196013=CARTESIAN_POINT('Ctrl Pts',(11.1336158662392,12.2,2.2426243684537));
#196014=CARTESIAN_POINT('Ctrl Pts',(11.1375450236954,12.2,2.24547106827567));
#196015=CARTESIAN_POINT('Ctrl Pts',(11.1404918919214,12.2,2.24760609323912));
#196016=CARTESIAN_POINT('Ctrl Pts',(11.1434418642139,12.2,2.24974856774373));
#196017=CARTESIAN_POINT('Ctrl Pts',(11.1463948963562,12.2,2.25189849228959));
#196018=CARTESIAN_POINT('Ctrl Pts',(11.1493479290349,12.2,2.25404841722602));
#196019=CARTESIAN_POINT('Ctrl Pts',(11.1523040214645,12.2,2.25620579383957));
#196020=CARTESIAN_POINT('Ctrl Pts',(11.1552631331034,12.2,2.25837062269688));
#196021=CARTESIAN_POINT('Ctrl Pts',(11.1582222442046,12.2,2.26053545116091));
#196022=CARTESIAN_POINT('Ctrl Pts',(11.1611843737996,12.2,2.26270773239117));
#196023=CARTESIAN_POINT('Ctrl Pts',(11.164149479007,12.2,2.2648874674634));
#196024=CARTESIAN_POINT('Ctrl Pts',(11.1671145842144,12.2,2.26706720253563));
#196025=CARTESIAN_POINT('Ctrl Pts',(11.1700826647982,12.2,2.26925439201835));
#196026=CARTESIAN_POINT('Ctrl Pts',(11.1730536798988,12.2,2.27144903652261));
#196027=CARTESIAN_POINT('Ctrl Pts',(11.1760246949995,12.2,2.27364368102686));
#196028=CARTESIAN_POINT('Ctrl Pts',(11.1789986447914,12.2,2.27584578101355));
#196029=CARTESIAN_POINT('Ctrl Pts',(11.1819754870166,12.2,2.27805533797493));
#196030=CARTESIAN_POINT('Ctrl Pts',(11.1849523292418,12.2,2.28026489493631));
#196031=CARTESIAN_POINT('Ctrl Pts',(11.1879320656002,12.2,2.28248190915573));
#196032=CARTESIAN_POINT('Ctrl Pts',(11.1909146536999,12.2,2.28470638153259));
#196033=CARTESIAN_POINT('Ctrl Pts',(11.1938972417996,12.2,2.28693085390945));
#196034=CARTESIAN_POINT('Ctrl Pts',(11.1968826812314,12.2,2.28916278328709));
#196035=CARTESIAN_POINT('Ctrl Pts',(11.1998709304385,12.2,2.29140217281674));
#196036=CARTESIAN_POINT('Ctrl Pts',(11.2028591796455,12.2,2.29364156234638));
#196037=CARTESIAN_POINT('Ctrl Pts',(11.2058502369064,12.2,2.29588841127475));
#196038=CARTESIAN_POINT('Ctrl Pts',(11.2088440626306,12.2,2.29814271977517));
#196039=CARTESIAN_POINT('Ctrl Pts',(11.2118378888987,12.2,2.30039702868511));
#196040=CARTESIAN_POINT('Ctrl Pts',(11.2148344848675,12.2,2.30265879861382));
#196041=CARTESIAN_POINT('Ctrl Pts',(11.2178338116788,12.2,2.3049280289863));
#196042=CARTESIAN_POINT('Ctrl Pts',(11.2208331379452,12.2,2.30719725894655));
#196043=CARTESIAN_POINT('Ctrl Pts',(11.2238351975198,12.2,2.30947394988138));
#196044=CARTESIAN_POINT('Ctrl Pts',(11.2268399461192,12.2,2.31175810275736));
#196045=CARTESIAN_POINT('Ctrl Pts',(11.2298446947185,12.2,2.31404225563335));
#196046=CARTESIAN_POINT('Ctrl Pts',(11.2328521331984,12.2,2.31633386937509));
#196047=CARTESIAN_POINT('Ctrl Pts',(11.2358622107693,12.2,2.31863294676036));
#196048=CARTESIAN_POINT('Ctrl Pts',(11.2398756473484,12.2,2.32169838313483));
#196049=CARTESIAN_POINT('Ctrl Pts',(11.2438937704077,12.2,2.32477708723464));
#196050=CARTESIAN_POINT('Ctrl Pts',(11.2479165051339,12.2,2.32786905903606));
#196051=CARTESIAN_POINT('Ctrl Pts',(11.2519392404082,12.2,2.33096103125876));
#196052=CARTESIAN_POINT('Ctrl Pts',(11.2559665935679,12.2,2.33406627148354));
#196053=CARTESIAN_POINT('Ctrl Pts',(11.2599985479999,12.2,2.33718477899998));
#196054=CARTESIAN_POINT('Ctrl Pts',(11.1757778679999,15.2,2.71145515299998));
#196055=CARTESIAN_POINT('Ctrl Pts',(11.1757778679999,11.6,2.71145515299998));
#196056=CARTESIAN_POINT('Ctrl Pts',(11.1750309949999,15.2,2.71161876799999));
#196057=CARTESIAN_POINT('Ctrl Pts',(11.1750309949999,11.6,2.71161876799999));
#196058=CARTESIAN_POINT('Ctrl Pts',(11.1735376169999,15.2,2.71194562399998));
#196059=CARTESIAN_POINT('Ctrl Pts',(11.1735376169999,11.6,2.71194562399998));
#196060=CARTESIAN_POINT('Ctrl Pts',(11.1712986599999,15.2,2.71243477999998));
#196061=CARTESIAN_POINT('Ctrl Pts',(11.1712986599999,11.6,2.71243477999998));
#196062=CARTESIAN_POINT('Ctrl Pts',(11.1683155989999,15.2,2.71308473599999));
#196063=CARTESIAN_POINT('Ctrl Pts',(11.1683155989999,11.6,2.71308473599999));
#196064=CARTESIAN_POINT('Ctrl Pts',(11.1645904639999,15.2,2.71389342499998));
#196065=CARTESIAN_POINT('Ctrl Pts',(11.1645904639999,11.6,2.71389342499998));
#196066=CARTESIAN_POINT('Ctrl Pts',(11.1608690239999,15.2,2.71469835899998));
#196067=CARTESIAN_POINT('Ctrl Pts',(11.1608690239999,11.6,2.71469835899998));
#196068=CARTESIAN_POINT('Ctrl Pts',(11.1571512799999,15.2,2.71549953899999));
#196069=CARTESIAN_POINT('Ctrl Pts',(11.1571512799999,11.6,2.71549953899999));
#196070=CARTESIAN_POINT('Ctrl Pts',(11.1534372359999,15.2,2.71629696699998));
#196071=CARTESIAN_POINT('Ctrl Pts',(11.1534372359999,11.6,2.71629696699998));
#196072=CARTESIAN_POINT('Ctrl Pts',(11.1497268969999,15.2,2.71709064499999));
#196073=CARTESIAN_POINT('Ctrl Pts',(11.1497268969999,11.6,2.71709064499999));
#196074=CARTESIAN_POINT('Ctrl Pts',(11.1460202709999,15.2,2.71788057599998));
#196075=CARTESIAN_POINT('Ctrl Pts',(11.1460202709999,11.6,2.71788057599998));
#196076=CARTESIAN_POINT('Ctrl Pts',(11.1423173659999,15.2,2.71866676499998));
#196077=CARTESIAN_POINT('Ctrl Pts',(11.1423173659999,11.6,2.71866676499998));
#196078=CARTESIAN_POINT('Ctrl Pts',(11.1386181909999,15.2,2.71944921899999));
#196079=CARTESIAN_POINT('Ctrl Pts',(11.1386181909999,11.6,2.71944921899998));
#196080=CARTESIAN_POINT('Ctrl Pts',(11.1349227589999,15.2,2.72022793899998));
#196081=CARTESIAN_POINT('Ctrl Pts',(11.1349227589999,11.6,2.72022793899998));
#196082=CARTESIAN_POINT('Ctrl Pts',(11.1312310749999,15.2,2.72100293299999));
#196083=CARTESIAN_POINT('Ctrl Pts',(11.1312310749999,11.6,2.72100293299999));
#196084=CARTESIAN_POINT('Ctrl Pts',(11.1275431529999,15.2,2.72177420499998));
#196085=CARTESIAN_POINT('Ctrl Pts',(11.1275431529999,11.6,2.72177420499998));
#196086=CARTESIAN_POINT('Ctrl Pts',(11.1238589999999,15.2,2.72254175699998));
#196087=CARTESIAN_POINT('Ctrl Pts',(11.1238589999999,11.6,2.72254175699998));
#196088=CARTESIAN_POINT('Ctrl Pts',(11.1201786229999,15.2,2.72330559599999));
#196089=CARTESIAN_POINT('Ctrl Pts',(11.1201786229999,11.6,2.72330559599998));
#196090=CARTESIAN_POINT('Ctrl Pts',(11.1165020289999,15.2,2.72406572399999));
#196091=CARTESIAN_POINT('Ctrl Pts',(11.1165020289999,11.6,2.72406572399999));
#196092=CARTESIAN_POINT('Ctrl Pts',(11.1128292269999,15.2,2.72482214499998));
#196093=CARTESIAN_POINT('Ctrl Pts',(11.1128292269999,11.6,2.72482214499998));
#196094=CARTESIAN_POINT('Ctrl Pts',(11.1091602219999,15.2,2.72557486299998));
#196095=CARTESIAN_POINT('Ctrl Pts',(11.1091602219999,11.6,2.72557486299998));
#196096=CARTESIAN_POINT('Ctrl Pts',(11.1054950239999,15.2,2.72632388099999));
#196097=CARTESIAN_POINT('Ctrl Pts',(11.1054950239999,11.6,2.72632388099999));
#196098=CARTESIAN_POINT('Ctrl Pts',(11.1018336399999,15.2,2.72706920299999));
#196099=CARTESIAN_POINT('Ctrl Pts',(11.1018336399999,11.6,2.72706920299999));
#196100=CARTESIAN_POINT('Ctrl Pts',(11.0981760779999,15.2,2.72781083499999));
#196101=CARTESIAN_POINT('Ctrl Pts',(11.0981760779999,11.6,2.72781083499999));
#196102=CARTESIAN_POINT('Ctrl Pts',(11.0945223469999,15.2,2.72854877899999));
#196103=CARTESIAN_POINT('Ctrl Pts',(11.0945223469999,11.6,2.72854877899999));
#196104=CARTESIAN_POINT('Ctrl Pts',(11.0908724549999,15.2,2.72928304099998));
#196105=CARTESIAN_POINT('Ctrl Pts',(11.0908724549999,11.6,2.72928304099998));
#196106=CARTESIAN_POINT('Ctrl Pts',(11.0872264109999,15.2,2.73001362299999));
#196107=CARTESIAN_POINT('Ctrl Pts',(11.0872264109999,11.6,2.73001362299999));
#196108=CARTESIAN_POINT('Ctrl Pts',(11.0835842229999,15.2,2.73074053299998));
#196109=CARTESIAN_POINT('Ctrl Pts',(11.0835842229999,11.6,2.73074053299998));
#196110=CARTESIAN_POINT('Ctrl Pts',(11.0799458989999,15.2,2.73146377099999));
#196111=CARTESIAN_POINT('Ctrl Pts',(11.0799458989999,11.6,2.73146377099999));
#196112=CARTESIAN_POINT('Ctrl Pts',(11.0763114489999,15.2,2.73218334499998));
#196113=CARTESIAN_POINT('Ctrl Pts',(11.0763114489999,11.6,2.73218334499998));
#196114=CARTESIAN_POINT('Ctrl Pts',(11.0726808779999,15.2,2.73289925699999));
#196115=CARTESIAN_POINT('Ctrl Pts',(11.0726808779999,11.6,2.73289925699999));
#196116=CARTESIAN_POINT('Ctrl Pts',(11.0690541959999,15.2,2.73361151099999));
#196117=CARTESIAN_POINT('Ctrl Pts',(11.0690541959999,11.6,2.73361151099999));
#196118=CARTESIAN_POINT('Ctrl Pts',(11.0654314099999,15.2,2.73432011199999));
#196119=CARTESIAN_POINT('Ctrl Pts',(11.0654314099999,11.6,2.73432011199999));
#196120=CARTESIAN_POINT('Ctrl Pts',(11.0618125299999,15.2,2.73502506399999));
#196121=CARTESIAN_POINT('Ctrl Pts',(11.0618125299999,11.6,2.73502506399998));
#196122=CARTESIAN_POINT('Ctrl Pts',(11.0581975619999,15.2,2.73572636999998));
#196123=CARTESIAN_POINT('Ctrl Pts',(11.0581975619999,11.6,2.73572636999998));
#196124=CARTESIAN_POINT('Ctrl Pts',(11.0545865169999,15.2,2.73642403699998));
#196125=CARTESIAN_POINT('Ctrl Pts',(11.0545865169999,11.6,2.73642403699998));
#196126=CARTESIAN_POINT('Ctrl Pts',(11.0509794009999,15.2,2.73711806699998));
#196127=CARTESIAN_POINT('Ctrl Pts',(11.0509794009999,11.6,2.73711806699998));
#196128=CARTESIAN_POINT('Ctrl Pts',(11.0473762219999,15.2,2.73780846599998));
#196129=CARTESIAN_POINT('Ctrl Pts',(11.0473762219999,11.6,2.73780846599998));
#196130=CARTESIAN_POINT('Ctrl Pts',(11.0437769909999,15.2,2.73849523599999));
#196131=CARTESIAN_POINT('Ctrl Pts',(11.0437769909999,11.6,2.73849523599999));
#196132=CARTESIAN_POINT('Ctrl Pts',(11.0401817149999,15.2,2.73917838399999));
#196133=CARTESIAN_POINT('Ctrl Pts',(11.0401817149999,11.6,2.73917838399999));
#196134=CARTESIAN_POINT('Ctrl Pts',(11.0365903999999,15.2,2.73985791299998));
#196135=CARTESIAN_POINT('Ctrl Pts',(11.0365903999999,11.6,2.73985791299998));
#196136=CARTESIAN_POINT('Ctrl Pts',(11.0330030589999,15.2,2.74053382799998));
#196137=CARTESIAN_POINT('Ctrl Pts',(11.0330030589999,11.6,2.74053382799998));
#196138=CARTESIAN_POINT('Ctrl Pts',(11.0294196959999,15.2,2.74120613199998));
#196139=CARTESIAN_POINT('Ctrl Pts',(11.0294196959999,11.6,2.74120613199998));
#196140=CARTESIAN_POINT('Ctrl Pts',(11.0258403219999,15.2,2.74187483099999));
#196141=CARTESIAN_POINT('Ctrl Pts',(11.0258403219999,11.6,2.74187483099999));
#196142=CARTESIAN_POINT('Ctrl Pts',(11.0222649439999,15.2,2.74253992799999));
#196143=CARTESIAN_POINT('Ctrl Pts',(11.0222649439999,11.6,2.74253992799998));
#196144=CARTESIAN_POINT('Ctrl Pts',(11.0186935709999,15.2,2.74320142899998));
#196145=CARTESIAN_POINT('Ctrl Pts',(11.0186935709999,11.6,2.74320142899998));
#196146=CARTESIAN_POINT('Ctrl Pts',(11.0151262099999,15.2,2.74385933599999));
#196147=CARTESIAN_POINT('Ctrl Pts',(11.0151262099999,11.6,2.74385933599999));
#196148=CARTESIAN_POINT('Ctrl Pts',(11.0115628719999,15.2,2.74451365599998));
#196149=CARTESIAN_POINT('Ctrl Pts',(11.0115628719999,11.6,2.74451365599998));
#196150=CARTESIAN_POINT('Ctrl Pts',(11.0080035629999,15.2,2.74516439199999));
#196151=CARTESIAN_POINT('Ctrl Pts',(11.0080035629999,11.6,2.74516439199999));
#196152=CARTESIAN_POINT('Ctrl Pts',(11.0044482939999,15.2,2.74581154899998));
#196153=CARTESIAN_POINT('Ctrl Pts',(11.0044482939999,11.6,2.74581154899998));
#196154=CARTESIAN_POINT('Ctrl Pts',(11.0008970699999,15.2,2.74645513199999));
#196155=CARTESIAN_POINT('Ctrl Pts',(11.0008970699999,11.6,2.74645513199999));
#196156=CARTESIAN_POINT('Ctrl Pts',(10.9973499019999,15.2,2.74709514499998));
#196157=CARTESIAN_POINT('Ctrl Pts',(10.9973499019999,11.6,2.74709514499998));
#196158=CARTESIAN_POINT('Ctrl Pts',(10.9938067979999,15.2,2.74773159199999));
#196159=CARTESIAN_POINT('Ctrl Pts',(10.9938067979999,11.6,2.74773159199999));
#196160=CARTESIAN_POINT('Ctrl Pts',(10.9902677649999,15.2,2.74836447799998));
#196161=CARTESIAN_POINT('Ctrl Pts',(10.9902677649999,11.6,2.74836447799998));
#196162=CARTESIAN_POINT('Ctrl Pts',(10.9867328139999,15.2,2.74899380799998));
#196163=CARTESIAN_POINT('Ctrl Pts',(10.9867328139999,11.6,2.74899380799998));
#196164=CARTESIAN_POINT('Ctrl Pts',(10.9832019509999,15.2,2.74961958599999));
#196165=CARTESIAN_POINT('Ctrl Pts',(10.9832019509999,11.6,2.74961958599999));
#196166=CARTESIAN_POINT('Ctrl Pts',(10.9796751869999,15.2,2.75024181699998));
#196167=CARTESIAN_POINT('Ctrl Pts',(10.9796751869999,11.6,2.75024181699998));
#196168=CARTESIAN_POINT('Ctrl Pts',(10.9761525279999,15.2,2.75086050399998));
#196169=CARTESIAN_POINT('Ctrl Pts',(10.9761525279999,11.6,2.75086050399998));
#196170=CARTESIAN_POINT('Ctrl Pts',(10.9726339839999,15.2,2.75147565399998));
#196171=CARTESIAN_POINT('Ctrl Pts',(10.9726339839999,11.6,2.75147565399998));
#196172=CARTESIAN_POINT('Ctrl Pts',(10.9691195629999,15.2,2.75208726999999));
#196173=CARTESIAN_POINT('Ctrl Pts',(10.9691195629999,11.6,2.75208726999998));
#196174=CARTESIAN_POINT('Ctrl Pts',(10.9656092739999,15.2,2.75269535799998));
#196175=CARTESIAN_POINT('Ctrl Pts',(10.9656092739999,11.6,2.75269535799998));
#196176=CARTESIAN_POINT('Ctrl Pts',(10.9621031259999,15.2,2.75329992099999));
#196177=CARTESIAN_POINT('Ctrl Pts',(10.9621031259999,11.6,2.75329992099999));
#196178=CARTESIAN_POINT('Ctrl Pts',(10.9586011259999,15.2,2.75390096599998));
#196179=CARTESIAN_POINT('Ctrl Pts',(10.9586011259999,11.6,2.75390096599998));
#196180=CARTESIAN_POINT('Ctrl Pts',(10.9551032829999,15.2,2.75449849499999));
#196181=CARTESIAN_POINT('Ctrl Pts',(10.9551032829999,11.6,2.75449849499999));
#196182=CARTESIAN_POINT('Ctrl Pts',(10.9516096059999,15.2,2.75509251399999));
#196183=CARTESIAN_POINT('Ctrl Pts',(10.9516096059999,11.6,2.75509251399999));
#196184=CARTESIAN_POINT('Ctrl Pts',(10.9481201049999,15.2,2.75568302799999));
#196185=CARTESIAN_POINT('Ctrl Pts',(10.9481201049999,11.6,2.75568302799999));
#196186=CARTESIAN_POINT('Ctrl Pts',(10.9446347859999,15.2,2.75627004099999));
#196187=CARTESIAN_POINT('Ctrl Pts',(10.9446347859999,11.6,2.75627004099999));
#196188=CARTESIAN_POINT('Ctrl Pts',(10.9411536579999,15.2,2.75685355899999));
#196189=CARTESIAN_POINT('Ctrl Pts',(10.9411536579999,11.6,2.75685355899998));
#196190=CARTESIAN_POINT('Ctrl Pts',(10.9376767319999,15.2,2.75743358499999));
#196191=CARTESIAN_POINT('Ctrl Pts',(10.9376767319999,11.6,2.75743358499999));
#196192=CARTESIAN_POINT('Ctrl Pts',(10.9342040149999,15.2,2.75801012499999));
#196193=CARTESIAN_POINT('Ctrl Pts',(10.9342040149999,11.6,2.75801012499999));
#196194=CARTESIAN_POINT('Ctrl Pts',(10.9307355149999,15.2,2.75858318399998));
#196195=CARTESIAN_POINT('Ctrl Pts',(10.9307355149999,11.6,2.75858318399998));
#196196=CARTESIAN_POINT('Ctrl Pts',(10.9272712419999,15.2,2.75915276599999));
#196197=CARTESIAN_POINT('Ctrl Pts',(10.9272712419999,11.6,2.75915276599999));
#196198=CARTESIAN_POINT('Ctrl Pts',(10.9238112039999,15.2,2.75971887599999));
#196199=CARTESIAN_POINT('Ctrl Pts',(10.9238112039999,11.6,2.75971887599999));
#196200=CARTESIAN_POINT('Ctrl Pts',(10.9203554099999,15.2,2.76028151899999));
#196201=CARTESIAN_POINT('Ctrl Pts',(10.9203554099999,11.6,2.76028151899998));
#196202=CARTESIAN_POINT('Ctrl Pts',(10.9169038679999,15.2,2.76084069999998));
#196203=CARTESIAN_POINT('Ctrl Pts',(10.9169038679999,11.6,2.76084069999998));
#196204=CARTESIAN_POINT('Ctrl Pts',(10.9134565879999,15.2,2.76139642399999));
#196205=CARTESIAN_POINT('Ctrl Pts',(10.9134565879999,11.6,2.76139642399999));
#196206=CARTESIAN_POINT('Ctrl Pts',(10.9100135769999,15.2,2.76194869599999));
#196207=CARTESIAN_POINT('Ctrl Pts',(10.9100135769999,11.6,2.76194869599998));
#196208=CARTESIAN_POINT('Ctrl Pts',(10.9065748449999,15.2,2.76249751999998));
#196209=CARTESIAN_POINT('Ctrl Pts',(10.9065748449999,11.6,2.76249751999998));
#196210=CARTESIAN_POINT('Ctrl Pts',(10.9031404009999,15.2,2.76304290199998));
#196211=CARTESIAN_POINT('Ctrl Pts',(10.9031404009999,11.6,2.76304290199998));
#196212=CARTESIAN_POINT('Ctrl Pts',(10.8997102529999,15.2,2.76358484599999));
#196213=CARTESIAN_POINT('Ctrl Pts',(10.8997102529999,11.6,2.76358484599999));
#196214=CARTESIAN_POINT('Ctrl Pts',(10.8962844109999,15.2,2.76412335799999));
#196215=CARTESIAN_POINT('Ctrl Pts',(10.8962844109999,11.6,2.76412335799999));
#196216=CARTESIAN_POINT('Ctrl Pts',(10.8928628809999,15.2,2.76465844099998));
#196217=CARTESIAN_POINT('Ctrl Pts',(10.8928628809999,11.6,2.76465844099998));
#196218=CARTESIAN_POINT('Ctrl Pts',(10.8894456749999,15.2,2.76519010299998));
#196219=CARTESIAN_POINT('Ctrl Pts',(10.8894456749999,11.6,2.76519010299998));
#196220=CARTESIAN_POINT('Ctrl Pts',(10.8860327999999,15.2,2.76571834699999));
#196221=CARTESIAN_POINT('Ctrl Pts',(10.8860327999999,11.6,2.76571834699999));
#196222=CARTESIAN_POINT('Ctrl Pts',(10.8826242649999,15.2,2.76624317899999));
#196223=CARTESIAN_POINT('Ctrl Pts',(10.8826242649999,11.6,2.76624317899999));
#196224=CARTESIAN_POINT('Ctrl Pts',(10.8792200789999,15.2,2.76676460199998));
#196225=CARTESIAN_POINT('Ctrl Pts',(10.8792200789999,11.6,2.76676460199998));
#196226=CARTESIAN_POINT('Ctrl Pts',(10.8758202519999,15.2,2.76728262299999));
#196227=CARTESIAN_POINT('Ctrl Pts',(10.8758202519999,11.6,2.76728262299999));
#196228=CARTESIAN_POINT('Ctrl Pts',(10.8724247909999,15.2,2.76779724699999));
#196229=CARTESIAN_POINT('Ctrl Pts',(10.8724247909999,11.6,2.76779724699999));
#196230=CARTESIAN_POINT('Ctrl Pts',(10.8690337059999,15.2,2.76830847799998));
#196231=CARTESIAN_POINT('Ctrl Pts',(10.8690337059999,11.6,2.76830847799998));
#196232=CARTESIAN_POINT('Ctrl Pts',(10.8656470049999,15.2,2.76881632399999));
#196233=CARTESIAN_POINT('Ctrl Pts',(10.8656470049999,11.6,2.76881632399998));
#196234=CARTESIAN_POINT('Ctrl Pts',(10.8622646979999,15.2,2.76932078499998));
#196235=CARTESIAN_POINT('Ctrl Pts',(10.8622646979999,11.6,2.76932078499998));
#196236=CARTESIAN_POINT('Ctrl Pts',(10.8588867929999,15.2,2.76982187099998));
#196237=CARTESIAN_POINT('Ctrl Pts',(10.8588867929999,11.6,2.76982187099998));
#196238=CARTESIAN_POINT('Ctrl Pts',(10.8555133009999,15.2,2.77031958499999));
#196239=CARTESIAN_POINT('Ctrl Pts',(10.8555133009999,11.6,2.77031958499998));
#196240=CARTESIAN_POINT('Ctrl Pts',(10.8521442279999,15.2,2.77081393199998));
#196241=CARTESIAN_POINT('Ctrl Pts',(10.8521442279999,11.6,2.77081393199998));
#196242=CARTESIAN_POINT('Ctrl Pts',(10.8487795839999,15.2,2.77130491799999));
#196243=CARTESIAN_POINT('Ctrl Pts',(10.8487795839999,11.6,2.77130491799999));
#196244=CARTESIAN_POINT('Ctrl Pts',(10.8454193789999,15.2,2.77179254799999));
#196245=CARTESIAN_POINT('Ctrl Pts',(10.8454193789999,11.6,2.77179254799999));
#196246=CARTESIAN_POINT('Ctrl Pts',(10.8420636209999,15.2,2.77227682699999));
#196247=CARTESIAN_POINT('Ctrl Pts',(10.8420636209999,11.6,2.77227682699999));
#196248=CARTESIAN_POINT('Ctrl Pts',(10.8387123189999,15.2,2.77275775999998));
#196249=CARTESIAN_POINT('Ctrl Pts',(10.8387123189999,11.6,2.77275775999998));
#196250=CARTESIAN_POINT('Ctrl Pts',(10.8353654819999,15.2,2.77323535299999));
#196251=CARTESIAN_POINT('Ctrl Pts',(10.8353654819999,11.6,2.77323535299998));
#196252=CARTESIAN_POINT('Ctrl Pts',(10.8320231199999,15.2,2.77370960999999));
#196253=CARTESIAN_POINT('Ctrl Pts',(10.8320231199999,11.6,2.77370960999999));
#196254=CARTESIAN_POINT('Ctrl Pts',(10.8286852409999,15.2,2.77418053799998));
#196255=CARTESIAN_POINT('Ctrl Pts',(10.8286852409999,11.6,2.77418053799998));
#196256=CARTESIAN_POINT('Ctrl Pts',(10.8253518549999,15.2,2.77464814099999));
#196257=CARTESIAN_POINT('Ctrl Pts',(10.8253518549999,11.6,2.77464814099999));
#196258=CARTESIAN_POINT('Ctrl Pts',(10.8220229679999,15.2,2.77511242599999));
#196259=CARTESIAN_POINT('Ctrl Pts',(10.8220229679999,11.6,2.77511242599999));
#196260=CARTESIAN_POINT('Ctrl Pts',(10.8186985939999,15.2,2.77557339599999));
#196261=CARTESIAN_POINT('Ctrl Pts',(10.8186985939999,11.6,2.77557339599999));
#196262=CARTESIAN_POINT('Ctrl Pts',(10.8153787389999,15.2,2.77603105699999));
#196263=CARTESIAN_POINT('Ctrl Pts',(10.8153787389999,11.6,2.77603105699999));
#196264=CARTESIAN_POINT('Ctrl Pts',(10.8120634119999,15.2,2.77648541599999));
#196265=CARTESIAN_POINT('Ctrl Pts',(10.8120634119999,11.6,2.77648541599999));
#196266=CARTESIAN_POINT('Ctrl Pts',(10.8087526239999,15.2,2.77693647799998));
#196267=CARTESIAN_POINT('Ctrl Pts',(10.8087526239999,11.6,2.77693647799998));
#196268=CARTESIAN_POINT('Ctrl Pts',(10.8054463819999,15.2,2.77738424699999));
#196269=CARTESIAN_POINT('Ctrl Pts',(10.8054463819999,11.6,2.77738424699999));
#196270=CARTESIAN_POINT('Ctrl Pts',(10.8021446959999,15.2,2.77782872899999));
#196271=CARTESIAN_POINT('Ctrl Pts',(10.8021446959999,11.6,2.77782872899999));
#196272=CARTESIAN_POINT('Ctrl Pts',(10.7988475759999,15.2,2.77826992999999));
#196273=CARTESIAN_POINT('Ctrl Pts',(10.7988475759999,11.6,2.77826992999999));
#196274=CARTESIAN_POINT('Ctrl Pts',(10.7955550299999,15.2,2.77870785499999));
#196275=CARTESIAN_POINT('Ctrl Pts',(10.7955550299999,11.6,2.77870785499999));
#196276=CARTESIAN_POINT('Ctrl Pts',(10.7922670679999,15.2,2.77914250999999));
#196277=CARTESIAN_POINT('Ctrl Pts',(10.7922670679999,11.6,2.77914250999999));
#196278=CARTESIAN_POINT('Ctrl Pts',(10.7889836979999,15.2,2.77957390099999));
#196279=CARTESIAN_POINT('Ctrl Pts',(10.7889836979999,11.6,2.77957390099999));
#196280=CARTESIAN_POINT('Ctrl Pts',(10.7857049309999,15.2,2.78000203199999));
#196281=CARTESIAN_POINT('Ctrl Pts',(10.7857049309999,11.6,2.78000203199999));
#196282=CARTESIAN_POINT('Ctrl Pts',(10.7824307749999,15.2,2.78042690799998));
#196283=CARTESIAN_POINT('Ctrl Pts',(10.7824307749999,11.6,2.78042690799998));
#196284=CARTESIAN_POINT('Ctrl Pts',(10.7791612379999,15.2,2.78084853699998));
#196285=CARTESIAN_POINT('Ctrl Pts',(10.7791612379999,11.6,2.78084853699998));
#196286=CARTESIAN_POINT('Ctrl Pts',(10.7758963329999,15.2,2.78126692399999));
#196287=CARTESIAN_POINT('Ctrl Pts',(10.7758963329999,11.6,2.78126692399999));
#196288=CARTESIAN_POINT('Ctrl Pts',(10.7726360659999,15.2,2.78168207299998));
#196289=CARTESIAN_POINT('Ctrl Pts',(10.7726360659999,11.6,2.78168207299998));
#196290=CARTESIAN_POINT('Ctrl Pts',(10.7693804469999,15.2,2.78209399099998));
#196291=CARTESIAN_POINT('Ctrl Pts',(10.7693804469999,11.6,2.78209399099998));
#196292=CARTESIAN_POINT('Ctrl Pts',(10.7661294859999,15.2,2.78250268399999));
#196293=CARTESIAN_POINT('Ctrl Pts',(10.7661294859999,11.6,2.78250268399999));
#196294=CARTESIAN_POINT('Ctrl Pts',(10.7628831919999,15.2,2.78290815599998));
#196295=CARTESIAN_POINT('Ctrl Pts',(10.7628831919999,11.6,2.78290815599998));
#196296=CARTESIAN_POINT('Ctrl Pts',(10.7596415739999,15.2,2.78331041399999));
#196297=CARTESIAN_POINT('Ctrl Pts',(10.7596415739999,11.6,2.78331041399999));
#196298=CARTESIAN_POINT('Ctrl Pts',(10.7564046409999,15.2,2.78370946299999));
#196299=CARTESIAN_POINT('Ctrl Pts',(10.7564046409999,11.6,2.78370946299999));
#196300=CARTESIAN_POINT('Ctrl Pts',(10.7531724039999,15.2,2.78410530999999));
#196301=CARTESIAN_POINT('Ctrl Pts',(10.7531724039999,11.6,2.78410530999999));
#196302=CARTESIAN_POINT('Ctrl Pts',(10.7499448709999,15.2,2.78449795899999));
#196303=CARTESIAN_POINT('Ctrl Pts',(10.7499448709999,11.6,2.78449795899998));
#196304=CARTESIAN_POINT('Ctrl Pts',(10.7467220519999,15.2,2.78488741599999));
#196305=CARTESIAN_POINT('Ctrl Pts',(10.7467220519999,11.6,2.78488741599999));
#196306=CARTESIAN_POINT('Ctrl Pts',(10.7435039549999,15.2,2.78527368799999));
#196307=CARTESIAN_POINT('Ctrl Pts',(10.7435039549999,11.6,2.78527368799998));
#196308=CARTESIAN_POINT('Ctrl Pts',(10.7402905919999,15.2,2.78565678199998));
#196309=CARTESIAN_POINT('Ctrl Pts',(10.7402905919999,11.6,2.78565678199998));
#196310=CARTESIAN_POINT('Ctrl Pts',(10.7370819699999,15.2,2.78603669899999));
#196311=CARTESIAN_POINT('Ctrl Pts',(10.7370819699999,11.6,2.78603669899999));
#196312=CARTESIAN_POINT('Ctrl Pts',(10.7338780989999,15.2,2.78641344999999));
#196313=CARTESIAN_POINT('Ctrl Pts',(10.7338780989999,11.6,2.78641344999999));
#196314=CARTESIAN_POINT('Ctrl Pts',(10.7306789899999,15.2,2.78678703799999));
#196315=CARTESIAN_POINT('Ctrl Pts',(10.7306789899999,11.6,2.78678703799999));
#196316=CARTESIAN_POINT('Ctrl Pts',(10.7274846509999,15.2,2.78715746999998));
#196317=CARTESIAN_POINT('Ctrl Pts',(10.7274846509999,11.6,2.78715746999998));
#196318=CARTESIAN_POINT('Ctrl Pts',(10.7242950909999,15.2,2.78752475099999));
#196319=CARTESIAN_POINT('Ctrl Pts',(10.7242950909999,11.6,2.78752475099999));
#196320=CARTESIAN_POINT('Ctrl Pts',(10.7211103209999,15.2,2.78788888599999));
#196321=CARTESIAN_POINT('Ctrl Pts',(10.7211103209999,11.6,2.78788888599998));
#196322=CARTESIAN_POINT('Ctrl Pts',(10.7179303499999,15.2,2.78824988399998));
#196323=CARTESIAN_POINT('Ctrl Pts',(10.7179303499999,11.6,2.78824988399998));
#196324=CARTESIAN_POINT('Ctrl Pts',(10.7147551869999,15.2,2.78860774899999));
#196325=CARTESIAN_POINT('Ctrl Pts',(10.7147551869999,11.6,2.78860774899999));
#196326=CARTESIAN_POINT('Ctrl Pts',(10.7115848429999,15.2,2.78896248699999));
#196327=CARTESIAN_POINT('Ctrl Pts',(10.7115848429999,11.6,2.78896248699999));
#196328=CARTESIAN_POINT('Ctrl Pts',(10.7084193239999,15.2,2.78931410399998));
#196329=CARTESIAN_POINT('Ctrl Pts',(10.7084193239999,11.6,2.78931410399998));
#196330=CARTESIAN_POINT('Ctrl Pts',(10.7052586439999,15.2,2.78966260699999));
#196331=CARTESIAN_POINT('Ctrl Pts',(10.7052586439999,11.6,2.78966260699998));
#196332=CARTESIAN_POINT('Ctrl Pts',(10.7021028099999,15.2,2.79000799999999));
#196333=CARTESIAN_POINT('Ctrl Pts',(10.7021028099999,11.6,2.79000799999999));
#196334=CARTESIAN_POINT('Ctrl Pts',(10.6989518329999,15.2,2.79035029099998));
#196335=CARTESIAN_POINT('Ctrl Pts',(10.6989518329999,11.6,2.79035029099998));
#196336=CARTESIAN_POINT('Ctrl Pts',(10.6958057219999,15.2,2.79068948499999));
#196337=CARTESIAN_POINT('Ctrl Pts',(10.6958057219999,11.6,2.79068948499999));
#196338=CARTESIAN_POINT('Ctrl Pts',(10.6926644859999,15.2,2.79102558999998));
#196339=CARTESIAN_POINT('Ctrl Pts',(10.6926644859999,11.6,2.79102558999998));
#196340=CARTESIAN_POINT('Ctrl Pts',(10.6895281349999,15.2,2.79135860899999));
#196341=CARTESIAN_POINT('Ctrl Pts',(10.6895281349999,11.6,2.79135860899998));
#196342=CARTESIAN_POINT('Ctrl Pts',(10.6863966799999,15.2,2.79168855099999));
#196343=CARTESIAN_POINT('Ctrl Pts',(10.6863966799999,11.6,2.79168855099999));
#196344=CARTESIAN_POINT('Ctrl Pts',(10.6832701279999,15.2,2.79201541999999));
#196345=CARTESIAN_POINT('Ctrl Pts',(10.6832701279999,11.6,2.79201541999999));
#196346=CARTESIAN_POINT('Ctrl Pts',(10.6801484919999,15.2,2.79233922399998));
#196347=CARTESIAN_POINT('Ctrl Pts',(10.6801484919999,11.6,2.79233922399998));
#196348=CARTESIAN_POINT('Ctrl Pts',(10.6770317779999,15.2,2.79265996699999));
#196349=CARTESIAN_POINT('Ctrl Pts',(10.6770317779999,11.6,2.79265996699999));
#196350=CARTESIAN_POINT('Ctrl Pts',(10.6739199989999,15.2,2.79297765699998));
#196351=CARTESIAN_POINT('Ctrl Pts',(10.6739199989999,11.6,2.79297765699998));
#196352=CARTESIAN_POINT('Ctrl Pts',(10.6708131629999,15.2,2.79329229999998));
#196353=CARTESIAN_POINT('Ctrl Pts',(10.6708131629999,11.6,2.79329229999998));
#196354=CARTESIAN_POINT('Ctrl Pts',(10.6677112809999,15.2,2.79360390199999));
#196355=CARTESIAN_POINT('Ctrl Pts',(10.6677112809999,11.6,2.79360390199999));
#196356=CARTESIAN_POINT('Ctrl Pts',(10.6646143609999,15.2,2.79391246899999));
#196357=CARTESIAN_POINT('Ctrl Pts',(10.6646143609999,11.6,2.79391246899999));
#196358=CARTESIAN_POINT('Ctrl Pts',(10.6615224159999,15.2,2.79421800799999));
#196359=CARTESIAN_POINT('Ctrl Pts',(10.6615224159999,11.6,2.79421800799999));
#196360=CARTESIAN_POINT('Ctrl Pts',(10.6584354509999,15.2,2.79452052399999));
#196361=CARTESIAN_POINT('Ctrl Pts',(10.6584354509999,11.6,2.79452052399999));
#196362=CARTESIAN_POINT('Ctrl Pts',(10.6553534799999,15.2,2.79482002499999));
#196363=CARTESIAN_POINT('Ctrl Pts',(10.6553534799999,11.6,2.79482002499999));
#196364=CARTESIAN_POINT('Ctrl Pts',(10.6522765109999,15.2,2.79511651699998));
#196365=CARTESIAN_POINT('Ctrl Pts',(10.6522765109999,11.6,2.79511651699998));
#196366=CARTESIAN_POINT('Ctrl Pts',(10.6492045549999,15.2,2.79541000599998));
#196367=CARTESIAN_POINT('Ctrl Pts',(10.6492045549999,11.6,2.79541000599998));
#196368=CARTESIAN_POINT('Ctrl Pts',(10.6461376199999,15.2,2.79570049699998));
#196369=CARTESIAN_POINT('Ctrl Pts',(10.6461376199999,11.6,2.79570049699998));
#196370=CARTESIAN_POINT('Ctrl Pts',(10.6430757179999,15.2,2.79598799899999));
#196371=CARTESIAN_POINT('Ctrl Pts',(10.6430757179999,11.6,2.79598799899999));
#196372=CARTESIAN_POINT('Ctrl Pts',(10.6400188569999,15.2,2.79627251799998));
#196373=CARTESIAN_POINT('Ctrl Pts',(10.6400188569999,11.6,2.79627251799998));
#196374=CARTESIAN_POINT('Ctrl Pts',(10.6369670479999,15.2,2.79655405899998));
#196375=CARTESIAN_POINT('Ctrl Pts',(10.6369670479999,11.6,2.79655405899998));
#196376=CARTESIAN_POINT('Ctrl Pts',(10.6339203009999,15.2,2.79683262899999));
#196377=CARTESIAN_POINT('Ctrl Pts',(10.6339203009999,11.6,2.79683262899999));
#196378=CARTESIAN_POINT('Ctrl Pts',(10.6308786259999,15.2,2.79710823499999));
#196379=CARTESIAN_POINT('Ctrl Pts',(10.6308786259999,11.6,2.79710823499998));
#196380=CARTESIAN_POINT('Ctrl Pts',(10.6278420329999,15.2,2.79738088399998));
#196381=CARTESIAN_POINT('Ctrl Pts',(10.6278420329999,11.6,2.79738088399998));
#196382=CARTESIAN_POINT('Ctrl Pts',(10.6248105309999,15.2,2.79765058099999));
#196383=CARTESIAN_POINT('Ctrl Pts',(10.6248105309999,11.6,2.79765058099999));
#196384=CARTESIAN_POINT('Ctrl Pts',(10.6217841319999,15.2,2.79791733399998));
#196385=CARTESIAN_POINT('Ctrl Pts',(10.6217841319999,11.6,2.79791733399998));
#196386=CARTESIAN_POINT('Ctrl Pts',(10.6187628439999,15.2,2.79818114899999));
#196387=CARTESIAN_POINT('Ctrl Pts',(10.6187628439999,11.6,2.79818114899999));
#196388=CARTESIAN_POINT('Ctrl Pts',(10.6157466779999,15.2,2.79844203299999));
#196389=CARTESIAN_POINT('Ctrl Pts',(10.6157466779999,11.6,2.79844203299999));
#196390=CARTESIAN_POINT('Ctrl Pts',(10.6127356429999,15.2,2.79869999199998));
#196391=CARTESIAN_POINT('Ctrl Pts',(10.6127356429999,11.6,2.79869999199998));
#196392=CARTESIAN_POINT('Ctrl Pts',(10.6097297519999,15.2,2.79895503299999));
#196393=CARTESIAN_POINT('Ctrl Pts',(10.6097297519999,11.6,2.79895503299999));
#196394=CARTESIAN_POINT('Ctrl Pts',(10.6067290119999,15.2,2.79920716299999));
#196395=CARTESIAN_POINT('Ctrl Pts',(10.6067290119999,11.6,2.79920716299999));
#196396=CARTESIAN_POINT('Ctrl Pts',(10.6037334349999,15.2,2.79945638899999));
#196397=CARTESIAN_POINT('Ctrl Pts',(10.6037334349999,11.6,2.79945638899999));
#196398=CARTESIAN_POINT('Ctrl Pts',(10.6007430289999,15.2,2.79970271699998));
#196399=CARTESIAN_POINT('Ctrl Pts',(10.6007430289999,11.6,2.79970271699998));
#196400=CARTESIAN_POINT('Ctrl Pts',(10.5977578069999,15.2,2.79994615399998));
#196401=CARTESIAN_POINT('Ctrl Pts',(10.5977578069999,11.6,2.79994615399998));
#196402=CARTESIAN_POINT('Ctrl Pts',(10.5947777769999,15.2,2.80018670699998));
#196403=CARTESIAN_POINT('Ctrl Pts',(10.5947777769999,11.6,2.80018670699998));
#196404=CARTESIAN_POINT('Ctrl Pts',(10.5918029509999,15.2,2.80042438199998));
#196405=CARTESIAN_POINT('Ctrl Pts',(10.5918029509999,11.6,2.80042438199998));
#196406=CARTESIAN_POINT('Ctrl Pts',(10.5888333369999,15.2,2.80065918699999));
#196407=CARTESIAN_POINT('Ctrl Pts',(10.5888333369999,11.6,2.80065918699999));
#196408=CARTESIAN_POINT('Ctrl Pts',(10.5858689469999,15.2,2.80089112799998));
#196409=CARTESIAN_POINT('Ctrl Pts',(10.5858689469999,11.6,2.80089112799998));
#196410=CARTESIAN_POINT('Ctrl Pts',(10.5829097899999,15.2,2.80112021299999));
#196411=CARTESIAN_POINT('Ctrl Pts',(10.5829097899999,11.6,2.80112021299999));
#196412=CARTESIAN_POINT('Ctrl Pts',(10.5799558779999,15.2,2.80134644699999));
#196413=CARTESIAN_POINT('Ctrl Pts',(10.5799558779999,11.6,2.80134644699999));
#196414=CARTESIAN_POINT('Ctrl Pts',(10.5770072199999,15.2,2.80156983799999));
#196415=CARTESIAN_POINT('Ctrl Pts',(10.5770072199999,11.6,2.80156983799999));
#196416=CARTESIAN_POINT('Ctrl Pts',(10.5740638259999,15.2,2.80179039399999));
#196417=CARTESIAN_POINT('Ctrl Pts',(10.5740638259999,11.6,2.80179039399999));
#196418=CARTESIAN_POINT('Ctrl Pts',(10.5711257059999,15.2,2.80200812099999));
#196419=CARTESIAN_POINT('Ctrl Pts',(10.5711257059999,11.6,2.80200812099999));
#196420=CARTESIAN_POINT('Ctrl Pts',(10.5681928729999,15.2,2.80222302499999));
#196421=CARTESIAN_POINT('Ctrl Pts',(10.5681928729999,11.6,2.80222302499999));
#196422=CARTESIAN_POINT('Ctrl Pts',(10.5652653349999,15.2,2.80243511499998));
#196423=CARTESIAN_POINT('Ctrl Pts',(10.5652653349999,11.6,2.80243511499998));
#196424=CARTESIAN_POINT('Ctrl Pts',(10.5623431029999,15.2,2.80264439699998));
#196425=CARTESIAN_POINT('Ctrl Pts',(10.5623431029999,11.6,2.80264439699998));
#196426=CARTESIAN_POINT('Ctrl Pts',(10.5594261859999,15.2,2.80285087799999));
#196427=CARTESIAN_POINT('Ctrl Pts',(10.5594261859999,11.6,2.80285087799999));
#196428=CARTESIAN_POINT('Ctrl Pts',(10.5565145969999,15.2,2.80305456499998));
#196429=CARTESIAN_POINT('Ctrl Pts',(10.5565145969999,11.6,2.80305456499998));
#196430=CARTESIAN_POINT('Ctrl Pts',(10.5536083449999,15.2,2.80325546599999));
#196431=CARTESIAN_POINT('Ctrl Pts',(10.5536083449999,11.6,2.80325546599998));
#196432=CARTESIAN_POINT('Ctrl Pts',(10.5507074409999,15.2,2.80345358699999));
#196433=CARTESIAN_POINT('Ctrl Pts',(10.5507074409999,11.6,2.80345358699999));
#196434=CARTESIAN_POINT('Ctrl Pts',(10.5478118939999,15.2,2.80364893599998));
#196435=CARTESIAN_POINT('Ctrl Pts',(10.5478118939999,11.6,2.80364893599998));
#196436=CARTESIAN_POINT('Ctrl Pts',(10.5449217159999,15.2,2.80384151899998));
#196437=CARTESIAN_POINT('Ctrl Pts',(10.5449217159999,11.6,2.80384151899998));
#196438=CARTESIAN_POINT('Ctrl Pts',(10.5420369179999,15.2,2.80403134499998));
#196439=CARTESIAN_POINT('Ctrl Pts',(10.5420369179999,11.6,2.80403134499998));
#196440=CARTESIAN_POINT('Ctrl Pts',(10.5391575079999,15.2,2.80421842099998));
#196441=CARTESIAN_POINT('Ctrl Pts',(10.5391575079999,11.6,2.80421842099998));
#196442=CARTESIAN_POINT('Ctrl Pts',(10.5362834999999,15.2,2.80440275299998));
#196443=CARTESIAN_POINT('Ctrl Pts',(10.5362834999999,11.6,2.80440275299998));
#196444=CARTESIAN_POINT('Ctrl Pts',(10.5334149019999,15.2,2.80458434899998));
#196445=CARTESIAN_POINT('Ctrl Pts',(10.5334149019999,11.6,2.80458434899998));
#196446=CARTESIAN_POINT('Ctrl Pts',(10.5305517249999,15.2,2.80476321599998));
#196447=CARTESIAN_POINT('Ctrl Pts',(10.5305517249999,11.6,2.80476321599998));
#196448=CARTESIAN_POINT('Ctrl Pts',(10.5276939799999,15.2,2.80493936099998));
#196449=CARTESIAN_POINT('Ctrl Pts',(10.5276939799999,11.6,2.80493936099998));
#196450=CARTESIAN_POINT('Ctrl Pts',(10.5248416769999,15.2,2.80511279299999));
#196451=CARTESIAN_POINT('Ctrl Pts',(10.5248416769999,11.6,2.80511279299999));
#196452=CARTESIAN_POINT('Ctrl Pts',(10.5219948289999,15.2,2.80528351899999));
#196453=CARTESIAN_POINT('Ctrl Pts',(10.5219948289999,11.6,2.80528351899999));
#196454=CARTESIAN_POINT('Ctrl Pts',(10.5191534429999,15.2,2.80545154499999));
#196455=CARTESIAN_POINT('Ctrl Pts',(10.5191534429999,11.6,2.80545154499999));
#196456=CARTESIAN_POINT('Ctrl Pts',(10.5163175329999,15.2,2.80561687899999));
#196457=CARTESIAN_POINT('Ctrl Pts',(10.5163175329999,11.6,2.80561687899999));
#196458=CARTESIAN_POINT('Ctrl Pts',(10.5134871079999,15.2,2.80577952899999));
#196459=CARTESIAN_POINT('Ctrl Pts',(10.5134871079999,11.6,2.80577952899998));
#196460=CARTESIAN_POINT('Ctrl Pts',(10.5106621789999,15.2,2.80593950299998));
#196461=CARTESIAN_POINT('Ctrl Pts',(10.5106621789999,11.6,2.80593950299998));
#196462=CARTESIAN_POINT('Ctrl Pts',(10.5078427569999,15.2,2.80609680699998));
#196463=CARTESIAN_POINT('Ctrl Pts',(10.5078427569999,11.6,2.80609680699998));
#196464=CARTESIAN_POINT('Ctrl Pts',(10.5050288509999,15.2,2.80625144999998));
#196465=CARTESIAN_POINT('Ctrl Pts',(10.5050288509999,11.6,2.80625144999998));
#196466=CARTESIAN_POINT('Ctrl Pts',(10.5022204749999,15.2,2.80640343899999));
#196467=CARTESIAN_POINT('Ctrl Pts',(10.5022204749999,11.6,2.80640343899999));
#196468=CARTESIAN_POINT('Ctrl Pts',(10.4994176369999,15.2,2.80655278099999));
#196469=CARTESIAN_POINT('Ctrl Pts',(10.4994176369999,11.6,2.80655278099999));
#196470=CARTESIAN_POINT('Ctrl Pts',(10.4966203499999,15.2,2.80669948499998));
#196471=CARTESIAN_POINT('Ctrl Pts',(10.4966203499999,11.6,2.80669948499998));
#196472=CARTESIAN_POINT('Ctrl Pts',(10.4938286229999,15.2,2.80684355699999));
#196473=CARTESIAN_POINT('Ctrl Pts',(10.4938286229999,11.6,2.80684355699999));
#196474=CARTESIAN_POINT('Ctrl Pts',(10.4910424679999,15.2,2.80698500599998));
#196475=CARTESIAN_POINT('Ctrl Pts',(10.4910424679999,11.6,2.80698500599998));
#196476=CARTESIAN_POINT('Ctrl Pts',(10.4882618969999,15.2,2.80712383899999));
#196477=CARTESIAN_POINT('Ctrl Pts',(10.4882618969999,11.6,2.80712383899999));
#196478=CARTESIAN_POINT('Ctrl Pts',(10.4854869179999,15.2,2.80726006499999));
#196479=CARTESIAN_POINT('Ctrl Pts',(10.4854869179999,11.6,2.80726006499999));
#196480=CARTESIAN_POINT('Ctrl Pts',(10.4827175439999,15.2,2.80739368999999));
#196481=CARTESIAN_POINT('Ctrl Pts',(10.4827175439999,11.6,2.80739368999999));
#196482=CARTESIAN_POINT('Ctrl Pts',(10.4799537849999,15.2,2.80752472299999));
#196483=CARTESIAN_POINT('Ctrl Pts',(10.4799537849999,11.6,2.80752472299999));
#196484=CARTESIAN_POINT('Ctrl Pts',(10.4771956519999,15.2,2.80765317099998));
#196485=CARTESIAN_POINT('Ctrl Pts',(10.4771956519999,11.6,2.80765317099998));
#196486=CARTESIAN_POINT('Ctrl Pts',(10.4744431569999,15.2,2.80777904299998));
#196487=CARTESIAN_POINT('Ctrl Pts',(10.4744431569999,11.6,2.80777904299998));
#196488=CARTESIAN_POINT('Ctrl Pts',(10.4716963109999,15.2,2.80790234499998));
#196489=CARTESIAN_POINT('Ctrl Pts',(10.4716963109999,11.6,2.80790234499998));
#196490=CARTESIAN_POINT('Ctrl Pts',(10.4689551229999,15.2,2.80802308599998));
#196491=CARTESIAN_POINT('Ctrl Pts',(10.4689551229999,11.6,2.80802308599998));
#196492=CARTESIAN_POINT('Ctrl Pts',(10.4662196059999,15.2,2.80814127499998));
#196493=CARTESIAN_POINT('Ctrl Pts',(10.4662196059999,11.6,2.80814127499998));
#196494=CARTESIAN_POINT('Ctrl Pts',(10.4634897709999,15.2,2.80825691999999));
#196495=CARTESIAN_POINT('Ctrl Pts',(10.4634897709999,11.6,2.80825691999999));
#196496=CARTESIAN_POINT('Ctrl Pts',(10.4607656289999,15.2,2.80837002599998));
#196497=CARTESIAN_POINT('Ctrl Pts',(10.4607656289999,11.6,2.80837002599998));
#196498=CARTESIAN_POINT('Ctrl Pts',(10.4580471909999,15.2,2.80848060399999));
#196499=CARTESIAN_POINT('Ctrl Pts',(10.4580471909999,11.6,2.80848060399999));
#196500=CARTESIAN_POINT('Ctrl Pts',(10.4553344669999,15.2,2.80858866099998));
#196501=CARTESIAN_POINT('Ctrl Pts',(10.4553344669999,11.6,2.80858866099998));
#196502=CARTESIAN_POINT('Ctrl Pts',(10.4526274699999,15.2,2.80869420399998));
#196503=CARTESIAN_POINT('Ctrl Pts',(10.4526274699999,11.6,2.80869420399998));
#196504=CARTESIAN_POINT('Ctrl Pts',(10.4499262109999,15.2,2.80879724399998));
#196505=CARTESIAN_POINT('Ctrl Pts',(10.4499262109999,11.6,2.80879724399998));
#196506=CARTESIAN_POINT('Ctrl Pts',(10.4472306989999,15.2,2.80889778599998));
#196507=CARTESIAN_POINT('Ctrl Pts',(10.4472306989999,11.6,2.80889778599998));
#196508=CARTESIAN_POINT('Ctrl Pts',(10.4445409479999,15.2,2.80899584099998));
#196509=CARTESIAN_POINT('Ctrl Pts',(10.4445409479999,11.6,2.80899584099998));
#196510=CARTESIAN_POINT('Ctrl Pts',(10.4418569669999,15.2,2.80909141499999));
#196511=CARTESIAN_POINT('Ctrl Pts',(10.4418569669999,11.6,2.80909141499999));
#196512=CARTESIAN_POINT('Ctrl Pts',(10.4391787699999,15.2,2.80918451599998));
#196513=CARTESIAN_POINT('Ctrl Pts',(10.4391787699999,11.6,2.80918451599998));
#196514=CARTESIAN_POINT('Ctrl Pts',(10.4365063659999,15.2,2.80927515599998));
#196515=CARTESIAN_POINT('Ctrl Pts',(10.4365063659999,11.6,2.80927515599998));
#196516=CARTESIAN_POINT('Ctrl Pts',(10.4338397659999,15.2,2.80936333799998));
#196517=CARTESIAN_POINT('Ctrl Pts',(10.4338397659999,11.6,2.80936333799998));
#196518=CARTESIAN_POINT('Ctrl Pts',(10.4311789839999,15.2,2.80944907299999));
#196519=CARTESIAN_POINT('Ctrl Pts',(10.4311789839999,11.6,2.80944907299999));
#196520=CARTESIAN_POINT('Ctrl Pts',(10.4285240289999,15.2,2.80953237099999));
#196521=CARTESIAN_POINT('Ctrl Pts',(10.4285240289999,11.6,2.80953237099998));
#196522=CARTESIAN_POINT('Ctrl Pts',(10.4258749129999,15.2,2.80961323599998));
#196523=CARTESIAN_POINT('Ctrl Pts',(10.4258749129999,11.6,2.80961323599998));
#196524=CARTESIAN_POINT('Ctrl Pts',(10.4232316479999,15.2,2.80969167999999));
#196525=CARTESIAN_POINT('Ctrl Pts',(10.4232316479999,11.6,2.80969167999999));
#196526=CARTESIAN_POINT('Ctrl Pts',(10.4205942449999,15.2,2.80976771199998));
#196527=CARTESIAN_POINT('Ctrl Pts',(10.4205942449999,11.6,2.80976771199998));
#196528=CARTESIAN_POINT('Ctrl Pts',(10.4179627159999,15.2,2.80984133699998));
#196529=CARTESIAN_POINT('Ctrl Pts',(10.4179627159999,11.6,2.80984133699998));
#196530=CARTESIAN_POINT('Ctrl Pts',(10.4153370719999,15.2,2.80991256599999));
#196531=CARTESIAN_POINT('Ctrl Pts',(10.4153370719999,11.6,2.80991256599999));
#196532=CARTESIAN_POINT('Ctrl Pts',(10.4127173239999,15.2,2.80998140599999));
#196533=CARTESIAN_POINT('Ctrl Pts',(10.4127173239999,11.6,2.80998140599999));
#196534=CARTESIAN_POINT('Ctrl Pts',(10.4101034849999,15.2,2.81004786799999));
#196535=CARTESIAN_POINT('Ctrl Pts',(10.4101034849999,11.6,2.81004786799999));
#196536=CARTESIAN_POINT('Ctrl Pts',(10.4074955649999,15.2,2.81011195799999));
#196537=CARTESIAN_POINT('Ctrl Pts',(10.4074955649999,11.6,2.81011195799999));
#196538=CARTESIAN_POINT('Ctrl Pts',(10.4048935769999,15.2,2.81017368599999));
#196539=CARTESIAN_POINT('Ctrl Pts',(10.4048935769999,11.6,2.81017368599999));
#196540=CARTESIAN_POINT('Ctrl Pts',(10.4022975309999,15.2,2.81023305999998));
#196541=CARTESIAN_POINT('Ctrl Pts',(10.4022975309999,11.6,2.81023305999998));
#196542=CARTESIAN_POINT('Ctrl Pts',(10.3997074399999,15.2,2.81029008999998));
#196543=CARTESIAN_POINT('Ctrl Pts',(10.3997074399999,11.6,2.81029008999998));
#196544=CARTESIAN_POINT('Ctrl Pts',(10.3971233149999,15.2,2.81034478199999));
#196545=CARTESIAN_POINT('Ctrl Pts',(10.3971233149999,11.6,2.81034478199999));
#196546=CARTESIAN_POINT('Ctrl Pts',(10.3945451689999,15.2,2.81039714699999));
#196547=CARTESIAN_POINT('Ctrl Pts',(10.3945451689999,11.6,2.81039714699999));
#196548=CARTESIAN_POINT('Ctrl Pts',(10.3919730119999,15.2,2.81044719399999));
#196549=CARTESIAN_POINT('Ctrl Pts',(10.3919730119999,11.6,2.81044719399999));
#196550=CARTESIAN_POINT('Ctrl Pts',(10.3894068559999,15.2,2.81049492999998));
#196551=CARTESIAN_POINT('Ctrl Pts',(10.3894068559999,11.6,2.81049492999998));
#196552=CARTESIAN_POINT('Ctrl Pts',(10.3868467139999,15.2,2.81054036599999));
#196553=CARTESIAN_POINT('Ctrl Pts',(10.3868467139999,11.6,2.81054036599999));
#196554=CARTESIAN_POINT('Ctrl Pts',(10.3842925959999,15.2,2.81058350899999));
#196555=CARTESIAN_POINT('Ctrl Pts',(10.3842925959999,11.6,2.81058350899999));
#196556=CARTESIAN_POINT('Ctrl Pts',(10.3817445159999,15.2,2.81062436799999));
#196557=CARTESIAN_POINT('Ctrl Pts',(10.3817445159999,11.6,2.81062436799999));
#196558=CARTESIAN_POINT('Ctrl Pts',(10.3792024839999,15.2,2.81066295399999));
#196559=CARTESIAN_POINT('Ctrl Pts',(10.3792024839999,11.6,2.81066295399999));
#196560=CARTESIAN_POINT('Ctrl Pts',(10.3766665119999,15.2,2.81069927299999));
#196561=CARTESIAN_POINT('Ctrl Pts',(10.3766665119999,11.6,2.81069927299999));
#196562=CARTESIAN_POINT('Ctrl Pts',(10.3741366129999,15.2,2.81073333699998));
#196563=CARTESIAN_POINT('Ctrl Pts',(10.3741366129999,11.6,2.81073333699998));
#196564=CARTESIAN_POINT('Ctrl Pts',(10.3716127979999,15.2,2.81076515299999));
#196565=CARTESIAN_POINT('Ctrl Pts',(10.3716127979999,11.6,2.81076515299999));
#196566=CARTESIAN_POINT('Ctrl Pts',(10.3690950799999,15.2,2.81079473099999));
#196567=CARTESIAN_POINT('Ctrl Pts',(10.3690950799999,11.6,2.81079473099999));
#196568=CARTESIAN_POINT('Ctrl Pts',(10.3665834699999,15.2,2.81082207899999));
#196569=CARTESIAN_POINT('Ctrl Pts',(10.3665834699999,11.6,2.81082207899999));
#196570=CARTESIAN_POINT('Ctrl Pts',(10.3640779799999,15.2,2.81084720699998));
#196571=CARTESIAN_POINT('Ctrl Pts',(10.3640779799999,11.6,2.81084720699998));
#196572=CARTESIAN_POINT('Ctrl Pts',(10.3615786239999,15.2,2.81087012399999));
#196573=CARTESIAN_POINT('Ctrl Pts',(10.3615786239999,11.6,2.81087012399999));
#196574=CARTESIAN_POINT('Ctrl Pts',(10.3590854099999,15.2,2.81089083999999));
#196575=CARTESIAN_POINT('Ctrl Pts',(10.3590854099999,11.6,2.81089083999999));
#196576=CARTESIAN_POINT('Ctrl Pts',(10.3565983529999,15.2,2.81090936199998));
#196577=CARTESIAN_POINT('Ctrl Pts',(10.3565983529999,11.6,2.81090936199998));
#196578=CARTESIAN_POINT('Ctrl Pts',(10.3541174659999,15.2,2.81092570199998));
#196579=CARTESIAN_POINT('Ctrl Pts',(10.3541174659999,11.6,2.81092570199998));
#196580=CARTESIAN_POINT('Ctrl Pts',(10.3516427589999,15.2,2.81093986799998));
#196581=CARTESIAN_POINT('Ctrl Pts',(10.3516427589999,11.6,2.81093986799998));
#196582=CARTESIAN_POINT('Ctrl Pts',(10.3491742439999,15.2,2.81095186899999));
#196583=CARTESIAN_POINT('Ctrl Pts',(10.3491742439999,11.6,2.81095186899999));
#196584=CARTESIAN_POINT('Ctrl Pts',(10.3467119339999,15.2,2.81096171499998));
#196585=CARTESIAN_POINT('Ctrl Pts',(10.3467119339999,11.6,2.81096171499998));
#196586=CARTESIAN_POINT('Ctrl Pts',(10.3442558419999,15.2,2.81096941599999));
#196587=CARTESIAN_POINT('Ctrl Pts',(10.3442558419999,11.6,2.81096941599999));
#196588=CARTESIAN_POINT('Ctrl Pts',(10.3418059809999,15.2,2.81097497899999));
#196589=CARTESIAN_POINT('Ctrl Pts',(10.3418059809999,11.6,2.81097497899999));
#196590=CARTESIAN_POINT('Ctrl Pts',(10.3393623599999,15.2,2.81097841599999));
#196591=CARTESIAN_POINT('Ctrl Pts',(10.3393623599999,11.6,2.81097841599998));
#196592=CARTESIAN_POINT('Ctrl Pts',(10.3369249929999,15.2,2.81097973599999));
#196593=CARTESIAN_POINT('Ctrl Pts',(10.3369249929999,11.6,2.81097973599999));
#196594=CARTESIAN_POINT('Ctrl Pts',(10.3344938929999,15.2,2.81097894699998));
#196595=CARTESIAN_POINT('Ctrl Pts',(10.3344938929999,11.6,2.81097894699998));
#196596=CARTESIAN_POINT('Ctrl Pts',(10.3320690709999,15.2,2.81097606099999));
#196597=CARTESIAN_POINT('Ctrl Pts',(10.3320690709999,11.6,2.81097606099999));
#196598=CARTESIAN_POINT('Ctrl Pts',(10.3296505419999,15.2,2.81097108499999));
#196599=CARTESIAN_POINT('Ctrl Pts',(10.3296505419999,11.6,2.81097108499999));
#196600=CARTESIAN_POINT('Ctrl Pts',(10.3272383149999,15.2,2.81096403199999));
#196601=CARTESIAN_POINT('Ctrl Pts',(10.3272383149999,11.6,2.81096403199999));
#196602=CARTESIAN_POINT('Ctrl Pts',(10.3248324049999,15.2,2.81095490799999));
#196603=CARTESIAN_POINT('Ctrl Pts',(10.3248324049999,11.6,2.81095490799998));
#196604=CARTESIAN_POINT('Ctrl Pts',(10.3224328229999,15.2,2.81094372499999));
#196605=CARTESIAN_POINT('Ctrl Pts',(10.3224328229999,11.6,2.81094372499999));
#196606=CARTESIAN_POINT('Ctrl Pts',(10.3200395829999,15.2,2.81093049299999));
#196607=CARTESIAN_POINT('Ctrl Pts',(10.3200395829999,11.6,2.81093049299999));
#196608=CARTESIAN_POINT('Ctrl Pts',(10.3176526949999,15.2,2.81091521999999));
#196609=CARTESIAN_POINT('Ctrl Pts',(10.3176526949999,11.6,2.81091521999999));
#196610=CARTESIAN_POINT('Ctrl Pts',(10.3152721739999,15.2,2.81089791699999));
#196611=CARTESIAN_POINT('Ctrl Pts',(10.3152721739999,11.6,2.81089791699999));
#196612=CARTESIAN_POINT('Ctrl Pts',(10.3128980319999,15.2,2.81087859499999));
#196613=CARTESIAN_POINT('Ctrl Pts',(10.3128980319999,11.6,2.81087859499999));
#196614=CARTESIAN_POINT('Ctrl Pts',(10.3105302809999,15.2,2.81085726199999));
#196615=CARTESIAN_POINT('Ctrl Pts',(10.3105302809999,11.6,2.81085726199999));
#196616=CARTESIAN_POINT('Ctrl Pts',(10.3081689339999,15.2,2.81083392699998));
#196617=CARTESIAN_POINT('Ctrl Pts',(10.3081689339999,11.6,2.81083392699998));
#196618=CARTESIAN_POINT('Ctrl Pts',(10.3058140039999,15.2,2.81080860299999));
#196619=CARTESIAN_POINT('Ctrl Pts',(10.3058140039999,11.6,2.81080860299999));
#196620=CARTESIAN_POINT('Ctrl Pts',(10.3034655029999,15.2,2.81078129899999));
#196621=CARTESIAN_POINT('Ctrl Pts',(10.3034655029999,11.6,2.81078129899999));
#196622=CARTESIAN_POINT('Ctrl Pts',(10.3011234449999,15.2,2.81075202499999));
#196623=CARTESIAN_POINT('Ctrl Pts',(10.3011234449999,11.6,2.81075202499998));
#196624=CARTESIAN_POINT('Ctrl Pts',(10.2987878399999,15.2,2.81072078899999));
#196625=CARTESIAN_POINT('Ctrl Pts',(10.2987878399999,11.6,2.81072078899999));
#196626=CARTESIAN_POINT('Ctrl Pts',(10.2964587039999,15.2,2.81068760399998));
#196627=CARTESIAN_POINT('Ctrl Pts',(10.2964587039999,11.6,2.81068760399998));
#196628=CARTESIAN_POINT('Ctrl Pts',(10.2941360499999,15.2,2.81065247899999));
#196629=CARTESIAN_POINT('Ctrl Pts',(10.2941360499999,11.6,2.81065247899999));
#196630=CARTESIAN_POINT('Ctrl Pts',(10.2918198869999,15.2,2.81061542499998));
#196631=CARTESIAN_POINT('Ctrl Pts',(10.2918198869999,11.6,2.81061542499998));
#196632=CARTESIAN_POINT('Ctrl Pts',(10.2895102319999,15.2,2.81057645199999));
#196633=CARTESIAN_POINT('Ctrl Pts',(10.2895102319999,11.6,2.81057645199999));
#196634=CARTESIAN_POINT('Ctrl Pts',(10.2872070959999,15.2,2.81053556799999));
#196635=CARTESIAN_POINT('Ctrl Pts',(10.2872070959999,11.6,2.81053556799999));
#196636=CARTESIAN_POINT('Ctrl Pts',(10.2849104899999,15.2,2.81049278699999));
#196637=CARTESIAN_POINT('Ctrl Pts',(10.2849104899999,11.6,2.81049278699999));
#196638=CARTESIAN_POINT('Ctrl Pts',(10.2826204319999,15.2,2.81044811699999));
#196639=CARTESIAN_POINT('Ctrl Pts',(10.2826204319999,11.6,2.81044811699999));
#196640=CARTESIAN_POINT('Ctrl Pts',(10.2803369309999,15.2,2.81040156799998));
#196641=CARTESIAN_POINT('Ctrl Pts',(10.2803369309999,11.6,2.81040156799998));
#196642=CARTESIAN_POINT('Ctrl Pts',(10.2780600009999,15.2,2.81035315199999));
#196643=CARTESIAN_POINT('Ctrl Pts',(10.2780600009999,11.6,2.81035315199999));
#196644=CARTESIAN_POINT('Ctrl Pts',(10.2757896559999,15.2,2.81030288099998));
#196645=CARTESIAN_POINT('Ctrl Pts',(10.2757896559999,11.6,2.81030288099998));
#196646=CARTESIAN_POINT('Ctrl Pts',(10.2735259089999,15.2,2.81025076199998));
#196647=CARTESIAN_POINT('Ctrl Pts',(10.2735259089999,11.6,2.81025076199998));
#196648=CARTESIAN_POINT('Ctrl Pts',(10.2712687709999,15.2,2.81019680599999));
#196649=CARTESIAN_POINT('Ctrl Pts',(10.2712687709999,11.6,2.81019680599999));
#196650=CARTESIAN_POINT('Ctrl Pts',(10.2690182579999,15.2,2.81014102599999));
#196651=CARTESIAN_POINT('Ctrl Pts',(10.2690182579999,11.6,2.81014102599999));
#196652=CARTESIAN_POINT('Ctrl Pts',(10.2667743819999,15.2,2.81008343199999));
#196653=CARTESIAN_POINT('Ctrl Pts',(10.2667743819999,11.6,2.81008343199999));
#196654=CARTESIAN_POINT('Ctrl Pts',(10.2645371559999,15.2,2.81002403399999));
#196655=CARTESIAN_POINT('Ctrl Pts',(10.2645371559999,11.6,2.81002403399999));
#196656=CARTESIAN_POINT('Ctrl Pts',(10.2623065929999,15.2,2.80996284199999));
#196657=CARTESIAN_POINT('Ctrl Pts',(10.2623065929999,11.6,2.80996284199999));
#196658=CARTESIAN_POINT('Ctrl Pts',(10.2600827069999,15.2,2.80989986699999));
#196659=CARTESIAN_POINT('Ctrl Pts',(10.2600827069999,11.6,2.80989986699998));
#196660=CARTESIAN_POINT('Ctrl Pts',(10.2578655119999,15.2,2.80983512099999));
#196661=CARTESIAN_POINT('Ctrl Pts',(10.2578655119999,11.6,2.80983512099999));
#196662=CARTESIAN_POINT('Ctrl Pts',(10.2556550209999,15.2,2.80976861599999));
#196663=CARTESIAN_POINT('Ctrl Pts',(10.2556550209999,11.6,2.80976861599999));
#196664=CARTESIAN_POINT('Ctrl Pts',(10.2534512459999,15.2,2.80970035899998));
#196665=CARTESIAN_POINT('Ctrl Pts',(10.2534512459999,11.6,2.80970035899998));
#196666=CARTESIAN_POINT('Ctrl Pts',(10.2512542019999,15.2,2.80963036499998));
#196667=CARTESIAN_POINT('Ctrl Pts',(10.2512542019999,11.6,2.80963036499998));
#196668=CARTESIAN_POINT('Ctrl Pts',(10.2490639019999,15.2,2.80955864199999));
#196669=CARTESIAN_POINT('Ctrl Pts',(10.2490639019999,11.6,2.80955864199999));
#196670=CARTESIAN_POINT('Ctrl Pts',(10.2468803589999,15.2,2.80948520299999));
#196671=CARTESIAN_POINT('Ctrl Pts',(10.2468803589999,11.6,2.80948520299999));
#196672=CARTESIAN_POINT('Ctrl Pts',(10.2447035879999,15.2,2.80941005799999));
#196673=CARTESIAN_POINT('Ctrl Pts',(10.2447035879999,11.6,2.80941005799999));
#196674=CARTESIAN_POINT('Ctrl Pts',(10.2425335999999,15.2,2.80933321799999));
#196675=CARTESIAN_POINT('Ctrl Pts',(10.2425335999999,11.6,2.80933321799999));
#196676=CARTESIAN_POINT('Ctrl Pts',(10.2403704109999,15.2,2.80925469399998));
#196677=CARTESIAN_POINT('Ctrl Pts',(10.2403704109999,11.6,2.80925469399998));
#196678=CARTESIAN_POINT('Ctrl Pts',(10.2382140349999,15.2,2.80917449999999));
#196679=CARTESIAN_POINT('Ctrl Pts',(10.2382140349999,11.6,2.80917449999999));
#196680=CARTESIAN_POINT('Ctrl Pts',(10.2360644839999,15.2,2.80909264399998));
#196681=CARTESIAN_POINT('Ctrl Pts',(10.2360644839999,11.6,2.80909264399998));
#196682=CARTESIAN_POINT('Ctrl Pts',(10.2339217719999,15.2,2.80900913799999));
#196683=CARTESIAN_POINT('Ctrl Pts',(10.2339217719999,11.6,2.80900913799999));
#196684=CARTESIAN_POINT('Ctrl Pts',(10.2317859129999,15.2,2.80892399399999));
#196685=CARTESIAN_POINT('Ctrl Pts',(10.2317859129999,11.6,2.80892399399999));
#196686=CARTESIAN_POINT('Ctrl Pts',(10.2296569209999,15.2,2.80883722299999));
#196687=CARTESIAN_POINT('Ctrl Pts',(10.2296569209999,11.6,2.80883722299999));
#196688=CARTESIAN_POINT('Ctrl Pts',(10.2275348109999,15.2,2.80874883799999));
#196689=CARTESIAN_POINT('Ctrl Pts',(10.2275348109999,11.6,2.80874883799999));
#196690=CARTESIAN_POINT('Ctrl Pts',(10.2254195939999,15.2,2.80865884799999));
#196691=CARTESIAN_POINT('Ctrl Pts',(10.2254195939999,11.6,2.80865884799999));
#196692=CARTESIAN_POINT('Ctrl Pts',(10.2233112869999,15.2,2.80856726499999));
#196693=CARTESIAN_POINT('Ctrl Pts',(10.2233112869999,11.6,2.80856726499999));
#196694=CARTESIAN_POINT('Ctrl Pts',(10.2212099009999,15.2,2.80847410299998));
#196695=CARTESIAN_POINT('Ctrl Pts',(10.2212099009999,11.6,2.80847410299998));
#196696=CARTESIAN_POINT('Ctrl Pts',(10.2191154529999,15.2,2.80837936999998));
#196697=CARTESIAN_POINT('Ctrl Pts',(10.2191154529999,11.6,2.80837936999998));
#196698=CARTESIAN_POINT('Ctrl Pts',(10.2170279549999,15.2,2.80828308099998));
#196699=CARTESIAN_POINT('Ctrl Pts',(10.2170279549999,11.6,2.80828308099998));
#196700=CARTESIAN_POINT('Ctrl Pts',(10.2149474219999,15.2,2.80818524499999));
#196701=CARTESIAN_POINT('Ctrl Pts',(10.2149474219999,11.6,2.80818524499999));
#196702=CARTESIAN_POINT('Ctrl Pts',(10.2128738679999,15.2,2.80808587499998));
#196703=CARTESIAN_POINT('Ctrl Pts',(10.2128738679999,11.6,2.80808587499998));
#196704=CARTESIAN_POINT('Ctrl Pts',(10.2108073059999,15.2,2.80798498399999));
#196705=CARTESIAN_POINT('Ctrl Pts',(10.2108073059999,11.6,2.80798498399999));
#196706=CARTESIAN_POINT('Ctrl Pts',(10.2087477509999,15.2,2.80788258099999));
#196707=CARTESIAN_POINT('Ctrl Pts',(10.2087477509999,11.6,2.80788258099999));
#196708=CARTESIAN_POINT('Ctrl Pts',(10.2066952179999,15.2,2.80777868099998));
#196709=CARTESIAN_POINT('Ctrl Pts',(10.2066952179999,11.6,2.80777868099998));
#196710=CARTESIAN_POINT('Ctrl Pts',(10.2046497199999,15.2,2.80767329399998));
#196711=CARTESIAN_POINT('Ctrl Pts',(10.2046497199999,11.6,2.80767329399998));
#196712=CARTESIAN_POINT('Ctrl Pts',(10.2026112719999,15.2,2.80756643299998));
#196713=CARTESIAN_POINT('Ctrl Pts',(10.2026112719999,11.6,2.80756643299998));
#196714=CARTESIAN_POINT('Ctrl Pts',(10.2005798889999,15.2,2.80745810899998));
#196715=CARTESIAN_POINT('Ctrl Pts',(10.2005798889999,11.6,2.80745810899998));
#196716=CARTESIAN_POINT('Ctrl Pts',(10.1985555829999,15.2,2.80734833399999));
#196717=CARTESIAN_POINT('Ctrl Pts',(10.1985555829999,11.6,2.80734833399999));
#196718=CARTESIAN_POINT('Ctrl Pts',(10.1965383709999,15.2,2.80723712199999));
#196719=CARTESIAN_POINT('Ctrl Pts',(10.1965383709999,11.6,2.80723712199999));
#196720=CARTESIAN_POINT('Ctrl Pts',(10.1945282669999,15.2,2.80712448399999));
#196721=CARTESIAN_POINT('Ctrl Pts',(10.1945282669999,11.6,2.80712448399999));
#196722=CARTESIAN_POINT('Ctrl Pts',(10.1925252829999,15.2,2.80701043199999));
#196723=CARTESIAN_POINT('Ctrl Pts',(10.1925252829999,11.6,2.80701043199999));
#196724=CARTESIAN_POINT('Ctrl Pts',(10.1905294369999,15.2,2.80689497899999));
#196725=CARTESIAN_POINT('Ctrl Pts',(10.1905294369999,11.6,2.80689497899999));
#196726=CARTESIAN_POINT('Ctrl Pts',(10.1885407419999,15.2,2.80677813699998));
#196727=CARTESIAN_POINT('Ctrl Pts',(10.1885407419999,11.6,2.80677813699998));
#196728=CARTESIAN_POINT('Ctrl Pts',(10.1865592119999,15.2,2.80665991699999));
#196729=CARTESIAN_POINT('Ctrl Pts',(10.1865592119999,11.6,2.80665991699998));
#196730=CARTESIAN_POINT('Ctrl Pts',(10.1845848629999,15.2,2.80654033399999));
#196731=CARTESIAN_POINT('Ctrl Pts',(10.1845848629999,11.6,2.80654033399998));
#196732=CARTESIAN_POINT('Ctrl Pts',(10.1826177079999,15.2,2.80641939899999));
#196733=CARTESIAN_POINT('Ctrl Pts',(10.1826177079999,11.6,2.80641939899999));
#196734=CARTESIAN_POINT('Ctrl Pts',(10.1806577639999,15.2,2.80629712499999));
#196735=CARTESIAN_POINT('Ctrl Pts',(10.1806577639999,11.6,2.80629712499999));
#196736=CARTESIAN_POINT('Ctrl Pts',(10.1787050449999,15.2,2.80617352499998));
#196737=CARTESIAN_POINT('Ctrl Pts',(10.1787050449999,11.6,2.80617352499998));
#196738=CARTESIAN_POINT('Ctrl Pts',(10.1767595639999,15.2,2.80604860999999));
#196739=CARTESIAN_POINT('Ctrl Pts',(10.1767595639999,11.6,2.80604860999999));
#196740=CARTESIAN_POINT('Ctrl Pts',(10.1748213379999,15.2,2.80592239499998));
#196741=CARTESIAN_POINT('Ctrl Pts',(10.1748213379999,11.6,2.80592239499998));
#196742=CARTESIAN_POINT('Ctrl Pts',(10.1728903809999,15.2,2.80579489099999));
#196743=CARTESIAN_POINT('Ctrl Pts',(10.1728903809999,11.6,2.80579489099999));
#196744=CARTESIAN_POINT('Ctrl Pts',(10.1709667089999,15.2,2.80566611099999));
#196745=CARTESIAN_POINT('Ctrl Pts',(10.1709667089999,11.6,2.80566611099999));
#196746=CARTESIAN_POINT('Ctrl Pts',(10.1690503349999,15.2,2.80553606899999));
#196747=CARTESIAN_POINT('Ctrl Pts',(10.1690503349999,11.6,2.80553606899998));
#196748=CARTESIAN_POINT('Ctrl Pts',(10.1671412759999,15.2,2.80540477799998));
#196749=CARTESIAN_POINT('Ctrl Pts',(10.1671412759999,11.6,2.80540477799998));
#196750=CARTESIAN_POINT('Ctrl Pts',(10.1652395459999,15.2,2.80527224899998));
#196751=CARTESIAN_POINT('Ctrl Pts',(10.1652395459999,11.6,2.80527224899998));
#196752=CARTESIAN_POINT('Ctrl Pts',(10.1633451609999,15.2,2.80513849699998));
#196753=CARTESIAN_POINT('Ctrl Pts',(10.1633451609999,11.6,2.80513849699998));
#196754=CARTESIAN_POINT('Ctrl Pts',(10.1614581339999,15.2,2.80500353399999));
#196755=CARTESIAN_POINT('Ctrl Pts',(10.1614581339999,11.6,2.80500353399999));
#196756=CARTESIAN_POINT('Ctrl Pts',(10.1595784839999,15.2,2.80486737399999));
#196757=CARTESIAN_POINT('Ctrl Pts',(10.1595784839999,11.6,2.80486737399999));
#196758=CARTESIAN_POINT('Ctrl Pts',(10.1577062229999,15.2,2.80473002899999));
#196759=CARTESIAN_POINT('Ctrl Pts',(10.1577062229999,11.6,2.80473002899999));
#196760=CARTESIAN_POINT('Ctrl Pts',(10.1558413669999,15.2,2.80459151299999));
#196761=CARTESIAN_POINT('Ctrl Pts',(10.1558413669999,11.6,2.80459151299999));
#196762=CARTESIAN_POINT('Ctrl Pts',(10.1539839329999,15.2,2.80445183999999));
#196763=CARTESIAN_POINT('Ctrl Pts',(10.1539839329999,11.6,2.80445183999999));
#196764=CARTESIAN_POINT('Ctrl Pts',(10.1521339339999,15.2,2.80431102199999));
#196765=CARTESIAN_POINT('Ctrl Pts',(10.1521339339999,11.6,2.80431102199999));
#196766=CARTESIAN_POINT('Ctrl Pts',(10.1502913879999,15.2,2.80416907399999));
#196767=CARTESIAN_POINT('Ctrl Pts',(10.1502913879999,11.6,2.80416907399999));
#196768=CARTESIAN_POINT('Ctrl Pts',(10.1484563089999,15.2,2.80402600799999));
#196769=CARTESIAN_POINT('Ctrl Pts',(10.1484563089999,11.6,2.80402600799999));
#196770=CARTESIAN_POINT('Ctrl Pts',(10.1466287129999,15.2,2.80388183699999));
#196771=CARTESIAN_POINT('Ctrl Pts',(10.1466287129999,11.6,2.80388183699999));
#196772=CARTESIAN_POINT('Ctrl Pts',(10.1448086139999,15.2,2.80373657799998));
#196773=CARTESIAN_POINT('Ctrl Pts',(10.1448086139999,11.6,2.80373657799998));
#196774=CARTESIAN_POINT('Ctrl Pts',(10.1429960289999,15.2,2.80359023999999));
#196775=CARTESIAN_POINT('Ctrl Pts',(10.1429960289999,11.6,2.80359023999999));
#196776=CARTESIAN_POINT('Ctrl Pts',(10.1411909749999,15.2,2.80344284099999));
#196777=CARTESIAN_POINT('Ctrl Pts',(10.1411909749999,11.6,2.80344284099999));
#196778=CARTESIAN_POINT('Ctrl Pts',(10.1393934659999,15.2,2.80329439199999));
#196779=CARTESIAN_POINT('Ctrl Pts',(10.1393934659999,11.6,2.80329439199999));
#196780=CARTESIAN_POINT('Ctrl Pts',(10.1376035179999,15.2,2.80314490699999));
#196781=CARTESIAN_POINT('Ctrl Pts',(10.1376035179999,11.6,2.80314490699999));
#196782=CARTESIAN_POINT('Ctrl Pts',(10.1358211459999,15.2,2.80299440199999));
#196783=CARTESIAN_POINT('Ctrl Pts',(10.1358211459999,11.6,2.80299440199998));
#196784=CARTESIAN_POINT('Ctrl Pts',(10.1340463689999,15.2,2.80284288899999));
#196785=CARTESIAN_POINT('Ctrl Pts',(10.1340463689999,11.6,2.80284288899999));
#196786=CARTESIAN_POINT('Ctrl Pts',(10.1322791999999,15.2,2.80269038199998));
#196787=CARTESIAN_POINT('Ctrl Pts',(10.1322791999999,11.6,2.80269038199998));
#196788=CARTESIAN_POINT('Ctrl Pts',(10.1305196549999,15.2,2.80253689599999));
#196789=CARTESIAN_POINT('Ctrl Pts',(10.1305196549999,11.6,2.80253689599998));
#196790=CARTESIAN_POINT('Ctrl Pts',(10.1287677519999,15.2,2.80238244599998));
#196791=CARTESIAN_POINT('Ctrl Pts',(10.1287677519999,11.6,2.80238244599998));
#196792=CARTESIAN_POINT('Ctrl Pts',(10.1270235059999,15.2,2.80222704299998));
#196793=CARTESIAN_POINT('Ctrl Pts',(10.1270235059999,11.6,2.80222704299998));
#196794=CARTESIAN_POINT('Ctrl Pts',(10.1252869329999,15.2,2.80207070399998));
#196795=CARTESIAN_POINT('Ctrl Pts',(10.1252869329999,11.6,2.80207070399998));
#196796=CARTESIAN_POINT('Ctrl Pts',(10.1235580499999,15.2,2.80191344299999));
#196797=CARTESIAN_POINT('Ctrl Pts',(10.1235580499999,11.6,2.80191344299999));
#196798=CARTESIAN_POINT('Ctrl Pts',(10.1218368709999,15.2,2.80175527399999));
#196799=CARTESIAN_POINT('Ctrl Pts',(10.1218368709999,11.6,2.80175527399999));
#196800=CARTESIAN_POINT('Ctrl Pts',(10.1201234149999,15.2,2.80159621099998));
#196801=CARTESIAN_POINT('Ctrl Pts',(10.1201234149999,11.6,2.80159621099998));
#196802=CARTESIAN_POINT('Ctrl Pts',(10.1184176969999,15.2,2.80143626899999));
#196803=CARTESIAN_POINT('Ctrl Pts',(10.1184176969999,11.6,2.80143626899999));
#196804=CARTESIAN_POINT('Ctrl Pts',(10.1167197329999,15.2,2.80127546199999));
#196805=CARTESIAN_POINT('Ctrl Pts',(10.1167197329999,11.6,2.80127546199999));
#196806=CARTESIAN_POINT('Ctrl Pts',(10.1150295409999,15.2,2.80111380599998));
#196807=CARTESIAN_POINT('Ctrl Pts',(10.1150295409999,11.6,2.80111380599998));
#196808=CARTESIAN_POINT('Ctrl Pts',(10.1133471369999,15.2,2.80095131499999));
#196809=CARTESIAN_POINT('Ctrl Pts',(10.1133471369999,11.6,2.80095131499999));
#196810=CARTESIAN_POINT('Ctrl Pts',(10.1116725359999,15.2,2.80078800299999));
#196811=CARTESIAN_POINT('Ctrl Pts',(10.1116725359999,11.6,2.80078800299999));
#196812=CARTESIAN_POINT('Ctrl Pts',(10.1100057559999,15.2,2.80062388499999));
#196813=CARTESIAN_POINT('Ctrl Pts',(10.1100057559999,11.6,2.80062388499999));
#196814=CARTESIAN_POINT('Ctrl Pts',(10.1083468139999,15.2,2.80045897699999));
#196815=CARTESIAN_POINT('Ctrl Pts',(10.1083468139999,11.6,2.80045897699999));
#196816=CARTESIAN_POINT('Ctrl Pts',(10.1066957249999,15.2,2.80029329299998));
#196817=CARTESIAN_POINT('Ctrl Pts',(10.1066957249999,11.6,2.80029329299998));
#196818=CARTESIAN_POINT('Ctrl Pts',(10.1050525089999,15.2,2.80012684799999));
#196819=CARTESIAN_POINT('Ctrl Pts',(10.1050525089999,11.6,2.80012684799999));
#196820=CARTESIAN_POINT('Ctrl Pts',(10.1034171789999,15.2,2.79995965799999));
#196821=CARTESIAN_POINT('Ctrl Pts',(10.1034171789999,11.6,2.79995965799999));
#196822=CARTESIAN_POINT('Ctrl Pts',(10.1017897539999,15.2,2.79979173799998));
#196823=CARTESIAN_POINT('Ctrl Pts',(10.1017897539999,11.6,2.79979173799998));
#196824=CARTESIAN_POINT('Ctrl Pts',(10.1001702509999,15.2,2.79962310199998));
#196825=CARTESIAN_POINT('Ctrl Pts',(10.1001702509999,11.6,2.79962310199998));
#196826=CARTESIAN_POINT('Ctrl Pts',(10.0985586869999,15.2,2.79945376699998));
#196827=CARTESIAN_POINT('Ctrl Pts',(10.0985586869999,11.6,2.79945376699998));
#196828=CARTESIAN_POINT('Ctrl Pts',(10.0969550769999,15.2,2.79928374699999));
#196829=CARTESIAN_POINT('Ctrl Pts',(10.0969550769999,11.6,2.79928374699998));
#196830=CARTESIAN_POINT('Ctrl Pts',(10.0953594409999,15.2,2.79911305799998));
#196831=CARTESIAN_POINT('Ctrl Pts',(10.0953594409999,11.6,2.79911305799998));
#196832=CARTESIAN_POINT('Ctrl Pts',(10.0937717949999,15.2,2.79894171599998));
#196833=CARTESIAN_POINT('Ctrl Pts',(10.0937717949999,11.6,2.79894171599998));
#196834=CARTESIAN_POINT('Ctrl Pts',(10.0921921569999,15.2,2.79876973499999));
#196835=CARTESIAN_POINT('Ctrl Pts',(10.0921921569999,11.6,2.79876973499999));
#196836=CARTESIAN_POINT('Ctrl Pts',(10.0906205419999,15.2,2.79859713299999));
#196837=CARTESIAN_POINT('Ctrl Pts',(10.0906205419999,11.6,2.79859713299999));
#196838=CARTESIAN_POINT('Ctrl Pts',(10.0890569699999,15.2,2.79842392399999));
#196839=CARTESIAN_POINT('Ctrl Pts',(10.0890569699999,11.6,2.79842392399999));
#196840=CARTESIAN_POINT('Ctrl Pts',(10.0875014559999,15.2,2.79825012399999));
#196841=CARTESIAN_POINT('Ctrl Pts',(10.0875014559999,11.6,2.79825012399999));
#196842=CARTESIAN_POINT('Ctrl Pts',(10.0859540199999,15.2,2.79807574899999));
#196843=CARTESIAN_POINT('Ctrl Pts',(10.0859540199999,11.6,2.79807574899999));
#196844=CARTESIAN_POINT('Ctrl Pts',(10.0844146779999,15.2,2.79790081599998));
#196845=CARTESIAN_POINT('Ctrl Pts',(10.0844146779999,11.6,2.79790081599998));
#196846=CARTESIAN_POINT('Ctrl Pts',(10.0828834479999,15.2,2.79772533899998));
#196847=CARTESIAN_POINT('Ctrl Pts',(10.0828834479999,11.6,2.79772533899998));
#196848=CARTESIAN_POINT('Ctrl Pts',(10.0813603479999,15.2,2.79754933599998));
#196849=CARTESIAN_POINT('Ctrl Pts',(10.0813603479999,11.6,2.79754933599998));
#196850=CARTESIAN_POINT('Ctrl Pts',(10.0798453939999,15.2,2.79737282199999));
#196851=CARTESIAN_POINT('Ctrl Pts',(10.0798453939999,11.6,2.79737282199999));
#196852=CARTESIAN_POINT('Ctrl Pts',(10.0783386059999,15.2,2.79719581399998));
#196853=CARTESIAN_POINT('Ctrl Pts',(10.0783386059999,11.6,2.79719581399998));
#196854=CARTESIAN_POINT('Ctrl Pts',(10.0768400009999,15.2,2.79701832799999));
#196855=CARTESIAN_POINT('Ctrl Pts',(10.0768400009999,11.6,2.79701832799999));
#196856=CARTESIAN_POINT('Ctrl Pts',(10.0753495959999,15.2,2.79684037999999));
#196857=CARTESIAN_POINT('Ctrl Pts',(10.0753495959999,11.6,2.79684037999999));
#196858=CARTESIAN_POINT('Ctrl Pts',(10.0738674099999,15.2,2.79666198699999));
#196859=CARTESIAN_POINT('Ctrl Pts',(10.0738674099999,11.6,2.79666198699999));
#196860=CARTESIAN_POINT('Ctrl Pts',(10.0723934619999,15.2,2.79648316499999));
#196861=CARTESIAN_POINT('Ctrl Pts',(10.0723934619999,11.6,2.79648316499999));
#196862=CARTESIAN_POINT('Ctrl Pts',(10.0709277689999,15.2,2.79630393099998));
#196863=CARTESIAN_POINT('Ctrl Pts',(10.0709277689999,11.6,2.79630393099998));
#196864=CARTESIAN_POINT('Ctrl Pts',(10.0694703469999,15.2,2.79612430099998));
#196865=CARTESIAN_POINT('Ctrl Pts',(10.0694703469999,11.6,2.79612430099998));
#196866=CARTESIAN_POINT('Ctrl Pts',(10.0680212179999,15.2,2.79594429399998));
#196867=CARTESIAN_POINT('Ctrl Pts',(10.0680212179999,11.6,2.79594429399998));
#196868=CARTESIAN_POINT('Ctrl Pts',(10.0665803979999,15.2,2.79576392499998));
#196869=CARTESIAN_POINT('Ctrl Pts',(10.0665803979999,11.6,2.79576392499998));
#196870=CARTESIAN_POINT('Ctrl Pts',(10.0651479059999,15.2,2.79558321099999));
#196871=CARTESIAN_POINT('Ctrl Pts',(10.0651479059999,11.6,2.79558321099999));
#196872=CARTESIAN_POINT('Ctrl Pts',(10.0637237609999,15.2,2.79540216899999));
#196873=CARTESIAN_POINT('Ctrl Pts',(10.0637237609999,11.6,2.79540216899999));
#196874=CARTESIAN_POINT('Ctrl Pts',(10.0623079809999,15.2,2.79522081599998));
#196875=CARTESIAN_POINT('Ctrl Pts',(10.0623079809999,11.6,2.79522081599998));
#196876=CARTESIAN_POINT('Ctrl Pts',(10.0609005839999,15.2,2.79503916999998));
#196877=CARTESIAN_POINT('Ctrl Pts',(10.0609005839999,11.6,2.79503916999998));
#196878=CARTESIAN_POINT('Ctrl Pts',(10.0595015889999,15.2,2.79485724899998));
#196879=CARTESIAN_POINT('Ctrl Pts',(10.0595015889999,11.6,2.79485724899998));
#196880=CARTESIAN_POINT('Ctrl Pts',(10.0581110159999,15.2,2.79467506799998));
#196881=CARTESIAN_POINT('Ctrl Pts',(10.0581110159999,11.6,2.79467506799998));
#196882=CARTESIAN_POINT('Ctrl Pts',(10.0567288819999,15.2,2.79449264599998));
#196883=CARTESIAN_POINT('Ctrl Pts',(10.0567288819999,11.6,2.79449264599998));
#196884=CARTESIAN_POINT('Ctrl Pts',(10.0553552059999,15.2,2.79430999899999));
#196885=CARTESIAN_POINT('Ctrl Pts',(10.0553552059999,11.6,2.79430999899999));
#196886=CARTESIAN_POINT('Ctrl Pts',(10.0539900079999,15.2,2.79412714599999));
#196887=CARTESIAN_POINT('Ctrl Pts',(10.0539900079999,11.6,2.79412714599999));
#196888=CARTESIAN_POINT('Ctrl Pts',(10.0526333059999,15.2,2.79394410499999));
#196889=CARTESIAN_POINT('Ctrl Pts',(10.0526333059999,11.6,2.79394410499999));
#196890=CARTESIAN_POINT('Ctrl Pts',(10.0512851199999,15.2,2.79376089299999));
#196891=CARTESIAN_POINT('Ctrl Pts',(10.0512851199999,11.6,2.79376089299999));
#196892=CARTESIAN_POINT('Ctrl Pts',(10.0499454679999,15.2,2.79357752799999));
#196893=CARTESIAN_POINT('Ctrl Pts',(10.0499454679999,11.6,2.79357752799999));
#196894=CARTESIAN_POINT('Ctrl Pts',(10.0486143699999,15.2,2.79339402899998));
#196895=CARTESIAN_POINT('Ctrl Pts',(10.0486143699999,11.6,2.79339402899998));
#196896=CARTESIAN_POINT('Ctrl Pts',(10.0472918449999,15.2,2.79321041199999));
#196897=CARTESIAN_POINT('Ctrl Pts',(10.0472918449999,11.6,2.79321041199999));
#196898=CARTESIAN_POINT('Ctrl Pts',(10.0459779129999,15.2,2.79302669599998));
#196899=CARTESIAN_POINT('Ctrl Pts',(10.0459779129999,11.6,2.79302669599998));
#196900=CARTESIAN_POINT('Ctrl Pts',(10.0446725919999,15.2,2.79284289899999));
#196901=CARTESIAN_POINT('Ctrl Pts',(10.0446725919999,11.6,2.79284289899999));
#196902=CARTESIAN_POINT('Ctrl Pts',(10.0433759029999,15.2,2.79265903999999));
#196903=CARTESIAN_POINT('Ctrl Pts',(10.0433759029999,11.6,2.79265903999998));
#196904=CARTESIAN_POINT('Ctrl Pts',(10.0420878649999,15.2,2.79247513699998));
#196905=CARTESIAN_POINT('Ctrl Pts',(10.0420878649999,11.6,2.79247513699998));
#196906=CARTESIAN_POINT('Ctrl Pts',(10.0408084969999,15.2,2.79229120899998));
#196907=CARTESIAN_POINT('Ctrl Pts',(10.0408084969999,11.6,2.79229120899998));
#196908=CARTESIAN_POINT('Ctrl Pts',(10.0395378199999,15.2,2.79210727399998));
#196909=CARTESIAN_POINT('Ctrl Pts',(10.0395378199999,11.6,2.79210727399998));
#196910=CARTESIAN_POINT('Ctrl Pts',(10.0382758529999,15.2,2.79192334999999));
#196911=CARTESIAN_POINT('Ctrl Pts',(10.0382758529999,11.6,2.79192334999998));
#196912=CARTESIAN_POINT('Ctrl Pts',(10.0370226159999,15.2,2.79173945599998));
#196913=CARTESIAN_POINT('Ctrl Pts',(10.0370226159999,11.6,2.79173945599998));
#196914=CARTESIAN_POINT('Ctrl Pts',(10.0357781289999,15.2,2.79155561199998));
#196915=CARTESIAN_POINT('Ctrl Pts',(10.0357781289999,11.6,2.79155561199998));
#196916=CARTESIAN_POINT('Ctrl Pts',(10.0345424119999,15.2,2.79137183599998));
#196917=CARTESIAN_POINT('Ctrl Pts',(10.0345424119999,11.6,2.79137183599998));
#196918=CARTESIAN_POINT('Ctrl Pts',(10.0333154849999,15.2,2.79118814799999));
#196919=CARTESIAN_POINT('Ctrl Pts',(10.0333154849999,11.6,2.79118814799999));
#196920=CARTESIAN_POINT('Ctrl Pts',(10.0320973689999,15.2,2.79100456599998));
#196921=CARTESIAN_POINT('Ctrl Pts',(10.0320973689999,11.6,2.79100456599998));
#196922=CARTESIAN_POINT('Ctrl Pts',(10.0308880829999,15.2,2.79082110899999));
#196923=CARTESIAN_POINT('Ctrl Pts',(10.0308880829999,11.6,2.79082110899999));
#196924=CARTESIAN_POINT('Ctrl Pts',(10.0296876489999,15.2,2.79063779799999));
#196925=CARTESIAN_POINT('Ctrl Pts',(10.0296876489999,11.6,2.79063779799999));
#196926=CARTESIAN_POINT('Ctrl Pts',(10.0284960859999,15.2,2.79045464999999));
#196927=CARTESIAN_POINT('Ctrl Pts',(10.0284960859999,11.6,2.79045464999999));
#196928=CARTESIAN_POINT('Ctrl Pts',(10.0273134139999,15.2,2.79027168599999));
#196929=CARTESIAN_POINT('Ctrl Pts',(10.0273134139999,11.6,2.79027168599998));
#196930=CARTESIAN_POINT('Ctrl Pts',(10.0261396569999,15.2,2.79008892699999));
#196931=CARTESIAN_POINT('Ctrl Pts',(10.0261396569999,11.6,2.79008892699998));
#196932=CARTESIAN_POINT('Ctrl Pts',(10.0249748309999,15.2,2.78990638999999));
#196933=CARTESIAN_POINT('Ctrl Pts',(10.0249748309999,11.6,2.78990638999998));
#196934=CARTESIAN_POINT('Ctrl Pts',(10.0238189609999,15.2,2.78972409599999));
#196935=CARTESIAN_POINT('Ctrl Pts',(10.0238189609999,11.6,2.78972409599999));
#196936=CARTESIAN_POINT('Ctrl Pts',(10.0226720649999,15.2,2.78954206499999));
#196937=CARTESIAN_POINT('Ctrl Pts',(10.0226720649999,11.6,2.78954206499999));
#196938=CARTESIAN_POINT('Ctrl Pts',(10.0215341659999,15.2,2.78936031699998));
#196939=CARTESIAN_POINT('Ctrl Pts',(10.0215341659999,11.6,2.78936031699998));
#196940=CARTESIAN_POINT('Ctrl Pts',(10.0204052839999,15.2,2.78917887199999));
#196941=CARTESIAN_POINT('Ctrl Pts',(10.0204052839999,11.6,2.78917887199999));
#196942=CARTESIAN_POINT('Ctrl Pts',(10.0192854389999,15.2,2.78899774999999));
#196943=CARTESIAN_POINT('Ctrl Pts',(10.0192854389999,11.6,2.78899774999999));
#196944=CARTESIAN_POINT('Ctrl Pts',(10.0181746539999,15.2,2.78881697199999));
#196945=CARTESIAN_POINT('Ctrl Pts',(10.0181746539999,11.6,2.78881697199999));
#196946=CARTESIAN_POINT('Ctrl Pts',(10.0170729509999,15.2,2.78863655799999));
#196947=CARTESIAN_POINT('Ctrl Pts',(10.0170729509999,11.6,2.78863655799999));
#196948=CARTESIAN_POINT('Ctrl Pts',(10.0159803479999,15.2,2.78845652899999));
#196949=CARTESIAN_POINT('Ctrl Pts',(10.0159803479999,11.6,2.78845652899999));
#196950=CARTESIAN_POINT('Ctrl Pts',(10.0148968709999,15.2,2.78827690399999));
#196951=CARTESIAN_POINT('Ctrl Pts',(10.0148968709999,11.6,2.78827690399999));
#196952=CARTESIAN_POINT('Ctrl Pts',(10.0138225379999,15.2,2.78809770699999));
#196953=CARTESIAN_POINT('Ctrl Pts',(10.0138225379999,11.6,2.78809770699999));
#196954=CARTESIAN_POINT('Ctrl Pts',(10.0127573729999,15.2,2.78791895599999));
#196955=CARTESIAN_POINT('Ctrl Pts',(10.0127573729999,11.6,2.78791895599999));
#196956=CARTESIAN_POINT('Ctrl Pts',(10.0117013959999,15.2,2.78774067199999));
#196957=CARTESIAN_POINT('Ctrl Pts',(10.0117013959999,11.6,2.78774067199999));
#196958=CARTESIAN_POINT('Ctrl Pts',(10.0106546299999,15.2,2.78756287699998));
#196959=CARTESIAN_POINT('Ctrl Pts',(10.0106546299999,11.6,2.78756287699998));
#196960=CARTESIAN_POINT('Ctrl Pts',(10.0096170959999,15.2,2.78738559299998));
#196961=CARTESIAN_POINT('Ctrl Pts',(10.0096170959999,11.6,2.78738559299998));
#196962=CARTESIAN_POINT('Ctrl Pts',(10.0085888169999,15.2,2.78720884099998));
#196963=CARTESIAN_POINT('Ctrl Pts',(10.0085888169999,11.6,2.78720884099998));
#196964=CARTESIAN_POINT('Ctrl Pts',(10.0075698159999,15.2,2.78703263999999));
#196965=CARTESIAN_POINT('Ctrl Pts',(10.0075698159999,11.6,2.78703263999999));
#196966=CARTESIAN_POINT('Ctrl Pts',(10.0065601129999,15.2,2.78685701499998));
#196967=CARTESIAN_POINT('Ctrl Pts',(10.0065601129999,11.6,2.78685701499998));
#196968=CARTESIAN_POINT('Ctrl Pts',(10.0055597309999,15.2,2.78668198499999));
#196969=CARTESIAN_POINT('Ctrl Pts',(10.0055597309999,11.6,2.78668198499999));
#196970=CARTESIAN_POINT('Ctrl Pts',(10.0045686949999,15.2,2.78650757299998));
#196971=CARTESIAN_POINT('Ctrl Pts',(10.0045686949999,11.6,2.78650757299998));
#196972=CARTESIAN_POINT('Ctrl Pts',(10.0035870229999,15.2,2.78633380099999));
#196973=CARTESIAN_POINT('Ctrl Pts',(10.0035870229999,11.6,2.78633380099999));
#196974=CARTESIAN_POINT('Ctrl Pts',(10.0026147409999,15.2,2.78616069099999));
#196975=CARTESIAN_POINT('Ctrl Pts',(10.0026147409999,11.6,2.78616069099999));
#196976=CARTESIAN_POINT('Ctrl Pts',(10.0016518709999,15.2,2.78598826499999));
#196977=CARTESIAN_POINT('Ctrl Pts',(10.0016518709999,11.6,2.78598826499999));
#196978=CARTESIAN_POINT('Ctrl Pts',(10.0006984369999,15.2,2.78581654399999));
#196979=CARTESIAN_POINT('Ctrl Pts',(10.0006984369999,11.6,2.78581654399999));
#196980=CARTESIAN_POINT('Ctrl Pts',(9.99975445999995,15.2,2.78564555199999));
#196981=CARTESIAN_POINT('Ctrl Pts',(9.99975445999995,11.6,2.78564555199999));
#196982=CARTESIAN_POINT('Ctrl Pts',(9.99881996399995,15.2,2.78547531199998));
#196983=CARTESIAN_POINT('Ctrl Pts',(9.99881996399995,11.6,2.78547531199998));
#196984=CARTESIAN_POINT('Ctrl Pts',(9.99789497199994,15.2,2.78530584299999));
#196985=CARTESIAN_POINT('Ctrl Pts',(9.99789497199994,11.6,2.78530584299999));
#196986=CARTESIAN_POINT('Ctrl Pts',(9.99697950699994,15.2,2.78513717199999));
#196987=CARTESIAN_POINT('Ctrl Pts',(9.99697950699994,11.6,2.78513717199999));
#196988=CARTESIAN_POINT('Ctrl Pts',(9.99607881099994,15.2,2.78497028699999));
#196989=CARTESIAN_POINT('Ctrl Pts',(9.99607881099994,11.6,2.78497028699999));
#196990=CARTESIAN_POINT('Ctrl Pts',(9.99536684599994,15.2,2.78483763599999));
#196991=CARTESIAN_POINT('Ctrl Pts',(9.99536684599994,11.6,2.78483763599999));
#196992=CARTESIAN_POINT('Ctrl Pts',(9.99483839999994,15.2,2.78473876999998));
#196993=CARTESIAN_POINT('Ctrl Pts',(9.99483839999994,11.6,2.78473876999998));
#196994=CARTESIAN_POINT('Ctrl Pts',(9.99448967699994,15.2,2.78467334899998));
#196995=CARTESIAN_POINT('Ctrl Pts',(9.99448967699994,11.6,2.78467334899998));
#196996=CARTESIAN_POINT('Ctrl Pts',(9.99431831699994,15.2,2.78464115899999));
#196997=CARTESIAN_POINT('Ctrl Pts',(9.99431831699994,11.6,2.78464115899998));
#196998=CARTESIAN_POINT('',(9.99431831699994,12.2,2.78464115899999));
#196999=CARTESIAN_POINT('',(9.99431831699994,15.2,2.78464115899999));
#197000=CARTESIAN_POINT('',(9.99431831699994,12.2,2.78464115899999));
#197001=CARTESIAN_POINT('Ctrl Pts',(11.1757778679999,12.2,2.71145515299998));
#197002=CARTESIAN_POINT('Ctrl Pts',(11.1750309949999,12.2,2.71161876799999));
#197003=CARTESIAN_POINT('Ctrl Pts',(11.1735376169999,12.2,2.71194562399998));
#197004=CARTESIAN_POINT('Ctrl Pts',(11.1712986599999,12.2,2.71243477999998));
#197005=CARTESIAN_POINT('Ctrl Pts',(11.1683155989999,12.2,2.71308473599999));
#197006=CARTESIAN_POINT('Ctrl Pts',(11.1645904639999,12.2,2.71389342499998));
#197007=CARTESIAN_POINT('Ctrl Pts',(11.1608690239999,12.2,2.71469835899998));
#197008=CARTESIAN_POINT('Ctrl Pts',(11.1571512799999,12.2,2.71549953899999));
#197009=CARTESIAN_POINT('Ctrl Pts',(11.1534372359999,12.2,2.71629696699998));
#197010=CARTESIAN_POINT('Ctrl Pts',(11.1497268969999,12.2,2.71709064499999));
#197011=CARTESIAN_POINT('Ctrl Pts',(11.1460202709999,12.2,2.71788057599998));
#197012=CARTESIAN_POINT('Ctrl Pts',(11.1423173659999,12.2,2.71866676499998));
#197013=CARTESIAN_POINT('Ctrl Pts',(11.1386181909999,12.2,2.71944921899999));
#197014=CARTESIAN_POINT('Ctrl Pts',(11.1349227589999,12.2,2.72022793899998));
#197015=CARTESIAN_POINT('Ctrl Pts',(11.1312310749999,12.2,2.72100293299999));
#197016=CARTESIAN_POINT('Ctrl Pts',(11.1275431529999,12.2,2.72177420499998));
#197017=CARTESIAN_POINT('Ctrl Pts',(11.1238589999999,12.2,2.72254175699998));
#197018=CARTESIAN_POINT('Ctrl Pts',(11.1201786229999,12.2,2.72330559599999));
#197019=CARTESIAN_POINT('Ctrl Pts',(11.1165020289999,12.2,2.72406572399999));
#197020=CARTESIAN_POINT('Ctrl Pts',(11.1128292269999,12.2,2.72482214499998));
#197021=CARTESIAN_POINT('Ctrl Pts',(11.1091602219999,12.2,2.72557486299998));
#197022=CARTESIAN_POINT('Ctrl Pts',(11.1054950239999,12.2,2.72632388099999));
#197023=CARTESIAN_POINT('Ctrl Pts',(11.1018336399999,12.2,2.72706920299999));
#197024=CARTESIAN_POINT('Ctrl Pts',(11.0981760779999,12.2,2.72781083499999));
#197025=CARTESIAN_POINT('Ctrl Pts',(11.0945223469999,12.2,2.72854877899999));
#197026=CARTESIAN_POINT('Ctrl Pts',(11.0908724549999,12.2,2.72928304099998));
#197027=CARTESIAN_POINT('Ctrl Pts',(11.0872264109999,12.2,2.73001362299999));
#197028=CARTESIAN_POINT('Ctrl Pts',(11.0835842229999,12.2,2.73074053299998));
#197029=CARTESIAN_POINT('Ctrl Pts',(11.0799458989999,12.2,2.73146377099999));
#197030=CARTESIAN_POINT('Ctrl Pts',(11.0763114489999,12.2,2.73218334499998));
#197031=CARTESIAN_POINT('Ctrl Pts',(11.0726808779999,12.2,2.73289925699999));
#197032=CARTESIAN_POINT('Ctrl Pts',(11.0690541959999,12.2,2.73361151099999));
#197033=CARTESIAN_POINT('Ctrl Pts',(11.0654314099999,12.2,2.73432011199999));
#197034=CARTESIAN_POINT('Ctrl Pts',(11.0618125299999,12.2,2.73502506399999));
#197035=CARTESIAN_POINT('Ctrl Pts',(11.0581975619999,12.2,2.73572636999998));
#197036=CARTESIAN_POINT('Ctrl Pts',(11.0545865169999,12.2,2.73642403699998));
#197037=CARTESIAN_POINT('Ctrl Pts',(11.0509794009999,12.2,2.73711806699998));
#197038=CARTESIAN_POINT('Ctrl Pts',(11.0473762219999,12.2,2.73780846599998));
#197039=CARTESIAN_POINT('Ctrl Pts',(11.0437769909999,12.2,2.73849523599999));
#197040=CARTESIAN_POINT('Ctrl Pts',(11.0401817149999,12.2,2.73917838399999));
#197041=CARTESIAN_POINT('Ctrl Pts',(11.0365903999999,12.2,2.73985791299998));
#197042=CARTESIAN_POINT('Ctrl Pts',(11.0330030589999,12.2,2.74053382799998));
#197043=CARTESIAN_POINT('Ctrl Pts',(11.0294196959999,12.2,2.74120613199998));
#197044=CARTESIAN_POINT('Ctrl Pts',(11.0258403219999,12.2,2.74187483099999));
#197045=CARTESIAN_POINT('Ctrl Pts',(11.0222649439999,12.2,2.74253992799999));
#197046=CARTESIAN_POINT('Ctrl Pts',(11.0186935709999,12.2,2.74320142899998));
#197047=CARTESIAN_POINT('Ctrl Pts',(11.0151262099999,12.2,2.74385933599999));
#197048=CARTESIAN_POINT('Ctrl Pts',(11.0115628719999,12.2,2.74451365599998));
#197049=CARTESIAN_POINT('Ctrl Pts',(11.0080035629999,12.2,2.74516439199999));
#197050=CARTESIAN_POINT('Ctrl Pts',(11.0044482939999,12.2,2.74581154899998));
#197051=CARTESIAN_POINT('Ctrl Pts',(11.0008970699999,12.2,2.74645513199999));
#197052=CARTESIAN_POINT('Ctrl Pts',(10.9973499019999,12.2,2.74709514499998));
#197053=CARTESIAN_POINT('Ctrl Pts',(10.9938067979999,12.2,2.74773159199999));
#197054=CARTESIAN_POINT('Ctrl Pts',(10.9902677649999,12.2,2.74836447799998));
#197055=CARTESIAN_POINT('Ctrl Pts',(10.9867328139999,12.2,2.74899380799998));
#197056=CARTESIAN_POINT('Ctrl Pts',(10.9832019509999,12.2,2.74961958599999));
#197057=CARTESIAN_POINT('Ctrl Pts',(10.9796751869999,12.2,2.75024181699998));
#197058=CARTESIAN_POINT('Ctrl Pts',(10.9761525279999,12.2,2.75086050399998));
#197059=CARTESIAN_POINT('Ctrl Pts',(10.9726339839999,12.2,2.75147565399998));
#197060=CARTESIAN_POINT('Ctrl Pts',(10.9691195629999,12.2,2.75208726999999));
#197061=CARTESIAN_POINT('Ctrl Pts',(10.9656092739999,12.2,2.75269535799998));
#197062=CARTESIAN_POINT('Ctrl Pts',(10.9621031259999,12.2,2.75329992099999));
#197063=CARTESIAN_POINT('Ctrl Pts',(10.9586011259999,12.2,2.75390096599998));
#197064=CARTESIAN_POINT('Ctrl Pts',(10.9551032829999,12.2,2.75449849499999));
#197065=CARTESIAN_POINT('Ctrl Pts',(10.9516096059999,12.2,2.75509251399999));
#197066=CARTESIAN_POINT('Ctrl Pts',(10.9481201049999,12.2,2.75568302799999));
#197067=CARTESIAN_POINT('Ctrl Pts',(10.9446347859999,12.2,2.75627004099999));
#197068=CARTESIAN_POINT('Ctrl Pts',(10.9411536579999,12.2,2.75685355899999));
#197069=CARTESIAN_POINT('Ctrl Pts',(10.9376767319999,12.2,2.75743358499999));
#197070=CARTESIAN_POINT('Ctrl Pts',(10.9342040149999,12.2,2.75801012499999));
#197071=CARTESIAN_POINT('Ctrl Pts',(10.9307355149999,12.2,2.75858318399998));
#197072=CARTESIAN_POINT('Ctrl Pts',(10.9272712419999,12.2,2.75915276599999));
#197073=CARTESIAN_POINT('Ctrl Pts',(10.9238112039999,12.2,2.75971887599999));
#197074=CARTESIAN_POINT('Ctrl Pts',(10.9203554099999,12.2,2.76028151899999));
#197075=CARTESIAN_POINT('Ctrl Pts',(10.9169038679999,12.2,2.76084069999998));
#197076=CARTESIAN_POINT('Ctrl Pts',(10.9134565879999,12.2,2.76139642399999));
#197077=CARTESIAN_POINT('Ctrl Pts',(10.9100135769999,12.2,2.76194869599999));
#197078=CARTESIAN_POINT('Ctrl Pts',(10.9065748449999,12.2,2.76249751999998));
#197079=CARTESIAN_POINT('Ctrl Pts',(10.9031404009999,12.2,2.76304290199998));
#197080=CARTESIAN_POINT('Ctrl Pts',(10.8997102529999,12.2,2.76358484599999));
#197081=CARTESIAN_POINT('Ctrl Pts',(10.8962844109999,12.2,2.76412335799999));
#197082=CARTESIAN_POINT('Ctrl Pts',(10.8928628809999,12.2,2.76465844099998));
#197083=CARTESIAN_POINT('Ctrl Pts',(10.8894456749999,12.2,2.76519010299998));
#197084=CARTESIAN_POINT('Ctrl Pts',(10.8860327999999,12.2,2.76571834699999));
#197085=CARTESIAN_POINT('Ctrl Pts',(10.8826242649999,12.2,2.76624317899999));
#197086=CARTESIAN_POINT('Ctrl Pts',(10.8792200789999,12.2,2.76676460199998));
#197087=CARTESIAN_POINT('Ctrl Pts',(10.8758202519999,12.2,2.76728262299999));
#197088=CARTESIAN_POINT('Ctrl Pts',(10.8724247909999,12.2,2.76779724699999));
#197089=CARTESIAN_POINT('Ctrl Pts',(10.8690337059999,12.2,2.76830847799998));
#197090=CARTESIAN_POINT('Ctrl Pts',(10.8656470049999,12.2,2.76881632399999));
#197091=CARTESIAN_POINT('Ctrl Pts',(10.8622646979999,12.2,2.76932078499998));
#197092=CARTESIAN_POINT('Ctrl Pts',(10.8588867929999,12.2,2.76982187099998));
#197093=CARTESIAN_POINT('Ctrl Pts',(10.8555133009999,12.2,2.77031958499999));
#197094=CARTESIAN_POINT('Ctrl Pts',(10.8521442279999,12.2,2.77081393199998));
#197095=CARTESIAN_POINT('Ctrl Pts',(10.8487795839999,12.2,2.77130491799999));
#197096=CARTESIAN_POINT('Ctrl Pts',(10.8454193789999,12.2,2.77179254799999));
#197097=CARTESIAN_POINT('Ctrl Pts',(10.8420636209999,12.2,2.77227682699999));
#197098=CARTESIAN_POINT('Ctrl Pts',(10.8387123189999,12.2,2.77275775999998));
#197099=CARTESIAN_POINT('Ctrl Pts',(10.8353654819999,12.2,2.77323535299999));
#197100=CARTESIAN_POINT('Ctrl Pts',(10.8320231199999,12.2,2.77370960999999));
#197101=CARTESIAN_POINT('Ctrl Pts',(10.8286852409999,12.2,2.77418053799998));
#197102=CARTESIAN_POINT('Ctrl Pts',(10.8253518549999,12.2,2.77464814099999));
#197103=CARTESIAN_POINT('Ctrl Pts',(10.8220229679999,12.2,2.77511242599999));
#197104=CARTESIAN_POINT('Ctrl Pts',(10.8186985939999,12.2,2.77557339599999));
#197105=CARTESIAN_POINT('Ctrl Pts',(10.8153787389999,12.2,2.77603105699999));
#197106=CARTESIAN_POINT('Ctrl Pts',(10.8120634119999,12.2,2.77648541599999));
#197107=CARTESIAN_POINT('Ctrl Pts',(10.8087526239999,12.2,2.77693647799998));
#197108=CARTESIAN_POINT('Ctrl Pts',(10.8054463819999,12.2,2.77738424699999));
#197109=CARTESIAN_POINT('Ctrl Pts',(10.8021446959999,12.2,2.77782872899999));
#197110=CARTESIAN_POINT('Ctrl Pts',(10.7988475759999,12.2,2.77826992999999));
#197111=CARTESIAN_POINT('Ctrl Pts',(10.7955550299999,12.2,2.77870785499999));
#197112=CARTESIAN_POINT('Ctrl Pts',(10.7922670679999,12.2,2.77914250999999));
#197113=CARTESIAN_POINT('Ctrl Pts',(10.7889836979999,12.2,2.77957390099999));
#197114=CARTESIAN_POINT('Ctrl Pts',(10.7857049309999,12.2,2.78000203199999));
#197115=CARTESIAN_POINT('Ctrl Pts',(10.7824307749999,12.2,2.78042690799998));
#197116=CARTESIAN_POINT('Ctrl Pts',(10.7791612379999,12.2,2.78084853699998));
#197117=CARTESIAN_POINT('Ctrl Pts',(10.7758963329999,12.2,2.78126692399999));
#197118=CARTESIAN_POINT('Ctrl Pts',(10.7726360659999,12.2,2.78168207299998));
#197119=CARTESIAN_POINT('Ctrl Pts',(10.7693804469999,12.2,2.78209399099998));
#197120=CARTESIAN_POINT('Ctrl Pts',(10.7661294859999,12.2,2.78250268399999));
#197121=CARTESIAN_POINT('Ctrl Pts',(10.7628831919999,12.2,2.78290815599998));
#197122=CARTESIAN_POINT('Ctrl Pts',(10.7596415739999,12.2,2.78331041399999));
#197123=CARTESIAN_POINT('Ctrl Pts',(10.7564046409999,12.2,2.78370946299999));
#197124=CARTESIAN_POINT('Ctrl Pts',(10.7531724039999,12.2,2.78410530999999));
#197125=CARTESIAN_POINT('Ctrl Pts',(10.7499448709999,12.2,2.78449795899999));
#197126=CARTESIAN_POINT('Ctrl Pts',(10.7467220519999,12.2,2.78488741599999));
#197127=CARTESIAN_POINT('Ctrl Pts',(10.7435039549999,12.2,2.78527368799999));
#197128=CARTESIAN_POINT('Ctrl Pts',(10.7402905919999,12.2,2.78565678199998));
#197129=CARTESIAN_POINT('Ctrl Pts',(10.7370819699999,12.2,2.78603669899999));
#197130=CARTESIAN_POINT('Ctrl Pts',(10.7338780989999,12.2,2.78641344999999));
#197131=CARTESIAN_POINT('Ctrl Pts',(10.7306789899999,12.2,2.78678703799999));
#197132=CARTESIAN_POINT('Ctrl Pts',(10.7274846509999,12.2,2.78715746999998));
#197133=CARTESIAN_POINT('Ctrl Pts',(10.7242950909999,12.2,2.78752475099999));
#197134=CARTESIAN_POINT('Ctrl Pts',(10.7211103209999,12.2,2.78788888599999));
#197135=CARTESIAN_POINT('Ctrl Pts',(10.7179303499999,12.2,2.78824988399998));
#197136=CARTESIAN_POINT('Ctrl Pts',(10.7147551869999,12.2,2.78860774899999));
#197137=CARTESIAN_POINT('Ctrl Pts',(10.7115848429999,12.2,2.78896248699999));
#197138=CARTESIAN_POINT('Ctrl Pts',(10.7084193239999,12.2,2.78931410399998));
#197139=CARTESIAN_POINT('Ctrl Pts',(10.7052586439999,12.2,2.78966260699999));
#197140=CARTESIAN_POINT('Ctrl Pts',(10.7021028099999,12.2,2.79000799999999));
#197141=CARTESIAN_POINT('Ctrl Pts',(10.6989518329999,12.2,2.79035029099998));
#197142=CARTESIAN_POINT('Ctrl Pts',(10.6958057219999,12.2,2.79068948499999));
#197143=CARTESIAN_POINT('Ctrl Pts',(10.6926644859999,12.2,2.79102558999998));
#197144=CARTESIAN_POINT('Ctrl Pts',(10.6895281349999,12.2,2.79135860899999));
#197145=CARTESIAN_POINT('Ctrl Pts',(10.6863966799999,12.2,2.79168855099999));
#197146=CARTESIAN_POINT('Ctrl Pts',(10.6832701279999,12.2,2.79201541999999));
#197147=CARTESIAN_POINT('Ctrl Pts',(10.6801484919999,12.2,2.79233922399998));
#197148=CARTESIAN_POINT('Ctrl Pts',(10.6770317779999,12.2,2.79265996699999));
#197149=CARTESIAN_POINT('Ctrl Pts',(10.6739199989999,12.2,2.79297765699998));
#197150=CARTESIAN_POINT('Ctrl Pts',(10.6708131629999,12.2,2.79329229999998));
#197151=CARTESIAN_POINT('Ctrl Pts',(10.6677112809999,12.2,2.79360390199999));
#197152=CARTESIAN_POINT('Ctrl Pts',(10.6646143609999,12.2,2.79391246899999));
#197153=CARTESIAN_POINT('Ctrl Pts',(10.6615224159999,12.2,2.79421800799999));
#197154=CARTESIAN_POINT('Ctrl Pts',(10.6584354509999,12.2,2.79452052399999));
#197155=CARTESIAN_POINT('Ctrl Pts',(10.6553534799999,12.2,2.79482002499999));
#197156=CARTESIAN_POINT('Ctrl Pts',(10.6522765109999,12.2,2.79511651699998));
#197157=CARTESIAN_POINT('Ctrl Pts',(10.6492045549999,12.2,2.79541000599998));
#197158=CARTESIAN_POINT('Ctrl Pts',(10.6461376199999,12.2,2.79570049699998));
#197159=CARTESIAN_POINT('Ctrl Pts',(10.6430757179999,12.2,2.79598799899999));
#197160=CARTESIAN_POINT('Ctrl Pts',(10.6400188569999,12.2,2.79627251799998));
#197161=CARTESIAN_POINT('Ctrl Pts',(10.6369670479999,12.2,2.79655405899998));
#197162=CARTESIAN_POINT('Ctrl Pts',(10.6339203009999,12.2,2.79683262899999));
#197163=CARTESIAN_POINT('Ctrl Pts',(10.6308786259999,12.2,2.79710823499999));
#197164=CARTESIAN_POINT('Ctrl Pts',(10.6278420329999,12.2,2.79738088399998));
#197165=CARTESIAN_POINT('Ctrl Pts',(10.6248105309999,12.2,2.79765058099999));
#197166=CARTESIAN_POINT('Ctrl Pts',(10.6217841319999,12.2,2.79791733399998));
#197167=CARTESIAN_POINT('Ctrl Pts',(10.6187628439999,12.2,2.79818114899999));
#197168=CARTESIAN_POINT('Ctrl Pts',(10.6157466779999,12.2,2.79844203299999));
#197169=CARTESIAN_POINT('Ctrl Pts',(10.6127356429999,12.2,2.79869999199998));
#197170=CARTESIAN_POINT('Ctrl Pts',(10.6097297519999,12.2,2.79895503299999));
#197171=CARTESIAN_POINT('Ctrl Pts',(10.6067290119999,12.2,2.79920716299999));
#197172=CARTESIAN_POINT('Ctrl Pts',(10.6037334349999,12.2,2.79945638899999));
#197173=CARTESIAN_POINT('Ctrl Pts',(10.6007430289999,12.2,2.79970271699998));
#197174=CARTESIAN_POINT('Ctrl Pts',(10.5977578069999,12.2,2.79994615399998));
#197175=CARTESIAN_POINT('Ctrl Pts',(10.5947777769999,12.2,2.80018670699998));
#197176=CARTESIAN_POINT('Ctrl Pts',(10.5918029509999,12.2,2.80042438199998));
#197177=CARTESIAN_POINT('Ctrl Pts',(10.5888333369999,12.2,2.80065918699999));
#197178=CARTESIAN_POINT('Ctrl Pts',(10.5858689469999,12.2,2.80089112799998));
#197179=CARTESIAN_POINT('Ctrl Pts',(10.5829097899999,12.2,2.80112021299999));
#197180=CARTESIAN_POINT('Ctrl Pts',(10.5799558779999,12.2,2.80134644699999));
#197181=CARTESIAN_POINT('Ctrl Pts',(10.5770072199999,12.2,2.80156983799999));
#197182=CARTESIAN_POINT('Ctrl Pts',(10.5740638259999,12.2,2.80179039399999));
#197183=CARTESIAN_POINT('Ctrl Pts',(10.5711257059999,12.2,2.80200812099999));
#197184=CARTESIAN_POINT('Ctrl Pts',(10.5681928729999,12.2,2.80222302499999));
#197185=CARTESIAN_POINT('Ctrl Pts',(10.5652653349999,12.2,2.80243511499998));
#197186=CARTESIAN_POINT('Ctrl Pts',(10.5623431029999,12.2,2.80264439699998));
#197187=CARTESIAN_POINT('Ctrl Pts',(10.5594261859999,12.2,2.80285087799999));
#197188=CARTESIAN_POINT('Ctrl Pts',(10.5565145969999,12.2,2.80305456499998));
#197189=CARTESIAN_POINT('Ctrl Pts',(10.5536083449999,12.2,2.80325546599999));
#197190=CARTESIAN_POINT('Ctrl Pts',(10.5507074409999,12.2,2.80345358699999));
#197191=CARTESIAN_POINT('Ctrl Pts',(10.5478118939999,12.2,2.80364893599998));
#197192=CARTESIAN_POINT('Ctrl Pts',(10.5449217159999,12.2,2.80384151899998));
#197193=CARTESIAN_POINT('Ctrl Pts',(10.5420369179999,12.2,2.80403134499998));
#197194=CARTESIAN_POINT('Ctrl Pts',(10.5391575079999,12.2,2.80421842099998));
#197195=CARTESIAN_POINT('Ctrl Pts',(10.5362834999999,12.2,2.80440275299998));
#197196=CARTESIAN_POINT('Ctrl Pts',(10.5334149019999,12.2,2.80458434899998));
#197197=CARTESIAN_POINT('Ctrl Pts',(10.5305517249999,12.2,2.80476321599998));
#197198=CARTESIAN_POINT('Ctrl Pts',(10.5276939799999,12.2,2.80493936099998));
#197199=CARTESIAN_POINT('Ctrl Pts',(10.5248416769999,12.2,2.80511279299999));
#197200=CARTESIAN_POINT('Ctrl Pts',(10.5219948289999,12.2,2.80528351899999));
#197201=CARTESIAN_POINT('Ctrl Pts',(10.5191534429999,12.2,2.80545154499999));
#197202=CARTESIAN_POINT('Ctrl Pts',(10.5163175329999,12.2,2.80561687899999));
#197203=CARTESIAN_POINT('Ctrl Pts',(10.5134871079999,12.2,2.80577952899999));
#197204=CARTESIAN_POINT('Ctrl Pts',(10.5106621789999,12.2,2.80593950299998));
#197205=CARTESIAN_POINT('Ctrl Pts',(10.5078427569999,12.2,2.80609680699998));
#197206=CARTESIAN_POINT('Ctrl Pts',(10.5050288509999,12.2,2.80625144999998));
#197207=CARTESIAN_POINT('Ctrl Pts',(10.5022204749999,12.2,2.80640343899999));
#197208=CARTESIAN_POINT('Ctrl Pts',(10.4994176369999,12.2,2.80655278099999));
#197209=CARTESIAN_POINT('Ctrl Pts',(10.4966203499999,12.2,2.80669948499998));
#197210=CARTESIAN_POINT('Ctrl Pts',(10.4938286229999,12.2,2.80684355699999));
#197211=CARTESIAN_POINT('Ctrl Pts',(10.4910424679999,12.2,2.80698500599998));
#197212=CARTESIAN_POINT('Ctrl Pts',(10.4882618969999,12.2,2.80712383899999));
#197213=CARTESIAN_POINT('Ctrl Pts',(10.4854869179999,12.2,2.80726006499999));
#197214=CARTESIAN_POINT('Ctrl Pts',(10.4827175439999,12.2,2.80739368999999));
#197215=CARTESIAN_POINT('Ctrl Pts',(10.4799537849999,12.2,2.80752472299999));
#197216=CARTESIAN_POINT('Ctrl Pts',(10.4771956519999,12.2,2.80765317099998));
#197217=CARTESIAN_POINT('Ctrl Pts',(10.4744431569999,12.2,2.80777904299998));
#197218=CARTESIAN_POINT('Ctrl Pts',(10.4716963109999,12.2,2.80790234499998));
#197219=CARTESIAN_POINT('Ctrl Pts',(10.4689551229999,12.2,2.80802308599998));
#197220=CARTESIAN_POINT('Ctrl Pts',(10.4662196059999,12.2,2.80814127499998));
#197221=CARTESIAN_POINT('Ctrl Pts',(10.4634897709999,12.2,2.80825691999999));
#197222=CARTESIAN_POINT('Ctrl Pts',(10.4607656289999,12.2,2.80837002599998));
#197223=CARTESIAN_POINT('Ctrl Pts',(10.4580471909999,12.2,2.80848060399999));
#197224=CARTESIAN_POINT('Ctrl Pts',(10.4553344669999,12.2,2.80858866099998));
#197225=CARTESIAN_POINT('Ctrl Pts',(10.4526274699999,12.2,2.80869420399998));
#197226=CARTESIAN_POINT('Ctrl Pts',(10.4499262109999,12.2,2.80879724399998));
#197227=CARTESIAN_POINT('Ctrl Pts',(10.4472306989999,12.2,2.80889778599998));
#197228=CARTESIAN_POINT('Ctrl Pts',(10.4445409479999,12.2,2.80899584099998));
#197229=CARTESIAN_POINT('Ctrl Pts',(10.4418569669999,12.2,2.80909141499999));
#197230=CARTESIAN_POINT('Ctrl Pts',(10.4391787699999,12.2,2.80918451599998));
#197231=CARTESIAN_POINT('Ctrl Pts',(10.4365063659999,12.2,2.80927515599998));
#197232=CARTESIAN_POINT('Ctrl Pts',(10.4338397659999,12.2,2.80936333799998));
#197233=CARTESIAN_POINT('Ctrl Pts',(10.4311789839999,12.2,2.80944907299999));
#197234=CARTESIAN_POINT('Ctrl Pts',(10.4285240289999,12.2,2.80953237099999));
#197235=CARTESIAN_POINT('Ctrl Pts',(10.4258749129999,12.2,2.80961323599998));
#197236=CARTESIAN_POINT('Ctrl Pts',(10.4232316479999,12.2,2.80969167999999));
#197237=CARTESIAN_POINT('Ctrl Pts',(10.4205942449999,12.2,2.80976771199998));
#197238=CARTESIAN_POINT('Ctrl Pts',(10.4179627159999,12.2,2.80984133699998));
#197239=CARTESIAN_POINT('Ctrl Pts',(10.4153370719999,12.2,2.80991256599999));
#197240=CARTESIAN_POINT('Ctrl Pts',(10.4127173239999,12.2,2.80998140599999));
#197241=CARTESIAN_POINT('Ctrl Pts',(10.4101034849999,12.2,2.81004786799999));
#197242=CARTESIAN_POINT('Ctrl Pts',(10.4074955649999,12.2,2.81011195799999));
#197243=CARTESIAN_POINT('Ctrl Pts',(10.4048935769999,12.2,2.81017368599999));
#197244=CARTESIAN_POINT('Ctrl Pts',(10.4022975309999,12.2,2.81023305999998));
#197245=CARTESIAN_POINT('Ctrl Pts',(10.3997074399999,12.2,2.81029008999998));
#197246=CARTESIAN_POINT('Ctrl Pts',(10.3971233149999,12.2,2.81034478199999));
#197247=CARTESIAN_POINT('Ctrl Pts',(10.3945451689999,12.2,2.81039714699999));
#197248=CARTESIAN_POINT('Ctrl Pts',(10.3919730119999,12.2,2.81044719399999));
#197249=CARTESIAN_POINT('Ctrl Pts',(10.3894068559999,12.2,2.81049492999998));
#197250=CARTESIAN_POINT('Ctrl Pts',(10.3868467139999,12.2,2.81054036599999));
#197251=CARTESIAN_POINT('Ctrl Pts',(10.3842925959999,12.2,2.81058350899999));
#197252=CARTESIAN_POINT('Ctrl Pts',(10.3817445159999,12.2,2.81062436799999));
#197253=CARTESIAN_POINT('Ctrl Pts',(10.3792024839999,12.2,2.81066295399999));
#197254=CARTESIAN_POINT('Ctrl Pts',(10.3766665119999,12.2,2.81069927299999));
#197255=CARTESIAN_POINT('Ctrl Pts',(10.3741366129999,12.2,2.81073333699998));
#197256=CARTESIAN_POINT('Ctrl Pts',(10.3716127979999,12.2,2.81076515299999));
#197257=CARTESIAN_POINT('Ctrl Pts',(10.3690950799999,12.2,2.81079473099999));
#197258=CARTESIAN_POINT('Ctrl Pts',(10.3665834699999,12.2,2.81082207899999));
#197259=CARTESIAN_POINT('Ctrl Pts',(10.3640779799999,12.2,2.81084720699998));
#197260=CARTESIAN_POINT('Ctrl Pts',(10.3615786239999,12.2,2.81087012399999));
#197261=CARTESIAN_POINT('Ctrl Pts',(10.3590854099999,12.2,2.81089083999999));
#197262=CARTESIAN_POINT('Ctrl Pts',(10.3565983529999,12.2,2.81090936199998));
#197263=CARTESIAN_POINT('Ctrl Pts',(10.3541174659999,12.2,2.81092570199998));
#197264=CARTESIAN_POINT('Ctrl Pts',(10.3516427589999,12.2,2.81093986799998));
#197265=CARTESIAN_POINT('Ctrl Pts',(10.3491742439999,12.2,2.81095186899999));
#197266=CARTESIAN_POINT('Ctrl Pts',(10.3467119339999,12.2,2.81096171499998));
#197267=CARTESIAN_POINT('Ctrl Pts',(10.3442558419999,12.2,2.81096941599999));
#197268=CARTESIAN_POINT('Ctrl Pts',(10.3418059809999,12.2,2.81097497899999));
#197269=CARTESIAN_POINT('Ctrl Pts',(10.3393623599999,12.2,2.81097841599999));
#197270=CARTESIAN_POINT('Ctrl Pts',(10.3369249929999,12.2,2.81097973599999));
#197271=CARTESIAN_POINT('Ctrl Pts',(10.3344938929999,12.2,2.81097894699998));
#197272=CARTESIAN_POINT('Ctrl Pts',(10.3320690709999,12.2,2.81097606099999));
#197273=CARTESIAN_POINT('Ctrl Pts',(10.3296505419999,12.2,2.81097108499999));
#197274=CARTESIAN_POINT('Ctrl Pts',(10.3272383149999,12.2,2.81096403199999));
#197275=CARTESIAN_POINT('Ctrl Pts',(10.3248324049999,12.2,2.81095490799999));
#197276=CARTESIAN_POINT('Ctrl Pts',(10.3224328229999,12.2,2.81094372499999));
#197277=CARTESIAN_POINT('Ctrl Pts',(10.3200395829999,12.2,2.81093049299999));
#197278=CARTESIAN_POINT('Ctrl Pts',(10.3176526949999,12.2,2.81091521999999));
#197279=CARTESIAN_POINT('Ctrl Pts',(10.3152721739999,12.2,2.81089791699999));
#197280=CARTESIAN_POINT('Ctrl Pts',(10.3128980319999,12.2,2.81087859499999));
#197281=CARTESIAN_POINT('Ctrl Pts',(10.3105302809999,12.2,2.81085726199999));
#197282=CARTESIAN_POINT('Ctrl Pts',(10.3081689339999,12.2,2.81083392699998));
#197283=CARTESIAN_POINT('Ctrl Pts',(10.3058140039999,12.2,2.81080860299999));
#197284=CARTESIAN_POINT('Ctrl Pts',(10.3034655029999,12.2,2.81078129899999));
#197285=CARTESIAN_POINT('Ctrl Pts',(10.3011234449999,12.2,2.81075202499999));
#197286=CARTESIAN_POINT('Ctrl Pts',(10.2987878399999,12.2,2.81072078899999));
#197287=CARTESIAN_POINT('Ctrl Pts',(10.2964587039999,12.2,2.81068760399998));
#197288=CARTESIAN_POINT('Ctrl Pts',(10.2941360499999,12.2,2.81065247899999));
#197289=CARTESIAN_POINT('Ctrl Pts',(10.2918198869999,12.2,2.81061542499998));
#197290=CARTESIAN_POINT('Ctrl Pts',(10.2895102319999,12.2,2.81057645199999));
#197291=CARTESIAN_POINT('Ctrl Pts',(10.2872070959999,12.2,2.81053556799999));
#197292=CARTESIAN_POINT('Ctrl Pts',(10.2849104899999,12.2,2.81049278699999));
#197293=CARTESIAN_POINT('Ctrl Pts',(10.2826204319999,12.2,2.81044811699999));
#197294=CARTESIAN_POINT('Ctrl Pts',(10.2803369309999,12.2,2.81040156799998));
#197295=CARTESIAN_POINT('Ctrl Pts',(10.2780600009999,12.2,2.81035315199999));
#197296=CARTESIAN_POINT('Ctrl Pts',(10.2757896559999,12.2,2.81030288099998));
#197297=CARTESIAN_POINT('Ctrl Pts',(10.2735259089999,12.2,2.81025076199998));
#197298=CARTESIAN_POINT('Ctrl Pts',(10.2712687709999,12.2,2.81019680599999));
#197299=CARTESIAN_POINT('Ctrl Pts',(10.2690182579999,12.2,2.81014102599999));
#197300=CARTESIAN_POINT('Ctrl Pts',(10.2667743819999,12.2,2.81008343199999));
#197301=CARTESIAN_POINT('Ctrl Pts',(10.2645371559999,12.2,2.81002403399999));
#197302=CARTESIAN_POINT('Ctrl Pts',(10.2623065929999,12.2,2.80996284199999));
#197303=CARTESIAN_POINT('Ctrl Pts',(10.2600827069999,12.2,2.80989986699999));
#197304=CARTESIAN_POINT('Ctrl Pts',(10.2578655119999,12.2,2.80983512099999));
#197305=CARTESIAN_POINT('Ctrl Pts',(10.2556550209999,12.2,2.80976861599999));
#197306=CARTESIAN_POINT('Ctrl Pts',(10.2534512459999,12.2,2.80970035899998));
#197307=CARTESIAN_POINT('Ctrl Pts',(10.2512542019999,12.2,2.80963036499998));
#197308=CARTESIAN_POINT('Ctrl Pts',(10.2490639019999,12.2,2.80955864199999));
#197309=CARTESIAN_POINT('Ctrl Pts',(10.2468803589999,12.2,2.80948520299999));
#197310=CARTESIAN_POINT('Ctrl Pts',(10.2447035879999,12.2,2.80941005799999));
#197311=CARTESIAN_POINT('Ctrl Pts',(10.2425335999999,12.2,2.80933321799999));
#197312=CARTESIAN_POINT('Ctrl Pts',(10.2403704109999,12.2,2.80925469399998));
#197313=CARTESIAN_POINT('Ctrl Pts',(10.2382140349999,12.2,2.80917449999999));
#197314=CARTESIAN_POINT('Ctrl Pts',(10.2360644839999,12.2,2.80909264399998));
#197315=CARTESIAN_POINT('Ctrl Pts',(10.2339217719999,12.2,2.80900913799999));
#197316=CARTESIAN_POINT('Ctrl Pts',(10.2317859129999,12.2,2.80892399399999));
#197317=CARTESIAN_POINT('Ctrl Pts',(10.2296569209999,12.2,2.80883722299999));
#197318=CARTESIAN_POINT('Ctrl Pts',(10.2275348109999,12.2,2.80874883799999));
#197319=CARTESIAN_POINT('Ctrl Pts',(10.2254195939999,12.2,2.80865884799999));
#197320=CARTESIAN_POINT('Ctrl Pts',(10.2233112869999,12.2,2.80856726499999));
#197321=CARTESIAN_POINT('Ctrl Pts',(10.2212099009999,12.2,2.80847410299998));
#197322=CARTESIAN_POINT('Ctrl Pts',(10.2191154529999,12.2,2.80837936999998));
#197323=CARTESIAN_POINT('Ctrl Pts',(10.2170279549999,12.2,2.80828308099998));
#197324=CARTESIAN_POINT('Ctrl Pts',(10.2149474219999,12.2,2.80818524499999));
#197325=CARTESIAN_POINT('Ctrl Pts',(10.2128738679999,12.2,2.80808587499998));
#197326=CARTESIAN_POINT('Ctrl Pts',(10.2108073059999,12.2,2.80798498399999));
#197327=CARTESIAN_POINT('Ctrl Pts',(10.2087477509999,12.2,2.80788258099999));
#197328=CARTESIAN_POINT('Ctrl Pts',(10.2066952179999,12.2,2.80777868099998));
#197329=CARTESIAN_POINT('Ctrl Pts',(10.2046497199999,12.2,2.80767329399998));
#197330=CARTESIAN_POINT('Ctrl Pts',(10.2026112719999,12.2,2.80756643299998));
#197331=CARTESIAN_POINT('Ctrl Pts',(10.2005798889999,12.2,2.80745810899998));
#197332=CARTESIAN_POINT('Ctrl Pts',(10.1985555829999,12.2,2.80734833399999));
#197333=CARTESIAN_POINT('Ctrl Pts',(10.1965383709999,12.2,2.80723712199999));
#197334=CARTESIAN_POINT('Ctrl Pts',(10.1945282669999,12.2,2.80712448399999));
#197335=CARTESIAN_POINT('Ctrl Pts',(10.1925252829999,12.2,2.80701043199999));
#197336=CARTESIAN_POINT('Ctrl Pts',(10.1905294369999,12.2,2.80689497899999));
#197337=CARTESIAN_POINT('Ctrl Pts',(10.1885407419999,12.2,2.80677813699998));
#197338=CARTESIAN_POINT('Ctrl Pts',(10.1865592119999,12.2,2.80665991699999));
#197339=CARTESIAN_POINT('Ctrl Pts',(10.1845848629999,12.2,2.80654033399999));
#197340=CARTESIAN_POINT('Ctrl Pts',(10.1826177079999,12.2,2.80641939899999));
#197341=CARTESIAN_POINT('Ctrl Pts',(10.1806577639999,12.2,2.80629712499999));
#197342=CARTESIAN_POINT('Ctrl Pts',(10.1787050449999,12.2,2.80617352499998));
#197343=CARTESIAN_POINT('Ctrl Pts',(10.1767595639999,12.2,2.80604860999999));
#197344=CARTESIAN_POINT('Ctrl Pts',(10.1748213379999,12.2,2.80592239499998));
#197345=CARTESIAN_POINT('Ctrl Pts',(10.1728903809999,12.2,2.80579489099999));
#197346=CARTESIAN_POINT('Ctrl Pts',(10.1709667089999,12.2,2.80566611099999));
#197347=CARTESIAN_POINT('Ctrl Pts',(10.1690503349999,12.2,2.80553606899999));
#197348=CARTESIAN_POINT('Ctrl Pts',(10.1671412759999,12.2,2.80540477799998));
#197349=CARTESIAN_POINT('Ctrl Pts',(10.1652395459999,12.2,2.80527224899998));
#197350=CARTESIAN_POINT('Ctrl Pts',(10.1633451609999,12.2,2.80513849699998));
#197351=CARTESIAN_POINT('Ctrl Pts',(10.1614581339999,12.2,2.80500353399999));
#197352=CARTESIAN_POINT('Ctrl Pts',(10.1595784839999,12.2,2.80486737399999));
#197353=CARTESIAN_POINT('Ctrl Pts',(10.1577062229999,12.2,2.80473002899999));
#197354=CARTESIAN_POINT('Ctrl Pts',(10.1558413669999,12.2,2.80459151299999));
#197355=CARTESIAN_POINT('Ctrl Pts',(10.1539839329999,12.2,2.80445183999999));
#197356=CARTESIAN_POINT('Ctrl Pts',(10.1521339339999,12.2,2.80431102199999));
#197357=CARTESIAN_POINT('Ctrl Pts',(10.1502913879999,12.2,2.80416907399999));
#197358=CARTESIAN_POINT('Ctrl Pts',(10.1484563089999,12.2,2.80402600799999));
#197359=CARTESIAN_POINT('Ctrl Pts',(10.1466287129999,12.2,2.80388183699999));
#197360=CARTESIAN_POINT('Ctrl Pts',(10.1448086139999,12.2,2.80373657799998));
#197361=CARTESIAN_POINT('Ctrl Pts',(10.1429960289999,12.2,2.80359023999999));
#197362=CARTESIAN_POINT('Ctrl Pts',(10.1411909749999,12.2,2.80344284099999));
#197363=CARTESIAN_POINT('Ctrl Pts',(10.1393934659999,12.2,2.80329439199999));
#197364=CARTESIAN_POINT('Ctrl Pts',(10.1376035179999,12.2,2.80314490699999));
#197365=CARTESIAN_POINT('Ctrl Pts',(10.1358211459999,12.2,2.80299440199999));
#197366=CARTESIAN_POINT('Ctrl Pts',(10.1340463689999,12.2,2.80284288899999));
#197367=CARTESIAN_POINT('Ctrl Pts',(10.1322791999999,12.2,2.80269038199998));
#197368=CARTESIAN_POINT('Ctrl Pts',(10.1305196549999,12.2,2.80253689599999));
#197369=CARTESIAN_POINT('Ctrl Pts',(10.1287677519999,12.2,2.80238244599998));
#197370=CARTESIAN_POINT('Ctrl Pts',(10.1270235059999,12.2,2.80222704299998));
#197371=CARTESIAN_POINT('Ctrl Pts',(10.1252869329999,12.2,2.80207070399998));
#197372=CARTESIAN_POINT('Ctrl Pts',(10.1235580499999,12.2,2.80191344299999));
#197373=CARTESIAN_POINT('Ctrl Pts',(10.1218368709999,12.2,2.80175527399999));
#197374=CARTESIAN_POINT('Ctrl Pts',(10.1201234149999,12.2,2.80159621099998));
#197375=CARTESIAN_POINT('Ctrl Pts',(10.1184176969999,12.2,2.80143626899999));
#197376=CARTESIAN_POINT('Ctrl Pts',(10.1167197329999,12.2,2.80127546199999));
#197377=CARTESIAN_POINT('Ctrl Pts',(10.1150295409999,12.2,2.80111380599998));
#197378=CARTESIAN_POINT('Ctrl Pts',(10.1133471369999,12.2,2.80095131499999));
#197379=CARTESIAN_POINT('Ctrl Pts',(10.1116725359999,12.2,2.80078800299999));
#197380=CARTESIAN_POINT('Ctrl Pts',(10.1100057559999,12.2,2.80062388499999));
#197381=CARTESIAN_POINT('Ctrl Pts',(10.1083468139999,12.2,2.80045897699999));
#197382=CARTESIAN_POINT('Ctrl Pts',(10.1066957249999,12.2,2.80029329299998));
#197383=CARTESIAN_POINT('Ctrl Pts',(10.1050525089999,12.2,2.80012684799999));
#197384=CARTESIAN_POINT('Ctrl Pts',(10.1034171789999,12.2,2.79995965799999));
#197385=CARTESIAN_POINT('Ctrl Pts',(10.1017897539999,12.2,2.79979173799998));
#197386=CARTESIAN_POINT('Ctrl Pts',(10.1001702509999,12.2,2.79962310199998));
#197387=CARTESIAN_POINT('Ctrl Pts',(10.0985586869999,12.2,2.79945376699998));
#197388=CARTESIAN_POINT('Ctrl Pts',(10.0969550769999,12.2,2.79928374699999));
#197389=CARTESIAN_POINT('Ctrl Pts',(10.0953594409999,12.2,2.79911305799998));
#197390=CARTESIAN_POINT('Ctrl Pts',(10.0937717949999,12.2,2.79894171599998));
#197391=CARTESIAN_POINT('Ctrl Pts',(10.0921921569999,12.2,2.79876973499999));
#197392=CARTESIAN_POINT('Ctrl Pts',(10.0906205419999,12.2,2.79859713299999));
#197393=CARTESIAN_POINT('Ctrl Pts',(10.0890569699999,12.2,2.79842392399999));
#197394=CARTESIAN_POINT('Ctrl Pts',(10.0875014559999,12.2,2.79825012399999));
#197395=CARTESIAN_POINT('Ctrl Pts',(10.0859540199999,12.2,2.79807574899999));
#197396=CARTESIAN_POINT('Ctrl Pts',(10.0844146779999,12.2,2.79790081599998));
#197397=CARTESIAN_POINT('Ctrl Pts',(10.0828834479999,12.2,2.79772533899998));
#197398=CARTESIAN_POINT('Ctrl Pts',(10.0813603479999,12.2,2.79754933599998));
#197399=CARTESIAN_POINT('Ctrl Pts',(10.0798453939999,12.2,2.79737282199999));
#197400=CARTESIAN_POINT('Ctrl Pts',(10.0783386059999,12.2,2.79719581399998));
#197401=CARTESIAN_POINT('Ctrl Pts',(10.0768400009999,12.2,2.79701832799999));
#197402=CARTESIAN_POINT('Ctrl Pts',(10.0753495959999,12.2,2.79684037999999));
#197403=CARTESIAN_POINT('Ctrl Pts',(10.0738674099999,12.2,2.79666198699999));
#197404=CARTESIAN_POINT('Ctrl Pts',(10.0723934619999,12.2,2.79648316499999));
#197405=CARTESIAN_POINT('Ctrl Pts',(10.0709277689999,12.2,2.79630393099998));
#197406=CARTESIAN_POINT('Ctrl Pts',(10.0694703469999,12.2,2.79612430099998));
#197407=CARTESIAN_POINT('Ctrl Pts',(10.0680212179999,12.2,2.79594429399998));
#197408=CARTESIAN_POINT('Ctrl Pts',(10.0665803979999,12.2,2.79576392499998));
#197409=CARTESIAN_POINT('Ctrl Pts',(10.0651479059999,12.2,2.79558321099999));
#197410=CARTESIAN_POINT('Ctrl Pts',(10.0637237609999,12.2,2.79540216899999));
#197411=CARTESIAN_POINT('Ctrl Pts',(10.0623079809999,12.2,2.79522081599998));
#197412=CARTESIAN_POINT('Ctrl Pts',(10.0609005839999,12.2,2.79503916999998));
#197413=CARTESIAN_POINT('Ctrl Pts',(10.0595015889999,12.2,2.79485724899998));
#197414=CARTESIAN_POINT('Ctrl Pts',(10.0581110159999,12.2,2.79467506799998));
#197415=CARTESIAN_POINT('Ctrl Pts',(10.0567288819999,12.2,2.79449264599998));
#197416=CARTESIAN_POINT('Ctrl Pts',(10.0553552059999,12.2,2.79430999899999));
#197417=CARTESIAN_POINT('Ctrl Pts',(10.0539900079999,12.2,2.79412714599999));
#197418=CARTESIAN_POINT('Ctrl Pts',(10.0526333059999,12.2,2.79394410499999));
#197419=CARTESIAN_POINT('Ctrl Pts',(10.0512851199999,12.2,2.79376089299999));
#197420=CARTESIAN_POINT('Ctrl Pts',(10.0499454679999,12.2,2.79357752799999));
#197421=CARTESIAN_POINT('Ctrl Pts',(10.0486143699999,12.2,2.79339402899998));
#197422=CARTESIAN_POINT('Ctrl Pts',(10.0472918449999,12.2,2.79321041199999));
#197423=CARTESIAN_POINT('Ctrl Pts',(10.0459779129999,12.2,2.79302669599998));
#197424=CARTESIAN_POINT('Ctrl Pts',(10.0446725919999,12.2,2.79284289899999));
#197425=CARTESIAN_POINT('Ctrl Pts',(10.0433759029999,12.2,2.79265903999999));
#197426=CARTESIAN_POINT('Ctrl Pts',(10.0420878649999,12.2,2.79247513699998));
#197427=CARTESIAN_POINT('Ctrl Pts',(10.0408084969999,12.2,2.79229120899998));
#197428=CARTESIAN_POINT('Ctrl Pts',(10.0395378199999,12.2,2.79210727399998));
#197429=CARTESIAN_POINT('Ctrl Pts',(10.0382758529999,12.2,2.79192334999999));
#197430=CARTESIAN_POINT('Ctrl Pts',(10.0370226159999,12.2,2.79173945599998));
#197431=CARTESIAN_POINT('Ctrl Pts',(10.0357781289999,12.2,2.79155561199998));
#197432=CARTESIAN_POINT('Ctrl Pts',(10.0345424119999,12.2,2.79137183599998));
#197433=CARTESIAN_POINT('Ctrl Pts',(10.0333154849999,12.2,2.79118814799999));
#197434=CARTESIAN_POINT('Ctrl Pts',(10.0320973689999,12.2,2.79100456599998));
#197435=CARTESIAN_POINT('Ctrl Pts',(10.0308880829999,12.2,2.79082110899999));
#197436=CARTESIAN_POINT('Ctrl Pts',(10.0296876489999,12.2,2.79063779799999));
#197437=CARTESIAN_POINT('Ctrl Pts',(10.0284960859999,12.2,2.79045464999999));
#197438=CARTESIAN_POINT('Ctrl Pts',(10.0273134139999,12.2,2.79027168599999));
#197439=CARTESIAN_POINT('Ctrl Pts',(10.0261396569999,12.2,2.79008892699999));
#197440=CARTESIAN_POINT('Ctrl Pts',(10.0249748309999,12.2,2.78990638999999));
#197441=CARTESIAN_POINT('Ctrl Pts',(10.0238189609999,12.2,2.78972409599999));
#197442=CARTESIAN_POINT('Ctrl Pts',(10.0226720649999,12.2,2.78954206499999));
#197443=CARTESIAN_POINT('Ctrl Pts',(10.0215341659999,12.2,2.78936031699998));
#197444=CARTESIAN_POINT('Ctrl Pts',(10.0204052839999,12.2,2.78917887199999));
#197445=CARTESIAN_POINT('Ctrl Pts',(10.0192854389999,12.2,2.78899774999999));
#197446=CARTESIAN_POINT('Ctrl Pts',(10.0181746539999,12.2,2.78881697199999));
#197447=CARTESIAN_POINT('Ctrl Pts',(10.0170729509999,12.2,2.78863655799999));
#197448=CARTESIAN_POINT('Ctrl Pts',(10.0159803479999,12.2,2.78845652899999));
#197449=CARTESIAN_POINT('Ctrl Pts',(10.0148968709999,12.2,2.78827690399999));
#197450=CARTESIAN_POINT('Ctrl Pts',(10.0138225379999,12.2,2.78809770699999));
#197451=CARTESIAN_POINT('Ctrl Pts',(10.0127573729999,12.2,2.78791895599999));
#197452=CARTESIAN_POINT('Ctrl Pts',(10.0117013959999,12.2,2.78774067199999));
#197453=CARTESIAN_POINT('Ctrl Pts',(10.0106546299999,12.2,2.78756287699998));
#197454=CARTESIAN_POINT('Ctrl Pts',(10.0096170959999,12.2,2.78738559299998));
#197455=CARTESIAN_POINT('Ctrl Pts',(10.0085888169999,12.2,2.78720884099998));
#197456=CARTESIAN_POINT('Ctrl Pts',(10.0075698159999,12.2,2.78703263999999));
#197457=CARTESIAN_POINT('Ctrl Pts',(10.0065601129999,12.2,2.78685701499998));
#197458=CARTESIAN_POINT('Ctrl Pts',(10.0055597309999,12.2,2.78668198499999));
#197459=CARTESIAN_POINT('Ctrl Pts',(10.0045686949999,12.2,2.78650757299998));
#197460=CARTESIAN_POINT('Ctrl Pts',(10.0035870229999,12.2,2.78633380099999));
#197461=CARTESIAN_POINT('Ctrl Pts',(10.0026147409999,12.2,2.78616069099999));
#197462=CARTESIAN_POINT('Ctrl Pts',(10.0016518709999,12.2,2.78598826499999));
#197463=CARTESIAN_POINT('Ctrl Pts',(10.0006984369999,12.2,2.78581654399999));
#197464=CARTESIAN_POINT('Ctrl Pts',(9.99975445999995,12.2,2.78564555199999));
#197465=CARTESIAN_POINT('Ctrl Pts',(9.99881996399995,12.2,2.78547531199998));
#197466=CARTESIAN_POINT('Ctrl Pts',(9.99789497199994,12.2,2.78530584299999));
#197467=CARTESIAN_POINT('Ctrl Pts',(9.99697950699994,12.2,2.78513717199999));
#197468=CARTESIAN_POINT('Ctrl Pts',(9.99607881099994,12.2,2.78497028699999));
#197469=CARTESIAN_POINT('Ctrl Pts',(9.99536684599994,12.2,2.78483763599999));
#197470=CARTESIAN_POINT('Ctrl Pts',(9.99483839899994,12.2,2.78473876899999));
#197471=CARTESIAN_POINT('Ctrl Pts',(9.99448967699994,12.2,2.78467334899998));
#197472=CARTESIAN_POINT('Ctrl Pts',(9.99431831699994,12.2,2.78464115899999));
#197473=CARTESIAN_POINT('Ctrl Pts',(9.99431831699994,15.2,2.78464115899999));
#197474=CARTESIAN_POINT('Ctrl Pts',(9.99448967699994,15.2,2.78467334899998));
#197475=CARTESIAN_POINT('Ctrl Pts',(9.99483839899994,15.2,2.78473876899999));
#197476=CARTESIAN_POINT('Ctrl Pts',(9.99536684599994,15.2,2.78483763599999));
#197477=CARTESIAN_POINT('Ctrl Pts',(9.99607881099994,15.2,2.78497028699999));
#197478=CARTESIAN_POINT('Ctrl Pts',(9.99697950699994,15.2,2.78513717199999));
#197479=CARTESIAN_POINT('Ctrl Pts',(9.99789497199994,15.2,2.78530584299999));
#197480=CARTESIAN_POINT('Ctrl Pts',(9.99881996399995,15.2,2.78547531199998));
#197481=CARTESIAN_POINT('Ctrl Pts',(9.99975445999995,15.2,2.78564555199999));
#197482=CARTESIAN_POINT('Ctrl Pts',(10.0006984369999,15.2,2.78581654399999));
#197483=CARTESIAN_POINT('Ctrl Pts',(10.0016518709999,15.2,2.78598826499999));
#197484=CARTESIAN_POINT('Ctrl Pts',(10.0026147409999,15.2,2.78616069099999));
#197485=CARTESIAN_POINT('Ctrl Pts',(10.0035870229999,15.2,2.78633380099999));
#197486=CARTESIAN_POINT('Ctrl Pts',(10.0045686949999,15.2,2.78650757299998));
#197487=CARTESIAN_POINT('Ctrl Pts',(10.0055597309999,15.2,2.78668198499999));
#197488=CARTESIAN_POINT('Ctrl Pts',(10.0065601129999,15.2,2.78685701499998));
#197489=CARTESIAN_POINT('Ctrl Pts',(10.0075698159999,15.2,2.78703263999999));
#197490=CARTESIAN_POINT('Ctrl Pts',(10.0085888169999,15.2,2.78720884099998));
#197491=CARTESIAN_POINT('Ctrl Pts',(10.0096170959999,15.2,2.78738559299998));
#197492=CARTESIAN_POINT('Ctrl Pts',(10.0106546299999,15.2,2.78756287699998));
#197493=CARTESIAN_POINT('Ctrl Pts',(10.0117013959999,15.2,2.78774067199999));
#197494=CARTESIAN_POINT('Ctrl Pts',(10.0127573729999,15.2,2.78791895599999));
#197495=CARTESIAN_POINT('Ctrl Pts',(10.0138225379999,15.2,2.78809770699999));
#197496=CARTESIAN_POINT('Ctrl Pts',(10.0148968709999,15.2,2.78827690399999));
#197497=CARTESIAN_POINT('Ctrl Pts',(10.0159803479999,15.2,2.78845652899999));
#197498=CARTESIAN_POINT('Ctrl Pts',(10.0170729509999,15.2,2.78863655799999));
#197499=CARTESIAN_POINT('Ctrl Pts',(10.0181746539999,15.2,2.78881697199999));
#197500=CARTESIAN_POINT('Ctrl Pts',(10.0192854389999,15.2,2.78899774999999));
#197501=CARTESIAN_POINT('Ctrl Pts',(10.0204052839999,15.2,2.78917887199999));
#197502=CARTESIAN_POINT('Ctrl Pts',(10.0215341659999,15.2,2.78936031699998));
#197503=CARTESIAN_POINT('Ctrl Pts',(10.0226720649999,15.2,2.78954206499999));
#197504=CARTESIAN_POINT('Ctrl Pts',(10.0238189609999,15.2,2.78972409599999));
#197505=CARTESIAN_POINT('Ctrl Pts',(10.0249748309999,15.2,2.78990638999999));
#197506=CARTESIAN_POINT('Ctrl Pts',(10.0261396569999,15.2,2.79008892699999));
#197507=CARTESIAN_POINT('Ctrl Pts',(10.0273134139999,15.2,2.79027168599999));
#197508=CARTESIAN_POINT('Ctrl Pts',(10.0284960859999,15.2,2.79045464999999));
#197509=CARTESIAN_POINT('Ctrl Pts',(10.0296876489999,15.2,2.79063779799999));
#197510=CARTESIAN_POINT('Ctrl Pts',(10.0308880829999,15.2,2.79082110899999));
#197511=CARTESIAN_POINT('Ctrl Pts',(10.0320973689999,15.2,2.79100456599998));
#197512=CARTESIAN_POINT('Ctrl Pts',(10.0333154849999,15.2,2.79118814799999));
#197513=CARTESIAN_POINT('Ctrl Pts',(10.0345424119999,15.2,2.79137183599998));
#197514=CARTESIAN_POINT('Ctrl Pts',(10.0357781289999,15.2,2.79155561199998));
#197515=CARTESIAN_POINT('Ctrl Pts',(10.0370226159999,15.2,2.79173945599998));
#197516=CARTESIAN_POINT('Ctrl Pts',(10.0382758529999,15.2,2.79192334999999));
#197517=CARTESIAN_POINT('Ctrl Pts',(10.0395378199999,15.2,2.79210727399998));
#197518=CARTESIAN_POINT('Ctrl Pts',(10.0408084969999,15.2,2.79229120899998));
#197519=CARTESIAN_POINT('Ctrl Pts',(10.0420878649999,15.2,2.79247513699998));
#197520=CARTESIAN_POINT('Ctrl Pts',(10.0433759029999,15.2,2.79265903999999));
#197521=CARTESIAN_POINT('Ctrl Pts',(10.0446725919999,15.2,2.79284289899999));
#197522=CARTESIAN_POINT('Ctrl Pts',(10.0459779129999,15.2,2.79302669599998));
#197523=CARTESIAN_POINT('Ctrl Pts',(10.0472918449999,15.2,2.79321041199999));
#197524=CARTESIAN_POINT('Ctrl Pts',(10.0486143699999,15.2,2.79339402899998));
#197525=CARTESIAN_POINT('Ctrl Pts',(10.0499454679999,15.2,2.79357752799999));
#197526=CARTESIAN_POINT('Ctrl Pts',(10.0512851199999,15.2,2.79376089299999));
#197527=CARTESIAN_POINT('Ctrl Pts',(10.0526333059999,15.2,2.79394410499999));
#197528=CARTESIAN_POINT('Ctrl Pts',(10.0539900079999,15.2,2.79412714599999));
#197529=CARTESIAN_POINT('Ctrl Pts',(10.0553552059999,15.2,2.79430999899999));
#197530=CARTESIAN_POINT('Ctrl Pts',(10.0567288819999,15.2,2.79449264599998));
#197531=CARTESIAN_POINT('Ctrl Pts',(10.0581110159999,15.2,2.79467506799998));
#197532=CARTESIAN_POINT('Ctrl Pts',(10.0595015889999,15.2,2.79485724899998));
#197533=CARTESIAN_POINT('Ctrl Pts',(10.0609005839999,15.2,2.79503916999998));
#197534=CARTESIAN_POINT('Ctrl Pts',(10.0623079809999,15.2,2.79522081599998));
#197535=CARTESIAN_POINT('Ctrl Pts',(10.0637237609999,15.2,2.79540216899999));
#197536=CARTESIAN_POINT('Ctrl Pts',(10.0651479059999,15.2,2.79558321099999));
#197537=CARTESIAN_POINT('Ctrl Pts',(10.0665803979999,15.2,2.79576392499998));
#197538=CARTESIAN_POINT('Ctrl Pts',(10.0680212179999,15.2,2.79594429399998));
#197539=CARTESIAN_POINT('Ctrl Pts',(10.0694703469999,15.2,2.79612430099998));
#197540=CARTESIAN_POINT('Ctrl Pts',(10.0709277689999,15.2,2.79630393099998));
#197541=CARTESIAN_POINT('Ctrl Pts',(10.0723934619999,15.2,2.79648316499999));
#197542=CARTESIAN_POINT('Ctrl Pts',(10.0738674099999,15.2,2.79666198699999));
#197543=CARTESIAN_POINT('Ctrl Pts',(10.0753495959999,15.2,2.79684037999999));
#197544=CARTESIAN_POINT('Ctrl Pts',(10.0768400009999,15.2,2.79701832799999));
#197545=CARTESIAN_POINT('Ctrl Pts',(10.0783386059999,15.2,2.79719581399998));
#197546=CARTESIAN_POINT('Ctrl Pts',(10.0798453939999,15.2,2.79737282199999));
#197547=CARTESIAN_POINT('Ctrl Pts',(10.0813603479999,15.2,2.79754933599998));
#197548=CARTESIAN_POINT('Ctrl Pts',(10.0828834479999,15.2,2.79772533899998));
#197549=CARTESIAN_POINT('Ctrl Pts',(10.0844146779999,15.2,2.79790081599998));
#197550=CARTESIAN_POINT('Ctrl Pts',(10.0859540199999,15.2,2.79807574899999));
#197551=CARTESIAN_POINT('Ctrl Pts',(10.0875014559999,15.2,2.79825012399999));
#197552=CARTESIAN_POINT('Ctrl Pts',(10.0890569699999,15.2,2.79842392399999));
#197553=CARTESIAN_POINT('Ctrl Pts',(10.0906205419999,15.2,2.79859713299999));
#197554=CARTESIAN_POINT('Ctrl Pts',(10.0921921569999,15.2,2.79876973499999));
#197555=CARTESIAN_POINT('Ctrl Pts',(10.0937717949999,15.2,2.79894171599998));
#197556=CARTESIAN_POINT('Ctrl Pts',(10.0953594409999,15.2,2.79911305799998));
#197557=CARTESIAN_POINT('Ctrl Pts',(10.0969550769999,15.2,2.79928374699999));
#197558=CARTESIAN_POINT('Ctrl Pts',(10.0985586869999,15.2,2.79945376699998));
#197559=CARTESIAN_POINT('Ctrl Pts',(10.1001702509999,15.2,2.79962310199998));
#197560=CARTESIAN_POINT('Ctrl Pts',(10.1017897539999,15.2,2.79979173799998));
#197561=CARTESIAN_POINT('Ctrl Pts',(10.1034171789999,15.2,2.79995965799999));
#197562=CARTESIAN_POINT('Ctrl Pts',(10.1050525089999,15.2,2.80012684799999));
#197563=CARTESIAN_POINT('Ctrl Pts',(10.1066957249999,15.2,2.80029329299998));
#197564=CARTESIAN_POINT('Ctrl Pts',(10.1083468139999,15.2,2.80045897699999));
#197565=CARTESIAN_POINT('Ctrl Pts',(10.1100057559999,15.2,2.80062388499999));
#197566=CARTESIAN_POINT('Ctrl Pts',(10.1116725359999,15.2,2.80078800299999));
#197567=CARTESIAN_POINT('Ctrl Pts',(10.1133471369999,15.2,2.80095131499999));
#197568=CARTESIAN_POINT('Ctrl Pts',(10.1150295409999,15.2,2.80111380599998));
#197569=CARTESIAN_POINT('Ctrl Pts',(10.1167197329999,15.2,2.80127546199999));
#197570=CARTESIAN_POINT('Ctrl Pts',(10.1184176969999,15.2,2.80143626899999));
#197571=CARTESIAN_POINT('Ctrl Pts',(10.1201234149999,15.2,2.80159621099998));
#197572=CARTESIAN_POINT('Ctrl Pts',(10.1218368709999,15.2,2.80175527399999));
#197573=CARTESIAN_POINT('Ctrl Pts',(10.1235580499999,15.2,2.80191344299999));
#197574=CARTESIAN_POINT('Ctrl Pts',(10.1252869329999,15.2,2.80207070399998));
#197575=CARTESIAN_POINT('Ctrl Pts',(10.1270235059999,15.2,2.80222704299998));
#197576=CARTESIAN_POINT('Ctrl Pts',(10.1287677519999,15.2,2.80238244599998));
#197577=CARTESIAN_POINT('Ctrl Pts',(10.1305196549999,15.2,2.80253689599999));
#197578=CARTESIAN_POINT('Ctrl Pts',(10.1322791999999,15.2,2.80269038199998));
#197579=CARTESIAN_POINT('Ctrl Pts',(10.1340463689999,15.2,2.80284288899999));
#197580=CARTESIAN_POINT('Ctrl Pts',(10.1358211459999,15.2,2.80299440199999));
#197581=CARTESIAN_POINT('Ctrl Pts',(10.1376035179999,15.2,2.80314490699999));
#197582=CARTESIAN_POINT('Ctrl Pts',(10.1393934659999,15.2,2.80329439199999));
#197583=CARTESIAN_POINT('Ctrl Pts',(10.1411909749999,15.2,2.80344284099999));
#197584=CARTESIAN_POINT('Ctrl Pts',(10.1429960289999,15.2,2.80359023999999));
#197585=CARTESIAN_POINT('Ctrl Pts',(10.1448086139999,15.2,2.80373657799998));
#197586=CARTESIAN_POINT('Ctrl Pts',(10.1466287129999,15.2,2.80388183699999));
#197587=CARTESIAN_POINT('Ctrl Pts',(10.1484563089999,15.2,2.80402600799999));
#197588=CARTESIAN_POINT('Ctrl Pts',(10.1502913879999,15.2,2.80416907399999));
#197589=CARTESIAN_POINT('Ctrl Pts',(10.1521339339999,15.2,2.80431102199999));
#197590=CARTESIAN_POINT('Ctrl Pts',(10.1539839329999,15.2,2.80445183999999));
#197591=CARTESIAN_POINT('Ctrl Pts',(10.1558413669999,15.2,2.80459151299999));
#197592=CARTESIAN_POINT('Ctrl Pts',(10.1577062229999,15.2,2.80473002899999));
#197593=CARTESIAN_POINT('Ctrl Pts',(10.1595784839999,15.2,2.80486737399999));
#197594=CARTESIAN_POINT('Ctrl Pts',(10.1614581339999,15.2,2.80500353399999));
#197595=CARTESIAN_POINT('Ctrl Pts',(10.1633451609999,15.2,2.80513849699998));
#197596=CARTESIAN_POINT('Ctrl Pts',(10.1652395459999,15.2,2.80527224899998));
#197597=CARTESIAN_POINT('Ctrl Pts',(10.1671412759999,15.2,2.80540477799998));
#197598=CARTESIAN_POINT('Ctrl Pts',(10.1690503349999,15.2,2.80553606899999));
#197599=CARTESIAN_POINT('Ctrl Pts',(10.1709667089999,15.2,2.80566611099999));
#197600=CARTESIAN_POINT('Ctrl Pts',(10.1728903809999,15.2,2.80579489099999));
#197601=CARTESIAN_POINT('Ctrl Pts',(10.1748213379999,15.2,2.80592239499998));
#197602=CARTESIAN_POINT('Ctrl Pts',(10.1767595639999,15.2,2.80604860999999));
#197603=CARTESIAN_POINT('Ctrl Pts',(10.1787050449999,15.2,2.80617352499998));
#197604=CARTESIAN_POINT('Ctrl Pts',(10.1806577639999,15.2,2.80629712499999));
#197605=CARTESIAN_POINT('Ctrl Pts',(10.1826177079999,15.2,2.80641939899999));
#197606=CARTESIAN_POINT('Ctrl Pts',(10.1845848629999,15.2,2.80654033399999));
#197607=CARTESIAN_POINT('Ctrl Pts',(10.1865592119999,15.2,2.80665991699999));
#197608=CARTESIAN_POINT('Ctrl Pts',(10.1885407419999,15.2,2.80677813699998));
#197609=CARTESIAN_POINT('Ctrl Pts',(10.1905294369999,15.2,2.80689497899999));
#197610=CARTESIAN_POINT('Ctrl Pts',(10.1925252829999,15.2,2.80701043199999));
#197611=CARTESIAN_POINT('Ctrl Pts',(10.1945282669999,15.2,2.80712448399999));
#197612=CARTESIAN_POINT('Ctrl Pts',(10.1965383709999,15.2,2.80723712199999));
#197613=CARTESIAN_POINT('Ctrl Pts',(10.1985555829999,15.2,2.80734833399999));
#197614=CARTESIAN_POINT('Ctrl Pts',(10.2005798889999,15.2,2.80745810899998));
#197615=CARTESIAN_POINT('Ctrl Pts',(10.2026112719999,15.2,2.80756643299998));
#197616=CARTESIAN_POINT('Ctrl Pts',(10.2046497199999,15.2,2.80767329399998));
#197617=CARTESIAN_POINT('Ctrl Pts',(10.2066952179999,15.2,2.80777868099998));
#197618=CARTESIAN_POINT('Ctrl Pts',(10.2087477509999,15.2,2.80788258099999));
#197619=CARTESIAN_POINT('Ctrl Pts',(10.2108073059999,15.2,2.80798498399999));
#197620=CARTESIAN_POINT('Ctrl Pts',(10.2128738679999,15.2,2.80808587499998));
#197621=CARTESIAN_POINT('Ctrl Pts',(10.2149474219999,15.2,2.80818524499999));
#197622=CARTESIAN_POINT('Ctrl Pts',(10.2170279549999,15.2,2.80828308099998));
#197623=CARTESIAN_POINT('Ctrl Pts',(10.2191154529999,15.2,2.80837936999998));
#197624=CARTESIAN_POINT('Ctrl Pts',(10.2212099009999,15.2,2.80847410299998));
#197625=CARTESIAN_POINT('Ctrl Pts',(10.2233112869999,15.2,2.80856726499999));
#197626=CARTESIAN_POINT('Ctrl Pts',(10.2254195939999,15.2,2.80865884799999));
#197627=CARTESIAN_POINT('Ctrl Pts',(10.2275348109999,15.2,2.80874883799999));
#197628=CARTESIAN_POINT('Ctrl Pts',(10.2296569209999,15.2,2.80883722299999));
#197629=CARTESIAN_POINT('Ctrl Pts',(10.2317859129999,15.2,2.80892399399999));
#197630=CARTESIAN_POINT('Ctrl Pts',(10.2339217719999,15.2,2.80900913799999));
#197631=CARTESIAN_POINT('Ctrl Pts',(10.2360644839999,15.2,2.80909264399998));
#197632=CARTESIAN_POINT('Ctrl Pts',(10.2382140349999,15.2,2.80917449999999));
#197633=CARTESIAN_POINT('Ctrl Pts',(10.2403704109999,15.2,2.80925469399998));
#197634=CARTESIAN_POINT('Ctrl Pts',(10.2425335999999,15.2,2.80933321799999));
#197635=CARTESIAN_POINT('Ctrl Pts',(10.2447035879999,15.2,2.80941005799999));
#197636=CARTESIAN_POINT('Ctrl Pts',(10.2468803589999,15.2,2.80948520299999));
#197637=CARTESIAN_POINT('Ctrl Pts',(10.2490639019999,15.2,2.80955864199999));
#197638=CARTESIAN_POINT('Ctrl Pts',(10.2512542019999,15.2,2.80963036499998));
#197639=CARTESIAN_POINT('Ctrl Pts',(10.2534512459999,15.2,2.80970035899998));
#197640=CARTESIAN_POINT('Ctrl Pts',(10.2556550209999,15.2,2.80976861599999));
#197641=CARTESIAN_POINT('Ctrl Pts',(10.2578655119999,15.2,2.80983512099999));
#197642=CARTESIAN_POINT('Ctrl Pts',(10.2600827069999,15.2,2.80989986699999));
#197643=CARTESIAN_POINT('Ctrl Pts',(10.2623065929999,15.2,2.80996284199999));
#197644=CARTESIAN_POINT('Ctrl Pts',(10.2645371559999,15.2,2.81002403399999));
#197645=CARTESIAN_POINT('Ctrl Pts',(10.2667743819999,15.2,2.81008343199999));
#197646=CARTESIAN_POINT('Ctrl Pts',(10.2690182579999,15.2,2.81014102599999));
#197647=CARTESIAN_POINT('Ctrl Pts',(10.2712687709999,15.2,2.81019680599999));
#197648=CARTESIAN_POINT('Ctrl Pts',(10.2735259089999,15.2,2.81025076199998));
#197649=CARTESIAN_POINT('Ctrl Pts',(10.2757896559999,15.2,2.81030288099998));
#197650=CARTESIAN_POINT('Ctrl Pts',(10.2780600009999,15.2,2.81035315199999));
#197651=CARTESIAN_POINT('Ctrl Pts',(10.2803369309999,15.2,2.81040156799998));
#197652=CARTESIAN_POINT('Ctrl Pts',(10.2826204319999,15.2,2.81044811699999));
#197653=CARTESIAN_POINT('Ctrl Pts',(10.2849104899999,15.2,2.81049278699999));
#197654=CARTESIAN_POINT('Ctrl Pts',(10.2872070959999,15.2,2.81053556799999));
#197655=CARTESIAN_POINT('Ctrl Pts',(10.2895102319999,15.2,2.81057645199999));
#197656=CARTESIAN_POINT('Ctrl Pts',(10.2918198869999,15.2,2.81061542499998));
#197657=CARTESIAN_POINT('Ctrl Pts',(10.2941360499999,15.2,2.81065247899999));
#197658=CARTESIAN_POINT('Ctrl Pts',(10.2964587039999,15.2,2.81068760399998));
#197659=CARTESIAN_POINT('Ctrl Pts',(10.2987878399999,15.2,2.81072078899999));
#197660=CARTESIAN_POINT('Ctrl Pts',(10.3011234449999,15.2,2.81075202499999));
#197661=CARTESIAN_POINT('Ctrl Pts',(10.3034655029999,15.2,2.81078129899999));
#197662=CARTESIAN_POINT('Ctrl Pts',(10.3058140039999,15.2,2.81080860299999));
#197663=CARTESIAN_POINT('Ctrl Pts',(10.3081689339999,15.2,2.81083392699998));
#197664=CARTESIAN_POINT('Ctrl Pts',(10.3105302809999,15.2,2.81085726199999));
#197665=CARTESIAN_POINT('Ctrl Pts',(10.3128980319999,15.2,2.81087859499999));
#197666=CARTESIAN_POINT('Ctrl Pts',(10.3152721739999,15.2,2.81089791699999));
#197667=CARTESIAN_POINT('Ctrl Pts',(10.3176526949999,15.2,2.81091521999999));
#197668=CARTESIAN_POINT('Ctrl Pts',(10.3200395829999,15.2,2.81093049299999));
#197669=CARTESIAN_POINT('Ctrl Pts',(10.3224328229999,15.2,2.81094372499999));
#197670=CARTESIAN_POINT('Ctrl Pts',(10.3248324049999,15.2,2.81095490799999));
#197671=CARTESIAN_POINT('Ctrl Pts',(10.3272383149999,15.2,2.81096403199999));
#197672=CARTESIAN_POINT('Ctrl Pts',(10.3296505419999,15.2,2.81097108499999));
#197673=CARTESIAN_POINT('Ctrl Pts',(10.3320690709999,15.2,2.81097606099999));
#197674=CARTESIAN_POINT('Ctrl Pts',(10.3344938929999,15.2,2.81097894699998));
#197675=CARTESIAN_POINT('Ctrl Pts',(10.3369249929999,15.2,2.81097973599999));
#197676=CARTESIAN_POINT('Ctrl Pts',(10.3393623599999,15.2,2.81097841599999));
#197677=CARTESIAN_POINT('Ctrl Pts',(10.3418059809999,15.2,2.81097497899999));
#197678=CARTESIAN_POINT('Ctrl Pts',(10.3442558419999,15.2,2.81096941599999));
#197679=CARTESIAN_POINT('Ctrl Pts',(10.3467119339999,15.2,2.81096171499998));
#197680=CARTESIAN_POINT('Ctrl Pts',(10.3491742439999,15.2,2.81095186899999));
#197681=CARTESIAN_POINT('Ctrl Pts',(10.3516427589999,15.2,2.81093986799998));
#197682=CARTESIAN_POINT('Ctrl Pts',(10.3541174659999,15.2,2.81092570199998));
#197683=CARTESIAN_POINT('Ctrl Pts',(10.3565983529999,15.2,2.81090936199998));
#197684=CARTESIAN_POINT('Ctrl Pts',(10.3590854099999,15.2,2.81089083999999));
#197685=CARTESIAN_POINT('Ctrl Pts',(10.3615786239999,15.2,2.81087012399999));
#197686=CARTESIAN_POINT('Ctrl Pts',(10.3640779799999,15.2,2.81084720699998));
#197687=CARTESIAN_POINT('Ctrl Pts',(10.3665834699999,15.2,2.81082207899999));
#197688=CARTESIAN_POINT('Ctrl Pts',(10.3690950799999,15.2,2.81079473099999));
#197689=CARTESIAN_POINT('Ctrl Pts',(10.3716127979999,15.2,2.81076515299999));
#197690=CARTESIAN_POINT('Ctrl Pts',(10.3741366129999,15.2,2.81073333699998));
#197691=CARTESIAN_POINT('Ctrl Pts',(10.3766665119999,15.2,2.81069927299999));
#197692=CARTESIAN_POINT('Ctrl Pts',(10.3792024839999,15.2,2.81066295399999));
#197693=CARTESIAN_POINT('Ctrl Pts',(10.3817445159999,15.2,2.81062436799999));
#197694=CARTESIAN_POINT('Ctrl Pts',(10.3842925959999,15.2,2.81058350899999));
#197695=CARTESIAN_POINT('Ctrl Pts',(10.3868467139999,15.2,2.81054036599999));
#197696=CARTESIAN_POINT('Ctrl Pts',(10.3894068559999,15.2,2.81049492999998));
#197697=CARTESIAN_POINT('Ctrl Pts',(10.3919730119999,15.2,2.81044719399999));
#197698=CARTESIAN_POINT('Ctrl Pts',(10.3945451689999,15.2,2.81039714699999));
#197699=CARTESIAN_POINT('Ctrl Pts',(10.3971233149999,15.2,2.81034478199999));
#197700=CARTESIAN_POINT('Ctrl Pts',(10.3997074399999,15.2,2.81029008999998));
#197701=CARTESIAN_POINT('Ctrl Pts',(10.4022975309999,15.2,2.81023305999998));
#197702=CARTESIAN_POINT('Ctrl Pts',(10.4048935769999,15.2,2.81017368599999));
#197703=CARTESIAN_POINT('Ctrl Pts',(10.4074955649999,15.2,2.81011195799999));
#197704=CARTESIAN_POINT('Ctrl Pts',(10.4101034849999,15.2,2.81004786799999));
#197705=CARTESIAN_POINT('Ctrl Pts',(10.4127173239999,15.2,2.80998140599999));
#197706=CARTESIAN_POINT('Ctrl Pts',(10.4153370719999,15.2,2.80991256599999));
#197707=CARTESIAN_POINT('Ctrl Pts',(10.4179627159999,15.2,2.80984133699998));
#197708=CARTESIAN_POINT('Ctrl Pts',(10.4205942449999,15.2,2.80976771199998));
#197709=CARTESIAN_POINT('Ctrl Pts',(10.4232316479999,15.2,2.80969167999999));
#197710=CARTESIAN_POINT('Ctrl Pts',(10.4258749129999,15.2,2.80961323599998));
#197711=CARTESIAN_POINT('Ctrl Pts',(10.4285240289999,15.2,2.80953237099999));
#197712=CARTESIAN_POINT('Ctrl Pts',(10.4311789839999,15.2,2.80944907299999));
#197713=CARTESIAN_POINT('Ctrl Pts',(10.4338397659999,15.2,2.80936333799998));
#197714=CARTESIAN_POINT('Ctrl Pts',(10.4365063659999,15.2,2.80927515599998));
#197715=CARTESIAN_POINT('Ctrl Pts',(10.4391787699999,15.2,2.80918451599998));
#197716=CARTESIAN_POINT('Ctrl Pts',(10.4418569669999,15.2,2.80909141499999));
#197717=CARTESIAN_POINT('Ctrl Pts',(10.4445409479999,15.2,2.80899584099998));
#197718=CARTESIAN_POINT('Ctrl Pts',(10.4472306989999,15.2,2.80889778599998));
#197719=CARTESIAN_POINT('Ctrl Pts',(10.4499262109999,15.2,2.80879724399998));
#197720=CARTESIAN_POINT('Ctrl Pts',(10.4526274699999,15.2,2.80869420399998));
#197721=CARTESIAN_POINT('Ctrl Pts',(10.4553344669999,15.2,2.80858866099998));
#197722=CARTESIAN_POINT('Ctrl Pts',(10.4580471909999,15.2,2.80848060399999));
#197723=CARTESIAN_POINT('Ctrl Pts',(10.4607656289999,15.2,2.80837002599998));
#197724=CARTESIAN_POINT('Ctrl Pts',(10.4634897709999,15.2,2.80825691999999));
#197725=CARTESIAN_POINT('Ctrl Pts',(10.4662196059999,15.2,2.80814127499998));
#197726=CARTESIAN_POINT('Ctrl Pts',(10.4689551229999,15.2,2.80802308599998));
#197727=CARTESIAN_POINT('Ctrl Pts',(10.4716963109999,15.2,2.80790234499998));
#197728=CARTESIAN_POINT('Ctrl Pts',(10.4744431569999,15.2,2.80777904299998));
#197729=CARTESIAN_POINT('Ctrl Pts',(10.4771956519999,15.2,2.80765317099998));
#197730=CARTESIAN_POINT('Ctrl Pts',(10.4799537849999,15.2,2.80752472299999));
#197731=CARTESIAN_POINT('Ctrl Pts',(10.4827175439999,15.2,2.80739368999999));
#197732=CARTESIAN_POINT('Ctrl Pts',(10.4854869179999,15.2,2.80726006499999));
#197733=CARTESIAN_POINT('Ctrl Pts',(10.4882618969999,15.2,2.80712383899999));
#197734=CARTESIAN_POINT('Ctrl Pts',(10.4910424679999,15.2,2.80698500599998));
#197735=CARTESIAN_POINT('Ctrl Pts',(10.4938286229999,15.2,2.80684355699999));
#197736=CARTESIAN_POINT('Ctrl Pts',(10.4966203499999,15.2,2.80669948499998));
#197737=CARTESIAN_POINT('Ctrl Pts',(10.4994176369999,15.2,2.80655278099999));
#197738=CARTESIAN_POINT('Ctrl Pts',(10.5022204749999,15.2,2.80640343899999));
#197739=CARTESIAN_POINT('Ctrl Pts',(10.5050288509999,15.2,2.80625144999998));
#197740=CARTESIAN_POINT('Ctrl Pts',(10.5078427569999,15.2,2.80609680699998));
#197741=CARTESIAN_POINT('Ctrl Pts',(10.5106621789999,15.2,2.80593950299998));
#197742=CARTESIAN_POINT('Ctrl Pts',(10.5134871079999,15.2,2.80577952899999));
#197743=CARTESIAN_POINT('Ctrl Pts',(10.5163175329999,15.2,2.80561687899999));
#197744=CARTESIAN_POINT('Ctrl Pts',(10.5191534429999,15.2,2.80545154499999));
#197745=CARTESIAN_POINT('Ctrl Pts',(10.5219948289999,15.2,2.80528351899999));
#197746=CARTESIAN_POINT('Ctrl Pts',(10.5248416769999,15.2,2.80511279299999));
#197747=CARTESIAN_POINT('Ctrl Pts',(10.5276939799999,15.2,2.80493936099998));
#197748=CARTESIAN_POINT('Ctrl Pts',(10.5305517249999,15.2,2.80476321599998));
#197749=CARTESIAN_POINT('Ctrl Pts',(10.5334149019999,15.2,2.80458434899998));
#197750=CARTESIAN_POINT('Ctrl Pts',(10.5362834999999,15.2,2.80440275299998));
#197751=CARTESIAN_POINT('Ctrl Pts',(10.5391575079999,15.2,2.80421842099998));
#197752=CARTESIAN_POINT('Ctrl Pts',(10.5420369179999,15.2,2.80403134499998));
#197753=CARTESIAN_POINT('Ctrl Pts',(10.5449217159999,15.2,2.80384151899998));
#197754=CARTESIAN_POINT('Ctrl Pts',(10.5478118939999,15.2,2.80364893599998));
#197755=CARTESIAN_POINT('Ctrl Pts',(10.5507074409999,15.2,2.80345358699999));
#197756=CARTESIAN_POINT('Ctrl Pts',(10.5536083449999,15.2,2.80325546599999));
#197757=CARTESIAN_POINT('Ctrl Pts',(10.5565145969999,15.2,2.80305456499998));
#197758=CARTESIAN_POINT('Ctrl Pts',(10.5594261859999,15.2,2.80285087799999));
#197759=CARTESIAN_POINT('Ctrl Pts',(10.5623431029999,15.2,2.80264439699998));
#197760=CARTESIAN_POINT('Ctrl Pts',(10.5652653349999,15.2,2.80243511499998));
#197761=CARTESIAN_POINT('Ctrl Pts',(10.5681928729999,15.2,2.80222302499999));
#197762=CARTESIAN_POINT('Ctrl Pts',(10.5711257059999,15.2,2.80200812099999));
#197763=CARTESIAN_POINT('Ctrl Pts',(10.5740638259999,15.2,2.80179039399999));
#197764=CARTESIAN_POINT('Ctrl Pts',(10.5770072199999,15.2,2.80156983799999));
#197765=CARTESIAN_POINT('Ctrl Pts',(10.5799558779999,15.2,2.80134644699999));
#197766=CARTESIAN_POINT('Ctrl Pts',(10.5829097899999,15.2,2.80112021299999));
#197767=CARTESIAN_POINT('Ctrl Pts',(10.5858689469999,15.2,2.80089112799998));
#197768=CARTESIAN_POINT('Ctrl Pts',(10.5888333369999,15.2,2.80065918699999));
#197769=CARTESIAN_POINT('Ctrl Pts',(10.5918029509999,15.2,2.80042438199998));
#197770=CARTESIAN_POINT('Ctrl Pts',(10.5947777769999,15.2,2.80018670699998));
#197771=CARTESIAN_POINT('Ctrl Pts',(10.5977578069999,15.2,2.79994615399998));
#197772=CARTESIAN_POINT('Ctrl Pts',(10.6007430289999,15.2,2.79970271699998));
#197773=CARTESIAN_POINT('Ctrl Pts',(10.6037334349999,15.2,2.79945638899999));
#197774=CARTESIAN_POINT('Ctrl Pts',(10.6067290119999,15.2,2.79920716299999));
#197775=CARTESIAN_POINT('Ctrl Pts',(10.6097297519999,15.2,2.79895503299999));
#197776=CARTESIAN_POINT('Ctrl Pts',(10.6127356429999,15.2,2.79869999199998));
#197777=CARTESIAN_POINT('Ctrl Pts',(10.6157466779999,15.2,2.79844203299999));
#197778=CARTESIAN_POINT('Ctrl Pts',(10.6187628439999,15.2,2.79818114899999));
#197779=CARTESIAN_POINT('Ctrl Pts',(10.6217841319999,15.2,2.79791733399998));
#197780=CARTESIAN_POINT('Ctrl Pts',(10.6248105309999,15.2,2.79765058099999));
#197781=CARTESIAN_POINT('Ctrl Pts',(10.6278420329999,15.2,2.79738088399998));
#197782=CARTESIAN_POINT('Ctrl Pts',(10.6308786259999,15.2,2.79710823499999));
#197783=CARTESIAN_POINT('Ctrl Pts',(10.6339203009999,15.2,2.79683262899999));
#197784=CARTESIAN_POINT('Ctrl Pts',(10.6369670479999,15.2,2.79655405899998));
#197785=CARTESIAN_POINT('Ctrl Pts',(10.6400188569999,15.2,2.79627251799998));
#197786=CARTESIAN_POINT('Ctrl Pts',(10.6430757179999,15.2,2.79598799899999));
#197787=CARTESIAN_POINT('Ctrl Pts',(10.6461376199999,15.2,2.79570049699998));
#197788=CARTESIAN_POINT('Ctrl Pts',(10.6492045549999,15.2,2.79541000599998));
#197789=CARTESIAN_POINT('Ctrl Pts',(10.6522765109999,15.2,2.79511651699998));
#197790=CARTESIAN_POINT('Ctrl Pts',(10.6553534799999,15.2,2.79482002499999));
#197791=CARTESIAN_POINT('Ctrl Pts',(10.6584354509999,15.2,2.79452052399999));
#197792=CARTESIAN_POINT('Ctrl Pts',(10.6615224159999,15.2,2.79421800799999));
#197793=CARTESIAN_POINT('Ctrl Pts',(10.6646143609999,15.2,2.79391246899999));
#197794=CARTESIAN_POINT('Ctrl Pts',(10.6677112809999,15.2,2.79360390199999));
#197795=CARTESIAN_POINT('Ctrl Pts',(10.6708131629999,15.2,2.79329229999998));
#197796=CARTESIAN_POINT('Ctrl Pts',(10.6739199989999,15.2,2.79297765699998));
#197797=CARTESIAN_POINT('Ctrl Pts',(10.6770317779999,15.2,2.79265996699999));
#197798=CARTESIAN_POINT('Ctrl Pts',(10.6801484919999,15.2,2.79233922399998));
#197799=CARTESIAN_POINT('Ctrl Pts',(10.6832701279999,15.2,2.79201541999999));
#197800=CARTESIAN_POINT('Ctrl Pts',(10.6863966799999,15.2,2.79168855099999));
#197801=CARTESIAN_POINT('Ctrl Pts',(10.6895281349999,15.2,2.79135860899999));
#197802=CARTESIAN_POINT('Ctrl Pts',(10.6926644859999,15.2,2.79102558999998));
#197803=CARTESIAN_POINT('Ctrl Pts',(10.6958057219999,15.2,2.79068948499999));
#197804=CARTESIAN_POINT('Ctrl Pts',(10.6989518329999,15.2,2.79035029099998));
#197805=CARTESIAN_POINT('Ctrl Pts',(10.7021028099999,15.2,2.79000799999999));
#197806=CARTESIAN_POINT('Ctrl Pts',(10.7052586439999,15.2,2.78966260699999));
#197807=CARTESIAN_POINT('Ctrl Pts',(10.7084193239999,15.2,2.78931410399998));
#197808=CARTESIAN_POINT('Ctrl Pts',(10.7115848429999,15.2,2.78896248699999));
#197809=CARTESIAN_POINT('Ctrl Pts',(10.7147551869999,15.2,2.78860774899999));
#197810=CARTESIAN_POINT('Ctrl Pts',(10.7179303499999,15.2,2.78824988399998));
#197811=CARTESIAN_POINT('Ctrl Pts',(10.7211103209999,15.2,2.78788888599999));
#197812=CARTESIAN_POINT('Ctrl Pts',(10.7242950909999,15.2,2.78752475099999));
#197813=CARTESIAN_POINT('Ctrl Pts',(10.7274846509999,15.2,2.78715746999998));
#197814=CARTESIAN_POINT('Ctrl Pts',(10.7306789899999,15.2,2.78678703799999));
#197815=CARTESIAN_POINT('Ctrl Pts',(10.7338780989999,15.2,2.78641344999999));
#197816=CARTESIAN_POINT('Ctrl Pts',(10.7370819699999,15.2,2.78603669899999));
#197817=CARTESIAN_POINT('Ctrl Pts',(10.7402905919999,15.2,2.78565678199998));
#197818=CARTESIAN_POINT('Ctrl Pts',(10.7435039549999,15.2,2.78527368799999));
#197819=CARTESIAN_POINT('Ctrl Pts',(10.7467220519999,15.2,2.78488741599999));
#197820=CARTESIAN_POINT('Ctrl Pts',(10.7499448709999,15.2,2.78449795899999));
#197821=CARTESIAN_POINT('Ctrl Pts',(10.7531724039999,15.2,2.78410530999999));
#197822=CARTESIAN_POINT('Ctrl Pts',(10.7564046409999,15.2,2.78370946299999));
#197823=CARTESIAN_POINT('Ctrl Pts',(10.7596415739999,15.2,2.78331041399999));
#197824=CARTESIAN_POINT('Ctrl Pts',(10.7628831919999,15.2,2.78290815599998));
#197825=CARTESIAN_POINT('Ctrl Pts',(10.7661294859999,15.2,2.78250268399999));
#197826=CARTESIAN_POINT('Ctrl Pts',(10.7693804469999,15.2,2.78209399099998));
#197827=CARTESIAN_POINT('Ctrl Pts',(10.7726360659999,15.2,2.78168207299998));
#197828=CARTESIAN_POINT('Ctrl Pts',(10.7758963329999,15.2,2.78126692399999));
#197829=CARTESIAN_POINT('Ctrl Pts',(10.7791612379999,15.2,2.78084853699998));
#197830=CARTESIAN_POINT('Ctrl Pts',(10.7824307749999,15.2,2.78042690799998));
#197831=CARTESIAN_POINT('Ctrl Pts',(10.7857049309999,15.2,2.78000203199999));
#197832=CARTESIAN_POINT('Ctrl Pts',(10.7889836979999,15.2,2.77957390099999));
#197833=CARTESIAN_POINT('Ctrl Pts',(10.7922670679999,15.2,2.77914250999999));
#197834=CARTESIAN_POINT('Ctrl Pts',(10.7955550299999,15.2,2.77870785499999));
#197835=CARTESIAN_POINT('Ctrl Pts',(10.7988475759999,15.2,2.77826992999999));
#197836=CARTESIAN_POINT('Ctrl Pts',(10.8021446959999,15.2,2.77782872899999));
#197837=CARTESIAN_POINT('Ctrl Pts',(10.8054463819999,15.2,2.77738424699999));
#197838=CARTESIAN_POINT('Ctrl Pts',(10.8087526239999,15.2,2.77693647799998));
#197839=CARTESIAN_POINT('Ctrl Pts',(10.8120634119999,15.2,2.77648541599999));
#197840=CARTESIAN_POINT('Ctrl Pts',(10.8153787389999,15.2,2.77603105699999));
#197841=CARTESIAN_POINT('Ctrl Pts',(10.8186985939999,15.2,2.77557339599999));
#197842=CARTESIAN_POINT('Ctrl Pts',(10.8220229679999,15.2,2.77511242599999));
#197843=CARTESIAN_POINT('Ctrl Pts',(10.8253518549999,15.2,2.77464814099999));
#197844=CARTESIAN_POINT('Ctrl Pts',(10.8286852409999,15.2,2.77418053799998));
#197845=CARTESIAN_POINT('Ctrl Pts',(10.8320231199999,15.2,2.77370960999999));
#197846=CARTESIAN_POINT('Ctrl Pts',(10.8353654819999,15.2,2.77323535299999));
#197847=CARTESIAN_POINT('Ctrl Pts',(10.8387123189999,15.2,2.77275775999998));
#197848=CARTESIAN_POINT('Ctrl Pts',(10.8420636209999,15.2,2.77227682699999));
#197849=CARTESIAN_POINT('Ctrl Pts',(10.8454193789999,15.2,2.77179254799999));
#197850=CARTESIAN_POINT('Ctrl Pts',(10.8487795839999,15.2,2.77130491799999));
#197851=CARTESIAN_POINT('Ctrl Pts',(10.8521442279999,15.2,2.77081393199998));
#197852=CARTESIAN_POINT('Ctrl Pts',(10.8555133009999,15.2,2.77031958499999));
#197853=CARTESIAN_POINT('Ctrl Pts',(10.8588867929999,15.2,2.76982187099998));
#197854=CARTESIAN_POINT('Ctrl Pts',(10.8622646979999,15.2,2.76932078499998));
#197855=CARTESIAN_POINT('Ctrl Pts',(10.8656470049999,15.2,2.76881632399999));
#197856=CARTESIAN_POINT('Ctrl Pts',(10.8690337059999,15.2,2.76830847799998));
#197857=CARTESIAN_POINT('Ctrl Pts',(10.8724247909999,15.2,2.76779724699999));
#197858=CARTESIAN_POINT('Ctrl Pts',(10.8758202519999,15.2,2.76728262299999));
#197859=CARTESIAN_POINT('Ctrl Pts',(10.8792200789999,15.2,2.76676460199998));
#197860=CARTESIAN_POINT('Ctrl Pts',(10.8826242649999,15.2,2.76624317899999));
#197861=CARTESIAN_POINT('Ctrl Pts',(10.8860327999999,15.2,2.76571834699999));
#197862=CARTESIAN_POINT('Ctrl Pts',(10.8894456749999,15.2,2.76519010299998));
#197863=CARTESIAN_POINT('Ctrl Pts',(10.8928628809999,15.2,2.76465844099998));
#197864=CARTESIAN_POINT('Ctrl Pts',(10.8962844109999,15.2,2.76412335799999));
#197865=CARTESIAN_POINT('Ctrl Pts',(10.8997102529999,15.2,2.76358484599999));
#197866=CARTESIAN_POINT('Ctrl Pts',(10.9031404009999,15.2,2.76304290199998));
#197867=CARTESIAN_POINT('Ctrl Pts',(10.9065748449999,15.2,2.76249751999998));
#197868=CARTESIAN_POINT('Ctrl Pts',(10.9100135769999,15.2,2.76194869599999));
#197869=CARTESIAN_POINT('Ctrl Pts',(10.9134565879999,15.2,2.76139642399999));
#197870=CARTESIAN_POINT('Ctrl Pts',(10.9169038679999,15.2,2.76084069999998));
#197871=CARTESIAN_POINT('Ctrl Pts',(10.9203554099999,15.2,2.76028151899999));
#197872=CARTESIAN_POINT('Ctrl Pts',(10.9238112039999,15.2,2.75971887599999));
#197873=CARTESIAN_POINT('Ctrl Pts',(10.9272712419999,15.2,2.75915276599999));
#197874=CARTESIAN_POINT('Ctrl Pts',(10.9307355149999,15.2,2.75858318399998));
#197875=CARTESIAN_POINT('Ctrl Pts',(10.9342040149999,15.2,2.75801012499999));
#197876=CARTESIAN_POINT('Ctrl Pts',(10.9376767319999,15.2,2.75743358499999));
#197877=CARTESIAN_POINT('Ctrl Pts',(10.9411536579999,15.2,2.75685355899999));
#197878=CARTESIAN_POINT('Ctrl Pts',(10.9446347859999,15.2,2.75627004099999));
#197879=CARTESIAN_POINT('Ctrl Pts',(10.9481201049999,15.2,2.75568302799999));
#197880=CARTESIAN_POINT('Ctrl Pts',(10.9516096059999,15.2,2.75509251399999));
#197881=CARTESIAN_POINT('Ctrl Pts',(10.9551032829999,15.2,2.75449849499999));
#197882=CARTESIAN_POINT('Ctrl Pts',(10.9586011259999,15.2,2.75390096599998));
#197883=CARTESIAN_POINT('Ctrl Pts',(10.9621031259999,15.2,2.75329992099999));
#197884=CARTESIAN_POINT('Ctrl Pts',(10.9656092739999,15.2,2.75269535799998));
#197885=CARTESIAN_POINT('Ctrl Pts',(10.9691195629999,15.2,2.75208726999999));
#197886=CARTESIAN_POINT('Ctrl Pts',(10.9726339839999,15.2,2.75147565399998));
#197887=CARTESIAN_POINT('Ctrl Pts',(10.9761525279999,15.2,2.75086050399998));
#197888=CARTESIAN_POINT('Ctrl Pts',(10.9796751869999,15.2,2.75024181699998));
#197889=CARTESIAN_POINT('Ctrl Pts',(10.9832019509999,15.2,2.74961958599999));
#197890=CARTESIAN_POINT('Ctrl Pts',(10.9867328139999,15.2,2.74899380799998));
#197891=CARTESIAN_POINT('Ctrl Pts',(10.9902677649999,15.2,2.74836447799998));
#197892=CARTESIAN_POINT('Ctrl Pts',(10.9938067979999,15.2,2.74773159199999));
#197893=CARTESIAN_POINT('Ctrl Pts',(10.9973499019999,15.2,2.74709514499998));
#197894=CARTESIAN_POINT('Ctrl Pts',(11.0008970699999,15.2,2.74645513199999));
#197895=CARTESIAN_POINT('Ctrl Pts',(11.0044482939999,15.2,2.74581154899998));
#197896=CARTESIAN_POINT('Ctrl Pts',(11.0080035629999,15.2,2.74516439199999));
#197897=CARTESIAN_POINT('Ctrl Pts',(11.0115628719999,15.2,2.74451365599998));
#197898=CARTESIAN_POINT('Ctrl Pts',(11.0151262099999,15.2,2.74385933599999));
#197899=CARTESIAN_POINT('Ctrl Pts',(11.0186935709999,15.2,2.74320142899998));
#197900=CARTESIAN_POINT('Ctrl Pts',(11.0222649439999,15.2,2.74253992799999));
#197901=CARTESIAN_POINT('Ctrl Pts',(11.0258403219999,15.2,2.74187483099999));
#197902=CARTESIAN_POINT('Ctrl Pts',(11.0294196959999,15.2,2.74120613199998));
#197903=CARTESIAN_POINT('Ctrl Pts',(11.0330030589999,15.2,2.74053382799998));
#197904=CARTESIAN_POINT('Ctrl Pts',(11.0365903999999,15.2,2.73985791299998));
#197905=CARTESIAN_POINT('Ctrl Pts',(11.0401817149999,15.2,2.73917838399999));
#197906=CARTESIAN_POINT('Ctrl Pts',(11.0437769909999,15.2,2.73849523599999));
#197907=CARTESIAN_POINT('Ctrl Pts',(11.0473762219999,15.2,2.73780846599998));
#197908=CARTESIAN_POINT('Ctrl Pts',(11.0509794009999,15.2,2.73711806699998));
#197909=CARTESIAN_POINT('Ctrl Pts',(11.0545865169999,15.2,2.73642403699998));
#197910=CARTESIAN_POINT('Ctrl Pts',(11.0581975619999,15.2,2.73572636999998));
#197911=CARTESIAN_POINT('Ctrl Pts',(11.0618125299999,15.2,2.73502506399999));
#197912=CARTESIAN_POINT('Ctrl Pts',(11.0654314099999,15.2,2.73432011199999));
#197913=CARTESIAN_POINT('Ctrl Pts',(11.0690541959999,15.2,2.73361151099999));
#197914=CARTESIAN_POINT('Ctrl Pts',(11.0726808779999,15.2,2.73289925699999));
#197915=CARTESIAN_POINT('Ctrl Pts',(11.0763114489999,15.2,2.73218334499998));
#197916=CARTESIAN_POINT('Ctrl Pts',(11.0799458989999,15.2,2.73146377099999));
#197917=CARTESIAN_POINT('Ctrl Pts',(11.0835842229999,15.2,2.73074053299998));
#197918=CARTESIAN_POINT('Ctrl Pts',(11.0872264109999,15.2,2.73001362299999));
#197919=CARTESIAN_POINT('Ctrl Pts',(11.0908724549999,15.2,2.72928304099998));
#197920=CARTESIAN_POINT('Ctrl Pts',(11.0945223469999,15.2,2.72854877899999));
#197921=CARTESIAN_POINT('Ctrl Pts',(11.0981760779999,15.2,2.72781083499999));
#197922=CARTESIAN_POINT('Ctrl Pts',(11.1018336399999,15.2,2.72706920299999));
#197923=CARTESIAN_POINT('Ctrl Pts',(11.1054950239999,15.2,2.72632388099999));
#197924=CARTESIAN_POINT('Ctrl Pts',(11.1091602219999,15.2,2.72557486299998));
#197925=CARTESIAN_POINT('Ctrl Pts',(11.1128292269999,15.2,2.72482214499998));
#197926=CARTESIAN_POINT('Ctrl Pts',(11.1165020289999,15.2,2.72406572399999));
#197927=CARTESIAN_POINT('Ctrl Pts',(11.1201786229999,15.2,2.72330559599999));
#197928=CARTESIAN_POINT('Ctrl Pts',(11.1238589999999,15.2,2.72254175699998));
#197929=CARTESIAN_POINT('Ctrl Pts',(11.1275431529999,15.2,2.72177420499998));
#197930=CARTESIAN_POINT('Ctrl Pts',(11.1312310749999,15.2,2.72100293299999));
#197931=CARTESIAN_POINT('Ctrl Pts',(11.1349227589999,15.2,2.72022793899998));
#197932=CARTESIAN_POINT('Ctrl Pts',(11.1386181909999,15.2,2.71944921899999));
#197933=CARTESIAN_POINT('Ctrl Pts',(11.1423173659999,15.2,2.71866676499998));
#197934=CARTESIAN_POINT('Ctrl Pts',(11.1460202709999,15.2,2.71788057599998));
#197935=CARTESIAN_POINT('Ctrl Pts',(11.1497268969999,15.2,2.71709064499999));
#197936=CARTESIAN_POINT('Ctrl Pts',(11.1534372359999,15.2,2.71629696699998));
#197937=CARTESIAN_POINT('Ctrl Pts',(11.1571512799999,15.2,2.71549953899999));
#197938=CARTESIAN_POINT('Ctrl Pts',(11.1608690239999,15.2,2.71469835899998));
#197939=CARTESIAN_POINT('Ctrl Pts',(11.1645904639999,15.2,2.71389342499998));
#197940=CARTESIAN_POINT('Ctrl Pts',(11.1683155989999,15.2,2.71308473599999));
#197941=CARTESIAN_POINT('Ctrl Pts',(11.1712986599999,15.2,2.71243477999998));
#197942=CARTESIAN_POINT('Ctrl Pts',(11.1735376169999,15.2,2.71194562399998));
#197943=CARTESIAN_POINT('Ctrl Pts',(11.1750309949999,15.2,2.71161876799999));
#197944=CARTESIAN_POINT('Ctrl Pts',(11.1757778679999,15.2,2.71145515299998));
#197945=CARTESIAN_POINT('Origin',(-5.66257110645729E-14,15.2,-1.77635683940025E-14));
#197946=CARTESIAN_POINT('',(9.86852965744612,15.2,3.20199116236993));
#197947=CARTESIAN_POINT('',(9.86852965744613,12.2,3.20199116236993));
#197948=CARTESIAN_POINT('',(9.86852965699994,15.2,3.20199116199999));
#197949=CARTESIAN_POINT('Origin',(-5.66257110645729E-14,12.2,-1.77635683940025E-14));
#197950=CARTESIAN_POINT('Origin',(-5.66257110645729E-14,15.2,-1.77635683940025E-14));
#197951=CARTESIAN_POINT('Origin',(-5.66257110645729E-14,15.2,-1.77635683940025E-14));
#197952=CARTESIAN_POINT('',(10.8127719249999,15.2,3.91586047999999));
#197953=CARTESIAN_POINT('',(10.6761442619999,15.2,4.27433546899999));
#197954=CARTESIAN_POINT('Origin',(-5.66257110645729E-14,15.2,-1.77635683940025E-14));
#197955=CARTESIAN_POINT('',(10.6761442619999,12.2,4.27433546899999));
#197956=CARTESIAN_POINT('',(10.6761442619999,15.2,4.27433546899999));
#197957=CARTESIAN_POINT('',(10.8127719249999,12.2,3.91586047999999));
#197958=CARTESIAN_POINT('Origin',(-5.66257110645729E-14,12.2,-1.77635683940025E-14));
#197959=CARTESIAN_POINT('',(10.8127719249999,15.2,3.91586047999999));
#197960=CARTESIAN_POINT('Ctrl Pts',(10.6761442619999,15.2,4.27433546899999));
#197961=CARTESIAN_POINT('Ctrl Pts',(10.6761442619999,11.6,4.27433546899999));
#197962=CARTESIAN_POINT('Ctrl Pts',(10.6753817049999,15.2,4.27439112799998));
#197963=CARTESIAN_POINT('Ctrl Pts',(10.6753817049999,11.6,4.27439112799998));
#197964=CARTESIAN_POINT('Ctrl Pts',(10.6738570129999,15.2,4.27450212599998));
#197965=CARTESIAN_POINT('Ctrl Pts',(10.6738570129999,11.6,4.27450212599998));
#197966=CARTESIAN_POINT('Ctrl Pts',(10.6715712299999,15.2,4.27466766699999));
#197967=CARTESIAN_POINT('Ctrl Pts',(10.6715712299999,11.6,4.27466766699998));
#197968=CARTESIAN_POINT('Ctrl Pts',(10.6685260339999,15.2,4.27488647299998));
#197969=CARTESIAN_POINT('Ctrl Pts',(10.6685260339999,11.6,4.27488647299998));
#197970=CARTESIAN_POINT('Ctrl Pts',(10.6647237269999,15.2,4.27515678899999));
#197971=CARTESIAN_POINT('Ctrl Pts',(10.6647237269999,11.6,4.27515678899999));
#197972=CARTESIAN_POINT('Ctrl Pts',(10.6609256119999,15.2,4.27542391299998));
#197973=CARTESIAN_POINT('Ctrl Pts',(10.6609256119999,11.6,4.27542391299998));
#197974=CARTESIAN_POINT('Ctrl Pts',(10.6571316899999,15.2,4.27568784899999));
#197975=CARTESIAN_POINT('Ctrl Pts',(10.6571316899999,11.6,4.27568784899999));
#197976=CARTESIAN_POINT('Ctrl Pts',(10.6533419639999,15.2,4.27594859599999));
#197977=CARTESIAN_POINT('Ctrl Pts',(10.6533419639999,11.6,4.27594859599999));
#197978=CARTESIAN_POINT('Ctrl Pts',(10.6495564379999,15.2,4.27620615899999));
#197979=CARTESIAN_POINT('Ctrl Pts',(10.6495564379999,11.6,4.27620615899999));
#197980=CARTESIAN_POINT('Ctrl Pts',(10.6457751209999,15.2,4.27646054299998));
#197981=CARTESIAN_POINT('Ctrl Pts',(10.6457751209999,11.6,4.27646054299998));
#197982=CARTESIAN_POINT('Ctrl Pts',(10.6419980199999,15.2,4.27671175199999));
#197983=CARTESIAN_POINT('Ctrl Pts',(10.6419980199999,11.6,4.27671175199999));
#197984=CARTESIAN_POINT('Ctrl Pts',(10.6382251429999,15.2,4.27695979399999));
#197985=CARTESIAN_POINT('Ctrl Pts',(10.6382251429999,11.6,4.27695979399999));
#197986=CARTESIAN_POINT('Ctrl Pts',(10.6344565009999,15.2,4.27720467299999));
#197987=CARTESIAN_POINT('Ctrl Pts',(10.6344565009999,11.6,4.27720467299998));
#197988=CARTESIAN_POINT('Ctrl Pts',(10.6306921009999,15.2,4.27744639699998));
#197989=CARTESIAN_POINT('Ctrl Pts',(10.6306921009999,11.6,4.27744639699998));
#197990=CARTESIAN_POINT('Ctrl Pts',(10.6269319529999,15.2,4.27768497199998));
#197991=CARTESIAN_POINT('Ctrl Pts',(10.6269319529999,11.6,4.27768497199998));
#197992=CARTESIAN_POINT('Ctrl Pts',(10.6231760649999,15.2,4.27792040299998));
#197993=CARTESIAN_POINT('Ctrl Pts',(10.6231760649999,11.6,4.27792040299998));
#197994=CARTESIAN_POINT('Ctrl Pts',(10.6194244419999,15.2,4.27815269399999));
#197995=CARTESIAN_POINT('Ctrl Pts',(10.6194244419999,11.6,4.27815269399998));
#197996=CARTESIAN_POINT('Ctrl Pts',(10.6156770939999,15.2,4.27838185099999));
#197997=CARTESIAN_POINT('Ctrl Pts',(10.6156770939999,11.6,4.27838185099999));
#197998=CARTESIAN_POINT('Ctrl Pts',(10.6119340259999,15.2,4.27860787899998));
#197999=CARTESIAN_POINT('Ctrl Pts',(10.6119340259999,11.6,4.27860787899998));
#198000=CARTESIAN_POINT('Ctrl Pts',(10.6081952429999,15.2,4.27883078099998));
#198001=CARTESIAN_POINT('Ctrl Pts',(10.6081952429999,11.6,4.27883078099998));
#198002=CARTESIAN_POINT('Ctrl Pts',(10.6044607549999,15.2,4.27905056299998));
#198003=CARTESIAN_POINT('Ctrl Pts',(10.6044607549999,11.6,4.27905056299998));
#198004=CARTESIAN_POINT('Ctrl Pts',(10.6007305679999,15.2,4.27926722899999));
#198005=CARTESIAN_POINT('Ctrl Pts',(10.6007305679999,11.6,4.27926722899999));
#198006=CARTESIAN_POINT('Ctrl Pts',(10.5970046899999,15.2,4.27948078699998));
#198007=CARTESIAN_POINT('Ctrl Pts',(10.5970046899999,11.6,4.27948078699998));
#198008=CARTESIAN_POINT('Ctrl Pts',(10.5932831279999,15.2,4.27969123999999));
#198009=CARTESIAN_POINT('Ctrl Pts',(10.5932831279999,11.6,4.27969123999999));
#198010=CARTESIAN_POINT('Ctrl Pts',(10.5895658899999,15.2,4.27989859399998));
#198011=CARTESIAN_POINT('Ctrl Pts',(10.5895658899999,11.6,4.27989859399998));
#198012=CARTESIAN_POINT('Ctrl Pts',(10.5858529849999,15.2,4.28010285499998));
#198013=CARTESIAN_POINT('Ctrl Pts',(10.5858529849999,11.6,4.28010285499998));
#198014=CARTESIAN_POINT('Ctrl Pts',(10.5821444189999,15.2,4.28030402799998));
#198015=CARTESIAN_POINT('Ctrl Pts',(10.5821444189999,11.6,4.28030402799998));
#198016=CARTESIAN_POINT('Ctrl Pts',(10.5784402009999,15.2,4.28050211799999));
#198017=CARTESIAN_POINT('Ctrl Pts',(10.5784402009999,11.6,4.28050211799999));
#198018=CARTESIAN_POINT('Ctrl Pts',(10.5747403369999,15.2,4.28069712999999));
#198019=CARTESIAN_POINT('Ctrl Pts',(10.5747403369999,11.6,4.28069712999999));
#198020=CARTESIAN_POINT('Ctrl Pts',(10.5710448359999,15.2,4.28088907099998));
#198021=CARTESIAN_POINT('Ctrl Pts',(10.5710448359999,11.6,4.28088907099998));
#198022=CARTESIAN_POINT('Ctrl Pts',(10.5673537039999,15.2,4.28107794499999));
#198023=CARTESIAN_POINT('Ctrl Pts',(10.5673537039999,11.6,4.28107794499999));
#198024=CARTESIAN_POINT('Ctrl Pts',(10.5636669489999,15.2,4.28126375699998));
#198025=CARTESIAN_POINT('Ctrl Pts',(10.5636669489999,11.6,4.28126375699998));
#198026=CARTESIAN_POINT('Ctrl Pts',(10.5599845779999,15.2,4.28144651299998));
#198027=CARTESIAN_POINT('Ctrl Pts',(10.5599845779999,11.6,4.28144651299998));
#198028=CARTESIAN_POINT('Ctrl Pts',(10.5563065999999,15.2,4.28162621899999));
#198029=CARTESIAN_POINT('Ctrl Pts',(10.5563065999999,11.6,4.28162621899998));
#198030=CARTESIAN_POINT('Ctrl Pts',(10.5526330209999,15.2,4.28180287899998));
#198031=CARTESIAN_POINT('Ctrl Pts',(10.5526330209999,11.6,4.28180287899998));
#198032=CARTESIAN_POINT('Ctrl Pts',(10.5489638489999,15.2,4.28197649899998));
#198033=CARTESIAN_POINT('Ctrl Pts',(10.5489638489999,11.6,4.28197649899998));
#198034=CARTESIAN_POINT('Ctrl Pts',(10.5452990929999,15.2,4.28214708399998));
#198035=CARTESIAN_POINT('Ctrl Pts',(10.5452990929999,11.6,4.28214708399998));
#198036=CARTESIAN_POINT('Ctrl Pts',(10.5416387579999,15.2,4.28231463999998));
#198037=CARTESIAN_POINT('Ctrl Pts',(10.5416387579999,11.6,4.28231463999998));
#198038=CARTESIAN_POINT('Ctrl Pts',(10.5379828539999,15.2,4.28247917299998));
#198039=CARTESIAN_POINT('Ctrl Pts',(10.5379828539999,11.6,4.28247917299998));
#198040=CARTESIAN_POINT('Ctrl Pts',(10.5343313879999,15.2,4.28264068899999));
#198041=CARTESIAN_POINT('Ctrl Pts',(10.5343313879999,11.6,4.28264068899998));
#198042=CARTESIAN_POINT('Ctrl Pts',(10.5306843669999,15.2,4.28279919099998));
#198043=CARTESIAN_POINT('Ctrl Pts',(10.5306843669999,11.6,4.28279919099998));
#198044=CARTESIAN_POINT('Ctrl Pts',(10.5270417989999,15.2,4.28295468699999));
#198045=CARTESIAN_POINT('Ctrl Pts',(10.5270417989999,11.6,4.28295468699999));
#198046=CARTESIAN_POINT('Ctrl Pts',(10.5234036919999,15.2,4.28310718099999));
#198047=CARTESIAN_POINT('Ctrl Pts',(10.5234036919999,11.6,4.28310718099999));
#198048=CARTESIAN_POINT('Ctrl Pts',(10.5197700539999,15.2,4.28325667899998));
#198049=CARTESIAN_POINT('Ctrl Pts',(10.5197700539999,11.6,4.28325667899998));
#198050=CARTESIAN_POINT('Ctrl Pts',(10.5161408899999,15.2,4.28340318599999));
#198051=CARTESIAN_POINT('Ctrl Pts',(10.5161408899999,11.6,4.28340318599999));
#198052=CARTESIAN_POINT('Ctrl Pts',(10.5125162099999,15.2,4.28354670899999));
#198053=CARTESIAN_POINT('Ctrl Pts',(10.5125162099999,11.6,4.28354670899999));
#198054=CARTESIAN_POINT('Ctrl Pts',(10.5088960219999,15.2,4.28368725399999));
#198055=CARTESIAN_POINT('Ctrl Pts',(10.5088960219999,11.6,4.28368725399999));
#198056=CARTESIAN_POINT('Ctrl Pts',(10.5052803329999,15.2,4.28382482399999));
#198057=CARTESIAN_POINT('Ctrl Pts',(10.5052803329999,11.6,4.28382482399999));
#198058=CARTESIAN_POINT('Ctrl Pts',(10.5016691499999,15.2,4.28395942599998));
#198059=CARTESIAN_POINT('Ctrl Pts',(10.5016691499999,11.6,4.28395942599998));
#198060=CARTESIAN_POINT('Ctrl Pts',(10.4980624809999,15.2,4.28409106699998));
#198061=CARTESIAN_POINT('Ctrl Pts',(10.4980624809999,11.6,4.28409106699998));
#198062=CARTESIAN_POINT('Ctrl Pts',(10.4944603349999,15.2,4.28421974999999));
#198063=CARTESIAN_POINT('Ctrl Pts',(10.4944603349999,11.6,4.28421974999999));
#198064=CARTESIAN_POINT('Ctrl Pts',(10.4908627189999,15.2,4.28434548299998));
#198065=CARTESIAN_POINT('Ctrl Pts',(10.4908627189999,11.6,4.28434548299998));
#198066=CARTESIAN_POINT('Ctrl Pts',(10.4872696399999,15.2,4.28446827099998));
#198067=CARTESIAN_POINT('Ctrl Pts',(10.4872696399999,11.6,4.28446827099998));
#198068=CARTESIAN_POINT('Ctrl Pts',(10.4836811069999,15.2,4.28458811899999));
#198069=CARTESIAN_POINT('Ctrl Pts',(10.4836811069999,11.6,4.28458811899999));
#198070=CARTESIAN_POINT('Ctrl Pts',(10.4800971249999,15.2,4.28470503199998));
#198071=CARTESIAN_POINT('Ctrl Pts',(10.4800971249999,11.6,4.28470503199998));
#198072=CARTESIAN_POINT('Ctrl Pts',(10.4765177049999,15.2,4.28481901899998));
#198073=CARTESIAN_POINT('Ctrl Pts',(10.4765177049999,11.6,4.28481901899998));
#198074=CARTESIAN_POINT('Ctrl Pts',(10.4729428539999,15.2,4.28493008299998));
#198075=CARTESIAN_POINT('Ctrl Pts',(10.4729428539999,11.6,4.28493008299998));
#198076=CARTESIAN_POINT('Ctrl Pts',(10.4693725789999,15.2,4.28503822999998));
#198077=CARTESIAN_POINT('Ctrl Pts',(10.4693725789999,11.6,4.28503822999998));
#198078=CARTESIAN_POINT('Ctrl Pts',(10.4658068879999,15.2,4.28514346699998));
#198079=CARTESIAN_POINT('Ctrl Pts',(10.4658068879999,11.6,4.28514346699998));
#198080=CARTESIAN_POINT('Ctrl Pts',(10.4622457879999,15.2,4.28524579899998));
#198081=CARTESIAN_POINT('Ctrl Pts',(10.4622457879999,11.6,4.28524579899998));
#198082=CARTESIAN_POINT('Ctrl Pts',(10.4586892889999,15.2,4.28534523199998));
#198083=CARTESIAN_POINT('Ctrl Pts',(10.4586892889999,11.6,4.28534523199998));
#198084=CARTESIAN_POINT('Ctrl Pts',(10.4551373969999,15.2,4.28544177099998));
#198085=CARTESIAN_POINT('Ctrl Pts',(10.4551373969999,11.6,4.28544177099998));
#198086=CARTESIAN_POINT('Ctrl Pts',(10.4515901199999,15.2,4.28553542399998));
#198087=CARTESIAN_POINT('Ctrl Pts',(10.4515901199999,11.6,4.28553542399998));
#198088=CARTESIAN_POINT('Ctrl Pts',(10.4480474659999,15.2,4.28562619399998));
#198089=CARTESIAN_POINT('Ctrl Pts',(10.4480474659999,11.6,4.28562619399998));
#198090=CARTESIAN_POINT('Ctrl Pts',(10.4445094429999,15.2,4.28571408999999));
#198091=CARTESIAN_POINT('Ctrl Pts',(10.4445094429999,11.6,4.28571408999998));
#198092=CARTESIAN_POINT('Ctrl Pts',(10.4409760589999,15.2,4.28579911599999));
#198093=CARTESIAN_POINT('Ctrl Pts',(10.4409760589999,11.6,4.28579911599999));
#198094=CARTESIAN_POINT('Ctrl Pts',(10.4374473219999,15.2,4.28588127799999));
#198095=CARTESIAN_POINT('Ctrl Pts',(10.4374473219999,11.6,4.28588127799998));
#198096=CARTESIAN_POINT('Ctrl Pts',(10.4339232389999,15.2,4.28596058199999));
#198097=CARTESIAN_POINT('Ctrl Pts',(10.4339232389999,11.6,4.28596058199999));
#198098=CARTESIAN_POINT('Ctrl Pts',(10.4304038179999,15.2,4.28603703499999));
#198099=CARTESIAN_POINT('Ctrl Pts',(10.4304038179999,11.6,4.28603703499998));
#198100=CARTESIAN_POINT('Ctrl Pts',(10.4268890689999,15.2,4.28611064199998));
#198101=CARTESIAN_POINT('Ctrl Pts',(10.4268890689999,11.6,4.28611064199998));
#198102=CARTESIAN_POINT('Ctrl Pts',(10.4233789969999,15.2,4.28618140899999));
#198103=CARTESIAN_POINT('Ctrl Pts',(10.4233789969999,11.6,4.28618140899999));
#198104=CARTESIAN_POINT('Ctrl Pts',(10.4198736109999,15.2,4.28624934199998));
#198105=CARTESIAN_POINT('Ctrl Pts',(10.4198736109999,11.6,4.28624934199998));
#198106=CARTESIAN_POINT('Ctrl Pts',(10.4163729199999,15.2,4.28631444799999));
#198107=CARTESIAN_POINT('Ctrl Pts',(10.4163729199999,11.6,4.28631444799999));
#198108=CARTESIAN_POINT('Ctrl Pts',(10.4128769299999,15.2,4.28637673099999));
#198109=CARTESIAN_POINT('Ctrl Pts',(10.4128769299999,11.6,4.28637673099998));
#198110=CARTESIAN_POINT('Ctrl Pts',(10.4093856499999,15.2,4.28643619999999));
#198111=CARTESIAN_POINT('Ctrl Pts',(10.4093856499999,11.6,4.28643619999998));
#198112=CARTESIAN_POINT('Ctrl Pts',(10.4058990889999,15.2,4.28649285799998));
#198113=CARTESIAN_POINT('Ctrl Pts',(10.4058990889999,11.6,4.28649285799998));
#198114=CARTESIAN_POINT('Ctrl Pts',(10.4024172519999,15.2,4.28654671399999));
#198115=CARTESIAN_POINT('Ctrl Pts',(10.4024172519999,11.6,4.28654671399998));
#198116=CARTESIAN_POINT('Ctrl Pts',(10.3989401499999,15.2,4.28659777199999));
#198117=CARTESIAN_POINT('Ctrl Pts',(10.3989401499999,11.6,4.28659777199999));
#198118=CARTESIAN_POINT('Ctrl Pts',(10.3954677879999,15.2,4.28664603899998));
#198119=CARTESIAN_POINT('Ctrl Pts',(10.3954677879999,11.6,4.28664603899998));
#198120=CARTESIAN_POINT('Ctrl Pts',(10.3920001779999,15.2,4.28669152099998));
#198121=CARTESIAN_POINT('Ctrl Pts',(10.3920001779999,11.6,4.28669152099998));
#198122=CARTESIAN_POINT('Ctrl Pts',(10.3885373239999,15.2,4.28673422399999));
#198123=CARTESIAN_POINT('Ctrl Pts',(10.3885373239999,11.6,4.28673422399999));
#198124=CARTESIAN_POINT('Ctrl Pts',(10.3850792369999,15.2,4.28677415499998));
#198125=CARTESIAN_POINT('Ctrl Pts',(10.3850792369999,11.6,4.28677415499998));
#198126=CARTESIAN_POINT('Ctrl Pts',(10.3816259229999,15.2,4.28681131999999));
#198127=CARTESIAN_POINT('Ctrl Pts',(10.3816259229999,11.6,4.28681131999998));
#198128=CARTESIAN_POINT('Ctrl Pts',(10.3781773909999,15.2,4.28684572399998));
#198129=CARTESIAN_POINT('Ctrl Pts',(10.3781773909999,11.6,4.28684572399998));
#198130=CARTESIAN_POINT('Ctrl Pts',(10.3747336489999,15.2,4.28687737299998));
#198131=CARTESIAN_POINT('Ctrl Pts',(10.3747336489999,11.6,4.28687737299998));
#198132=CARTESIAN_POINT('Ctrl Pts',(10.3712947049999,15.2,4.28690627599998));
#198133=CARTESIAN_POINT('Ctrl Pts',(10.3712947049999,11.6,4.28690627599998));
#198134=CARTESIAN_POINT('Ctrl Pts',(10.3678605659999,15.2,4.28693243699998));
#198135=CARTESIAN_POINT('Ctrl Pts',(10.3678605659999,11.6,4.28693243699998));
#198136=CARTESIAN_POINT('Ctrl Pts',(10.3644312409999,15.2,4.28695586399999));
#198137=CARTESIAN_POINT('Ctrl Pts',(10.3644312409999,11.6,4.28695586399999));
#198138=CARTESIAN_POINT('Ctrl Pts',(10.3610067379999,15.2,4.28697656099998));
#198139=CARTESIAN_POINT('Ctrl Pts',(10.3610067379999,11.6,4.28697656099998));
#198140=CARTESIAN_POINT('Ctrl Pts',(10.3575870659999,15.2,4.28699453699998));
#198141=CARTESIAN_POINT('Ctrl Pts',(10.3575870659999,11.6,4.28699453699998));
#198142=CARTESIAN_POINT('Ctrl Pts',(10.3541722309999,15.2,4.28700979599999));
#198143=CARTESIAN_POINT('Ctrl Pts',(10.3541722309999,11.6,4.28700979599998));
#198144=CARTESIAN_POINT('Ctrl Pts',(10.3507622439999,15.2,4.28702234599999));
#198145=CARTESIAN_POINT('Ctrl Pts',(10.3507622439999,11.6,4.28702234599999));
#198146=CARTESIAN_POINT('Ctrl Pts',(10.3473571099999,15.2,4.28703219199999));
#198147=CARTESIAN_POINT('Ctrl Pts',(10.3473571099999,11.6,4.28703219199999));
#198148=CARTESIAN_POINT('Ctrl Pts',(10.3439568399999,15.2,4.28703934199999));
#198149=CARTESIAN_POINT('Ctrl Pts',(10.3439568399999,11.6,4.28703934199999));
#198150=CARTESIAN_POINT('Ctrl Pts',(10.3405614389999,15.2,4.28704380099998));
#198151=CARTESIAN_POINT('Ctrl Pts',(10.3405614389999,11.6,4.28704380099998));
#198152=CARTESIAN_POINT('Ctrl Pts',(10.3371709179999,15.2,4.28704557699999));
#198153=CARTESIAN_POINT('Ctrl Pts',(10.3371709179999,11.6,4.28704557699999));
#198154=CARTESIAN_POINT('Ctrl Pts',(10.3337852839999,15.2,4.28704467399999));
#198155=CARTESIAN_POINT('Ctrl Pts',(10.3337852839999,11.6,4.28704467399999));
#198156=CARTESIAN_POINT('Ctrl Pts',(10.3304045439999,15.2,4.28704110199998));
#198157=CARTESIAN_POINT('Ctrl Pts',(10.3304045439999,11.6,4.28704110199998));
#198158=CARTESIAN_POINT('Ctrl Pts',(10.3270287089999,15.2,4.28703486399999));
#198159=CARTESIAN_POINT('Ctrl Pts',(10.3270287089999,11.6,4.28703486399998));
#198160=CARTESIAN_POINT('Ctrl Pts',(10.3236577839999,15.2,4.28702596899999));
#198161=CARTESIAN_POINT('Ctrl Pts',(10.3236577839999,11.6,4.28702596899999));
#198162=CARTESIAN_POINT('Ctrl Pts',(10.3202917799999,15.2,4.28701442299998));
#198163=CARTESIAN_POINT('Ctrl Pts',(10.3202917799999,11.6,4.28701442299998));
#198164=CARTESIAN_POINT('Ctrl Pts',(10.3169307029999,15.2,4.28700023099999));
#198165=CARTESIAN_POINT('Ctrl Pts',(10.3169307029999,11.6,4.28700023099999));
#198166=CARTESIAN_POINT('Ctrl Pts',(10.3135745629999,15.2,4.28698340099999));
#198167=CARTESIAN_POINT('Ctrl Pts',(10.3135745629999,11.6,4.28698340099999));
#198168=CARTESIAN_POINT('Ctrl Pts',(10.3102233669999,15.2,4.28696393999999));
#198169=CARTESIAN_POINT('Ctrl Pts',(10.3102233669999,11.6,4.28696393999999));
#198170=CARTESIAN_POINT('Ctrl Pts',(10.3068771239999,15.2,4.28694185499998));
#198171=CARTESIAN_POINT('Ctrl Pts',(10.3068771239999,11.6,4.28694185499998));
#198172=CARTESIAN_POINT('Ctrl Pts',(10.3035358409999,15.2,4.28691714999999));
#198173=CARTESIAN_POINT('Ctrl Pts',(10.3035358409999,11.6,4.28691714999999));
#198174=CARTESIAN_POINT('Ctrl Pts',(10.3001995279999,15.2,4.28688983399999));
#198175=CARTESIAN_POINT('Ctrl Pts',(10.3001995279999,11.6,4.28688983399999));
#198176=CARTESIAN_POINT('Ctrl Pts',(10.2968681929999,15.2,4.28685991399998));
#198177=CARTESIAN_POINT('Ctrl Pts',(10.2968681929999,11.6,4.28685991399998));
#198178=CARTESIAN_POINT('Ctrl Pts',(10.2935418419999,15.2,4.28682739499998));
#198179=CARTESIAN_POINT('Ctrl Pts',(10.2935418419999,11.6,4.28682739499998));
#198180=CARTESIAN_POINT('Ctrl Pts',(10.2902204869999,15.2,4.28679228399999));
#198181=CARTESIAN_POINT('Ctrl Pts',(10.2902204869999,11.6,4.28679228399999));
#198182=CARTESIAN_POINT('Ctrl Pts',(10.2869041329999,15.2,4.28675458899999));
#198183=CARTESIAN_POINT('Ctrl Pts',(10.2869041329999,11.6,4.28675458899998));
#198184=CARTESIAN_POINT('Ctrl Pts',(10.2835927899999,15.2,4.28671431599999));
#198185=CARTESIAN_POINT('Ctrl Pts',(10.2835927899999,11.6,4.28671431599999));
#198186=CARTESIAN_POINT('Ctrl Pts',(10.2802864669999,15.2,4.28667147199998));
#198187=CARTESIAN_POINT('Ctrl Pts',(10.2802864669999,11.6,4.28667147199998));
#198188=CARTESIAN_POINT('Ctrl Pts',(10.2769851699999,15.2,4.28662606299999));
#198189=CARTESIAN_POINT('Ctrl Pts',(10.2769851699999,11.6,4.28662606299999));
#198190=CARTESIAN_POINT('Ctrl Pts',(10.2736889099999,15.2,4.28657809699998));
#198191=CARTESIAN_POINT('Ctrl Pts',(10.2736889099999,11.6,4.28657809699998));
#198192=CARTESIAN_POINT('Ctrl Pts',(10.2703976929999,15.2,4.28652758099999));
#198193=CARTESIAN_POINT('Ctrl Pts',(10.2703976929999,11.6,4.28652758099999));
#198194=CARTESIAN_POINT('Ctrl Pts',(10.2671115289999,15.2,4.28647451899998));
#198195=CARTESIAN_POINT('Ctrl Pts',(10.2671115289999,11.6,4.28647451899998));
#198196=CARTESIAN_POINT('Ctrl Pts',(10.2638304259999,15.2,4.28641892199998));
#198197=CARTESIAN_POINT('Ctrl Pts',(10.2638304259999,11.6,4.28641892199998));
#198198=CARTESIAN_POINT('Ctrl Pts',(10.2605543909999,15.2,4.28636079499999));
#198199=CARTESIAN_POINT('Ctrl Pts',(10.2605543909999,11.6,4.28636079499999));
#198200=CARTESIAN_POINT('Ctrl Pts',(10.2572834349999,15.2,4.28630014399998));
#198201=CARTESIAN_POINT('Ctrl Pts',(10.2572834349999,11.6,4.28630014399998));
#198202=CARTESIAN_POINT('Ctrl Pts',(10.2540175649999,15.2,4.28623697799999));
#198203=CARTESIAN_POINT('Ctrl Pts',(10.2540175649999,11.6,4.28623697799999));
#198204=CARTESIAN_POINT('Ctrl Pts',(10.2507567889999,15.2,4.28617130199999));
#198205=CARTESIAN_POINT('Ctrl Pts',(10.2507567889999,11.6,4.28617130199999));
#198206=CARTESIAN_POINT('Ctrl Pts',(10.2475011169999,15.2,4.28610312399999));
#198207=CARTESIAN_POINT('Ctrl Pts',(10.2475011169999,11.6,4.28610312399999));
#198208=CARTESIAN_POINT('Ctrl Pts',(10.2442505549999,15.2,4.28603244999999));
#198209=CARTESIAN_POINT('Ctrl Pts',(10.2442505549999,11.6,4.28603244999999));
#198210=CARTESIAN_POINT('Ctrl Pts',(10.2410051139999,15.2,4.28595928999999));
#198211=CARTESIAN_POINT('Ctrl Pts',(10.2410051139999,11.6,4.28595928999999));
#198212=CARTESIAN_POINT('Ctrl Pts',(10.2377648009999,15.2,4.28588364599998));
#198213=CARTESIAN_POINT('Ctrl Pts',(10.2377648009999,11.6,4.28588364599998));
#198214=CARTESIAN_POINT('Ctrl Pts',(10.2345296249999,15.2,4.28580552999998));
#198215=CARTESIAN_POINT('Ctrl Pts',(10.2345296249999,11.6,4.28580552999998));
#198216=CARTESIAN_POINT('Ctrl Pts',(10.2312995949999,15.2,4.28572494799998));
#198217=CARTESIAN_POINT('Ctrl Pts',(10.2312995949999,11.6,4.28572494799998));
#198218=CARTESIAN_POINT('Ctrl Pts',(10.2280747169999,15.2,4.28564190499999));
#198219=CARTESIAN_POINT('Ctrl Pts',(10.2280747169999,11.6,4.28564190499999));
#198220=CARTESIAN_POINT('Ctrl Pts',(10.2248550039999,15.2,4.28555640899998));
#198221=CARTESIAN_POINT('Ctrl Pts',(10.2248550039999,11.6,4.28555640899998));
#198222=CARTESIAN_POINT('Ctrl Pts',(10.2216404599999,15.2,4.28546846799998));
#198223=CARTESIAN_POINT('Ctrl Pts',(10.2216404599999,11.6,4.28546846799998));
#198224=CARTESIAN_POINT('Ctrl Pts',(10.2184310959999,15.2,4.28537808899998));
#198225=CARTESIAN_POINT('Ctrl Pts',(10.2184310959999,11.6,4.28537808899998));
#198226=CARTESIAN_POINT('Ctrl Pts',(10.2152269199999,15.2,4.28528527899999));
#198227=CARTESIAN_POINT('Ctrl Pts',(10.2152269199999,11.6,4.28528527899999));
#198228=CARTESIAN_POINT('Ctrl Pts',(10.2120279409999,15.2,4.28519004499999));
#198229=CARTESIAN_POINT('Ctrl Pts',(10.2120279409999,11.6,4.28519004499999));
#198230=CARTESIAN_POINT('Ctrl Pts',(10.2088341669999,15.2,4.28509239499999));
#198231=CARTESIAN_POINT('Ctrl Pts',(10.2088341669999,11.6,4.28509239499998));
#198232=CARTESIAN_POINT('Ctrl Pts',(10.2056456079999,15.2,4.28499233499998));
#198233=CARTESIAN_POINT('Ctrl Pts',(10.2056456079999,11.6,4.28499233499998));
#198234=CARTESIAN_POINT('Ctrl Pts',(10.2024622709999,15.2,4.28488987299998));
#198235=CARTESIAN_POINT('Ctrl Pts',(10.2024622709999,11.6,4.28488987299998));
#198236=CARTESIAN_POINT('Ctrl Pts',(10.1992841639999,15.2,4.28478501599999));
#198237=CARTESIAN_POINT('Ctrl Pts',(10.1992841639999,11.6,4.28478501599999));
#198238=CARTESIAN_POINT('Ctrl Pts',(10.1961112979999,15.2,4.28467777199998));
#198239=CARTESIAN_POINT('Ctrl Pts',(10.1961112979999,11.6,4.28467777199998));
#198240=CARTESIAN_POINT('Ctrl Pts',(10.1929436789999,15.2,4.28456814899998));
#198241=CARTESIAN_POINT('Ctrl Pts',(10.1929436789999,11.6,4.28456814899998));
#198242=CARTESIAN_POINT('Ctrl Pts',(10.1897813189999,15.2,4.28445615199998));
#198243=CARTESIAN_POINT('Ctrl Pts',(10.1897813189999,11.6,4.28445615199998));
#198244=CARTESIAN_POINT('Ctrl Pts',(10.1866242239999,15.2,4.28434178999999));
#198245=CARTESIAN_POINT('Ctrl Pts',(10.1866242239999,11.6,4.28434178999998));
#198246=CARTESIAN_POINT('Ctrl Pts',(10.1834724029999,15.2,4.28422507099998));
#198247=CARTESIAN_POINT('Ctrl Pts',(10.1834724029999,11.6,4.28422507099998));
#198248=CARTESIAN_POINT('Ctrl Pts',(10.1803258649999,15.2,4.28410600199999));
#198249=CARTESIAN_POINT('Ctrl Pts',(10.1803258649999,11.6,4.28410600199999));
#198250=CARTESIAN_POINT('Ctrl Pts',(10.1771846189999,15.2,4.28398458999999));
#198251=CARTESIAN_POINT('Ctrl Pts',(10.1771846189999,11.6,4.28398458999998));
#198252=CARTESIAN_POINT('Ctrl Pts',(10.1740486739999,15.2,4.28386084199998));
#198253=CARTESIAN_POINT('Ctrl Pts',(10.1740486739999,11.6,4.28386084199998));
#198254=CARTESIAN_POINT('Ctrl Pts',(10.1709180389999,15.2,4.28373476599998));
#198255=CARTESIAN_POINT('Ctrl Pts',(10.1709180389999,11.6,4.28373476599998));
#198256=CARTESIAN_POINT('Ctrl Pts',(10.1677927209999,15.2,4.28360636999999));
#198257=CARTESIAN_POINT('Ctrl Pts',(10.1677927209999,11.6,4.28360636999999));
#198258=CARTESIAN_POINT('Ctrl Pts',(10.1646727299999,15.2,4.28347566199999));
#198259=CARTESIAN_POINT('Ctrl Pts',(10.1646727299999,11.6,4.28347566199999));
#198260=CARTESIAN_POINT('Ctrl Pts',(10.1615580749999,15.2,4.28334264799999));
#198261=CARTESIAN_POINT('Ctrl Pts',(10.1615580749999,11.6,4.28334264799999));
#198262=CARTESIAN_POINT('Ctrl Pts',(10.1584487639999,15.2,4.28320733699999));
#198263=CARTESIAN_POINT('Ctrl Pts',(10.1584487639999,11.6,4.28320733699999));
#198264=CARTESIAN_POINT('Ctrl Pts',(10.1553448059999,15.2,4.28306973499998));
#198265=CARTESIAN_POINT('Ctrl Pts',(10.1553448059999,11.6,4.28306973499998));
#198266=CARTESIAN_POINT('Ctrl Pts',(10.1522462099999,15.2,4.28292985199998));
#198267=CARTESIAN_POINT('Ctrl Pts',(10.1522462099999,11.6,4.28292985199998));
#198268=CARTESIAN_POINT('Ctrl Pts',(10.1491529859999,15.2,4.28278769499999));
#198269=CARTESIAN_POINT('Ctrl Pts',(10.1491529859999,11.6,4.28278769499998));
#198270=CARTESIAN_POINT('Ctrl Pts',(10.1460651409999,15.2,4.28264326999999));
#198271=CARTESIAN_POINT('Ctrl Pts',(10.1460651409999,11.6,4.28264326999999));
#198272=CARTESIAN_POINT('Ctrl Pts',(10.1429826849999,15.2,4.28249658699999));
#198273=CARTESIAN_POINT('Ctrl Pts',(10.1429826849999,11.6,4.28249658699999));
#198274=CARTESIAN_POINT('Ctrl Pts',(10.1399056249999,15.2,4.28234765099998));
#198275=CARTESIAN_POINT('Ctrl Pts',(10.1399056249999,11.6,4.28234765099998));
#198276=CARTESIAN_POINT('Ctrl Pts',(10.1368339729999,15.2,4.28219647199998));
#198277=CARTESIAN_POINT('Ctrl Pts',(10.1368339729999,11.6,4.28219647199998));
#198278=CARTESIAN_POINT('Ctrl Pts',(10.1337677349999,15.2,4.28204305799999));
#198279=CARTESIAN_POINT('Ctrl Pts',(10.1337677349999,11.6,4.28204305799999));
#198280=CARTESIAN_POINT('Ctrl Pts',(10.1307069219999,15.2,4.28188741599998));
#198281=CARTESIAN_POINT('Ctrl Pts',(10.1307069219999,11.6,4.28188741599998));
#198282=CARTESIAN_POINT('Ctrl Pts',(10.1276515429999,15.2,4.28172955299999));
#198283=CARTESIAN_POINT('Ctrl Pts',(10.1276515429999,11.6,4.28172955299999));
#198284=CARTESIAN_POINT('Ctrl Pts',(10.1246016049999,15.2,4.28156947899998));
#198285=CARTESIAN_POINT('Ctrl Pts',(10.1246016049999,11.6,4.28156947899998));
#198286=CARTESIAN_POINT('Ctrl Pts',(10.1215571169999,15.2,4.28140719999998));
#198287=CARTESIAN_POINT('Ctrl Pts',(10.1215571169999,11.6,4.28140719999998));
#198288=CARTESIAN_POINT('Ctrl Pts',(10.1185180899999,15.2,4.28124272399998));
#198289=CARTESIAN_POINT('Ctrl Pts',(10.1185180899999,11.6,4.28124272399998));
#198290=CARTESIAN_POINT('Ctrl Pts',(10.1154845319999,15.2,4.28107605999998));
#198291=CARTESIAN_POINT('Ctrl Pts',(10.1154845319999,11.6,4.28107605999998));
#198292=CARTESIAN_POINT('Ctrl Pts',(10.1124564509999,15.2,4.28090721599999));
#198293=CARTESIAN_POINT('Ctrl Pts',(10.1124564509999,11.6,4.28090721599998));
#198294=CARTESIAN_POINT('Ctrl Pts',(10.1094338579999,15.2,4.28073619999999));
#198295=CARTESIAN_POINT('Ctrl Pts',(10.1094338579999,11.6,4.28073619999999));
#198296=CARTESIAN_POINT('Ctrl Pts',(10.1064167609999,15.2,4.28056301899999));
#198297=CARTESIAN_POINT('Ctrl Pts',(10.1064167609999,11.6,4.28056301899998));
#198298=CARTESIAN_POINT('Ctrl Pts',(10.1034051679999,15.2,4.28038767999999));
#198299=CARTESIAN_POINT('Ctrl Pts',(10.1034051679999,11.6,4.28038767999999));
#198300=CARTESIAN_POINT('Ctrl Pts',(10.1003990899999,15.2,4.28021019499998));
#198301=CARTESIAN_POINT('Ctrl Pts',(10.1003990899999,11.6,4.28021019499998));
#198302=CARTESIAN_POINT('Ctrl Pts',(10.0973985339999,15.2,4.28003056799999));
#198303=CARTESIAN_POINT('Ctrl Pts',(10.0973985339999,11.6,4.28003056799999));
#198304=CARTESIAN_POINT('Ctrl Pts',(10.0944035109999,15.2,4.27984880999999));
#198305=CARTESIAN_POINT('Ctrl Pts',(10.0944035109999,11.6,4.27984880999999));
#198306=CARTESIAN_POINT('Ctrl Pts',(10.0914140299999,15.2,4.27966492799998));
#198307=CARTESIAN_POINT('Ctrl Pts',(10.0914140299999,11.6,4.27966492799998));
#198308=CARTESIAN_POINT('Ctrl Pts',(10.0884300979999,15.2,4.27947892899999));
#198309=CARTESIAN_POINT('Ctrl Pts',(10.0884300979999,11.6,4.27947892899999));
#198310=CARTESIAN_POINT('Ctrl Pts',(10.0854517259999,15.2,4.27929082399999));
#198311=CARTESIAN_POINT('Ctrl Pts',(10.0854517259999,11.6,4.27929082399999));
#198312=CARTESIAN_POINT('Ctrl Pts',(10.0824789229999,15.2,4.27910061799999));
#198313=CARTESIAN_POINT('Ctrl Pts',(10.0824789229999,11.6,4.27910061799999));
#198314=CARTESIAN_POINT('Ctrl Pts',(10.0795116959999,15.2,4.27890832199999));
#198315=CARTESIAN_POINT('Ctrl Pts',(10.0795116959999,11.6,4.27890832199999));
#198316=CARTESIAN_POINT('Ctrl Pts',(10.0765500579999,15.2,4.27871394299999));
#198317=CARTESIAN_POINT('Ctrl Pts',(10.0765500579999,11.6,4.27871394299998));
#198318=CARTESIAN_POINT('Ctrl Pts',(10.0735940149999,15.2,4.27851748899998));
#198319=CARTESIAN_POINT('Ctrl Pts',(10.0735940149999,11.6,4.27851748899998));
#198320=CARTESIAN_POINT('Ctrl Pts',(10.0706435779999,15.2,4.27831896899999));
#198321=CARTESIAN_POINT('Ctrl Pts',(10.0706435779999,11.6,4.27831896899998));
#198322=CARTESIAN_POINT('Ctrl Pts',(10.0676987549999,15.2,4.27811839099999));
#198323=CARTESIAN_POINT('Ctrl Pts',(10.0676987549999,11.6,4.27811839099998));
#198324=CARTESIAN_POINT('Ctrl Pts',(10.0647595569999,15.2,4.27791576399999));
#198325=CARTESIAN_POINT('Ctrl Pts',(10.0647595569999,11.6,4.27791576399999));
#198326=CARTESIAN_POINT('Ctrl Pts',(10.0618259909999,15.2,4.27771109499999));
#198327=CARTESIAN_POINT('Ctrl Pts',(10.0618259909999,11.6,4.27771109499999));
#198328=CARTESIAN_POINT('Ctrl Pts',(10.0588980669999,15.2,4.27750439399999));
#198329=CARTESIAN_POINT('Ctrl Pts',(10.0588980669999,11.6,4.27750439399999));
#198330=CARTESIAN_POINT('Ctrl Pts',(10.0559757949999,15.2,4.27729566799999));
#198331=CARTESIAN_POINT('Ctrl Pts',(10.0559757949999,11.6,4.27729566799999));
#198332=CARTESIAN_POINT('Ctrl Pts',(10.0530591839999,15.2,4.27708492699999));
#198333=CARTESIAN_POINT('Ctrl Pts',(10.0530591839999,11.6,4.27708492699998));
#198334=CARTESIAN_POINT('Ctrl Pts',(10.0501482429999,15.2,4.27687217799999));
#198335=CARTESIAN_POINT('Ctrl Pts',(10.0501482429999,11.6,4.27687217799999));
#198336=CARTESIAN_POINT('Ctrl Pts',(10.0472429809999,15.2,4.27665743099999));
#198337=CARTESIAN_POINT('Ctrl Pts',(10.0472429809999,11.6,4.27665743099999));
#198338=CARTESIAN_POINT('Ctrl Pts',(10.0443434079999,15.2,4.27644069399998));
#198339=CARTESIAN_POINT('Ctrl Pts',(10.0443434079999,11.6,4.27644069399998));
#198340=CARTESIAN_POINT('Ctrl Pts',(10.0414495329999,15.2,4.27622197499999));
#198341=CARTESIAN_POINT('Ctrl Pts',(10.0414495329999,11.6,4.27622197499998));
#198342=CARTESIAN_POINT('Ctrl Pts',(10.0385613659999,15.2,4.27600128499999));
#198343=CARTESIAN_POINT('Ctrl Pts',(10.0385613659999,11.6,4.27600128499999));
#198344=CARTESIAN_POINT('Ctrl Pts',(10.0356789149999,15.2,4.27577862799998));
#198345=CARTESIAN_POINT('Ctrl Pts',(10.0356789149999,11.6,4.27577862799998));
#198346=CARTESIAN_POINT('Ctrl Pts',(10.0328021909999,15.2,4.27555401699999));
#198347=CARTESIAN_POINT('Ctrl Pts',(10.0328021909999,11.6,4.27555401699998));
#198348=CARTESIAN_POINT('Ctrl Pts',(10.0299312019999,15.2,4.27532745799999));
#198349=CARTESIAN_POINT('Ctrl Pts',(10.0299312019999,11.6,4.27532745799999));
#198350=CARTESIAN_POINT('Ctrl Pts',(10.0270659569999,15.2,4.27509896199999));
#198351=CARTESIAN_POINT('Ctrl Pts',(10.0270659569999,11.6,4.27509896199999));
#198352=CARTESIAN_POINT('Ctrl Pts',(10.0242064689999,15.2,4.27486853499998));
#198353=CARTESIAN_POINT('Ctrl Pts',(10.0242064689999,11.6,4.27486853499998));
#198354=CARTESIAN_POINT('Ctrl Pts',(10.0213527429999,15.2,4.27463618899999));
#198355=CARTESIAN_POINT('Ctrl Pts',(10.0213527429999,11.6,4.27463618899999));
#198356=CARTESIAN_POINT('Ctrl Pts',(10.0185047909999,15.2,4.27440193099999));
#198357=CARTESIAN_POINT('Ctrl Pts',(10.0185047909999,11.6,4.27440193099999));
#198358=CARTESIAN_POINT('Ctrl Pts',(10.0156626229999,15.2,4.27416576999998));
#198359=CARTESIAN_POINT('Ctrl Pts',(10.0156626229999,11.6,4.27416576999998));
#198360=CARTESIAN_POINT('Ctrl Pts',(10.0128262459999,15.2,4.27392771499999));
#198361=CARTESIAN_POINT('Ctrl Pts',(10.0128262459999,11.6,4.27392771499999));
#198362=CARTESIAN_POINT('Ctrl Pts',(10.0099956719999,15.2,4.27368777399998));
#198363=CARTESIAN_POINT('Ctrl Pts',(10.0099956719999,11.6,4.27368777399998));
#198364=CARTESIAN_POINT('Ctrl Pts',(10.0071709079999,15.2,4.27344595699999));
#198365=CARTESIAN_POINT('Ctrl Pts',(10.0071709079999,11.6,4.27344595699999));
#198366=CARTESIAN_POINT('Ctrl Pts',(10.0043519659999,15.2,4.27320227299998));
#198367=CARTESIAN_POINT('Ctrl Pts',(10.0043519659999,11.6,4.27320227299998));
#198368=CARTESIAN_POINT('Ctrl Pts',(10.0015388549999,15.2,4.27295673099999));
#198369=CARTESIAN_POINT('Ctrl Pts',(10.0015388549999,11.6,4.27295673099999));
#198370=CARTESIAN_POINT('Ctrl Pts',(9.99873158399994,15.2,4.27270933899998));
#198371=CARTESIAN_POINT('Ctrl Pts',(9.99873158399994,11.6,4.27270933899998));
#198372=CARTESIAN_POINT('Ctrl Pts',(9.99593016199994,15.2,4.27246010699999));
#198373=CARTESIAN_POINT('Ctrl Pts',(9.99593016199994,11.6,4.27246010699999));
#198374=CARTESIAN_POINT('Ctrl Pts',(9.99313459899994,15.2,4.27220904299999));
#198375=CARTESIAN_POINT('Ctrl Pts',(9.99313459899994,11.6,4.27220904299999));
#198376=CARTESIAN_POINT('Ctrl Pts',(9.99034490599995,15.2,4.27195615799998));
#198377=CARTESIAN_POINT('Ctrl Pts',(9.99034490599995,11.6,4.27195615799998));
#198378=CARTESIAN_POINT('Ctrl Pts',(9.98756109199994,15.2,4.27170146099999));
#198379=CARTESIAN_POINT('Ctrl Pts',(9.98756109199994,11.6,4.27170146099999));
#198380=CARTESIAN_POINT('Ctrl Pts',(9.98478316599994,15.2,4.27144495899999));
#198381=CARTESIAN_POINT('Ctrl Pts',(9.98478316599994,11.6,4.27144495899998));
#198382=CARTESIAN_POINT('Ctrl Pts',(9.98201113799994,15.2,4.27118666199998));
#198383=CARTESIAN_POINT('Ctrl Pts',(9.98201113799994,11.6,4.27118666199998));
#198384=CARTESIAN_POINT('Ctrl Pts',(9.97924501799995,15.2,4.27092657899999));
#198385=CARTESIAN_POINT('Ctrl Pts',(9.97924501799995,11.6,4.27092657899998));
#198386=CARTESIAN_POINT('Ctrl Pts',(9.97648481499994,15.2,4.27066472199999));
#198387=CARTESIAN_POINT('Ctrl Pts',(9.97648481499994,11.6,4.27066472199999));
#198388=CARTESIAN_POINT('Ctrl Pts',(9.97373053899994,15.2,4.27040109699998));
#198389=CARTESIAN_POINT('Ctrl Pts',(9.97373053899994,11.6,4.27040109699998));
#198390=CARTESIAN_POINT('Ctrl Pts',(9.97098220099994,15.2,4.27013571499998));
#198391=CARTESIAN_POINT('Ctrl Pts',(9.97098220099994,11.6,4.27013571499998));
#198392=CARTESIAN_POINT('Ctrl Pts',(9.96823980799994,15.2,4.26986858399999));
#198393=CARTESIAN_POINT('Ctrl Pts',(9.96823980799994,11.6,4.26986858399999));
#198394=CARTESIAN_POINT('Ctrl Pts',(9.96550337299994,15.2,4.26959971399998));
#198395=CARTESIAN_POINT('Ctrl Pts',(9.96550337299994,11.6,4.26959971399998));
#198396=CARTESIAN_POINT('Ctrl Pts',(9.96277290299994,15.2,4.26932911599998));
#198397=CARTESIAN_POINT('Ctrl Pts',(9.96277290299994,11.6,4.26932911599998));
#198398=CARTESIAN_POINT('Ctrl Pts',(9.96004841099994,15.2,4.26905679799999));
#198399=CARTESIAN_POINT('Ctrl Pts',(9.96004841099994,11.6,4.26905679799999));
#198400=CARTESIAN_POINT('Ctrl Pts',(9.95732990299994,15.2,4.26878276699998));
#198401=CARTESIAN_POINT('Ctrl Pts',(9.95732990299994,11.6,4.26878276699998));
#198402=CARTESIAN_POINT('Ctrl Pts',(9.95461739199994,15.2,4.26850703699999));
#198403=CARTESIAN_POINT('Ctrl Pts',(9.95461739199994,11.6,4.26850703699999));
#198404=CARTESIAN_POINT('Ctrl Pts',(9.95191088699995,15.2,4.26822961499998));
#198405=CARTESIAN_POINT('Ctrl Pts',(9.95191088699995,11.6,4.26822961499998));
#198406=CARTESIAN_POINT('Ctrl Pts',(9.94921039699994,15.2,4.26795051099998));
#198407=CARTESIAN_POINT('Ctrl Pts',(9.94921039699994,11.6,4.26795051099998));
#198408=CARTESIAN_POINT('Ctrl Pts',(9.94651593299994,15.2,4.26766973499999));
#198409=CARTESIAN_POINT('Ctrl Pts',(9.94651593299994,11.6,4.26766973499999));
#198410=CARTESIAN_POINT('Ctrl Pts',(9.94382750299994,15.2,4.26738729599998));
#198411=CARTESIAN_POINT('Ctrl Pts',(9.94382750299994,11.6,4.26738729599998));
#198412=CARTESIAN_POINT('Ctrl Pts',(9.94114511999994,15.2,4.26710320399999));
#198413=CARTESIAN_POINT('Ctrl Pts',(9.94114511999994,11.6,4.26710320399999));
#198414=CARTESIAN_POINT('Ctrl Pts',(9.93846879199995,15.2,4.26681746899998));
#198415=CARTESIAN_POINT('Ctrl Pts',(9.93846879199995,11.6,4.26681746899998));
#198416=CARTESIAN_POINT('Ctrl Pts',(9.93579852899994,15.2,4.26653009999999));
#198417=CARTESIAN_POINT('Ctrl Pts',(9.93579852899994,11.6,4.26653009999998));
#198418=CARTESIAN_POINT('Ctrl Pts',(9.93313434199995,15.2,4.26624110699999));
#198419=CARTESIAN_POINT('Ctrl Pts',(9.93313434199995,11.6,4.26624110699999));
#198420=CARTESIAN_POINT('Ctrl Pts',(9.93047623999994,15.2,4.26595049999998));
#198421=CARTESIAN_POINT('Ctrl Pts',(9.93047623999994,11.6,4.26595049999998));
#198422=CARTESIAN_POINT('Ctrl Pts',(9.92782423299994,15.2,4.26565828799998));
#198423=CARTESIAN_POINT('Ctrl Pts',(9.92782423299994,11.6,4.26565828799998));
#198424=CARTESIAN_POINT('Ctrl Pts',(9.92517833199994,15.2,4.26536448199998));
#198425=CARTESIAN_POINT('Ctrl Pts',(9.92517833199994,11.6,4.26536448199998));
#198426=CARTESIAN_POINT('Ctrl Pts',(9.92253854699995,15.2,4.26506909199999));
#198427=CARTESIAN_POINT('Ctrl Pts',(9.92253854699995,11.6,4.26506909199999));
#198428=CARTESIAN_POINT('Ctrl Pts',(9.91990488599994,15.2,4.26477212699999));
#198429=CARTESIAN_POINT('Ctrl Pts',(9.91990488599994,11.6,4.26477212699999));
#198430=CARTESIAN_POINT('Ctrl Pts',(9.91727736199995,15.2,4.26447359699999));
#198431=CARTESIAN_POINT('Ctrl Pts',(9.91727736199995,11.6,4.26447359699999));
#198432=CARTESIAN_POINT('Ctrl Pts',(9.91465598399994,15.2,4.26417351199999));
#198433=CARTESIAN_POINT('Ctrl Pts',(9.91465598399994,11.6,4.26417351199999));
#198434=CARTESIAN_POINT('Ctrl Pts',(9.91204076099995,15.2,4.26387188299999));
#198435=CARTESIAN_POINT('Ctrl Pts',(9.91204076099995,11.6,4.26387188299999));
#198436=CARTESIAN_POINT('Ctrl Pts',(9.90943170599994,15.2,4.26356871799998));
#198437=CARTESIAN_POINT('Ctrl Pts',(9.90943170599994,11.6,4.26356871799998));
#198438=CARTESIAN_POINT('Ctrl Pts',(9.90682882599994,15.2,4.26326402999998));
#198439=CARTESIAN_POINT('Ctrl Pts',(9.90682882599994,11.6,4.26326402999998));
#198440=CARTESIAN_POINT('Ctrl Pts',(9.90423213299995,15.2,4.26295782599999));
#198441=CARTESIAN_POINT('Ctrl Pts',(9.90423213299995,11.6,4.26295782599999));
#198442=CARTESIAN_POINT('Ctrl Pts',(9.90164163699994,15.2,4.26265011899999));
#198443=CARTESIAN_POINT('Ctrl Pts',(9.90164163699994,11.6,4.26265011899999));
#198444=CARTESIAN_POINT('Ctrl Pts',(9.89905734899994,15.2,4.26234091699998));
#198445=CARTESIAN_POINT('Ctrl Pts',(9.89905734899994,11.6,4.26234091699998));
#198446=CARTESIAN_POINT('Ctrl Pts',(9.89647927699994,15.2,4.26203023099998));
#198447=CARTESIAN_POINT('Ctrl Pts',(9.89647927699994,11.6,4.26203023099998));
#198448=CARTESIAN_POINT('Ctrl Pts',(9.89390743399994,15.2,4.26171807099998));
#198449=CARTESIAN_POINT('Ctrl Pts',(9.89390743399994,11.6,4.26171807099998));
#198450=CARTESIAN_POINT('Ctrl Pts',(9.89134182899994,15.2,4.26140444699998));
#198451=CARTESIAN_POINT('Ctrl Pts',(9.89134182899994,11.6,4.26140444699998));
#198452=CARTESIAN_POINT('Ctrl Pts',(9.88878247099995,15.2,4.26108937099999));
#198453=CARTESIAN_POINT('Ctrl Pts',(9.88878247099995,11.6,4.26108937099999));
#198454=CARTESIAN_POINT('Ctrl Pts',(9.88622937299995,15.2,4.26077285299999));
#198455=CARTESIAN_POINT('Ctrl Pts',(9.88622937299995,11.6,4.26077285299998));
#198456=CARTESIAN_POINT('Ctrl Pts',(9.88368254299995,15.2,4.26045490099998));
#198457=CARTESIAN_POINT('Ctrl Pts',(9.88368254299995,11.6,4.26045490099998));
#198458=CARTESIAN_POINT('Ctrl Pts',(9.88114199299994,15.2,4.26013552799999));
#198459=CARTESIAN_POINT('Ctrl Pts',(9.88114199299994,11.6,4.26013552799999));
#198460=CARTESIAN_POINT('Ctrl Pts',(9.87860773299994,15.2,4.25981474199999));
#198461=CARTESIAN_POINT('Ctrl Pts',(9.87860773299994,11.6,4.25981474199998));
#198462=CARTESIAN_POINT('Ctrl Pts',(9.87607977299995,15.2,4.25949255699998));
#198463=CARTESIAN_POINT('Ctrl Pts',(9.87607977299995,11.6,4.25949255699998));
#198464=CARTESIAN_POINT('Ctrl Pts',(9.87355812499995,15.2,4.25916897999999));
#198465=CARTESIAN_POINT('Ctrl Pts',(9.87355812499995,11.6,4.25916897999999));
#198466=CARTESIAN_POINT('Ctrl Pts',(9.87104279699994,15.2,4.25884402399999));
#198467=CARTESIAN_POINT('Ctrl Pts',(9.87104279699994,11.6,4.25884402399998));
#198468=CARTESIAN_POINT('Ctrl Pts',(9.86853379999994,15.2,4.25851769899998));
#198469=CARTESIAN_POINT('Ctrl Pts',(9.86853379999994,11.6,4.25851769899998));
#198470=CARTESIAN_POINT('Ctrl Pts',(9.86603114699994,15.2,4.25819001399999));
#198471=CARTESIAN_POINT('Ctrl Pts',(9.86603114699994,11.6,4.25819001399999));
#198472=CARTESIAN_POINT('Ctrl Pts',(9.86353484599995,15.2,4.25786098199998));
#198473=CARTESIAN_POINT('Ctrl Pts',(9.86353484599995,11.6,4.25786098199998));
#198474=CARTESIAN_POINT('Ctrl Pts',(9.86104490799995,15.2,4.25753061299999));
#198475=CARTESIAN_POINT('Ctrl Pts',(9.86104490799995,11.6,4.25753061299999));
#198476=CARTESIAN_POINT('Ctrl Pts',(9.85856134499994,15.2,4.25719891699998));
#198477=CARTESIAN_POINT('Ctrl Pts',(9.85856134499994,11.6,4.25719891699998));
#198478=CARTESIAN_POINT('Ctrl Pts',(9.85608416599994,15.2,4.25686590499998));
#198479=CARTESIAN_POINT('Ctrl Pts',(9.85608416599994,11.6,4.25686590499998));
#198480=CARTESIAN_POINT('Ctrl Pts',(9.85361338199995,15.2,4.25653158799999));
#198481=CARTESIAN_POINT('Ctrl Pts',(9.85361338199995,11.6,4.25653158799999));
#198482=CARTESIAN_POINT('Ctrl Pts',(9.85114900399994,15.2,4.25619597799999));
#198483=CARTESIAN_POINT('Ctrl Pts',(9.85114900399994,11.6,4.25619597799999));
#198484=CARTESIAN_POINT('Ctrl Pts',(9.84869104299994,15.2,4.25585908399999));
#198485=CARTESIAN_POINT('Ctrl Pts',(9.84869104299994,11.6,4.25585908399999));
#198486=CARTESIAN_POINT('Ctrl Pts',(9.84623950799994,15.2,4.25552091799998));
#198487=CARTESIAN_POINT('Ctrl Pts',(9.84623950799994,11.6,4.25552091799998));
#198488=CARTESIAN_POINT('Ctrl Pts',(9.84379441199994,15.2,4.25518149099998));
#198489=CARTESIAN_POINT('Ctrl Pts',(9.84379441199994,11.6,4.25518149099998));
#198490=CARTESIAN_POINT('Ctrl Pts',(9.84135576399994,15.2,4.25484081399999));
#198491=CARTESIAN_POINT('Ctrl Pts',(9.84135576399994,11.6,4.25484081399999));
#198492=CARTESIAN_POINT('Ctrl Pts',(9.83892357499995,15.2,4.25449889699999));
#198493=CARTESIAN_POINT('Ctrl Pts',(9.83892357499995,11.6,4.25449889699998));
#198494=CARTESIAN_POINT('Ctrl Pts',(9.83649785699994,15.2,4.25415575299999));
#198495=CARTESIAN_POINT('Ctrl Pts',(9.83649785699994,11.6,4.25415575299999));
#198496=CARTESIAN_POINT('Ctrl Pts',(9.83407861999994,15.2,4.25381139099999));
#198497=CARTESIAN_POINT('Ctrl Pts',(9.83407861999994,11.6,4.25381139099999));
#198498=CARTESIAN_POINT('Ctrl Pts',(9.83166587499994,15.2,4.25346582299999));
#198499=CARTESIAN_POINT('Ctrl Pts',(9.83166587499994,11.6,4.25346582299999));
#198500=CARTESIAN_POINT('Ctrl Pts',(9.82925963199994,15.2,4.25311906199998));
#198501=CARTESIAN_POINT('Ctrl Pts',(9.82925963199994,11.6,4.25311906199998));
#198502=CARTESIAN_POINT('Ctrl Pts',(9.82685990299995,15.2,4.25277111699998));
#198503=CARTESIAN_POINT('Ctrl Pts',(9.82685990299995,11.6,4.25277111699998));
#198504=CARTESIAN_POINT('Ctrl Pts',(9.82446669799995,15.2,4.25242199999998));
#198505=CARTESIAN_POINT('Ctrl Pts',(9.82446669799995,11.6,4.25242199999998));
#198506=CARTESIAN_POINT('Ctrl Pts',(9.82208002799995,15.2,4.25207172099999));
#198507=CARTESIAN_POINT('Ctrl Pts',(9.82208002799995,11.6,4.25207172099998));
#198508=CARTESIAN_POINT('Ctrl Pts',(9.81969990499995,15.2,4.25172029499999));
#198509=CARTESIAN_POINT('Ctrl Pts',(9.81969990499995,11.6,4.25172029499999));
#198510=CARTESIAN_POINT('Ctrl Pts',(9.81732633899994,15.2,4.25136772899998));
#198511=CARTESIAN_POINT('Ctrl Pts',(9.81732633899994,11.6,4.25136772899998));
#198512=CARTESIAN_POINT('Ctrl Pts',(9.81495934099994,15.2,4.25101403799999));
#198513=CARTESIAN_POINT('Ctrl Pts',(9.81495934099994,11.6,4.25101403799999));
#198514=CARTESIAN_POINT('Ctrl Pts',(9.81259892299994,15.2,4.25065923199998));
#198515=CARTESIAN_POINT('Ctrl Pts',(9.81259892299994,11.6,4.25065923199998));
#198516=CARTESIAN_POINT('Ctrl Pts',(9.81024509399995,15.2,4.25030332099999));
#198517=CARTESIAN_POINT('Ctrl Pts',(9.81024509399995,11.6,4.25030332099999));
#198518=CARTESIAN_POINT('Ctrl Pts',(9.80789786799994,15.2,4.24994631899998));
#198519=CARTESIAN_POINT('Ctrl Pts',(9.80789786799994,11.6,4.24994631899998));
#198520=CARTESIAN_POINT('Ctrl Pts',(9.80555725299994,15.2,4.24958823699999));
#198521=CARTESIAN_POINT('Ctrl Pts',(9.80555725299994,11.6,4.24958823699999));
#198522=CARTESIAN_POINT('Ctrl Pts',(9.80322326199994,15.2,4.24922908599999));
#198523=CARTESIAN_POINT('Ctrl Pts',(9.80322326199994,11.6,4.24922908599999));
#198524=CARTESIAN_POINT('Ctrl Pts',(9.80089590499994,15.2,4.24886887799998));
#198525=CARTESIAN_POINT('Ctrl Pts',(9.80089590499994,11.6,4.24886887799998));
#198526=CARTESIAN_POINT('Ctrl Pts',(9.79857519499994,15.2,4.24850762499998));
#198527=CARTESIAN_POINT('Ctrl Pts',(9.79857519499994,11.6,4.24850762499998));
#198528=CARTESIAN_POINT('Ctrl Pts',(9.79626114099995,15.2,4.24814533899998));
#198529=CARTESIAN_POINT('Ctrl Pts',(9.79626114099995,11.6,4.24814533899998));
#198530=CARTESIAN_POINT('Ctrl Pts',(9.79395375499994,15.2,4.24778202999998));
#198531=CARTESIAN_POINT('Ctrl Pts',(9.79395375499994,11.6,4.24778202999998));
#198532=CARTESIAN_POINT('Ctrl Pts',(9.79165304999994,15.2,4.24741771299999));
#198533=CARTESIAN_POINT('Ctrl Pts',(9.79165304999994,11.6,4.24741771299998));
#198534=CARTESIAN_POINT('Ctrl Pts',(9.78935903399995,15.2,4.24705239699998));
#198535=CARTESIAN_POINT('Ctrl Pts',(9.78935903399995,11.6,4.24705239699998));
#198536=CARTESIAN_POINT('Ctrl Pts',(9.78707171999995,15.2,4.24668609599999));
#198537=CARTESIAN_POINT('Ctrl Pts',(9.78707171999995,11.6,4.24668609599998));
#198538=CARTESIAN_POINT('Ctrl Pts',(9.78479111999994,15.2,4.24631881999999));
#198539=CARTESIAN_POINT('Ctrl Pts',(9.78479111999994,11.6,4.24631881999998));
#198540=CARTESIAN_POINT('Ctrl Pts',(9.78251724499994,15.2,4.24595058299998));
#198541=CARTESIAN_POINT('Ctrl Pts',(9.78251724499994,11.6,4.24595058299998));
#198542=CARTESIAN_POINT('Ctrl Pts',(9.78025010499995,15.2,4.24558139499998));
#198543=CARTESIAN_POINT('Ctrl Pts',(9.78025010499995,11.6,4.24558139499998));
#198544=CARTESIAN_POINT('Ctrl Pts',(9.77798971299995,15.2,4.24521127099998));
#198545=CARTESIAN_POINT('Ctrl Pts',(9.77798971299995,11.6,4.24521127099998));
#198546=CARTESIAN_POINT('Ctrl Pts',(9.77573607899994,15.2,4.24484021999999));
#198547=CARTESIAN_POINT('Ctrl Pts',(9.77573607899994,11.6,4.24484021999999));
#198548=CARTESIAN_POINT('Ctrl Pts',(9.77348921599994,15.2,4.24446825699999));
#198549=CARTESIAN_POINT('Ctrl Pts',(9.77348921599994,11.6,4.24446825699999));
#198550=CARTESIAN_POINT('Ctrl Pts',(9.77124913399994,15.2,4.24409539199999));
#198551=CARTESIAN_POINT('Ctrl Pts',(9.77124913399994,11.6,4.24409539199999));
#198552=CARTESIAN_POINT('Ctrl Pts',(9.76901584499995,15.2,4.24372163899999));
#198553=CARTESIAN_POINT('Ctrl Pts',(9.76901584499995,11.6,4.24372163899999));
#198554=CARTESIAN_POINT('Ctrl Pts',(9.76678936099994,15.2,4.24334700899998));
#198555=CARTESIAN_POINT('Ctrl Pts',(9.76678936099994,11.6,4.24334700899998));
#198556=CARTESIAN_POINT('Ctrl Pts',(9.76456969299995,15.2,4.24297151599998));
#198557=CARTESIAN_POINT('Ctrl Pts',(9.76456969299995,11.6,4.24297151599998));
#198558=CARTESIAN_POINT('Ctrl Pts',(9.76235685299994,15.2,4.24259516999999));
#198559=CARTESIAN_POINT('Ctrl Pts',(9.76235685299994,11.6,4.24259516999999));
#198560=CARTESIAN_POINT('Ctrl Pts',(9.76015085199995,15.2,4.24221798599999));
#198561=CARTESIAN_POINT('Ctrl Pts',(9.76015085199995,11.6,4.24221798599999));
#198562=CARTESIAN_POINT('Ctrl Pts',(9.75795170099994,15.2,4.24183997499998));
#198563=CARTESIAN_POINT('Ctrl Pts',(9.75795170099994,11.6,4.24183997499998));
#198564=CARTESIAN_POINT('Ctrl Pts',(9.75575941399994,15.2,4.24146114999999));
#198565=CARTESIAN_POINT('Ctrl Pts',(9.75575941399994,11.6,4.24146114999999));
#198566=CARTESIAN_POINT('Ctrl Pts',(9.75357400199995,15.2,4.24108152299999));
#198567=CARTESIAN_POINT('Ctrl Pts',(9.75357400199995,11.6,4.24108152299999));
#198568=CARTESIAN_POINT('Ctrl Pts',(9.75139547399994,15.2,4.24070110799998));
#198569=CARTESIAN_POINT('Ctrl Pts',(9.75139547399994,11.6,4.24070110799998));
#198570=CARTESIAN_POINT('Ctrl Pts',(9.74922384499994,15.2,4.24031991699999));
#198571=CARTESIAN_POINT('Ctrl Pts',(9.74922384499994,11.6,4.24031991699999));
#198572=CARTESIAN_POINT('Ctrl Pts',(9.74705912399994,15.2,4.23993796299998));
#198573=CARTESIAN_POINT('Ctrl Pts',(9.74705912399994,11.6,4.23993796299998));
#198574=CARTESIAN_POINT('Ctrl Pts',(9.74490132599995,15.2,4.23955525799999));
#198575=CARTESIAN_POINT('Ctrl Pts',(9.74490132599995,11.6,4.23955525799998));
#198576=CARTESIAN_POINT('Ctrl Pts',(9.74275045999994,15.2,4.23917181499998));
#198577=CARTESIAN_POINT('Ctrl Pts',(9.74275045999994,11.6,4.23917181499998));
#198578=CARTESIAN_POINT('Ctrl Pts',(9.74060653799994,15.2,4.23878764799999));
#198579=CARTESIAN_POINT('Ctrl Pts',(9.74060653799994,11.6,4.23878764799999));
#198580=CARTESIAN_POINT('Ctrl Pts',(9.73846957399994,15.2,4.23840276899998));
#198581=CARTESIAN_POINT('Ctrl Pts',(9.73846957399994,11.6,4.23840276899998));
#198582=CARTESIAN_POINT('Ctrl Pts',(9.73633957899994,15.2,4.23801719199999));
#198583=CARTESIAN_POINT('Ctrl Pts',(9.73633957899994,11.6,4.23801719199999));
#198584=CARTESIAN_POINT('Ctrl Pts',(9.73421656399994,15.2,4.23763092799998));
#198585=CARTESIAN_POINT('Ctrl Pts',(9.73421656399994,11.6,4.23763092799998));
#198586=CARTESIAN_POINT('Ctrl Pts',(9.73210054099994,15.2,4.23724399299999));
#198587=CARTESIAN_POINT('Ctrl Pts',(9.73210054099994,11.6,4.23724399299999));
#198588=CARTESIAN_POINT('Ctrl Pts',(9.72999152299994,15.2,4.23685639699999));
#198589=CARTESIAN_POINT('Ctrl Pts',(9.72999152299994,11.6,4.23685639699999));
#198590=CARTESIAN_POINT('Ctrl Pts',(9.72788952199994,15.2,4.23646815499998));
#198591=CARTESIAN_POINT('Ctrl Pts',(9.72788952199994,11.6,4.23646815499998));
#198592=CARTESIAN_POINT('Ctrl Pts',(9.72579454899994,15.2,4.23607928199999));
#198593=CARTESIAN_POINT('Ctrl Pts',(9.72579454899994,11.6,4.23607928199999));
#198594=CARTESIAN_POINT('Ctrl Pts',(9.72370661699994,15.2,4.23568978799998));
#198595=CARTESIAN_POINT('Ctrl Pts',(9.72370661699994,11.6,4.23568978799998));
#198596=CARTESIAN_POINT('Ctrl Pts',(9.72162573699995,15.2,4.23529968699999));
#198597=CARTESIAN_POINT('Ctrl Pts',(9.72162573699995,11.6,4.23529968699999));
#198598=CARTESIAN_POINT('Ctrl Pts',(9.71955192299994,15.2,4.23490899299999));
#198599=CARTESIAN_POINT('Ctrl Pts',(9.71955192299994,11.6,4.23490899299999));
#198600=CARTESIAN_POINT('Ctrl Pts',(9.71748518499994,15.2,4.23451771999999));
#198601=CARTESIAN_POINT('Ctrl Pts',(9.71748518499994,11.6,4.23451771999999));
#198602=CARTESIAN_POINT('Ctrl Pts',(9.71542553799994,15.2,4.23412587999999));
#198603=CARTESIAN_POINT('Ctrl Pts',(9.71542553799994,11.6,4.23412587999999));
#198604=CARTESIAN_POINT('Ctrl Pts',(9.71337299099994,15.2,4.23373348899998));
#198605=CARTESIAN_POINT('Ctrl Pts',(9.71337299099994,11.6,4.23373348899998));
#198606=CARTESIAN_POINT('Ctrl Pts',(9.71132755699994,15.2,4.23334055899999));
#198607=CARTESIAN_POINT('Ctrl Pts',(9.71132755699994,11.6,4.23334055899998));
#198608=CARTESIAN_POINT('Ctrl Pts',(9.70928924999994,15.2,4.23294710199999));
#198609=CARTESIAN_POINT('Ctrl Pts',(9.70928924999994,11.6,4.23294710199999));
#198610=CARTESIAN_POINT('Ctrl Pts',(9.70725808099995,15.2,4.23255313599999));
#198611=CARTESIAN_POINT('Ctrl Pts',(9.70725808099995,11.6,4.23255313599998));
#198612=CARTESIAN_POINT('Ctrl Pts',(9.70523406399994,15.2,4.23215867099999));
#198613=CARTESIAN_POINT('Ctrl Pts',(9.70523406399994,11.6,4.23215867099999));
#198614=CARTESIAN_POINT('Ctrl Pts',(9.70321720799994,15.2,4.23176372099999));
#198615=CARTESIAN_POINT('Ctrl Pts',(9.70321720799994,11.6,4.23176372099998));
#198616=CARTESIAN_POINT('Ctrl Pts',(9.70120752899994,15.2,4.23136830299998));
#198617=CARTESIAN_POINT('Ctrl Pts',(9.70120752899994,11.6,4.23136830299998));
#198618=CARTESIAN_POINT('Ctrl Pts',(9.69920503699995,15.2,4.23097242699999));
#198619=CARTESIAN_POINT('Ctrl Pts',(9.69920503699995,11.6,4.23097242699999));
#198620=CARTESIAN_POINT('Ctrl Pts',(9.69720974699994,15.2,4.23057611099999));
#198621=CARTESIAN_POINT('Ctrl Pts',(9.69720974699994,11.6,4.23057611099999));
#198622=CARTESIAN_POINT('Ctrl Pts',(9.69522166799995,15.2,4.23017936499999));
#198623=CARTESIAN_POINT('Ctrl Pts',(9.69522166799995,11.6,4.23017936499999));
#198624=CARTESIAN_POINT('Ctrl Pts',(9.69324081599994,15.2,4.22978220499999));
#198625=CARTESIAN_POINT('Ctrl Pts',(9.69324081599994,11.6,4.22978220499999));
#198626=CARTESIAN_POINT('Ctrl Pts',(9.69126720099995,15.2,4.22938464599999));
#198627=CARTESIAN_POINT('Ctrl Pts',(9.69126720099995,11.6,4.22938464599999));
#198628=CARTESIAN_POINT('Ctrl Pts',(9.68930083599994,15.2,4.22898670099999));
#198629=CARTESIAN_POINT('Ctrl Pts',(9.68930083599994,11.6,4.22898670099999));
#198630=CARTESIAN_POINT('Ctrl Pts',(9.68734173699995,15.2,4.22858838399998));
#198631=CARTESIAN_POINT('Ctrl Pts',(9.68734173699995,11.6,4.22858838399998));
#198632=CARTESIAN_POINT('Ctrl Pts',(9.68538991099994,15.2,4.22818970999998));
#198633=CARTESIAN_POINT('Ctrl Pts',(9.68538991099994,11.6,4.22818970999998));
#198634=CARTESIAN_POINT('Ctrl Pts',(9.68344537499994,15.2,4.22779069299998));
#198635=CARTESIAN_POINT('Ctrl Pts',(9.68344537499994,11.6,4.22779069299998));
#198636=CARTESIAN_POINT('Ctrl Pts',(9.68150813999994,15.2,4.22739134799999));
#198637=CARTESIAN_POINT('Ctrl Pts',(9.68150813999994,11.6,4.22739134799999));
#198638=CARTESIAN_POINT('Ctrl Pts',(9.67957821999994,15.2,4.22699168799999));
#198639=CARTESIAN_POINT('Ctrl Pts',(9.67957821999994,11.6,4.22699168799998));
#198640=CARTESIAN_POINT('Ctrl Pts',(9.67765562599994,15.2,4.22659172999998));
#198641=CARTESIAN_POINT('Ctrl Pts',(9.67765562599994,11.6,4.22659172999998));
#198642=CARTESIAN_POINT('Ctrl Pts',(9.67574037299994,15.2,4.22619148699999));
#198643=CARTESIAN_POINT('Ctrl Pts',(9.67574037299994,11.6,4.22619148699999));
#198644=CARTESIAN_POINT('Ctrl Pts',(9.67383247099994,15.2,4.22579097199999));
#198645=CARTESIAN_POINT('Ctrl Pts',(9.67383247099994,11.6,4.22579097199998));
#198646=CARTESIAN_POINT('Ctrl Pts',(9.67193193599994,15.2,4.22539020399999));
#198647=CARTESIAN_POINT('Ctrl Pts',(9.67193193599994,11.6,4.22539020399998));
#198648=CARTESIAN_POINT('Ctrl Pts',(9.67003877899995,15.2,4.22498919399998));
#198649=CARTESIAN_POINT('Ctrl Pts',(9.67003877899995,11.6,4.22498919399998));
#198650=CARTESIAN_POINT('Ctrl Pts',(9.66815301399994,15.2,4.22458795799999));
#198651=CARTESIAN_POINT('Ctrl Pts',(9.66815301399994,11.6,4.22458795799999));
#198652=CARTESIAN_POINT('Ctrl Pts',(9.66627465299995,15.2,4.22418651099999));
#198653=CARTESIAN_POINT('Ctrl Pts',(9.66627465299995,11.6,4.22418651099999));
#198654=CARTESIAN_POINT('Ctrl Pts',(9.66440370999995,15.2,4.22378486799998));
#198655=CARTESIAN_POINT('Ctrl Pts',(9.66440370999995,11.6,4.22378486799998));
#198656=CARTESIAN_POINT('Ctrl Pts',(9.66254019799995,15.2,4.22338304499998));
#198657=CARTESIAN_POINT('Ctrl Pts',(9.66254019799995,11.6,4.22338304499998));
#198658=CARTESIAN_POINT('Ctrl Pts',(9.66068412999994,15.2,4.22298105399998));
#198659=CARTESIAN_POINT('Ctrl Pts',(9.66068412999994,11.6,4.22298105399998));
#198660=CARTESIAN_POINT('Ctrl Pts',(9.65883551799994,15.2,4.22257891399998));
#198661=CARTESIAN_POINT('Ctrl Pts',(9.65883551799994,11.6,4.22257891399998));
#198662=CARTESIAN_POINT('Ctrl Pts',(9.65699437699995,15.2,4.22217663699998));
#198663=CARTESIAN_POINT('Ctrl Pts',(9.65699437699995,11.6,4.22217663699998));
#198664=CARTESIAN_POINT('Ctrl Pts',(9.65516071899994,15.2,4.22177423999998));
#198665=CARTESIAN_POINT('Ctrl Pts',(9.65516071899994,11.6,4.22177423999998));
#198666=CARTESIAN_POINT('Ctrl Pts',(9.65333455799994,15.2,4.22137173699999));
#198667=CARTESIAN_POINT('Ctrl Pts',(9.65333455799994,11.6,4.22137173699999));
#198668=CARTESIAN_POINT('Ctrl Pts',(9.65151590799995,15.2,4.22096914499999));
#198669=CARTESIAN_POINT('Ctrl Pts',(9.65151590799995,11.6,4.22096914499999));
#198670=CARTESIAN_POINT('Ctrl Pts',(9.64970477999995,15.2,4.22056647799998));
#198671=CARTESIAN_POINT('Ctrl Pts',(9.64970477999995,11.6,4.22056647799998));
#198672=CARTESIAN_POINT('Ctrl Pts',(9.64790118899994,15.2,4.22016375299999));
#198673=CARTESIAN_POINT('Ctrl Pts',(9.64790118899994,11.6,4.22016375299999));
#198674=CARTESIAN_POINT('Ctrl Pts',(9.64610514899995,15.2,4.21976098399998));
#198675=CARTESIAN_POINT('Ctrl Pts',(9.64610514899995,11.6,4.21976098399998));
#198676=CARTESIAN_POINT('Ctrl Pts',(9.64431667199995,15.2,4.21935818699998));
#198677=CARTESIAN_POINT('Ctrl Pts',(9.64431667199995,11.6,4.21935818699998));
#198678=CARTESIAN_POINT('Ctrl Pts',(9.64253577199995,15.2,4.21895537799998));
#198679=CARTESIAN_POINT('Ctrl Pts',(9.64253577199995,11.6,4.21895537799998));
#198680=CARTESIAN_POINT('Ctrl Pts',(9.64076246299994,15.2,4.21855257399999));
#198681=CARTESIAN_POINT('Ctrl Pts',(9.64076246299994,11.6,4.21855257399999));
#198682=CARTESIAN_POINT('Ctrl Pts',(9.63899675899994,15.2,4.21814978799999));
#198683=CARTESIAN_POINT('Ctrl Pts',(9.63899675899994,11.6,4.21814978799999));
#198684=CARTESIAN_POINT('Ctrl Pts',(9.63723867199995,15.2,4.21774703799999));
#198685=CARTESIAN_POINT('Ctrl Pts',(9.63723867199995,11.6,4.21774703799999));
#198686=CARTESIAN_POINT('Ctrl Pts',(9.63548821799994,15.2,4.21734433899999));
#198687=CARTESIAN_POINT('Ctrl Pts',(9.63548821799994,11.6,4.21734433899999));
#198688=CARTESIAN_POINT('Ctrl Pts',(9.63374540699995,15.2,4.21694170799999));
#198689=CARTESIAN_POINT('Ctrl Pts',(9.63374540699995,11.6,4.21694170799999));
#198690=CARTESIAN_POINT('Ctrl Pts',(9.63201025599994,15.2,4.21653915999999));
#198691=CARTESIAN_POINT('Ctrl Pts',(9.63201025599994,11.6,4.21653915999998));
#198692=CARTESIAN_POINT('Ctrl Pts',(9.63028277899994,15.2,4.21613671099998));
#198693=CARTESIAN_POINT('Ctrl Pts',(9.63028277899994,11.6,4.21613671099998));
#198694=CARTESIAN_POINT('Ctrl Pts',(9.62856298699995,15.2,4.21573437799999));
#198695=CARTESIAN_POINT('Ctrl Pts',(9.62856298699995,11.6,4.21573437799999));
#198696=CARTESIAN_POINT('Ctrl Pts',(9.62685089699994,15.2,4.21533217699999));
#198697=CARTESIAN_POINT('Ctrl Pts',(9.62685089699994,11.6,4.21533217699999));
#198698=CARTESIAN_POINT('Ctrl Pts',(9.62514652099994,15.2,4.21493012499998));
#198699=CARTESIAN_POINT('Ctrl Pts',(9.62514652099994,11.6,4.21493012499998));
#198700=CARTESIAN_POINT('Ctrl Pts',(9.62344987299995,15.2,4.21452823799999));
#198701=CARTESIAN_POINT('Ctrl Pts',(9.62344987299995,11.6,4.21452823799999));
#198702=CARTESIAN_POINT('Ctrl Pts',(9.62176096699995,15.2,4.21412653099999));
#198703=CARTESIAN_POINT('Ctrl Pts',(9.62176096699995,11.6,4.21412653099999));
#198704=CARTESIAN_POINT('Ctrl Pts',(9.62007981799994,15.2,4.21372502199999));
#198705=CARTESIAN_POINT('Ctrl Pts',(9.62007981799994,11.6,4.21372502199999));
#198706=CARTESIAN_POINT('Ctrl Pts',(9.61840643899994,15.2,4.21332372799998));
#198707=CARTESIAN_POINT('Ctrl Pts',(9.61840643899994,11.6,4.21332372799998));
#198708=CARTESIAN_POINT('Ctrl Pts',(9.61674084499995,15.2,4.21292266499999));
#198709=CARTESIAN_POINT('Ctrl Pts',(9.61674084499995,11.6,4.21292266499999));
#198710=CARTESIAN_POINT('Ctrl Pts',(9.61508304999995,15.2,4.21252184999998));
#198711=CARTESIAN_POINT('Ctrl Pts',(9.61508304999995,11.6,4.21252184999998));
#198712=CARTESIAN_POINT('Ctrl Pts',(9.61343306699994,15.2,4.21212129899998));
#198713=CARTESIAN_POINT('Ctrl Pts',(9.61343306699994,11.6,4.21212129899998));
#198714=CARTESIAN_POINT('Ctrl Pts',(9.61179091199994,15.2,4.21172103099998));
#198715=CARTESIAN_POINT('Ctrl Pts',(9.61179091199994,11.6,4.21172103099998));
#198716=CARTESIAN_POINT('Ctrl Pts',(9.61015659699994,15.2,4.21132105999998));
#198717=CARTESIAN_POINT('Ctrl Pts',(9.61015659699994,11.6,4.21132105999998));
#198718=CARTESIAN_POINT('Ctrl Pts',(9.60853013999994,15.2,4.21092140599999));
#198719=CARTESIAN_POINT('Ctrl Pts',(9.60853013999994,11.6,4.21092140599998));
#198720=CARTESIAN_POINT('Ctrl Pts',(9.60691155199994,15.2,4.21052208399999));
#198721=CARTESIAN_POINT('Ctrl Pts',(9.60691155199994,11.6,4.21052208399998));
#198722=CARTESIAN_POINT('Ctrl Pts',(9.60530084799995,15.2,4.21012311199998));
#198723=CARTESIAN_POINT('Ctrl Pts',(9.60530084799995,11.6,4.21012311199998));
#198724=CARTESIAN_POINT('Ctrl Pts',(9.60369804399994,15.2,4.20972450799999));
#198725=CARTESIAN_POINT('Ctrl Pts',(9.60369804399994,11.6,4.20972450799999));
#198726=CARTESIAN_POINT('Ctrl Pts',(9.60210315399994,15.2,4.20932628799999));
#198727=CARTESIAN_POINT('Ctrl Pts',(9.60210315399994,11.6,4.20932628799999));
#198728=CARTESIAN_POINT('Ctrl Pts',(9.60051619099995,15.2,4.20892846999998));
#198729=CARTESIAN_POINT('Ctrl Pts',(9.60051619099995,11.6,4.20892846999998));
#198730=CARTESIAN_POINT('Ctrl Pts',(9.59893717199994,15.2,4.20853107199999));
#198731=CARTESIAN_POINT('Ctrl Pts',(9.59893717199994,11.6,4.20853107199999));
#198732=CARTESIAN_POINT('Ctrl Pts',(9.59736610999995,15.2,4.20813410999998));
#198733=CARTESIAN_POINT('Ctrl Pts',(9.59736610999995,11.6,4.20813410999998));
#198734=CARTESIAN_POINT('Ctrl Pts',(9.59580301899994,15.2,4.20773760399998));
#198735=CARTESIAN_POINT('Ctrl Pts',(9.59580301899994,11.6,4.20773760399998));
#198736=CARTESIAN_POINT('Ctrl Pts',(9.59424791599995,15.2,4.20734156899999));
#198737=CARTESIAN_POINT('Ctrl Pts',(9.59424791599995,11.6,4.20734156899999));
#198738=CARTESIAN_POINT('Ctrl Pts',(9.59270081499995,15.2,4.20694602499999));
#198739=CARTESIAN_POINT('Ctrl Pts',(9.59270081499995,11.6,4.20694602499999));
#198740=CARTESIAN_POINT('Ctrl Pts',(9.59116172899994,15.2,4.20655098899999));
#198741=CARTESIAN_POINT('Ctrl Pts',(9.59116172899994,11.6,4.20655098899999));
#198742=CARTESIAN_POINT('Ctrl Pts',(9.58963067599995,15.2,4.20615647899999));
#198743=CARTESIAN_POINT('Ctrl Pts',(9.58963067599995,11.6,4.20615647899999));
#198744=CARTESIAN_POINT('Ctrl Pts',(9.58810766899994,15.2,4.20576251499998));
#198745=CARTESIAN_POINT('Ctrl Pts',(9.58810766899994,11.6,4.20576251499998));
#198746=CARTESIAN_POINT('Ctrl Pts',(9.58659272199995,15.2,4.20536911099998));
#198747=CARTESIAN_POINT('Ctrl Pts',(9.58659272199995,11.6,4.20536911099998));
#198748=CARTESIAN_POINT('Ctrl Pts',(9.58508585299995,15.2,4.20497628799998));
#198749=CARTESIAN_POINT('Ctrl Pts',(9.58508585299995,11.6,4.20497628799998));
#198750=CARTESIAN_POINT('Ctrl Pts',(9.58358707499994,15.2,4.20458406399998));
#198751=CARTESIAN_POINT('Ctrl Pts',(9.58358707499994,11.6,4.20458406399998));
#198752=CARTESIAN_POINT('Ctrl Pts',(9.58209640399994,15.2,4.20419245699998));
#198753=CARTESIAN_POINT('Ctrl Pts',(9.58209640399994,11.6,4.20419245699998));
#198754=CARTESIAN_POINT('Ctrl Pts',(9.58061385399994,15.2,4.20380148499999));
#198755=CARTESIAN_POINT('Ctrl Pts',(9.58061385399994,11.6,4.20380148499999));
#198756=CARTESIAN_POINT('Ctrl Pts',(9.57913944099994,15.2,4.20341116699999));
#198757=CARTESIAN_POINT('Ctrl Pts',(9.57913944099994,11.6,4.20341116699999));
#198758=CARTESIAN_POINT('Ctrl Pts',(9.57767318099994,15.2,4.20302152199999));
#198759=CARTESIAN_POINT('Ctrl Pts',(9.57767318099994,11.6,4.20302152199999));
#198760=CARTESIAN_POINT('Ctrl Pts',(9.57621508799994,15.2,4.20263256899998));
#198761=CARTESIAN_POINT('Ctrl Pts',(9.57621508799994,11.6,4.20263256899998));
#198762=CARTESIAN_POINT('Ctrl Pts',(9.57476517899994,15.2,4.20224432599999));
#198763=CARTESIAN_POINT('Ctrl Pts',(9.57476517899994,11.6,4.20224432599999));
#198764=CARTESIAN_POINT('Ctrl Pts',(9.57332346799994,15.2,4.20185681099999));
#198765=CARTESIAN_POINT('Ctrl Pts',(9.57332346799994,11.6,4.20185681099999));
#198766=CARTESIAN_POINT('Ctrl Pts',(9.57188996999994,15.2,4.20147004499999));
#198767=CARTESIAN_POINT('Ctrl Pts',(9.57188996999994,11.6,4.20147004499999));
#198768=CARTESIAN_POINT('Ctrl Pts',(9.57046470299994,15.2,4.20108404499998));
#198769=CARTESIAN_POINT('Ctrl Pts',(9.57046470299994,11.6,4.20108404499998));
#198770=CARTESIAN_POINT('Ctrl Pts',(9.56904768099994,15.2,4.20069883199999));
#198771=CARTESIAN_POINT('Ctrl Pts',(9.56904768099994,11.6,4.20069883199999));
#198772=CARTESIAN_POINT('Ctrl Pts',(9.56763891899995,15.2,4.20031442499998));
#198773=CARTESIAN_POINT('Ctrl Pts',(9.56763891899995,11.6,4.20031442499998));
#198774=CARTESIAN_POINT('Ctrl Pts',(9.56623843399995,15.2,4.19993084099998));
#198775=CARTESIAN_POINT('Ctrl Pts',(9.56623843399995,11.6,4.19993084099998));
#198776=CARTESIAN_POINT('Ctrl Pts',(9.56484624099994,15.2,4.19954810099998));
#198777=CARTESIAN_POINT('Ctrl Pts',(9.56484624099994,11.6,4.19954810099998));
#198778=CARTESIAN_POINT('Ctrl Pts',(9.56346235699994,15.2,4.19916622499999));
#198779=CARTESIAN_POINT('Ctrl Pts',(9.56346235699994,11.6,4.19916622499999));
#198780=CARTESIAN_POINT('Ctrl Pts',(9.56208679599994,15.2,4.19878523199999));
#198781=CARTESIAN_POINT('Ctrl Pts',(9.56208679599994,11.6,4.19878523199999));
#198782=CARTESIAN_POINT('Ctrl Pts',(9.56071957599995,15.2,4.19840514199999));
#198783=CARTESIAN_POINT('Ctrl Pts',(9.56071957599995,11.6,4.19840514199999));
#198784=CARTESIAN_POINT('Ctrl Pts',(9.55936071099994,15.2,4.19802597299999));
#198785=CARTESIAN_POINT('Ctrl Pts',(9.55936071099994,11.6,4.19802597299998));
#198786=CARTESIAN_POINT('Ctrl Pts',(9.55801021799994,15.2,4.19764774799999));
#198787=CARTESIAN_POINT('Ctrl Pts',(9.55801021799994,11.6,4.19764774799999));
#198788=CARTESIAN_POINT('Ctrl Pts',(9.55666811299994,15.2,4.19727048399999));
#198789=CARTESIAN_POINT('Ctrl Pts',(9.55666811299994,11.6,4.19727048399999));
#198790=CARTESIAN_POINT('Ctrl Pts',(9.55533441299995,15.2,4.19689420199998));
#198791=CARTESIAN_POINT('Ctrl Pts',(9.55533441299995,11.6,4.19689420199998));
#198792=CARTESIAN_POINT('Ctrl Pts',(9.55400913299994,15.2,4.19651892299999));
#198793=CARTESIAN_POINT('Ctrl Pts',(9.55400913299994,11.6,4.19651892299999));
#198794=CARTESIAN_POINT('Ctrl Pts',(9.55269228999994,15.2,4.19614466599998));
#198795=CARTESIAN_POINT('Ctrl Pts',(9.55269228999994,11.6,4.19614466599998));
#198796=CARTESIAN_POINT('Ctrl Pts',(9.55138389999994,15.2,4.19577145199998));
#198797=CARTESIAN_POINT('Ctrl Pts',(9.55138389999994,11.6,4.19577145199998));
#198798=CARTESIAN_POINT('Ctrl Pts',(9.55008397999995,15.2,4.19539930199999));
#198799=CARTESIAN_POINT('Ctrl Pts',(9.55008397999995,11.6,4.19539930199999));
#198800=CARTESIAN_POINT('Ctrl Pts',(9.54879254499994,15.2,4.19502823399998));
#198801=CARTESIAN_POINT('Ctrl Pts',(9.54879254499994,11.6,4.19502823399998));
#198802=CARTESIAN_POINT('Ctrl Pts',(9.54750961299995,15.2,4.19465827199998));
#198803=CARTESIAN_POINT('Ctrl Pts',(9.54750961299995,11.6,4.19465827199998));
#198804=CARTESIAN_POINT('Ctrl Pts',(9.54623519999994,15.2,4.19428943299998));
#198805=CARTESIAN_POINT('Ctrl Pts',(9.54623519999994,11.6,4.19428943299998));
#198806=CARTESIAN_POINT('Ctrl Pts',(9.54496932299995,15.2,4.19392174099999));
#198807=CARTESIAN_POINT('Ctrl Pts',(9.54496932299995,11.6,4.19392174099999));
#198808=CARTESIAN_POINT('Ctrl Pts',(9.54371199799994,15.2,4.19355521499998));
#198809=CARTESIAN_POINT('Ctrl Pts',(9.54371199799994,11.6,4.19355521499998));
#198810=CARTESIAN_POINT('Ctrl Pts',(9.54246324199995,15.2,4.19318987699998));
#198811=CARTESIAN_POINT('Ctrl Pts',(9.54246324199995,11.6,4.19318987699998));
#198812=CARTESIAN_POINT('Ctrl Pts',(9.54122307199994,15.2,4.19282574899999));
#198813=CARTESIAN_POINT('Ctrl Pts',(9.54122307199994,11.6,4.19282574899999));
#198814=CARTESIAN_POINT('Ctrl Pts',(9.53999150599994,15.2,4.19246284899998));
#198815=CARTESIAN_POINT('Ctrl Pts',(9.53999150599994,11.6,4.19246284899998));
#198816=CARTESIAN_POINT('Ctrl Pts',(9.53876855799994,15.2,4.19210119999998));
#198817=CARTESIAN_POINT('Ctrl Pts',(9.53876855799994,11.6,4.19210119999998));
#198818=CARTESIAN_POINT('Ctrl Pts',(9.53755424799994,15.2,4.19174082399999));
#198819=CARTESIAN_POINT('Ctrl Pts',(9.53755424799994,11.6,4.19174082399999));
#198820=CARTESIAN_POINT('Ctrl Pts',(9.53634859199994,15.2,4.19138174299999));
#198821=CARTESIAN_POINT('Ctrl Pts',(9.53634859199994,11.6,4.19138174299999));
#198822=CARTESIAN_POINT('Ctrl Pts',(9.53515160699995,15.2,4.19102397699999));
#198823=CARTESIAN_POINT('Ctrl Pts',(9.53515160699995,11.6,4.19102397699999));
#198824=CARTESIAN_POINT('Ctrl Pts',(9.53396331099994,15.2,4.19066754699998));
#198825=CARTESIAN_POINT('Ctrl Pts',(9.53396331099994,11.6,4.19066754699998));
#198826=CARTESIAN_POINT('Ctrl Pts',(9.53278371899994,15.2,4.19031247799998));
#198827=CARTESIAN_POINT('Ctrl Pts',(9.53278371899994,11.6,4.19031247799998));
#198828=CARTESIAN_POINT('Ctrl Pts',(9.53161285099995,15.2,4.18995878899998));
#198829=CARTESIAN_POINT('Ctrl Pts',(9.53161285099995,11.6,4.18995878899998));
#198830=CARTESIAN_POINT('Ctrl Pts',(9.53045072299994,15.2,4.18960650399999));
#198831=CARTESIAN_POINT('Ctrl Pts',(9.53045072299994,11.6,4.18960650399998));
#198832=CARTESIAN_POINT('Ctrl Pts',(9.52929735299995,15.2,4.18925564399999));
#198833=CARTESIAN_POINT('Ctrl Pts',(9.52929735299995,11.6,4.18925564399998));
#198834=CARTESIAN_POINT('Ctrl Pts',(9.52815275799994,15.2,4.18890623099998));
#198835=CARTESIAN_POINT('Ctrl Pts',(9.52815275799994,11.6,4.18890623099998));
#198836=CARTESIAN_POINT('Ctrl Pts',(9.52701695699995,15.2,4.18855828699999));
#198837=CARTESIAN_POINT('Ctrl Pts',(9.52701695699995,11.6,4.18855828699999));
#198838=CARTESIAN_POINT('Ctrl Pts',(9.52588996599994,15.2,4.18821183699999));
#198839=CARTESIAN_POINT('Ctrl Pts',(9.52588996599994,11.6,4.18821183699999));
#198840=CARTESIAN_POINT('Ctrl Pts',(9.52477180299995,15.2,4.18786690099999));
#198841=CARTESIAN_POINT('Ctrl Pts',(9.52477180299995,11.6,4.18786690099999));
#198842=CARTESIAN_POINT('Ctrl Pts',(9.52366248699994,15.2,4.18752350299999));
#198843=CARTESIAN_POINT('Ctrl Pts',(9.52366248699994,11.6,4.18752350299999));
#198844=CARTESIAN_POINT('Ctrl Pts',(9.52256203499994,15.2,4.18718166499998));
#198845=CARTESIAN_POINT('Ctrl Pts',(9.52256203499994,11.6,4.18718166499998));
#198846=CARTESIAN_POINT('Ctrl Pts',(9.52147046599995,15.2,4.18684140999999));
#198847=CARTESIAN_POINT('Ctrl Pts',(9.52147046599995,11.6,4.18684140999999));
#198848=CARTESIAN_POINT('Ctrl Pts',(9.52038779599994,15.2,4.18650276199998));
#198849=CARTESIAN_POINT('Ctrl Pts',(9.52038779599994,11.6,4.18650276199998));
#198850=CARTESIAN_POINT('Ctrl Pts',(9.51931404499994,15.2,4.18616574199999));
#198851=CARTESIAN_POINT('Ctrl Pts',(9.51931404499994,11.6,4.18616574199999));
#198852=CARTESIAN_POINT('Ctrl Pts',(9.51824922999995,15.2,4.18583037599999));
#198853=CARTESIAN_POINT('Ctrl Pts',(9.51824922999995,11.6,4.18583037599999));
#198854=CARTESIAN_POINT('Ctrl Pts',(9.51719337099994,15.2,4.18549668499999));
#198855=CARTESIAN_POINT('Ctrl Pts',(9.51719337099994,11.6,4.18549668499998));
#198856=CARTESIAN_POINT('Ctrl Pts',(9.51614648399995,15.2,4.18516469399999));
#198857=CARTESIAN_POINT('Ctrl Pts',(9.51614648399995,11.6,4.18516469399999));
#198858=CARTESIAN_POINT('Ctrl Pts',(9.51510858899995,15.2,4.18483442699999));
#198859=CARTESIAN_POINT('Ctrl Pts',(9.51510858899995,11.6,4.18483442699999));
#198860=CARTESIAN_POINT('Ctrl Pts',(9.51407970499995,15.2,4.18450590599999));
#198861=CARTESIAN_POINT('Ctrl Pts',(9.51407970499995,11.6,4.18450590599999));
#198862=CARTESIAN_POINT('Ctrl Pts',(9.51305984899994,15.2,4.18417915699998));
#198863=CARTESIAN_POINT('Ctrl Pts',(9.51305984899994,11.6,4.18417915699998));
#198864=CARTESIAN_POINT('Ctrl Pts',(9.51204903999994,15.2,4.18385420099998));
#198865=CARTESIAN_POINT('Ctrl Pts',(9.51204903999994,11.6,4.18385420099998));
#198866=CARTESIAN_POINT('Ctrl Pts',(9.51104729599994,15.2,4.18353106499998));
#198867=CARTESIAN_POINT('Ctrl Pts',(9.51104729599994,11.6,4.18353106499998));
#198868=CARTESIAN_POINT('Ctrl Pts',(9.51005463899994,15.2,4.18320977199999));
#198869=CARTESIAN_POINT('Ctrl Pts',(9.51005463899994,11.6,4.18320977199999));
#198870=CARTESIAN_POINT('Ctrl Pts',(9.50907108499995,15.2,4.18289034599999));
#198871=CARTESIAN_POINT('Ctrl Pts',(9.50907108499995,11.6,4.18289034599999));
#198872=CARTESIAN_POINT('Ctrl Pts',(9.50809665399994,15.2,4.18257281199998));
#198873=CARTESIAN_POINT('Ctrl Pts',(9.50809665399994,11.6,4.18257281199998));
#198874=CARTESIAN_POINT('Ctrl Pts',(9.50713136399994,15.2,4.18225719599998));
#198875=CARTESIAN_POINT('Ctrl Pts',(9.50713136399994,11.6,4.18225719599998));
#198876=CARTESIAN_POINT('Ctrl Pts',(9.50617523599995,15.2,4.18194351999999));
#198877=CARTESIAN_POINT('Ctrl Pts',(9.50617523599995,11.6,4.18194351999999));
#198878=CARTESIAN_POINT('Ctrl Pts',(9.50522828699994,15.2,4.18163180999999));
#198879=CARTESIAN_POINT('Ctrl Pts',(9.50522828699994,11.6,4.18163180999999));
#198880=CARTESIAN_POINT('Ctrl Pts',(9.50429053899994,15.2,4.18132209199998));
#198881=CARTESIAN_POINT('Ctrl Pts',(9.50429053899994,11.6,4.18132209199998));
#198882=CARTESIAN_POINT('Ctrl Pts',(9.50336200799994,15.2,4.18101438999999));
#198883=CARTESIAN_POINT('Ctrl Pts',(9.50336200799994,11.6,4.18101438999999));
#198884=CARTESIAN_POINT('Ctrl Pts',(9.50244271599994,15.2,4.18070872899998));
#198885=CARTESIAN_POINT('Ctrl Pts',(9.50244271599994,11.6,4.18070872899998));
#198886=CARTESIAN_POINT('Ctrl Pts',(9.50153268199994,15.2,4.18040513599998));
#198887=CARTESIAN_POINT('Ctrl Pts',(9.50153268199994,11.6,4.18040513599998));
#198888=CARTESIAN_POINT('Ctrl Pts',(9.50063192599995,15.2,4.18010363499998));
#198889=CARTESIAN_POINT('Ctrl Pts',(9.50063192599995,11.6,4.18010363499998));
#198890=CARTESIAN_POINT('Ctrl Pts',(9.49974046599994,15.2,4.17980425199998));
#198891=CARTESIAN_POINT('Ctrl Pts',(9.49974046599994,11.6,4.17980425199998));
#198892=CARTESIAN_POINT('Ctrl Pts',(9.49885832399995,15.2,4.17950701299999));
#198893=CARTESIAN_POINT('Ctrl Pts',(9.49885832399995,11.6,4.17950701299999));
#198894=CARTESIAN_POINT('Ctrl Pts',(9.49799054499995,15.2,4.17921364399999));
#198895=CARTESIAN_POINT('Ctrl Pts',(9.49799054499995,11.6,4.17921364399999));
#198896=CARTESIAN_POINT('Ctrl Pts',(9.49730470599994,15.2,4.17898101999998));
#198897=CARTESIAN_POINT('Ctrl Pts',(9.49730470599994,11.6,4.17898101999998));
#198898=CARTESIAN_POINT('Ctrl Pts',(9.49679570899994,15.2,4.17880795499999));
#198899=CARTESIAN_POINT('Ctrl Pts',(9.49679570899994,11.6,4.17880795499998));
#198900=CARTESIAN_POINT('Ctrl Pts',(9.49645984599995,15.2,4.17869357199999));
#198901=CARTESIAN_POINT('Ctrl Pts',(9.49645984599995,11.6,4.17869357199999));
#198902=CARTESIAN_POINT('Ctrl Pts',(9.49629481099995,15.2,4.17863732199999));
#198903=CARTESIAN_POINT('Ctrl Pts',(9.49629481099995,11.6,4.17863732199999));
#198904=CARTESIAN_POINT('',(9.49629481052083,12.2,4.17863732208252));
#198905=CARTESIAN_POINT('',(9.49629481052083,15.2,4.17863732208252));
#198906=CARTESIAN_POINT('',(9.49629481099995,12.2,4.17863732199999));
#198907=CARTESIAN_POINT('Ctrl Pts',(10.6761442619999,12.2,4.27433546899999));
#198908=CARTESIAN_POINT('Ctrl Pts',(10.669789618948,12.2,4.27479929410106));
#198909=CARTESIAN_POINT('Ctrl Pts',(10.663452445214,12.2,4.27524981568719));
#198910=CARTESIAN_POINT('Ctrl Pts',(10.6571327390048,12.2,4.27568705180026));
#198911=CARTESIAN_POINT('Ctrl Pts',(10.653340915417,12.2,4.27594939345856));
#198912=CARTESIAN_POINT('Ctrl Pts',(10.6495553832665,12.2,4.27620695229114));
#198913=CARTESIAN_POINT('Ctrl Pts',(10.6457761750117,12.2,4.27645974928312));
#198914=CARTESIAN_POINT('Ctrl Pts',(10.6419969667568,12.2,4.2767125462751));
#198915=CARTESIAN_POINT('Ctrl Pts',(10.6382240820909,12.2,4.27696058213185));
#198916=CARTESIAN_POINT('Ctrl Pts',(10.6344575619356,12.2,4.27720388420675));
#198917=CARTESIAN_POINT('Ctrl Pts',(10.6306910417802,12.2,4.27744718628166));
#198918=CARTESIAN_POINT('Ctrl Pts',(10.6269308868494,12.2,4.27768575655688));
#198919=CARTESIAN_POINT('Ctrl Pts',(10.6231771321099,12.2,4.2779196179657));
#198920=CARTESIAN_POINT('Ctrl Pts',(10.618172125336,12.2,4.27823143320577));
#198921=CARTESIAN_POINT('Ctrl Pts',(10.6131784967851,12.2,4.27853487774393));
#198922=CARTESIAN_POINT('Ctrl Pts',(10.6081963167132,12.2,4.27883000098355));
#198923=CARTESIAN_POINT('Ctrl Pts',(10.6032141373201,12.2,4.27912512418296));
#198924=CARTESIAN_POINT('Ctrl Pts',(10.5982434084704,12.2,4.27941192655973));
#198925=CARTESIAN_POINT('Ctrl Pts',(10.5932842098191,12.2,4.27969046520447));
#198926=CARTESIAN_POINT('Ctrl Pts',(10.589564809986,12.2,4.27989936923547));
#198927=CARTESIAN_POINT('Ctrl Pts',(10.5858518970797,12.2,4.28010362534848));
#198928=CARTESIAN_POINT('Ctrl Pts',(10.5821455051669,12.2,4.28030325729353));
#198929=CARTESIAN_POINT('Ctrl Pts',(10.5784391139275,12.2,4.28050288920232));
#198930=CARTESIAN_POINT('Ctrl Pts',(10.574739243646,12.2,4.28069789641135));
#198931=CARTESIAN_POINT('Ctrl Pts',(10.5710459278641,12.2,4.28088830427903));
#198932=CARTESIAN_POINT('Ctrl Pts',(10.5661215070452,12.2,4.28114218142441));
#198933=CARTESIAN_POINT('Ctrl Pts',(10.5612087375452,12.2,4.28138787960012));
#198934=CARTESIAN_POINT('Ctrl Pts',(10.5563077004778,12.2,4.28162545748217));
#198935=CARTESIAN_POINT('Ctrl Pts',(10.5501814036427,12.2,4.28192242985899));
#198936=CARTESIAN_POINT('Ctrl Pts',(10.544073437927,12.2,4.28220671058151));
#198937=CARTESIAN_POINT('Ctrl Pts',(10.5379839638983,12.2,4.28247841870717));
#198938=CARTESIAN_POINT('Ctrl Pts',(10.5343302796138,12.2,4.28264144357664));
#198939=CARTESIAN_POINT('Ctrl Pts',(10.5306832517455,12.2,4.28279994107142));
#198940=CARTESIAN_POINT('Ctrl Pts',(10.5270429150435,12.2,4.28295393648311));
#198941=CARTESIAN_POINT('Ctrl Pts',(10.5234025776802,12.2,4.28310793192277));
#198942=CARTESIAN_POINT('Ctrl Pts',(10.5197689319688,12.2,4.28325742446116));
#198943=CARTESIAN_POINT('Ctrl Pts',(10.5161420101926,12.2,4.28340244002329));
#198944=CARTESIAN_POINT('Ctrl Pts',(10.5113061155891,12.2,4.28359579406223));
#198945=CARTESIAN_POINT('Ctrl Pts',(10.5064821785289,12.2,4.28378118984135));
#198946=CARTESIAN_POINT('Ctrl Pts',(10.5016702785115,12.2,4.28395868571656));
#198947=CARTESIAN_POINT('Ctrl Pts',(10.4980613533346,12.2,4.28409180762901));
#198948=CARTESIAN_POINT('Ctrl Pts',(10.4944592003619,12.2,4.28422048582386));
#198949=CARTESIAN_POINT('Ctrl Pts',(10.4908638536586,12.2,4.2843447467364));
#198950=CARTESIAN_POINT('Ctrl Pts',(10.4860700576187,12.2,4.28451042796816));
#198951=CARTESIAN_POINT('Ctrl Pts',(10.4812883603415,12.2,4.28466825377954));
#198952=CARTESIAN_POINT('Ctrl Pts',(10.4765188468601,12.2,4.28481828828721));
#198953=CARTESIAN_POINT('Ctrl Pts',(10.472941712074,12.2,4.28493081415774));
#198954=CARTESIAN_POINT('Ctrl Pts',(10.4693714304371,12.2,4.28503895580379));
#198955=CARTESIAN_POINT('Ctrl Pts',(10.4658080357749,12.2,4.28514274075835));
#198956=CARTESIAN_POINT('Ctrl Pts',(10.4622446411127,12.2,4.28524652571291));
#198957=CARTESIAN_POINT('Ctrl Pts',(10.4586881348419,12.2,4.28534595299265));
#198958=CARTESIAN_POINT('Ctrl Pts',(10.4551385511369,12.2,4.28544104944791));
#198959=CARTESIAN_POINT('Ctrl Pts',(10.4515889674319,12.2,4.28553614590316));
#198960=CARTESIAN_POINT('Ctrl Pts',(10.4480463063163,12.2,4.28562691108157));
#198961=CARTESIAN_POINT('Ctrl Pts',(10.444510603434,12.2,4.28571337249991));
#198962=CARTESIAN_POINT('Ctrl Pts',(10.4409749005517,12.2,4.28579983391826));
#198963=CARTESIAN_POINT('Ctrl Pts',(10.4374461564073,12.2,4.28588199021861));
#198964=CARTESIAN_POINT('Ctrl Pts',(10.4339244052843,12.2,4.28595986921637));
#198965=CARTESIAN_POINT('Ctrl Pts',(10.4304026535215,12.2,4.28603774822827));
#198966=CARTESIAN_POINT('Ctrl Pts',(10.426887896494,12.2,4.2861113499723));
#198967=CARTESIAN_POINT('Ctrl Pts',(10.4233801677352,12.2,4.28618070052346));
#198968=CARTESIAN_POINT('Ctrl Pts',(10.4198724396136,12.2,4.28625005106203));
#198969=CARTESIAN_POINT('Ctrl Pts',(10.4163717412417,12.2,4.28631515095916));
#198970=CARTESIAN_POINT('Ctrl Pts',(10.4128781071192,12.2,4.28637602745658));
#198971=CARTESIAN_POINT('Ctrl Pts',(10.4082199285008,12.2,4.28645719611612));
#198972=CARTESIAN_POINT('Ctrl Pts',(10.4035743106399,12.2,4.2865308568446));
#198973=CARTESIAN_POINT('Ctrl Pts',(10.3989413357306,12.2,4.28659707423203));
#198974=CARTESIAN_POINT('Ctrl Pts',(10.3954666043907,12.2,4.28664673727486));
#198975=CARTESIAN_POINT('Ctrl Pts',(10.3919989861295,12.2,4.28669221344194));
#198976=CARTESIAN_POINT('Ctrl Pts',(10.3885385164626,12.2,4.28673353098267));
#198977=CARTESIAN_POINT('Ctrl Pts',(10.3850780461671,12.2,4.28677484853091));
#198978=CARTESIAN_POINT('Ctrl Pts',(10.3816247245818,12.2,4.28681200815297));
#198979=CARTESIAN_POINT('Ctrl Pts',(10.3781785877486,12.2,4.28684503528221));
#198980=CARTESIAN_POINT('Ctrl Pts',(10.3735837396811,12.2,4.28688907144452));
#198981=CARTESIAN_POINT('Ctrl Pts',(10.3690016642314,12.2,4.28692576481891));
#198982=CARTESIAN_POINT('Ctrl Pts',(10.3644324468819,12.2,4.28695518153921));
#198983=CARTESIAN_POINT('Ctrl Pts',(10.3610055337141,12.2,4.28697724408043));
#198984=CARTESIAN_POINT('Ctrl Pts',(10.3575858539909,12.2,4.28699521367995));
#198985=CARTESIAN_POINT('Ctrl Pts',(10.3541734436102,12.2,4.28700911872228));
#198986=CARTESIAN_POINT('Ctrl Pts',(10.3507610332295,12.2,4.28702302376461));
#198987=CARTESIAN_POINT('Ctrl Pts',(10.3473558927515,12.2,4.28703286423174));
#198988=CARTESIAN_POINT('Ctrl Pts',(10.3439580580406,12.2,4.28703866927374));
#198989=CARTESIAN_POINT('Ctrl Pts',(10.3405602227125,12.2,4.2870444743168));
#198990=CARTESIAN_POINT('Ctrl Pts',(10.3371696935364,12.2,4.2870462436504));
#198991=CARTESIAN_POINT('Ctrl Pts',(10.3337865067957,12.2,4.28704400669119));
#198992=CARTESIAN_POINT('Ctrl Pts',(10.3304033206696,12.2,4.28704176973239));
#198993=CARTESIAN_POINT('Ctrl Pts',(10.3270274775098,12.2,4.28703552628214));
#198994=CARTESIAN_POINT('Ctrl Pts',(10.3236590138412,12.2,4.2870253062405));
#198995=CARTESIAN_POINT('Ctrl Pts',(10.3202905501726,12.2,4.28701508619885));
#198996=CARTESIAN_POINT('Ctrl Pts',(10.3169294662402,12.2,4.28700088816611));
#198997=CARTESIAN_POINT('Ctrl Pts',(10.3135757990135,12.2,4.28698274325));
#198998=CARTESIAN_POINT('Ctrl Pts',(10.3102221317868,12.2,4.28696459833389));
#198999=CARTESIAN_POINT('Ctrl Pts',(10.3068758806301,12.2,4.28694250706586));
#199000=CARTESIAN_POINT('Ctrl Pts',(10.3035370834863,12.2,4.28691649723337));
#199001=CARTESIAN_POINT('Ctrl Pts',(10.2990853535567,12.2,4.28688181745357));
#199002=CARTESIAN_POINT('Ctrl Pts',(10.2946468753079,12.2,4.28684017453431));
#199003=CARTESIAN_POINT('Ctrl Pts',(10.2902217365681,12.2,4.28679163797541));
#199004=CARTESIAN_POINT('Ctrl Pts',(10.2857965984312,12.2,4.28674310142312));
#199005=CARTESIAN_POINT('Ctrl Pts',(10.2813847995981,12.2,4.28668767290783));
#199006=CARTESIAN_POINT('Ctrl Pts',(10.2769864295679,12.2,4.2866254237467));
#199007=CARTESIAN_POINT('Ctrl Pts',(10.269289281266,12.2,4.28651648770412));
#199008=CARTESIAN_POINT('Ctrl Pts',(10.2616332568613,12.2,4.28638666492381));
#199009=CARTESIAN_POINT('Ctrl Pts',(10.254018838161,12.2,4.28623635051793));
#199010=CARTESIAN_POINT('Ctrl Pts',(10.2496677421842,12.2,4.28615045658007));
#199011=CARTESIAN_POINT('Ctrl Pts',(10.2453302314825,12.2,4.28605787097967));
#199012=CARTESIAN_POINT('Ctrl Pts',(10.2410063967235,12.2,4.28595866909956));
#199013=CARTESIAN_POINT('Ctrl Pts',(10.2366825613754,12.2,4.28585946720594));
#199014=CARTESIAN_POINT('Ctrl Pts',(10.2323724014811,12.2,4.28575365020103));
#199015=CARTESIAN_POINT('Ctrl Pts',(10.228076008172,12.2,4.28564129174993));
#199016=CARTESIAN_POINT('Ctrl Pts',(10.2237796154482,12.2,4.28552893331414));
#199017=CARTESIAN_POINT('Ctrl Pts',(10.2194969886475,12.2,4.28541003485126));
#199018=CARTESIAN_POINT('Ctrl Pts',(10.2152282199395,12.2,4.28528467302884));
#199019=CARTESIAN_POINT('Ctrl Pts',(10.2109594506499,12.2,4.28515931118933));
#199020=CARTESIAN_POINT('Ctrl Pts',(10.2067045403671,12.2,4.28502748609921));
#199021=CARTESIAN_POINT('Ctrl Pts',(10.2024635785249,12.2,4.28488927425835));
#199022=CARTESIAN_POINT('Ctrl Pts',(10.197162376511,12.2,4.28471650946668));
#199023=CARTESIAN_POINT('Ctrl Pts',(10.1918829712708,12.2,4.28453376720081));
#199024=CARTESIAN_POINT('Ctrl Pts',(10.186625542497,12.2,4.28434120074157));
#199025=CARTESIAN_POINT('Ctrl Pts',(10.1824195998218,12.2,4.28418714758678));
#199026=CARTESIAN_POINT('Ctrl Pts',(10.1782277209373,12.2,4.28402680845743));
#199027=CARTESIAN_POINT('Ctrl Pts',(10.1740500021663,12.2,4.28386026002723));
#199028=CARTESIAN_POINT('Ctrl Pts',(10.169872282826,12.2,4.28369371157435));
#199029=CARTESIAN_POINT('Ctrl Pts',(10.1657087209566,12.2,4.28352095623476));
#199030=CARTESIAN_POINT('Ctrl Pts',(10.1615594110082,12.2,4.28334207372501));
#199031=CARTESIAN_POINT('Ctrl Pts',(10.1574101010599,12.2,4.28316319121526));
#199032=CARTESIAN_POINT('Ctrl Pts',(10.1532750420465,12.2,4.2829781817909));
#199033=CARTESIAN_POINT('Ctrl Pts',(10.1491543301012,12.2,4.2827871280021));
#199034=CARTESIAN_POINT('Ctrl Pts',(10.141943085039,12.2,4.28245278391074));
#199035=CARTESIAN_POINT('Ctrl Pts',(10.1347757714352,12.2,4.28209992515461));
#199036=CARTESIAN_POINT('Ctrl Pts',(10.1276529035994,12.2,4.28172900023395));
#199037=CARTESIAN_POINT('Ctrl Pts',(10.1235826929322,12.2,4.28151704311167));
#199038=CARTESIAN_POINT('Ctrl Pts',(10.1195269927751,12.2,4.28129918610534));
#199039=CARTESIAN_POINT('Ctrl Pts',(10.1154859009447,12.2,4.28107551498167));
#199040=CARTESIAN_POINT('Ctrl Pts',(10.1114448096649,12.2,4.28085184388846));
#199041=CARTESIAN_POINT('Ctrl Pts',(10.1074183267127,12.2,4.28062235856309));
#199042=CARTESIAN_POINT('Ctrl Pts',(10.1034065473725,12.2,4.2803871434718));
#199043=CARTESIAN_POINT('Ctrl Pts',(10.0993947674857,12.2,4.28015192834845));
#199044=CARTESIAN_POINT('Ctrl Pts',(10.0953976918489,12.2,4.27991098513108));
#199045=CARTESIAN_POINT('Ctrl Pts',(10.0914154172805,12.2,4.27966439878317));
#199046=CARTESIAN_POINT('Ctrl Pts',(10.0874331432547,12.2,4.27941781246886));
#199047=CARTESIAN_POINT('Ctrl Pts',(10.0834656691273,12.2,4.27916558377884));
#199048=CARTESIAN_POINT('Ctrl Pts',(10.0795130938378,12.2,4.27890780130049));
#199049=CARTESIAN_POINT('Ctrl Pts',(10.0755605180098,12.2,4.278650018787));
#199050=CARTESIAN_POINT('Ctrl Pts',(10.071622841097,12.2,4.27838668119244));
#199051=CARTESIAN_POINT('Ctrl Pts',(10.0677001612165,12.2,4.27811787873334));
#199052=CARTESIAN_POINT('Ctrl Pts',(10.0637774813361,12.2,4.27784907627425));
#199053=CARTESIAN_POINT('Ctrl Pts',(10.0598697974907,12.2,4.2775748079173));
#199054=CARTESIAN_POINT('Ctrl Pts',(10.0559772096135,12.2,4.27729516417928));
#199055=CARTESIAN_POINT('Ctrl Pts',(10.0520846222666,12.2,4.27701552047937));
#199056=CARTESIAN_POINT('Ctrl Pts',(10.0482071298238,12.2,4.27673050144721));
#199057=CARTESIAN_POINT('Ctrl Pts',(10.0443448325109,12.2,4.2764401985252));
#199058=CARTESIAN_POINT('Ctrl Pts',(10.0404825346717,12.2,4.27614989556363));
#199059=CARTESIAN_POINT('Ctrl Pts',(10.0366354320612,12.2,4.27585430906497));
#199060=CARTESIAN_POINT('Ctrl Pts',(10.0328036241317,12.2,4.27555352999249));
#199061=CARTESIAN_POINT('Ctrl Pts',(10.0289718167243,12.2,4.275252750961));
#199062=CARTESIAN_POINT('Ctrl Pts',(10.0251553039288,12.2,4.27494677946073));
#199063=CARTESIAN_POINT('Ctrl Pts',(10.0213541867941,12.2,4.27463571104205));
#199064=CARTESIAN_POINT('Ctrl Pts',(10.0175530691415,12.2,4.27432464258099));
#199065=CARTESIAN_POINT('Ctrl Pts',(10.0137673486648,12.2,4.27400847592347));
#199066=CARTESIAN_POINT('Ctrl Pts',(10.0099971239946,12.2,4.27368730494504));
#199067=CARTESIAN_POINT('Ctrl Pts',(10.006226899838,12.2,4.27336613401037));
#199068=CARTESIAN_POINT('Ctrl Pts',(10.0024721738705,12.2,4.27303996064964));
#199069=CARTESIAN_POINT('Ctrl Pts',(9.99873304656404,12.2,4.27270887901036));
#199070=CARTESIAN_POINT('Ctrl Pts',(9.99499391874812,12.2,4.27237779732597));
#199071=CARTESIAN_POINT('Ctrl Pts',(9.99127038951741,12.2,4.27204180815487));
#199072=CARTESIAN_POINT('Ctrl Pts',(9.98756256370525,12.2,4.2717010097471));
#199073=CARTESIAN_POINT('Ctrl Pts',(9.98385473839828,12.2,4.27136021138576));
#199074=CARTESIAN_POINT('Ctrl Pts',(9.98016261534292,12.2,4.27101460046982));
#199075=CARTESIAN_POINT('Ctrl Pts',(9.97648629729176,12.2,4.27066428009248));
#199076=CARTESIAN_POINT('Ctrl Pts',(9.9728099787397,12.2,4.2703139596674));
#199077=CARTESIAN_POINT('Ctrl Pts',(9.9691494664219,12.2,4.26995892624324));
#199078=CARTESIAN_POINT('Ctrl Pts',(9.96550486400209,12.2,4.26959928194556));
#199079=CARTESIAN_POINT('Ctrl Pts',(9.96186026207885,12.2,4.26923963769688));
#199080=CARTESIAN_POINT('Ctrl Pts',(9.9582315701302,12.2,4.26887538111024));
#199081=CARTESIAN_POINT('Ctrl Pts',(9.95461889409056,12.2,4.26850661408529));
#199082=CARTESIAN_POINT('Ctrl Pts',(9.9510062175587,12.2,4.2681378470101));
#199083=CARTESIAN_POINT('Ctrl Pts',(9.94740955575046,12.2,4.26776456899428));
#199084=CARTESIAN_POINT('Ctrl Pts',(9.94382901470578,12.2,4.26738688274974));
#199085=CARTESIAN_POINT('Ctrl Pts',(9.94024847414895,12.2,4.26700919655667));
#199086=CARTESIAN_POINT('Ctrl Pts',(9.93668405516105,12.2,4.26662710246726));
#199087=CARTESIAN_POINT('Ctrl Pts',(9.93313586383835,12.2,4.26624070355484));
#199088=CARTESIAN_POINT('Ctrl Pts',(9.92958767203221,12.2,4.26585430458978));
#199089=CARTESIAN_POINT('Ctrl Pts',(9.92605570773315,12.2,4.26546360055764));
#199090=CARTESIAN_POINT('Ctrl Pts',(9.92254007804154,12.2,4.26506869825834));
#199091=CARTESIAN_POINT('Ctrl Pts',(9.91902444834994,12.2,4.26467379595904));
#199092=CARTESIAN_POINT('Ctrl Pts',(9.91552515345747,12.2,4.26427469383147));
#199093=CARTESIAN_POINT('Ctrl Pts',(9.91204230238044,12.2,4.26387149897574));
#199094=CARTESIAN_POINT('Ctrl Pts',(9.90855945177796,12.2,4.26346830417495));
#199095=CARTESIAN_POINT('Ctrl Pts',(9.90509304365537,12.2,4.26306101685463));
#199096=CARTESIAN_POINT('Ctrl Pts',(9.90164318897723,12.2,4.26264974527528));
#199097=CARTESIAN_POINT('Ctrl Pts',(9.89819333382905,12.2,4.2622384736399));
#199098=CARTESIAN_POINT('Ctrl Pts',(9.89476003118688,12.2,4.26182321604915));
#199099=CARTESIAN_POINT('Ctrl Pts',(9.8913433902246,12.2,4.2614040839148));
#199100=CARTESIAN_POINT('Ctrl Pts',(9.88792674972784,12.2,4.26098495183756));
#199101=CARTESIAN_POINT('Ctrl Pts',(9.88452677105669,12.2,4.26056194624416));
#199102=CARTESIAN_POINT('Ctrl Pts',(9.88114356577661,12.2,4.26013517483485));
#199103=CARTESIAN_POINT('Ctrl Pts',(9.87776036003559,12.2,4.2597084033674));
#199104=CARTESIAN_POINT('Ctrl Pts',(9.87439392829569,12.2,4.2592778680021));
#199105=CARTESIAN_POINT('Ctrl Pts',(9.87104437928059,12.2,4.25884368167864));
#199106=CARTESIAN_POINT('Ctrl Pts',(9.86769483072188,12.2,4.25840949541435));
#199107=CARTESIAN_POINT('Ctrl Pts',(9.86436216789282,12.2,4.25797165675806));
#199108=CARTESIAN_POINT('Ctrl Pts',(9.86104650199609,12.2,4.25753028129438));
#199109=CARTESIAN_POINT('Ctrl Pts',(9.85690191928636,12.2,4.25697856191967));
#199110=CARTESIAN_POINT('Ctrl Pts',(9.85278389494122,12.2,4.25642131443093));
#199111=CARTESIAN_POINT('Ctrl Pts',(9.84869264980094,12.2,4.25585876602842));
#199112=CARTESIAN_POINT('Ctrl Pts',(9.84460140466066,12.2,4.25529621762592));
#199113=CARTESIAN_POINT('Ctrl Pts',(9.84053693832048,12.2,4.25472836873623));
#199114=CARTESIAN_POINT('Ctrl Pts',(9.83649947726041,12.2,4.25415544852531));
#199115=CARTESIAN_POINT('Ctrl Pts',(9.83246201620035,12.2,4.25358252831439));
#199116=CARTESIAN_POINT('Ctrl Pts',(9.82845155932765,12.2,4.25300453780555));
#199117=CARTESIAN_POINT('Ctrl Pts',(9.8244683317582,12.2,4.25242170954166));
#199118=CARTESIAN_POINT('Ctrl Pts',(9.82048510418876,12.2,4.25183888127778));
#199119=CARTESIAN_POINT('Ctrl Pts',(9.81652910786098,12.2,4.25125121828333));
#199120=CARTESIAN_POINT('Ctrl Pts',(9.81260057029154,12.2,4.25065895578333));
#199121=CARTESIAN_POINT('Ctrl Pts',(9.8086720327221,12.2,4.25006669328333));
#199122=CARTESIAN_POINT('Ctrl Pts',(9.80477095437084,12.2,4.24946983258574));
#199123=CARTESIAN_POINT('Ctrl Pts',(9.80089756671443,12.2,4.24886861674967));
#199124=CARTESIAN_POINT('Ctrl Pts',(9.79702417905803,12.2,4.24826740091359));
#199125=CARTESIAN_POINT('Ctrl Pts',(9.79317848250446,12.2,4.24766182984364));
#199126=CARTESIAN_POINT('Ctrl Pts',(9.78936070924203,12.2,4.24705215067676));
#199127=CARTESIAN_POINT('Ctrl Pts',(9.78554293597961,12.2,4.24644247150988));
#199128=CARTESIAN_POINT('Ctrl Pts',(9.78175308901367,12.2,4.24582868342644));
#199129=CARTESIAN_POINT('Ctrl Pts',(9.77799140227903,12.2,4.24521103925958));
#199130=CARTESIAN_POINT('Ctrl Pts',(9.77422971554439,12.2,4.24459339509271));
#199131=CARTESIAN_POINT('Ctrl Pts',(9.77049618983077,12.2,4.2439718940089));
#199132=CARTESIAN_POINT('Ctrl Pts',(9.7667910645782,12.2,4.24334679314408));
#199133=CARTESIAN_POINT('Ctrl Pts',(9.76234491443666,12.2,4.24259667213356));
#199134=CARTESIAN_POINT('Ctrl Pts',(9.75793966089131,12.2,4.24184136578905));
#199135=CARTESIAN_POINT('Ctrl Pts',(9.75357572304987,12.2,4.24108132598333));
#199136=CARTESIAN_POINT('Ctrl Pts',(9.74993910804987,12.2,4.24044795945555));
#199137=CARTESIAN_POINT('Ctrl Pts',(9.74633118422521,12.2,4.23981130718033));
#199138=CARTESIAN_POINT('Ctrl Pts',(9.74275219601459,12.2,4.23917163398298));
#199139=CARTESIAN_POINT('Ctrl Pts',(9.73917320780397,12.2,4.23853196078562));
#199140=CARTESIAN_POINT('Ctrl Pts',(9.7356231577738,12.2,4.23788926851346));
#199141=CARTESIAN_POINT('Ctrl Pts',(9.73210229201145,12.2,4.23724382774943));
#199142=CARTESIAN_POINT('Ctrl Pts',(9.72858142624908,12.2,4.2365983869854));
#199143=CARTESIAN_POINT('Ctrl Pts',(9.7250897465721,12.2,4.23595019926311));
#199144=CARTESIAN_POINT('Ctrl Pts',(9.72162750324028,12.2,4.23529953870742));
#199145=CARTESIAN_POINT('Ctrl Pts',(9.71816525990848,12.2,4.23464887815174));
#199146=CARTESIAN_POINT('Ctrl Pts',(9.71473245426177,12.2,4.23399574767347));
#199147=CARTESIAN_POINT('Ctrl Pts',(9.71132933832993,12.2,4.23334042722391));
#199148=CARTESIAN_POINT('Ctrl Pts',(9.70792622239808,12.2,4.23268510677435));
#199149=CARTESIAN_POINT('Ctrl Pts',(9.70455279944898,12.2,4.23202759820278));
#199150=CARTESIAN_POINT('Ctrl Pts',(9.70120932535422,12.2,4.2313681884804));
#199151=CARTESIAN_POINT('Ctrl Pts',(9.69786585125945,12.2,4.23070877875803));
#199152=CARTESIAN_POINT('Ctrl Pts',(9.69455232774573,12.2,4.23004746754675));
#199153=CARTESIAN_POINT('Ctrl Pts',(9.69126901309542,12.2,4.22938454942161));
#199154=CARTESIAN_POINT('Ctrl Pts',(9.68732903565819,12.2,4.22858904770036));
#199155=CARTESIAN_POINT('Ctrl Pts',(9.68343256301487,12.2,4.2277912288941));
#199156=CARTESIAN_POINT('Ctrl Pts',(9.67958005132343,12.2,4.22699161342307));
#199157=CARTESIAN_POINT('Ctrl Pts',(9.675727539632,12.2,4.22619199795204));
#199158=CARTESIAN_POINT('Ctrl Pts',(9.67191898892038,12.2,4.22539058576451));
#199159=CARTESIAN_POINT('Ctrl Pts',(9.66815486522187,12.2,4.22458790529373));
#199160=CARTESIAN_POINT('Ctrl Pts',(9.66439074152335,12.2,4.22378522482295));
#199161=CARTESIAN_POINT('Ctrl Pts',(9.66067104486998,12.2,4.22298127845007));
#199162=CARTESIAN_POINT('Ctrl Pts',(9.6569962481671,12.2,4.22217660706269));
#199163=CARTESIAN_POINT('Ctrl Pts',(9.65270898512455,12.2,4.22123782372868));
#199164=CARTESIAN_POINT('Ctrl Pts',(9.64848283695619,12.2,4.22029805452518));
#199165=CARTESIAN_POINT('Ctrl Pts',(9.64431856644459,12.2,4.21935818405222));
#199166=CARTESIAN_POINT('Ctrl Pts',(9.64074919190563,12.2,4.21855258083149));
#199167=CARTESIAN_POINT('Ctrl Pts',(9.63722528164741,12.2,4.21774690523353));
#199168=CARTESIAN_POINT('Ctrl Pts',(9.63374732235397,12.2,4.21694172884608));
#199169=CARTESIAN_POINT('Ctrl Pts',(9.63026936274461,12.2,4.2161365523855));
#199170=CARTESIAN_POINT('Ctrl Pts',(9.62683736008971,12.2,4.21533187427494));
#199171=CARTESIAN_POINT('Ctrl Pts',(9.62345180832388,12.2,4.21452828298119));
#199172=CARTESIAN_POINT('Ctrl Pts',(9.62006625686557,12.2,4.21372469176044));
#199173=CARTESIAN_POINT('Ctrl Pts',(9.61672715953014,12.2,4.21292218593322));
#199174=CARTESIAN_POINT('Ctrl Pts',(9.61343502396803,12.2,4.21212136970868));
#199175=CARTESIAN_POINT('Ctrl Pts',(9.61014288840592,12.2,4.21132055348413));
#199176=CARTESIAN_POINT('Ctrl Pts',(9.60689771447714,12.2,4.21052142524137));
#199177=CARTESIAN_POINT('Ctrl Pts',(9.60370002284009,12.2,4.2097246041035));
#199178=CARTESIAN_POINT('Ctrl Pts',(9.60050233091258,12.2,4.20892778289326));
#199179=CARTESIAN_POINT('Ctrl Pts',(9.59735211823965,12.2,4.20813326764152));
#199180=CARTESIAN_POINT('Ctrl Pts',(9.59424991632266,12.2,4.20734169168185));
#199181=CARTESIAN_POINT('Ctrl Pts',(9.59063068117553,12.2,4.20641818650342));
#199182=CARTESIAN_POINT('Ctrl Pts',(9.58707678942903,12.2,4.20549868427875));
#199183=CARTESIAN_POINT('Ctrl Pts',(9.58358910205906,12.2,4.20458421833542));
#199184=CARTESIAN_POINT('Ctrl Pts',(9.58059965539281,12.2,4.20380039029244));
#199185=CARTESIAN_POINT('Ctrl Pts',(9.57765884608958,12.2,4.2030202627748));
#199186=CARTESIAN_POINT('Ctrl Pts',(9.57476722835081,12.2,4.20224450798272));
#199187=CARTESIAN_POINT('Ctrl Pts',(9.57187561087468,12.2,4.20146875326109));
#199188=CARTESIAN_POINT('Ctrl Pts',(9.56903318226246,12.2,4.20069737255097));
#199189=CARTESIAN_POINT('Ctrl Pts',(9.5662405070178,12.2,4.19993105199199));
#199190=CARTESIAN_POINT('Ctrl Pts',(9.56298238572992,12.2,4.19903701129344));
#199191=CARTESIAN_POINT('Ctrl Pts',(9.55979198352252,12.2,4.19814986238899));
#199192=CARTESIAN_POINT('Ctrl Pts',(9.55667021408757,12.2,4.19727072945893));
#199193=CARTESIAN_POINT('Ctrl Pts',(9.55399441185365,12.2,4.19651718698656));
#199194=CARTESIAN_POINT('Ctrl Pts',(9.5513690348193,12.2,4.19576953700177));
#199195=CARTESIAN_POINT('Ctrl Pts',(9.54879467073436,12.2,4.19502851044198));
#199196=CARTESIAN_POINT('Ctrl Pts',(9.54622030664942,12.2,4.19428748388219));
#199197=CARTESIAN_POINT('Ctrl Pts',(9.54369695648298,12.2,4.19355308067831));
#199198=CARTESIAN_POINT('Ctrl Pts',(9.54122522323595,12.2,4.19282605612088));
#199199=CARTESIAN_POINT('Ctrl Pts',(9.5387534897644,12.2,4.19209903149743));
#199200=CARTESIAN_POINT('Ctrl Pts',(9.53633337214024,12.2,4.19137938253835));
#199201=CARTESIAN_POINT('Ctrl Pts',(9.53396548681259,12.2,4.19066788713116));
#199202=CARTESIAN_POINT('Ctrl Pts',(9.53159760170003,12.2,4.18995639178861));
#199203=CARTESIAN_POINT('Ctrl Pts',(9.52928194860096,12.2,4.18925305068308));
#199204=CARTESIAN_POINT('Ctrl Pts',(9.52701915951651,12.2,4.1885586604583));
#199205=CARTESIAN_POINT('Ctrl Pts',(9.52475637043206,12.2,4.18786427023353));
#199206=CARTESIAN_POINT('Ctrl Pts',(9.52254644388275,12.2,4.18717883320012));
#199207=CARTESIAN_POINT('Ctrl Pts',(9.52039002593359,12.2,4.18650316910702));
#199208=CARTESIAN_POINT('Ctrl Pts',(9.51823360778857,12.2,4.18582750495255));
#199209=CARTESIAN_POINT('Ctrl Pts',(9.51613069890119,12.2,4.1851616150052));
#199210=CARTESIAN_POINT('Ctrl Pts',(9.51408196179321,12.2,4.18450634888688));
#199211=CARTESIAN_POINT('Ctrl Pts',(9.51203322487133,12.2,4.18385108282807));
#199212=CARTESIAN_POINT('Ctrl Pts',(9.5100386569622,12.2,4.1832064374462));
#199213=CARTESIAN_POINT('Ctrl Pts',(9.50809893927397,12.2,4.18257329146634));
#199214=CARTESIAN_POINT('Ctrl Pts',(9.50615922158575,12.2,4.18194014548649));
#199215=CARTESIAN_POINT('Ctrl Pts',(9.50427435329407,12.2,4.18131849573663));
#199216=CARTESIAN_POINT('Ctrl Pts',(9.50244503060811,12.2,4.18070924600822));
#199217=CARTESIAN_POINT('Ctrl Pts',(9.50031960011077,12.2,4.18000137857554));
#199218=CARTESIAN_POINT('Ctrl Pts',(9.49826915599089,12.2,4.17931025141339));
#199219=CARTESIAN_POINT('Ctrl Pts',(9.49629481099995,12.2,4.17863732199999));
#199220=CARTESIAN_POINT('Ctrl Pts',(9.49629481099995,15.2,4.17863732199999));
#199221=CARTESIAN_POINT('Ctrl Pts',(9.49798594157082,15.2,4.17921372151895));
#199222=CARTESIAN_POINT('Ctrl Pts',(9.49973290497691,15.2,4.17980347312964));
#199223=CARTESIAN_POINT('Ctrl Pts',(9.50153500128582,15.2,4.18040565895068));
#199224=CARTESIAN_POINT('Ctrl Pts',(9.50334578821404,15.2,4.18101074881613));
#199225=CARTESIAN_POINT('Ctrl Pts',(9.50521223961529,15.2,4.1816283930278));
#199226=CARTESIAN_POINT('Ctrl Pts',(9.50713365465252,15.2,4.1822576810942));
#199227=CARTESIAN_POINT('Ctrl Pts',(9.50905506951522,15.2,4.18288696910345));
#199228=CARTESIAN_POINT('Ctrl Pts',(9.51103144889862,15.2,4.18352790432364));
#199229=CARTESIAN_POINT('Ctrl Pts',(9.51306211074151,15.2,4.18417960529996));
#199230=CARTESIAN_POINT('Ctrl Pts',(9.5150927725844,15.2,4.18483130627629));
#199231=CARTESIAN_POINT('Ctrl Pts',(9.51717771587541,15.2,4.18549377330137));
#199232=CARTESIAN_POINT('Ctrl Pts',(9.5193162788181,15.2,4.18616615539328));
#199233=CARTESIAN_POINT('Ctrl Pts',(9.52145484195506,15.2,4.18683853754627));
#199234=CARTESIAN_POINT('Ctrl Pts',(9.52364702221027,15.2,4.18752083323704));
#199235=CARTESIAN_POINT('Ctrl Pts',(9.52589217325292,15.2,4.18821221560867));
#199236=CARTESIAN_POINT('Ctrl Pts',(9.5285115158301,15.2,4.18901882828137));
#199237=CARTESIAN_POINT('Ctrl Pts',(9.53120295425296,15.2,4.18983780925306));
#199238=CARTESIAN_POINT('Ctrl Pts',(9.53396548681259,15.2,4.19066788713116));
#199239=CARTESIAN_POINT('Ctrl Pts',(9.53633337214024,15.2,4.19137938253835));
#199240=CARTESIAN_POINT('Ctrl Pts',(9.53875348976439,15.2,4.19209903149742));
#199241=CARTESIAN_POINT('Ctrl Pts',(9.54122522323595,15.2,4.19282605612089));
#199242=CARTESIAN_POINT('Ctrl Pts',(9.54369695648298,15.2,4.19355308067831));
#199243=CARTESIAN_POINT('Ctrl Pts',(9.54622030664941,15.2,4.19428748388218));
#199244=CARTESIAN_POINT('Ctrl Pts',(9.54879467073436,15.2,4.19502851044198));
#199245=CARTESIAN_POINT('Ctrl Pts',(9.55136903481931,15.2,4.19576953700178));
#199246=CARTESIAN_POINT('Ctrl Pts',(9.55399441185365,15.2,4.19651718698656));
#199247=CARTESIAN_POINT('Ctrl Pts',(9.55667021408757,15.2,4.19727072945893));
#199248=CARTESIAN_POINT('Ctrl Pts',(9.55934601656456,15.2,4.19802427199975));
#199249=CARTESIAN_POINT('Ctrl Pts',(9.56207224395609,15.2,4.19878370428296));
#199250=CARTESIAN_POINT('Ctrl Pts',(9.56484831852746,15.2,4.19954831707499));
#199251=CARTESIAN_POINT('Ctrl Pts',(9.56901243000625,15.2,4.20069523615885));
#199252=CARTESIAN_POINT('Ctrl Pts',(9.57328869730923,15.2,4.20185380265907));
#199253=CARTESIAN_POINT('Ctrl Pts',(9.57767522277485,15.2,4.20302169499165));
#199254=CARTESIAN_POINT('Ctrl Pts',(9.58059957308527,15.2,4.20380028988003));
#199255=CARTESIAN_POINT('Ctrl Pts',(9.58357292771095,15.2,4.20458303238842));
#199256=CARTESIAN_POINT('Ctrl Pts',(9.58659474116599,15.2,4.20536925614893));
#199257=CARTESIAN_POINT('Ctrl Pts',(9.5896165548955,15.2,4.20615547998085));
#199258=CARTESIAN_POINT('Ctrl Pts',(9.59268682472488,15.2,4.20694518375132));
#199259=CARTESIAN_POINT('Ctrl Pts',(9.59580501631476,15.2,4.20773772187803));
#199260=CARTESIAN_POINT('Ctrl Pts',(9.59892320762139,15.2,4.20853025993276));
#199261=CARTESIAN_POINT('Ctrl Pts',(9.60208931759995,15.2,4.20932563084563));
#199262=CARTESIAN_POINT('Ctrl Pts',(9.60530282298319,15.2,4.21012320398331));
#199263=CARTESIAN_POINT('Ctrl Pts',(9.60905191279156,15.2,4.21105370602558));
#199264=CARTESIAN_POINT('Ctrl Pts',(9.61286551026422,15.2,4.21198720588282));
#199265=CARTESIAN_POINT('Ctrl Pts',(9.61674279506314,15.2,4.21292272706922));
#199266=CARTESIAN_POINT('Ctrl Pts',(9.62006618186113,15.2,4.21372460233024));
#199267=CARTESIAN_POINT('Ctrl Pts',(9.62343636180731,15.2,4.21452796402086));
#199268=CARTESIAN_POINT('Ctrl Pts',(9.62685282551652,15.2,4.21533221424165));
#199269=CARTESIAN_POINT('Ctrl Pts',(9.63026928922573,15.2,4.21613646446244));
#199270=CARTESIAN_POINT('Ctrl Pts',(9.63373204098209,15.2,4.21694160434445));
#199271=CARTESIAN_POINT('Ctrl Pts',(9.63724057986057,15.2,4.21774705068874));
#199272=CARTESIAN_POINT('Ctrl Pts',(9.64133387543126,15.2,4.21868673813918));
#199273=CARTESIAN_POINT('Ctrl Pts',(9.64548949482863,15.2,4.21962684247424));
#199274=CARTESIAN_POINT('Ctrl Pts',(9.64970666424153,15.2,4.22056646347498));
#199275=CARTESIAN_POINT('Ctrl Pts',(9.65332138069351,15.2,4.22137185286239));
#199276=CARTESIAN_POINT('Ctrl Pts',(9.65698131586871,15.2,4.22217688818619));
#199277=CARTESIAN_POINT('Ctrl Pts',(9.6606859936666,15.2,4.22298101661386));
#199278=CARTESIAN_POINT('Ctrl Pts',(9.66439067180099,15.2,4.22378514511458));
#199279=CARTESIAN_POINT('Ctrl Pts',(9.66814009081196,15.2,4.22458836783545));
#199280=CARTESIAN_POINT('Ctrl Pts',(9.67193378093839,15.2,4.22539014362905));
#199281=CARTESIAN_POINT('Ctrl Pts',(9.67572747072024,15.2,4.22619191934981));
#199282=CARTESIAN_POINT('Ctrl Pts',(9.67956543148328,15.2,4.22699225134241));
#199283=CARTESIAN_POINT('Ctrl Pts',(9.68344720027664,15.2,4.22779061098368));
#199284=CARTESIAN_POINT('Ctrl Pts',(9.68732896906999,15.2,4.22858897062496));
#199285=CARTESIAN_POINT('Ctrl Pts',(9.69125454579651,15.2,4.22938535806045));
#199286=CARTESIAN_POINT('Ctrl Pts',(9.69522347448375,15.2,4.23017926144838));
#199287=CARTESIAN_POINT('Ctrl Pts',(9.69853091517662,15.2,4.23084084762902));
#199288=CARTESIAN_POINT('Ctrl Pts',(9.70186846165916,15.2,4.2315007060513));
#199289=CARTESIAN_POINT('Ctrl Pts',(9.70523585408815,15.2,4.23215854973196));
#199290=CARTESIAN_POINT('Ctrl Pts',(9.70860324651715,15.2,4.23281639341262));
#199291=CARTESIAN_POINT('Ctrl Pts',(9.71200048621029,15.2,4.23347221832444));
#199292=CARTESIAN_POINT('Ctrl Pts',(9.71542731303134,15.2,4.2341257422163));
#199293=CARTESIAN_POINT('Ctrl Pts',(9.71953950506719,15.2,4.23490997085804));
#199294=CARTESIAN_POINT('Ctrl Pts',(9.72369430671445,15.2,4.23569088423493));
#199295=CARTESIAN_POINT('Ctrl Pts',(9.72789127855908,15.2,4.23646799712362));
#199296=CARTESIAN_POINT('Ctrl Pts',(9.73138875522334,15.2,4.23711559122106));
#199297=CARTESIAN_POINT('Ctrl Pts',(9.73491551802269,15.2,4.23776054943762));
#199298=CARTESIAN_POINT('Ctrl Pts',(9.7384713158372,15.2,4.23840259440045));
#199299=CARTESIAN_POINT('Ctrl Pts',(9.74273827344717,15.2,4.23917304839784));
#199300=CARTESIAN_POINT('Ctrl Pts',(9.74704704393414,15.2,4.23993931013349));
#199301=CARTESIAN_POINT('Ctrl Pts',(9.75139719917405,15.2,4.24070091409134));
#199302=CARTESIAN_POINT('Ctrl Pts',(9.75502232834309,15.2,4.24133558402163));
#199303=CARTESIAN_POINT('Ctrl Pts',(9.75867619725699,15.2,4.24196702068798));
#199304=CARTESIAN_POINT('Ctrl Pts',(9.76235856323153,15.2,4.2425949605488));
#199305=CARTESIAN_POINT('Ctrl Pts',(9.76677740224046,15.2,4.24334848835441));
#199306=CARTESIAN_POINT('Ctrl Pts',(9.77123727704875,15.2,4.24409698010938));
#199307=CARTESIAN_POINT('Ctrl Pts',(9.77573777197032,15.2,4.2448399919988));
#199308=CARTESIAN_POINT('Ctrl Pts',(9.77948818454122,15.2,4.24545916859582));
#199309=CARTESIAN_POINT('Ctrl Pts',(9.78326680533643,15.2,4.24607453982349));
#199310=CARTESIAN_POINT('Ctrl Pts',(9.78707339874066,15.2,4.24668585232328));
#199311=CARTESIAN_POINT('Ctrl Pts',(9.7908799921449,15.2,4.24729716482307));
#199312=CARTESIAN_POINT('Ctrl Pts',(9.79471455740344,15.2,4.2479044191346));
#199313=CARTESIAN_POINT('Ctrl Pts',(9.79857685947333,15.2,4.24850736680331));
#199314=CARTESIAN_POINT('Ctrl Pts',(9.80243916154321,15.2,4.24911031447202));
#199315=CARTESIAN_POINT('Ctrl Pts',(9.8063292009045,15.2,4.24970895587251));
#199316=CARTESIAN_POINT('Ctrl Pts',(9.8102467452123,15.2,4.2503030483027));
#199317=CARTESIAN_POINT('Ctrl Pts',(9.81416428952011,15.2,4.25089714073288));
#199318=CARTESIAN_POINT('Ctrl Pts',(9.81810933927836,15.2,4.25148668162132));
#199319=CARTESIAN_POINT('Ctrl Pts',(9.8220816652528,15.2,4.25207143425981));
#199320=CARTESIAN_POINT('Ctrl Pts',(9.82605399122725,15.2,4.25265618689831));
#199321=CARTESIAN_POINT('Ctrl Pts',(9.83005359330769,15.2,4.25323614965339));
#199322=CARTESIAN_POINT('Ctrl Pts',(9.83408024351824,15.2,4.25381108958353));
#199323=CARTESIAN_POINT('Ctrl Pts',(9.83810689328988,15.2,4.25438602945101));
#199324=CARTESIAN_POINT('Ctrl Pts',(9.84216059332423,15.2,4.2549559434317));
#199325=CARTESIAN_POINT('Ctrl Pts',(9.84624111718282,15.2,4.25552060267614));
#199326=CARTESIAN_POINT('Ctrl Pts',(9.85032164148619,15.2,4.25608526198213));
#199327=CARTESIAN_POINT('Ctrl Pts',(9.85442899020022,15.2,4.25664466612154));
#199328=CARTESIAN_POINT('Ctrl Pts',(9.85856294047583,15.2,4.25719858792754));
#199329=CARTESIAN_POINT('Ctrl Pts',(9.86435047095179,15.2,4.25797407846802));
#199330=CARTESIAN_POINT('Ctrl Pts',(9.87019014345699,15.2,4.25873882197897));
#199331=CARTESIAN_POINT('Ctrl Pts',(9.87608135096425,15.2,4.25949220904971));
#199332=CARTESIAN_POINT('Ctrl Pts',(9.88028935626106,15.2,4.26003034266327));
#199333=CARTESIAN_POINT('Ctrl Pts',(9.88452365741654,15.2,4.2605626834));
#199334=CARTESIAN_POINT('Ctrl Pts',(9.88878403595821,15.2,4.26108901048334));
#199335=CARTESIAN_POINT('Ctrl Pts',(9.89304441449987,15.2,4.26161533756667));
#199336=CARTESIAN_POINT('Ctrl Pts',(9.89733087027703,15.2,4.26213565575907));
#199337=CARTESIAN_POINT('Ctrl Pts',(9.90164318897723,15.2,4.26264974527528));
#199338=CARTESIAN_POINT('Ctrl Pts',(9.90509304365537,15.2,4.26306101685463));
#199339=CARTESIAN_POINT('Ctrl Pts',(9.90855945177796,15.2,4.26346830417495));
#199340=CARTESIAN_POINT('Ctrl Pts',(9.91204230238044,15.2,4.26387149897575));
#199341=CARTESIAN_POINT('Ctrl Pts',(9.91552515345746,15.2,4.26427469383147));
#199342=CARTESIAN_POINT('Ctrl Pts',(9.91902444834994,15.2,4.26467379595904));
#199343=CARTESIAN_POINT('Ctrl Pts',(9.92254007804154,15.2,4.26506869825834));
#199344=CARTESIAN_POINT('Ctrl Pts',(9.92693461491655,15.2,4.26556232610556));
#199345=CARTESIAN_POINT('Ctrl Pts',(9.93135467435427,15.2,4.26604939372033));
#199346=CARTESIAN_POINT('Ctrl Pts',(9.93580004798564,15.2,4.26652969400026));
#199347=CARTESIAN_POINT('Ctrl Pts',(9.93935634660001,15.2,4.2669139341928));
#199348=CARTESIAN_POINT('Ctrl Pts',(9.9429288464165,15.2,4.26729384361607));
#199349=CARTESIAN_POINT('Ctrl Pts',(9.94651744095482,15.2,4.26766931919694));
#199350=CARTESIAN_POINT('Ctrl Pts',(9.95010603598209,15.2,4.26804479482897));
#199351=CARTESIAN_POINT('Ctrl Pts',(9.9537107239081,15.2,4.26841583600502));
#199352=CARTESIAN_POINT('Ctrl Pts',(9.95733140221654,15.2,4.26878234219167));
#199353=CARTESIAN_POINT('Ctrl Pts',(9.96095208052498,15.2,4.26914884837832));
#199354=CARTESIAN_POINT('Ctrl Pts',(9.96458874695751,15.2,4.26951081646443));
#199355=CARTESIAN_POINT('Ctrl Pts',(9.96824129804708,15.2,4.26986814931676));
#199356=CARTESIAN_POINT('Ctrl Pts',(9.97189384863901,15.2,4.27022548212041));
#199357=CARTESIAN_POINT('Ctrl Pts',(9.97556228326243,15.2,4.27057817647662));
#199358=CARTESIAN_POINT('Ctrl Pts',(9.97924649725571,15.2,4.27092613544977));
#199359=CARTESIAN_POINT('Ctrl Pts',(9.98385176512377,15.2,4.27136108420176));
#199360=CARTESIAN_POINT('Ctrl Pts',(9.98848168787209,15.2,4.27178863162222));
#199361=CARTESIAN_POINT('Ctrl Pts',(9.99313606648321,15.2,4.27220858773334));
#199362=CARTESIAN_POINT('Ctrl Pts',(9.99779044509433,15.2,4.27262854384445));
#199363=CARTESIAN_POINT('Ctrl Pts',(10.002469276581,15.2,4.27304090733174));
#199364=CARTESIAN_POINT('Ctrl Pts',(10.0071723634774,15.2,4.27344549025022));
#199365=CARTESIAN_POINT('Ctrl Pts',(10.010934832687,15.2,4.27376915655855));
#199366=CARTESIAN_POINT('Ctrl Pts',(10.0147128242775,15.2,4.27408784355718));
#199367=CARTESIAN_POINT('Ctrl Pts',(10.0185062363547,15.2,4.27440145519873));
#199368=CARTESIAN_POINT('Ctrl Pts',(10.0232480018388,15.2,4.27479346978271));
#199369=CARTESIAN_POINT('Ctrl Pts',(10.0280138644809,15.2,4.27517755617239));
#199370=CARTESIAN_POINT('Ctrl Pts',(10.0328036241317,15.2,4.27555352999249));
#199371=CARTESIAN_POINT('Ctrl Pts',(10.0375933837825,15.2,4.2759295038126));
#199372=CARTESIAN_POINT('Ctrl Pts',(10.0424070412595,15.2,4.2762973645508));
#199373=CARTESIAN_POINT('Ctrl Pts',(10.0472444026801,15.2,4.27665693345824));
#199374=CARTESIAN_POINT('Ctrl Pts',(10.0511142920274,15.2,4.27694458859986));
#199375=CARTESIAN_POINT('Ctrl Pts',(10.0549993504859,15.2,4.27722693739397));
#199376=CARTESIAN_POINT('Ctrl Pts',(10.0588994803105,15.2,4.2775038877976));
#199377=CARTESIAN_POINT('Ctrl Pts',(10.0627996096038,15.2,4.27778083816349));
#199378=CARTESIAN_POINT('Ctrl Pts',(10.0667148089273,15.2,4.27805239009714));
#199379=CARTESIAN_POINT('Ctrl Pts',(10.0706449808823,15.2,4.27831845446484));
#199380=CARTESIAN_POINT('Ctrl Pts',(10.0745751533728,15.2,4.27858451886878));
#199381=CARTESIAN_POINT('Ctrl Pts',(10.0785202979298,15.2,4.27884509511848));
#199382=CARTESIAN_POINT('Ctrl Pts',(10.0824803170526,15.2,4.27910009546685));
#199383=CARTESIAN_POINT('Ctrl Pts',(10.0864403356358,15.2,4.27935509578047));
#199384=CARTESIAN_POINT('Ctrl Pts',(10.0904152277141,15.2,4.27960451975727));
#199385=CARTESIAN_POINT('Ctrl Pts',(10.0944048958309,15.2,4.27984827896015));
#199386=CARTESIAN_POINT('Ctrl Pts',(10.0983945644913,15.2,4.28009203819624));
#199387=CARTESIAN_POINT('Ctrl Pts',(10.1023990111947,15.2,4.2803301339179));
#199388=CARTESIAN_POINT('Ctrl Pts',(10.1064181370249,15.2,4.28056247954168));
#199389=CARTESIAN_POINT('Ctrl Pts',(10.1114420440388,15.2,4.28085291155556));
#199390=CARTESIAN_POINT('Ctrl Pts',(10.116488887711,15.2,4.28113435610556));
#199391=CARTESIAN_POINT('Ctrl Pts',(10.1215584822249,15.2,4.28140665075834));
#199392=CARTESIAN_POINT('Ctrl Pts',(10.1266280767388,15.2,4.28167894541112));
#199393=CARTESIAN_POINT('Ctrl Pts',(10.1317204193683,15.2,4.28194208678235));
#199394=CARTESIAN_POINT('Ctrl Pts',(10.1368353265443,15.2,4.28219591324181));
#199395=CARTESIAN_POINT('Ctrl Pts',(10.1409272519507,15.2,4.28239897439278));
#199396=CARTESIAN_POINT('Ctrl Pts',(10.1450336187173,15.2,4.28259607423933));
#199397=CARTESIAN_POINT('Ctrl Pts',(10.1491543301012,15.2,4.2827871280021));
#199398=CARTESIAN_POINT('Ctrl Pts',(10.1532750420465,15.2,4.28297818179091));
#199399=CARTESIAN_POINT('Ctrl Pts',(10.1574101010599,15.2,4.28316319121526));
#199400=CARTESIAN_POINT('Ctrl Pts',(10.1615594110082,15.2,4.28334207372501));
#199401=CARTESIAN_POINT('Ctrl Pts',(10.1677833753654,15.2,4.28361039746527));
#199402=CARTESIAN_POINT('Ctrl Pts',(10.1740394048079,15.2,4.28386493638929));
#199403=CARTESIAN_POINT('Ctrl Pts',(10.1803271873917,15.2,4.28410541622671));
#199404=CARTESIAN_POINT('Ctrl Pts',(10.1855670064019,15.2,4.28430581609852));
#199405=CARTESIAN_POINT('Ctrl Pts',(10.1908288732056,15.2,4.28449645561538));
#199406=CARTESIAN_POINT('Ctrl Pts',(10.1961126094545,15.2,4.28467717721313));
#199407=CARTESIAN_POINT('Ctrl Pts',(10.2003395986839,15.2,4.28482175449921));
#199408=CARTESIAN_POINT('Ctrl Pts',(10.2045805831178,15.2,4.28495998663174));
#199409=CARTESIAN_POINT('Ctrl Pts',(10.2088354710729,15.2,4.28509179252739));
#199410=CARTESIAN_POINT('Ctrl Pts',(10.2130903584481,15.2,4.28522359840509));
#199411=CARTESIAN_POINT('Ctrl Pts',(10.2173591502131,15.2,4.28534897926372));
#199412=CARTESIAN_POINT('Ctrl Pts',(10.2216417543535,15.2,4.28546785848272));
#199413=CARTESIAN_POINT('Ctrl Pts',(10.2259243590775,15.2,4.28558673771793));
#199414=CARTESIAN_POINT('Ctrl Pts',(10.2302207750916,15.2,4.28569911543937));
#199415=CARTESIAN_POINT('Ctrl Pts',(10.2345309118274,15.2,4.28580491350026));
#199416=CARTESIAN_POINT('Ctrl Pts',(10.2388410479759,15.2,4.28591071154674));
#199417=CARTESIAN_POINT('Ctrl Pts',(10.2431649057995,15.2,4.28600993291398));
#199418=CARTESIAN_POINT('Ctrl Pts',(10.2475023938324,15.2,4.28610250001821));
#199419=CARTESIAN_POINT('Ctrl Pts',(10.2518398824563,15.2,4.28619506713505));
#199420=CARTESIAN_POINT('Ctrl Pts',(10.2561910007951,15.2,4.28628097952041));
#199421=CARTESIAN_POINT('Ctrl Pts',(10.2605556607195,15.2,4.28636016402506));
#199422=CARTESIAN_POINT('Ctrl Pts',(10.2649203200493,15.2,4.28643934851893));
#199423=CARTESIAN_POINT('Ctrl Pts',(10.2692985199811,15.2,4.28651180541339));
#199424=CARTESIAN_POINT('Ctrl Pts',(10.2736901700652,15.2,4.28657745946427));
#199425=CARTESIAN_POINT('Ctrl Pts',(10.2802776460888,15.2,4.28667594055402));
#199426=CARTESIAN_POINT('Ctrl Pts',(10.286895386357,15.2,4.28675911825896));
#199427=CARTESIAN_POINT('Ctrl Pts',(10.293543091304,15.2,4.28682674701196));
#199428=CARTESIAN_POINT('Ctrl Pts',(10.3001907956471,15.2,4.28689437575882));
#199429=CARTESIAN_POINT('Ctrl Pts',(10.3068684645602,15.2,4.28694645341778));
#199430=CARTESIAN_POINT('Ctrl Pts',(10.3135757990135,15.2,4.28698274325));
#199431=CARTESIAN_POINT('Ctrl Pts',(10.3169294662402,15.2,4.28700088816611));
#199432=CARTESIAN_POINT('Ctrl Pts',(10.3202905501726,15.2,4.28701508619886));
#199433=CARTESIAN_POINT('Ctrl Pts',(10.3236590138412,15.2,4.2870253062405));
#199434=CARTESIAN_POINT('Ctrl Pts',(10.3270274775098,15.2,4.28703552628215));
#199435=CARTESIAN_POINT('Ctrl Pts',(10.3304033206696,15.2,4.28704176973239));
#199436=CARTESIAN_POINT('Ctrl Pts',(10.3337865067957,15.2,4.28704400669119));
#199437=CARTESIAN_POINT('Ctrl Pts',(10.3371696935364,15.2,4.2870462436504));
#199438=CARTESIAN_POINT('Ctrl Pts',(10.3405602227125,15.2,4.2870444743168));
#199439=CARTESIAN_POINT('Ctrl Pts',(10.3439580580406,15.2,4.28703866927374));
#199440=CARTESIAN_POINT('Ctrl Pts',(10.3473558927515,15.2,4.28703286423174));
#199441=CARTESIAN_POINT('Ctrl Pts',(10.3507610332295,15.2,4.28702302376461));
#199442=CARTESIAN_POINT('Ctrl Pts',(10.3541734436102,15.2,4.28700911872228));
#199443=CARTESIAN_POINT('Ctrl Pts',(10.3575858539909,15.2,4.28699521367995));
#199444=CARTESIAN_POINT('Ctrl Pts',(10.3610055337141,15.2,4.28697724408043));
#199445=CARTESIAN_POINT('Ctrl Pts',(10.3644324468819,15.2,4.28695518153921));
#199446=CARTESIAN_POINT('Ctrl Pts',(10.3678593600497,15.2,4.28693311899799));
#199447=CARTESIAN_POINT('Ctrl Pts',(10.3712935062416,15.2,4.28690696299891));
#199448=CARTESIAN_POINT('Ctrl Pts',(10.3747348484916,15.2,4.28687668645835));
#199449=CARTESIAN_POINT('Ctrl Pts',(10.3781761907415,15.2,4.28684640991778));
#199450=CARTESIAN_POINT('Ctrl Pts',(10.3816247301495,15.2,4.28681201195238));
#199451=CARTESIAN_POINT('Ctrl Pts',(10.3850804298983,15.2,4.28677346349581));
#199452=CARTESIAN_POINT('Ctrl Pts',(10.3885361296472,15.2,4.28673491503924));
#199453=CARTESIAN_POINT('Ctrl Pts',(10.3919989898822,15.2,4.2866922177592));
#199454=CARTESIAN_POINT('Ctrl Pts',(10.3954689752619,15.2,4.28664534275904));
#199455=CARTESIAN_POINT('Ctrl Pts',(10.3989389606417,15.2,4.28659846775889));
#199456=CARTESIAN_POINT('Ctrl Pts',(10.4024160710846,15.2,4.28654741500947));
#199457=CARTESIAN_POINT('Ctrl Pts',(10.4059002692903,15.2,4.28649215747039));
#199458=CARTESIAN_POINT('Ctrl Pts',(10.411707266511,15.2,4.28640006156857));
#199459=CARTESIAN_POINT('Ctrl Pts',(10.4175339539868,15.2,4.28629628475861));
#199460=CARTESIAN_POINT('Ctrl Pts',(10.4233801677352,15.2,4.28618070052346));
#199461=CARTESIAN_POINT('Ctrl Pts',(10.426887896494,15.2,4.2861113499723));
#199462=CARTESIAN_POINT('Ctrl Pts',(10.4304026535215,15.2,4.28603774822827));
#199463=CARTESIAN_POINT('Ctrl Pts',(10.4339244052843,15.2,4.28595986921637));
#199464=CARTESIAN_POINT('Ctrl Pts',(10.4374461564073,15.2,4.28588199021861));
#199465=CARTESIAN_POINT('Ctrl Pts',(10.4409749005517,15.2,4.28579983391826));
#199466=CARTESIAN_POINT('Ctrl Pts',(10.444510603434,15.2,4.28571337249991));
#199467=CARTESIAN_POINT('Ctrl Pts',(10.4480463063163,15.2,4.28562691108157));
#199468=CARTESIAN_POINT('Ctrl Pts',(10.4515889674319,15.2,4.28553614590317));
#199469=CARTESIAN_POINT('Ctrl Pts',(10.4551385511369,15.2,4.28544104944791));
#199470=CARTESIAN_POINT('Ctrl Pts',(10.4598713291953,15.2,4.28531425417999));
#199471=CARTESIAN_POINT('Ctrl Pts',(10.4646164147706,15.2,4.28517975916085));
#199472=CARTESIAN_POINT('Ctrl Pts',(10.4693737242137,15.2,4.2850375025066));
#199473=CARTESIAN_POINT('Ctrl Pts',(10.4753203615039,15.2,4.28485968167426));
#199474=CARTESIAN_POINT('Ctrl Pts',(10.4812860999909,15.2,4.28466973338657));
#199475=CARTESIAN_POINT('Ctrl Pts',(10.4872707756838,15.2,4.28446753602646));
#199476=CARTESIAN_POINT('Ctrl Pts',(10.4932554513767,15.2,4.28426533866635));
#199477=CARTESIAN_POINT('Ctrl Pts',(10.499259066218,15.2,4.28405089300899));
#199478=CARTESIAN_POINT('Ctrl Pts',(10.5052814588092,15.2,4.2838240820263));
#199479=CARTESIAN_POINT('Ctrl Pts',(10.5113038514004,15.2,4.28359727104361));
#199480=CARTESIAN_POINT('Ctrl Pts',(10.5173450222325,15.2,4.2833580927713));
#199481=CARTESIAN_POINT('Ctrl Pts',(10.5234048088287,15.2,4.28310643200807));
#199482=CARTESIAN_POINT('Ctrl Pts',(10.5270406806543,15.2,4.28295543555561));
#199483=CARTESIAN_POINT('Ctrl Pts',(10.5306832557212,15.2,4.28279994502846));
#199484=CARTESIAN_POINT('Ctrl Pts',(10.5343324984627,15.2,4.28263993557656));
#199485=CARTESIAN_POINT('Ctrl Pts',(10.5379817418672,15.2,4.28247992609559));
#199486=CARTESIAN_POINT('Ctrl Pts',(10.5416376536818,15.2,4.28231539773834));
#199487=CARTESIAN_POINT('Ctrl Pts',(10.54530019909,15.2,4.28214632671315));
#199488=CARTESIAN_POINT('Ctrl Pts',(10.5514044398845,15.2,4.28186454174283));
#199489=CARTESIAN_POINT('Ctrl Pts',(10.557527107662,15.2,4.281570133839));
#199490=CARTESIAN_POINT('Ctrl Pts',(10.5636680442133,15.2,4.28126299304019));
#199491=CARTESIAN_POINT('Ctrl Pts',(10.5673526070813,15.2,4.28107870851403));
#199492=CARTESIAN_POINT('Ctrl Pts',(10.5710437461177,15.2,4.28088983916992));
#199493=CARTESIAN_POINT('Ctrl Pts',(10.574741428531,15.2,4.28069636218284));
#199494=CARTESIAN_POINT('Ctrl Pts',(10.5784391102725,15.2,4.28050288523091));
#199495=CARTESIAN_POINT('Ctrl Pts',(10.5821433354387,15.2,4.28030480038755));
#199496=CARTESIAN_POINT('Ctrl Pts',(10.5858540701795,15.2,4.28010208297784));
#199497=CARTESIAN_POINT('Ctrl Pts',(10.5908017162758,15.2,4.27983179311051));
#199498=CARTESIAN_POINT('Ctrl Pts',(10.5957609355127,15.2,4.2795532686012));
#199499=CARTESIAN_POINT('Ctrl Pts',(10.6007316445204,15.2,4.27926645199992));
#199500=CARTESIAN_POINT('Ctrl Pts',(10.6044596764454,15.2,4.2790513395392));
#199501=CARTESIAN_POINT('Ctrl Pts',(10.6081941717378,15.2,4.27883156294015));
#199502=CARTESIAN_POINT('Ctrl Pts',(10.6119350964761,15.2,4.27860709757395));
#199503=CARTESIAN_POINT('Ctrl Pts',(10.6156760218939,15.2,4.27838263216697));
#199504=CARTESIAN_POINT('Ctrl Pts',(10.6194233766885,15.2,4.27815347941699));
#199505=CARTESIAN_POINT('Ctrl Pts',(10.6231771321099,15.2,4.2779196179657));
#199506=CARTESIAN_POINT('Ctrl Pts',(10.6269308868494,15.2,4.27768575655688));
#199507=CARTESIAN_POINT('Ctrl Pts',(10.6306910417802,15.2,4.27744718628166));
#199508=CARTESIAN_POINT('Ctrl Pts',(10.6344575619356,15.2,4.27720388420675));
#199509=CARTESIAN_POINT('Ctrl Pts',(10.6394795885813,15.2,4.27687948145495));
#199510=CARTESIAN_POINT('Ctrl Pts',(10.6445129285515,15.2,4.27654666277957));
#199511=CARTESIAN_POINT('Ctrl Pts',(10.6495574895013,15.2,4.27620536429116));
#199512=CARTESIAN_POINT('Ctrl Pts',(10.6533409103855,15.2,4.27594939041323));
#199513=CARTESIAN_POINT('Ctrl Pts',(10.6571306412445,15.2,4.27568864613094));
#199514=CARTESIAN_POINT('Ctrl Pts',(10.660926659439,15.2,4.27542311601623));
#199515=CARTESIAN_POINT('Ctrl Pts',(10.6659880174915,15.2,4.27506907583115));
#199516=CARTESIAN_POINT('Ctrl Pts',(10.6710605472813,15.2,4.27470652910107));
#199517=CARTESIAN_POINT('Ctrl Pts',(10.6761442619999,15.2,4.27433546899999));
#199518=CARTESIAN_POINT('Ctrl Pts',(9.86852965799994,15.2,3.20199116299998));
#199519=CARTESIAN_POINT('Ctrl Pts',(9.86852965799994,11.6,3.20199116299998));
#199520=CARTESIAN_POINT('Ctrl Pts',(9.86869026599994,15.2,3.20205902699998));
#199521=CARTESIAN_POINT('Ctrl Pts',(9.86869026599994,11.6,3.20205902699998));
#199522=CARTESIAN_POINT('Ctrl Pts',(9.86901705899994,15.2,3.20219720599999));
#199523=CARTESIAN_POINT('Ctrl Pts',(9.86901705899994,11.6,3.20219720599999));
#199524=CARTESIAN_POINT('Ctrl Pts',(9.86951212399994,15.2,3.20240682499998));
#199525=CARTESIAN_POINT('Ctrl Pts',(9.86951212399994,11.6,3.20240682499998));
#199526=CARTESIAN_POINT('Ctrl Pts',(9.87017881199994,15.2,3.20268969799999));
#199527=CARTESIAN_POINT('Ctrl Pts',(9.87017881199994,11.6,3.20268969799999));
#199528=CARTESIAN_POINT('Ctrl Pts',(9.87102171699994,15.2,3.20304833099998));
#199529=CARTESIAN_POINT('Ctrl Pts',(9.87102171699994,11.6,3.20304833099998));
#199530=CARTESIAN_POINT('Ctrl Pts',(9.87187791599995,15.2,3.20341363599999));
#199531=CARTESIAN_POINT('Ctrl Pts',(9.87187791599995,11.6,3.20341363599999));
#199532=CARTESIAN_POINT('Ctrl Pts',(9.87274249599994,15.2,3.20378354299999));
#199533=CARTESIAN_POINT('Ctrl Pts',(9.87274249599994,11.6,3.20378354299999));
#199534=CARTESIAN_POINT('Ctrl Pts',(9.87361542499994,15.2,3.20415805699999));
#199535=CARTESIAN_POINT('Ctrl Pts',(9.87361542499994,11.6,3.20415805699999));
#199536=CARTESIAN_POINT('Ctrl Pts',(9.87449666999994,15.2,3.20453718399998));
#199537=CARTESIAN_POINT('Ctrl Pts',(9.87449666999994,11.6,3.20453718399998));
#199538=CARTESIAN_POINT('Ctrl Pts',(9.87538619999994,15.2,3.20492093099999));
#199539=CARTESIAN_POINT('Ctrl Pts',(9.87538619999994,11.6,3.20492093099999));
#199540=CARTESIAN_POINT('Ctrl Pts',(9.87628398399995,15.2,3.20530930299999));
#199541=CARTESIAN_POINT('Ctrl Pts',(9.87628398399995,11.6,3.20530930299999));
#199542=CARTESIAN_POINT('Ctrl Pts',(9.87718998999994,15.2,3.20570230499998));
#199543=CARTESIAN_POINT('Ctrl Pts',(9.87718998999994,11.6,3.20570230499998));
#199544=CARTESIAN_POINT('Ctrl Pts',(9.87810418799994,15.2,3.20609994499998));
#199545=CARTESIAN_POINT('Ctrl Pts',(9.87810418799994,11.6,3.20609994499998));
#199546=CARTESIAN_POINT('Ctrl Pts',(9.87902654599995,15.2,3.20650222699999));
#199547=CARTESIAN_POINT('Ctrl Pts',(9.87902654599995,11.6,3.20650222699999));
#199548=CARTESIAN_POINT('Ctrl Pts',(9.87995703199994,15.2,3.20690915799998));
#199549=CARTESIAN_POINT('Ctrl Pts',(9.87995703199994,11.6,3.20690915799998));
#199550=CARTESIAN_POINT('Ctrl Pts',(9.88089561699995,15.2,3.20732074399999));
#199551=CARTESIAN_POINT('Ctrl Pts',(9.88089561699995,11.6,3.20732074399999));
#199552=CARTESIAN_POINT('Ctrl Pts',(9.88184226899994,15.2,3.20773698999999));
#199553=CARTESIAN_POINT('Ctrl Pts',(9.88184226899994,11.6,3.20773698999999));
#199554=CARTESIAN_POINT('Ctrl Pts',(9.88279695999994,15.2,3.20815789999998));
#199555=CARTESIAN_POINT('Ctrl Pts',(9.88279695999994,11.6,3.20815789999998));
#199556=CARTESIAN_POINT('Ctrl Pts',(9.88375965599994,15.2,3.20858348199998));
#199557=CARTESIAN_POINT('Ctrl Pts',(9.88375965599994,11.6,3.20858348199998));
#199558=CARTESIAN_POINT('Ctrl Pts',(9.88473033099995,15.2,3.20901374099999));
#199559=CARTESIAN_POINT('Ctrl Pts',(9.88473033099995,11.6,3.20901374099999));
#199560=CARTESIAN_POINT('Ctrl Pts',(9.88570895099994,15.2,3.20944868299998));
#199561=CARTESIAN_POINT('Ctrl Pts',(9.88570895099994,11.6,3.20944868299998));
#199562=CARTESIAN_POINT('Ctrl Pts',(9.88669548799994,15.2,3.20988831199998));
#199563=CARTESIAN_POINT('Ctrl Pts',(9.88669548799994,11.6,3.20988831199998));
#199564=CARTESIAN_POINT('Ctrl Pts',(9.88768991199995,15.2,3.21033263399999));
#199565=CARTESIAN_POINT('Ctrl Pts',(9.88768991199995,11.6,3.21033263399999));
#199566=CARTESIAN_POINT('Ctrl Pts',(9.88869219599994,15.2,3.21078165399998));
#199567=CARTESIAN_POINT('Ctrl Pts',(9.88869219599994,11.6,3.21078165399998));
#199568=CARTESIAN_POINT('Ctrl Pts',(9.88970230599995,15.2,3.21123537899999));
#199569=CARTESIAN_POINT('Ctrl Pts',(9.88970230599995,11.6,3.21123537899999));
#199570=CARTESIAN_POINT('Ctrl Pts',(9.89072021399994,15.2,3.21169381299999));
#199571=CARTESIAN_POINT('Ctrl Pts',(9.89072021399994,11.6,3.21169381299998));
#199572=CARTESIAN_POINT('Ctrl Pts',(9.89174589299994,15.2,3.21215696299999));
#199573=CARTESIAN_POINT('Ctrl Pts',(9.89174589299994,11.6,3.21215696299999));
#199574=CARTESIAN_POINT('Ctrl Pts',(9.89277931199994,15.2,3.21262483099999));
#199575=CARTESIAN_POINT('Ctrl Pts',(9.89277931199994,11.6,3.21262483099999));
#199576=CARTESIAN_POINT('Ctrl Pts',(9.89382044199995,15.2,3.21309742499999));
#199577=CARTESIAN_POINT('Ctrl Pts',(9.89382044199995,11.6,3.21309742499999));
#199578=CARTESIAN_POINT('Ctrl Pts',(9.89486925599994,15.2,3.21357474899998));
#199579=CARTESIAN_POINT('Ctrl Pts',(9.89486925599994,11.6,3.21357474899998));
#199580=CARTESIAN_POINT('Ctrl Pts',(9.89592572299994,15.2,3.21405680799998));
#199581=CARTESIAN_POINT('Ctrl Pts',(9.89592572299994,11.6,3.21405680799998));
#199582=CARTESIAN_POINT('Ctrl Pts',(9.89698981699994,15.2,3.21454360699998));
#199583=CARTESIAN_POINT('Ctrl Pts',(9.89698981699994,11.6,3.21454360699998));
#199584=CARTESIAN_POINT('Ctrl Pts',(9.89806150699994,15.2,3.21503515299998));
#199585=CARTESIAN_POINT('Ctrl Pts',(9.89806150699994,11.6,3.21503515299998));
#199586=CARTESIAN_POINT('Ctrl Pts',(9.89914076599995,15.2,3.21553144899998));
#199587=CARTESIAN_POINT('Ctrl Pts',(9.89914076599995,11.6,3.21553144899998));
#199588=CARTESIAN_POINT('Ctrl Pts',(9.90022756499994,15.2,3.21603250099999));
#199589=CARTESIAN_POINT('Ctrl Pts',(9.90022756499994,11.6,3.21603250099999));
#199590=CARTESIAN_POINT('Ctrl Pts',(9.90132187699994,15.2,3.21653831299999));
#199591=CARTESIAN_POINT('Ctrl Pts',(9.90132187699994,11.6,3.21653831299999));
#199592=CARTESIAN_POINT('Ctrl Pts',(9.90242367499994,15.2,3.21704888999999));
#199593=CARTESIAN_POINT('Ctrl Pts',(9.90242367499994,11.6,3.21704888999999));
#199594=CARTESIAN_POINT('Ctrl Pts',(9.90353292899995,15.2,3.21756423799999));
#199595=CARTESIAN_POINT('Ctrl Pts',(9.90353292899995,11.6,3.21756423799999));
#199596=CARTESIAN_POINT('Ctrl Pts',(9.90464961299995,15.2,3.21808436099998));
#199597=CARTESIAN_POINT('Ctrl Pts',(9.90464961299995,11.6,3.21808436099998));
#199598=CARTESIAN_POINT('Ctrl Pts',(9.90577369799994,15.2,3.21860926399999));
#199599=CARTESIAN_POINT('Ctrl Pts',(9.90577369799994,11.6,3.21860926399999));
#199600=CARTESIAN_POINT('Ctrl Pts',(9.90690515799994,15.2,3.21913895099998));
#199601=CARTESIAN_POINT('Ctrl Pts',(9.90690515799994,11.6,3.21913895099998));
#199602=CARTESIAN_POINT('Ctrl Pts',(9.90804396399995,15.2,3.21967342899999));
#199603=CARTESIAN_POINT('Ctrl Pts',(9.90804396399995,11.6,3.21967342899998));
#199604=CARTESIAN_POINT('Ctrl Pts',(9.90919009099994,15.2,3.22021269999999));
#199605=CARTESIAN_POINT('Ctrl Pts',(9.90919009099994,11.6,3.22021269999999));
#199606=CARTESIAN_POINT('Ctrl Pts',(9.91034350999995,15.2,3.22075676899999));
#199607=CARTESIAN_POINT('Ctrl Pts',(9.91034350999995,11.6,3.22075676899999));
#199608=CARTESIAN_POINT('Ctrl Pts',(9.91150419599995,15.2,3.22130564299999));
#199609=CARTESIAN_POINT('Ctrl Pts',(9.91150419599995,11.6,3.22130564299999));
#199610=CARTESIAN_POINT('Ctrl Pts',(9.91267211999994,15.2,3.22185932499998));
#199611=CARTESIAN_POINT('Ctrl Pts',(9.91267211999994,11.6,3.22185932499998));
#199612=CARTESIAN_POINT('Ctrl Pts',(9.91384725799995,15.2,3.22241781899999));
#199613=CARTESIAN_POINT('Ctrl Pts',(9.91384725799995,11.6,3.22241781899999));
#199614=CARTESIAN_POINT('Ctrl Pts',(9.91502957999994,15.2,3.22298113099999));
#199615=CARTESIAN_POINT('Ctrl Pts',(9.91502957999994,11.6,3.22298113099999));
#199616=CARTESIAN_POINT('Ctrl Pts',(9.91621906199994,15.2,3.22354926399999));
#199617=CARTESIAN_POINT('Ctrl Pts',(9.91621906199994,11.6,3.22354926399999));
#199618=CARTESIAN_POINT('Ctrl Pts',(9.91741567699994,15.2,3.22412222299998));
#199619=CARTESIAN_POINT('Ctrl Pts',(9.91741567699994,11.6,3.22412222299998));
#199620=CARTESIAN_POINT('Ctrl Pts',(9.91861939899995,15.2,3.22470001299998));
#199621=CARTESIAN_POINT('Ctrl Pts',(9.91861939899995,11.6,3.22470001299998));
#199622=CARTESIAN_POINT('Ctrl Pts',(9.91983020199994,15.2,3.22528263799998));
#199623=CARTESIAN_POINT('Ctrl Pts',(9.91983020199994,11.6,3.22528263799998));
#199624=CARTESIAN_POINT('Ctrl Pts',(9.92104805799995,15.2,3.22587010299999));
#199625=CARTESIAN_POINT('Ctrl Pts',(9.92104805799995,11.6,3.22587010299999));
#199626=CARTESIAN_POINT('Ctrl Pts',(9.92227294399994,15.2,3.22646241099999));
#199627=CARTESIAN_POINT('Ctrl Pts',(9.92227294399994,11.6,3.22646241099999));
#199628=CARTESIAN_POINT('Ctrl Pts',(9.92350483199995,15.2,3.22705956599999));
#199629=CARTESIAN_POINT('Ctrl Pts',(9.92350483199995,11.6,3.22705956599999));
#199630=CARTESIAN_POINT('Ctrl Pts',(9.92474369699995,15.2,3.22766157499998));
#199631=CARTESIAN_POINT('Ctrl Pts',(9.92474369699995,11.6,3.22766157499998));
#199632=CARTESIAN_POINT('Ctrl Pts',(9.92598951399994,15.2,3.22826843999999));
#199633=CARTESIAN_POINT('Ctrl Pts',(9.92598951399994,11.6,3.22826843999999));
#199634=CARTESIAN_POINT('Ctrl Pts',(9.92724225599994,15.2,3.22888016499999));
#199635=CARTESIAN_POINT('Ctrl Pts',(9.92724225599994,11.6,3.22888016499998));
#199636=CARTESIAN_POINT('Ctrl Pts',(9.92850189999994,15.2,3.22949675599999));
#199637=CARTESIAN_POINT('Ctrl Pts',(9.92850189999994,11.6,3.22949675599998));
#199638=CARTESIAN_POINT('Ctrl Pts',(9.92976841899995,15.2,3.23011821499998));
#199639=CARTESIAN_POINT('Ctrl Pts',(9.92976841899995,11.6,3.23011821499998));
#199640=CARTESIAN_POINT('Ctrl Pts',(9.93104178699994,15.2,3.23074454899999));
#199641=CARTESIAN_POINT('Ctrl Pts',(9.93104178699994,11.6,3.23074454899999));
#199642=CARTESIAN_POINT('Ctrl Pts',(9.93232198099994,15.2,3.23137575799999));
#199643=CARTESIAN_POINT('Ctrl Pts',(9.93232198099994,11.6,3.23137575799999));
#199644=CARTESIAN_POINT('Ctrl Pts',(9.93360897499995,15.2,3.23201184999999));
#199645=CARTESIAN_POINT('Ctrl Pts',(9.93360897499995,11.6,3.23201184999998));
#199646=CARTESIAN_POINT('Ctrl Pts',(9.93490274399995,15.2,3.23265282699998));
#199647=CARTESIAN_POINT('Ctrl Pts',(9.93490274399995,11.6,3.23265282699998));
#199648=CARTESIAN_POINT('Ctrl Pts',(9.93620326399995,15.2,3.23329869199998));
#199649=CARTESIAN_POINT('Ctrl Pts',(9.93620326399995,11.6,3.23329869199998));
#199650=CARTESIAN_POINT('Ctrl Pts',(9.93751050999995,15.2,3.23394945199999));
#199651=CARTESIAN_POINT('Ctrl Pts',(9.93751050999995,11.6,3.23394945199999));
#199652=CARTESIAN_POINT('Ctrl Pts',(9.93882445599995,15.2,3.23460510899999));
#199653=CARTESIAN_POINT('Ctrl Pts',(9.93882445599995,11.6,3.23460510899999));
#199654=CARTESIAN_POINT('Ctrl Pts',(9.94014507999994,15.2,3.23526566699999));
#199655=CARTESIAN_POINT('Ctrl Pts',(9.94014507999994,11.6,3.23526566699999));
#199656=CARTESIAN_POINT('Ctrl Pts',(9.94147235499995,15.2,3.23593112999998));
#199657=CARTESIAN_POINT('Ctrl Pts',(9.94147235499995,11.6,3.23593112999998));
#199658=CARTESIAN_POINT('Ctrl Pts',(9.94280625999994,15.2,3.23660150199998));
#199659=CARTESIAN_POINT('Ctrl Pts',(9.94280625999994,11.6,3.23660150199998));
#199660=CARTESIAN_POINT('Ctrl Pts',(9.94414676699994,15.2,3.23727678699999));
#199661=CARTESIAN_POINT('Ctrl Pts',(9.94414676699994,11.6,3.23727678699999));
#199662=CARTESIAN_POINT('Ctrl Pts',(9.94549385499995,15.2,3.23795698799999));
#199663=CARTESIAN_POINT('Ctrl Pts',(9.94549385499995,11.6,3.23795698799999));
#199664=CARTESIAN_POINT('Ctrl Pts',(9.94684749899994,15.2,3.23864210899998));
#199665=CARTESIAN_POINT('Ctrl Pts',(9.94684749899994,11.6,3.23864210899998));
#199666=CARTESIAN_POINT('Ctrl Pts',(9.94820767499995,15.2,3.23933215499999));
#199667=CARTESIAN_POINT('Ctrl Pts',(9.94820767499995,11.6,3.23933215499998));
#199668=CARTESIAN_POINT('Ctrl Pts',(9.94957435799994,15.2,3.24002712799999));
#199669=CARTESIAN_POINT('Ctrl Pts',(9.94957435799994,11.6,3.24002712799999));
#199670=CARTESIAN_POINT('Ctrl Pts',(9.95094752599995,15.2,3.24072703399998));
#199671=CARTESIAN_POINT('Ctrl Pts',(9.95094752599995,11.6,3.24072703399998));
#199672=CARTESIAN_POINT('Ctrl Pts',(9.95232715499995,15.2,3.24143187399999));
#199673=CARTESIAN_POINT('Ctrl Pts',(9.95232715499995,11.6,3.24143187399999));
#199674=CARTESIAN_POINT('Ctrl Pts',(9.95371322099994,15.2,3.24214165199999));
#199675=CARTESIAN_POINT('Ctrl Pts',(9.95371322099994,11.6,3.24214165199999));
#199676=CARTESIAN_POINT('Ctrl Pts',(9.95510570199994,15.2,3.24285637299998));
#199677=CARTESIAN_POINT('Ctrl Pts',(9.95510570199994,11.6,3.24285637299998));
#199678=CARTESIAN_POINT('Ctrl Pts',(9.95650457299995,15.2,3.24357603999999));
#199679=CARTESIAN_POINT('Ctrl Pts',(9.95650457299995,11.6,3.24357603999999));
#199680=CARTESIAN_POINT('Ctrl Pts',(9.95790981099995,15.2,3.24430065599999));
#199681=CARTESIAN_POINT('Ctrl Pts',(9.95790981099995,11.6,3.24430065599999));
#199682=CARTESIAN_POINT('Ctrl Pts',(9.95932139299994,15.2,3.24503022499999));
#199683=CARTESIAN_POINT('Ctrl Pts',(9.95932139299994,11.6,3.24503022499999));
#199684=CARTESIAN_POINT('Ctrl Pts',(9.96073929699994,15.2,3.24576475099998));
#199685=CARTESIAN_POINT('Ctrl Pts',(9.96073929699994,11.6,3.24576475099998));
#199686=CARTESIAN_POINT('Ctrl Pts',(9.96216349899995,15.2,3.24650423599999));
#199687=CARTESIAN_POINT('Ctrl Pts',(9.96216349899995,11.6,3.24650423599999));
#199688=CARTESIAN_POINT('Ctrl Pts',(9.96359397499995,15.2,3.24724868599999));
#199689=CARTESIAN_POINT('Ctrl Pts',(9.96359397499995,11.6,3.24724868599999));
#199690=CARTESIAN_POINT('Ctrl Pts',(9.96503070399994,15.2,3.24799810099999));
#199691=CARTESIAN_POINT('Ctrl Pts',(9.96503070399994,11.6,3.24799810099999));
#199692=CARTESIAN_POINT('Ctrl Pts',(9.96647366299995,15.2,3.24875248699998));
#199693=CARTESIAN_POINT('Ctrl Pts',(9.96647366299995,11.6,3.24875248699998));
#199694=CARTESIAN_POINT('Ctrl Pts',(9.96792282999994,15.2,3.24951184599998));
#199695=CARTESIAN_POINT('Ctrl Pts',(9.96792282999994,11.6,3.24951184599998));
#199696=CARTESIAN_POINT('Ctrl Pts',(9.96937817999994,15.2,3.25027618299998));
#199697=CARTESIAN_POINT('Ctrl Pts',(9.96937817999994,11.6,3.25027618299998));
#199698=CARTESIAN_POINT('Ctrl Pts',(9.97083969299995,15.2,3.25104549899999));
#199699=CARTESIAN_POINT('Ctrl Pts',(9.97083969299995,11.6,3.25104549899999));
#199700=CARTESIAN_POINT('Ctrl Pts',(9.97230734499994,15.2,3.25181979899998));
#199701=CARTESIAN_POINT('Ctrl Pts',(9.97230734499994,11.6,3.25181979899998));
#199702=CARTESIAN_POINT('Ctrl Pts',(9.97378111499994,15.2,3.25259908499999));
#199703=CARTESIAN_POINT('Ctrl Pts',(9.97378111499994,11.6,3.25259908499999));
#199704=CARTESIAN_POINT('Ctrl Pts',(9.97526097999994,15.2,3.25338336199999));
#199705=CARTESIAN_POINT('Ctrl Pts',(9.97526097999994,11.6,3.25338336199999));
#199706=CARTESIAN_POINT('Ctrl Pts',(9.97674691799994,15.2,3.25417263099999));
#199707=CARTESIAN_POINT('Ctrl Pts',(9.97674691799994,11.6,3.25417263099998));
#199708=CARTESIAN_POINT('Ctrl Pts',(9.97823890599994,15.2,3.25496689699998));
#199709=CARTESIAN_POINT('Ctrl Pts',(9.97823890599994,11.6,3.25496689699998));
#199710=CARTESIAN_POINT('Ctrl Pts',(9.97973692499994,15.2,3.25576616199999));
#199711=CARTESIAN_POINT('Ctrl Pts',(9.97973692499994,11.6,3.25576616199999));
#199712=CARTESIAN_POINT('Ctrl Pts',(9.98124094999995,15.2,3.25657042999998));
#199713=CARTESIAN_POINT('Ctrl Pts',(9.98124094999995,11.6,3.25657042999998));
#199714=CARTESIAN_POINT('Ctrl Pts',(9.98275095899994,15.2,3.25737970399998));
#199715=CARTESIAN_POINT('Ctrl Pts',(9.98275095899994,11.6,3.25737970399998));
#199716=CARTESIAN_POINT('Ctrl Pts',(9.98426693399994,15.2,3.25819398599998));
#199717=CARTESIAN_POINT('Ctrl Pts',(9.98426693399994,11.6,3.25819398599998));
#199718=CARTESIAN_POINT('Ctrl Pts',(9.98578884999995,15.2,3.25901328099999));
#199719=CARTESIAN_POINT('Ctrl Pts',(9.98578884999995,11.6,3.25901328099999));
#199720=CARTESIAN_POINT('Ctrl Pts',(9.98731668699994,15.2,3.25983759099999));
#199721=CARTESIAN_POINT('Ctrl Pts',(9.98731668699994,11.6,3.25983759099999));
#199722=CARTESIAN_POINT('Ctrl Pts',(9.98885042199994,15.2,3.26066691799999));
#199723=CARTESIAN_POINT('Ctrl Pts',(9.98885042199994,11.6,3.26066691799999));
#199724=CARTESIAN_POINT('Ctrl Pts',(9.99039003499995,15.2,3.26150126599998));
#199725=CARTESIAN_POINT('Ctrl Pts',(9.99039003499995,11.6,3.26150126599998));
#199726=CARTESIAN_POINT('Ctrl Pts',(9.99193550399994,15.2,3.26234063799999));
#199727=CARTESIAN_POINT('Ctrl Pts',(9.99193550399994,11.6,3.26234063799998));
#199728=CARTESIAN_POINT('Ctrl Pts',(9.99348680799995,15.2,3.26318503599998));
#199729=CARTESIAN_POINT('Ctrl Pts',(9.99348680799995,11.6,3.26318503599998));
#199730=CARTESIAN_POINT('Ctrl Pts',(9.99504392599994,15.2,3.26403446499998));
#199731=CARTESIAN_POINT('Ctrl Pts',(9.99504392599994,11.6,3.26403446499998));
#199732=CARTESIAN_POINT('Ctrl Pts',(9.99660683599994,15.2,3.26488892599999));
#199733=CARTESIAN_POINT('Ctrl Pts',(9.99660683599994,11.6,3.26488892599999));
#199734=CARTESIAN_POINT('Ctrl Pts',(9.99817551899995,15.2,3.26574842299999));
#199735=CARTESIAN_POINT('Ctrl Pts',(9.99817551899995,11.6,3.26574842299999));
#199736=CARTESIAN_POINT('Ctrl Pts',(9.99974995099995,15.2,3.26661295799998));
#199737=CARTESIAN_POINT('Ctrl Pts',(9.99974995099995,11.6,3.26661295799998));
#199738=CARTESIAN_POINT('Ctrl Pts',(10.0013301129999,15.2,3.26748253399998));
#199739=CARTESIAN_POINT('Ctrl Pts',(10.0013301129999,11.6,3.26748253399998));
#199740=CARTESIAN_POINT('Ctrl Pts',(10.0029159849999,15.2,3.26835715499998));
#199741=CARTESIAN_POINT('Ctrl Pts',(10.0029159849999,11.6,3.26835715499998));
#199742=CARTESIAN_POINT('Ctrl Pts',(10.0045075449999,15.2,3.26923682199999));
#199743=CARTESIAN_POINT('Ctrl Pts',(10.0045075449999,11.6,3.26923682199999));
#199744=CARTESIAN_POINT('Ctrl Pts',(10.0061047719999,15.2,3.27012153799998));
#199745=CARTESIAN_POINT('Ctrl Pts',(10.0061047719999,11.6,3.27012153799998));
#199746=CARTESIAN_POINT('Ctrl Pts',(10.0077076459999,15.2,3.27101130699998));
#199747=CARTESIAN_POINT('Ctrl Pts',(10.0077076459999,11.6,3.27101130699998));
#199748=CARTESIAN_POINT('Ctrl Pts',(10.0093161469999,15.2,3.27190612999999));
#199749=CARTESIAN_POINT('Ctrl Pts',(10.0093161469999,11.6,3.27190612999999));
#199750=CARTESIAN_POINT('Ctrl Pts',(10.0109302539999,15.2,3.27280601199998));
#199751=CARTESIAN_POINT('Ctrl Pts',(10.0109302539999,11.6,3.27280601199998));
#199752=CARTESIAN_POINT('Ctrl Pts',(10.0125499459999,15.2,3.27371095399998));
#199753=CARTESIAN_POINT('Ctrl Pts',(10.0125499459999,11.6,3.27371095399998));
#199754=CARTESIAN_POINT('Ctrl Pts',(10.0141752039999,15.2,3.27462095899998));
#199755=CARTESIAN_POINT('Ctrl Pts',(10.0141752039999,11.6,3.27462095899998));
#199756=CARTESIAN_POINT('Ctrl Pts',(10.0158060069999,15.2,3.27553602899999));
#199757=CARTESIAN_POINT('Ctrl Pts',(10.0158060069999,11.6,3.27553602899999));
#199758=CARTESIAN_POINT('Ctrl Pts',(10.0174423339999,15.2,3.27645616799998));
#199759=CARTESIAN_POINT('Ctrl Pts',(10.0174423339999,11.6,3.27645616799998));
#199760=CARTESIAN_POINT('Ctrl Pts',(10.0190841679999,15.2,3.27738137699999));
#199761=CARTESIAN_POINT('Ctrl Pts',(10.0190841679999,11.6,3.27738137699999));
#199762=CARTESIAN_POINT('Ctrl Pts',(10.0207314849999,15.2,3.27831165999999));
#199763=CARTESIAN_POINT('Ctrl Pts',(10.0207314849999,11.6,3.27831165999999));
#199764=CARTESIAN_POINT('Ctrl Pts',(10.0223842669999,15.2,3.27924701899998));
#199765=CARTESIAN_POINT('Ctrl Pts',(10.0223842669999,11.6,3.27924701899998));
#199766=CARTESIAN_POINT('Ctrl Pts',(10.0240424949999,15.2,3.28018745599999));
#199767=CARTESIAN_POINT('Ctrl Pts',(10.0240424949999,11.6,3.28018745599999));
#199768=CARTESIAN_POINT('Ctrl Pts',(10.0257061469999,15.2,3.28113297399998));
#199769=CARTESIAN_POINT('Ctrl Pts',(10.0257061469999,11.6,3.28113297399998));
#199770=CARTESIAN_POINT('Ctrl Pts',(10.0273752059999,15.2,3.28208357499998));
#199771=CARTESIAN_POINT('Ctrl Pts',(10.0273752059999,11.6,3.28208357499998));
#199772=CARTESIAN_POINT('Ctrl Pts',(10.0290496499999,15.2,3.28303926299998));
#199773=CARTESIAN_POINT('Ctrl Pts',(10.0290496499999,11.6,3.28303926299998));
#199774=CARTESIAN_POINT('Ctrl Pts',(10.0307294589999,15.2,3.28400003799998));
#199775=CARTESIAN_POINT('Ctrl Pts',(10.0307294589999,11.6,3.28400003799998));
#199776=CARTESIAN_POINT('Ctrl Pts',(10.0324146159999,15.2,3.28496590599999));
#199777=CARTESIAN_POINT('Ctrl Pts',(10.0324146159999,11.6,3.28496590599999));
#199778=CARTESIAN_POINT('Ctrl Pts',(10.0341050999999,15.2,3.28593686499998));
#199779=CARTESIAN_POINT('Ctrl Pts',(10.0341050999999,11.6,3.28593686499998));
#199780=CARTESIAN_POINT('Ctrl Pts',(10.0358008909999,15.2,3.28691291999998));
#199781=CARTESIAN_POINT('Ctrl Pts',(10.0358008909999,11.6,3.28691291999998));
#199782=CARTESIAN_POINT('Ctrl Pts',(10.0375019699999,15.2,3.28789407399999));
#199783=CARTESIAN_POINT('Ctrl Pts',(10.0375019699999,11.6,3.28789407399999));
#199784=CARTESIAN_POINT('Ctrl Pts',(10.0392083189999,15.2,3.28888032699999));
#199785=CARTESIAN_POINT('Ctrl Pts',(10.0392083189999,11.6,3.28888032699999));
#199786=CARTESIAN_POINT('Ctrl Pts',(10.0409199179999,15.2,3.28987168299999));
#199787=CARTESIAN_POINT('Ctrl Pts',(10.0409199179999,11.6,3.28987168299999));
#199788=CARTESIAN_POINT('Ctrl Pts',(10.0426367469999,15.2,3.29086814299998));
#199789=CARTESIAN_POINT('Ctrl Pts',(10.0426367469999,11.6,3.29086814299998));
#199790=CARTESIAN_POINT('Ctrl Pts',(10.0443587869999,15.2,3.29186971099999));
#199791=CARTESIAN_POINT('Ctrl Pts',(10.0443587869999,11.6,3.29186971099999));
#199792=CARTESIAN_POINT('Ctrl Pts',(10.0460860199999,15.2,3.29287638799999));
#199793=CARTESIAN_POINT('Ctrl Pts',(10.0460860199999,11.6,3.29287638799999));
#199794=CARTESIAN_POINT('Ctrl Pts',(10.0478184259999,15.2,3.29388817699999));
#199795=CARTESIAN_POINT('Ctrl Pts',(10.0478184259999,11.6,3.29388817699999));
#199796=CARTESIAN_POINT('Ctrl Pts',(10.0495559859999,15.2,3.29490507899998));
#199797=CARTESIAN_POINT('Ctrl Pts',(10.0495559859999,11.6,3.29490507899998));
#199798=CARTESIAN_POINT('Ctrl Pts',(10.0512986829999,15.2,3.29592709799999));
#199799=CARTESIAN_POINT('Ctrl Pts',(10.0512986829999,11.6,3.29592709799999));
#199800=CARTESIAN_POINT('Ctrl Pts',(10.0530464969999,15.2,3.29695423399999));
#199801=CARTESIAN_POINT('Ctrl Pts',(10.0530464969999,11.6,3.29695423399999));
#199802=CARTESIAN_POINT('Ctrl Pts',(10.0547994079999,15.2,3.29798649099998));
#199803=CARTESIAN_POINT('Ctrl Pts',(10.0547994079999,11.6,3.29798649099998));
#199804=CARTESIAN_POINT('Ctrl Pts',(10.0565573989999,15.2,3.29902387099998));
#199805=CARTESIAN_POINT('Ctrl Pts',(10.0565573989999,11.6,3.29902387099998));
#199806=CARTESIAN_POINT('Ctrl Pts',(10.0583204519999,15.2,3.30006637499999));
#199807=CARTESIAN_POINT('Ctrl Pts',(10.0583204519999,11.6,3.30006637499999));
#199808=CARTESIAN_POINT('Ctrl Pts',(10.0600885459999,15.2,3.30111400599999));
#199809=CARTESIAN_POINT('Ctrl Pts',(10.0600885459999,11.6,3.30111400599999));
#199810=CARTESIAN_POINT('Ctrl Pts',(10.0618616649999,15.2,3.30216676499998));
#199811=CARTESIAN_POINT('Ctrl Pts',(10.0618616649999,11.6,3.30216676499998));
#199812=CARTESIAN_POINT('Ctrl Pts',(10.0636397889999,15.2,3.30322465599998));
#199813=CARTESIAN_POINT('Ctrl Pts',(10.0636397889999,11.6,3.30322465599998));
#199814=CARTESIAN_POINT('Ctrl Pts',(10.0654228989999,15.2,3.30428767999998));
#199815=CARTESIAN_POINT('Ctrl Pts',(10.0654228989999,11.6,3.30428767999998));
#199816=CARTESIAN_POINT('Ctrl Pts',(10.0672109789999,15.2,3.30535583799998));
#199817=CARTESIAN_POINT('Ctrl Pts',(10.0672109789999,11.6,3.30535583799998));
#199818=CARTESIAN_POINT('Ctrl Pts',(10.0690040089999,15.2,3.30642913399998));
#199819=CARTESIAN_POINT('Ctrl Pts',(10.0690040089999,11.6,3.30642913399998));
#199820=CARTESIAN_POINT('Ctrl Pts',(10.0708019709999,15.2,3.30750756799999));
#199821=CARTESIAN_POINT('Ctrl Pts',(10.0708019709999,11.6,3.30750756799999));
#199822=CARTESIAN_POINT('Ctrl Pts',(10.0726048469999,15.2,3.30859114399999));
#199823=CARTESIAN_POINT('Ctrl Pts',(10.0726048469999,11.6,3.30859114399999));
#199824=CARTESIAN_POINT('Ctrl Pts',(10.0744126189999,15.2,3.30967986199998));
#199825=CARTESIAN_POINT('Ctrl Pts',(10.0744126189999,11.6,3.30967986199998));
#199826=CARTESIAN_POINT('Ctrl Pts',(10.0762252689999,15.2,3.31077372499998));
#199827=CARTESIAN_POINT('Ctrl Pts',(10.0762252689999,11.6,3.31077372499998));
#199828=CARTESIAN_POINT('Ctrl Pts',(10.0780427799999,15.2,3.31187273499999));
#199829=CARTESIAN_POINT('Ctrl Pts',(10.0780427799999,11.6,3.31187273499999));
#199830=CARTESIAN_POINT('Ctrl Pts',(10.0798651319999,15.2,3.31297689299999));
#199831=CARTESIAN_POINT('Ctrl Pts',(10.0798651319999,11.6,3.31297689299999));
#199832=CARTESIAN_POINT('Ctrl Pts',(10.0816923089999,15.2,3.31408620199999));
#199833=CARTESIAN_POINT('Ctrl Pts',(10.0816923089999,11.6,3.31408620199999));
#199834=CARTESIAN_POINT('Ctrl Pts',(10.0835242919999,15.2,3.31520066399998));
#199835=CARTESIAN_POINT('Ctrl Pts',(10.0835242919999,11.6,3.31520066399998));
#199836=CARTESIAN_POINT('Ctrl Pts',(10.0853610639999,15.2,3.31632027999999));
#199837=CARTESIAN_POINT('Ctrl Pts',(10.0853610639999,11.6,3.31632027999999));
#199838=CARTESIAN_POINT('Ctrl Pts',(10.0872026069999,15.2,3.31744505199998));
#199839=CARTESIAN_POINT('Ctrl Pts',(10.0872026069999,11.6,3.31744505199998));
#199840=CARTESIAN_POINT('Ctrl Pts',(10.0890489029999,15.2,3.31857498099998));
#199841=CARTESIAN_POINT('Ctrl Pts',(10.0890489029999,11.6,3.31857498099998));
#199842=CARTESIAN_POINT('Ctrl Pts',(10.0908999359999,15.2,3.31971007099998));
#199843=CARTESIAN_POINT('Ctrl Pts',(10.0908999359999,11.6,3.31971007099998));
#199844=CARTESIAN_POINT('Ctrl Pts',(10.0927556859999,15.2,3.32085032099998));
#199845=CARTESIAN_POINT('Ctrl Pts',(10.0927556859999,11.6,3.32085032099998));
#199846=CARTESIAN_POINT('Ctrl Pts',(10.0946161369999,15.2,3.32199573599999));
#199847=CARTESIAN_POINT('Ctrl Pts',(10.0946161369999,11.6,3.32199573599999));
#199848=CARTESIAN_POINT('Ctrl Pts',(10.0964812719999,15.2,3.32314631499998));
#199849=CARTESIAN_POINT('Ctrl Pts',(10.0964812719999,11.6,3.32314631499998));
#199850=CARTESIAN_POINT('Ctrl Pts',(10.0983510719999,15.2,3.32430206099998));
#199851=CARTESIAN_POINT('Ctrl Pts',(10.0983510719999,11.6,3.32430206099998));
#199852=CARTESIAN_POINT('Ctrl Pts',(10.1002255209999,15.2,3.32546297599999));
#199853=CARTESIAN_POINT('Ctrl Pts',(10.1002255209999,11.6,3.32546297599999));
#199854=CARTESIAN_POINT('Ctrl Pts',(10.1021046009999,15.2,3.32662905999998));
#199855=CARTESIAN_POINT('Ctrl Pts',(10.1021046009999,11.6,3.32662905999998));
#199856=CARTESIAN_POINT('Ctrl Pts',(10.1039882969999,15.2,3.32780031599999));
#199857=CARTESIAN_POINT('Ctrl Pts',(10.1039882969999,11.6,3.32780031599999));
#199858=CARTESIAN_POINT('Ctrl Pts',(10.1058765879999,15.2,3.32897674599998));
#199859=CARTESIAN_POINT('Ctrl Pts',(10.1058765879999,11.6,3.32897674599998));
#199860=CARTESIAN_POINT('Ctrl Pts',(10.1077694589999,15.2,3.33015835099999));
#199861=CARTESIAN_POINT('Ctrl Pts',(10.1077694589999,11.6,3.33015835099999));
#199862=CARTESIAN_POINT('Ctrl Pts',(10.1096668939999,15.2,3.33134513399998));
#199863=CARTESIAN_POINT('Ctrl Pts',(10.1096668939999,11.6,3.33134513399998));
#199864=CARTESIAN_POINT('Ctrl Pts',(10.1115688739999,15.2,3.33253709299999));
#199865=CARTESIAN_POINT('Ctrl Pts',(10.1115688739999,11.6,3.33253709299999));
#199866=CARTESIAN_POINT('Ctrl Pts',(10.1134753829999,15.2,3.33373423299999));
#199867=CARTESIAN_POINT('Ctrl Pts',(10.1134753829999,11.6,3.33373423299999));
#199868=CARTESIAN_POINT('Ctrl Pts',(10.1153864039999,15.2,3.33493655599998));
#199869=CARTESIAN_POINT('Ctrl Pts',(10.1153864039999,11.6,3.33493655599998));
#199870=CARTESIAN_POINT('Ctrl Pts',(10.1173019199999,15.2,3.33614405999998));
#199871=CARTESIAN_POINT('Ctrl Pts',(10.1173019199999,11.6,3.33614405999998));
#199872=CARTESIAN_POINT('Ctrl Pts',(10.1192219139999,15.2,3.33735674999998));
#199873=CARTESIAN_POINT('Ctrl Pts',(10.1192219139999,11.6,3.33735674999998));
#199874=CARTESIAN_POINT('Ctrl Pts',(10.1211463699999,15.2,3.33857462599998));
#199875=CARTESIAN_POINT('Ctrl Pts',(10.1211463699999,11.6,3.33857462599998));
#199876=CARTESIAN_POINT('Ctrl Pts',(10.1230752719999,15.2,3.33979768899999));
#199877=CARTESIAN_POINT('Ctrl Pts',(10.1230752719999,11.6,3.33979768899999));
#199878=CARTESIAN_POINT('Ctrl Pts',(10.1250086009999,15.2,3.34102594199998));
#199879=CARTESIAN_POINT('Ctrl Pts',(10.1250086009999,11.6,3.34102594199998));
#199880=CARTESIAN_POINT('Ctrl Pts',(10.1269463409999,15.2,3.34225938499999));
#199881=CARTESIAN_POINT('Ctrl Pts',(10.1269463409999,11.6,3.34225938499999));
#199882=CARTESIAN_POINT('Ctrl Pts',(10.1288884769999,15.2,3.34349802099998));
#199883=CARTESIAN_POINT('Ctrl Pts',(10.1288884769999,11.6,3.34349802099998));
#199884=CARTESIAN_POINT('Ctrl Pts',(10.1308349909999,15.2,3.34474184999999));
#199885=CARTESIAN_POINT('Ctrl Pts',(10.1308349909999,11.6,3.34474184999999));
#199886=CARTESIAN_POINT('Ctrl Pts',(10.1327858669999,15.2,3.34599087499999));
#199887=CARTESIAN_POINT('Ctrl Pts',(10.1327858669999,11.6,3.34599087499999));
#199888=CARTESIAN_POINT('Ctrl Pts',(10.1347410889999,15.2,3.34724509499999));
#199889=CARTESIAN_POINT('Ctrl Pts',(10.1347410889999,11.6,3.34724509499999));
#199890=CARTESIAN_POINT('Ctrl Pts',(10.1367006399999,15.2,3.34850451399999));
#199891=CARTESIAN_POINT('Ctrl Pts',(10.1367006399999,11.6,3.34850451399999));
#199892=CARTESIAN_POINT('Ctrl Pts',(10.1386645039999,15.2,3.34976913299998));
#199893=CARTESIAN_POINT('Ctrl Pts',(10.1386645039999,11.6,3.34976913299998));
#199894=CARTESIAN_POINT('Ctrl Pts',(10.1406326639999,15.2,3.35103894999998));
#199895=CARTESIAN_POINT('Ctrl Pts',(10.1406326639999,11.6,3.35103894999998));
#199896=CARTESIAN_POINT('Ctrl Pts',(10.1426051049999,15.2,3.35231397199999));
#199897=CARTESIAN_POINT('Ctrl Pts',(10.1426051049999,11.6,3.35231397199998));
#199898=CARTESIAN_POINT('Ctrl Pts',(10.1445818109999,15.2,3.35359419599998));
#199899=CARTESIAN_POINT('Ctrl Pts',(10.1445818109999,11.6,3.35359419599998));
#199900=CARTESIAN_POINT('Ctrl Pts',(10.1465627639999,15.2,3.35487962499998));
#199901=CARTESIAN_POINT('Ctrl Pts',(10.1465627639999,11.6,3.35487962499998));
#199902=CARTESIAN_POINT('Ctrl Pts',(10.1485479489999,15.2,3.35617025999999));
#199903=CARTESIAN_POINT('Ctrl Pts',(10.1485479489999,11.6,3.35617025999999));
#199904=CARTESIAN_POINT('Ctrl Pts',(10.1505373509999,15.2,3.35746610199998));
#199905=CARTESIAN_POINT('Ctrl Pts',(10.1505373509999,11.6,3.35746610199998));
#199906=CARTESIAN_POINT('Ctrl Pts',(10.1525309519999,15.2,3.35876715399999));
#199907=CARTESIAN_POINT('Ctrl Pts',(10.1525309519999,11.6,3.35876715399999));
#199908=CARTESIAN_POINT('Ctrl Pts',(10.1545287359999,15.2,3.36007341499998));
#199909=CARTESIAN_POINT('Ctrl Pts',(10.1545287359999,11.6,3.36007341499998));
#199910=CARTESIAN_POINT('Ctrl Pts',(10.1565306899999,15.2,3.36138488699999));
#199911=CARTESIAN_POINT('Ctrl Pts',(10.1565306899999,11.6,3.36138488699999));
#199912=CARTESIAN_POINT('Ctrl Pts',(10.1585367949999,15.2,3.36270157099998));
#199913=CARTESIAN_POINT('Ctrl Pts',(10.1585367949999,11.6,3.36270157099998));
#199914=CARTESIAN_POINT('Ctrl Pts',(10.1605470379999,15.2,3.36402346999999));
#199915=CARTESIAN_POINT('Ctrl Pts',(10.1605470379999,11.6,3.36402346999999));
#199916=CARTESIAN_POINT('Ctrl Pts',(10.1625613999999,15.2,3.36535058299999));
#199917=CARTESIAN_POINT('Ctrl Pts',(10.1625613999999,11.6,3.36535058299999));
#199918=CARTESIAN_POINT('Ctrl Pts',(10.1645798679999,15.2,3.36668291199998));
#199919=CARTESIAN_POINT('Ctrl Pts',(10.1645798679999,11.6,3.36668291199998));
#199920=CARTESIAN_POINT('Ctrl Pts',(10.1666024249999,15.2,3.36802045899999));
#199921=CARTESIAN_POINT('Ctrl Pts',(10.1666024249999,11.6,3.36802045899999));
#199922=CARTESIAN_POINT('Ctrl Pts',(10.1686290549999,15.2,3.36936322399998));
#199923=CARTESIAN_POINT('Ctrl Pts',(10.1686290549999,11.6,3.36936322399998));
#199924=CARTESIAN_POINT('Ctrl Pts',(10.1706597439999,15.2,3.37071120799998));
#199925=CARTESIAN_POINT('Ctrl Pts',(10.1706597439999,11.6,3.37071120799998));
#199926=CARTESIAN_POINT('Ctrl Pts',(10.1726944739999,15.2,3.37206441399999));
#199927=CARTESIAN_POINT('Ctrl Pts',(10.1726944739999,11.6,3.37206441399999));
#199928=CARTESIAN_POINT('Ctrl Pts',(10.1747332319999,15.2,3.37342283999998));
#199929=CARTESIAN_POINT('Ctrl Pts',(10.1747332319999,11.6,3.37342283999998));
#199930=CARTESIAN_POINT('Ctrl Pts',(10.1767759999999,15.2,3.37478648999999));
#199931=CARTESIAN_POINT('Ctrl Pts',(10.1767759999999,11.6,3.37478648999999));
#199932=CARTESIAN_POINT('Ctrl Pts',(10.1788227659999,15.2,3.37615536499998));
#199933=CARTESIAN_POINT('Ctrl Pts',(10.1788227659999,11.6,3.37615536499998));
#199934=CARTESIAN_POINT('Ctrl Pts',(10.1808735109999,15.2,3.37752946399998));
#199935=CARTESIAN_POINT('Ctrl Pts',(10.1808735109999,11.6,3.37752946399998));
#199936=CARTESIAN_POINT('Ctrl Pts',(10.1829282219999,15.2,3.37890878899999));
#199937=CARTESIAN_POINT('Ctrl Pts',(10.1829282219999,11.6,3.37890878899999));
#199938=CARTESIAN_POINT('Ctrl Pts',(10.1849868839999,15.2,3.38029334299998));
#199939=CARTESIAN_POINT('Ctrl Pts',(10.1849868839999,11.6,3.38029334299998));
#199940=CARTESIAN_POINT('Ctrl Pts',(10.1870494789999,15.2,3.38168312399999));
#199941=CARTESIAN_POINT('Ctrl Pts',(10.1870494789999,11.6,3.38168312399999));
#199942=CARTESIAN_POINT('Ctrl Pts',(10.1891159949999,15.2,3.38307813399998));
#199943=CARTESIAN_POINT('Ctrl Pts',(10.1891159949999,11.6,3.38307813399998));
#199944=CARTESIAN_POINT('Ctrl Pts',(10.1911864149999,15.2,3.38447837499999));
#199945=CARTESIAN_POINT('Ctrl Pts',(10.1911864149999,11.6,3.38447837499999));
#199946=CARTESIAN_POINT('Ctrl Pts',(10.1932607229999,15.2,3.38588384799999));
#199947=CARTESIAN_POINT('Ctrl Pts',(10.1932607229999,11.6,3.38588384799999));
#199948=CARTESIAN_POINT('Ctrl Pts',(10.1953389059999,15.2,3.38729455299998));
#199949=CARTESIAN_POINT('Ctrl Pts',(10.1953389059999,11.6,3.38729455299998));
#199950=CARTESIAN_POINT('Ctrl Pts',(10.1974209479999,15.2,3.38871049099998));
#199951=CARTESIAN_POINT('Ctrl Pts',(10.1974209479999,11.6,3.38871049099998));
#199952=CARTESIAN_POINT('Ctrl Pts',(10.1995068349999,15.2,3.39013166499999));
#199953=CARTESIAN_POINT('Ctrl Pts',(10.1995068349999,11.6,3.39013166499999));
#199954=CARTESIAN_POINT('Ctrl Pts',(10.2015965499999,15.2,3.39155807199998));
#199955=CARTESIAN_POINT('Ctrl Pts',(10.2015965499999,11.6,3.39155807199998));
#199956=CARTESIAN_POINT('Ctrl Pts',(10.2036900789999,15.2,3.39298971699999));
#199957=CARTESIAN_POINT('Ctrl Pts',(10.2036900789999,11.6,3.39298971699999));
#199958=CARTESIAN_POINT('Ctrl Pts',(10.2057874069999,15.2,3.39442659799998));
#199959=CARTESIAN_POINT('Ctrl Pts',(10.2057874069999,11.6,3.39442659799998));
#199960=CARTESIAN_POINT('Ctrl Pts',(10.2078885199999,15.2,3.39586871799998));
#199961=CARTESIAN_POINT('Ctrl Pts',(10.2078885199999,11.6,3.39586871799998));
#199962=CARTESIAN_POINT('Ctrl Pts',(10.2099934029999,15.2,3.39731607599998));
#199963=CARTESIAN_POINT('Ctrl Pts',(10.2099934029999,11.6,3.39731607599998));
#199964=CARTESIAN_POINT('Ctrl Pts',(10.2121020399999,15.2,3.39876867499999));
#199965=CARTESIAN_POINT('Ctrl Pts',(10.2121020399999,11.6,3.39876867499999));
#199966=CARTESIAN_POINT('Ctrl Pts',(10.2142144169999,15.2,3.40022651399998));
#199967=CARTESIAN_POINT('Ctrl Pts',(10.2142144169999,11.6,3.40022651399998));
#199968=CARTESIAN_POINT('Ctrl Pts',(10.2163305199999,15.2,3.40168959499999));
#199969=CARTESIAN_POINT('Ctrl Pts',(10.2163305199999,11.6,3.40168959499999));
#199970=CARTESIAN_POINT('Ctrl Pts',(10.2184503329999,15.2,3.40315791799998));
#199971=CARTESIAN_POINT('Ctrl Pts',(10.2184503329999,11.6,3.40315791799998));
#199972=CARTESIAN_POINT('Ctrl Pts',(10.2205738429999,15.2,3.40463148499998));
#199973=CARTESIAN_POINT('Ctrl Pts',(10.2205738429999,11.6,3.40463148499998));
#199974=CARTESIAN_POINT('Ctrl Pts',(10.2227010339999,15.2,3.40611029599999));
#199975=CARTESIAN_POINT('Ctrl Pts',(10.2227010339999,11.6,3.40611029599999));
#199976=CARTESIAN_POINT('Ctrl Pts',(10.2248318919999,15.2,3.40759435099999));
#199977=CARTESIAN_POINT('Ctrl Pts',(10.2248318919999,11.6,3.40759435099999));
#199978=CARTESIAN_POINT('Ctrl Pts',(10.2269664019999,15.2,3.40908365299998));
#199979=CARTESIAN_POINT('Ctrl Pts',(10.2269664019999,11.6,3.40908365299998));
#199980=CARTESIAN_POINT('Ctrl Pts',(10.2291045509999,15.2,3.41057820099999));
#199981=CARTESIAN_POINT('Ctrl Pts',(10.2291045509999,11.6,3.41057820099999));
#199982=CARTESIAN_POINT('Ctrl Pts',(10.2312463229999,15.2,3.41207799699998));
#199983=CARTESIAN_POINT('Ctrl Pts',(10.2312463229999,11.6,3.41207799699998));
#199984=CARTESIAN_POINT('Ctrl Pts',(10.2333917049999,15.2,3.41358303999999));
#199985=CARTESIAN_POINT('Ctrl Pts',(10.2333917049999,11.6,3.41358303999999));
#199986=CARTESIAN_POINT('Ctrl Pts',(10.2355406799999,15.2,3.41509333299998));
#199987=CARTESIAN_POINT('Ctrl Pts',(10.2355406799999,11.6,3.41509333299998));
#199988=CARTESIAN_POINT('Ctrl Pts',(10.2376932379999,15.2,3.41660887399998));
#199989=CARTESIAN_POINT('Ctrl Pts',(10.2376932379999,11.6,3.41660887399998));
#199990=CARTESIAN_POINT('Ctrl Pts',(10.2398493599999,15.2,3.41812966599999));
#199991=CARTESIAN_POINT('Ctrl Pts',(10.2398493599999,11.6,3.41812966599999));
#199992=CARTESIAN_POINT('Ctrl Pts',(10.2420090349999,15.2,3.41965570899998));
#199993=CARTESIAN_POINT('Ctrl Pts',(10.2420090349999,11.6,3.41965570899998));
#199994=CARTESIAN_POINT('Ctrl Pts',(10.2441722479999,15.2,3.42118700399999));
#199995=CARTESIAN_POINT('Ctrl Pts',(10.2441722479999,11.6,3.42118700399999));
#199996=CARTESIAN_POINT('Ctrl Pts',(10.2463389839999,15.2,3.42272355099999));
#199997=CARTESIAN_POINT('Ctrl Pts',(10.2463389839999,11.6,3.42272355099999));
#199998=CARTESIAN_POINT('Ctrl Pts',(10.2485092299999,15.2,3.42426535099998));
#199999=CARTESIAN_POINT('Ctrl Pts',(10.2485092299999,11.6,3.42426535099998));
#200000=CARTESIAN_POINT('Ctrl Pts',(10.2506829709999,15.2,3.42581240499998));
#200001=CARTESIAN_POINT('Ctrl Pts',(10.2506829709999,11.6,3.42581240499998));
#200002=CARTESIAN_POINT('Ctrl Pts',(10.2528601939999,15.2,3.42736471399999));
#200003=CARTESIAN_POINT('Ctrl Pts',(10.2528601939999,11.6,3.42736471399998));
#200004=CARTESIAN_POINT('Ctrl Pts',(10.2550408839999,15.2,3.42892227699998));
#200005=CARTESIAN_POINT('Ctrl Pts',(10.2550408839999,11.6,3.42892227699998));
#200006=CARTESIAN_POINT('Ctrl Pts',(10.2572250269999,15.2,3.43048509599999));
#200007=CARTESIAN_POINT('Ctrl Pts',(10.2572250269999,11.6,3.43048509599999));
#200008=CARTESIAN_POINT('Ctrl Pts',(10.2594126089999,15.2,3.43205317199998));
#200009=CARTESIAN_POINT('Ctrl Pts',(10.2594126089999,11.6,3.43205317199998));
#200010=CARTESIAN_POINT('Ctrl Pts',(10.2616036169999,15.2,3.43362650399998));
#200011=CARTESIAN_POINT('Ctrl Pts',(10.2616036169999,11.6,3.43362650399998));
#200012=CARTESIAN_POINT('Ctrl Pts',(10.2637980359999,15.2,3.43520509299999));
#200013=CARTESIAN_POINT('Ctrl Pts',(10.2637980359999,11.6,3.43520509299999));
#200014=CARTESIAN_POINT('Ctrl Pts',(10.2659958539999,15.2,3.43678894099998));
#200015=CARTESIAN_POINT('Ctrl Pts',(10.2659958539999,11.6,3.43678894099998));
#200016=CARTESIAN_POINT('Ctrl Pts',(10.2681970539999,15.2,3.43837804599998));
#200017=CARTESIAN_POINT('Ctrl Pts',(10.2681970539999,11.6,3.43837804599998));
#200018=CARTESIAN_POINT('Ctrl Pts',(10.2704016259999,15.2,3.43997241199999));
#200019=CARTESIAN_POINT('Ctrl Pts',(10.2704016259999,11.6,3.43997241199998));
#200020=CARTESIAN_POINT('Ctrl Pts',(10.2726095529999,15.2,3.44157203699999));
#200021=CARTESIAN_POINT('Ctrl Pts',(10.2726095529999,11.6,3.44157203699999));
#200022=CARTESIAN_POINT('Ctrl Pts',(10.2748208229999,15.2,3.44317692199999));
#200023=CARTESIAN_POINT('Ctrl Pts',(10.2748208229999,11.6,3.44317692199999));
#200024=CARTESIAN_POINT('Ctrl Pts',(10.2770354219999,15.2,3.44478706899999));
#200025=CARTESIAN_POINT('Ctrl Pts',(10.2770354219999,11.6,3.44478706899999));
#200026=CARTESIAN_POINT('Ctrl Pts',(10.2792533369999,15.2,3.44640247699999));
#200027=CARTESIAN_POINT('Ctrl Pts',(10.2792533369999,11.6,3.44640247699999));
#200028=CARTESIAN_POINT('Ctrl Pts',(10.2814745529999,15.2,3.44802314599999));
#200029=CARTESIAN_POINT('Ctrl Pts',(10.2814745529999,11.6,3.44802314599999));
#200030=CARTESIAN_POINT('Ctrl Pts',(10.2836990579999,15.2,3.44964907699998));
#200031=CARTESIAN_POINT('Ctrl Pts',(10.2836990579999,11.6,3.44964907699998));
#200032=CARTESIAN_POINT('Ctrl Pts',(10.2859268359999,15.2,3.45128027099998));
#200033=CARTESIAN_POINT('Ctrl Pts',(10.2859268359999,11.6,3.45128027099998));
#200034=CARTESIAN_POINT('Ctrl Pts',(10.2881578759999,15.2,3.45291672899998));
#200035=CARTESIAN_POINT('Ctrl Pts',(10.2881578759999,11.6,3.45291672899998));
#200036=CARTESIAN_POINT('Ctrl Pts',(10.2903921639999,15.2,3.45455845099998));
#200037=CARTESIAN_POINT('Ctrl Pts',(10.2903921639999,11.6,3.45455845099998));
#200038=CARTESIAN_POINT('Ctrl Pts',(10.2926296859999,15.2,3.45620543599999));
#200039=CARTESIAN_POINT('Ctrl Pts',(10.2926296859999,11.6,3.45620543599999));
#200040=CARTESIAN_POINT('Ctrl Pts',(10.2948704289999,15.2,3.45785768599999));
#200041=CARTESIAN_POINT('Ctrl Pts',(10.2948704289999,11.6,3.45785768599998));
#200042=CARTESIAN_POINT('Ctrl Pts',(10.2971143779999,15.2,3.45951520099998));
#200043=CARTESIAN_POINT('Ctrl Pts',(10.2971143779999,11.6,3.45951520099998));
#200044=CARTESIAN_POINT('Ctrl Pts',(10.2993615219999,15.2,3.46117798099999));
#200045=CARTESIAN_POINT('Ctrl Pts',(10.2993615219999,11.6,3.46117798099998));
#200046=CARTESIAN_POINT('Ctrl Pts',(10.3016118469999,15.2,3.46284602699999));
#200047=CARTESIAN_POINT('Ctrl Pts',(10.3016118469999,11.6,3.46284602699999));
#200048=CARTESIAN_POINT('Ctrl Pts',(10.3038653379999,15.2,3.46451933999998));
#200049=CARTESIAN_POINT('Ctrl Pts',(10.3038653379999,11.6,3.46451933999998));
#200050=CARTESIAN_POINT('Ctrl Pts',(10.3061219849999,15.2,3.46619791899998));
#200051=CARTESIAN_POINT('Ctrl Pts',(10.3061219849999,11.6,3.46619791899998));
#200052=CARTESIAN_POINT('Ctrl Pts',(10.3083817719999,15.2,3.46788176399999));
#200053=CARTESIAN_POINT('Ctrl Pts',(10.3083817719999,11.6,3.46788176399999));
#200054=CARTESIAN_POINT('Ctrl Pts',(10.3106446869999,15.2,3.46957087799999));
#200055=CARTESIAN_POINT('Ctrl Pts',(10.3106446869999,11.6,3.46957087799999));
#200056=CARTESIAN_POINT('Ctrl Pts',(10.3129107159999,15.2,3.47126525799998));
#200057=CARTESIAN_POINT('Ctrl Pts',(10.3129107159999,11.6,3.47126525799998));
#200058=CARTESIAN_POINT('Ctrl Pts',(10.3151798469999,15.2,3.47296490699998));
#200059=CARTESIAN_POINT('Ctrl Pts',(10.3151798469999,11.6,3.47296490699998));
#200060=CARTESIAN_POINT('Ctrl Pts',(10.3174520669999,15.2,3.47466982499999));
#200061=CARTESIAN_POINT('Ctrl Pts',(10.3174520669999,11.6,3.47466982499998));
#200062=CARTESIAN_POINT('Ctrl Pts',(10.3197273619999,15.2,3.47638000999999));
#200063=CARTESIAN_POINT('Ctrl Pts',(10.3197273619999,11.6,3.47638000999999));
#200064=CARTESIAN_POINT('Ctrl Pts',(10.3220057189999,15.2,3.47809546499998));
#200065=CARTESIAN_POINT('Ctrl Pts',(10.3220057189999,11.6,3.47809546499998));
#200066=CARTESIAN_POINT('Ctrl Pts',(10.3242871249999,15.2,3.47981618899999));
#200067=CARTESIAN_POINT('Ctrl Pts',(10.3242871249999,11.6,3.47981618899999));
#200068=CARTESIAN_POINT('Ctrl Pts',(10.3265715679999,15.2,3.48154218199999));
#200069=CARTESIAN_POINT('Ctrl Pts',(10.3265715679999,11.6,3.48154218199999));
#200070=CARTESIAN_POINT('Ctrl Pts',(10.3288590349999,15.2,3.48327344499998));
#200071=CARTESIAN_POINT('Ctrl Pts',(10.3288590349999,11.6,3.48327344499998));
#200072=CARTESIAN_POINT('Ctrl Pts',(10.3311495119999,15.2,3.48500997899999));
#200073=CARTESIAN_POINT('Ctrl Pts',(10.3311495119999,11.6,3.48500997899999));
#200074=CARTESIAN_POINT('Ctrl Pts',(10.3334429859999,15.2,3.48675178299998));
#200075=CARTESIAN_POINT('Ctrl Pts',(10.3334429859999,11.6,3.48675178299998));
#200076=CARTESIAN_POINT('Ctrl Pts',(10.3357394449999,15.2,3.48849885599999));
#200077=CARTESIAN_POINT('Ctrl Pts',(10.3357394449999,11.6,3.48849885599999));
#200078=CARTESIAN_POINT('Ctrl Pts',(10.3380388769999,15.2,3.49025120199999));
#200079=CARTESIAN_POINT('Ctrl Pts',(10.3380388769999,11.6,3.49025120199998));
#200080=CARTESIAN_POINT('Ctrl Pts',(10.3403412679999,15.2,3.49200881799998));
#200081=CARTESIAN_POINT('Ctrl Pts',(10.3403412679999,11.6,3.49200881799998));
#200082=CARTESIAN_POINT('Ctrl Pts',(10.3426466049999,15.2,3.49377170499999));
#200083=CARTESIAN_POINT('Ctrl Pts',(10.3426466049999,11.6,3.49377170499999));
#200084=CARTESIAN_POINT('Ctrl Pts',(10.3449548749999,15.2,3.49553986399999));
#200085=CARTESIAN_POINT('Ctrl Pts',(10.3449548749999,11.6,3.49553986399999));
#200086=CARTESIAN_POINT('Ctrl Pts',(10.3472660669999,15.2,3.49731329399999));
#200087=CARTESIAN_POINT('Ctrl Pts',(10.3472660669999,11.6,3.49731329399999));
#200088=CARTESIAN_POINT('Ctrl Pts',(10.3495801669999,15.2,3.49909199599999));
#200089=CARTESIAN_POINT('Ctrl Pts',(10.3495801669999,11.6,3.49909199599999));
#200090=CARTESIAN_POINT('Ctrl Pts',(10.3518971629999,15.2,3.50087596999998));
#200091=CARTESIAN_POINT('Ctrl Pts',(10.3518971629999,11.6,3.50087596999998));
#200092=CARTESIAN_POINT('Ctrl Pts',(10.3542170419999,15.2,3.50266521699999));
#200093=CARTESIAN_POINT('Ctrl Pts',(10.3542170419999,11.6,3.50266521699999));
#200094=CARTESIAN_POINT('Ctrl Pts',(10.3565397919999,15.2,3.50445973499999));
#200095=CARTESIAN_POINT('Ctrl Pts',(10.3565397919999,11.6,3.50445973499998));
#200096=CARTESIAN_POINT('Ctrl Pts',(10.3588653989999,15.2,3.50625952599999));
#200097=CARTESIAN_POINT('Ctrl Pts',(10.3588653989999,11.6,3.50625952599999));
#200098=CARTESIAN_POINT('Ctrl Pts',(10.3611938519999,15.2,3.50806458899999));
#200099=CARTESIAN_POINT('Ctrl Pts',(10.3611938519999,11.6,3.50806458899999));
#200100=CARTESIAN_POINT('Ctrl Pts',(10.3635251379999,15.2,3.50987492599998));
#200101=CARTESIAN_POINT('Ctrl Pts',(10.3635251379999,11.6,3.50987492599998));
#200102=CARTESIAN_POINT('Ctrl Pts',(10.3658592459999,15.2,3.51169053399998));
#200103=CARTESIAN_POINT('Ctrl Pts',(10.3658592459999,11.6,3.51169053399998));
#200104=CARTESIAN_POINT('Ctrl Pts',(10.3681961589999,15.2,3.51351141599999));
#200105=CARTESIAN_POINT('Ctrl Pts',(10.3681961589999,11.6,3.51351141599999));
#200106=CARTESIAN_POINT('Ctrl Pts',(10.3705358699999,15.2,3.51533757099999));
#200107=CARTESIAN_POINT('Ctrl Pts',(10.3705358699999,11.6,3.51533757099999));
#200108=CARTESIAN_POINT('Ctrl Pts',(10.3728783639999,15.2,3.51716899899999));
#200109=CARTESIAN_POINT('Ctrl Pts',(10.3728783639999,11.6,3.51716899899999));
#200110=CARTESIAN_POINT('Ctrl Pts',(10.3752236289999,15.2,3.51900569999999));
#200111=CARTESIAN_POINT('Ctrl Pts',(10.3752236289999,11.6,3.51900569999999));
#200112=CARTESIAN_POINT('Ctrl Pts',(10.3775716529999,15.2,3.52084767399998));
#200113=CARTESIAN_POINT('Ctrl Pts',(10.3775716529999,11.6,3.52084767399998));
#200114=CARTESIAN_POINT('Ctrl Pts',(10.3799224219999,15.2,3.52269492299998));
#200115=CARTESIAN_POINT('Ctrl Pts',(10.3799224219999,11.6,3.52269492299998));
#200116=CARTESIAN_POINT('Ctrl Pts',(10.3822759259999,15.2,3.52454744299998));
#200117=CARTESIAN_POINT('Ctrl Pts',(10.3822759259999,11.6,3.52454744299998));
#200118=CARTESIAN_POINT('Ctrl Pts',(10.3846321519999,15.2,3.52640523799998));
#200119=CARTESIAN_POINT('Ctrl Pts',(10.3846321519999,11.6,3.52640523799998));
#200120=CARTESIAN_POINT('Ctrl Pts',(10.3869910869999,15.2,3.52826830499998));
#200121=CARTESIAN_POINT('Ctrl Pts',(10.3869910869999,11.6,3.52826830499998));
#200122=CARTESIAN_POINT('Ctrl Pts',(10.3893527199999,15.2,3.53013664599998));
#200123=CARTESIAN_POINT('Ctrl Pts',(10.3893527199999,11.6,3.53013664599998));
#200124=CARTESIAN_POINT('Ctrl Pts',(10.3917170389999,15.2,3.53201026099998));
#200125=CARTESIAN_POINT('Ctrl Pts',(10.3917170389999,11.6,3.53201026099998));
#200126=CARTESIAN_POINT('Ctrl Pts',(10.3940840299999,15.2,3.53388914899998));
#200127=CARTESIAN_POINT('Ctrl Pts',(10.3940840299999,11.6,3.53388914899998));
#200128=CARTESIAN_POINT('Ctrl Pts',(10.3964536819999,15.2,3.53577330999999));
#200129=CARTESIAN_POINT('Ctrl Pts',(10.3964536819999,11.6,3.53577330999999));
#200130=CARTESIAN_POINT('Ctrl Pts',(10.3988259839999,15.2,3.53766274499999));
#200131=CARTESIAN_POINT('Ctrl Pts',(10.3988259839999,11.6,3.53766274499998));
#200132=CARTESIAN_POINT('Ctrl Pts',(10.4012009229999,15.2,3.53955745299999));
#200133=CARTESIAN_POINT('Ctrl Pts',(10.4012009229999,11.6,3.53955745299999));
#200134=CARTESIAN_POINT('Ctrl Pts',(10.4035784859999,15.2,3.54145743499998));
#200135=CARTESIAN_POINT('Ctrl Pts',(10.4035784859999,11.6,3.54145743499998));
#200136=CARTESIAN_POINT('Ctrl Pts',(10.4059586629999,15.2,3.54336268899999));
#200137=CARTESIAN_POINT('Ctrl Pts',(10.4059586629999,11.6,3.54336268899999));
#200138=CARTESIAN_POINT('Ctrl Pts',(10.4083414399999,15.2,3.54527321699998));
#200139=CARTESIAN_POINT('Ctrl Pts',(10.4083414399999,11.6,3.54527321699998));
#200140=CARTESIAN_POINT('Ctrl Pts',(10.4107268069999,15.2,3.54718901799998));
#200141=CARTESIAN_POINT('Ctrl Pts',(10.4107268069999,11.6,3.54718901799998));
#200142=CARTESIAN_POINT('Ctrl Pts',(10.4131147519999,15.2,3.54911009199999));
#200143=CARTESIAN_POINT('Ctrl Pts',(10.4131147519999,11.6,3.54911009199998));
#200144=CARTESIAN_POINT('Ctrl Pts',(10.4155052599999,15.2,3.55103643999998));
#200145=CARTESIAN_POINT('Ctrl Pts',(10.4155052599999,11.6,3.55103643999998));
#200146=CARTESIAN_POINT('Ctrl Pts',(10.4178983229999,15.2,3.55296805999998));
#200147=CARTESIAN_POINT('Ctrl Pts',(10.4178983229999,11.6,3.55296805999998));
#200148=CARTESIAN_POINT('Ctrl Pts',(10.4202939269999,15.2,3.55490495299998));
#200149=CARTESIAN_POINT('Ctrl Pts',(10.4202939269999,11.6,3.55490495299998));
#200150=CARTESIAN_POINT('Ctrl Pts',(10.4226920599999,15.2,3.55684711799999));
#200151=CARTESIAN_POINT('Ctrl Pts',(10.4226920599999,11.6,3.55684711799999));
#200152=CARTESIAN_POINT('Ctrl Pts',(10.4250927119999,15.2,3.55879455599998));
#200153=CARTESIAN_POINT('Ctrl Pts',(10.4250927119999,11.6,3.55879455599998));
#200154=CARTESIAN_POINT('Ctrl Pts',(10.4274958709999,15.2,3.56074726699998));
#200155=CARTESIAN_POINT('Ctrl Pts',(10.4274958709999,11.6,3.56074726699998));
#200156=CARTESIAN_POINT('Ctrl Pts',(10.4299015229999,15.2,3.56270524999999));
#200157=CARTESIAN_POINT('Ctrl Pts',(10.4299015229999,11.6,3.56270524999999));
#200158=CARTESIAN_POINT('Ctrl Pts',(10.4323096579999,15.2,3.56466850499999));
#200159=CARTESIAN_POINT('Ctrl Pts',(10.4323096579999,11.6,3.56466850499999));
#200160=CARTESIAN_POINT('Ctrl Pts',(10.4347202649999,15.2,3.56663703199998));
#200161=CARTESIAN_POINT('Ctrl Pts',(10.4347202649999,11.6,3.56663703199998));
#200162=CARTESIAN_POINT('Ctrl Pts',(10.4371333319999,15.2,3.56861083099999));
#200163=CARTESIAN_POINT('Ctrl Pts',(10.4371333319999,11.6,3.56861083099999));
#200164=CARTESIAN_POINT('Ctrl Pts',(10.4395488449999,15.2,3.57058990199998));
#200165=CARTESIAN_POINT('Ctrl Pts',(10.4395488449999,11.6,3.57058990199998));
#200166=CARTESIAN_POINT('Ctrl Pts',(10.4419667949999,15.2,3.57257424399998));
#200167=CARTESIAN_POINT('Ctrl Pts',(10.4419667949999,11.6,3.57257424399998));
#200168=CARTESIAN_POINT('Ctrl Pts',(10.4443871699999,15.2,3.57456385699999));
#200169=CARTESIAN_POINT('Ctrl Pts',(10.4443871699999,11.6,3.57456385699999));
#200170=CARTESIAN_POINT('Ctrl Pts',(10.4468099579999,15.2,3.57655874199998));
#200171=CARTESIAN_POINT('Ctrl Pts',(10.4468099579999,11.6,3.57655874199998));
#200172=CARTESIAN_POINT('Ctrl Pts',(10.4492351469999,15.2,3.57855889799998));
#200173=CARTESIAN_POINT('Ctrl Pts',(10.4492351469999,11.6,3.57855889799998));
#200174=CARTESIAN_POINT('Ctrl Pts',(10.4516627269999,15.2,3.58056432399999));
#200175=CARTESIAN_POINT('Ctrl Pts',(10.4516627269999,11.6,3.58056432399999));
#200176=CARTESIAN_POINT('Ctrl Pts',(10.4540926849999,15.2,3.58257501999999));
#200177=CARTESIAN_POINT('Ctrl Pts',(10.4540926849999,11.6,3.58257501999999));
#200178=CARTESIAN_POINT('Ctrl Pts',(10.4565250109999,15.2,3.58459098699999));
#200179=CARTESIAN_POINT('Ctrl Pts',(10.4565250109999,11.6,3.58459098699999));
#200180=CARTESIAN_POINT('Ctrl Pts',(10.4589596909999,15.2,3.58661222399999));
#200181=CARTESIAN_POINT('Ctrl Pts',(10.4589596909999,11.6,3.58661222399998));
#200182=CARTESIAN_POINT('Ctrl Pts',(10.4613967169999,15.2,3.58863873099998));
#200183=CARTESIAN_POINT('Ctrl Pts',(10.4613967169999,11.6,3.58863873099998));
#200184=CARTESIAN_POINT('Ctrl Pts',(10.4638360759999,15.2,3.59067050699998));
#200185=CARTESIAN_POINT('Ctrl Pts',(10.4638360759999,11.6,3.59067050699998));
#200186=CARTESIAN_POINT('Ctrl Pts',(10.4662777559999,15.2,3.59270755199999));
#200187=CARTESIAN_POINT('Ctrl Pts',(10.4662777559999,11.6,3.59270755199999));
#200188=CARTESIAN_POINT('Ctrl Pts',(10.4687217459999,15.2,3.59474986699999));
#200189=CARTESIAN_POINT('Ctrl Pts',(10.4687217459999,11.6,3.59474986699999));
#200190=CARTESIAN_POINT('Ctrl Pts',(10.4711680339999,15.2,3.59679744999998));
#200191=CARTESIAN_POINT('Ctrl Pts',(10.4711680339999,11.6,3.59679744999998));
#200192=CARTESIAN_POINT('Ctrl Pts',(10.4736166109999,15.2,3.59885030099999));
#200193=CARTESIAN_POINT('Ctrl Pts',(10.4736166109999,11.6,3.59885030099999));
#200194=CARTESIAN_POINT('Ctrl Pts',(10.4760674639999,15.2,3.60090842099999));
#200195=CARTESIAN_POINT('Ctrl Pts',(10.4760674639999,11.6,3.60090842099999));
#200196=CARTESIAN_POINT('Ctrl Pts',(10.4785205819999,15.2,3.60297180799999));
#200197=CARTESIAN_POINT('Ctrl Pts',(10.4785205819999,11.6,3.60297180799999));
#200198=CARTESIAN_POINT('Ctrl Pts',(10.4809759539999,15.2,3.60504046299998));
#200199=CARTESIAN_POINT('Ctrl Pts',(10.4809759539999,11.6,3.60504046299998));
#200200=CARTESIAN_POINT('Ctrl Pts',(10.4834335689999,15.2,3.60711438399999));
#200201=CARTESIAN_POINT('Ctrl Pts',(10.4834335689999,11.6,3.60711438399999));
#200202=CARTESIAN_POINT('Ctrl Pts',(10.4858934149999,15.2,3.60919357299998));
#200203=CARTESIAN_POINT('Ctrl Pts',(10.4858934149999,11.6,3.60919357299998));
#200204=CARTESIAN_POINT('Ctrl Pts',(10.4883554829999,15.2,3.61127802799999));
#200205=CARTESIAN_POINT('Ctrl Pts',(10.4883554829999,11.6,3.61127802799999));
#200206=CARTESIAN_POINT('Ctrl Pts',(10.4908197579999,15.2,3.61336774899998));
#200207=CARTESIAN_POINT('Ctrl Pts',(10.4908197579999,11.6,3.61336774899998));
#200208=CARTESIAN_POINT('Ctrl Pts',(10.4932862329999,15.2,3.61546273599998));
#200209=CARTESIAN_POINT('Ctrl Pts',(10.4932862329999,11.6,3.61546273599998));
#200210=CARTESIAN_POINT('Ctrl Pts',(10.4957548949999,15.2,3.61756298899999));
#200211=CARTESIAN_POINT('Ctrl Pts',(10.4957548949999,11.6,3.61756298899999));
#200212=CARTESIAN_POINT('Ctrl Pts',(10.4982257319999,15.2,3.61966850599998));
#200213=CARTESIAN_POINT('Ctrl Pts',(10.4982257319999,11.6,3.61966850599998));
#200214=CARTESIAN_POINT('Ctrl Pts',(10.5006987339999,15.2,3.62177928899998));
#200215=CARTESIAN_POINT('Ctrl Pts',(10.5006987339999,11.6,3.62177928899998));
#200216=CARTESIAN_POINT('Ctrl Pts',(10.5031738909999,15.2,3.62389533499999));
#200217=CARTESIAN_POINT('Ctrl Pts',(10.5031738909999,11.6,3.62389533499999));
#200218=CARTESIAN_POINT('Ctrl Pts',(10.5056511899999,15.2,3.62601664499999));
#200219=CARTESIAN_POINT('Ctrl Pts',(10.5056511899999,11.6,3.62601664499999));
#200220=CARTESIAN_POINT('Ctrl Pts',(10.5081306219999,15.2,3.62814321899998));
#200221=CARTESIAN_POINT('Ctrl Pts',(10.5081306219999,11.6,3.62814321899998));
#200222=CARTESIAN_POINT('Ctrl Pts',(10.5106121749999,15.2,3.63027505599998));
#200223=CARTESIAN_POINT('Ctrl Pts',(10.5106121749999,11.6,3.63027505599998));
#200224=CARTESIAN_POINT('Ctrl Pts',(10.5130958379999,15.2,3.63241215499999));
#200225=CARTESIAN_POINT('Ctrl Pts',(10.5130958379999,11.6,3.63241215499999));
#200226=CARTESIAN_POINT('Ctrl Pts',(10.5155816019999,15.2,3.63455451599999));
#200227=CARTESIAN_POINT('Ctrl Pts',(10.5155816019999,11.6,3.63455451599999));
#200228=CARTESIAN_POINT('Ctrl Pts',(10.5180694529999,15.2,3.63670213999999));
#200229=CARTESIAN_POINT('Ctrl Pts',(10.5180694529999,11.6,3.63670213999999));
#200230=CARTESIAN_POINT('Ctrl Pts',(10.5205593819999,15.2,3.63885502499999));
#200231=CARTESIAN_POINT('Ctrl Pts',(10.5205593819999,11.6,3.63885502499999));
#200232=CARTESIAN_POINT('Ctrl Pts',(10.5230513769999,15.2,3.64101317099998));
#200233=CARTESIAN_POINT('Ctrl Pts',(10.5230513769999,11.6,3.64101317099998));
#200234=CARTESIAN_POINT('Ctrl Pts',(10.5255454289999,15.2,3.64317657699999));
#200235=CARTESIAN_POINT('Ctrl Pts',(10.5255454289999,11.6,3.64317657699999));
#200236=CARTESIAN_POINT('Ctrl Pts',(10.5280415259999,15.2,3.64534524299999));
#200237=CARTESIAN_POINT('Ctrl Pts',(10.5280415259999,11.6,3.64534524299999));
#200238=CARTESIAN_POINT('Ctrl Pts',(10.5305396569999,15.2,3.64751916899999));
#200239=CARTESIAN_POINT('Ctrl Pts',(10.5305396569999,11.6,3.64751916899999));
#200240=CARTESIAN_POINT('Ctrl Pts',(10.5330398119999,15.2,3.64969835299998));
#200241=CARTESIAN_POINT('Ctrl Pts',(10.5330398119999,11.6,3.64969835299998));
#200242=CARTESIAN_POINT('Ctrl Pts',(10.5355419799999,15.2,3.65188279699999));
#200243=CARTESIAN_POINT('Ctrl Pts',(10.5355419799999,11.6,3.65188279699999));
#200244=CARTESIAN_POINT('Ctrl Pts',(10.5380461509999,15.2,3.65407249799999));
#200245=CARTESIAN_POINT('Ctrl Pts',(10.5380461509999,11.6,3.65407249799999));
#200246=CARTESIAN_POINT('Ctrl Pts',(10.5405523129999,15.2,3.65626745699998));
#200247=CARTESIAN_POINT('Ctrl Pts',(10.5405523129999,11.6,3.65626745699998));
#200248=CARTESIAN_POINT('Ctrl Pts',(10.5430604559999,15.2,3.65846767299999));
#200249=CARTESIAN_POINT('Ctrl Pts',(10.5430604559999,11.6,3.65846767299998));
#200250=CARTESIAN_POINT('Ctrl Pts',(10.5455705689999,15.2,3.66067314599999));
#200251=CARTESIAN_POINT('Ctrl Pts',(10.5455705689999,11.6,3.66067314599999));
#200252=CARTESIAN_POINT('Ctrl Pts',(10.5480826419999,15.2,3.66288387299999));
#200253=CARTESIAN_POINT('Ctrl Pts',(10.5480826419999,11.6,3.66288387299999));
#200254=CARTESIAN_POINT('Ctrl Pts',(10.5505966639999,15.2,3.66509985799999));
#200255=CARTESIAN_POINT('Ctrl Pts',(10.5505966639999,11.6,3.66509985799999));
#200256=CARTESIAN_POINT('Ctrl Pts',(10.5531126259999,15.2,3.66732109599998));
#200257=CARTESIAN_POINT('Ctrl Pts',(10.5531126259999,11.6,3.66732109599998));
#200258=CARTESIAN_POINT('Ctrl Pts',(10.5556305149999,15.2,3.66954758899999));
#200259=CARTESIAN_POINT('Ctrl Pts',(10.5556305149999,11.6,3.66954758899999));
#200260=CARTESIAN_POINT('Ctrl Pts',(10.5581503209999,15.2,3.67177933599999));
#200261=CARTESIAN_POINT('Ctrl Pts',(10.5581503209999,11.6,3.67177933599999));
#200262=CARTESIAN_POINT('Ctrl Pts',(10.5606720349999,15.2,3.67401633699998));
#200263=CARTESIAN_POINT('Ctrl Pts',(10.5606720349999,11.6,3.67401633699998));
#200264=CARTESIAN_POINT('Ctrl Pts',(10.5631956449999,15.2,3.67625858999999));
#200265=CARTESIAN_POINT('Ctrl Pts',(10.5631956449999,11.6,3.67625858999999));
#200266=CARTESIAN_POINT('Ctrl Pts',(10.5657211419999,15.2,3.67850609499998));
#200267=CARTESIAN_POINT('Ctrl Pts',(10.5657211419999,11.6,3.67850609499998));
#200268=CARTESIAN_POINT('Ctrl Pts',(10.5682485129999,15.2,3.68075884999998));
#200269=CARTESIAN_POINT('Ctrl Pts',(10.5682485129999,11.6,3.68075884999998));
#200270=CARTESIAN_POINT('Ctrl Pts',(10.5707777509999,15.2,3.68301685799998));
#200271=CARTESIAN_POINT('Ctrl Pts',(10.5707777509999,11.6,3.68301685799998));
#200272=CARTESIAN_POINT('Ctrl Pts',(10.5733088419999,15.2,3.68528011699999));
#200273=CARTESIAN_POINT('Ctrl Pts',(10.5733088419999,11.6,3.68528011699999));
#200274=CARTESIAN_POINT('Ctrl Pts',(10.5758417789999,15.2,3.68754862399998));
#200275=CARTESIAN_POINT('Ctrl Pts',(10.5758417789999,11.6,3.68754862399998));
#200276=CARTESIAN_POINT('Ctrl Pts',(10.5783765499999,15.2,3.68982238099999));
#200277=CARTESIAN_POINT('Ctrl Pts',(10.5783765499999,11.6,3.68982238099999));
#200278=CARTESIAN_POINT('Ctrl Pts',(10.5809131429999,15.2,3.69210138599998));
#200279=CARTESIAN_POINT('Ctrl Pts',(10.5809131429999,11.6,3.69210138599998));
#200280=CARTESIAN_POINT('Ctrl Pts',(10.5834515509999,15.2,3.69438563899998));
#200281=CARTESIAN_POINT('Ctrl Pts',(10.5834515509999,11.6,3.69438563899998));
#200282=CARTESIAN_POINT('Ctrl Pts',(10.5859917629999,15.2,3.69667513899999));
#200283=CARTESIAN_POINT('Ctrl Pts',(10.5859917629999,11.6,3.69667513899999));
#200284=CARTESIAN_POINT('Ctrl Pts',(10.5885337649999,15.2,3.69896988599999));
#200285=CARTESIAN_POINT('Ctrl Pts',(10.5885337649999,11.6,3.69896988599999));
#200286=CARTESIAN_POINT('Ctrl Pts',(10.5910775529999,15.2,3.70126987899998));
#200287=CARTESIAN_POINT('Ctrl Pts',(10.5910775529999,11.6,3.70126987899998));
#200288=CARTESIAN_POINT('Ctrl Pts',(10.5936231109999,15.2,3.70357511699999));
#200289=CARTESIAN_POINT('Ctrl Pts',(10.5936231109999,11.6,3.70357511699999));
#200290=CARTESIAN_POINT('Ctrl Pts',(10.5961704319999,15.2,3.70588559899999));
#200291=CARTESIAN_POINT('Ctrl Pts',(10.5961704319999,11.6,3.70588559899998));
#200292=CARTESIAN_POINT('Ctrl Pts',(10.5987195039999,15.2,3.70820132699999));
#200293=CARTESIAN_POINT('Ctrl Pts',(10.5987195039999,11.6,3.70820132699999));
#200294=CARTESIAN_POINT('Ctrl Pts',(10.6012703189999,15.2,3.71052229699998));
#200295=CARTESIAN_POINT('Ctrl Pts',(10.6012703189999,11.6,3.71052229699998));
#200296=CARTESIAN_POINT('Ctrl Pts',(10.6038228649999,15.2,3.71284850999999));
#200297=CARTESIAN_POINT('Ctrl Pts',(10.6038228649999,11.6,3.71284850999999));
#200298=CARTESIAN_POINT('Ctrl Pts',(10.6063771329999,15.2,3.71517996499998));
#200299=CARTESIAN_POINT('Ctrl Pts',(10.6063771329999,11.6,3.71517996499998));
#200300=CARTESIAN_POINT('Ctrl Pts',(10.6089331119999,15.2,3.71751665999999));
#200301=CARTESIAN_POINT('Ctrl Pts',(10.6089331119999,11.6,3.71751665999999));
#200302=CARTESIAN_POINT('Ctrl Pts',(10.6114907919999,15.2,3.71985859599998));
#200303=CARTESIAN_POINT('Ctrl Pts',(10.6114907919999,11.6,3.71985859599998));
#200304=CARTESIAN_POINT('Ctrl Pts',(10.6140501629999,15.2,3.72220577299998));
#200305=CARTESIAN_POINT('Ctrl Pts',(10.6140501629999,11.6,3.72220577299998));
#200306=CARTESIAN_POINT('Ctrl Pts',(10.6166112159999,15.2,3.72455818799998));
#200307=CARTESIAN_POINT('Ctrl Pts',(10.6166112159999,11.6,3.72455818799998));
#200308=CARTESIAN_POINT('Ctrl Pts',(10.6191739399999,15.2,3.72691584199998));
#200309=CARTESIAN_POINT('Ctrl Pts',(10.6191739399999,11.6,3.72691584199998));
#200310=CARTESIAN_POINT('Ctrl Pts',(10.6217383239999,15.2,3.72927873299999));
#200311=CARTESIAN_POINT('Ctrl Pts',(10.6217383239999,11.6,3.72927873299999));
#200312=CARTESIAN_POINT('Ctrl Pts',(10.6243043599999,15.2,3.73164686199999));
#200313=CARTESIAN_POINT('Ctrl Pts',(10.6243043599999,11.6,3.73164686199999));
#200314=CARTESIAN_POINT('Ctrl Pts',(10.6268720369999,15.2,3.73402022499998));
#200315=CARTESIAN_POINT('Ctrl Pts',(10.6268720369999,11.6,3.73402022499998));
#200316=CARTESIAN_POINT('Ctrl Pts',(10.6294413449999,15.2,3.73639882599999));
#200317=CARTESIAN_POINT('Ctrl Pts',(10.6294413449999,11.6,3.73639882599999));
#200318=CARTESIAN_POINT('Ctrl Pts',(10.6320122749999,15.2,3.73878265999998));
#200319=CARTESIAN_POINT('Ctrl Pts',(10.6320122749999,11.6,3.73878265999998));
#200320=CARTESIAN_POINT('Ctrl Pts',(10.6345848139999,15.2,3.74117172899999));
#200321=CARTESIAN_POINT('Ctrl Pts',(10.6345848139999,11.6,3.74117172899999));
#200322=CARTESIAN_POINT('Ctrl Pts',(10.6371589569999,15.2,3.74356603099999));
#200323=CARTESIAN_POINT('Ctrl Pts',(10.6371589569999,11.6,3.74356603099999));
#200324=CARTESIAN_POINT('Ctrl Pts',(10.6397346889999,15.2,3.74596556499998));
#200325=CARTESIAN_POINT('Ctrl Pts',(10.6397346889999,11.6,3.74596556499998));
#200326=CARTESIAN_POINT('Ctrl Pts',(10.6423120039999,15.2,3.74837032999999));
#200327=CARTESIAN_POINT('Ctrl Pts',(10.6423120039999,11.6,3.74837032999999));
#200328=CARTESIAN_POINT('Ctrl Pts',(10.6448908909999,15.2,3.75078032599999));
#200329=CARTESIAN_POINT('Ctrl Pts',(10.6448908909999,11.6,3.75078032599998));
#200330=CARTESIAN_POINT('Ctrl Pts',(10.6474713389999,15.2,3.75319555299999));
#200331=CARTESIAN_POINT('Ctrl Pts',(10.6474713389999,11.6,3.75319555299999));
#200332=CARTESIAN_POINT('Ctrl Pts',(10.6500533389999,15.2,3.75561600899999));
#200333=CARTESIAN_POINT('Ctrl Pts',(10.6500533389999,11.6,3.75561600899999));
#200334=CARTESIAN_POINT('Ctrl Pts',(10.6526368819999,15.2,3.75804169199998));
#200335=CARTESIAN_POINT('Ctrl Pts',(10.6526368819999,11.6,3.75804169199998));
#200336=CARTESIAN_POINT('Ctrl Pts',(10.6552219569999,15.2,3.76047260399999));
#200337=CARTESIAN_POINT('Ctrl Pts',(10.6552219569999,11.6,3.76047260399999));
#200338=CARTESIAN_POINT('Ctrl Pts',(10.6578085549999,15.2,3.76290874199999));
#200339=CARTESIAN_POINT('Ctrl Pts',(10.6578085549999,11.6,3.76290874199999));
#200340=CARTESIAN_POINT('Ctrl Pts',(10.6603966649999,15.2,3.76535010599999));
#200341=CARTESIAN_POINT('Ctrl Pts',(10.6603966649999,11.6,3.76535010599999));
#200342=CARTESIAN_POINT('Ctrl Pts',(10.6629862789999,15.2,3.76779669499999));
#200343=CARTESIAN_POINT('Ctrl Pts',(10.6629862789999,11.6,3.76779669499999));
#200344=CARTESIAN_POINT('Ctrl Pts',(10.6655773879999,15.2,3.77024850899998));
#200345=CARTESIAN_POINT('Ctrl Pts',(10.6655773879999,11.6,3.77024850899998));
#200346=CARTESIAN_POINT('Ctrl Pts',(10.6681699789999,15.2,3.77270554599999));
#200347=CARTESIAN_POINT('Ctrl Pts',(10.6681699789999,11.6,3.77270554599999));
#200348=CARTESIAN_POINT('Ctrl Pts',(10.6707640449999,15.2,3.77516780499998));
#200349=CARTESIAN_POINT('Ctrl Pts',(10.6707640449999,11.6,3.77516780499998));
#200350=CARTESIAN_POINT('Ctrl Pts',(10.6733595749999,15.2,3.77763528599999));
#200351=CARTESIAN_POINT('Ctrl Pts',(10.6733595749999,11.6,3.77763528599999));
#200352=CARTESIAN_POINT('Ctrl Pts',(10.6759565599999,15.2,3.78010798799998));
#200353=CARTESIAN_POINT('Ctrl Pts',(10.6759565599999,11.6,3.78010798799998));
#200354=CARTESIAN_POINT('Ctrl Pts',(10.6785549909999,15.2,3.78258590999998));
#200355=CARTESIAN_POINT('Ctrl Pts',(10.6785549909999,11.6,3.78258590999998));
#200356=CARTESIAN_POINT('Ctrl Pts',(10.6811548569999,15.2,3.78506904999998));
#200357=CARTESIAN_POINT('Ctrl Pts',(10.6811548569999,11.6,3.78506904999998));
#200358=CARTESIAN_POINT('Ctrl Pts',(10.6837561499999,15.2,3.78755740899998));
#200359=CARTESIAN_POINT('Ctrl Pts',(10.6837561499999,11.6,3.78755740899998));
#200360=CARTESIAN_POINT('Ctrl Pts',(10.6863588589999,15.2,3.79005098599999));
#200361=CARTESIAN_POINT('Ctrl Pts',(10.6863588589999,11.6,3.79005098599999));
#200362=CARTESIAN_POINT('Ctrl Pts',(10.6889629749999,15.2,3.79254977899999));
#200363=CARTESIAN_POINT('Ctrl Pts',(10.6889629749999,11.6,3.79254977899999));
#200364=CARTESIAN_POINT('Ctrl Pts',(10.6915684889999,15.2,3.79505378599998));
#200365=CARTESIAN_POINT('Ctrl Pts',(10.6915684889999,11.6,3.79505378599998));
#200366=CARTESIAN_POINT('Ctrl Pts',(10.6941753909999,15.2,3.79756300999999));
#200367=CARTESIAN_POINT('Ctrl Pts',(10.6941753909999,11.6,3.79756300999999));
#200368=CARTESIAN_POINT('Ctrl Pts',(10.6967836699999,15.2,3.80007744599999));
#200369=CARTESIAN_POINT('Ctrl Pts',(10.6967836699999,11.6,3.80007744599998));
#200370=CARTESIAN_POINT('Ctrl Pts',(10.6993933199999,15.2,3.80259709499998));
#200371=CARTESIAN_POINT('Ctrl Pts',(10.6993933199999,11.6,3.80259709499998));
#200372=CARTESIAN_POINT('Ctrl Pts',(10.7020043289999,15.2,3.80512195599999));
#200373=CARTESIAN_POINT('Ctrl Pts',(10.7020043289999,11.6,3.80512195599999));
#200374=CARTESIAN_POINT('Ctrl Pts',(10.7046166879999,15.2,3.80765202799999));
#200375=CARTESIAN_POINT('Ctrl Pts',(10.7046166879999,11.6,3.80765202799999));
#200376=CARTESIAN_POINT('Ctrl Pts',(10.7072303869999,15.2,3.81018730899999));
#200377=CARTESIAN_POINT('Ctrl Pts',(10.7072303869999,11.6,3.81018730899999));
#200378=CARTESIAN_POINT('Ctrl Pts',(10.7098454179999,15.2,3.81272779999998));
#200379=CARTESIAN_POINT('Ctrl Pts',(10.7098454179999,11.6,3.81272779999998));
#200380=CARTESIAN_POINT('Ctrl Pts',(10.7124617709999,15.2,3.81527349799998));
#200381=CARTESIAN_POINT('Ctrl Pts',(10.7124617709999,11.6,3.81527349799998));
#200382=CARTESIAN_POINT('Ctrl Pts',(10.7150794359999,15.2,3.81782440399999));
#200383=CARTESIAN_POINT('Ctrl Pts',(10.7150794359999,11.6,3.81782440399998));
#200384=CARTESIAN_POINT('Ctrl Pts',(10.7176984049999,15.2,3.82038051699999));
#200385=CARTESIAN_POINT('Ctrl Pts',(10.7176984049999,11.6,3.82038051699999));
#200386=CARTESIAN_POINT('Ctrl Pts',(10.7203186669999,15.2,3.82294183299998));
#200387=CARTESIAN_POINT('Ctrl Pts',(10.7203186669999,11.6,3.82294183299998));
#200388=CARTESIAN_POINT('Ctrl Pts',(10.7229402149999,15.2,3.82550835499998));
#200389=CARTESIAN_POINT('Ctrl Pts',(10.7229402149999,11.6,3.82550835499998));
#200390=CARTESIAN_POINT('Ctrl Pts',(10.7255630379999,15.2,3.82808007899998));
#200391=CARTESIAN_POINT('Ctrl Pts',(10.7255630379999,11.6,3.82808007899998));
#200392=CARTESIAN_POINT('Ctrl Pts',(10.7281871259999,15.2,3.83065700599998));
#200393=CARTESIAN_POINT('Ctrl Pts',(10.7281871259999,11.6,3.83065700599998));
#200394=CARTESIAN_POINT('Ctrl Pts',(10.7308124709999,15.2,3.83323913299999));
#200395=CARTESIAN_POINT('Ctrl Pts',(10.7308124709999,11.6,3.83323913299999));
#200396=CARTESIAN_POINT('Ctrl Pts',(10.7334390639999,15.2,3.83582646099998));
#200397=CARTESIAN_POINT('Ctrl Pts',(10.7334390639999,11.6,3.83582646099998));
#200398=CARTESIAN_POINT('Ctrl Pts',(10.7360668939999,15.2,3.83841898799999));
#200399=CARTESIAN_POINT('Ctrl Pts',(10.7360668939999,11.6,3.83841898799999));
#200400=CARTESIAN_POINT('Ctrl Pts',(10.7386959529999,15.2,3.84101671299998));
#200401=CARTESIAN_POINT('Ctrl Pts',(10.7386959529999,11.6,3.84101671299998));
#200402=CARTESIAN_POINT('Ctrl Pts',(10.7413262329999,15.2,3.84361963599999));
#200403=CARTESIAN_POINT('Ctrl Pts',(10.7413262329999,11.6,3.84361963599999));
#200404=CARTESIAN_POINT('Ctrl Pts',(10.7439577219999,15.2,3.84622775399999));
#200405=CARTESIAN_POINT('Ctrl Pts',(10.7439577219999,11.6,3.84622775399999));
#200406=CARTESIAN_POINT('Ctrl Pts',(10.7465904139999,15.2,3.84884106799999));
#200407=CARTESIAN_POINT('Ctrl Pts',(10.7465904139999,11.6,3.84884106799999));
#200408=CARTESIAN_POINT('Ctrl Pts',(10.7492242979999,15.2,3.85145957599998));
#200409=CARTESIAN_POINT('Ctrl Pts',(10.7492242979999,11.6,3.85145957599998));
#200410=CARTESIAN_POINT('Ctrl Pts',(10.7518593659999,15.2,3.85408327699999));
#200411=CARTESIAN_POINT('Ctrl Pts',(10.7518593659999,11.6,3.85408327699999));
#200412=CARTESIAN_POINT('Ctrl Pts',(10.7544956079999,15.2,3.85671216899999));
#200413=CARTESIAN_POINT('Ctrl Pts',(10.7544956079999,11.6,3.85671216899999));
#200414=CARTESIAN_POINT('Ctrl Pts',(10.7571330149999,15.2,3.85934625299999));
#200415=CARTESIAN_POINT('Ctrl Pts',(10.7571330149999,11.6,3.85934625299999));
#200416=CARTESIAN_POINT('Ctrl Pts',(10.7597715779999,15.2,3.86198552599998));
#200417=CARTESIAN_POINT('Ctrl Pts',(10.7597715779999,11.6,3.86198552599998));
#200418=CARTESIAN_POINT('Ctrl Pts',(10.7624112859999,15.2,3.86462998899999));
#200419=CARTESIAN_POINT('Ctrl Pts',(10.7624112859999,11.6,3.86462998899999));
#200420=CARTESIAN_POINT('Ctrl Pts',(10.7650521309999,15.2,3.86727963899999));
#200421=CARTESIAN_POINT('Ctrl Pts',(10.7650521309999,11.6,3.86727963899998));
#200422=CARTESIAN_POINT('Ctrl Pts',(10.7676941039999,15.2,3.86993447499999));
#200423=CARTESIAN_POINT('Ctrl Pts',(10.7676941039999,11.6,3.86993447499999));
#200424=CARTESIAN_POINT('Ctrl Pts',(10.7703371949999,15.2,3.87259449799998));
#200425=CARTESIAN_POINT('Ctrl Pts',(10.7703371949999,11.6,3.87259449799998));
#200426=CARTESIAN_POINT('Ctrl Pts',(10.7729813979999,15.2,3.87525970399999));
#200427=CARTESIAN_POINT('Ctrl Pts',(10.7729813979999,11.6,3.87525970399999));
#200428=CARTESIAN_POINT('Ctrl Pts',(10.7756267029999,15.2,3.87793009399999));
#200429=CARTESIAN_POINT('Ctrl Pts',(10.7756267029999,11.6,3.87793009399999));
#200430=CARTESIAN_POINT('Ctrl Pts',(10.7782731039999,15.2,3.88060566599999));
#200431=CARTESIAN_POINT('Ctrl Pts',(10.7782731039999,11.6,3.88060566599999));
#200432=CARTESIAN_POINT('Ctrl Pts',(10.7809205909999,15.2,3.88328641999999));
#200433=CARTESIAN_POINT('Ctrl Pts',(10.7809205909999,11.6,3.88328641999998));
#200434=CARTESIAN_POINT('Ctrl Pts',(10.7835691559999,15.2,3.88597235399998));
#200435=CARTESIAN_POINT('Ctrl Pts',(10.7835691559999,11.6,3.88597235399998));
#200436=CARTESIAN_POINT('Ctrl Pts',(10.7862187859999,15.2,3.88866346799999));
#200437=CARTESIAN_POINT('Ctrl Pts',(10.7862187859999,11.6,3.88866346799999));
#200438=CARTESIAN_POINT('Ctrl Pts',(10.7888694719999,15.2,3.89135975899999));
#200439=CARTESIAN_POINT('Ctrl Pts',(10.7888694719999,11.6,3.89135975899999));
#200440=CARTESIAN_POINT('Ctrl Pts',(10.7915212029999,15.2,3.89406122599999));
#200441=CARTESIAN_POINT('Ctrl Pts',(10.7915212029999,11.6,3.89406122599999));
#200442=CARTESIAN_POINT('Ctrl Pts',(10.7941739669999,15.2,3.89676786899999));
#200443=CARTESIAN_POINT('Ctrl Pts',(10.7941739669999,11.6,3.89676786899999));
#200444=CARTESIAN_POINT('Ctrl Pts',(10.7968277549999,15.2,3.89947968499998));
#200445=CARTESIAN_POINT('Ctrl Pts',(10.7968277549999,11.6,3.89947968499998));
#200446=CARTESIAN_POINT('Ctrl Pts',(10.7994825589999,15.2,3.90219667399998));
#200447=CARTESIAN_POINT('Ctrl Pts',(10.7994825589999,11.6,3.90219667399998));
#200448=CARTESIAN_POINT('Ctrl Pts',(10.8021383729999,15.2,3.90491883499998));
#200449=CARTESIAN_POINT('Ctrl Pts',(10.8021383729999,11.6,3.90491883499998));
#200450=CARTESIAN_POINT('Ctrl Pts',(10.8047951939999,15.2,3.90764616699999));
#200451=CARTESIAN_POINT('Ctrl Pts',(10.8047951939999,11.6,3.90764616699998));
#200452=CARTESIAN_POINT('Ctrl Pts',(10.8074530179999,15.2,3.91037866999999));
#200453=CARTESIAN_POINT('Ctrl Pts',(10.8074530179999,11.6,3.91037866999999));
#200454=CARTESIAN_POINT('Ctrl Pts',(10.8095800799999,15.2,3.91256880899999));
#200455=CARTESIAN_POINT('Ctrl Pts',(10.8095800799999,11.6,3.91256880899999));
#200456=CARTESIAN_POINT('Ctrl Pts',(10.8111758269999,15.2,3.91421373899998));
#200457=CARTESIAN_POINT('Ctrl Pts',(10.8111758269999,11.6,3.91421373899998));
#200458=CARTESIAN_POINT('Ctrl Pts',(10.8122398589999,15.2,3.91531139399999));
#200459=CARTESIAN_POINT('Ctrl Pts',(10.8122398589999,11.6,3.91531139399999));
#200460=CARTESIAN_POINT('Ctrl Pts',(10.8127719249999,15.2,3.91586047999999));
#200461=CARTESIAN_POINT('Ctrl Pts',(10.8127719249999,11.6,3.91586047999999));
#200462=CARTESIAN_POINT('Ctrl Pts',(9.86852965799994,15.2,3.20199116299998));
#200463=CARTESIAN_POINT('Ctrl Pts',(9.87017542602826,15.2,3.2026865729514));
#200464=CARTESIAN_POINT('Ctrl Pts',(9.87187175395476,15.2,3.20340918505387));
#200465=CARTESIAN_POINT('Ctrl Pts',(9.87361750382533,15.2,3.20415921017613));
#200466=CARTESIAN_POINT('Ctrl Pts',(9.8753716725842,15.2,3.20491285229864));
#200467=CARTESIAN_POINT('Ctrl Pts',(9.87717573909119,15.2,3.20569417515048));
#200468=CARTESIAN_POINT('Ctrl Pts',(9.87902857820422,15.2,3.20650338931996));
#200469=CARTESIAN_POINT('Ctrl Pts',(9.88088141714894,15.2,3.20731260341592));
#200470=CARTESIAN_POINT('Ctrl Pts',(9.88278302753734,15.2,3.20814970993136));
#200471=CARTESIAN_POINT('Ctrl Pts',(9.88473231729986,15.2,3.20901491173327));
#200472=CARTESIAN_POINT('Ctrl Pts',(9.88668160706237,15.2,3.20988011353517));
#200473=CARTESIAN_POINT('Ctrl Pts',(9.88867857432713,15.2,3.21077340710827));
#200474=CARTESIAN_POINT('Ctrl Pts',(9.89072215651895,15.2,3.21169499186919));
#200475=CARTESIAN_POINT('Ctrl Pts',(9.8927657388964,15.2,3.21261657671382));
#200476=CARTESIAN_POINT('Ctrl Pts',(9.89485593697986,15.2,3.21356644793465));
#200477=CARTESIAN_POINT('Ctrl Pts',(9.89699171626601,15.2,3.21454479382325));
#200478=CARTESIAN_POINT('Ctrl Pts',(9.89948345847554,15.2,3.21568619722663));
#200479=CARTESIAN_POINT('Ctrl Pts',(9.90203723794068,15.2,3.21686635803255));
#200480=CARTESIAN_POINT('Ctrl Pts',(9.90465146305821,15.2,3.21808555589058));
#200481=CARTESIAN_POINT('Ctrl Pts',(9.90689222770636,15.2,3.21913058274808));
#200482=CARTESIAN_POINT('Ctrl Pts',(9.90917740008215,15.2,3.22020428848307));
#200483=CARTESIAN_POINT('Ctrl Pts',(9.91150600579537,15.2,3.22130684512845));
#200484=CARTESIAN_POINT('Ctrl Pts',(9.91383461129706,15.2,3.22240940167369));
#200485=CARTESIAN_POINT('Ctrl Pts',(9.91620664881097,15.2,3.22354080604563));
#200486=CARTESIAN_POINT('Ctrl Pts',(9.9186211692343,15.2,3.22470122175879));
#200487=CARTESIAN_POINT('Ctrl Pts',(9.92103568965765,15.2,3.22586163747197));
#200488=CARTESIAN_POINT('Ctrl Pts',(9.92349269040646,15.2,3.22705106416252));
#200489=CARTESIAN_POINT('Ctrl Pts',(9.92599124514721,15.2,3.22826965495031));
#200490=CARTESIAN_POINT('Ctrl Pts',(9.9284898001149,15.2,3.22948824584879));
#200491=CARTESIAN_POINT('Ctrl Pts',(9.93102990997944,15.2,3.23073600190922));
#200492=CARTESIAN_POINT('Ctrl Pts',(9.93361066903952,15.2,3.23201307139747));
#200493=CARTESIAN_POINT('Ctrl Pts',(9.93619142786518,15.2,3.23329014076973));
#200494=CARTESIAN_POINT('Ctrl Pts',(9.93881283676505,15.2,3.23459652170345));
#200495=CARTESIAN_POINT('Ctrl Pts',(9.94147401258674,15.2,3.23593235732286));
#200496=CARTESIAN_POINT('Ctrl Pts',(9.94413518840844,15.2,3.23726819294227));
#200497=CARTESIAN_POINT('Ctrl Pts',(9.94683613201863,15.2,3.23863348160101));
#200498=CARTESIAN_POINT('Ctrl Pts',(9.94957597908405,15.2,3.24002836113237));
#200499=CARTESIAN_POINT('Ctrl Pts',(9.95231582614947,15.2,3.24142324066374));
#200500=CARTESIAN_POINT('Ctrl Pts',(9.95509458055612,15.2,3.24284770847963));
#200501=CARTESIAN_POINT('Ctrl Pts',(9.95791139670119,15.2,3.24430189409144));
#200502=CARTESIAN_POINT('Ctrl Pts',(9.96072821310213,15.2,3.24575607983533));
#200503=CARTESIAN_POINT('Ctrl Pts',(9.96358309289007,15.2,3.24723998469043));
#200504=CARTESIAN_POINT('Ctrl Pts',(9.96647521513266,15.2,3.24875373035756));
#200505=CARTESIAN_POINT('Ctrl Pts',(9.96936733711254,15.2,3.25026747588719));
#200506=CARTESIAN_POINT('Ctrl Pts',(9.97229669893939,15.2,3.25181106350611));
#200507=CARTESIAN_POINT('Ctrl Pts',(9.97526249808007,15.2,3.25338460994764));
#200508=CARTESIAN_POINT('Ctrl Pts',(9.97822829722075,15.2,3.25495815638917));
#200509=CARTESIAN_POINT('Ctrl Pts',(9.98123053182321,15.2,3.25656166152494));
#200510=CARTESIAN_POINT('Ctrl Pts',(9.98426841896043,15.2,3.25819523904688));
#200511=CARTESIAN_POINT('Ctrl Pts',(9.98730630637357,15.2,3.2598288167172));
#200512=CARTESIAN_POINT('Ctrl Pts',(9.9903798430735,15.2,3.2614924662154));
#200513=CARTESIAN_POINT('Ctrl Pts',(9.9934882616611,15.2,3.26318629380904));
#200514=CARTESIAN_POINT('Ctrl Pts',(9.99659667996637,15.2,3.26488012124881));
#200515=CARTESIAN_POINT('Ctrl Pts',(9.9997399786912,15.2,3.2666041282383));
#200516=CARTESIAN_POINT('Ctrl Pts',(10.0029174070068,15.2,3.2683584165158));
#200517=CARTESIAN_POINT('Ctrl Pts',(10.0066244069007,15.2,3.27040508627912));
#200518=CARTESIAN_POINT('Ctrl Pts',(10.0103778566166,15.2,3.27249297058149));
#200519=CARTESIAN_POINT('Ctrl Pts',(10.0141765904275,15.2,3.27462222536619));
#200520=CARTESIAN_POINT('Ctrl Pts',(10.0174326478106,15.2,3.27644730080122));
#200521=CARTESIAN_POINT('Ctrl Pts',(10.0207219743957,15.2,3.27830277088412));
#200522=CARTESIAN_POINT('Ctrl Pts',(10.02404385104,15.2,3.28018872624074));
#200523=CARTESIAN_POINT('Ctrl Pts',(10.0273657276843,15.2,3.28207468159738));
#200524=CARTESIAN_POINT('Ctrl Pts',(10.0307201547644,15.2,3.28399112417722));
#200525=CARTESIAN_POINT('Ctrl Pts',(10.0341064263891,15.2,3.28593813877105));
#200526=CARTESIAN_POINT('Ctrl Pts',(10.0374926983215,15.2,3.28788515354173));
#200527=CARTESIAN_POINT('Ctrl Pts',(10.0409108153715,15.2,3.28986274291605));
#200528=CARTESIAN_POINT('Ctrl Pts',(10.044360085567,15.2,3.29187098846095));
#200529=CARTESIAN_POINT('Ctrl Pts',(10.0472344772399,15.2,3.29354452632382));
#200530=CARTESIAN_POINT('Ctrl Pts',(10.0501305033909,15.2,3.29523935320601));
#200531=CARTESIAN_POINT('Ctrl Pts',(10.0530477716565,15.2,3.29695551445775));
#200532=CARTESIAN_POINT('Ctrl Pts',(10.0559650399221,15.2,3.29867167570949));
#200533=CARTESIAN_POINT('Ctrl Pts',(10.0589035501853,15.2,3.30040917285603));
#200534=CARTESIAN_POINT('Ctrl Pts',(10.0618629166453,15.2,3.302168048205));
#200535=CARTESIAN_POINT('Ctrl Pts',(10.0654141562683,15.2,3.30427869854707));
#200536=CARTESIAN_POINT('Ctrl Pts',(10.0689954263267,15.2,3.30642013547104));
#200537=CARTESIAN_POINT('Ctrl Pts',(10.0726060711968,15.2,3.30859242964345));
#200538=CARTESIAN_POINT('Ctrl Pts',(10.0756149420312,15.2,3.3104026748529));
#200539=CARTESIAN_POINT('Ctrl Pts',(10.078644213215,15.2,3.31223434765347));
#200540=CARTESIAN_POINT('Ctrl Pts',(10.0816935107161,15.2,3.31408749036292));
#200541=CARTESIAN_POINT('Ctrl Pts',(10.0847428082172,15.2,3.31594063307238));
#200542=CARTESIAN_POINT('Ctrl Pts',(10.0878121321529,15.2,3.31781524422945));
#200543=CARTESIAN_POINT('Ctrl Pts',(10.0909011156419,15.2,3.31971136127012));
#200544=CARTESIAN_POINT('Ctrl Pts',(10.0939900991309,15.2,3.32160747831078));
#200545=CARTESIAN_POINT('Ctrl Pts',(10.0970987406408,15.2,3.32352510248517));
#200546=CARTESIAN_POINT('Ctrl Pts',(10.100226679184,15.2,3.32546426852858));
#200547=CARTESIAN_POINT('Ctrl Pts',(10.1033546177273,15.2,3.327403434572));
#200548=CARTESIAN_POINT('Ctrl Pts',(10.1065018539514,15.2,3.32936414310745));
#200549=CARTESIAN_POINT('Ctrl Pts',(10.109668030689,15.2,3.33134642831755));
#200550=CARTESIAN_POINT('Ctrl Pts',(10.1128342070816,15.2,3.33332871331159));
#200551=CARTESIAN_POINT('Ctrl Pts',(10.1160193233205,15.2,3.33533257472978));
#200552=CARTESIAN_POINT('Ctrl Pts',(10.1192230290809,15.2,3.33735804624334));
#200553=CARTESIAN_POINT('Ctrl Pts',(10.1224267351904,15.2,3.33938351797768));
#200554=CARTESIAN_POINT('Ctrl Pts',(10.1256490317887,15.2,3.34143059796446));
#200555=CARTESIAN_POINT('Ctrl Pts',(10.1288895710927,15.2,3.34349931900435));
#200556=CARTESIAN_POINT('Ctrl Pts',(10.1321301103968,15.2,3.34556804004424));
#200557=CARTESIAN_POINT('Ctrl Pts',(10.1353888930293,15.2,3.3476584018786));
#200558=CARTESIAN_POINT('Ctrl Pts',(10.1386655776363,15.2,3.34977043232983));
#200559=CARTESIAN_POINT('Ctrl Pts',(10.1419422622431,15.2,3.35188246278107));
#200560=CARTESIAN_POINT('Ctrl Pts',(10.1452368494678,15.2,3.35401616384925));
#200561=CARTESIAN_POINT('Ctrl Pts',(10.1485490030083,15.2,3.35617156162571));
#200562=CARTESIAN_POINT('Ctrl Pts',(10.1518611565488,15.2,3.35832695940218));
#200563=CARTESIAN_POINT('Ctrl Pts',(10.1551908747876,15.2,3.36050405526851));
#200564=CARTESIAN_POINT('Ctrl Pts',(10.1585378292311,15.2,3.36270287457292));
#200565=CARTESIAN_POINT('Ctrl Pts',(10.1618847836746,15.2,3.36490169387733));
#200566=CARTESIAN_POINT('Ctrl Pts',(10.165248972552,15.2,3.36712223751011));
#200567=CARTESIAN_POINT('Ctrl Pts',(10.1686300694955,15.2,3.36936452862008));
#200568=CARTESIAN_POINT('Ctrl Pts',(10.1720111664391,15.2,3.37160681973005));
#200569=CARTESIAN_POINT('Ctrl Pts',(10.1754091705048,15.2,3.37387085927725));
#200570=CARTESIAN_POINT('Ctrl Pts',(10.178823760798,15.2,3.37615667102369));
#200571=CARTESIAN_POINT('Ctrl Pts',(10.1822383510913,15.2,3.37844248277012));
#200572=CARTESIAN_POINT('Ctrl Pts',(10.1856695266332,15.2,3.38075006569993));
#200573=CARTESIAN_POINT('Ctrl Pts',(10.1891169710082,15.2,3.38307944174159));
#200574=CARTESIAN_POINT('Ctrl Pts',(10.1918749266585,15.2,3.38494294267648));
#200575=CARTESIAN_POINT('Ctrl Pts',(10.1946432919156,15.2,3.38682039215467));
#200576=CARTESIAN_POINT('Ctrl Pts',(10.1974219096792,15.2,3.38871180025918));
#200577=CARTESIAN_POINT('Ctrl Pts',(10.2002005270642,15.2,3.39060320810599));
#200578=CARTESIAN_POINT('Ctrl Pts',(10.2029893944002,15.2,3.39250857375242));
#200579=CARTESIAN_POINT('Ctrl Pts',(10.2057883532397,15.2,3.39442790771529));
#200580=CARTESIAN_POINT('Ctrl Pts',(10.2085873124604,15.2,3.39634724193967));
#200581=CARTESIAN_POINT('Ctrl Pts',(10.2113963637895,15.2,3.39828054458298));
#200582=CARTESIAN_POINT('Ctrl Pts',(10.2142153489442,15.2,3.40022782480165));
#200583=CARTESIAN_POINT('Ctrl Pts',(10.2170343337147,15.2,3.40217510475501));
#200584=CARTESIAN_POINT('Ctrl Pts',(10.2198632530201,15.2,3.4041363628593));
#200585=CARTESIAN_POINT('Ctrl Pts',(10.2227019505096,15.2,3.40611160686359));
#200586=CARTESIAN_POINT('Ctrl Pts',(10.2255406483859,15.2,3.408086851137));
#200587=CARTESIAN_POINT('Ctrl Pts',(10.228389124582,15.2,3.41007608275244));
#200588=CARTESIAN_POINT('Ctrl Pts',(10.2312472258814,15.2,3.41207930907402));
#200589=CARTESIAN_POINT('Ctrl Pts',(10.2341053267913,15.2,3.41408253512266));
#200590=CARTESIAN_POINT('Ctrl Pts',(10.2369730516617,15.2,3.41609975537043));
#200591=CARTESIAN_POINT('Ctrl Pts',(10.2398502479815,15.2,3.41813097859234));
#200592=CARTESIAN_POINT('Ctrl Pts',(10.2427274446932,15.2,3.42016220209101));
#200593=CARTESIAN_POINT('Ctrl Pts',(10.2456141140672,15.2,3.42220742844416));
#200594=CARTESIAN_POINT('Ctrl Pts',(10.2485101040034,15.2,3.4242666646684));
#200595=CARTESIAN_POINT('Ctrl Pts',(10.251406093545,15.2,3.42632590061207));
#200596=CARTESIAN_POINT('Ctrl Pts',(10.2543114045955,15.2,3.4283991466647));
#200597=CARTESIAN_POINT('Ctrl Pts',(10.2572258863354,15.2,3.43048640993047));
#200598=CARTESIAN_POINT('Ctrl Pts',(10.2601403684724,15.2,3.43257367348062));
#200599=CARTESIAN_POINT('Ctrl Pts',(10.263064022471,15.2,3.43467495324568));
#200600=CARTESIAN_POINT('Ctrl Pts',(10.2659966997981,15.2,3.43679025547299));
#200601=CARTESIAN_POINT('Ctrl Pts',(10.2689293767256,15.2,3.43890555741208));
#200602=CARTESIAN_POINT('Ctrl Pts',(10.2718710771846,15.2,3.44103488257895));
#200603=CARTESIAN_POINT('Ctrl Pts',(10.2748216547758,15.2,3.4431782371245));
#200604=CARTESIAN_POINT('Ctrl Pts',(10.277772232769,15.2,3.44532159196209));
#200605=CARTESIAN_POINT('Ctrl Pts',(10.2807316889517,15.2,3.44747897584539));
#200606=CARTESIAN_POINT('Ctrl Pts',(10.2836998762936,15.2,3.44965039275141));
#200607=CARTESIAN_POINT('Ctrl Pts',(10.2866680632311,15.2,3.45182180936158));
#200608=CARTESIAN_POINT('Ctrl Pts',(10.2896449825456,15.2,3.45400726194379));
#200609=CARTESIAN_POINT('Ctrl Pts',(10.2926304907451,15.2,3.45620675187366));
#200610=CARTESIAN_POINT('Ctrl Pts',(10.2963623762996,15.2,3.45895611451075));
#200611=CARTESIAN_POINT('Ctrl Pts',(10.3001076799316,15.2,3.46172741288083));
#200612=CARTESIAN_POINT('Ctrl Pts',(10.3038661264583,15.2,3.46452065614291));
#200613=CARTESIAN_POINT('Ctrl Pts',(10.3068728838435,15.2,3.46675525087436));
#200614=CARTESIAN_POINT('Ctrl Pts',(10.309888052704,15.2,3.46900388892616));
#200615=CARTESIAN_POINT('Ctrl Pts',(10.3129114914936,15.2,3.47126657522648));
#200616=CARTESIAN_POINT('Ctrl Pts',(10.3159349298714,15.2,3.4735292612185));
#200617=CARTESIAN_POINT('Ctrl Pts',(10.3189666403995,15.2,3.475805996128));
#200618=CARTESIAN_POINT('Ctrl Pts',(10.3220064807612,15.2,3.47809678188373));
#200619=CARTESIAN_POINT('Ctrl Pts',(10.3258062815241,15.2,3.48096026431247));
#200620=CARTESIAN_POINT('Ctrl Pts',(10.3296187892507,15.2,3.48384570220479));
#200621=CARTESIAN_POINT('Ctrl Pts',(10.3334437317496,15.2,3.48675309991132));
#200622=CARTESIAN_POINT('Ctrl Pts',(10.3365036859155,15.2,3.4890790182033));
#200623=CARTESIAN_POINT('Ctrl Pts',(10.3395716014204,15.2,3.49141899217916));
#200624=CARTESIAN_POINT('Ctrl Pts',(10.3426473382687,15.2,3.49377302298487));
#200625=CARTESIAN_POINT('Ctrl Pts',(10.3464920091195,15.2,3.49671556133164));
#200626=CARTESIAN_POINT('Ctrl Pts',(10.3503489042913,15.2,3.49968006414424));
#200627=CARTESIAN_POINT('Ctrl Pts',(10.3542177599863,15.2,3.50266653497871));
#200628=CARTESIAN_POINT('Ctrl Pts',(10.3573128442894,15.2,3.50505571145097));
#200629=CARTESIAN_POINT('Ctrl Pts',(10.3604155820853,15.2,3.50745894693709));
#200630=CARTESIAN_POINT('Ctrl Pts',(10.3635258429414,15.2,3.50987624340471));
#200631=CARTESIAN_POINT('Ctrl Pts',(10.3666361042213,15.2,3.51229354020169));
#200632=CARTESIAN_POINT('Ctrl Pts',(10.3697538852342,15.2,3.51472489777383));
#200633=CARTESIAN_POINT('Ctrl Pts',(10.372879056752,15.2,3.5171703172516));
#200634=CARTESIAN_POINT('Ctrl Pts',(10.3767855209365,15.2,3.52022709143221));
#200635=CARTESIAN_POINT('Ctrl Pts',(10.3807035303564,15.2,3.52330583797949));
#200636=CARTESIAN_POINT('Ctrl Pts',(10.3846328295236,15.2,3.52640655624451));
#200637=CARTESIAN_POINT('Ctrl Pts',(10.3877762686004,15.2,3.52888713065374));
#200638=CARTESIAN_POINT('Ctrl Pts',(10.3909269342147,15.2,3.53138176766572));
#200639=CARTESIAN_POINT('Ctrl Pts',(10.3940846947336,15.2,3.5338904668481));
#200640=CARTESIAN_POINT('Ctrl Pts',(10.3972424556828,15.2,3.53639916637228));
#200641=CARTESIAN_POINT('Ctrl Pts',(10.4004073139604,15.2,3.53892192889499));
#200642=CARTESIAN_POINT('Ctrl Pts',(10.4035791394666,15.2,3.54145875303326));
#200643=CARTESIAN_POINT('Ctrl Pts',(10.4067509649728,15.2,3.54399557717152));
#200644=CARTESIAN_POINT('Ctrl Pts',(10.4099297590992,15.2,3.54654646280864));
#200645=CARTESIAN_POINT('Ctrl Pts',(10.4131153933291,15.2,3.54911141089431));
#200646=CARTESIAN_POINT('Ctrl Pts',(10.4163010271249,15.2,3.55167635863051));
#200647=CARTESIAN_POINT('Ctrl Pts',(10.4194935012003,15.2,3.55425536771787));
#200648=CARTESIAN_POINT('Ctrl Pts',(10.4226926897311,15.2,3.55684843623983));
#200649=CARTESIAN_POINT('Ctrl Pts',(10.4258918786977,15.2,3.55944150511511));
#200650=CARTESIAN_POINT('Ctrl Pts',(10.4290977829522,15.2,3.56204863528421));
#200651=CARTESIAN_POINT('Ctrl Pts',(10.4323102765168,15.2,3.5646698234285));
#200652=CARTESIAN_POINT('Ctrl Pts',(10.4355227696438,15.2,3.56729101121566));
#200653=CARTESIAN_POINT('Ctrl Pts',(10.4387418525837,15.2,3.56992625837041));
#200654=CARTESIAN_POINT('Ctrl Pts',(10.4419674009863,15.2,3.57257556154181));
#200655=CARTESIAN_POINT('Ctrl Pts',(10.4451929498283,15.2,3.57522486507418));
#200656=CARTESIAN_POINT('Ctrl Pts',(10.4484249642672,15.2,3.57788822689373));
#200657=CARTESIAN_POINT('Ctrl Pts',(10.4516633219949,15.2,3.58056564189685));
#200658=CARTESIAN_POINT('Ctrl Pts',(10.4549016792813,15.2,3.58324305653518));
#200659=CARTESIAN_POINT('Ctrl Pts',(10.4581463783143,15.2,3.58593452631486));
#200660=CARTESIAN_POINT('Ctrl Pts',(10.4613972999926,15.2,3.58864004803722));
#200661=CARTESIAN_POINT('Ctrl Pts',(10.4646482221138,15.2,3.59134557012821));
#200662=CARTESIAN_POINT('Ctrl Pts',(10.4679053641941,15.2,3.59406514435976));
#200663=CARTESIAN_POINT('Ctrl Pts',(10.4711686064834,15.2,3.59679876723187));
#200664=CARTESIAN_POINT('Ctrl Pts',(10.4744318483282,15.2,3.59953238973153));
#200665=CARTESIAN_POINT('Ctrl Pts',(10.4777011909821,15.2,3.60228006188829));
#200666=CARTESIAN_POINT('Ctrl Pts',(10.4809765142663,15.2,3.60504177913259));
#200667=CARTESIAN_POINT('Ctrl Pts',(10.4850706687063,15.2,3.60849392597017));
#200668=CARTESIAN_POINT('Ctrl Pts',(10.4891741670593,15.2,3.61196801906145));
#200669=CARTESIAN_POINT('Ctrl Pts',(10.4932867794893,15.2,3.61546405225475));
#200670=CARTESIAN_POINT('Ctrl Pts',(10.4965768696127,15.2,3.61826087896182));
#200671=CARTESIAN_POINT('Ctrl Pts',(10.4998727905118,15.2,3.62107174701222));
#200672=CARTESIAN_POINT('Ctrl Pts',(10.5031744268032,15.2,3.62389665122267));
#200673=CARTESIAN_POINT('Ctrl Pts',(10.5064760626448,15.2,3.62672155504822));
#200674=CARTESIAN_POINT('Ctrl Pts',(10.5097834127778,15.2,3.62956049679738));
#200675=CARTESIAN_POINT('Ctrl Pts',(10.5130963627276,15.2,3.63241347009436));
#200676=CARTESIAN_POINT('Ctrl Pts',(10.5164093131287,15.2,3.63526644378005));
#200677=CARTESIAN_POINT('Ctrl Pts',(10.5197278611485,15.2,3.63813345147489));
#200678=CARTESIAN_POINT('Ctrl Pts',(10.5230518914967,15.2,3.64101448624392));
#200679=CARTESIAN_POINT('Ctrl Pts',(10.5272069292055,15.2,3.64461577950895));
#200680=CARTESIAN_POINT('Ctrl Pts',(10.5313705333668,15.2,3.64823899082619));
#200681=CARTESIAN_POINT('Ctrl Pts',(10.5355424810062,15.2,3.65188411152179));
#200682=CARTESIAN_POINT('Ctrl Pts',(10.5388800388448,15.2,3.65480020783988));
#200683=CARTESIAN_POINT('Ctrl Pts',(10.5422229357793,15.2,3.65773032583704));
#200684=CARTESIAN_POINT('Ctrl Pts',(10.5455710585058,15.2,3.66067445913113));
#200685=CARTESIAN_POINT('Ctrl Pts',(10.5480821506647,15.2,3.66288255920198));
#200686=CARTESIAN_POINT('Ctrl Pts',(10.5505961827764,15.2,3.66509854378035));
#200687=CARTESIAN_POINT('Ctrl Pts',(10.5531131072262,15.2,3.66732240924013));
#200688=CARTESIAN_POINT('Ctrl Pts',(10.5556300321333,15.2,3.66954627510392));
#200689=CARTESIAN_POINT('Ctrl Pts',(10.5581498480828,15.2,3.67177802326162));
#200690=CARTESIAN_POINT('Ctrl Pts',(10.5606725095749,15.2,3.67401765050484));
#200691=CARTESIAN_POINT('Ctrl Pts',(10.5631951706086,15.2,3.6762572773412));
#200692=CARTESIAN_POINT('Ctrl Pts',(10.5657206764339,15.2,3.67850478199383));
#200693=CARTESIAN_POINT('Ctrl Pts',(10.5682489799672,15.2,3.68076016345423));
#200694=CARTESIAN_POINT('Ctrl Pts',(10.5707772835006,15.2,3.68301554491463));
#200695=CARTESIAN_POINT('Ctrl Pts',(10.5733083845828,15.2,3.68527880454083));
#200696=CARTESIAN_POINT('Ctrl Pts',(10.5758422375022,15.2,3.68754993646866));
#200697=CARTESIAN_POINT('Ctrl Pts',(10.5783760904217,15.2,3.68982106839649));
#200698=CARTESIAN_POINT('Ctrl Pts',(10.580912693095,15.2,3.6921000743706));
#200699=CARTESIAN_POINT('Ctrl Pts',(10.5834520019726,15.2,3.69438695075619));
#200700=CARTESIAN_POINT('Ctrl Pts',(10.5859913108502,15.2,3.69667382714178));
#200701=CARTESIAN_POINT('Ctrl Pts',(10.5885333233486,15.2,3.69896857466676));
#200702=CARTESIAN_POINT('Ctrl Pts',(10.5910779952976,15.2,3.70127118999908));
#200703=CARTESIAN_POINT('Ctrl Pts',(10.5944708915378,15.2,3.70434134405438));
#200704=CARTESIAN_POINT('Ctrl Pts',(10.5978685123674,15.2,3.70742548581691));
#200705=CARTESIAN_POINT('Ctrl Pts',(10.6012707520531,15.2,3.71052360798667));
#200706=CARTESIAN_POINT('Ctrl Pts',(10.6046729912753,15.2,3.7136217297343));
#200707=CARTESIAN_POINT('Ctrl Pts',(10.6080798480943,15.2,3.71673383070532));
#200708=CARTESIAN_POINT('Ctrl Pts',(10.6114912142633,15.2,3.71985990577139));
#200709=CARTESIAN_POINT('Ctrl Pts',(10.614902580897,15.2,3.72298598126339));
#200710=CARTESIAN_POINT('Ctrl Pts',(10.6183184581234,15.2,3.72612602937675));
#200711=CARTESIAN_POINT('Ctrl Pts',(10.6217387372546,15.2,3.72928004271624));
#200712=CARTESIAN_POINT('Ctrl Pts',(10.6243039463699,15.2,3.73164555250598));
#200713=CARTESIAN_POINT('Ctrl Pts',(10.6268716324766,15.2,3.73401891701978));
#200714=CARTESIAN_POINT('Ctrl Pts',(10.6294417504666,15.2,3.73640013430827));
#200715=CARTESIAN_POINT('Ctrl Pts',(10.6328685747645,15.2,3.73957509098132));
#200716=CARTESIAN_POINT('Ctrl Pts',(10.6362997213601,15.2,3.74276400716153));
#200717=CARTESIAN_POINT('Ctrl Pts',(10.6397350852699,15.2,3.74596687328194));
#200718=CARTESIAN_POINT('Ctrl Pts',(10.6431704487117,15.2,3.74916973896596));
#200719=CARTESIAN_POINT('Ctrl Pts',(10.6466100307746,15.2,3.75238655669723));
#200720=CARTESIAN_POINT('Ctrl Pts',(10.6500537247309,15.2,3.75561731578107));
#200721=CARTESIAN_POINT('Ctrl Pts',(10.6526364953155,15.2,3.75804038520399));
#200722=CARTESIAN_POINT('Ctrl Pts',(10.6552215796288,15.2,3.76047129735686));
#200723=CARTESIAN_POINT('Ctrl Pts',(10.6578089327429,15.2,3.76291004822591));
#200724=CARTESIAN_POINT('Ctrl Pts',(10.6603962858571,15.2,3.76534879909495));
#200725=CARTESIAN_POINT('Ctrl Pts',(10.6629859089127,15.2,3.76779538893845));
#200726=CARTESIAN_POINT('Ctrl Pts',(10.6655777579849,15.2,3.77024981422321));
#200727=CARTESIAN_POINT('Ctrl Pts',(10.668169607528,15.2,3.77270423995386));
#200728=CARTESIAN_POINT('Ctrl Pts',(10.6707636821883,15.2,3.7751665000117));
#200729=CARTESIAN_POINT('Ctrl Pts',(10.6733599393159,15.2,3.77763659178842));
#200730=CARTESIAN_POINT('Ctrl Pts',(10.6768216147,15.2,3.78093004674283));
#200731=CARTESIAN_POINT('Ctrl Pts',(10.6802871704613,15.2,3.78423742299263));
#200732=CARTESIAN_POINT('Ctrl Pts',(10.683756503733,15.2,3.78755871322021));
#200733=CARTESIAN_POINT('Ctrl Pts',(10.686358503805,15.2,3.79004968100403));
#200734=CARTESIAN_POINT('Ctrl Pts',(10.6889626283271,15.2,3.79254847424846));
#200735=CARTESIAN_POINT('Ctrl Pts',(10.6915688354874,15.2,3.79505508969837));
#200736=CARTESIAN_POINT('Ctrl Pts',(10.6941750426476,15.2,3.79756170514828));
#200737=CARTESIAN_POINT('Ctrl Pts',(10.696783330676,15.2,3.80007614262613));
#200738=CARTESIAN_POINT('Ctrl Pts',(10.6993936592059,15.2,3.80259839745008));
#200739=CARTESIAN_POINT('Ctrl Pts',(10.70200398821,15.2,3.80512065273224));
#200740=CARTESIAN_POINT('Ctrl Pts',(10.704616355923,15.2,3.80765072573329));
#200741=CARTESIAN_POINT('Ctrl Pts',(10.7072307205532,15.2,3.81018861201987));
#200742=CARTESIAN_POINT('Ctrl Pts',(10.7098450847085,15.2,3.81272649784541));
#200743=CARTESIAN_POINT('Ctrl Pts',(10.712461446147,15.2,3.81527219680382));
#200744=CARTESIAN_POINT('Ctrl Pts',(10.7150797622604,15.2,3.81782570600339));
#200745=CARTESIAN_POINT('Ctrl Pts',(10.7176980783737,15.2,3.82037921520297));
#200746=CARTESIAN_POINT('Ctrl Pts',(10.720318349219,15.2,3.82294053275057));
#200747=CARTESIAN_POINT('Ctrl Pts',(10.7229405337606,15.2,3.82550965554393));
#200748=CARTESIAN_POINT('Ctrl Pts',(10.7255627183023,15.2,3.82807877833729));
#200749=CARTESIAN_POINT('Ctrl Pts',(10.7281868148977,15.2,3.83065570584646));
#200750=CARTESIAN_POINT('Ctrl Pts',(10.7308127829809,15.2,3.83324043322259));
#200751=CARTESIAN_POINT('Ctrl Pts',(10.7343140740765,15.2,3.83668673670379));
#200752=CARTESIAN_POINT('Ctrl Pts',(10.737818690682,15.2,3.84014690793831));
#200753=CARTESIAN_POINT('Ctrl Pts',(10.7413265358735,15.2,3.84362093535128));
#200754=CARTESIAN_POINT('Ctrl Pts',(10.744834380587,15.2,3.84709496229092));
#200755=CARTESIAN_POINT('Ctrl Pts',(10.7483454538974,15.2,3.85058284616485));
#200756=CARTESIAN_POINT('Ctrl Pts',(10.751859659221,15.2,3.8540845744888));
#200757=CARTESIAN_POINT('Ctrl Pts',(10.7553738650234,15.2,3.85758630328985));
#200758=CARTESIAN_POINT('Ctrl Pts',(10.7588912026622,15.2,3.86110187746449));
#200759=CARTESIAN_POINT('Ctrl Pts',(10.7624115707524,15.2,3.86463128627882));
#200760=CARTESIAN_POINT('Ctrl Pts',(10.7650518465803,15.2,3.86727834264912));
#200761=CARTESIAN_POINT('Ctrl Pts',(10.7676938270174,15.2,3.86993317980302));
#200762=CARTESIAN_POINT('Ctrl Pts',(10.7703374732548,15.2,3.87259579408196));
#200763=CARTESIAN_POINT('Ctrl Pts',(10.7729811194922,15.2,3.87525840836091));
#200764=CARTESIAN_POINT('Ctrl Pts',(10.7756264323628,15.2,3.87792879866391));
#200765=CARTESIAN_POINT('Ctrl Pts',(10.7782733755166,15.2,3.88060696148326));
#200766=CARTESIAN_POINT('Ctrl Pts',(10.7809203186704,15.2,3.88328512430262));
#200767=CARTESIAN_POINT('Ctrl Pts',(10.7835688926242,15.2,3.88597105973833));
#200768=CARTESIAN_POINT('Ctrl Pts',(10.7862190496944,15.2,3.88866476197311));
#200769=CARTESIAN_POINT('Ctrl Pts',(10.7897525927757,15.2,3.89225636527905));
#200770=CARTESIAN_POINT('Ctrl Pts',(10.7932889486047,15.2,3.89586177510982));
#200771=CARTESIAN_POINT('Ctrl Pts',(10.7968280095302,15.2,3.89948097876684));
#200772=CARTESIAN_POINT('Ctrl Pts',(10.7994823049832,15.2,3.90219538126305));
#200773=CARTESIAN_POINT('Ctrl Pts',(10.8021381228242,15.2,3.90491754265944));
#200774=CARTESIAN_POINT('Ctrl Pts',(10.8047954450759,15.2,3.90764746004429));
#200775=CARTESIAN_POINT('Ctrl Pts',(10.8074527673276,15.2,3.91037737742914));
#200776=CARTESIAN_POINT('Ctrl Pts',(10.8101115945167,15.2,3.91311504950123));
#200777=CARTESIAN_POINT('Ctrl Pts',(10.8127719249999,15.2,3.91586047999999));
#200778=CARTESIAN_POINT('Ctrl Pts',(9.86852965799994,12.2,3.20199116299998));
#200779=CARTESIAN_POINT('Ctrl Pts',(9.87017542602826,12.2,3.2026865729514));
#200780=CARTESIAN_POINT('Ctrl Pts',(9.87187175395476,12.2,3.20340918505387));
#200781=CARTESIAN_POINT('Ctrl Pts',(9.87361750382533,12.2,3.20415921017613));
#200782=CARTESIAN_POINT('Ctrl Pts',(9.8753716725842,12.2,3.20491285229865));
#200783=CARTESIAN_POINT('Ctrl Pts',(9.87717573909119,12.2,3.20569417515048));
#200784=CARTESIAN_POINT('Ctrl Pts',(9.87902857820422,12.2,3.20650338931995));
#200785=CARTESIAN_POINT('Ctrl Pts',(9.88088141714894,12.2,3.20731260341592));
#200786=CARTESIAN_POINT('Ctrl Pts',(9.88278302753734,12.2,3.20814970993136));
#200787=CARTESIAN_POINT('Ctrl Pts',(9.88473231729986,12.2,3.20901491173327));
#200788=CARTESIAN_POINT('Ctrl Pts',(9.88668160706237,12.2,3.20988011353516));
#200789=CARTESIAN_POINT('Ctrl Pts',(9.88867857432713,12.2,3.21077340710827));
#200790=CARTESIAN_POINT('Ctrl Pts',(9.89072215651895,12.2,3.21169499186919));
#200791=CARTESIAN_POINT('Ctrl Pts',(9.8927657388964,12.2,3.21261657671382));
#200792=CARTESIAN_POINT('Ctrl Pts',(9.89485593697986,12.2,3.21356644793466));
#200793=CARTESIAN_POINT('Ctrl Pts',(9.89699171626601,12.2,3.21454479382324));
#200794=CARTESIAN_POINT('Ctrl Pts',(9.89912749535818,12.2,3.21552313962297));
#200795=CARTESIAN_POINT('Ctrl Pts',(9.90130885312988,12.2,3.2165299600416));
#200796=CARTESIAN_POINT('Ctrl Pts',(9.90353478647588,12.2,3.21756543175874));
#200797=CARTESIAN_POINT('Ctrl Pts',(9.90576071982188,12.2,3.21860090347588));
#200798=CARTESIAN_POINT('Ctrl Pts',(9.90803122617659,12.2,3.21966502636479));
#200799=CARTESIAN_POINT('Ctrl Pts',(9.9103453265906,12.2,3.22075797015716));
#200800=CARTESIAN_POINT('Ctrl Pts',(9.91265942721481,12.2,3.22185091404879));
#200801=CARTESIAN_POINT('Ctrl Pts',(9.91501712121113,12.2,3.22297268105235));
#200802=CARTESIAN_POINT('Ctrl Pts',(9.91741745401152,12.2,3.22412343086704));
#200803=CARTESIAN_POINT('Ctrl Pts',(9.91981778659389,12.2,3.2252741805772));
#200804=CARTESIAN_POINT('Ctrl Pts',(9.9222607575406,12.2,3.22645391462526));
#200805=CARTESIAN_POINT('Ctrl Pts',(9.9247454351188,12.2,3.22766278908261));
#200806=CARTESIAN_POINT('Ctrl Pts',(9.92723011269699,12.2,3.22887166353995));
#200807=CARTESIAN_POINT('Ctrl Pts',(9.92975649721356,12.2,3.23010967684499));
#200808=CARTESIAN_POINT('Ctrl Pts',(9.93232368086846,12.2,3.23137697863099));
#200809=CARTESIAN_POINT('Ctrl Pts',(9.93489086452338,12.2,3.23264428041699));
#200810=CARTESIAN_POINT('Ctrl Pts',(9.93749884761017,12.2,3.23394087148892));
#200811=CARTESIAN_POINT('Ctrl Pts',(9.94014674251127,12.2,3.2352668931054));
#200812=CARTESIAN_POINT('Ctrl Pts',(9.94279463765287,12.2,3.23659291484234));
#200813=CARTESIAN_POINT('Ctrl Pts',(9.94548244668999,12.2,3.23794836711543));
#200814=CARTESIAN_POINT('Ctrl Pts',(9.94820930192366,12.2,3.23933338685888));
#200815=CARTESIAN_POINT('Ctrl Pts',(9.95093615690962,12.2,3.24071840647652));
#200816=CARTESIAN_POINT('Ctrl Pts',(9.95370205967116,12.2,3.24213299372027));
#200817=CARTESIAN_POINT('Ctrl Pts',(9.9565061647486,12.2,3.24357727725761));
#200818=CARTESIAN_POINT('Ctrl Pts',(9.95931026982602,12.2,3.24502156079496));
#200819=CARTESIAN_POINT('Ctrl Pts',(9.96215257705149,12.2,3.2464955419427));
#200820=CARTESIAN_POINT('Ctrl Pts',(9.96503226119433,12.2,3.24799934355269));
#200821=CARTESIAN_POINT('Ctrl Pts',(9.96791194559875,12.2,3.24950314529928));
#200822=CARTESIAN_POINT('Ctrl Pts',(9.97082900750678,12.2,3.25103676921541));
#200823=CARTESIAN_POINT('Ctrl Pts',(9.97378263891934,12.2,3.25260033280194));
#200824=CARTESIAN_POINT('Ctrl Pts',(9.97673627006362,12.2,3.25416389624644));
#200825=CARTESIAN_POINT('Ctrl Pts',(9.97972647011979,12.2,3.25575739949255));
#200826=CARTESIAN_POINT('Ctrl Pts',(9.98275245044018,12.2,3.25738095602419));
#200827=CARTESIAN_POINT('Ctrl Pts',(9.98577843076056,12.2,3.25900451255585));
#200828=CARTESIAN_POINT('Ctrl Pts',(9.98884019302724,12.2,3.2606581238213));
#200829=CARTESIAN_POINT('Ctrl Pts',(9.99193696241234,12.2,3.26234189434141));
#200830=CARTESIAN_POINT('Ctrl Pts',(9.99503373207875,12.2,3.26402566501445));
#200831=CARTESIAN_POINT('Ctrl Pts',(9.99816550995689,12.2,3.26573959779312));
#200832=CARTESIAN_POINT('Ctrl Pts',(10.0013315407896,12.2,3.26748379539373));
#200833=CARTESIAN_POINT('Ctrl Pts',(10.0044975713347,12.2,3.26922799283592));
#200834=CARTESIAN_POINT('Ctrl Pts',(10.0076978547174,12.2,3.27100245274884));
#200835=CARTESIAN_POINT('Ctrl Pts',(10.0109316502666,12.2,3.27280727701659));
#200836=CARTESIAN_POINT('Ctrl Pts',(10.0141654458157,12.2,3.27461210128435));
#200837=CARTESIAN_POINT('Ctrl Pts',(10.0174327549627,12.2,3.27644728646254));
#200838=CARTESIAN_POINT('Ctrl Pts',(10.0207328509224,12.2,3.27831292881953));
#200839=CARTESIAN_POINT('Ctrl Pts',(10.0240329471819,12.2,3.28017857134599));
#200840=CARTESIAN_POINT('Ctrl Pts',(10.0273658333144,12.2,3.28207466795285));
#200841=CARTESIAN_POINT('Ctrl Pts',(10.0307307963333,12.2,3.28400131139327));
#200842=CARTESIAN_POINT('Ctrl Pts',(10.0340957590466,12.2,3.28592795465869));
#200843=CARTESIAN_POINT('Ctrl Pts',(10.0374928008687,12.2,3.2878851426723));
#200844=CARTESIAN_POINT('Ctrl Pts',(10.0409212255098,12.2,3.28987295902584));
#200845=CARTESIAN_POINT('Ctrl Pts',(10.0443496501508,12.2,3.29186077537937));
#200846=CARTESIAN_POINT('Ctrl Pts',(10.0478094545213,12.2,3.29387922191417));
#200847=CARTESIAN_POINT('Ctrl Pts',(10.0512999620598,12.2,3.29592837717172));
#200848=CARTESIAN_POINT('Ctrl Pts',(10.0542087184476,12.2,3.29763600661505));
#200849=CARTESIAN_POINT('Ctrl Pts',(10.0571387936914,12.2,3.29936496256449));
#200850=CARTESIAN_POINT('Ctrl Pts',(10.0600898020237,12.2,3.30111528791059));
#200851=CARTESIAN_POINT('Ctrl Pts',(10.0630408103559,12.2,3.30286561325669));
#200852=CARTESIAN_POINT('Ctrl Pts',(10.0660127511514,12.2,3.30463730991309));
#200853=CARTESIAN_POINT('Ctrl Pts',(10.0690052419983,12.2,3.30643041853229));
#200854=CARTESIAN_POINT('Ctrl Pts',(10.0719977328451,12.2,3.30822352715149));
#200855=CARTESIAN_POINT('Ctrl Pts',(10.0750107736166,12.2,3.31003804840549));
#200856=CARTESIAN_POINT('Ctrl Pts',(10.0780439902832,12.2,3.3118740220166));
#200857=CARTESIAN_POINT('Ctrl Pts',(10.0810772069499,12.2,3.31370999562771));
#200858=CARTESIAN_POINT('Ctrl Pts',(10.0841305984486,12.2,3.31556742342013));
#200859=CARTESIAN_POINT('Ctrl Pts',(10.0872037952682,12.2,3.31744634127596));
#200860=CARTESIAN_POINT('Ctrl Pts',(10.0902769920878,12.2,3.31932525913178));
#200861=CARTESIAN_POINT('Ctrl Pts',(10.0933699950748,12.2,3.32122566901908));
#200862=CARTESIAN_POINT('Ctrl Pts',(10.0964824384786,12.2,3.32314760686743));
#200863=CARTESIAN_POINT('Ctrl Pts',(10.0995948818824,12.2,3.32506954471577));
#200864=CARTESIAN_POINT('Ctrl Pts',(10.1027267670162,12.2,3.32701301044966));
#200865=CARTESIAN_POINT('Ctrl Pts',(10.1058777331978,12.2,3.32897803989524));
#200866=CARTESIAN_POINT('Ctrl Pts',(10.1090286993793,12.2,3.33094306934082));
#200867=CARTESIAN_POINT('Ctrl Pts',(10.1121987494873,12.2,3.33292966206464));
#200868=CARTESIAN_POINT('Ctrl Pts',(10.1153875281201,12.2,3.33493785154146));
#200869=CARTESIAN_POINT('Ctrl Pts',(10.118576306753,12.2,3.33694604101829));
#200870=CARTESIAN_POINT('Ctrl Pts',(10.1217838154981,12.2,3.33897582624982));
#200871=CARTESIAN_POINT('Ctrl Pts',(10.1250097041802,12.2,3.34102723979325));
#200872=CARTESIAN_POINT('Ctrl Pts',(10.1282355928622,12.2,3.3430786533367));
#200873=CARTESIAN_POINT('Ctrl Pts',(10.1314798631418,12.2,3.34515169548326));
#200874=CARTESIAN_POINT('Ctrl Pts',(10.1347421716849,12.2,3.34724639499893));
#200875=CARTESIAN_POINT('Ctrl Pts',(10.1380044798725,12.2,3.34934109428628));
#200876=CARTESIAN_POINT('Ctrl Pts',(10.1412848258294,12.2,3.35145745274398));
#200877=CARTESIAN_POINT('Ctrl Pts',(10.1445828723435,12.2,3.35359549695362));
#200878=CARTESIAN_POINT('Ctrl Pts',(10.1478809192171,12.2,3.35573354139629));
#200879=CARTESIAN_POINT('Ctrl Pts',(10.1511966652375,12.2,3.35789327308303));
#200880=CARTESIAN_POINT('Ctrl Pts',(10.1545297780139,12.2,3.36007471745627));
#200881=CARTESIAN_POINT('Ctrl Pts',(10.1578628907903,12.2,3.36225616182951));
#200882=CARTESIAN_POINT('Ctrl Pts',(10.1612133712775,12.2,3.3644593193885));
#200883=CARTESIAN_POINT('Ctrl Pts',(10.1645808898178,12.2,3.36668421619226));
#200884=CARTESIAN_POINT('Ctrl Pts',(10.167948408358,12.2,3.36890911299601));
#200885=CARTESIAN_POINT('Ctrl Pts',(10.171332964403,12.2,3.37115574858598));
#200886=CARTESIAN_POINT('Ctrl Pts',(10.1747342341551,12.2,3.37342414571168));
#200887=CARTESIAN_POINT('Ctrl Pts',(10.1781355039072,12.2,3.37569254283738));
#200888=CARTESIAN_POINT('Ctrl Pts',(10.1815534883263,12.2,3.37798270380001));
#200889=CARTESIAN_POINT('Ctrl Pts',(10.1849878670754,12.2,3.38029464963219));
#200890=CARTESIAN_POINT('Ctrl Pts',(10.1884222458245,12.2,3.38260659546438));
#200891=CARTESIAN_POINT('Ctrl Pts',(10.1918730184574,12.2,3.38494032500271));
#200892=CARTESIAN_POINT('Ctrl Pts',(10.1953398705399,12.2,3.38729586111267));
#200893=CARTESIAN_POINT('Ctrl Pts',(10.1981133523571,12.2,3.38918029010334));
#200894=CARTESIAN_POINT('Ctrl Pts',(10.2008971258154,12.2,3.39107867539597));
#200895=CARTESIAN_POINT('Ctrl Pts',(10.2036910291637,12.2,3.39299102631917));
#200896=CARTESIAN_POINT('Ctrl Pts',(10.2064849321313,12.2,3.3949033769818));
#200897=CARTESIAN_POINT('Ctrl Pts',(10.2092889672229,12.2,3.39682969297042));
#200898=CARTESIAN_POINT('Ctrl Pts',(10.2121029747699,12.2,3.39876998486644));
#200899=CARTESIAN_POINT('Ctrl Pts',(10.2149169827004,12.2,3.40071027702682));
#200900=CARTESIAN_POINT('Ctrl Pts',(10.2177409643432,12.2,3.40266454405278));
#200901=CARTESIAN_POINT('Ctrl Pts',(10.2205747634983,12.2,3.40463279616097));
#200902=CARTESIAN_POINT('Ctrl Pts',(10.2234085622673,12.2,3.40660104800098));
#200903=CARTESIAN_POINT('Ctrl Pts',(10.2262521773969,12.2,3.40858328336113));
#200904=CARTESIAN_POINT('Ctrl Pts',(10.2291054563609,12.2,3.41057951268534));
#200905=CARTESIAN_POINT('Ctrl Pts',(10.2319587357137,12.2,3.41257574228154));
#200906=CARTESIAN_POINT('Ctrl Pts',(10.2348216774777,12.2,3.41458596461265));
#200907=CARTESIAN_POINT('Ctrl Pts',(10.2376941293015,12.2,3.41661018689054));
#200908=CARTESIAN_POINT('Ctrl Pts',(10.2405665807339,12.2,3.41863440889263));
#200909=CARTESIAN_POINT('Ctrl Pts',(10.2434485414701,12.2,3.42067263263917));
#200910=CARTESIAN_POINT('Ctrl Pts',(10.2463398610105,12.2,3.4227248639144));
#200911=CARTESIAN_POINT('Ctrl Pts',(10.2492311809449,12.2,3.42477709546924));
#200912=CARTESIAN_POINT('Ctrl Pts',(10.252131859969,12.2,3.42684333603682));
#200913=CARTESIAN_POINT('Ctrl Pts',(10.2550417472519,12.2,3.42892359099302));
#200914=CARTESIAN_POINT('Ctrl Pts',(10.2579516341384,12.2,3.43100384566577));
#200915=CARTESIAN_POINT('Ctrl Pts',(10.2608707290809,12.2,3.43309811621235));
#200916=CARTESIAN_POINT('Ctrl Pts',(10.2637988852295,12.2,3.43520640737189));
#200917=CARTESIAN_POINT('Ctrl Pts',(10.266727041777,12.2,3.43731469881869));
#200918=CARTESIAN_POINT('Ctrl Pts',(10.2696642586838,12.2,3.43943701172515));
#200919=CARTESIAN_POINT('Ctrl Pts',(10.2726103887332,12.2,3.44157335200826));
#200920=CARTESIAN_POINT('Ctrl Pts',(10.2755565187827,12.2,3.44370969229137));
#200921=CARTESIAN_POINT('Ctrl Pts',(10.2785115630943,12.2,3.44586006162332));
#200922=CARTESIAN_POINT('Ctrl Pts',(10.2814753757012,12.2,3.44802446185382));
#200923=CARTESIAN_POINT('Ctrl Pts',(10.2844391879042,12.2,3.45018886178941));
#200924=CARTESIAN_POINT('Ctrl Pts',(10.2874117675698,12.2,3.45236729555388));
#200925=CARTESIAN_POINT('Ctrl Pts',(10.2903929725062,12.2,3.45455976677344));
#200926=CARTESIAN_POINT('Ctrl Pts',(10.2933741778489,12.2,3.45675223829172));
#200927=CARTESIAN_POINT('Ctrl Pts',(10.296364006512,12.2,3.45895874696276));
#200928=CARTESIAN_POINT('Ctrl Pts',(10.2993623177318,12.2,3.461179297863));
#200929=CARTESIAN_POINT('Ctrl Pts',(10.3023606285431,12.2,3.46339984846069));
#200930=CARTESIAN_POINT('Ctrl Pts',(10.3053674207616,12.2,3.46563444186764));
#200931=CARTESIAN_POINT('Ctrl Pts',(10.3083825537368,12.2,3.46788308101624));
#200932=CARTESIAN_POINT('Ctrl Pts',(10.3113976871228,12.2,3.4701317204712));
#200933=CARTESIAN_POINT('Ctrl Pts',(10.3144211607142,12.2,3.47239440649412));
#200934=CARTESIAN_POINT('Ctrl Pts',(10.3174528361982,12.2,3.47467114212204));
#200935=CARTESIAN_POINT('Ctrl Pts',(10.3204845112692,12.2,3.47694787743977));
#200936=CARTESIAN_POINT('Ctrl Pts',(10.3235243854922,12.2,3.47923866205654));
#200937=CARTESIAN_POINT('Ctrl Pts',(10.3265723237425,12.2,3.48154349931164));
#200938=CARTESIAN_POINT('Ctrl Pts',(10.329620262408,12.2,3.48384833688077));
#200939=CARTESIAN_POINT('Ctrl Pts',(10.3326762624274,12.2,3.48616722819883));
#200940=CARTESIAN_POINT('Ctrl Pts',(10.3357401884838,12.2,3.48850017438245));
#200941=CARTESIAN_POINT('Ctrl Pts',(10.3388041141227,12.2,3.49083312024821));
#200942=CARTESIAN_POINT('Ctrl Pts',(10.3418759651823,12.2,3.49318012216704));
#200943=CARTESIAN_POINT('Ctrl Pts',(10.3449556050281,12.2,3.49554118142408));
#200944=CARTESIAN_POINT('Ctrl Pts',(10.3480352452935,12.2,3.4979022410028));
#200945=CARTESIAN_POINT('Ctrl Pts',(10.3511226752616,12.2,3.50027735818093));
#200946=CARTESIAN_POINT('Ctrl Pts',(10.3542177599863,12.2,3.50266653497871));
#200947=CARTESIAN_POINT('Ctrl Pts',(10.3573128442894,12.2,3.50505571145097));
#200948=CARTESIAN_POINT('Ctrl Pts',(10.3604155820853,12.2,3.50745894693709));
#200949=CARTESIAN_POINT('Ctrl Pts',(10.3635258429414,12.2,3.50987624340471));
#200950=CARTESIAN_POINT('Ctrl Pts',(10.3666361042213,12.2,3.51229354020168));
#200951=CARTESIAN_POINT('Ctrl Pts',(10.3697538852342,12.2,3.51472489777384));
#200952=CARTESIAN_POINT('Ctrl Pts',(10.372879056752,12.2,3.5171703172516));
#200953=CARTESIAN_POINT('Ctrl Pts',(10.3760042278441,12.2,3.51961573639617));
#200954=CARTESIAN_POINT('Ctrl Pts',(10.3791367876884,12.2,3.52207521810194));
#200955=CARTESIAN_POINT('Ctrl Pts',(10.3822766059866,12.2,3.52454876128718));
#200956=CARTESIAN_POINT('Ctrl Pts',(10.3854164247125,12.2,3.52702230480944));
#200957=CARTESIAN_POINT('Ctrl Pts',(10.3885635015752,12.2,3.5295099105108));
#200958=CARTESIAN_POINT('Ctrl Pts',(10.3917177070249,12.2,3.53201157925826));
#200959=CARTESIAN_POINT('Ctrl Pts',(10.3956604636221,12.2,3.53513866502214));
#200960=CARTESIAN_POINT('Ctrl Pts',(10.3996143577999,12.2,3.53828772303325));
#200961=CARTESIAN_POINT('Ctrl Pts',(10.4035791394666,12.2,3.54145875303325));
#200962=CARTESIAN_POINT('Ctrl Pts',(10.4067509649728,12.2,3.54399557717152));
#200963=CARTESIAN_POINT('Ctrl Pts',(10.4099297590992,12.2,3.54654646280864));
#200964=CARTESIAN_POINT('Ctrl Pts',(10.4131153933291,12.2,3.54911141089431));
#200965=CARTESIAN_POINT('Ctrl Pts',(10.4163010271249,12.2,3.55167635863051));
#200966=CARTESIAN_POINT('Ctrl Pts',(10.4194935012003,12.2,3.55425536771786));
#200967=CARTESIAN_POINT('Ctrl Pts',(10.4226926897311,12.2,3.55684843623983));
#200968=CARTESIAN_POINT('Ctrl Pts',(10.4258918786977,12.2,3.55944150511511));
#200969=CARTESIAN_POINT('Ctrl Pts',(10.4290977829522,12.2,3.56204863528421));
#200970=CARTESIAN_POINT('Ctrl Pts',(10.4323102765168,12.2,3.5646698234285));
#200971=CARTESIAN_POINT('Ctrl Pts',(10.4355227696438,12.2,3.56729101121566));
#200972=CARTESIAN_POINT('Ctrl Pts',(10.4387418525837,12.2,3.56992625837041));
#200973=CARTESIAN_POINT('Ctrl Pts',(10.4419674009863,12.2,3.57257556154181));
#200974=CARTESIAN_POINT('Ctrl Pts',(10.4451929498283,12.2,3.57522486507418));
#200975=CARTESIAN_POINT('Ctrl Pts',(10.4484249642672,12.2,3.57788822689373));
#200976=CARTESIAN_POINT('Ctrl Pts',(10.4516633219949,12.2,3.58056564189685));
#200977=CARTESIAN_POINT('Ctrl Pts',(10.4549016792813,12.2,3.58324305653518));
#200978=CARTESIAN_POINT('Ctrl Pts',(10.4581463783143,12.2,3.58593452631486));
#200979=CARTESIAN_POINT('Ctrl Pts',(10.4613972999926,12.2,3.58864004803722));
#200980=CARTESIAN_POINT('Ctrl Pts',(10.4646482221138,12.2,3.59134557012821));
#200981=CARTESIAN_POINT('Ctrl Pts',(10.4679053641941,12.2,3.59406514435976));
#200982=CARTESIAN_POINT('Ctrl Pts',(10.4711686064834,12.2,3.59679876723187));
#200983=CARTESIAN_POINT('Ctrl Pts',(10.4744318483282,12.2,3.59953238973153));
#200984=CARTESIAN_POINT('Ctrl Pts',(10.4777011909821,12.2,3.60228006188829));
#200985=CARTESIAN_POINT('Ctrl Pts',(10.4809765142663,12.2,3.60504177913259));
#200986=CARTESIAN_POINT('Ctrl Pts',(10.4850706687063,12.2,3.60849392597017));
#200987=CARTESIAN_POINT('Ctrl Pts',(10.4891741670593,12.2,3.61196801906145));
#200988=CARTESIAN_POINT('Ctrl Pts',(10.4932867794893,12.2,3.61546405225475));
#200989=CARTESIAN_POINT('Ctrl Pts',(10.4965768696127,12.2,3.61826087896182));
#200990=CARTESIAN_POINT('Ctrl Pts',(10.4998727905118,12.2,3.62107174701222));
#200991=CARTESIAN_POINT('Ctrl Pts',(10.5031744268032,12.2,3.62389665122267));
#200992=CARTESIAN_POINT('Ctrl Pts',(10.5064760626448,12.2,3.62672155504822));
#200993=CARTESIAN_POINT('Ctrl Pts',(10.5097834127778,12.2,3.62956049679738));
#200994=CARTESIAN_POINT('Ctrl Pts',(10.5130963627276,12.2,3.63241347009436));
#200995=CARTESIAN_POINT('Ctrl Pts',(10.5164093131287,12.2,3.63526644378005));
#200996=CARTESIAN_POINT('Ctrl Pts',(10.5197278611485,12.2,3.63813345147488));
#200997=CARTESIAN_POINT('Ctrl Pts',(10.5230518914967,12.2,3.64101448624392));
#200998=CARTESIAN_POINT('Ctrl Pts',(10.5272069292055,12.2,3.64461577950895));
#200999=CARTESIAN_POINT('Ctrl Pts',(10.5313705333668,12.2,3.64823899082619));
#201000=CARTESIAN_POINT('Ctrl Pts',(10.5355424810062,12.2,3.65188411152179));
#201001=CARTESIAN_POINT('Ctrl Pts',(10.5388800388448,12.2,3.65480020783988));
#201002=CARTESIAN_POINT('Ctrl Pts',(10.5422229357793,12.2,3.65773032583704));
#201003=CARTESIAN_POINT('Ctrl Pts',(10.5455710585058,12.2,3.66067445913113));
#201004=CARTESIAN_POINT('Ctrl Pts',(10.5480821506647,12.2,3.66288255920198));
#201005=CARTESIAN_POINT('Ctrl Pts',(10.5505961827764,12.2,3.66509854378035));
#201006=CARTESIAN_POINT('Ctrl Pts',(10.5531131072262,12.2,3.66732240924013));
#201007=CARTESIAN_POINT('Ctrl Pts',(10.5556300321333,12.2,3.66954627510392));
#201008=CARTESIAN_POINT('Ctrl Pts',(10.5581498480828,12.2,3.67177802326162));
#201009=CARTESIAN_POINT('Ctrl Pts',(10.5606725095749,12.2,3.67401765050484));
#201010=CARTESIAN_POINT('Ctrl Pts',(10.5631951706086,12.2,3.6762572773412));
#201011=CARTESIAN_POINT('Ctrl Pts',(10.5657206764339,12.2,3.67850478199383));
#201012=CARTESIAN_POINT('Ctrl Pts',(10.5682489799672,12.2,3.68076016345423));
#201013=CARTESIAN_POINT('Ctrl Pts',(10.5707772835006,12.2,3.68301554491463));
#201014=CARTESIAN_POINT('Ctrl Pts',(10.5733083845828,12.2,3.68527880454083));
#201015=CARTESIAN_POINT('Ctrl Pts',(10.5758422375022,12.2,3.68754993646866));
#201016=CARTESIAN_POINT('Ctrl Pts',(10.5792207079081,12.2,3.6905781122349));
#201017=CARTESIAN_POINT('Ctrl Pts',(10.5826040686401,12.2,3.6936202858821));
#201018=CARTESIAN_POINT('Ctrl Pts',(10.5859922100293,12.2,3.69667645024192));
#201019=CARTESIAN_POINT('Ctrl Pts',(10.5885333166482,12.2,3.69896857403229));
#201020=CARTESIAN_POINT('Ctrl Pts',(10.5910771131846,12.2,3.70126856814991));
#201021=CARTESIAN_POINT('Ctrl Pts',(10.5936235522634,12.2,3.70357642852805));
#201022=CARTESIAN_POINT('Ctrl Pts',(10.5970188035974,12.2,3.70665357500014));
#201023=CARTESIAN_POINT('Ctrl Pts',(10.6004187539281,12.2,3.70974470865931));
#201024=CARTESIAN_POINT('Ctrl Pts',(10.603823295205,12.2,3.71284982023789));
#201025=CARTESIAN_POINT('Ctrl Pts',(10.6063767012787,12.2,3.71517865402759));
#201026=CARTESIAN_POINT('Ctrl Pts',(10.6089326895204,12.2,3.71751534936536));
#201027=CARTESIAN_POINT('Ctrl Pts',(10.6114912142633,12.2,3.71985990577139));
#201028=CARTESIAN_POINT('Ctrl Pts',(10.6140497390062,12.2,3.72220446217743));
#201029=CARTESIAN_POINT('Ctrl Pts',(10.6166108013512,12.2,3.72455687838889));
#201030=CARTESIAN_POINT('Ctrl Pts',(10.6191743544661,12.2,3.72691715076039));
#201031=CARTESIAN_POINT('Ctrl Pts',(10.6217379080466,12.2,3.72927742356068));
#201032=CARTESIAN_POINT('Ctrl Pts',(10.6243039532362,12.2,3.73164555263819));
#201033=CARTESIAN_POINT('Ctrl Pts',(10.6268724453182,12.2,3.7340215349429));
#201034=CARTESIAN_POINT('Ctrl Pts',(10.6294409369336,12.2,3.73639751681597));
#201035=CARTESIAN_POINT('Ctrl Pts',(10.6320118751237,12.2,3.73878135223031));
#201036=CARTESIAN_POINT('Ctrl Pts',(10.6345852151971,12.2,3.74117303751909));
#201037=CARTESIAN_POINT('Ctrl Pts',(10.6371585552705,12.2,3.74356472280788));
#201038=CARTESIAN_POINT('Ctrl Pts',(10.6397342970009,12.2,3.74596425732862));
#201039=CARTESIAN_POINT('Ctrl Pts',(10.6423123970023,12.2,3.74837163775212));
#201040=CARTESIAN_POINT('Ctrl Pts',(10.6448904970036,12.2,3.75077901817562));
#201041=CARTESIAN_POINT('Ctrl Pts',(10.6474709541464,12.2,3.75319424635814));
#201042=CARTESIAN_POINT('Ctrl Pts',(10.6500537247309,12.2,3.75561731578107));
#201043=CARTESIAN_POINT('Ctrl Pts',(10.6526364953155,12.2,3.75804038520399));
#201044=CARTESIAN_POINT('Ctrl Pts',(10.6552215796288,12.2,3.76047129735686));
#201045=CARTESIAN_POINT('Ctrl Pts',(10.6578089327429,12.2,3.76291004822591));
#201046=CARTESIAN_POINT('Ctrl Pts',(10.6603962858571,12.2,3.76534879909495));
#201047=CARTESIAN_POINT('Ctrl Pts',(10.6629859089127,12.2,3.76779538893845));
#201048=CARTESIAN_POINT('Ctrl Pts',(10.6655777579849,12.2,3.77024981422321));
#201049=CARTESIAN_POINT('Ctrl Pts',(10.668169607528,12.2,3.77270423995386));
#201050=CARTESIAN_POINT('Ctrl Pts',(10.6707636821883,12.2,3.7751665000117));
#201051=CARTESIAN_POINT('Ctrl Pts',(10.6733599393159,12.2,3.77763659178842));
#201052=CARTESIAN_POINT('Ctrl Pts',(10.6759561959719,12.2,3.78010668311641));
#201053=CARTESIAN_POINT('Ctrl Pts',(10.6785546353944,12.2,3.78258460559397));
#201054=CARTESIAN_POINT('Ctrl Pts',(10.6811552140084,12.2,3.78507035500434));
#201055=CARTESIAN_POINT('Ctrl Pts',(10.6837557926225,12.2,3.78755610441471));
#201056=CARTESIAN_POINT('Ctrl Pts',(10.6863585103684,12.2,3.79004968258171));
#201057=CARTESIAN_POINT('Ctrl Pts',(10.688963324494,12.2,3.79255108254387));
#201058=CARTESIAN_POINT('Ctrl Pts',(10.6915681386195,12.2,3.79505248250604));
#201059=CARTESIAN_POINT('Ctrl Pts',(10.6941750490305,12.2,3.79756170681105));
#201060=CARTESIAN_POINT('Ctrl Pts',(10.6967840126976,12.2,3.80007874923098));
#201061=CARTESIAN_POINT('Ctrl Pts',(10.6993929763646,12.2,3.80259579165091));
#201062=CARTESIAN_POINT('Ctrl Pts',(10.7020039945769,12.2,3.80512065363337));
#201063=CARTESIAN_POINT('Ctrl Pts',(10.7046170227318,12.2,3.807653329999));
#201064=CARTESIAN_POINT('Ctrl Pts',(10.7072300508867,12.2,3.81018600636464));
#201065=CARTESIAN_POINT('Ctrl Pts',(10.7098450902914,12.2,3.8127264975214));
#201066=CARTESIAN_POINT('Ctrl Pts',(10.7124620984461,12.2,3.81527479942774));
#201067=CARTESIAN_POINT('Ctrl Pts',(10.7150791070762,12.2,3.81782310179702));
#201068=CARTESIAN_POINT('Ctrl Pts',(10.7176980844068,12.2,3.82037921566852));
#201069=CARTESIAN_POINT('Ctrl Pts',(10.720318989038,12.2,3.82294313500054));
#201070=CARTESIAN_POINT('Ctrl Pts',(10.722939893193,12.2,3.82550705386679));
#201071=CARTESIAN_POINT('Ctrl Pts',(10.7255627249218,12.2,3.82807877957969));
#201072=CARTESIAN_POINT('Ctrl Pts',(10.7281874407494,12.2,3.83065830653241));
#201073=CARTESIAN_POINT('Ctrl Pts',(10.7308121565771,12.2,3.83323783348514));
#201074=CARTESIAN_POINT('Ctrl Pts',(10.7334387577985,12.2,3.83582516192653));
#201075=CARTESIAN_POINT('Ctrl Pts',(10.7360672015365,12.2,3.83842028779126));
#201076=CARTESIAN_POINT('Ctrl Pts',(10.739571793028,12.2,3.84188045545376));
#201077=CARTESIAN_POINT('Ctrl Pts',(10.7430796621271,12.2,3.84535448505789));
#201078=CARTESIAN_POINT('Ctrl Pts',(10.7465907114509,12.2,3.848842365938));
#201079=CARTESIAN_POINT('Ctrl Pts',(10.7492239990417,12.2,3.85145827719211));
#201080=CARTESIAN_POINT('Ctrl Pts',(10.7518590756913,12.2,3.85408197924009));
#201081=CARTESIAN_POINT('Ctrl Pts',(10.7544958998248,12.2,3.85671346754028));
#201082=CARTESIAN_POINT('Ctrl Pts',(10.7571327234792,12.2,3.8593449553624));
#201083=CARTESIAN_POINT('Ctrl Pts',(10.7597712949246,12.2,3.86198422990851));
#201084=CARTESIAN_POINT('Ctrl Pts',(10.7624115707524,12.2,3.86463128627882));
#201085=CARTESIAN_POINT('Ctrl Pts',(10.7650518465803,12.2,3.86727834264912));
#201086=CARTESIAN_POINT('Ctrl Pts',(10.7676938270174,12.2,3.86993317980302));
#201087=CARTESIAN_POINT('Ctrl Pts',(10.7703374732548,12.2,3.87259579408196));
#201088=CARTESIAN_POINT('Ctrl Pts',(10.7729811194922,12.2,3.8752584083609));
#201089=CARTESIAN_POINT('Ctrl Pts',(10.7756264323628,12.2,3.87792879866391));
#201090=CARTESIAN_POINT('Ctrl Pts',(10.7782733755166,12.2,3.88060696148326));
#201091=CARTESIAN_POINT('Ctrl Pts',(10.7809203186704,12.2,3.88328512430262));
#201092=CARTESIAN_POINT('Ctrl Pts',(10.7835688926242,12.2,3.88597105973833));
#201093=CARTESIAN_POINT('Ctrl Pts',(10.7862190496944,12.2,3.88866476197311));
#201094=CARTESIAN_POINT('Ctrl Pts',(10.7888692067647,12.2,3.89135846420789));
#201095=CARTESIAN_POINT('Ctrl Pts',(10.7915209471673,12.2,3.89405993233984));
#201096=CARTESIAN_POINT('Ctrl Pts',(10.7941742224949,12.2,3.89676916175084));
#201097=CARTESIAN_POINT('Ctrl Pts',(10.7968274978226,12.2,3.89947839116184));
#201098=CARTESIAN_POINT('Ctrl Pts',(10.7994823070509,12.2,3.902195380806));
#201099=CARTESIAN_POINT('Ctrl Pts',(10.8021386241625,12.2,3.90492012716428));
#201100=CARTESIAN_POINT('Ctrl Pts',(10.8056803806331,12.2,3.90855312263864));
#201101=CARTESIAN_POINT('Ctrl Pts',(10.8092248173667,12.2,3.91219990566914));
#201102=CARTESIAN_POINT('Ctrl Pts',(10.8127719249999,12.2,3.91586047999999));
#201103=CARTESIAN_POINT('Origin',(-5.66257110645729E-14,15.2,-1.77635683940025E-14));
#201104=CARTESIAN_POINT('',(9.31239139999994,15.2,4.57383771099998));
#201105=CARTESIAN_POINT('',(9.31239139999994,12.2,4.57383771099998));
#201106=CARTESIAN_POINT('',(9.31239139999994,15.2,4.57383771099998));
#201107=CARTESIAN_POINT('Origin',(-5.66257110645729E-14,12.2,-1.77635683940025E-14));
#201108=CARTESIAN_POINT('Origin',(-5.66257110645729E-14,15.2,-1.77635683940025E-14));
#201109=CARTESIAN_POINT('Origin',(-5.66257110645729E-14,15.2,-1.77635683940025E-14));
#201110=CARTESIAN_POINT('',(10.1454284469999,15.2,5.41482055399998));
#201111=CARTESIAN_POINT('',(9.95917514599994,15.2,5.75020264099999));
#201112=CARTESIAN_POINT('Origin',(-5.66257110645729E-14,15.2,-1.77635683940025E-14));
#201113=CARTESIAN_POINT('',(9.95917514599994,12.2,5.75020264099999));
#201114=CARTESIAN_POINT('',(9.95917514599994,15.2,5.75020264099999));
#201115=CARTESIAN_POINT('',(10.1454284469999,12.2,5.41482055399998));
#201116=CARTESIAN_POINT('Origin',(-5.66257110645729E-14,12.2,-1.77635683940025E-14));
#201117=CARTESIAN_POINT('',(10.1454284469999,15.2,5.41482055399998));
#201118=CARTESIAN_POINT('Ctrl Pts',(9.31239140099994,15.2,4.57383771099998));
#201119=CARTESIAN_POINT('Ctrl Pts',(9.31239140099994,11.6,4.57383771099998));
#201120=CARTESIAN_POINT('Ctrl Pts',(9.31254071599994,15.2,4.57392774199998));
#201121=CARTESIAN_POINT('Ctrl Pts',(9.31254071599994,11.6,4.57392774199998));
#201122=CARTESIAN_POINT('Ctrl Pts',(9.31284451699995,15.2,4.57411102199998));
#201123=CARTESIAN_POINT('Ctrl Pts',(9.31284451699995,11.6,4.57411102199998));
#201124=CARTESIAN_POINT('Ctrl Pts',(9.31330471199994,15.2,4.57438896299998));
#201125=CARTESIAN_POINT('Ctrl Pts',(9.31330471199994,11.6,4.57438896299998));
#201126=CARTESIAN_POINT('Ctrl Pts',(9.31392435699994,15.2,4.57476383599998));
#201127=CARTESIAN_POINT('Ctrl Pts',(9.31392435699994,11.6,4.57476383599998));
#201128=CARTESIAN_POINT('Ctrl Pts',(9.31470764299995,15.2,4.57523877599999));
#201129=CARTESIAN_POINT('Ctrl Pts',(9.31470764299995,11.6,4.57523877599998));
#201130=CARTESIAN_POINT('Ctrl Pts',(9.31550313899994,15.2,4.57572221299999));
#201131=CARTESIAN_POINT('Ctrl Pts',(9.31550313899994,11.6,4.57572221299999));
#201132=CARTESIAN_POINT('Ctrl Pts',(9.31630627599995,15.2,4.57621139699998));
#201133=CARTESIAN_POINT('Ctrl Pts',(9.31630627599995,11.6,4.57621139699998));
#201134=CARTESIAN_POINT('Ctrl Pts',(9.31711701999994,15.2,4.57670632999999));
#201135=CARTESIAN_POINT('Ctrl Pts',(9.31711701999994,11.6,4.57670632999999));
#201136=CARTESIAN_POINT('Ctrl Pts',(9.31793533999994,15.2,4.57720701299999));
#201137=CARTESIAN_POINT('Ctrl Pts',(9.31793533999994,11.6,4.57720701299999));
#201138=CARTESIAN_POINT('Ctrl Pts',(9.31876120399994,15.2,4.57771344699999));
#201139=CARTESIAN_POINT('Ctrl Pts',(9.31876120399994,11.6,4.57771344699999));
#201140=CARTESIAN_POINT('Ctrl Pts',(9.31959457899995,15.2,4.57822563399999));
#201141=CARTESIAN_POINT('Ctrl Pts',(9.31959457899995,11.6,4.57822563399999));
#201142=CARTESIAN_POINT('Ctrl Pts',(9.32043543399995,15.2,4.57874357399999));
#201143=CARTESIAN_POINT('Ctrl Pts',(9.32043543399995,11.6,4.57874357399999));
#201144=CARTESIAN_POINT('Ctrl Pts',(9.32128373599994,15.2,4.57926727099998));
#201145=CARTESIAN_POINT('Ctrl Pts',(9.32128373599994,11.6,4.57926727099998));
#201146=CARTESIAN_POINT('Ctrl Pts',(9.32213945299995,15.2,4.57979672299999));
#201147=CARTESIAN_POINT('Ctrl Pts',(9.32213945299995,11.6,4.57979672299999));
#201148=CARTESIAN_POINT('Ctrl Pts',(9.32300255699994,15.2,4.58033193499999));
#201149=CARTESIAN_POINT('Ctrl Pts',(9.32300255699994,11.6,4.58033193499999));
#201150=CARTESIAN_POINT('Ctrl Pts',(9.32387301399995,15.2,4.58087290499999));
#201151=CARTESIAN_POINT('Ctrl Pts',(9.32387301399995,11.6,4.58087290499999));
#201152=CARTESIAN_POINT('Ctrl Pts',(9.32475079199994,15.2,4.58141963599999));
#201153=CARTESIAN_POINT('Ctrl Pts',(9.32475079199994,11.6,4.58141963599999));
#201154=CARTESIAN_POINT('Ctrl Pts',(9.32563586399995,15.2,4.58197212999998));
#201155=CARTESIAN_POINT('Ctrl Pts',(9.32563586399995,11.6,4.58197212999998));
#201156=CARTESIAN_POINT('Ctrl Pts',(9.32652819499994,15.2,4.58253038599998));
#201157=CARTESIAN_POINT('Ctrl Pts',(9.32652819499994,11.6,4.58253038599998));
#201158=CARTESIAN_POINT('Ctrl Pts',(9.32742775699994,15.2,4.58309440699999));
#201159=CARTESIAN_POINT('Ctrl Pts',(9.32742775699994,11.6,4.58309440699998));
#201160=CARTESIAN_POINT('Ctrl Pts',(9.32833451799995,15.2,4.58366419299999));
#201161=CARTESIAN_POINT('Ctrl Pts',(9.32833451799995,11.6,4.58366419299998));
#201162=CARTESIAN_POINT('Ctrl Pts',(9.32924844799994,15.2,4.58423974599998));
#201163=CARTESIAN_POINT('Ctrl Pts',(9.32924844799994,11.6,4.58423974599998));
#201164=CARTESIAN_POINT('Ctrl Pts',(9.33016951599994,15.2,4.58482106699999));
#201165=CARTESIAN_POINT('Ctrl Pts',(9.33016951599994,11.6,4.58482106699999));
#201166=CARTESIAN_POINT('Ctrl Pts',(9.33109769499995,15.2,4.58540815699998));
#201167=CARTESIAN_POINT('Ctrl Pts',(9.33109769499995,11.6,4.58540815699998));
#201168=CARTESIAN_POINT('Ctrl Pts',(9.33203295199995,15.2,4.58600101799998));
#201169=CARTESIAN_POINT('Ctrl Pts',(9.33203295199995,11.6,4.58600101799998));
#201170=CARTESIAN_POINT('Ctrl Pts',(9.33297525899994,15.2,4.58659964899999));
#201171=CARTESIAN_POINT('Ctrl Pts',(9.33297525899994,11.6,4.58659964899999));
#201172=CARTESIAN_POINT('Ctrl Pts',(9.33392458399994,15.2,4.58720405299999));
#201173=CARTESIAN_POINT('Ctrl Pts',(9.33392458399994,11.6,4.58720405299999));
#201174=CARTESIAN_POINT('Ctrl Pts',(9.33488089999994,15.2,4.58781422999999));
#201175=CARTESIAN_POINT('Ctrl Pts',(9.33488089999994,11.6,4.58781422999999));
#201176=CARTESIAN_POINT('Ctrl Pts',(9.33584417599995,15.2,4.58843018099999));
#201177=CARTESIAN_POINT('Ctrl Pts',(9.33584417599995,11.6,4.58843018099999));
#201178=CARTESIAN_POINT('Ctrl Pts',(9.33681438399995,15.2,4.58905190899999));
#201179=CARTESIAN_POINT('Ctrl Pts',(9.33681438399995,11.6,4.58905190899999));
#201180=CARTESIAN_POINT('Ctrl Pts',(9.33779149399994,15.2,4.58967941299999));
#201181=CARTESIAN_POINT('Ctrl Pts',(9.33779149399994,11.6,4.58967941299999));
#201182=CARTESIAN_POINT('Ctrl Pts',(9.33877547699994,15.2,4.59031269399999));
#201183=CARTESIAN_POINT('Ctrl Pts',(9.33877547699994,11.6,4.59031269399999));
#201184=CARTESIAN_POINT('Ctrl Pts',(9.33976630399994,15.2,4.59095175399998));
#201185=CARTESIAN_POINT('Ctrl Pts',(9.33976630399994,11.6,4.59095175399998));
#201186=CARTESIAN_POINT('Ctrl Pts',(9.34076394799994,15.2,4.59159659299999));
#201187=CARTESIAN_POINT('Ctrl Pts',(9.34076394799994,11.6,4.59159659299999));
#201188=CARTESIAN_POINT('Ctrl Pts',(9.34176837799994,15.2,4.59224721199998));
#201189=CARTESIAN_POINT('Ctrl Pts',(9.34176837799994,11.6,4.59224721199998));
#201190=CARTESIAN_POINT('Ctrl Pts',(9.34277956799994,15.2,4.59290361199999));
#201191=CARTESIAN_POINT('Ctrl Pts',(9.34277956799994,11.6,4.59290361199999));
#201192=CARTESIAN_POINT('Ctrl Pts',(9.34379748799994,15.2,4.59356579499998));
#201193=CARTESIAN_POINT('Ctrl Pts',(9.34379748799994,11.6,4.59356579499998));
#201194=CARTESIAN_POINT('Ctrl Pts',(9.34482210899995,15.2,4.59423375999998));
#201195=CARTESIAN_POINT('Ctrl Pts',(9.34482210899995,11.6,4.59423375999998));
#201196=CARTESIAN_POINT('Ctrl Pts',(9.34585340499994,15.2,4.59490750999999));
#201197=CARTESIAN_POINT('Ctrl Pts',(9.34585340499994,11.6,4.59490750999999));
#201198=CARTESIAN_POINT('Ctrl Pts',(9.34689134699994,15.2,4.59558704399999));
#201199=CARTESIAN_POINT('Ctrl Pts',(9.34689134699994,11.6,4.59558704399999));
#201200=CARTESIAN_POINT('Ctrl Pts',(9.34793590799995,15.2,4.59627236399999));
#201201=CARTESIAN_POINT('Ctrl Pts',(9.34793590799995,11.6,4.59627236399999));
#201202=CARTESIAN_POINT('Ctrl Pts',(9.34898705999995,15.2,4.59696346999999));
#201203=CARTESIAN_POINT('Ctrl Pts',(9.34898705999995,11.6,4.59696346999999));
#201204=CARTESIAN_POINT('Ctrl Pts',(9.35004477499995,15.2,4.59766036199999));
#201205=CARTESIAN_POINT('Ctrl Pts',(9.35004477499995,11.6,4.59766036199999));
#201206=CARTESIAN_POINT('Ctrl Pts',(9.35110902499994,15.2,4.59836304399998));
#201207=CARTESIAN_POINT('Ctrl Pts',(9.35110902499994,11.6,4.59836304399998));
#201208=CARTESIAN_POINT('Ctrl Pts',(9.35217978299994,15.2,4.59907151299999));
#201209=CARTESIAN_POINT('Ctrl Pts',(9.35217978299994,11.6,4.59907151299999));
#201210=CARTESIAN_POINT('Ctrl Pts',(9.35325702299994,15.2,4.59978577299999));
#201211=CARTESIAN_POINT('Ctrl Pts',(9.35325702299994,11.6,4.59978577299999));
#201212=CARTESIAN_POINT('Ctrl Pts',(9.35434071699994,15.2,4.60050582099999));
#201213=CARTESIAN_POINT('Ctrl Pts',(9.35434071699994,11.6,4.60050582099999));
#201214=CARTESIAN_POINT('Ctrl Pts',(9.35543083699995,15.2,4.60123166099999));
#201215=CARTESIAN_POINT('Ctrl Pts',(9.35543083699995,11.6,4.60123166099999));
#201216=CARTESIAN_POINT('Ctrl Pts',(9.35652735799994,15.2,4.60196329299999));
#201217=CARTESIAN_POINT('Ctrl Pts',(9.35652735799994,11.6,4.60196329299999));
#201218=CARTESIAN_POINT('Ctrl Pts',(9.35763025299994,15.2,4.60270071599999));
#201219=CARTESIAN_POINT('Ctrl Pts',(9.35763025299994,11.6,4.60270071599999));
#201220=CARTESIAN_POINT('Ctrl Pts',(9.35873949399994,15.2,4.60344393199998));
#201221=CARTESIAN_POINT('Ctrl Pts',(9.35873949399994,11.6,4.60344393199998));
#201222=CARTESIAN_POINT('Ctrl Pts',(9.35985505599995,15.2,4.60419294199998));
#201223=CARTESIAN_POINT('Ctrl Pts',(9.35985505599995,11.6,4.60419294199998));
#201224=CARTESIAN_POINT('Ctrl Pts',(9.36097691199994,15.2,4.60494774699999));
#201225=CARTESIAN_POINT('Ctrl Pts',(9.36097691199994,11.6,4.60494774699998));
#201226=CARTESIAN_POINT('Ctrl Pts',(9.36210503599994,15.2,4.60570834399999));
#201227=CARTESIAN_POINT('Ctrl Pts',(9.36210503599994,11.6,4.60570834399998));
#201228=CARTESIAN_POINT('Ctrl Pts',(9.36323940099994,15.2,4.60647473799998));
#201229=CARTESIAN_POINT('Ctrl Pts',(9.36323940099994,11.6,4.60647473799998));
#201230=CARTESIAN_POINT('Ctrl Pts',(9.36437998199994,15.2,4.60724692899999));
#201231=CARTESIAN_POINT('Ctrl Pts',(9.36437998199994,11.6,4.60724692899999));
#201232=CARTESIAN_POINT('Ctrl Pts',(9.36552675199994,15.2,4.60802491399999));
#201233=CARTESIAN_POINT('Ctrl Pts',(9.36552675199994,11.6,4.60802491399999));
#201234=CARTESIAN_POINT('Ctrl Pts',(9.36667968599994,15.2,4.60880869699999));
#201235=CARTESIAN_POINT('Ctrl Pts',(9.36667968599994,11.6,4.60880869699999));
#201236=CARTESIAN_POINT('Ctrl Pts',(9.36783875799994,15.2,4.60959827699998));
#201237=CARTESIAN_POINT('Ctrl Pts',(9.36783875799994,11.6,4.60959827699998));
#201238=CARTESIAN_POINT('Ctrl Pts',(9.36900394199995,15.2,4.61039365599999));
#201239=CARTESIAN_POINT('Ctrl Pts',(9.36900394199995,11.6,4.61039365599999));
#201240=CARTESIAN_POINT('Ctrl Pts',(9.37017521299994,15.2,4.61119483299999));
#201241=CARTESIAN_POINT('Ctrl Pts',(9.37017521299994,11.6,4.61119483299999));
#201242=CARTESIAN_POINT('Ctrl Pts',(9.37135254599994,15.2,4.61200180799998));
#201243=CARTESIAN_POINT('Ctrl Pts',(9.37135254599994,11.6,4.61200180799998));
#201244=CARTESIAN_POINT('Ctrl Pts',(9.37253591499994,15.2,4.61281458399998));
#201245=CARTESIAN_POINT('Ctrl Pts',(9.37253591499994,11.6,4.61281458399998));
#201246=CARTESIAN_POINT('Ctrl Pts',(9.37372529599994,15.2,4.61363315899998));
#201247=CARTESIAN_POINT('Ctrl Pts',(9.37372529599994,11.6,4.61363315899998));
#201248=CARTESIAN_POINT('Ctrl Pts',(9.37492066099994,15.2,4.61445753499999));
#201249=CARTESIAN_POINT('Ctrl Pts',(9.37492066099994,11.6,4.61445753499999));
#201250=CARTESIAN_POINT('Ctrl Pts',(9.37612198799994,15.2,4.61528771099999));
#201251=CARTESIAN_POINT('Ctrl Pts',(9.37612198799994,11.6,4.61528771099999));
#201252=CARTESIAN_POINT('Ctrl Pts',(9.37732925099995,15.2,4.61612368799998));
#201253=CARTESIAN_POINT('Ctrl Pts',(9.37732925099995,11.6,4.61612368799998));
#201254=CARTESIAN_POINT('Ctrl Pts',(9.37854242599995,15.2,4.61696546699999));
#201255=CARTESIAN_POINT('Ctrl Pts',(9.37854242599995,11.6,4.61696546699999));
#201256=CARTESIAN_POINT('Ctrl Pts',(9.37976148599994,15.2,4.61781304799998));
#201257=CARTESIAN_POINT('Ctrl Pts',(9.37976148599994,11.6,4.61781304799998));
#201258=CARTESIAN_POINT('Ctrl Pts',(9.38098640899995,15.2,4.61866643099999));
#201259=CARTESIAN_POINT('Ctrl Pts',(9.38098640899995,11.6,4.61866643099999));
#201260=CARTESIAN_POINT('Ctrl Pts',(9.38221716999994,15.2,4.61952561599999));
#201261=CARTESIAN_POINT('Ctrl Pts',(9.38221716999994,11.6,4.61952561599999));
#201262=CARTESIAN_POINT('Ctrl Pts',(9.38345374299994,15.2,4.62039060399999));
#201263=CARTESIAN_POINT('Ctrl Pts',(9.38345374299994,11.6,4.62039060399999));
#201264=CARTESIAN_POINT('Ctrl Pts',(9.38469610599994,15.2,4.62126139599999));
#201265=CARTESIAN_POINT('Ctrl Pts',(9.38469610599994,11.6,4.62126139599999));
#201266=CARTESIAN_POINT('Ctrl Pts',(9.38594423299994,15.2,4.62213799099998));
#201267=CARTESIAN_POINT('Ctrl Pts',(9.38594423299994,11.6,4.62213799099998));
#201268=CARTESIAN_POINT('Ctrl Pts',(9.38719809999995,15.2,4.62302038999999));
#201269=CARTESIAN_POINT('Ctrl Pts',(9.38719809999995,11.6,4.62302038999999));
#201270=CARTESIAN_POINT('Ctrl Pts',(9.38845768499995,15.2,4.62390859299998));
#201271=CARTESIAN_POINT('Ctrl Pts',(9.38845768499995,11.6,4.62390859299998));
#201272=CARTESIAN_POINT('Ctrl Pts',(9.38972296199994,15.2,4.62480259999998));
#201273=CARTESIAN_POINT('Ctrl Pts',(9.38972296199994,11.6,4.62480259999998));
#201274=CARTESIAN_POINT('Ctrl Pts',(9.39099390899995,15.2,4.62570241299999));
#201275=CARTESIAN_POINT('Ctrl Pts',(9.39099390899995,11.6,4.62570241299998));
#201276=CARTESIAN_POINT('Ctrl Pts',(9.39227049999994,15.2,4.62660802899999));
#201277=CARTESIAN_POINT('Ctrl Pts',(9.39227049999994,11.6,4.62660802899998));
#201278=CARTESIAN_POINT('Ctrl Pts',(9.39355271299994,15.2,4.62751945099999));
#201279=CARTESIAN_POINT('Ctrl Pts',(9.39355271299994,11.6,4.62751945099999));
#201280=CARTESIAN_POINT('Ctrl Pts',(9.39484052399994,15.2,4.62843667799999));
#201281=CARTESIAN_POINT('Ctrl Pts',(9.39484052399994,11.6,4.62843667799999));
#201282=CARTESIAN_POINT('Ctrl Pts',(9.39613390999994,15.2,4.62935970999999));
#201283=CARTESIAN_POINT('Ctrl Pts',(9.39613390999994,11.6,4.62935970999998));
#201284=CARTESIAN_POINT('Ctrl Pts',(9.39743284699994,15.2,4.63028854799998));
#201285=CARTESIAN_POINT('Ctrl Pts',(9.39743284699994,11.6,4.63028854799998));
#201286=CARTESIAN_POINT('Ctrl Pts',(9.39873731199994,15.2,4.63122319099998));
#201287=CARTESIAN_POINT('Ctrl Pts',(9.39873731199994,11.6,4.63122319099998));
#201288=CARTESIAN_POINT('Ctrl Pts',(9.40004728399994,15.2,4.63216364099999));
#201289=CARTESIAN_POINT('Ctrl Pts',(9.40004728399994,11.6,4.63216364099999));
#201290=CARTESIAN_POINT('Ctrl Pts',(9.40136273499995,15.2,4.63310989699998));
#201291=CARTESIAN_POINT('Ctrl Pts',(9.40136273499995,11.6,4.63310989699998));
#201292=CARTESIAN_POINT('Ctrl Pts',(9.40268364699994,15.2,4.63406195899999));
#201293=CARTESIAN_POINT('Ctrl Pts',(9.40268364699994,11.6,4.63406195899999));
#201294=CARTESIAN_POINT('Ctrl Pts',(9.40400999399994,15.2,4.63501982699999));
#201295=CARTESIAN_POINT('Ctrl Pts',(9.40400999399994,11.6,4.63501982699999));
#201296=CARTESIAN_POINT('Ctrl Pts',(9.40534175499995,15.2,4.63598350099999));
#201297=CARTESIAN_POINT('Ctrl Pts',(9.40534175499995,11.6,4.63598350099998));
#201298=CARTESIAN_POINT('Ctrl Pts',(9.40667890599994,15.2,4.63695298199998));
#201299=CARTESIAN_POINT('Ctrl Pts',(9.40667890599994,11.6,4.63695298199998));
#201300=CARTESIAN_POINT('Ctrl Pts',(9.40802142599994,15.2,4.63792826899999));
#201301=CARTESIAN_POINT('Ctrl Pts',(9.40802142599994,11.6,4.63792826899999));
#201302=CARTESIAN_POINT('Ctrl Pts',(9.40936929099994,15.2,4.63890936299999));
#201303=CARTESIAN_POINT('Ctrl Pts',(9.40936929099994,11.6,4.63890936299998));
#201304=CARTESIAN_POINT('Ctrl Pts',(9.41072247899994,15.2,4.63989626299998));
#201305=CARTESIAN_POINT('Ctrl Pts',(9.41072247899994,11.6,4.63989626299998));
#201306=CARTESIAN_POINT('Ctrl Pts',(9.41208096699994,15.2,4.64088896999999));
#201307=CARTESIAN_POINT('Ctrl Pts',(9.41208096699994,11.6,4.64088896999998));
#201308=CARTESIAN_POINT('Ctrl Pts',(9.41344473399995,15.2,4.64188748299998));
#201309=CARTESIAN_POINT('Ctrl Pts',(9.41344473399995,11.6,4.64188748299998));
#201310=CARTESIAN_POINT('Ctrl Pts',(9.41481375699994,15.2,4.64289180399999));
#201311=CARTESIAN_POINT('Ctrl Pts',(9.41481375699994,11.6,4.64289180399999));
#201312=CARTESIAN_POINT('Ctrl Pts',(9.41618801399994,15.2,4.64390192999999));
#201313=CARTESIAN_POINT('Ctrl Pts',(9.41618801399994,11.6,4.64390192999998));
#201314=CARTESIAN_POINT('Ctrl Pts',(9.41756748299994,15.2,4.64491786399999));
#201315=CARTESIAN_POINT('Ctrl Pts',(9.41756748299994,11.6,4.64491786399999));
#201316=CARTESIAN_POINT('Ctrl Pts',(9.41895214199995,15.2,4.64593960399998));
#201317=CARTESIAN_POINT('Ctrl Pts',(9.41895214199995,11.6,4.64593960399998));
#201318=CARTESIAN_POINT('Ctrl Pts',(9.42034196999994,15.2,4.64696714999998));
#201319=CARTESIAN_POINT('Ctrl Pts',(9.42034196999994,11.6,4.64696714999998));
#201320=CARTESIAN_POINT('Ctrl Pts',(9.42173694299994,15.2,4.64800050299999));
#201321=CARTESIAN_POINT('Ctrl Pts',(9.42173694299994,11.6,4.64800050299999));
#201322=CARTESIAN_POINT('Ctrl Pts',(9.42313704199995,15.2,4.64903966199999));
#201323=CARTESIAN_POINT('Ctrl Pts',(9.42313704199995,11.6,4.64903966199999));
#201324=CARTESIAN_POINT('Ctrl Pts',(9.42454224399994,15.2,4.65008462799998));
#201325=CARTESIAN_POINT('Ctrl Pts',(9.42454224399994,11.6,4.65008462799998));
#201326=CARTESIAN_POINT('Ctrl Pts',(9.42595252799994,15.2,4.65113539899999));
#201327=CARTESIAN_POINT('Ctrl Pts',(9.42595252799994,11.6,4.65113539899999));
#201328=CARTESIAN_POINT('Ctrl Pts',(9.42736787099994,15.2,4.65219197699999));
#201329=CARTESIAN_POINT('Ctrl Pts',(9.42736787099994,11.6,4.65219197699999));
#201330=CARTESIAN_POINT('Ctrl Pts',(9.42878825299994,15.2,4.65325436099998));
#201331=CARTESIAN_POINT('Ctrl Pts',(9.42878825299994,11.6,4.65325436099998));
#201332=CARTESIAN_POINT('Ctrl Pts',(9.43021365299994,15.2,4.65432254999998));
#201333=CARTESIAN_POINT('Ctrl Pts',(9.43021365299994,11.6,4.65432254999998));
#201334=CARTESIAN_POINT('Ctrl Pts',(9.43164404899994,15.2,4.65539654499998));
#201335=CARTESIAN_POINT('Ctrl Pts',(9.43164404899994,11.6,4.65539654499998));
#201336=CARTESIAN_POINT('Ctrl Pts',(9.43307941999995,15.2,4.65647634499998));
#201337=CARTESIAN_POINT('Ctrl Pts',(9.43307941999995,11.6,4.65647634499998));
#201338=CARTESIAN_POINT('Ctrl Pts',(9.43451974499995,15.2,4.65756195099999));
#201339=CARTESIAN_POINT('Ctrl Pts',(9.43451974499995,11.6,4.65756195099999));
#201340=CARTESIAN_POINT('Ctrl Pts',(9.43596500299994,15.2,4.65865336199998));
#201341=CARTESIAN_POINT('Ctrl Pts',(9.43596500299994,11.6,4.65865336199998));
#201342=CARTESIAN_POINT('Ctrl Pts',(9.43741517299994,15.2,4.65975057799999));
#201343=CARTESIAN_POINT('Ctrl Pts',(9.43741517299994,11.6,4.65975057799999));
#201344=CARTESIAN_POINT('Ctrl Pts',(9.43887023499994,15.2,4.66085359799998));
#201345=CARTESIAN_POINT('Ctrl Pts',(9.43887023499994,11.6,4.66085359799998));
#201346=CARTESIAN_POINT('Ctrl Pts',(9.44033016699995,15.2,4.66196242299999));
#201347=CARTESIAN_POINT('Ctrl Pts',(9.44033016699995,11.6,4.66196242299999));
#201348=CARTESIAN_POINT('Ctrl Pts',(9.44179494899995,15.2,4.66307705199998));
#201349=CARTESIAN_POINT('Ctrl Pts',(9.44179494899995,11.6,4.66307705199998));
#201350=CARTESIAN_POINT('Ctrl Pts',(9.44326455999994,15.2,4.66419748599999));
#201351=CARTESIAN_POINT('Ctrl Pts',(9.44326455999994,11.6,4.66419748599998));
#201352=CARTESIAN_POINT('Ctrl Pts',(9.44473897999995,15.2,4.66532372299999));
#201353=CARTESIAN_POINT('Ctrl Pts',(9.44473897999995,11.6,4.66532372299999));
#201354=CARTESIAN_POINT('Ctrl Pts',(9.44621818699994,15.2,4.66645576299998));
#201355=CARTESIAN_POINT('Ctrl Pts',(9.44621818699994,11.6,4.66645576299998));
#201356=CARTESIAN_POINT('Ctrl Pts',(9.44770216299995,15.2,4.66759360699999));
#201357=CARTESIAN_POINT('Ctrl Pts',(9.44770216299995,11.6,4.66759360699999));
#201358=CARTESIAN_POINT('Ctrl Pts',(9.44919088599995,15.2,4.66873725399999));
#201359=CARTESIAN_POINT('Ctrl Pts',(9.44919088599995,11.6,4.66873725399999));
#201360=CARTESIAN_POINT('Ctrl Pts',(9.45068433699995,15.2,4.66988670299998));
#201361=CARTESIAN_POINT('Ctrl Pts',(9.45068433699995,11.6,4.66988670299998));
#201362=CARTESIAN_POINT('Ctrl Pts',(9.45218249399994,15.2,4.67104195499999));
#201363=CARTESIAN_POINT('Ctrl Pts',(9.45218249399994,11.6,4.67104195499999));
#201364=CARTESIAN_POINT('Ctrl Pts',(9.45368533799994,15.2,4.67220300799998));
#201365=CARTESIAN_POINT('Ctrl Pts',(9.45368533799994,11.6,4.67220300799998));
#201366=CARTESIAN_POINT('Ctrl Pts',(9.45519284899994,15.2,4.67336986399999));
#201367=CARTESIAN_POINT('Ctrl Pts',(9.45519284899994,11.6,4.67336986399999));
#201368=CARTESIAN_POINT('Ctrl Pts',(9.45670500599994,15.2,4.67454251999998));
#201369=CARTESIAN_POINT('Ctrl Pts',(9.45670500599994,11.6,4.67454251999998));
#201370=CARTESIAN_POINT('Ctrl Pts',(9.45822179099994,15.2,4.67572097799999));
#201371=CARTESIAN_POINT('Ctrl Pts',(9.45822179099994,11.6,4.67572097799999));
#201372=CARTESIAN_POINT('Ctrl Pts',(9.45974318299994,15.2,4.67690523599998));
#201373=CARTESIAN_POINT('Ctrl Pts',(9.45974318299994,11.6,4.67690523599998));
#201374=CARTESIAN_POINT('Ctrl Pts',(9.46126916199994,15.2,4.67809529399998));
#201375=CARTESIAN_POINT('Ctrl Pts',(9.46126916199994,11.6,4.67809529399998));
#201376=CARTESIAN_POINT('Ctrl Pts',(9.46279970999995,15.2,4.67929115199999));
#201377=CARTESIAN_POINT('Ctrl Pts',(9.46279970999995,11.6,4.67929115199999));
#201378=CARTESIAN_POINT('Ctrl Pts',(9.46433480399994,15.2,4.68049280999999));
#201379=CARTESIAN_POINT('Ctrl Pts',(9.46433480399994,11.6,4.68049280999998));
#201380=CARTESIAN_POINT('Ctrl Pts',(9.46587442699995,15.2,4.68170026699998));
#201381=CARTESIAN_POINT('Ctrl Pts',(9.46587442699995,11.6,4.68170026699998));
#201382=CARTESIAN_POINT('Ctrl Pts',(9.46741855999995,15.2,4.68291352199999));
#201383=CARTESIAN_POINT('Ctrl Pts',(9.46741855999995,11.6,4.68291352199999));
#201384=CARTESIAN_POINT('Ctrl Pts',(9.46896718199995,15.2,4.68413257599998));
#201385=CARTESIAN_POINT('Ctrl Pts',(9.46896718199995,11.6,4.68413257599998));
#201386=CARTESIAN_POINT('Ctrl Pts',(9.47052027399995,15.2,4.68535742699999));
#201387=CARTESIAN_POINT('Ctrl Pts',(9.47052027399995,11.6,4.68535742699998));
#201388=CARTESIAN_POINT('Ctrl Pts',(9.47207781699994,15.2,4.68658807499998));
#201389=CARTESIAN_POINT('Ctrl Pts',(9.47207781699994,11.6,4.68658807499998));
#201390=CARTESIAN_POINT('Ctrl Pts',(9.47363979099995,15.2,4.68782451999999));
#201391=CARTESIAN_POINT('Ctrl Pts',(9.47363979099995,11.6,4.68782451999999));
#201392=CARTESIAN_POINT('Ctrl Pts',(9.47520617799994,15.2,4.68906676099999));
#201393=CARTESIAN_POINT('Ctrl Pts',(9.47520617799994,11.6,4.68906676099999));
#201394=CARTESIAN_POINT('Ctrl Pts',(9.47677695899995,15.2,4.69031479799998));
#201395=CARTESIAN_POINT('Ctrl Pts',(9.47677695899995,11.6,4.69031479799998));
#201396=CARTESIAN_POINT('Ctrl Pts',(9.47835211299994,15.2,4.69156863099998));
#201397=CARTESIAN_POINT('Ctrl Pts',(9.47835211299994,11.6,4.69156863099998));
#201398=CARTESIAN_POINT('Ctrl Pts',(9.47993162399994,15.2,4.69282825799999));
#201399=CARTESIAN_POINT('Ctrl Pts',(9.47993162399994,11.6,4.69282825799999));
#201400=CARTESIAN_POINT('Ctrl Pts',(9.48151547099994,15.2,4.69409367999998));
#201401=CARTESIAN_POINT('Ctrl Pts',(9.48151547099994,11.6,4.69409367999998));
#201402=CARTESIAN_POINT('Ctrl Pts',(9.48310363399995,15.2,4.69536489599999));
#201403=CARTESIAN_POINT('Ctrl Pts',(9.48310363399995,11.6,4.69536489599999));
#201404=CARTESIAN_POINT('Ctrl Pts',(9.48469609699995,15.2,4.69664190399998));
#201405=CARTESIAN_POINT('Ctrl Pts',(9.48469609699995,11.6,4.69664190399998));
#201406=CARTESIAN_POINT('Ctrl Pts',(9.48629283999994,15.2,4.69792470599998));
#201407=CARTESIAN_POINT('Ctrl Pts',(9.48629283999994,11.6,4.69792470599998));
#201408=CARTESIAN_POINT('Ctrl Pts',(9.48789384499995,15.2,4.69921329999998));
#201409=CARTESIAN_POINT('Ctrl Pts',(9.48789384499995,11.6,4.69921329999998));
#201410=CARTESIAN_POINT('Ctrl Pts',(9.48949909199994,15.2,4.70050768499998));
#201411=CARTESIAN_POINT('Ctrl Pts',(9.48949909199994,11.6,4.70050768499998));
#201412=CARTESIAN_POINT('Ctrl Pts',(9.49110856299994,15.2,4.70180786099998));
#201413=CARTESIAN_POINT('Ctrl Pts',(9.49110856299994,11.6,4.70180786099998));
#201414=CARTESIAN_POINT('Ctrl Pts',(9.49272223999994,15.2,4.70311382799999));
#201415=CARTESIAN_POINT('Ctrl Pts',(9.49272223999994,11.6,4.70311382799998));
#201416=CARTESIAN_POINT('Ctrl Pts',(9.49434010399995,15.2,4.70442558399998));
#201417=CARTESIAN_POINT('Ctrl Pts',(9.49434010399995,11.6,4.70442558399998));
#201418=CARTESIAN_POINT('Ctrl Pts',(9.49596213899994,15.2,4.70574312999998));
#201419=CARTESIAN_POINT('Ctrl Pts',(9.49596213899994,11.6,4.70574312999998));
#201420=CARTESIAN_POINT('Ctrl Pts',(9.49758832299995,15.2,4.70706646399999));
#201421=CARTESIAN_POINT('Ctrl Pts',(9.49758832299995,11.6,4.70706646399999));
#201422=CARTESIAN_POINT('Ctrl Pts',(9.49921863899995,15.2,4.70839558599998));
#201423=CARTESIAN_POINT('Ctrl Pts',(9.49921863899995,11.6,4.70839558599998));
#201424=CARTESIAN_POINT('Ctrl Pts',(9.50085307099994,15.2,4.70973049499998));
#201425=CARTESIAN_POINT('Ctrl Pts',(9.50085307099994,11.6,4.70973049499998));
#201426=CARTESIAN_POINT('Ctrl Pts',(9.50249159799995,15.2,4.71107119199999));
#201427=CARTESIAN_POINT('Ctrl Pts',(9.50249159799995,11.6,4.71107119199999));
#201428=CARTESIAN_POINT('Ctrl Pts',(9.50413420299995,15.2,4.71241767399999));
#201429=CARTESIAN_POINT('Ctrl Pts',(9.50413420299995,11.6,4.71241767399999));
#201430=CARTESIAN_POINT('Ctrl Pts',(9.50578086799995,15.2,4.71376994199999));
#201431=CARTESIAN_POINT('Ctrl Pts',(9.50578086799995,11.6,4.71376994199998));
#201432=CARTESIAN_POINT('Ctrl Pts',(9.50743157599995,15.2,4.71512799399999));
#201433=CARTESIAN_POINT('Ctrl Pts',(9.50743157599995,11.6,4.71512799399999));
#201434=CARTESIAN_POINT('Ctrl Pts',(9.50908630799994,15.2,4.71649182999998));
#201435=CARTESIAN_POINT('Ctrl Pts',(9.50908630799994,11.6,4.71649182999998));
#201436=CARTESIAN_POINT('Ctrl Pts',(9.51074504599994,15.2,4.71786144999999));
#201437=CARTESIAN_POINT('Ctrl Pts',(9.51074504599994,11.6,4.71786144999999));
#201438=CARTESIAN_POINT('Ctrl Pts',(9.51240777299994,15.2,4.71923685199998));
#201439=CARTESIAN_POINT('Ctrl Pts',(9.51240777299994,11.6,4.71923685199998));
#201440=CARTESIAN_POINT('Ctrl Pts',(9.51407447099994,15.2,4.72061803599999));
#201441=CARTESIAN_POINT('Ctrl Pts',(9.51407447099994,11.6,4.72061803599999));
#201442=CARTESIAN_POINT('Ctrl Pts',(9.51574512199995,15.2,4.72200500099999));
#201443=CARTESIAN_POINT('Ctrl Pts',(9.51574512199995,11.6,4.72200500099999));
#201444=CARTESIAN_POINT('Ctrl Pts',(9.51741970899995,15.2,4.72339774699999));
#201445=CARTESIAN_POINT('Ctrl Pts',(9.51741970899995,11.6,4.72339774699999));
#201446=CARTESIAN_POINT('Ctrl Pts',(9.51909821399994,15.2,4.72479627299998));
#201447=CARTESIAN_POINT('Ctrl Pts',(9.51909821399994,11.6,4.72479627299998));
#201448=CARTESIAN_POINT('Ctrl Pts',(9.52078061899994,15.2,4.72620057699999));
#201449=CARTESIAN_POINT('Ctrl Pts',(9.52078061899994,11.6,4.72620057699999));
#201450=CARTESIAN_POINT('Ctrl Pts',(9.52246690899995,15.2,4.72761065899999));
#201451=CARTESIAN_POINT('Ctrl Pts',(9.52246690899995,11.6,4.72761065899998));
#201452=CARTESIAN_POINT('Ctrl Pts',(9.52415706299995,15.2,4.72902651899999));
#201453=CARTESIAN_POINT('Ctrl Pts',(9.52415706299995,11.6,4.72902651899999));
#201454=CARTESIAN_POINT('Ctrl Pts',(9.52585106599994,15.2,4.73044815499998));
#201455=CARTESIAN_POINT('Ctrl Pts',(9.52585106599994,11.6,4.73044815499998));
#201456=CARTESIAN_POINT('Ctrl Pts',(9.52754889999994,15.2,4.73187556799999));
#201457=CARTESIAN_POINT('Ctrl Pts',(9.52754889999994,11.6,4.73187556799999));
#201458=CARTESIAN_POINT('Ctrl Pts',(9.52925054799995,15.2,4.73330875599999));
#201459=CARTESIAN_POINT('Ctrl Pts',(9.52925054799995,11.6,4.73330875599998));
#201460=CARTESIAN_POINT('Ctrl Pts',(9.53095599299994,15.2,4.73474771699999));
#201461=CARTESIAN_POINT('Ctrl Pts',(9.53095599299994,11.6,4.73474771699998));
#201462=CARTESIAN_POINT('Ctrl Pts',(9.53266521799994,15.2,4.73619245199998));
#201463=CARTESIAN_POINT('Ctrl Pts',(9.53266521799994,11.6,4.73619245199998));
#201464=CARTESIAN_POINT('Ctrl Pts',(9.53437820499994,15.2,4.73764295999998));
#201465=CARTESIAN_POINT('Ctrl Pts',(9.53437820499994,11.6,4.73764295999998));
#201466=CARTESIAN_POINT('Ctrl Pts',(9.53609493699994,15.2,4.73909923999998));
#201467=CARTESIAN_POINT('Ctrl Pts',(9.53609493699994,11.6,4.73909923999998));
#201468=CARTESIAN_POINT('Ctrl Pts',(9.53781539899994,15.2,4.74056128999998));
#201469=CARTESIAN_POINT('Ctrl Pts',(9.53781539899994,11.6,4.74056128999998));
#201470=CARTESIAN_POINT('Ctrl Pts',(9.53953957299994,15.2,4.74202910999999));
#201471=CARTESIAN_POINT('Ctrl Pts',(9.53953957299994,11.6,4.74202910999998));
#201472=CARTESIAN_POINT('Ctrl Pts',(9.54126743999995,15.2,4.74350269999999));
#201473=CARTESIAN_POINT('Ctrl Pts',(9.54126743999995,11.6,4.74350269999999));
#201474=CARTESIAN_POINT('Ctrl Pts',(9.54299898599994,15.2,4.74498205899998));
#201475=CARTESIAN_POINT('Ctrl Pts',(9.54299898599994,11.6,4.74498205899998));
#201476=CARTESIAN_POINT('Ctrl Pts',(9.54473419399994,15.2,4.74646718399999));
#201477=CARTESIAN_POINT('Ctrl Pts',(9.54473419399994,11.6,4.74646718399998));
#201478=CARTESIAN_POINT('Ctrl Pts',(9.54647304499994,15.2,4.74795807599998));
#201479=CARTESIAN_POINT('Ctrl Pts',(9.54647304499994,11.6,4.74795807599998));
#201480=CARTESIAN_POINT('Ctrl Pts',(9.54821552499994,15.2,4.74945473499999));
#201481=CARTESIAN_POINT('Ctrl Pts',(9.54821552499994,11.6,4.74945473499999));
#201482=CARTESIAN_POINT('Ctrl Pts',(9.54996161699994,15.2,4.75095715699998));
#201483=CARTESIAN_POINT('Ctrl Pts',(9.54996161699994,11.6,4.75095715699998));
#201484=CARTESIAN_POINT('Ctrl Pts',(9.55171130299994,15.2,4.75246534399999));
#201485=CARTESIAN_POINT('Ctrl Pts',(9.55171130299994,11.6,4.75246534399999));
#201486=CARTESIAN_POINT('Ctrl Pts',(9.55346456699995,15.2,4.75397929399998));
#201487=CARTESIAN_POINT('Ctrl Pts',(9.55346456699995,11.6,4.75397929399998));
#201488=CARTESIAN_POINT('Ctrl Pts',(9.55522139299994,15.2,4.75549900599999));
#201489=CARTESIAN_POINT('Ctrl Pts',(9.55522139299994,11.6,4.75549900599999));
#201490=CARTESIAN_POINT('Ctrl Pts',(9.55698176499994,15.2,4.75702447899998));
#201491=CARTESIAN_POINT('Ctrl Pts',(9.55698176499994,11.6,4.75702447899998));
#201492=CARTESIAN_POINT('Ctrl Pts',(9.55874566599995,15.2,4.75855571199999));
#201493=CARTESIAN_POINT('Ctrl Pts',(9.55874566599995,11.6,4.75855571199998));
#201494=CARTESIAN_POINT('Ctrl Pts',(9.56051307899994,15.2,4.76009270399998));
#201495=CARTESIAN_POINT('Ctrl Pts',(9.56051307899994,11.6,4.76009270399998));
#201496=CARTESIAN_POINT('Ctrl Pts',(9.56228398899994,15.2,4.76163545499999));
#201497=CARTESIAN_POINT('Ctrl Pts',(9.56228398899994,11.6,4.76163545499999));
#201498=CARTESIAN_POINT('Ctrl Pts',(9.56405837899995,15.2,4.76318396199999));
#201499=CARTESIAN_POINT('Ctrl Pts',(9.56405837899995,11.6,4.76318396199999));
#201500=CARTESIAN_POINT('Ctrl Pts',(9.56583623399995,15.2,4.76473822599999));
#201501=CARTESIAN_POINT('Ctrl Pts',(9.56583623399995,11.6,4.76473822599999));
#201502=CARTESIAN_POINT('Ctrl Pts',(9.56761753699995,15.2,4.76629824599998));
#201503=CARTESIAN_POINT('Ctrl Pts',(9.56761753699995,11.6,4.76629824599998));
#201504=CARTESIAN_POINT('Ctrl Pts',(9.56940227099994,15.2,4.76786401999998));
#201505=CARTESIAN_POINT('Ctrl Pts',(9.56940227099994,11.6,4.76786401999998));
#201506=CARTESIAN_POINT('Ctrl Pts',(9.57119042099994,15.2,4.76943554699999));
#201507=CARTESIAN_POINT('Ctrl Pts',(9.57119042099994,11.6,4.76943554699999));
#201508=CARTESIAN_POINT('Ctrl Pts',(9.57298197099995,15.2,4.77101282699999));
#201509=CARTESIAN_POINT('Ctrl Pts',(9.57298197099995,11.6,4.77101282699999));
#201510=CARTESIAN_POINT('Ctrl Pts',(9.57477690499994,15.2,4.77259585799998));
#201511=CARTESIAN_POINT('Ctrl Pts',(9.57477690499994,11.6,4.77259585799998));
#201512=CARTESIAN_POINT('Ctrl Pts',(9.57657520799994,15.2,4.77418463899999));
#201513=CARTESIAN_POINT('Ctrl Pts',(9.57657520799994,11.6,4.77418463899998));
#201514=CARTESIAN_POINT('Ctrl Pts',(9.57837686399994,15.2,4.77577916999999));
#201515=CARTESIAN_POINT('Ctrl Pts',(9.57837686399994,11.6,4.77577916999999));
#201516=CARTESIAN_POINT('Ctrl Pts',(9.58018185399995,15.2,4.77737944799999));
#201517=CARTESIAN_POINT('Ctrl Pts',(9.58018185399995,11.6,4.77737944799998));
#201518=CARTESIAN_POINT('Ctrl Pts',(9.58199016599995,15.2,4.77898547499999));
#201519=CARTESIAN_POINT('Ctrl Pts',(9.58199016599995,11.6,4.77898547499999));
#201520=CARTESIAN_POINT('Ctrl Pts',(9.58380178399995,15.2,4.78059724599999));
#201521=CARTESIAN_POINT('Ctrl Pts',(9.58380178399995,11.6,4.78059724599999));
#201522=CARTESIAN_POINT('Ctrl Pts',(9.58561669099995,15.2,4.78221476299999));
#201523=CARTESIAN_POINT('Ctrl Pts',(9.58561669099995,11.6,4.78221476299998));
#201524=CARTESIAN_POINT('Ctrl Pts',(9.58743487199994,15.2,4.78383802399998));
#201525=CARTESIAN_POINT('Ctrl Pts',(9.58743487199994,11.6,4.78383802399998));
#201526=CARTESIAN_POINT('Ctrl Pts',(9.58925631099994,15.2,4.78546702899998));
#201527=CARTESIAN_POINT('Ctrl Pts',(9.58925631099994,11.6,4.78546702899998));
#201528=CARTESIAN_POINT('Ctrl Pts',(9.59108099299995,15.2,4.78710177399999));
#201529=CARTESIAN_POINT('Ctrl Pts',(9.59108099299995,11.6,4.78710177399999));
#201530=CARTESIAN_POINT('Ctrl Pts',(9.59290890099994,15.2,4.78874226099999));
#201531=CARTESIAN_POINT('Ctrl Pts',(9.59290890099994,11.6,4.78874226099998));
#201532=CARTESIAN_POINT('Ctrl Pts',(9.59474002199994,15.2,4.79038848699999));
#201533=CARTESIAN_POINT('Ctrl Pts',(9.59474002199994,11.6,4.79038848699999));
#201534=CARTESIAN_POINT('Ctrl Pts',(9.59657433999995,15.2,4.79204045099999));
#201535=CARTESIAN_POINT('Ctrl Pts',(9.59657433999995,11.6,4.79204045099998));
#201536=CARTESIAN_POINT('Ctrl Pts',(9.59841183799995,15.2,4.79369815299999));
#201537=CARTESIAN_POINT('Ctrl Pts',(9.59841183799995,11.6,4.79369815299999));
#201538=CARTESIAN_POINT('Ctrl Pts',(9.60025250199994,15.2,4.79536159099998));
#201539=CARTESIAN_POINT('Ctrl Pts',(9.60025250199994,11.6,4.79536159099998));
#201540=CARTESIAN_POINT('Ctrl Pts',(9.60209631699995,15.2,4.79703076499998));
#201541=CARTESIAN_POINT('Ctrl Pts',(9.60209631699995,11.6,4.79703076499998));
#201542=CARTESIAN_POINT('Ctrl Pts',(9.60394326799995,15.2,4.79870567199999));
#201543=CARTESIAN_POINT('Ctrl Pts',(9.60394326799995,11.6,4.79870567199998));
#201544=CARTESIAN_POINT('Ctrl Pts',(9.60579333899994,15.2,4.80038631299998));
#201545=CARTESIAN_POINT('Ctrl Pts',(9.60579333899994,11.6,4.80038631299998));
#201546=CARTESIAN_POINT('Ctrl Pts',(9.60764651399994,15.2,4.80207268499999));
#201547=CARTESIAN_POINT('Ctrl Pts',(9.60764651399994,11.6,4.80207268499999));
#201548=CARTESIAN_POINT('Ctrl Pts',(9.60950277999994,15.2,4.80376478599998));
#201549=CARTESIAN_POINT('Ctrl Pts',(9.60950277999994,11.6,4.80376478599998));
#201550=CARTESIAN_POINT('Ctrl Pts',(9.61136212099994,15.2,4.80546261799999));
#201551=CARTESIAN_POINT('Ctrl Pts',(9.61136212099994,11.6,4.80546261799999));
#201552=CARTESIAN_POINT('Ctrl Pts',(9.61322452199994,15.2,4.80716617799998));
#201553=CARTESIAN_POINT('Ctrl Pts',(9.61322452199994,11.6,4.80716617799998));
#201554=CARTESIAN_POINT('Ctrl Pts',(9.61508996699994,15.2,4.80887546399998));
#201555=CARTESIAN_POINT('Ctrl Pts',(9.61508996699994,11.6,4.80887546399998));
#201556=CARTESIAN_POINT('Ctrl Pts',(9.61695844299994,15.2,4.81059047699999));
#201557=CARTESIAN_POINT('Ctrl Pts',(9.61695844299994,11.6,4.81059047699999));
#201558=CARTESIAN_POINT('Ctrl Pts',(9.61882993399995,15.2,4.81231121399999));
#201559=CARTESIAN_POINT('Ctrl Pts',(9.61882993399995,11.6,4.81231121399999));
#201560=CARTESIAN_POINT('Ctrl Pts',(9.62070442599994,15.2,4.81403767499998));
#201561=CARTESIAN_POINT('Ctrl Pts',(9.62070442599994,11.6,4.81403767499998));
#201562=CARTESIAN_POINT('Ctrl Pts',(9.62258190299995,15.2,4.81576985699999));
#201563=CARTESIAN_POINT('Ctrl Pts',(9.62258190299995,11.6,4.81576985699998));
#201564=CARTESIAN_POINT('Ctrl Pts',(9.62446235099994,15.2,4.81750776099998));
#201565=CARTESIAN_POINT('Ctrl Pts',(9.62446235099994,11.6,4.81750776099998));
#201566=CARTESIAN_POINT('Ctrl Pts',(9.62634575599994,15.2,4.81925138399999));
#201567=CARTESIAN_POINT('Ctrl Pts',(9.62634575599994,11.6,4.81925138399998));
#201568=CARTESIAN_POINT('Ctrl Pts',(9.62823210099994,15.2,4.82100072599999));
#201569=CARTESIAN_POINT('Ctrl Pts',(9.62823210099994,11.6,4.82100072599999));
#201570=CARTESIAN_POINT('Ctrl Pts',(9.63012137399994,15.2,4.82275578399998));
#201571=CARTESIAN_POINT('Ctrl Pts',(9.63012137399994,11.6,4.82275578399998));
#201572=CARTESIAN_POINT('Ctrl Pts',(9.63201355899994,15.2,4.82451655899998));
#201573=CARTESIAN_POINT('Ctrl Pts',(9.63201355899994,11.6,4.82451655899998));
#201574=CARTESIAN_POINT('Ctrl Pts',(9.63390864199994,15.2,4.82628304899999));
#201575=CARTESIAN_POINT('Ctrl Pts',(9.63390864199994,11.6,4.82628304899999));
#201576=CARTESIAN_POINT('Ctrl Pts',(9.63580660699994,15.2,4.82805525099998));
#201577=CARTESIAN_POINT('Ctrl Pts',(9.63580660699994,11.6,4.82805525099998));
#201578=CARTESIAN_POINT('Ctrl Pts',(9.63770744199994,15.2,4.82983316599999));
#201579=CARTESIAN_POINT('Ctrl Pts',(9.63770744199994,11.6,4.82983316599999));
#201580=CARTESIAN_POINT('Ctrl Pts',(9.63961113099994,15.2,4.83161679299998));
#201581=CARTESIAN_POINT('Ctrl Pts',(9.63961113099994,11.6,4.83161679299998));
#201582=CARTESIAN_POINT('Ctrl Pts',(9.64151765999994,15.2,4.83340612899998));
#201583=CARTESIAN_POINT('Ctrl Pts',(9.64151765999994,11.6,4.83340612899998));
#201584=CARTESIAN_POINT('Ctrl Pts',(9.64342701399995,15.2,4.83520117199999));
#201585=CARTESIAN_POINT('Ctrl Pts',(9.64342701399995,11.6,4.83520117199998));
#201586=CARTESIAN_POINT('Ctrl Pts',(9.64533917899994,15.2,4.83700192299998));
#201587=CARTESIAN_POINT('Ctrl Pts',(9.64533917899994,11.6,4.83700192299998));
#201588=CARTESIAN_POINT('Ctrl Pts',(9.64725414199994,15.2,4.83880837999998));
#201589=CARTESIAN_POINT('Ctrl Pts',(9.64725414199994,11.6,4.83880837999998));
#201590=CARTESIAN_POINT('Ctrl Pts',(9.64917188799994,15.2,4.84062053999998));
#201591=CARTESIAN_POINT('Ctrl Pts',(9.64917188799994,11.6,4.84062053999998));
#201592=CARTESIAN_POINT('Ctrl Pts',(9.65109240199994,15.2,4.84243840399999));
#201593=CARTESIAN_POINT('Ctrl Pts',(9.65109240199994,11.6,4.84243840399999));
#201594=CARTESIAN_POINT('Ctrl Pts',(9.65301566999995,15.2,4.84426196999999));
#201595=CARTESIAN_POINT('Ctrl Pts',(9.65301566999995,11.6,4.84426196999998));
#201596=CARTESIAN_POINT('Ctrl Pts',(9.65494167899994,15.2,4.84609123599999));
#201597=CARTESIAN_POINT('Ctrl Pts',(9.65494167899994,11.6,4.84609123599998));
#201598=CARTESIAN_POINT('Ctrl Pts',(9.65687041399995,15.2,4.84792620099999));
#201599=CARTESIAN_POINT('Ctrl Pts',(9.65687041399995,11.6,4.84792620099998));
#201600=CARTESIAN_POINT('Ctrl Pts',(9.65880185999995,15.2,4.84976686399998));
#201601=CARTESIAN_POINT('Ctrl Pts',(9.65880185999995,11.6,4.84976686399998));
#201602=CARTESIAN_POINT('Ctrl Pts',(9.66073600599995,15.2,4.85161322299999));
#201603=CARTESIAN_POINT('Ctrl Pts',(9.66073600599995,11.6,4.85161322299999));
#201604=CARTESIAN_POINT('Ctrl Pts',(9.66267283399995,15.2,4.85346527699999));
#201605=CARTESIAN_POINT('Ctrl Pts',(9.66267283399995,11.6,4.85346527699999));
#201606=CARTESIAN_POINT('Ctrl Pts',(9.66461233399994,15.2,4.85532302499998));
#201607=CARTESIAN_POINT('Ctrl Pts',(9.66461233399994,11.6,4.85532302499998));
#201608=CARTESIAN_POINT('Ctrl Pts',(9.66655448999994,15.2,4.85718646399998));
#201609=CARTESIAN_POINT('Ctrl Pts',(9.66655448999994,11.6,4.85718646399998));
#201610=CARTESIAN_POINT('Ctrl Pts',(9.66849928799994,15.2,4.85905559599999));
#201611=CARTESIAN_POINT('Ctrl Pts',(9.66849928799994,11.6,4.85905559599999));
#201612=CARTESIAN_POINT('Ctrl Pts',(9.67044671499995,15.2,4.86093041599998));
#201613=CARTESIAN_POINT('Ctrl Pts',(9.67044671499995,11.6,4.86093041599998));
#201614=CARTESIAN_POINT('Ctrl Pts',(9.67239675599994,15.2,4.86281092499999));
#201615=CARTESIAN_POINT('Ctrl Pts',(9.67239675599994,11.6,4.86281092499999));
#201616=CARTESIAN_POINT('Ctrl Pts',(9.67434939899994,15.2,4.86469711899999));
#201617=CARTESIAN_POINT('Ctrl Pts',(9.67434939899994,11.6,4.86469711899998));
#201618=CARTESIAN_POINT('Ctrl Pts',(9.67630462799994,15.2,4.86658899999998));
#201619=CARTESIAN_POINT('Ctrl Pts',(9.67630462799994,11.6,4.86658899999998));
#201620=CARTESIAN_POINT('Ctrl Pts',(9.67826243199994,15.2,4.86848656399999));
#201621=CARTESIAN_POINT('Ctrl Pts',(9.67826243199994,11.6,4.86848656399999));
#201622=CARTESIAN_POINT('Ctrl Pts',(9.68022279599994,15.2,4.87038981099998));
#201623=CARTESIAN_POINT('Ctrl Pts',(9.68022279599994,11.6,4.87038981099998));
#201624=CARTESIAN_POINT('Ctrl Pts',(9.68218570499995,15.2,4.87229873799999));
#201625=CARTESIAN_POINT('Ctrl Pts',(9.68218570499995,11.6,4.87229873799999));
#201626=CARTESIAN_POINT('Ctrl Pts',(9.68415114899994,15.2,4.87421334499999));
#201627=CARTESIAN_POINT('Ctrl Pts',(9.68415114899994,11.6,4.87421334499999));
#201628=CARTESIAN_POINT('Ctrl Pts',(9.68611910999994,15.2,4.87613362999999));
#201629=CARTESIAN_POINT('Ctrl Pts',(9.68611910999994,11.6,4.87613362999998));
#201630=CARTESIAN_POINT('Ctrl Pts',(9.68808957799994,15.2,4.87805959199999));
#201631=CARTESIAN_POINT('Ctrl Pts',(9.68808957799994,11.6,4.87805959199999));
#201632=CARTESIAN_POINT('Ctrl Pts',(9.69006253799994,15.2,4.87999122899998));
#201633=CARTESIAN_POINT('Ctrl Pts',(9.69006253799994,11.6,4.87999122899998));
#201634=CARTESIAN_POINT('Ctrl Pts',(9.69203797799995,15.2,4.88192853999998));
#201635=CARTESIAN_POINT('Ctrl Pts',(9.69203797799995,11.6,4.88192853999998));
#201636=CARTESIAN_POINT('Ctrl Pts',(9.69401588199995,15.2,4.88387152299998));
#201637=CARTESIAN_POINT('Ctrl Pts',(9.69401588199995,11.6,4.88387152299998));
#201638=CARTESIAN_POINT('Ctrl Pts',(9.69599623899994,15.2,4.88582017699999));
#201639=CARTESIAN_POINT('Ctrl Pts',(9.69599623899994,11.6,4.88582017699999));
#201640=CARTESIAN_POINT('Ctrl Pts',(9.69797903399994,15.2,4.88777450099998));
#201641=CARTESIAN_POINT('Ctrl Pts',(9.69797903399994,11.6,4.88777450099998));
#201642=CARTESIAN_POINT('Ctrl Pts',(9.69996425399994,15.2,4.88973449099999));
#201643=CARTESIAN_POINT('Ctrl Pts',(9.69996425399994,11.6,4.88973449099999));
#201644=CARTESIAN_POINT('Ctrl Pts',(9.70195188699994,15.2,4.89170014899998));
#201645=CARTESIAN_POINT('Ctrl Pts',(9.70195188699994,11.6,4.89170014899998));
#201646=CARTESIAN_POINT('Ctrl Pts',(9.70394191899994,15.2,4.89367147199999));
#201647=CARTESIAN_POINT('Ctrl Pts',(9.70394191899994,11.6,4.89367147199999));
#201648=CARTESIAN_POINT('Ctrl Pts',(9.70593433699995,15.2,4.89564845699999));
#201649=CARTESIAN_POINT('Ctrl Pts',(9.70593433699995,11.6,4.89564845699998));
#201650=CARTESIAN_POINT('Ctrl Pts',(9.70792912699994,15.2,4.89763110499998));
#201651=CARTESIAN_POINT('Ctrl Pts',(9.70792912699994,11.6,4.89763110499998));
#201652=CARTESIAN_POINT('Ctrl Pts',(9.70992627599994,15.2,4.89961941299998));
#201653=CARTESIAN_POINT('Ctrl Pts',(9.70992627599994,11.6,4.89961941299998));
#201654=CARTESIAN_POINT('Ctrl Pts',(9.71192577199995,15.2,4.90161337999999));
#201655=CARTESIAN_POINT('Ctrl Pts',(9.71192577199995,11.6,4.90161337999999));
#201656=CARTESIAN_POINT('Ctrl Pts',(9.71392760099994,15.2,4.90361300399999));
#201657=CARTESIAN_POINT('Ctrl Pts',(9.71392760099994,11.6,4.90361300399999));
#201658=CARTESIAN_POINT('Ctrl Pts',(9.71593175099994,15.2,4.90561828399999));
#201659=CARTESIAN_POINT('Ctrl Pts',(9.71593175099994,11.6,4.90561828399999));
#201660=CARTESIAN_POINT('Ctrl Pts',(9.71793820699995,15.2,4.90762921799998));
#201661=CARTESIAN_POINT('Ctrl Pts',(9.71793820699995,11.6,4.90762921799998));
#201662=CARTESIAN_POINT('Ctrl Pts',(9.71994695799994,15.2,4.90964580499998));
#201663=CARTESIAN_POINT('Ctrl Pts',(9.71994695799994,11.6,4.90964580499998));
#201664=CARTESIAN_POINT('Ctrl Pts',(9.72195798999994,15.2,4.91166804299999));
#201665=CARTESIAN_POINT('Ctrl Pts',(9.72195798999994,11.6,4.91166804299999));
#201666=CARTESIAN_POINT('Ctrl Pts',(9.72397129099994,15.2,4.91369592999998));
#201667=CARTESIAN_POINT('Ctrl Pts',(9.72397129099994,11.6,4.91369592999998));
#201668=CARTESIAN_POINT('Ctrl Pts',(9.72598684699994,15.2,4.91572946599998));
#201669=CARTESIAN_POINT('Ctrl Pts',(9.72598684699994,11.6,4.91572946599998));
#201670=CARTESIAN_POINT('Ctrl Pts',(9.72800464599995,15.2,4.91776864699998));
#201671=CARTESIAN_POINT('Ctrl Pts',(9.72800464599995,11.6,4.91776864699998));
#201672=CARTESIAN_POINT('Ctrl Pts',(9.73002467399994,15.2,4.91981347399999));
#201673=CARTESIAN_POINT('Ctrl Pts',(9.73002467399994,11.6,4.91981347399999));
#201674=CARTESIAN_POINT('Ctrl Pts',(9.73204691999995,15.2,4.92186394399998));
#201675=CARTESIAN_POINT('Ctrl Pts',(9.73204691999995,11.6,4.92186394399998));
#201676=CARTESIAN_POINT('Ctrl Pts',(9.73407136999995,15.2,4.92392005599999));
#201677=CARTESIAN_POINT('Ctrl Pts',(9.73407136999995,11.6,4.92392005599999));
#201678=CARTESIAN_POINT('Ctrl Pts',(9.73609801199995,15.2,4.92598180799998));
#201679=CARTESIAN_POINT('Ctrl Pts',(9.73609801199995,11.6,4.92598180799998));
#201680=CARTESIAN_POINT('Ctrl Pts',(9.73812683299995,15.2,4.92804919799998));
#201681=CARTESIAN_POINT('Ctrl Pts',(9.73812683299995,11.6,4.92804919799998));
#201682=CARTESIAN_POINT('Ctrl Pts',(9.74015781999995,15.2,4.93012222599998));
#201683=CARTESIAN_POINT('Ctrl Pts',(9.74015781999995,11.6,4.93012222599998));
#201684=CARTESIAN_POINT('Ctrl Pts',(9.74219095999995,15.2,4.93220088799998));
#201685=CARTESIAN_POINT('Ctrl Pts',(9.74219095999995,11.6,4.93220088799998));
#201686=CARTESIAN_POINT('Ctrl Pts',(9.74422624199994,15.2,4.93428518399998));
#201687=CARTESIAN_POINT('Ctrl Pts',(9.74422624199994,11.6,4.93428518399998));
#201688=CARTESIAN_POINT('Ctrl Pts',(9.74626365199994,15.2,4.93637511299998));
#201689=CARTESIAN_POINT('Ctrl Pts',(9.74626365199994,11.6,4.93637511299998));
#201690=CARTESIAN_POINT('Ctrl Pts',(9.74830317899994,15.2,4.93847067099999));
#201691=CARTESIAN_POINT('Ctrl Pts',(9.74830317899994,11.6,4.93847067099999));
#201692=CARTESIAN_POINT('Ctrl Pts',(9.75034480799994,15.2,4.94057185899998));
#201693=CARTESIAN_POINT('Ctrl Pts',(9.75034480799994,11.6,4.94057185899998));
#201694=CARTESIAN_POINT('Ctrl Pts',(9.75238852899994,15.2,4.94267867299998));
#201695=CARTESIAN_POINT('Ctrl Pts',(9.75238852899994,11.6,4.94267867299998));
#201696=CARTESIAN_POINT('Ctrl Pts',(9.75443432899995,15.2,4.94479111299999));
#201697=CARTESIAN_POINT('Ctrl Pts',(9.75443432899995,11.6,4.94479111299999));
#201698=CARTESIAN_POINT('Ctrl Pts',(9.75648219399995,15.2,4.94690917699998));
#201699=CARTESIAN_POINT('Ctrl Pts',(9.75648219399995,11.6,4.94690917699998));
#201700=CARTESIAN_POINT('Ctrl Pts',(9.75853211299994,15.2,4.94903286299999));
#201701=CARTESIAN_POINT('Ctrl Pts',(9.75853211299994,11.6,4.94903286299999));
#201702=CARTESIAN_POINT('Ctrl Pts',(9.76058407399995,15.2,4.95116216999998));
#201703=CARTESIAN_POINT('Ctrl Pts',(9.76058407399995,11.6,4.95116216999998));
#201704=CARTESIAN_POINT('Ctrl Pts',(9.76263806299994,15.2,4.95329709499998));
#201705=CARTESIAN_POINT('Ctrl Pts',(9.76263806299994,11.6,4.95329709499998));
#201706=CARTESIAN_POINT('Ctrl Pts',(9.76469407099994,15.2,4.95543763899998));
#201707=CARTESIAN_POINT('Ctrl Pts',(9.76469407099994,11.6,4.95543763899998));
#201708=CARTESIAN_POINT('Ctrl Pts',(9.76675208199994,15.2,4.95758379699998));
#201709=CARTESIAN_POINT('Ctrl Pts',(9.76675208199994,11.6,4.95758379699998));
#201710=CARTESIAN_POINT('Ctrl Pts',(9.76881208499995,15.2,4.95973556899998));
#201711=CARTESIAN_POINT('Ctrl Pts',(9.76881208499995,11.6,4.95973556899998));
#201712=CARTESIAN_POINT('Ctrl Pts',(9.77087406899994,15.2,4.96189295299998));
#201713=CARTESIAN_POINT('Ctrl Pts',(9.77087406899994,11.6,4.96189295299998));
#201714=CARTESIAN_POINT('Ctrl Pts',(9.77293801999994,15.2,4.96405594799998));
#201715=CARTESIAN_POINT('Ctrl Pts',(9.77293801999994,11.6,4.96405594799998));
#201716=CARTESIAN_POINT('Ctrl Pts',(9.77500392799995,15.2,4.96622455099998));
#201717=CARTESIAN_POINT('Ctrl Pts',(9.77500392799995,11.6,4.96622455099998));
#201718=CARTESIAN_POINT('Ctrl Pts',(9.77707177899994,15.2,4.96839876199999));
#201719=CARTESIAN_POINT('Ctrl Pts',(9.77707177899994,11.6,4.96839876199999));
#201720=CARTESIAN_POINT('Ctrl Pts',(9.77914156199994,15.2,4.97057857799999));
#201721=CARTESIAN_POINT('Ctrl Pts',(9.77914156199994,11.6,4.97057857799999));
#201722=CARTESIAN_POINT('Ctrl Pts',(9.78121326399994,15.2,4.97276399699999));
#201723=CARTESIAN_POINT('Ctrl Pts',(9.78121326399994,11.6,4.97276399699999));
#201724=CARTESIAN_POINT('Ctrl Pts',(9.78328687399994,15.2,4.97495501899999));
#201725=CARTESIAN_POINT('Ctrl Pts',(9.78328687399994,11.6,4.97495501899999));
#201726=CARTESIAN_POINT('Ctrl Pts',(9.78536237899995,15.2,4.97715163999998));
#201727=CARTESIAN_POINT('Ctrl Pts',(9.78536237899995,11.6,4.97715163999998));
#201728=CARTESIAN_POINT('Ctrl Pts',(9.78743976799995,15.2,4.97935385999998));
#201729=CARTESIAN_POINT('Ctrl Pts',(9.78743976799995,11.6,4.97935385999998));
#201730=CARTESIAN_POINT('Ctrl Pts',(9.78951902799994,15.2,4.98156167799999));
#201731=CARTESIAN_POINT('Ctrl Pts',(9.78951902799994,11.6,4.98156167799999));
#201732=CARTESIAN_POINT('Ctrl Pts',(9.79160014799995,15.2,4.98377508899999));
#201733=CARTESIAN_POINT('Ctrl Pts',(9.79160014799995,11.6,4.98377508899999));
#201734=CARTESIAN_POINT('Ctrl Pts',(9.79368311599995,15.2,4.98599409399999));
#201735=CARTESIAN_POINT('Ctrl Pts',(9.79368311599995,11.6,4.98599409399999));
#201736=CARTESIAN_POINT('Ctrl Pts',(9.79576791999994,15.2,4.98821869099999));
#201737=CARTESIAN_POINT('Ctrl Pts',(9.79576791999994,11.6,4.98821869099999));
#201738=CARTESIAN_POINT('Ctrl Pts',(9.79785454699994,15.2,4.99044887699998));
#201739=CARTESIAN_POINT('Ctrl Pts',(9.79785454699994,11.6,4.99044887699998));
#201740=CARTESIAN_POINT('Ctrl Pts',(9.79994298799994,15.2,4.99268464999999));
#201741=CARTESIAN_POINT('Ctrl Pts',(9.79994298799994,11.6,4.99268464999999));
#201742=CARTESIAN_POINT('Ctrl Pts',(9.80203322899994,15.2,4.99492601099998));
#201743=CARTESIAN_POINT('Ctrl Pts',(9.80203322899994,11.6,4.99492601099998));
#201744=CARTESIAN_POINT('Ctrl Pts',(9.80412525799995,15.2,4.99717295599999));
#201745=CARTESIAN_POINT('Ctrl Pts',(9.80412525799995,11.6,4.99717295599999));
#201746=CARTESIAN_POINT('Ctrl Pts',(9.80621906499995,15.2,4.99942548299998));
#201747=CARTESIAN_POINT('Ctrl Pts',(9.80621906499995,11.6,4.99942548299998));
#201748=CARTESIAN_POINT('Ctrl Pts',(9.80831463599995,15.2,5.00168359099998));
#201749=CARTESIAN_POINT('Ctrl Pts',(9.80831463599995,11.6,5.00168359099998));
#201750=CARTESIAN_POINT('Ctrl Pts',(9.81041196099994,15.2,5.00394727899998));
#201751=CARTESIAN_POINT('Ctrl Pts',(9.81041196099994,11.6,5.00394727899998));
#201752=CARTESIAN_POINT('Ctrl Pts',(9.81251102899994,15.2,5.00621654299999));
#201753=CARTESIAN_POINT('Ctrl Pts',(9.81251102899994,11.6,5.00621654299999));
#201754=CARTESIAN_POINT('Ctrl Pts',(9.81461182699995,15.2,5.00849138199998));
#201755=CARTESIAN_POINT('Ctrl Pts',(9.81461182699995,11.6,5.00849138199998));
#201756=CARTESIAN_POINT('Ctrl Pts',(9.81671434399994,15.2,5.01077179599999));
#201757=CARTESIAN_POINT('Ctrl Pts',(9.81671434399994,11.6,5.01077179599999));
#201758=CARTESIAN_POINT('Ctrl Pts',(9.81881856699994,15.2,5.01305778199999));
#201759=CARTESIAN_POINT('Ctrl Pts',(9.81881856699994,11.6,5.01305778199999));
#201760=CARTESIAN_POINT('Ctrl Pts',(9.82092448599994,15.2,5.01534933699999));
#201761=CARTESIAN_POINT('Ctrl Pts',(9.82092448599994,11.6,5.01534933699999));
#201762=CARTESIAN_POINT('Ctrl Pts',(9.82303208999994,15.2,5.01764645999998));
#201763=CARTESIAN_POINT('Ctrl Pts',(9.82303208999994,11.6,5.01764645999998));
#201764=CARTESIAN_POINT('Ctrl Pts',(9.82514136599995,15.2,5.01994915099999));
#201765=CARTESIAN_POINT('Ctrl Pts',(9.82514136599995,11.6,5.01994915099999));
#201766=CARTESIAN_POINT('Ctrl Pts',(9.82725230399994,15.2,5.02225740599999));
#201767=CARTESIAN_POINT('Ctrl Pts',(9.82725230399994,11.6,5.02225740599999));
#201768=CARTESIAN_POINT('Ctrl Pts',(9.82936489099995,15.2,5.02457122199999));
#201769=CARTESIAN_POINT('Ctrl Pts',(9.82936489099995,11.6,5.02457122199999));
#201770=CARTESIAN_POINT('Ctrl Pts',(9.83147911699995,15.2,5.02689060099998));
#201771=CARTESIAN_POINT('Ctrl Pts',(9.83147911699995,11.6,5.02689060099998));
#201772=CARTESIAN_POINT('Ctrl Pts',(9.83359496999994,15.2,5.02921553799998));
#201773=CARTESIAN_POINT('Ctrl Pts',(9.83359496999994,11.6,5.02921553799998));
#201774=CARTESIAN_POINT('Ctrl Pts',(9.83571243799994,15.2,5.03154603299999));
#201775=CARTESIAN_POINT('Ctrl Pts',(9.83571243799994,11.6,5.03154603299999));
#201776=CARTESIAN_POINT('Ctrl Pts',(9.83783150999994,15.2,5.03388208199999));
#201777=CARTESIAN_POINT('Ctrl Pts',(9.83783150999994,11.6,5.03388208199999));
#201778=CARTESIAN_POINT('Ctrl Pts',(9.83995217599994,15.2,5.03622368599999));
#201779=CARTESIAN_POINT('Ctrl Pts',(9.83995217599994,11.6,5.03622368599999));
#201780=CARTESIAN_POINT('Ctrl Pts',(9.84207442399994,15.2,5.03857083999999));
#201781=CARTESIAN_POINT('Ctrl Pts',(9.84207442399994,11.6,5.03857083999999));
#201782=CARTESIAN_POINT('Ctrl Pts',(9.84419824199994,15.2,5.04092354499999));
#201783=CARTESIAN_POINT('Ctrl Pts',(9.84419824199994,11.6,5.04092354499999));
#201784=CARTESIAN_POINT('Ctrl Pts',(9.84632361899994,15.2,5.04328179799998));
#201785=CARTESIAN_POINT('Ctrl Pts',(9.84632361899994,11.6,5.04328179799998));
#201786=CARTESIAN_POINT('Ctrl Pts',(9.84845054499995,15.2,5.04564559599999));
#201787=CARTESIAN_POINT('Ctrl Pts',(9.84845054499995,11.6,5.04564559599999));
#201788=CARTESIAN_POINT('Ctrl Pts',(9.85057900699994,15.2,5.04801493799999));
#201789=CARTESIAN_POINT('Ctrl Pts',(9.85057900699994,11.6,5.04801493799999));
#201790=CARTESIAN_POINT('Ctrl Pts',(9.85270899399995,15.2,5.05038982299999));
#201791=CARTESIAN_POINT('Ctrl Pts',(9.85270899399995,11.6,5.05038982299999));
#201792=CARTESIAN_POINT('Ctrl Pts',(9.85484049599994,15.2,5.05277024799998));
#201793=CARTESIAN_POINT('Ctrl Pts',(9.85484049599994,11.6,5.05277024799998));
#201794=CARTESIAN_POINT('Ctrl Pts',(9.85697350299995,15.2,5.05515621099998));
#201795=CARTESIAN_POINT('Ctrl Pts',(9.85697350299995,11.6,5.05515621099998));
#201796=CARTESIAN_POINT('Ctrl Pts',(9.85910800099994,15.2,5.05754771199998));
#201797=CARTESIAN_POINT('Ctrl Pts',(9.85910800099994,11.6,5.05754771199998));
#201798=CARTESIAN_POINT('Ctrl Pts',(9.86124398099994,15.2,5.05994474699998));
#201799=CARTESIAN_POINT('Ctrl Pts',(9.86124398099994,11.6,5.05994474699998));
#201800=CARTESIAN_POINT('Ctrl Pts',(9.86338143099994,15.2,5.06234731299998));
#201801=CARTESIAN_POINT('Ctrl Pts',(9.86338143099994,11.6,5.06234731299998));
#201802=CARTESIAN_POINT('Ctrl Pts',(9.86552033999994,15.2,5.06475541199999));
#201803=CARTESIAN_POINT('Ctrl Pts',(9.86552033999994,11.6,5.06475541199999));
#201804=CARTESIAN_POINT('Ctrl Pts',(9.86766069799994,15.2,5.06716903899999));
#201805=CARTESIAN_POINT('Ctrl Pts',(9.86766069799994,11.6,5.06716903899999));
#201806=CARTESIAN_POINT('Ctrl Pts',(9.86980249199994,15.2,5.06958819299999));
#201807=CARTESIAN_POINT('Ctrl Pts',(9.86980249199994,11.6,5.06958819299999));
#201808=CARTESIAN_POINT('Ctrl Pts',(9.87194571399994,15.2,5.07201287199998));
#201809=CARTESIAN_POINT('Ctrl Pts',(9.87194571399994,11.6,5.07201287199998));
#201810=CARTESIAN_POINT('Ctrl Pts',(9.87409035199994,15.2,5.07444307399999));
#201811=CARTESIAN_POINT('Ctrl Pts',(9.87409035199994,11.6,5.07444307399999));
#201812=CARTESIAN_POINT('Ctrl Pts',(9.87623639299994,15.2,5.07687879699999));
#201813=CARTESIAN_POINT('Ctrl Pts',(9.87623639299994,11.6,5.07687879699999));
#201814=CARTESIAN_POINT('Ctrl Pts',(9.87838382799995,15.2,5.07932003999999));
#201815=CARTESIAN_POINT('Ctrl Pts',(9.87838382799995,11.6,5.07932003999999));
#201816=CARTESIAN_POINT('Ctrl Pts',(9.88053264699994,15.2,5.08176679899999));
#201817=CARTESIAN_POINT('Ctrl Pts',(9.88053264699994,11.6,5.08176679899999));
#201818=CARTESIAN_POINT('Ctrl Pts',(9.88268283699995,15.2,5.08421907399998));
#201819=CARTESIAN_POINT('Ctrl Pts',(9.88268283699995,11.6,5.08421907399998));
#201820=CARTESIAN_POINT('Ctrl Pts',(9.88483438899994,15.2,5.08667686299999));
#201821=CARTESIAN_POINT('Ctrl Pts',(9.88483438899994,11.6,5.08667686299999));
#201822=CARTESIAN_POINT('Ctrl Pts',(9.88698729099994,15.2,5.08914016199999));
#201823=CARTESIAN_POINT('Ctrl Pts',(9.88698729099994,11.6,5.08914016199999));
#201824=CARTESIAN_POINT('Ctrl Pts',(9.88914153299995,15.2,5.09160897099999));
#201825=CARTESIAN_POINT('Ctrl Pts',(9.88914153299995,11.6,5.09160897099999));
#201826=CARTESIAN_POINT('Ctrl Pts',(9.89129710499994,15.2,5.09408328799999));
#201827=CARTESIAN_POINT('Ctrl Pts',(9.89129710499994,11.6,5.09408328799999));
#201828=CARTESIAN_POINT('Ctrl Pts',(9.89345399399994,15.2,5.09656310999999));
#201829=CARTESIAN_POINT('Ctrl Pts',(9.89345399399994,11.6,5.09656310999999));
#201830=CARTESIAN_POINT('Ctrl Pts',(9.89561219199994,15.2,5.09904843499999));
#201831=CARTESIAN_POINT('Ctrl Pts',(9.89561219199994,11.6,5.09904843499999));
#201832=CARTESIAN_POINT('Ctrl Pts',(9.89777168699994,15.2,5.10153926199998));
#201833=CARTESIAN_POINT('Ctrl Pts',(9.89777168699994,11.6,5.10153926199998));
#201834=CARTESIAN_POINT('Ctrl Pts',(9.89993246699994,15.2,5.10403558799998));
#201835=CARTESIAN_POINT('Ctrl Pts',(9.89993246699994,11.6,5.10403558799998));
#201836=CARTESIAN_POINT('Ctrl Pts',(9.90209452399995,15.2,5.10653741199998));
#201837=CARTESIAN_POINT('Ctrl Pts',(9.90209452399995,11.6,5.10653741199998));
#201838=CARTESIAN_POINT('Ctrl Pts',(9.90425784599994,15.2,5.10904473199999));
#201839=CARTESIAN_POINT('Ctrl Pts',(9.90425784599994,11.6,5.10904473199999));
#201840=CARTESIAN_POINT('Ctrl Pts',(9.90642242299995,15.2,5.11155754499999));
#201841=CARTESIAN_POINT('Ctrl Pts',(9.90642242299995,11.6,5.11155754499999));
#201842=CARTESIAN_POINT('Ctrl Pts',(9.90858824399995,15.2,5.11407584799999));
#201843=CARTESIAN_POINT('Ctrl Pts',(9.90858824399995,11.6,5.11407584799999));
#201844=CARTESIAN_POINT('Ctrl Pts',(9.91075529899994,15.2,5.11659964199998));
#201845=CARTESIAN_POINT('Ctrl Pts',(9.91075529899994,11.6,5.11659964199998));
#201846=CARTESIAN_POINT('Ctrl Pts',(9.91292357699994,15.2,5.11912892399998));
#201847=CARTESIAN_POINT('Ctrl Pts',(9.91292357699994,11.6,5.11912892399998));
#201848=CARTESIAN_POINT('Ctrl Pts',(9.91509306699994,15.2,5.12166369099998));
#201849=CARTESIAN_POINT('Ctrl Pts',(9.91509306699994,11.6,5.12166369099998));
#201850=CARTESIAN_POINT('Ctrl Pts',(9.91726375999994,15.2,5.12420394099999));
#201851=CARTESIAN_POINT('Ctrl Pts',(9.91726375999994,11.6,5.12420394099999));
#201852=CARTESIAN_POINT('Ctrl Pts',(9.91943564399994,15.2,5.12674967299999));
#201853=CARTESIAN_POINT('Ctrl Pts',(9.91943564399994,11.6,5.12674967299999));
#201854=CARTESIAN_POINT('Ctrl Pts',(9.92160870899994,15.2,5.12930088399998));
#201855=CARTESIAN_POINT('Ctrl Pts',(9.92160870899994,11.6,5.12930088399998));
#201856=CARTESIAN_POINT('Ctrl Pts',(9.92378294699994,15.2,5.13185757199999));
#201857=CARTESIAN_POINT('Ctrl Pts',(9.92378294699994,11.6,5.13185757199999));
#201858=CARTESIAN_POINT('Ctrl Pts',(9.92595834399994,15.2,5.13441973499998));
#201859=CARTESIAN_POINT('Ctrl Pts',(9.92595834399994,11.6,5.13441973499998));
#201860=CARTESIAN_POINT('Ctrl Pts',(9.92813489199994,15.2,5.13698737299999));
#201861=CARTESIAN_POINT('Ctrl Pts',(9.92813489199994,11.6,5.13698737299999));
#201862=CARTESIAN_POINT('Ctrl Pts',(9.93031257999995,15.2,5.13956047999999));
#201863=CARTESIAN_POINT('Ctrl Pts',(9.93031257999995,11.6,5.13956047999999));
#201864=CARTESIAN_POINT('Ctrl Pts',(9.93249139799994,15.2,5.14213905799998));
#201865=CARTESIAN_POINT('Ctrl Pts',(9.93249139799994,11.6,5.14213905799998));
#201866=CARTESIAN_POINT('Ctrl Pts',(9.93467133499994,15.2,5.14472310099999));
#201867=CARTESIAN_POINT('Ctrl Pts',(9.93467133499994,11.6,5.14472310099999));
#201868=CARTESIAN_POINT('Ctrl Pts',(9.93685238099994,15.2,5.14731261099998));
#201869=CARTESIAN_POINT('Ctrl Pts',(9.93685238099994,11.6,5.14731261099998));
#201870=CARTESIAN_POINT('Ctrl Pts',(9.93903452599995,15.2,5.14990758299999));
#201871=CARTESIAN_POINT('Ctrl Pts',(9.93903452599995,11.6,5.14990758299999));
#201872=CARTESIAN_POINT('Ctrl Pts',(9.94121775999995,15.2,5.15250801599999));
#201873=CARTESIAN_POINT('Ctrl Pts',(9.94121775999995,11.6,5.15250801599999));
#201874=CARTESIAN_POINT('Ctrl Pts',(9.94340207299994,15.2,5.15511390799999));
#201875=CARTESIAN_POINT('Ctrl Pts',(9.94340207299994,11.6,5.15511390799999));
#201876=CARTESIAN_POINT('Ctrl Pts',(9.94558745299994,15.2,5.15772525699998));
#201877=CARTESIAN_POINT('Ctrl Pts',(9.94558745299994,11.6,5.15772525699998));
#201878=CARTESIAN_POINT('Ctrl Pts',(9.94777389299994,15.2,5.16034205899999));
#201879=CARTESIAN_POINT('Ctrl Pts',(9.94777389299994,11.6,5.16034205899999));
#201880=CARTESIAN_POINT('Ctrl Pts',(9.94996137999994,15.2,5.16296431599999));
#201881=CARTESIAN_POINT('Ctrl Pts',(9.94996137999994,11.6,5.16296431599999));
#201882=CARTESIAN_POINT('Ctrl Pts',(9.95214990599995,15.2,5.16559202199999));
#201883=CARTESIAN_POINT('Ctrl Pts',(9.95214990599995,11.6,5.16559202199999));
#201884=CARTESIAN_POINT('Ctrl Pts',(9.95433945899994,15.2,5.16822517599999));
#201885=CARTESIAN_POINT('Ctrl Pts',(9.95433945899994,11.6,5.16822517599999));
#201886=CARTESIAN_POINT('Ctrl Pts',(9.95653002999994,15.2,5.17086377699999));
#201887=CARTESIAN_POINT('Ctrl Pts',(9.95653002999994,11.6,5.17086377699999));
#201888=CARTESIAN_POINT('Ctrl Pts',(9.95872160899994,15.2,5.17350782199999));
#201889=CARTESIAN_POINT('Ctrl Pts',(9.95872160899994,11.6,5.17350782199999));
#201890=CARTESIAN_POINT('Ctrl Pts',(9.96091418499994,15.2,5.17615730899998));
#201891=CARTESIAN_POINT('Ctrl Pts',(9.96091418499994,11.6,5.17615730899998));
#201892=CARTESIAN_POINT('Ctrl Pts',(9.96310774999994,15.2,5.17881223599999));
#201893=CARTESIAN_POINT('Ctrl Pts',(9.96310774999994,11.6,5.17881223599999));
#201894=CARTESIAN_POINT('Ctrl Pts',(9.96530229299994,15.2,5.18147260099998));
#201895=CARTESIAN_POINT('Ctrl Pts',(9.96530229299994,11.6,5.18147260099998));
#201896=CARTESIAN_POINT('Ctrl Pts',(9.96749780299995,15.2,5.18413840099999));
#201897=CARTESIAN_POINT('Ctrl Pts',(9.96749780299995,11.6,5.18413840099999));
#201898=CARTESIAN_POINT('Ctrl Pts',(9.96969427099994,15.2,5.18680963599999));
#201899=CARTESIAN_POINT('Ctrl Pts',(9.96969427099994,11.6,5.18680963599999));
#201900=CARTESIAN_POINT('Ctrl Pts',(9.97189168699995,15.2,5.18948630099998));
#201901=CARTESIAN_POINT('Ctrl Pts',(9.97189168699995,11.6,5.18948630099998));
#201902=CARTESIAN_POINT('Ctrl Pts',(9.97409004199995,15.2,5.19216839499999));
#201903=CARTESIAN_POINT('Ctrl Pts',(9.97409004199995,11.6,5.19216839499999));
#201904=CARTESIAN_POINT('Ctrl Pts',(9.97628932499994,15.2,5.19485591699999));
#201905=CARTESIAN_POINT('Ctrl Pts',(9.97628932499994,11.6,5.19485591699999));
#201906=CARTESIAN_POINT('Ctrl Pts',(9.97848952599995,15.2,5.19754886499998));
#201907=CARTESIAN_POINT('Ctrl Pts',(9.97848952599995,11.6,5.19754886499998));
#201908=CARTESIAN_POINT('Ctrl Pts',(9.98069063599995,15.2,5.20024723399998));
#201909=CARTESIAN_POINT('Ctrl Pts',(9.98069063599995,11.6,5.20024723399998));
#201910=CARTESIAN_POINT('Ctrl Pts',(9.98289264399994,15.2,5.20295102499999));
#201911=CARTESIAN_POINT('Ctrl Pts',(9.98289264399994,11.6,5.20295102499999));
#201912=CARTESIAN_POINT('Ctrl Pts',(9.98509554099994,15.2,5.20566023299998));
#201913=CARTESIAN_POINT('Ctrl Pts',(9.98509554099994,11.6,5.20566023299998));
#201914=CARTESIAN_POINT('Ctrl Pts',(9.98729931799994,15.2,5.20837485899998));
#201915=CARTESIAN_POINT('Ctrl Pts',(9.98729931799994,11.6,5.20837485899998));
#201916=CARTESIAN_POINT('Ctrl Pts',(9.98950396399995,15.2,5.21109489899998));
#201917=CARTESIAN_POINT('Ctrl Pts',(9.98950396399995,11.6,5.21109489899998));
#201918=CARTESIAN_POINT('Ctrl Pts',(9.99170946999994,15.2,5.21382035199998));
#201919=CARTESIAN_POINT('Ctrl Pts',(9.99170946999994,11.6,5.21382035199998));
#201920=CARTESIAN_POINT('Ctrl Pts',(9.99391582599995,15.2,5.21655121299998));
#201921=CARTESIAN_POINT('Ctrl Pts',(9.99391582599995,11.6,5.21655121299998));
#201922=CARTESIAN_POINT('Ctrl Pts',(9.99612302199995,15.2,5.21928748299998));
#201923=CARTESIAN_POINT('Ctrl Pts',(9.99612302199995,11.6,5.21928748299998));
#201924=CARTESIAN_POINT('Ctrl Pts',(9.99833104799994,15.2,5.22202915799999));
#201925=CARTESIAN_POINT('Ctrl Pts',(9.99833104799994,11.6,5.22202915799999));
#201926=CARTESIAN_POINT('Ctrl Pts',(10.0005398949999,15.2,5.22477623699999));
#201927=CARTESIAN_POINT('Ctrl Pts',(10.0005398949999,11.6,5.22477623699999));
#201928=CARTESIAN_POINT('Ctrl Pts',(10.0027495549999,15.2,5.22752871599998));
#201929=CARTESIAN_POINT('Ctrl Pts',(10.0027495549999,11.6,5.22752871599998));
#201930=CARTESIAN_POINT('Ctrl Pts',(10.0049600139999,15.2,5.23028659599999));
#201931=CARTESIAN_POINT('Ctrl Pts',(10.0049600139999,11.6,5.23028659599999));
#201932=CARTESIAN_POINT('Ctrl Pts',(10.0071712669999,15.2,5.23304987199998));
#201933=CARTESIAN_POINT('Ctrl Pts',(10.0071712669999,11.6,5.23304987199998));
#201934=CARTESIAN_POINT('Ctrl Pts',(10.0093833019999,15.2,5.23581854099999));
#201935=CARTESIAN_POINT('Ctrl Pts',(10.0093833019999,11.6,5.23581854099999));
#201936=CARTESIAN_POINT('Ctrl Pts',(10.0115961109999,15.2,5.23859260499999));
#201937=CARTESIAN_POINT('Ctrl Pts',(10.0115961109999,11.6,5.23859260499999));
#201938=CARTESIAN_POINT('Ctrl Pts',(10.0138096819999,15.2,5.24137205699999));
#201939=CARTESIAN_POINT('Ctrl Pts',(10.0138096819999,11.6,5.24137205699999));
#201940=CARTESIAN_POINT('Ctrl Pts',(10.0160240069999,15.2,5.24415689899998));
#201941=CARTESIAN_POINT('Ctrl Pts',(10.0160240069999,11.6,5.24415689899998));
#201942=CARTESIAN_POINT('Ctrl Pts',(10.0182390769999,15.2,5.24694712599998));
#201943=CARTESIAN_POINT('Ctrl Pts',(10.0182390769999,11.6,5.24694712599998));
#201944=CARTESIAN_POINT('Ctrl Pts',(10.0204548809999,15.2,5.24974273599998));
#201945=CARTESIAN_POINT('Ctrl Pts',(10.0204548809999,11.6,5.24974273599998));
#201946=CARTESIAN_POINT('Ctrl Pts',(10.0226714119999,15.2,5.25254372899998));
#201947=CARTESIAN_POINT('Ctrl Pts',(10.0226714119999,11.6,5.25254372899998));
#201948=CARTESIAN_POINT('Ctrl Pts',(10.0248886579999,15.2,5.25535009899999));
#201949=CARTESIAN_POINT('Ctrl Pts',(10.0248886579999,11.6,5.25535009899999));
#201950=CARTESIAN_POINT('Ctrl Pts',(10.0271066099999,15.2,5.25816184799999));
#201951=CARTESIAN_POINT('Ctrl Pts',(10.0271066099999,11.6,5.25816184799999));
#201952=CARTESIAN_POINT('Ctrl Pts',(10.0293252589999,15.2,5.26097896999998));
#201953=CARTESIAN_POINT('Ctrl Pts',(10.0293252589999,11.6,5.26097896999998));
#201954=CARTESIAN_POINT('Ctrl Pts',(10.0315445959999,15.2,5.26380146499999));
#201955=CARTESIAN_POINT('Ctrl Pts',(10.0315445959999,11.6,5.26380146499999));
#201956=CARTESIAN_POINT('Ctrl Pts',(10.0337646119999,15.2,5.26662933099999));
#201957=CARTESIAN_POINT('Ctrl Pts',(10.0337646119999,11.6,5.26662933099999));
#201958=CARTESIAN_POINT('Ctrl Pts',(10.0359852959999,15.2,5.26946256499999));
#201959=CARTESIAN_POINT('Ctrl Pts',(10.0359852959999,11.6,5.26946256499999));
#201960=CARTESIAN_POINT('Ctrl Pts',(10.0382066409999,15.2,5.27230116399998));
#201961=CARTESIAN_POINT('Ctrl Pts',(10.0382066409999,11.6,5.27230116399998));
#201962=CARTESIAN_POINT('Ctrl Pts',(10.0404286359999,15.2,5.27514512699998));
#201963=CARTESIAN_POINT('Ctrl Pts',(10.0404286359999,11.6,5.27514512699998));
#201964=CARTESIAN_POINT('Ctrl Pts',(10.0426512719999,15.2,5.27799445199998));
#201965=CARTESIAN_POINT('Ctrl Pts',(10.0426512719999,11.6,5.27799445199998));
#201966=CARTESIAN_POINT('Ctrl Pts',(10.0448745389999,15.2,5.28084913399999));
#201967=CARTESIAN_POINT('Ctrl Pts',(10.0448745389999,11.6,5.28084913399999));
#201968=CARTESIAN_POINT('Ctrl Pts',(10.0470984289999,15.2,5.28370917499998));
#201969=CARTESIAN_POINT('Ctrl Pts',(10.0470984289999,11.6,5.28370917499998));
#201970=CARTESIAN_POINT('Ctrl Pts',(10.0493229319999,15.2,5.28657456899998));
#201971=CARTESIAN_POINT('Ctrl Pts',(10.0493229319999,11.6,5.28657456899998));
#201972=CARTESIAN_POINT('Ctrl Pts',(10.0515480399999,15.2,5.28944531599999));
#201973=CARTESIAN_POINT('Ctrl Pts',(10.0515480399999,11.6,5.28944531599999));
#201974=CARTESIAN_POINT('Ctrl Pts',(10.0537737409999,15.2,5.29232141299998));
#201975=CARTESIAN_POINT('Ctrl Pts',(10.0537737409999,11.6,5.29232141299998));
#201976=CARTESIAN_POINT('Ctrl Pts',(10.0560000299999,15.2,5.29520285799999));
#201977=CARTESIAN_POINT('Ctrl Pts',(10.0560000299999,11.6,5.29520285799999));
#201978=CARTESIAN_POINT('Ctrl Pts',(10.0582268939999,15.2,5.29808964699999));
#201979=CARTESIAN_POINT('Ctrl Pts',(10.0582268939999,11.6,5.29808964699999));
#201980=CARTESIAN_POINT('Ctrl Pts',(10.0604543249999,15.2,5.30098177999999));
#201981=CARTESIAN_POINT('Ctrl Pts',(10.0604543249999,11.6,5.30098177999999));
#201982=CARTESIAN_POINT('Ctrl Pts',(10.0626823149999,15.2,5.30387925299999));
#201983=CARTESIAN_POINT('Ctrl Pts',(10.0626823149999,11.6,5.30387925299999));
#201984=CARTESIAN_POINT('Ctrl Pts',(10.0649108539999,15.2,5.30678206699999));
#201985=CARTESIAN_POINT('Ctrl Pts',(10.0649108539999,11.6,5.30678206699999));
#201986=CARTESIAN_POINT('Ctrl Pts',(10.0671399319999,15.2,5.30969021499998));
#201987=CARTESIAN_POINT('Ctrl Pts',(10.0671399319999,11.6,5.30969021499998));
#201988=CARTESIAN_POINT('Ctrl Pts',(10.0693695419999,15.2,5.31260369799998));
#201989=CARTESIAN_POINT('Ctrl Pts',(10.0693695419999,11.6,5.31260369799998));
#201990=CARTESIAN_POINT('Ctrl Pts',(10.0715996729999,15.2,5.31552251199999));
#201991=CARTESIAN_POINT('Ctrl Pts',(10.0715996729999,11.6,5.31552251199999));
#201992=CARTESIAN_POINT('Ctrl Pts',(10.0738303179999,15.2,5.31844665599999));
#201993=CARTESIAN_POINT('Ctrl Pts',(10.0738303179999,11.6,5.31844665599999));
#201994=CARTESIAN_POINT('Ctrl Pts',(10.0760614659999,15.2,5.32137612699999));
#201995=CARTESIAN_POINT('Ctrl Pts',(10.0760614659999,11.6,5.32137612699999));
#201996=CARTESIAN_POINT('Ctrl Pts',(10.0782931079999,15.2,5.32431092299999));
#201997=CARTESIAN_POINT('Ctrl Pts',(10.0782931079999,11.6,5.32431092299999));
#201998=CARTESIAN_POINT('Ctrl Pts',(10.0805252349999,15.2,5.32725104099999));
#201999=CARTESIAN_POINT('Ctrl Pts',(10.0805252349999,11.6,5.32725104099999));
#202000=CARTESIAN_POINT('Ctrl Pts',(10.0827578399999,15.2,5.33019647899999));
#202001=CARTESIAN_POINT('Ctrl Pts',(10.0827578399999,11.6,5.33019647899999));
#202002=CARTESIAN_POINT('Ctrl Pts',(10.0849909119999,15.2,5.33314723499998));
#202003=CARTESIAN_POINT('Ctrl Pts',(10.0849909119999,11.6,5.33314723499998));
#202004=CARTESIAN_POINT('Ctrl Pts',(10.0872244429999,15.2,5.33610330699998));
#202005=CARTESIAN_POINT('Ctrl Pts',(10.0872244429999,11.6,5.33610330699998));
#202006=CARTESIAN_POINT('Ctrl Pts',(10.0894584239999,15.2,5.33906469199999));
#202007=CARTESIAN_POINT('Ctrl Pts',(10.0894584239999,11.6,5.33906469199999));
#202008=CARTESIAN_POINT('Ctrl Pts',(10.0916928469999,15.2,5.34203138799998));
#202009=CARTESIAN_POINT('Ctrl Pts',(10.0916928469999,11.6,5.34203138799998));
#202010=CARTESIAN_POINT('Ctrl Pts',(10.0939277019999,15.2,5.34500339199998));
#202011=CARTESIAN_POINT('Ctrl Pts',(10.0939277019999,11.6,5.34500339199998));
#202012=CARTESIAN_POINT('Ctrl Pts',(10.0961629809999,15.2,5.34798070299999));
#202013=CARTESIAN_POINT('Ctrl Pts',(10.0961629809999,11.6,5.34798070299999));
#202014=CARTESIAN_POINT('Ctrl Pts',(10.0983986739999,15.2,5.35096331799998));
#202015=CARTESIAN_POINT('Ctrl Pts',(10.0983986739999,11.6,5.35096331799998));
#202016=CARTESIAN_POINT('Ctrl Pts',(10.1006347719999,15.2,5.35395123399999));
#202017=CARTESIAN_POINT('Ctrl Pts',(10.1006347719999,11.6,5.35395123399999));
#202018=CARTESIAN_POINT('Ctrl Pts',(10.1028712649999,15.2,5.35694444899999));
#202019=CARTESIAN_POINT('Ctrl Pts',(10.1028712649999,11.6,5.35694444899999));
#202020=CARTESIAN_POINT('Ctrl Pts',(10.1051081459999,15.2,5.35994296199998));
#202021=CARTESIAN_POINT('Ctrl Pts',(10.1051081459999,11.6,5.35994296199998));
#202022=CARTESIAN_POINT('Ctrl Pts',(10.1073454039999,15.2,5.36294676699999));
#202023=CARTESIAN_POINT('Ctrl Pts',(10.1073454039999,11.6,5.36294676699999));
#202024=CARTESIAN_POINT('Ctrl Pts',(10.1095830319999,15.2,5.36595586499999));
#202025=CARTESIAN_POINT('Ctrl Pts',(10.1095830319999,11.6,5.36595586499999));
#202026=CARTESIAN_POINT('Ctrl Pts',(10.1118210219999,15.2,5.36897025299999));
#202027=CARTESIAN_POINT('Ctrl Pts',(10.1118210219999,11.6,5.36897025299999));
#202028=CARTESIAN_POINT('Ctrl Pts',(10.1140593669999,15.2,5.37198992899998));
#202029=CARTESIAN_POINT('Ctrl Pts',(10.1140593669999,11.6,5.37198992899998));
#202030=CARTESIAN_POINT('Ctrl Pts',(10.1162980569999,15.2,5.37501488899998));
#202031=CARTESIAN_POINT('Ctrl Pts',(10.1162980569999,11.6,5.37501488899998));
#202032=CARTESIAN_POINT('Ctrl Pts',(10.1185370849999,15.2,5.37804513399998));
#202033=CARTESIAN_POINT('Ctrl Pts',(10.1185370849999,11.6,5.37804513399998));
#202034=CARTESIAN_POINT('Ctrl Pts',(10.1207764439999,15.2,5.38108065899999));
#202035=CARTESIAN_POINT('Ctrl Pts',(10.1207764439999,11.6,5.38108065899999));
#202036=CARTESIAN_POINT('Ctrl Pts',(10.1230161179999,15.2,5.38412146299999));
#202037=CARTESIAN_POINT('Ctrl Pts',(10.1230161179999,11.6,5.38412146299999));
#202038=CARTESIAN_POINT('Ctrl Pts',(10.1252561029999,15.2,5.38716754199999));
#202039=CARTESIAN_POINT('Ctrl Pts',(10.1252561029999,11.6,5.38716754199999));
#202040=CARTESIAN_POINT('Ctrl Pts',(10.1274963839999,15.2,5.39021889299999));
#202041=CARTESIAN_POINT('Ctrl Pts',(10.1274963839999,11.6,5.39021889299999));
#202042=CARTESIAN_POINT('Ctrl Pts',(10.1297369509999,15.2,5.39327551299999));
#202043=CARTESIAN_POINT('Ctrl Pts',(10.1297369509999,11.6,5.39327551299999));
#202044=CARTESIAN_POINT('Ctrl Pts',(10.1319777959999,15.2,5.39633739999999));
#202045=CARTESIAN_POINT('Ctrl Pts',(10.1319777959999,11.6,5.39633739999999));
#202046=CARTESIAN_POINT('Ctrl Pts',(10.1342189099999,15.2,5.39940455199999));
#202047=CARTESIAN_POINT('Ctrl Pts',(10.1342189099999,11.6,5.39940455199999));
#202048=CARTESIAN_POINT('Ctrl Pts',(10.1364602879999,15.2,5.40247696699999));
#202049=CARTESIAN_POINT('Ctrl Pts',(10.1364602879999,11.6,5.40247696699999));
#202050=CARTESIAN_POINT('Ctrl Pts',(10.1387019259999,15.2,5.40555464399999));
#202051=CARTESIAN_POINT('Ctrl Pts',(10.1387019259999,11.6,5.40555464399999));
#202052=CARTESIAN_POINT('Ctrl Pts',(10.1409438219999,15.2,5.40863758099999));
#202053=CARTESIAN_POINT('Ctrl Pts',(10.1409438219999,11.6,5.40863758099999));
#202054=CARTESIAN_POINT('Ctrl Pts',(10.1427375439999,15.2,5.41110813999998));
#202055=CARTESIAN_POINT('Ctrl Pts',(10.1427375439999,11.6,5.41110813999998));
#202056=CARTESIAN_POINT('Ctrl Pts',(10.1440829499999,15.2,5.41296342599999));
#202057=CARTESIAN_POINT('Ctrl Pts',(10.1440829499999,11.6,5.41296342599999));
#202058=CARTESIAN_POINT('Ctrl Pts',(10.1449799389999,15.2,5.41420133599999));
#202059=CARTESIAN_POINT('Ctrl Pts',(10.1449799389999,11.6,5.41420133599999));
#202060=CARTESIAN_POINT('Ctrl Pts',(10.1454284469999,15.2,5.41482055299999));
#202061=CARTESIAN_POINT('Ctrl Pts',(10.1454284469999,11.6,5.41482055299999));
#202062=CARTESIAN_POINT('Ctrl Pts',(9.31239140099994,15.2,4.57383771099998));
#202063=CARTESIAN_POINT('Ctrl Pts',(9.31392144680189,15.2,4.57476026769956));
#202064=CARTESIAN_POINT('Ctrl Pts',(9.31549767341897,15.2,4.57571692949402));
#202065=CARTESIAN_POINT('Ctrl Pts',(9.31711891381397,15.2,4.57670776739141));
#202066=CARTESIAN_POINT('Ctrl Pts',(9.31874797264965,15.2,4.57770338360999));
#202067=CARTESIAN_POINT('Ctrl Pts',(9.32042248385082,15.2,4.57873349868146));
#202068=CARTESIAN_POINT('Ctrl Pts',(9.32214129986625,15.2,4.57979816304467));
#202069=CARTESIAN_POINT('Ctrl Pts',(9.3241465849834,15.2,4.58104027132335));
#202070=CARTESIAN_POINT('Ctrl Pts',(9.32621217660936,15.2,4.58232940557774));
#202071=CARTESIAN_POINT('Ctrl Pts',(9.32833631004309,15.2,4.58366563461676));
#202072=CARTESIAN_POINT('Ctrl Pts',(9.33015699605605,15.2,4.58481097392682));
#202073=CARTESIAN_POINT('Ctrl Pts',(9.33202069553284,15.2,4.58599091516364));
#202074=CARTESIAN_POINT('Ctrl Pts',(9.33392633190099,15.2,4.58720549637584));
#202075=CARTESIAN_POINT('Ctrl Pts',(9.33614957407085,15.2,4.58862250762459));
#202076=CARTESIAN_POINT('Ctrl Pts',(9.33842989701372,15.2,4.59008667009452));
#202077=CARTESIAN_POINT('Ctrl Pts',(9.34076564432333,15.2,4.59159803785873));
#202078=CARTESIAN_POINT('Ctrl Pts',(9.34276771367966,15.2,4.59289349609363));
#202079=CARTESIAN_POINT('Ctrl Pts',(9.34481050330659,15.2,4.59422363630412));
#202080=CARTESIAN_POINT('Ctrl Pts',(9.3468930019431,15.2,4.59558849061538));
#202081=CARTESIAN_POINT('Ctrl Pts',(9.34932258340195,15.2,4.59718082045921));
#202082=CARTESIAN_POINT('Ctrl Pts',(9.35180621226842,15.2,4.59882039919461));
#202083=CARTESIAN_POINT('Ctrl Pts',(9.35434232328794,15.2,4.600507268809));
#202084=CARTESIAN_POINT('Ctrl Pts',(9.35651613298711,15.2,4.60195315721876));
#202085=CARTESIAN_POINT('Ctrl Pts',(9.35872850338876,15.2,4.6034337928863));
#202086=CARTESIAN_POINT('Ctrl Pts',(9.3609784792093,15.2,4.60494919521327));
#202087=CARTESIAN_POINT('Ctrl Pts',(9.36360345069336,15.2,4.60671716438827));
#202088=CARTESIAN_POINT('Ctrl Pts',(9.36627960436232,15.2,4.60853245688356));
#202089=CARTESIAN_POINT('Ctrl Pts',(9.36900546349522,15.2,4.61039510533424));
#202090=CARTESIAN_POINT('Ctrl Pts',(9.37134191445341,15.2,4.61199166133557));
#202091=CARTESIAN_POINT('Ctrl Pts',(9.37371488616263,15.2,4.61362300806846));
#202092=CARTESIAN_POINT('Ctrl Pts',(9.37612347224964,15.2,4.61528916141119));
#202093=CARTESIAN_POINT('Ctrl Pts',(9.37853205811786,15.2,4.61695531460258));
#202094=CARTESIAN_POINT('Ctrl Pts',(9.38097625855661,15.2,4.61865627504632));
#202095=CARTESIAN_POINT('Ctrl Pts',(9.38345519046654,15.2,4.62039205498325));
#202096=CARTESIAN_POINT('Ctrl Pts',(9.38593412237647,15.2,4.62212783492018));
#202097=CARTESIAN_POINT('Ctrl Pts',(9.38844778575411,15.2,4.62389843460277));
#202098=CARTESIAN_POINT('Ctrl Pts',(9.39099531978686,15.2,4.62570386362536));
#202099=CARTESIAN_POINT('Ctrl Pts',(9.39354285405101,15.2,4.62750929281193));
#202100=CARTESIAN_POINT('Ctrl Pts',(9.39612425591511,15.2,4.62934954974141));
#202101=CARTESIAN_POINT('Ctrl Pts',(9.39873868897653,15.2,4.63122464292932));
#202102=CARTESIAN_POINT('Ctrl Pts',(9.40135312180048,15.2,4.63309973594691));
#202103=CARTESIAN_POINT('Ctrl Pts',(9.40400058107225,15.2,4.63500966558724));
#202104=CARTESIAN_POINT('Ctrl Pts',(9.40668024822489,15.2,4.63695443351659));
#202105=CARTESIAN_POINT('Ctrl Pts',(9.4098065267319,15.2,4.63922332955191));
#202106=CARTESIAN_POINT('Ctrl Pts',(9.41297664099816,15.2,4.6415396452332));
#202107=CARTESIAN_POINT('Ctrl Pts',(9.41618931726636,15.2,4.64390338215434));
#202108=CARTESIAN_POINT('Ctrl Pts',(9.41894303963903,15.2,4.6459294422673));
#202109=CARTESIAN_POINT('Ctrl Pts',(9.42172803225219,15.2,4.6479903423594));
#202110=CARTESIAN_POINT('Ctrl Pts',(9.42454351448322,15.2,4.65008607928325));
#202111=CARTESIAN_POINT('Ctrl Pts',(9.42735899671425,15.2,4.65218181620711));
#202112=CARTESIAN_POINT('Ctrl Pts',(9.43020496568432,15.2,4.65431239024637));
#202113=CARTESIAN_POINT('Ctrl Pts',(9.43308065822178,15.2,4.65647779627387));
#202114=CARTESIAN_POINT('Ctrl Pts',(9.43595635102045,15.2,4.65864320249805));
#202115=CARTESIAN_POINT('Ctrl Pts',(9.43886176683284,15.2,4.6608434404277));
#202116=CARTESIAN_POINT('Ctrl Pts',(9.44179615657809,15.2,4.66307850346856));
#202117=CARTESIAN_POINT('Ctrl Pts',(9.44473054605679,15.2,4.6653135663064));
#202118=CARTESIAN_POINT('Ctrl Pts',(9.44769390903798,15.2,4.66758345288251));
#202119=CARTESIAN_POINT('Ctrl Pts',(9.45068551352626,15.2,4.66988815372597));
#202120=CARTESIAN_POINT('Ctrl Pts',(9.45367711801453,15.2,4.67219285456944));
#202121=CARTESIAN_POINT('Ctrl Pts',(9.45669696187919,15.2,4.67453236995845));
#202122=CARTESIAN_POINT('Ctrl Pts',(9.4597443296006,15.2,4.67690668587067));
#202123=CARTESIAN_POINT('Ctrl Pts',(9.46279169759881,15.2,4.67928100199854));
#202124=CARTESIAN_POINT('Ctrl Pts',(9.46586658883378,15.2,4.68169012056408));
#202125=CARTESIAN_POINT('Ctrl Pts',(9.46896829983799,15.2,4.68413402553298));
#202126=CARTESIAN_POINT('Ctrl Pts',(9.47207001056045,15.2,4.68657793027989));
#202127=CARTESIAN_POINT('Ctrl Pts',(9.47519854057708,15.2,4.68905661983519));
#202128=CARTESIAN_POINT('Ctrl Pts',(9.47835320238027,15.2,4.69157007966205));
#202129=CARTESIAN_POINT('Ctrl Pts',(9.48098208731177,15.2,4.69366462959387));
#202130=CARTESIAN_POINT('Ctrl Pts',(9.48362911829559,15.2,4.69578332435561));
#202131=CARTESIAN_POINT('Ctrl Pts',(9.48629390565762,15.2,4.69792615414854));
#202132=CARTESIAN_POINT('Ctrl Pts',(9.48895869301966,15.2,4.70006898394147));
#202133=CARTESIAN_POINT('Ctrl Pts',(9.49164123368286,15.2,4.70223594668768));
#202134=CARTESIAN_POINT('Ctrl Pts',(9.49434114701338,15.2,4.70442703172936));
#202135=CARTESIAN_POINT('Ctrl Pts',(9.49758104289229,15.2,4.70705633368384));
#202136=CARTESIAN_POINT('Ctrl Pts',(9.50084595104441,15.2,4.70972037065632));
#202137=CARTESIAN_POINT('Ctrl Pts',(9.50413521800823,15.2,4.71241912047492));
#202138=CARTESIAN_POINT('Ctrl Pts',(9.506876273911,15.2,4.7146680787388));
#202139=CARTESIAN_POINT('Ctrl Pts',(9.50963424740545,15.2,4.71694114255181));
#202140=CARTESIAN_POINT('Ctrl Pts',(9.51240876575141,15.2,4.71923829749285));
#202141=CARTESIAN_POINT('Ctrl Pts',(9.51518328409738,15.2,4.72153545243388));
#202142=CARTESIAN_POINT('Ctrl Pts',(9.51797434704942,15.2,4.72385669998554));
#202143=CARTESIAN_POINT('Ctrl Pts',(9.52078159038359,15.2,4.72620202165345));
#202144=CARTESIAN_POINT('Ctrl Pts',(9.52358883371776,15.2,4.72854734332137));
#202145=CARTESIAN_POINT('Ctrl Pts',(9.5264122556293,15.2,4.73091674199979));
#202146=CARTESIAN_POINT('Ctrl Pts',(9.52925149743569,15.2,4.73331019943161));
#202147=CARTESIAN_POINT('Ctrl Pts',(9.5320907392421,15.2,4.73570365686343));
#202148=CARTESIAN_POINT('Ctrl Pts',(9.53494579974981,15.2,4.73812117432644));
#202149=CARTESIAN_POINT('Ctrl Pts',(9.53781632732485,15.2,4.74056273278344));
#202150=CARTESIAN_POINT('Ctrl Pts',(9.5406868548999,15.2,4.74300429124043));
#202151=CARTESIAN_POINT('Ctrl Pts',(9.54357284558923,15.2,4.74546989248472));
#202152=CARTESIAN_POINT('Ctrl Pts',(9.54647395260438,15.2,4.74795951804224));
#202153=CARTESIAN_POINT('Ctrl Pts',(9.54937505961951,15.2,4.75044914359977));
#202154=CARTESIAN_POINT('Ctrl Pts',(9.55229128383209,15.2,4.75296279255213));
#202155=CARTESIAN_POINT('Ctrl Pts',(9.55522227987495,15.2,4.75550044658186));
#202156=CARTESIAN_POINT('Ctrl Pts',(9.55815327559833,15.2,4.75803810033498));
#202157=CARTESIAN_POINT('Ctrl Pts',(9.56109904322545,15.2,4.76059975867886));
#202158=CARTESIAN_POINT('Ctrl Pts',(9.56405924484605,15.2,4.76318540089507));
#202159=CARTESIAN_POINT('Ctrl Pts',(9.56701944678933,15.2,4.76577104339312));
#202160=CARTESIAN_POINT('Ctrl Pts',(9.56999408210459,15.2,4.76838067212409));
#202161=CARTESIAN_POINT('Ctrl Pts',(9.57298281661732,15.2,4.77101426441379));
#202162=CARTESIAN_POINT('Ctrl Pts',(9.57597155113005,15.2,4.77364785670349));
#202163=CARTESIAN_POINT('Ctrl Pts',(9.57897438605647,15.2,4.77630541258449));
#202164=CARTESIAN_POINT('Ctrl Pts',(9.58199099209701,15.2,4.77898691070753));
#202165=CARTESIAN_POINT('Ctrl Pts',(9.58500759813753,15.2,4.78166840883055));
#202166=CARTESIAN_POINT('Ctrl Pts',(9.58803797611216,15.2,4.78437384907626));
#202167=CARTESIAN_POINT('Ctrl Pts',(9.59108179917995,15.2,4.78710320914151));
#202168=CARTESIAN_POINT('Ctrl Pts',(9.59412562224773,15.2,4.78983256920675));
#202169=CARTESIAN_POINT('Ctrl Pts',(9.59718289246654,15.2,4.79258584833636));
#202170=CARTESIAN_POINT('Ctrl Pts',(9.60025328954919,15.2,4.79536302479344));
#202171=CARTESIAN_POINT('Ctrl Pts',(9.60332368663183,15.2,4.79814020125053));
#202172=CARTESIAN_POINT('Ctrl Pts',(9.60640721154263,15.2,4.8009412744277));
#202173=CARTESIAN_POINT('Ctrl Pts',(9.60950354855582,15.2,4.80376621852365));
#202174=CARTESIAN_POINT('Ctrl Pts',(9.61198061830137,15.2,4.80602617392358));
#202175=CARTESIAN_POINT('Ctrl Pts',(9.61446588720061,15.2,4.80830140828345));
#202176=CARTESIAN_POINT('Ctrl Pts',(9.61695919712842,15.2,4.81059190835738));
#202177=CARTESIAN_POINT('Ctrl Pts',(9.62007583436833,15.2,4.81345503329373));
#202178=CARTESIAN_POINT('Ctrl Pts',(9.62320503513204,15.2,4.81634201014538));
#202179=CARTESIAN_POINT('Ctrl Pts',(9.62634649145248,15.2,4.81925281410566));
#202180=CARTESIAN_POINT('Ctrl Pts',(9.62885965630339,15.2,4.82158145708352));
#202181=CARTESIAN_POINT('Ctrl Pts',(9.6313806654227,15.2,4.82392534914551));
#202182=CARTESIAN_POINT('Ctrl Pts',(9.6339093623266,15.2,4.82628447684054));
#202183=CARTESIAN_POINT('Ctrl Pts',(9.63707023371486,15.2,4.82923338670041));
#202184=CARTESIAN_POINT('Ctrl Pts',(9.64024311945042,15.2,4.8322061040292));
#202185=CARTESIAN_POINT('Ctrl Pts',(9.64342771675651,15.2,4.83520259897329));
#202186=CARTESIAN_POINT('Ctrl Pts',(9.64597539474023,15.2,4.83759979505921));
#202187=CARTESIAN_POINT('Ctrl Pts',(9.64853057095349,15.2,4.84001220998522));
#202188=CARTESIAN_POINT('Ctrl Pts',(9.65109309092722,15.2,4.84243982989685));
#202189=CARTESIAN_POINT('Ctrl Pts',(9.65429624071982,15.2,4.845474354621));
#202190=CARTESIAN_POINT('Ctrl Pts',(9.65751086726542,15.2,4.8485326364567));
#202191=CARTESIAN_POINT('Ctrl Pts',(9.66073667698853,15.2,4.85161464715307));
#202192=CARTESIAN_POINT('Ctrl Pts',(9.66396248636002,15.2,4.85469665751349));
#202193=CARTESIAN_POINT('Ctrl Pts',(9.66719948033001,15.2,4.85780239751699));
#202194=CARTESIAN_POINT('Ctrl Pts',(9.6704473681001,15.2,4.86093183779893));
#202195=CARTESIAN_POINT('Ctrl Pts',(9.67304567874099,15.2,4.86343539043382));
#202196=CARTESIAN_POINT('Ctrl Pts',(9.6756509615242,15.2,4.86595411075348));
#202197=CARTESIAN_POINT('Ctrl Pts',(9.67826307199992,15.2,4.86848798472493));
#202198=CARTESIAN_POINT('Ctrl Pts',(9.68087518247563,15.2,4.87102185869638));
#202199=CARTESIAN_POINT('Ctrl Pts',(9.68349411904933,15.2,4.87357088501956));
#202200=CARTESIAN_POINT('Ctrl Pts',(9.68611973713754,15.2,4.87613504966084));
#202201=CARTESIAN_POINT('Ctrl Pts',(9.68874535486801,15.2,4.87869921395275));
#202202=CARTESIAN_POINT('Ctrl Pts',(9.69137765619632,15.2,4.88127851639296));
#202203=CARTESIAN_POINT('Ctrl Pts',(9.69401649521479,15.2,4.88387294074816));
#202204=CARTESIAN_POINT('Ctrl Pts',(9.69665533459279,15.2,4.88646736545686));
#202205=CARTESIAN_POINT('Ctrl Pts',(9.69930071187999,15.2,4.88907691186781));
#202206=CARTESIAN_POINT('Ctrl Pts',(9.70195248719182,15.2,4.89170156567906));
#202207=CARTESIAN_POINT('Ctrl Pts',(9.70460426214236,15.2,4.89432621913271));
#202208=CARTESIAN_POINT('Ctrl Pts',(9.70726243417816,15.2,4.89696597790938));
#202209=CARTESIAN_POINT('Ctrl Pts',(9.70992686251549,15.2,4.8996208275247));
#202210=CARTESIAN_POINT('Ctrl Pts',(9.71325739820943,15.2,4.90293938981514));
#202211=CARTESIAN_POINT('Ctrl Pts',(9.71659771088846,15.2,4.90628153051064));
#202212=CARTESIAN_POINT('Ctrl Pts',(9.71994752826477,15.2,4.9096472177481));
#202213=CARTESIAN_POINT('Ctrl Pts',(9.72262738231187,15.2,4.91233976768481));
#202214=CARTESIAN_POINT('Ctrl Pts',(9.72531332028995,15.2,4.91504738687294));
#202215=CARTESIAN_POINT('Ctrl Pts',(9.72800520371505,15.2,4.91777005891176));
#202216=CARTESIAN_POINT('Ctrl Pts',(9.73137005781304,15.2,4.92117339877481));
#202217=CARTESIAN_POINT('Ctrl Pts',(9.73474420341393,15.2,4.92460025986044));
#202218=CARTESIAN_POINT('Ctrl Pts',(9.73812737494245,15.2,4.92805060791791));
#202219=CARTESIAN_POINT('Ctrl Pts',(9.74218718062915,15.2,4.93219102543644));
#202220=CARTESIAN_POINT('Ctrl Pts',(9.74625998326219,15.2,4.93636526424749));
#202221=CARTESIAN_POINT('Ctrl Pts',(9.75034533119763,15.2,4.94057326576273));
#202222=CARTESIAN_POINT('Ctrl Pts',(9.75306889636423,15.2,4.94337859997882));
#202223=CARTESIAN_POINT('Ctrl Pts',(9.75579803803804,15.2,4.94619893955857));
#202224=CARTESIAN_POINT('Ctrl Pts',(9.75853262303615,15.2,4.94903426776969));
#202225=CARTESIAN_POINT('Ctrl Pts',(9.76126720840685,15.2,4.95186959636712));
#202226=CARTESIAN_POINT('Ctrl Pts',(9.76400723839524,15.2,4.95471991376043));
#202227=CARTESIAN_POINT('Ctrl Pts',(9.76675258000179,15.2,4.95758520048521));
#202228=CARTESIAN_POINT('Ctrl Pts',(9.77018425682296,15.2,4.961166808696));
#202229=CARTESIAN_POINT('Ctrl Pts',(9.77362423554171,15.2,4.96477180800835));
#202230=CARTESIAN_POINT('Ctrl Pts',(9.7770722622088,15.2,4.96840016349569));
#202231=CARTESIAN_POINT('Ctrl Pts',(9.78120989405898,15.2,4.9727541899223));
#202232=CARTESIAN_POINT('Ctrl Pts',(9.7853591148332,15.2,4.97714184755452));
#202233=CARTESIAN_POINT('Ctrl Pts',(9.7895194927649,15.2,4.98156307605911));
#202234=CARTESIAN_POINT('Ctrl Pts',(9.79229307830464,15.2,4.98451056199657));
#202235=CARTESIAN_POINT('Ctrl Pts',(9.79507162314495,15.2,4.98747296791077));
#202236=CARTESIAN_POINT('Ctrl Pts',(9.79785500068584,15.2,4.99045027401846));
#202237=CARTESIAN_POINT('Ctrl Pts',(9.80063837784751,15.2,4.99342757972049));
#202238=CARTESIAN_POINT('Ctrl Pts',(9.80342658838388,15.2,4.99641978802167));
#202239=CARTESIAN_POINT('Ctrl Pts',(9.80621950562802,15.2,4.99942687781366));
#202240=CARTESIAN_POINT('Ctrl Pts',(9.80901242325269,15.2,5.00243396801537));
#202241=CARTESIAN_POINT('Ctrl Pts',(9.81181004814268,15.2,5.00545594064017));
#202242=CARTESIAN_POINT('Ctrl Pts',(9.81461225696239,15.2,5.00849277597333));
#202243=CARTESIAN_POINT('Ctrl Pts',(9.81811501779612,15.2,5.0122888199329));
#202244=CARTESIAN_POINT('Ctrl Pts',(9.82162493830183,15.2,5.0161080877446));
#202245=CARTESIAN_POINT('Ctrl Pts',(9.82514178170497,15.2,5.0199505422597));
#202246=CARTESIAN_POINT('Ctrl Pts',(9.82795525619748,15.2,5.02302450562049));
#202247=CARTESIAN_POINT('Ctrl Pts',(9.83077316071664,15.2,5.02611330600517));
#202248=CARTESIAN_POINT('Ctrl Pts',(9.83359537334877,15.2,5.02921692701632));
#202249=CARTESIAN_POINT('Ctrl Pts',(9.83641758636542,15.2,5.03232054845034));
#202250=CARTESIAN_POINT('Ctrl Pts',(9.83924410719627,15.2,5.03543898857892));
#202251=CARTESIAN_POINT('Ctrl Pts',(9.84207481673971,15.2,5.03857222797288));
#202252=CARTESIAN_POINT('Ctrl Pts',(9.8463208806692,15.2,5.04327208663693));
#202253=CARTESIAN_POINT('Ctrl Pts',(9.85057636513958,15.2,5.04800524459828));
#202254=CARTESIAN_POINT('Ctrl Pts',(9.85484087198422,15.2,5.05277163225696));
#202255=CARTESIAN_POINT('Ctrl Pts',(9.8583946278172,15.2,5.05674362211684));
#202256=CARTESIAN_POINT('Ctrl Pts',(9.86195464797069,15.2,5.06073868942956));
#202257=CARTESIAN_POINT('Ctrl Pts',(9.86552070222298,15.2,5.06475679403107));
#202258=CARTESIAN_POINT('Ctrl Pts',(9.86837354578029,15.2,5.06797127788747));
#202259=CARTESIAN_POINT('Ctrl Pts',(9.87123025165023,15.2,5.07120050477702));
#202260=CARTESIAN_POINT('Ctrl Pts',(9.87409070325095,15.2,5.07444445478866));
#202261=CARTESIAN_POINT('Ctrl Pts',(9.87695115446193,15.2,5.07768840435831));
#202262=CARTESIAN_POINT('Ctrl Pts',(9.87981535064186,15.2,5.08094707681769));
#202263=CARTESIAN_POINT('Ctrl Pts',(9.88268317724052,15.2,5.0842204522158));
#202264=CARTESIAN_POINT('Ctrl Pts',(9.88555100422991,15.2,5.08749382805992));
#202265=CARTESIAN_POINT('Ctrl Pts',(9.88842246157484,15.2,5.09078190533578));
#202266=CARTESIAN_POINT('Ctrl Pts',(9.8912974347088,15.2,5.0940846647376));
#202267=CARTESIAN_POINT('Ctrl Pts',(9.89417240745102,15.2,5.09738742368943));
#202268=CARTESIAN_POINT('Ctrl Pts',(9.89705089599465,15.2,5.10070486265938));
#202269=CARTESIAN_POINT('Ctrl Pts',(9.89993278598103,15.2,5.10403696221933));
#202270=CARTESIAN_POINT('Ctrl Pts',(9.90425562154958,15.2,5.10903511224024));
#202271=CARTESIAN_POINT('Ctrl Pts',(9.90858611391919,15.2,5.11406624694868));
#202272=CARTESIAN_POINT('Ctrl Pts',(9.91292388048942,15.2,5.11913029581025));
#202273=CARTESIAN_POINT('Ctrl Pts',(9.91509276357754,15.2,5.12166232001104));
#202274=CARTESIAN_POINT('Ctrl Pts',(9.91726346590713,15.2,5.12420257192406));
#202275=CARTESIAN_POINT('Ctrl Pts',(9.91943593968694,15.2,5.12675104325142));
#202276=CARTESIAN_POINT('Ctrl Pts',(9.92160841346676,15.2,5.12929951457876));
#202277=CARTESIAN_POINT('Ctrl Pts',(9.92378266033273,15.2,5.13185620382213));
#202278=CARTESIAN_POINT('Ctrl Pts',(9.92595863196215,15.2,5.13442110397965));
#202279=CARTESIAN_POINT('Ctrl Pts',(9.92813460359157,15.2,5.13698600413717));
#202280=CARTESIAN_POINT('Ctrl Pts',(9.93031230121245,15.2,5.13955911407704));
#202281=CARTESIAN_POINT('Ctrl Pts',(9.93249167775827,15.2,5.14214042431659));
#202282=CARTESIAN_POINT('Ctrl Pts',(9.93467105430408,15.2,5.14472173455614));
#202283=CARTESIAN_POINT('Ctrl Pts',(9.93685210942485,15.2,5.1473112456787));
#202284=CARTESIAN_POINT('Ctrl Pts',(9.93903479801204,15.2,5.14990894795858));
#202285=CARTESIAN_POINT('Ctrl Pts',(9.94121748659924,15.2,5.15250665023845));
#202286=CARTESIAN_POINT('Ctrl Pts',(9.94340180833077,15.2,5.15511254434293));
#202287=CARTESIAN_POINT('Ctrl Pts',(9.94558771752703,15.2,5.15772661979425));
#202288=CARTESIAN_POINT('Ctrl Pts',(9.94777362672328,15.2,5.16034069524556));
#202289=CARTESIAN_POINT('Ctrl Pts',(9.94996112375248,15.2,5.16296295360654));
#202290=CARTESIAN_POINT('Ctrl Pts',(9.95215016229772,15.2,5.1655933834265));
#202291=CARTESIAN_POINT('Ctrl Pts',(9.95433920124064,15.2,5.16822381372433));
#202292=CARTESIAN_POINT('Ctrl Pts',(9.9565297817257,15.2,5.17086241685783));
#202293=CARTESIAN_POINT('Ctrl Pts',(9.95872185875282,15.2,5.17350918307693));
#202294=CARTESIAN_POINT('Ctrl Pts',(9.96237531993369,15.2,5.17792045946768));
#202295=CARTESIAN_POINT('Ctrl Pts',(9.96603293980633,15.2,5.18235441119767));
#202296=CARTESIAN_POINT('Ctrl Pts',(9.9696945084872,15.2,5.18681099411619));
#202297=CARTESIAN_POINT('Ctrl Pts',(9.97189144961591,15.2,5.18948494377015));
#202298=CARTESIAN_POINT('Ctrl Pts',(9.97408981369542,15.2,5.19216703924958));
#202299=CARTESIAN_POINT('Ctrl Pts',(9.97628955493388,15.2,5.1948572739955));
#202300=CARTESIAN_POINT('Ctrl Pts',(9.97848929617234,15.2,5.19754750874142));
#202301=CARTESIAN_POINT('Ctrl Pts',(9.98069041481994,15.2,5.20024588035938));
#202302=CARTESIAN_POINT('Ctrl Pts',(9.98289286649003,15.2,5.20295237959508));
#202303=CARTESIAN_POINT('Ctrl Pts',(9.98509531816012,15.2,5.20565887883078));
#202304=CARTESIAN_POINT('Ctrl Pts',(9.98729910386338,15.2,5.20837350606551));
#202305=CARTESIAN_POINT('Ctrl Pts',(9.98950417899161,15.2,5.21109625221659));
#202306=CARTESIAN_POINT('Ctrl Pts',(9.99170925411983,15.2,5.21381899836768));
#202307=CARTESIAN_POINT('Ctrl Pts',(9.99391561913965,15.2,5.21654986178508));
#202308=CARTESIAN_POINT('Ctrl Pts',(9.99612322926766,15.2,5.21928883397652));
#202309=CARTESIAN_POINT('Ctrl Pts',(9.99833083939567,15.2,5.22202780616795));
#202310=CARTESIAN_POINT('Ctrl Pts',(10.0005396956591,15.2,5.22477488629702));
#202311=CARTESIAN_POINT('Ctrl Pts',(10.0027497543974,15.2,5.22753006566695));
#202312=CARTESIAN_POINT('Ctrl Pts',(10.0049598131356,15.2,5.23028524503687));
#202313=CARTESIAN_POINT('Ctrl Pts',(10.0071710738982,15.2,5.2330485228809));
#202314=CARTESIAN_POINT('Ctrl Pts',(10.0093834949843,15.2,5.23581988907078));
#202315=CARTESIAN_POINT('Ctrl Pts',(10.0115959164723,15.2,5.23859125576412));
#202316=CARTESIAN_POINT('Ctrl Pts',(10.0138094967274,15.2,5.24137071126807));
#202317=CARTESIAN_POINT('Ctrl Pts',(10.0160241937161,15.2,5.24415824588262));
#202318=CARTESIAN_POINT('Ctrl Pts',(10.0182388903024,15.2,5.24694577999077));
#202319=CARTESIAN_POINT('Ctrl Pts',(10.0204547034721,15.2,5.24974139239017));
#202320=CARTESIAN_POINT('Ctrl Pts',(10.0226715910166,15.2,5.25254507362233));
#202321=CARTESIAN_POINT('Ctrl Pts',(10.0256274409417,15.2,5.25628331509543));
#202322=CARTESIAN_POINT('Ctrl Pts',(10.0285851979359,15.2,5.26003590037957));
#202323=CARTESIAN_POINT('Ctrl Pts',(10.0315447652494,15.2,5.26380280712571));
#202324=CARTESIAN_POINT('Ctrl Pts',(10.0337644412385,15.2,5.26662798782687));
#202325=CARTESIAN_POINT('Ctrl Pts',(10.0359851345113,15.2,5.26946122432197));
#202326=CARTESIAN_POINT('Ctrl Pts',(10.0382068040009,15.2,5.272302505611));
#202327=CARTESIAN_POINT('Ctrl Pts',(10.040428473087,15.2,5.27514378638386));
#202328=CARTESIAN_POINT('Ctrl Pts',(10.0426511173831,15.2,5.27799311286298));
#202329=CARTESIAN_POINT('Ctrl Pts',(10.0448746951635,15.2,5.28085047423617));
#202330=CARTESIAN_POINT('Ctrl Pts',(10.0470982729439,15.2,5.28370783560936));
#202331=CARTESIAN_POINT('Ctrl Pts',(10.04932278484,15.2,5.28657323213364));
#202332=CARTESIAN_POINT('Ctrl Pts',(10.0515481885509,15.2,5.2894466538216));
#202333=CARTESIAN_POINT('Ctrl Pts',(10.0537735922617,15.2,5.29232007550957));
#202334=CARTESIAN_POINT('Ctrl Pts',(10.0559998889975,15.2,5.29520152223825));
#202335=CARTESIAN_POINT('Ctrl Pts',(10.0582270357499,15.2,5.2980909829666));
#202336=CARTESIAN_POINT('Ctrl Pts',(10.0604541825023,15.2,5.30098044369494));
#202337=CARTESIAN_POINT('Ctrl Pts',(10.0626821808214,15.2,5.30387791960631));
#202338=CARTESIAN_POINT('Ctrl Pts',(10.064910988532,15.2,5.30678340025003));
#202339=CARTESIAN_POINT('Ctrl Pts',(10.0678827324161,15.2,5.31065737479357));
#202340=CARTESIAN_POINT('Ctrl Pts',(10.0708559163318,15.2,5.31454557819352));
#202341=CARTESIAN_POINT('Ctrl Pts',(10.0738304441982,15.2,5.31844798832461));
#202342=CARTESIAN_POINT('Ctrl Pts',(10.0760613398954,15.2,5.32137479565708));
#202343=CARTESIAN_POINT('Ctrl Pts',(10.078292989541,15.2,5.32430959359372));
#202344=CARTESIAN_POINT('Ctrl Pts',(10.08052535471,15.2,5.32725237132083));
#202345=CARTESIAN_POINT('Ctrl Pts',(10.0827577198789,15.2,5.33019514904794));
#202346=CARTESIAN_POINT('Ctrl Pts',(10.0849908002978,15.2,5.33314590707409));
#202347=CARTESIAN_POINT('Ctrl Pts',(10.0872245555083,15.2,5.33610463525826));
#202348=CARTESIAN_POINT('Ctrl Pts',(10.0894583107188,15.2,5.33906336344242));
#202349=CARTESIAN_POINT('Ctrl Pts',(10.0916927415709,15.2,5.34203006118459));
#202350=CARTESIAN_POINT('Ctrl Pts',(10.0939278077397,15.2,5.34500471840916));
#202351=CARTESIAN_POINT('Ctrl Pts',(10.0961628739084,15.2,5.34797937563372));
#202352=CARTESIAN_POINT('Ctrl Pts',(10.0983985755202,15.2,5.35096199276492));
#202353=CARTESIAN_POINT('Ctrl Pts',(10.1006348703423,15.2,5.35395255817974));
#202354=CARTESIAN_POINT('Ctrl Pts',(10.1036165970425,15.2,5.35793997909502));
#202355=CARTESIAN_POINT('Ctrl Pts',(10.1065993780895,15.2,5.36194153056136));
#202356=CARTESIAN_POINT('Ctrl Pts',(10.1095831227522,15.2,5.36595718783667));
#202357=CARTESIAN_POINT('Ctrl Pts',(10.1118209310459,15.2,5.36896893051959));
#202358=CARTESIAN_POINT('Ctrl Pts',(10.1140592831646,15.2,5.3719886079766));
#202359=CARTESIAN_POINT('Ctrl Pts',(10.1162981414999,15.2,5.37501621019993));
#202360=CARTESIAN_POINT('Ctrl Pts',(10.1185369998353,15.2,5.37804381242326));
#202361=CARTESIAN_POINT('Ctrl Pts',(10.1207763667872,15.2,5.3810793403296));
#202362=CARTESIAN_POINT('Ctrl Pts',(10.1230161954141,15.2,5.38412278142666));
#202363=CARTESIAN_POINT('Ctrl Pts',(10.1252560240411,15.2,5.38716622252373));
#202364=CARTESIAN_POINT('Ctrl Pts',(10.127496314736,15.2,5.39021757578404));
#202365=CARTESIAN_POINT('Ctrl Pts',(10.1297370200581,15.2,5.39327682915811));
#202366=CARTESIAN_POINT('Ctrl Pts',(10.1319777253802,15.2,5.39633608253219));
#202367=CARTESIAN_POINT('Ctrl Pts',(10.1342188448594,15.2,5.39940323605904));
#202368=CARTESIAN_POINT('Ctrl Pts',(10.136460352528,15.2,5.40247828182125));
#202369=CARTESIAN_POINT('Ctrl Pts',(10.1394490296908,15.2,5.40657834320993));
#202370=CARTESIAN_POINT('Ctrl Pts',(10.1424383928518,15.2,5.41069243854174));
#202371=CARTESIAN_POINT('Ctrl Pts',(10.1454284469999,15.2,5.41482055299999));
#202372=CARTESIAN_POINT('Ctrl Pts',(9.31239140099994,12.2,4.57383771099998));
#202373=CARTESIAN_POINT('Ctrl Pts',(9.31392144680189,12.2,4.57476026769956));
#202374=CARTESIAN_POINT('Ctrl Pts',(9.31549767341897,12.2,4.57571692949402));
#202375=CARTESIAN_POINT('Ctrl Pts',(9.31711891381397,12.2,4.57670776739141));
#202376=CARTESIAN_POINT('Ctrl Pts',(9.31874797264965,12.2,4.57770338360999));
#202377=CARTESIAN_POINT('Ctrl Pts',(9.32042248385082,12.2,4.57873349868146));
#202378=CARTESIAN_POINT('Ctrl Pts',(9.32214129986625,12.2,4.57979816304467));
#202379=CARTESIAN_POINT('Ctrl Pts',(9.3241465849834,12.2,4.58104027132335));
#202380=CARTESIAN_POINT('Ctrl Pts',(9.32621217660936,12.2,4.58232940557774));
#202381=CARTESIAN_POINT('Ctrl Pts',(9.32833631004309,12.2,4.58366563461676));
#202382=CARTESIAN_POINT('Ctrl Pts',(9.33015699605605,12.2,4.58481097392682));
#202383=CARTESIAN_POINT('Ctrl Pts',(9.33202069553284,12.2,4.58599091516364));
#202384=CARTESIAN_POINT('Ctrl Pts',(9.33392633190098,12.2,4.58720549637584));
#202385=CARTESIAN_POINT('Ctrl Pts',(9.33614957407084,12.2,4.58862250762459));
#202386=CARTESIAN_POINT('Ctrl Pts',(9.33842989701372,12.2,4.59008667009452));
#202387=CARTESIAN_POINT('Ctrl Pts',(9.34076564432333,12.2,4.59159803785873));
#202388=CARTESIAN_POINT('Ctrl Pts',(9.34276771367966,12.2,4.59289349609363));
#202389=CARTESIAN_POINT('Ctrl Pts',(9.34481050330659,12.2,4.59422363630412));
#202390=CARTESIAN_POINT('Ctrl Pts',(9.3468930019431,12.2,4.59558849061538));
#202391=CARTESIAN_POINT('Ctrl Pts',(9.34932258340195,12.2,4.59718082045921));
#202392=CARTESIAN_POINT('Ctrl Pts',(9.35180621226842,12.2,4.59882039919461));
#202393=CARTESIAN_POINT('Ctrl Pts',(9.35434232328794,12.2,4.600507268809));
#202394=CARTESIAN_POINT('Ctrl Pts',(9.35651613298711,12.2,4.60195315721876));
#202395=CARTESIAN_POINT('Ctrl Pts',(9.35872850338876,12.2,4.6034337928863));
#202396=CARTESIAN_POINT('Ctrl Pts',(9.36097847920929,12.2,4.60494919521327));
#202397=CARTESIAN_POINT('Ctrl Pts',(9.36322845482546,12.2,4.6064645974026));
#202398=CARTESIAN_POINT('Ctrl Pts',(9.36551603434266,12.2,4.60801476769917));
#202399=CARTESIAN_POINT('Ctrl Pts',(9.36784028600821,12.2,4.60959972672492));
#202400=CARTESIAN_POINT('Ctrl Pts',(9.37016453767377,12.2,4.61118468575067));
#202401=CARTESIAN_POINT('Ctrl Pts',(9.37252546320421,12.2,4.61280443283609));
#202402=CARTESIAN_POINT('Ctrl Pts',(9.37492215123479,12.2,4.61445898485662));
#202403=CARTESIAN_POINT('Ctrl Pts',(9.37731883948308,12.2,4.61611353702745));
#202404=CARTESIAN_POINT('Ctrl Pts',(9.37975129316532,12.2,4.61780289367487));
#202405=CARTESIAN_POINT('Ctrl Pts',(9.38221862330217,12.2,4.61952706693787));
#202406=CARTESIAN_POINT('Ctrl Pts',(9.38468595321489,12.2,4.62125124004426));
#202407=CARTESIAN_POINT('Ctrl Pts',(9.38718815954827,12.2,4.62301023159936));
#202408=CARTESIAN_POINT('Ctrl Pts',(9.38972437946771,12.2,4.62480405145907));
#202409=CARTESIAN_POINT('Ctrl Pts',(9.39226059938715,12.2,4.62659787131879));
#202410=CARTESIAN_POINT('Ctrl Pts',(9.3948308306375,12.2,4.62842651815939));
#202411=CARTESIAN_POINT('Ctrl Pts',(9.39743422887481,12.2,4.63028999917351));
#202412=CARTESIAN_POINT('Ctrl Pts',(9.4000376273486,12.2,4.63215348035689));
#202413=CARTESIAN_POINT('Ctrl Pts',(9.40267419441815,12.2,4.63405179783625));
#202414=CARTESIAN_POINT('Ctrl Pts',(9.40534310281581,12.2,4.63598495294398));
#202415=CARTESIAN_POINT('Ctrl Pts',(9.40801201097104,12.2,4.63791810787611));
#202416=CARTESIAN_POINT('Ctrl Pts',(9.41071326184628,12.2,4.63988610110609));
#202417=CARTESIAN_POINT('Ctrl Pts',(9.41344604800947,12.2,4.64188893495917));
#202418=CARTESIAN_POINT('Ctrl Pts',(9.41617883417266,12.2,4.64389176881224));
#202419=CARTESIAN_POINT('Ctrl Pts',(9.41894315591726,12.2,4.64592944248062));
#202420=CARTESIAN_POINT('Ctrl Pts',(9.42173822431436,12.2,4.64800195440379));
#202421=CARTESIAN_POINT('Ctrl Pts',(9.42453329296533,12.2,4.65007446651521));
#202422=CARTESIAN_POINT('Ctrl Pts',(9.42735910974518,12.2,4.65218181759766));
#202423=CARTESIAN_POINT('Ctrl Pts',(9.43021490231951,12.2,4.65432400171676));
#202424=CARTESIAN_POINT('Ctrl Pts',(9.43307069463444,12.2,4.65646618564129));
#202425=CARTESIAN_POINT('Ctrl Pts',(9.43595646228017,12.2,4.65864320443279));
#202426=CARTESIAN_POINT('Ctrl Pts',(9.43887145267555,12.2,4.66085504935395));
#202427=CARTESIAN_POINT('Ctrl Pts',(9.44178644307091,12.2,4.6630668942751));
#202428=CARTESIAN_POINT('Ctrl Pts',(9.4447306541389,12.2,4.66531356687679));
#202429=CARTESIAN_POINT('Ctrl Pts',(9.447703349613,12.2,4.66759505762573));
#202430=CARTESIAN_POINT('Ctrl Pts',(9.45067604508711,12.2,4.66987654837468));
#202431=CARTESIAN_POINT('Ctrl Pts',(9.45367722400671,12.2,4.67219285629814));
#202432=CARTESIAN_POINT('Ctrl Pts',(9.45670616264474,12.2,4.67454397021032));
#202433=CARTESIAN_POINT('Ctrl Pts',(9.45973510155791,12.2,4.67689508433607));
#202434=CARTESIAN_POINT('Ctrl Pts',(9.46279180181548,12.2,4.67928100451521));
#202435=CARTESIAN_POINT('Ctrl Pts',(9.46587555465141,12.2,4.68170171664866));
#202436=CARTESIAN_POINT('Ctrl Pts',(9.46895930720722,12.2,4.68412242856224));
#202437=CARTESIAN_POINT('Ctrl Pts',(9.47207011191492,12.2,4.68657793207805));
#202438=CARTESIAN_POINT('Ctrl Pts',(9.47520727648181,12.2,4.6890682099988));
#202439=CARTESIAN_POINT('Ctrl Pts',(9.47782158038254,12.2,4.69114344167482));
#202440=CARTESIAN_POINT('Ctrl Pts',(9.48045418979989,12.2,4.69324282403325));
#202441=CARTESIAN_POINT('Ctrl Pts',(9.48310470896656,12.2,4.69536634403325));
#202442=CARTESIAN_POINT('Ctrl Pts',(9.48575522813323,12.2,4.69748986403325));
#202443=CARTESIAN_POINT('Ctrl Pts',(9.48842366038359,12.2,4.69963752303009));
#202444=CARTESIAN_POINT('Ctrl Pts',(9.49110961449303,12.2,4.70180930873444));
#202445=CARTESIAN_POINT('Ctrl Pts',(9.49379556860247,12.2,4.7039810944388));
#202446=CARTESIAN_POINT('Ctrl Pts',(9.49649904737149,12.2,4.70617700707734));
#202447=CARTESIAN_POINT('Ctrl Pts',(9.49921966813626,12.2,4.70839703291192));
#202448=CARTESIAN_POINT('Ctrl Pts',(9.50194028890104,12.2,4.7106170587465));
#202449=CARTESIAN_POINT('Ctrl Pts',(9.50467805142371,12.2,4.71286120014716));
#202450=CARTESIAN_POINT('Ctrl Pts',(9.50743258218848,12.2,4.71512944014841));
#202451=CARTESIAN_POINT('Ctrl Pts',(9.51018711295324,12.2,4.71739768014967));
#202452=CARTESIAN_POINT('Ctrl Pts',(9.51295841027204,12.2,4.7196900206293));
#202453=CARTESIAN_POINT('Ctrl Pts',(9.51574610631524,12.2,4.72200644651058));
#202454=CARTESIAN_POINT('Ctrl Pts',(9.51853380235842,12.2,4.72432287239186));
#202455=CARTESIAN_POINT('Ctrl Pts',(9.52133789705082,12.2,4.72666338340171));
#202456=CARTESIAN_POINT('Ctrl Pts',(9.52415802559378,12.2,4.72902796333422));
#202457=CARTESIAN_POINT('Ctrl Pts',(9.52697815413675,12.2,4.73139254326673));
#202458=CARTESIAN_POINT('Ctrl Pts',(9.52981431797721,12.2,4.73378119320244));
#202459=CARTESIAN_POINT('Ctrl Pts',(9.53266615888126,12.2,4.73619389556551));
#202460=CARTESIAN_POINT('Ctrl Pts',(9.53551799947446,12.2,4.73860659766559));
#202461=CARTESIAN_POINT('Ctrl Pts',(9.53838551764944,12.2,4.74104335162605));
#202462=CARTESIAN_POINT('Ctrl Pts',(9.54126835934783,12.2,4.74350414191139));
#202463=CARTESIAN_POINT('Ctrl Pts',(9.54415120136044,12.2,4.74596493246496));
#202464=CARTESIAN_POINT('Ctrl Pts',(9.54704936916453,12.2,4.74844975705706));
#202465=CARTESIAN_POINT('Ctrl Pts',(9.54996251513554,12.2,4.75095859788845));
#202466=CARTESIAN_POINT('Ctrl Pts',(9.55287566110655,12.2,4.75346743871982));
#202467=CARTESIAN_POINT('Ctrl Pts',(9.55580378408458,12.2,4.75600029723823));
#202468=CARTESIAN_POINT('Ctrl Pts',(9.55874654367502,12.2,4.75855715146153));
#202469=CARTESIAN_POINT('Ctrl Pts',(9.56168930326545,12.2,4.76111400568482));
#202470=CARTESIAN_POINT('Ctrl Pts',(9.56464669929527,12.2,4.76369485621429));
#202471=CARTESIAN_POINT('Ctrl Pts',(9.56761839457232,12.2,4.76629968433805));
#202472=CARTESIAN_POINT('Ctrl Pts',(9.57059008984936,12.2,4.76890451246181));
#202473=CARTESIAN_POINT('Ctrl Pts',(9.57357608262674,12.2,4.77153331651116));
#202474=CARTESIAN_POINT('Ctrl Pts',(9.5765760460288,12.2,4.77418607630158));
#202475=CARTESIAN_POINT('Ctrl Pts',(9.57957600943086,12.2,4.77683883609201));
#202476=CARTESIAN_POINT('Ctrl Pts',(9.58258993811383,12.2,4.77951555064693));
#202477=CARTESIAN_POINT('Ctrl Pts',(9.58561750929366,12.2,4.78221619884011));
#202478=CARTESIAN_POINT('Ctrl Pts',(9.58864508047348,12.2,4.78491684703329));
#202479=CARTESIAN_POINT('Ctrl Pts',(9.59168629101776,12.2,4.78764142989713));
#202480=CARTESIAN_POINT('Ctrl Pts',(9.59474082123992,12.2,4.79038992150677));
#202481=CARTESIAN_POINT('Ctrl Pts',(9.59779535146208,12.2,4.7931384131164));
#202482=CARTESIAN_POINT('Ctrl Pts',(9.60086319855546,12.2,4.79591081560547));
#202483=CARTESIAN_POINT('Ctrl Pts',(9.60394404799991,12.2,4.79870710546659));
#202484=CARTESIAN_POINT('Ctrl Pts',(9.6064087276898,12.2,4.8009441374774));
#202485=CARTESIAN_POINT('Ctrl Pts',(9.6088817266501,12.2,4.803196455865));
#202486=CARTESIAN_POINT('Ctrl Pts',(9.61136288639726,12.2,4.80546405037902));
#202487=CARTESIAN_POINT('Ctrl Pts',(9.61384404580635,12.2,4.80773164458409));
#202488=CARTESIAN_POINT('Ctrl Pts',(9.61633336409106,12.2,4.81001451331751));
#202489=CARTESIAN_POINT('Ctrl Pts',(9.61883068423155,12.2,4.81231264497336));
#202490=CARTESIAN_POINT('Ctrl Pts',(9.62132800471231,12.2,4.81461077694233));
#202491=CARTESIAN_POINT('Ctrl Pts',(9.62383332625916,12.2,4.81692417081053));
#202492=CARTESIAN_POINT('Ctrl Pts',(9.62634649145248,12.2,4.81925281410566));
#202493=CARTESIAN_POINT('Ctrl Pts',(9.62885965630339,12.2,4.82158145708352));
#202494=CARTESIAN_POINT('Ctrl Pts',(9.63138066542271,12.2,4.82392534914551));
#202495=CARTESIAN_POINT('Ctrl Pts',(9.6339093623266,12.2,4.82628447684054));
#202496=CARTESIAN_POINT('Ctrl Pts',(9.63643805957503,12.2,4.82864360485701));
#202497=CARTESIAN_POINT('Ctrl Pts',(9.63897444597214,12.2,4.83101796992636));
#202498=CARTESIAN_POINT('Ctrl Pts',(9.64151836662743,12.2,4.83340755612175));
#202499=CARTESIAN_POINT('Ctrl Pts',(9.64406228693611,12.2,4.83579714199156));
#202500=CARTESIAN_POINT('Ctrl Pts',(9.6466137416199,12.2,4.83820195003162));
#202501=CARTESIAN_POINT('Ctrl Pts',(9.64917257979913,12.2,4.84062196577723));
#202502=CARTESIAN_POINT('Ctrl Pts',(9.65173141832699,12.2,4.84304198185257));
#202503=CARTESIAN_POINT('Ctrl Pts',(9.6542976392974,12.2,4.8454772070575));
#202504=CARTESIAN_POINT('Ctrl Pts',(9.65687109199369,12.2,4.84792762569205));
#202505=CARTESIAN_POINT('Ctrl Pts',(9.65944454433934,12.2,4.85037804399273));
#202506=CARTESIAN_POINT('Ctrl Pts',(9.66202522872402,12.2,4.85284365623412));
#202507=CARTESIAN_POINT('Ctrl Pts',(9.66461299764112,12.2,4.85532444743169));
#202508=CARTESIAN_POINT('Ctrl Pts',(9.66720076691081,12.2,4.85780523896728));
#202509=CARTESIAN_POINT('Ctrl Pts',(9.66979561875931,12.2,4.86030121114528));
#202510=CARTESIAN_POINT('Ctrl Pts',(9.67239740667934,12.2,4.86281234650535));
#202511=CARTESIAN_POINT('Ctrl Pts',(9.67499919424488,12.2,4.86532348152328));
#202512=CARTESIAN_POINT('Ctrl Pts',(9.67760791813403,12.2,4.86784978165206));
#202513=CARTESIAN_POINT('Ctrl Pts',(9.68022343186395,12.2,4.87039123060941));
#202514=CARTESIAN_POINT('Ctrl Pts',(9.68283894595024,12.2,4.87293267991302));
#202515=CARTESIAN_POINT('Ctrl Pts',(9.68546125037149,12.2,4.87548927810815));
#202516=CARTESIAN_POINT('Ctrl Pts',(9.68809020102671,12.2,4.87806101076002));
#202517=CARTESIAN_POINT('Ctrl Pts',(9.69071915132374,12.2,4.88063274306148));
#202518=CARTESIAN_POINT('Ctrl Pts',(9.69335474852347,12.2,4.8832196092082));
#202519=CARTESIAN_POINT('Ctrl Pts',(9.69599684808461,12.2,4.88582159404951));
#202520=CARTESIAN_POINT('Ctrl Pts',(9.69863894800573,12.2,4.88842357924534));
#202521=CARTESIAN_POINT('Ctrl Pts',(9.70128755018022,12.2,4.89104068216757));
#202522=CARTESIAN_POINT('Ctrl Pts',(9.70394251549158,12.2,4.89367288753326));
#202523=CARTESIAN_POINT('Ctrl Pts',(9.70659748080295,12.2,4.89630509289894));
#202524=CARTESIAN_POINT('Ctrl Pts',(9.70925880700115,12.2,4.89895240071358));
#202525=CARTESIAN_POINT('Ctrl Pts',(9.71192635570274,12.2,4.90161479469357));
#202526=CARTESIAN_POINT('Ctrl Pts',(9.71459390404087,12.2,4.90427718831081));
#202527=CARTESIAN_POINT('Ctrl Pts',(9.7172676745828,12.2,4.90695466817825));
#202528=CARTESIAN_POINT('Ctrl Pts',(9.71994752826477,12.2,4.9096472177481));
#202529=CARTESIAN_POINT('Ctrl Pts',(9.72262738231187,12.2,4.91233976768481));
#202530=CARTESIAN_POINT('Ctrl Pts',(9.72531332028995,12.2,4.91504738687293));
#202531=CARTESIAN_POINT('Ctrl Pts',(9.72800520371505,12.2,4.91777005891176));
#202532=CARTESIAN_POINT('Ctrl Pts',(9.73069708677338,12.2,4.92049273057962));
#202533=CARTESIAN_POINT('Ctrl Pts',(9.7333949161948,12.2,4.9232304562955));
#202534=CARTESIAN_POINT('Ctrl Pts',(9.73609855652896,12.2,4.9259832172917));
#202535=CARTESIAN_POINT('Ctrl Pts',(9.73880219723148,12.2,4.92873597866296));
#202536=CARTESIAN_POINT('Ctrl Pts',(9.7415116475237,12.2,4.93150377594792));
#202537=CARTESIAN_POINT('Ctrl Pts',(9.74422677441894,12.2,4.93428659262881));
#202538=CARTESIAN_POINT('Ctrl Pts',(9.74694190094423,12.2,4.93706940893054));
#202539=CARTESIAN_POINT('Ctrl Pts',(9.74966270290867,12.2,4.93986724359549));
#202540=CARTESIAN_POINT('Ctrl Pts',(9.75238904851876,12.2,4.94268007925345));
#202541=CARTESIAN_POINT('Ctrl Pts',(9.75511539450032,12.2,4.94549291529466));
#202542=CARTESIAN_POINT('Ctrl Pts',(9.75784728239366,12.2,4.94832075338767));
#202543=CARTESIAN_POINT('Ctrl Pts',(9.76058458126542,12.2,4.9511635747658));
#202544=CARTESIAN_POINT('Ctrl Pts',(9.76332187976422,12.2,4.9540063957566));
#202545=CARTESIAN_POINT('Ctrl Pts',(9.76606458996958,12.2,4.95686420118412));
#202546=CARTESIAN_POINT('Ctrl Pts',(9.7688125798262,12.2,4.95973697159148));
#202547=CARTESIAN_POINT('Ctrl Pts',(9.77156057005723,12.2,4.96260974239025));
#202548=CARTESIAN_POINT('Ctrl Pts',(9.7743138407248,12.2,4.96549747894763));
#202549=CARTESIAN_POINT('Ctrl Pts',(9.77707226220881,12.2,4.9684001634957));
#202550=CARTESIAN_POINT('Ctrl Pts',(9.77983068331699,12.2,4.97130284764828));
#202551=CARTESIAN_POINT('Ctrl Pts',(9.7825942550908,12.2,4.97422047889231));
#202552=CARTESIAN_POINT('Ctrl Pts',(9.78536284953059,12.2,4.97715303926212));
#202553=CARTESIAN_POINT('Ctrl Pts',(9.78813144434761,12.2,4.9800856000315));
#202554=CARTESIAN_POINT('Ctrl Pts',(9.79090506156238,12.2,4.98303309077458));
#202555=CARTESIAN_POINT('Ctrl Pts',(9.79368357499159,12.2,4.98599549199159));
#202556=CARTESIAN_POINT('Ctrl Pts',(9.79646208842081,12.2,4.98895789320861));
#202557=CARTESIAN_POINT('Ctrl Pts',(9.79924549754225,12.2,4.99193520367457));
#202558=CARTESIAN_POINT('Ctrl Pts',(9.80203367647246,12.2,4.99492740750583));
#202559=CARTESIAN_POINT('Ctrl Pts',(9.80482185502279,12.2,4.9979196109294));
#202560=CARTESIAN_POINT('Ctrl Pts',(9.80761480294737,12.2,5.00092670553401));
#202561=CARTESIAN_POINT('Ctrl Pts',(9.81041239673136,12.2,5.00394867302287));
#202562=CARTESIAN_POINT('Ctrl Pts',(9.81320999089653,12.2,5.00697064092348));
#202563=CARTESIAN_POINT('Ctrl Pts',(9.81601223113041,12.2,5.01000748081996));
#202564=CARTESIAN_POINT('Ctrl Pts',(9.81881899145051,12.2,5.01305917476556));
#202565=CARTESIAN_POINT('Ctrl Pts',(9.82162575138817,12.2,5.01611086829536));
#202566=CARTESIAN_POINT('Ctrl Pts',(9.82443703421968,12.2,5.01917741568158));
#202567=CARTESIAN_POINT('Ctrl Pts',(9.82725271604479,12.2,5.02225879603983));
#202568=CARTESIAN_POINT('Ctrl Pts',(9.83006839825352,12.2,5.02534017681792));
#202569=CARTESIAN_POINT('Ctrl Pts',(9.83288848028938,12.2,5.02843639250017));
#202570=CARTESIAN_POINT('Ctrl Pts',(9.83571283941812,12.2,5.03154742199311));
#202571=CARTESIAN_POINT('Ctrl Pts',(9.83853719816205,12.2,5.03465845106218));
#202572=CARTESIAN_POINT('Ctrl Pts',(9.84136583625859,12.2,5.03778429366772));
#202573=CARTESIAN_POINT('Ctrl Pts',(9.84419863152672,12.2,5.04092493174332));
#202574=CARTESIAN_POINT('Ctrl Pts',(9.84703142718082,12.2,5.04406557024682));
#202575=CARTESIAN_POINT('Ctrl Pts',(9.84986838127157,12.2,5.04722100170495));
#202576=CARTESIAN_POINT('Ctrl Pts',(9.85270937298221,12.2,5.05039120826756));
#202577=CARTESIAN_POINT('Ctrl Pts',(9.85555036430577,12.2,5.05356141439823));
#202578=CARTESIAN_POINT('Ctrl Pts',(9.85839539613025,12.2,5.05674639548595));
#202579=CARTESIAN_POINT('Ctrl Pts',(9.86124434809488,12.2,5.05994612932737));
#202580=CARTESIAN_POINT('Ctrl Pts',(9.86480553834178,12.2,5.06394579695611));
#202581=CARTESIAN_POINT('Ctrl Pts',(9.86837285282768,12.2,5.06796851859778));
#202582=CARTESIAN_POINT('Ctrl Pts',(9.87194606775794,12.2,5.07201425248547));
#202583=CARTESIAN_POINT('Ctrl Pts',(9.87480463985795,12.2,5.07525083977203));
#202584=CARTESIAN_POINT('Ctrl Pts',(9.87766698508338,12.2,5.07850215551588));
#202585=CARTESIAN_POINT('Ctrl Pts',(9.88053299001759,12.2,5.0817681782504));
#202586=CARTESIAN_POINT('Ctrl Pts',(9.88339899456131,12.2,5.08503420053992));
#202587=CARTESIAN_POINT('Ctrl Pts',(9.88626865709412,12.2,5.08831493056397));
#202588=CARTESIAN_POINT('Ctrl Pts',(9.88914186505803,12.2,5.09161034751349));
#202589=CARTESIAN_POINT('Ctrl Pts',(9.89201507341341,12.2,5.09490576491201));
#202590=CARTESIAN_POINT('Ctrl Pts',(9.89489182613933,12.2,5.09821586841193));
#202591=CARTESIAN_POINT('Ctrl Pts',(9.89777200851875,12.2,5.10154063703853));
#202592=CARTESIAN_POINT('Ctrl Pts',(9.90065219050575,12.2,5.10486540521214));
#202593=CARTESIAN_POINT('Ctrl Pts',(9.90353580293927,12.2,5.10820484003835));
#202594=CARTESIAN_POINT('Ctrl Pts',(9.90642273353625,12.2,5.11155891698487));
#202595=CARTESIAN_POINT('Ctrl Pts',(9.90930966452657,12.2,5.11491299438837));
#202596=CARTESIAN_POINT('Ctrl Pts',(9.91219991338939,12.2,5.11828171706076));
#202597=CARTESIAN_POINT('Ctrl Pts',(9.9150933677269,12.2,5.12166506176056));
#202598=CARTESIAN_POINT('Ctrl Pts',(9.91726345828292,12.2,5.12420257005493));
#202599=CARTESIAN_POINT('Ctrl Pts',(9.91943535168372,12.2,5.1267483039955));
#202600=CARTESIAN_POINT('Ctrl Pts',(9.92160900219796,12.2,5.12930225324761));
#202601=CARTESIAN_POINT('Ctrl Pts',(9.92378265271218,12.2,5.13185620249971));
#202602=CARTESIAN_POINT('Ctrl Pts',(9.92595805972523,12.2,5.13441836779733));
#202603=CARTESIAN_POINT('Ctrl Pts',(9.92813517677099,12.2,5.13698874003657));
#202604=CARTESIAN_POINT('Ctrl Pts',(9.93031229381675,12.2,5.1395591122758));
#202605=CARTESIAN_POINT('Ctrl Pts',(9.93249112118739,12.2,5.14213769084781));
#202606=CARTESIAN_POINT('Ctrl Pts',(9.93467161177458,12.2,5.14472446712768));
#202607=CARTESIAN_POINT('Ctrl Pts',(9.93685210275791,12.2,5.14731124387749));
#202608=CARTESIAN_POINT('Ctrl Pts',(9.9390342573084,12.2,5.14990621860465));
#202609=CARTESIAN_POINT('Ctrl Pts',(9.94121803020934,12.2,5.15250938131743));
#202610=CARTESIAN_POINT('Ctrl Pts',(9.94340180271356,12.2,5.15511254355731));
#202611=CARTESIAN_POINT('Ctrl Pts',(9.94558719255975,12.2,5.15772389382017));
#202612=CARTESIAN_POINT('Ctrl Pts',(9.94777415521473,12.2,5.16034342319014));
#202613=CARTESIAN_POINT('Ctrl Pts',(9.94996111786971,12.2,5.16296295256011));
#202614=CARTESIAN_POINT('Ctrl Pts',(9.95214965260145,12.2,5.16559066078244));
#202615=CARTESIAN_POINT('Ctrl Pts',(9.95433971373034,12.2,5.16822653802071));
#202616=CARTESIAN_POINT('Ctrl Pts',(9.95725979510292,12.2,5.17174104084547));
#202617=CARTESIAN_POINT('Ctrl Pts',(9.96018259014993,12.2,5.17527006748119));
#202618=CARTESIAN_POINT('Ctrl Pts',(9.96310799402163,12.2,5.17881359491223));
#202619=CARTESIAN_POINT('Ctrl Pts',(9.96530204742362,12.2,5.18147124108902));
#202620=CARTESIAN_POINT('Ctrl Pts',(9.96749756695938,12.2,5.18413704397646));
#202621=CARTESIAN_POINT('Ctrl Pts',(9.9696945084872,12.2,5.18681099411619));
#202622=CARTESIAN_POINT('Ctrl Pts',(9.97189144961591,12.2,5.18948494377014));
#202623=CARTESIAN_POINT('Ctrl Pts',(9.97408981369543,12.2,5.19216703924959));
#202624=CARTESIAN_POINT('Ctrl Pts',(9.97628955493388,12.2,5.1948572739955));
#202625=CARTESIAN_POINT('Ctrl Pts',(9.97848929617234,12.2,5.19754750874143));
#202626=CARTESIAN_POINT('Ctrl Pts',(9.98069041481993,12.2,5.20024588035938));
#202627=CARTESIAN_POINT('Ctrl Pts',(9.98289286649003,12.2,5.20295237959508));
#202628=CARTESIAN_POINT('Ctrl Pts',(9.98509531816012,12.2,5.20565887883078));
#202629=CARTESIAN_POINT('Ctrl Pts',(9.98729910386338,12.2,5.20837350606551));
#202630=CARTESIAN_POINT('Ctrl Pts',(9.98950417899161,12.2,5.21109625221659));
#202631=CARTESIAN_POINT('Ctrl Pts',(9.99170925411983,12.2,5.21381899836768));
#202632=CARTESIAN_POINT('Ctrl Pts',(9.99391561913965,12.2,5.21654986178508));
#202633=CARTESIAN_POINT('Ctrl Pts',(9.99612322926766,12.2,5.21928883397652));
#202634=CARTESIAN_POINT('Ctrl Pts',(9.99833083939567,12.2,5.22202780616795));
#202635=CARTESIAN_POINT('Ctrl Pts',(10.0005396956591,12.2,5.22477488629703));
#202636=CARTESIAN_POINT('Ctrl Pts',(10.0027497543974,12.2,5.22753006566695));
#202637=CARTESIAN_POINT('Ctrl Pts',(10.0049598131356,12.2,5.23028524503687));
#202638=CARTESIAN_POINT('Ctrl Pts',(10.0071710738982,12.2,5.2330485228809));
#202639=CARTESIAN_POINT('Ctrl Pts',(10.0093834949843,12.2,5.23581988907078));
#202640=CARTESIAN_POINT('Ctrl Pts',(10.0115959164723,12.2,5.23859125576411));
#202641=CARTESIAN_POINT('Ctrl Pts',(10.0138094967274,12.2,5.24137071126807));
#202642=CARTESIAN_POINT('Ctrl Pts',(10.0160241937161,12.2,5.24415824588262));
#202643=CARTESIAN_POINT('Ctrl Pts',(10.0182388903024,12.2,5.24694577999077));
#202644=CARTESIAN_POINT('Ctrl Pts',(10.0204547034721,12.2,5.24974139239017));
#202645=CARTESIAN_POINT('Ctrl Pts',(10.0226715910166,12.2,5.25254507362233));
#202646=CARTESIAN_POINT('Ctrl Pts',(10.0248884785611,12.2,5.25534875485449));
#202647=CARTESIAN_POINT('Ctrl Pts',(10.0271064388306,12.2,5.25816050491905));
#202648=CARTESIAN_POINT('Ctrl Pts',(10.0293254309999,12.2,5.26098031323327));
#202649=CARTESIAN_POINT('Ctrl Pts',(10.0315444231693,12.2,5.26380012154749));
#202650=CARTESIAN_POINT('Ctrl Pts',(10.0337644473053,12.2,5.26662798972803));
#202651=CARTESIAN_POINT('Ctrl Pts',(10.0359854609745,12.2,5.26946390595762));
#202652=CARTESIAN_POINT('Ctrl Pts',(10.0382064746437,12.2,5.27229982218721));
#202653=CARTESIAN_POINT('Ctrl Pts',(10.0404284785563,12.2,5.27514378734362));
#202654=CARTESIAN_POINT('Ctrl Pts',(10.0426514293365,12.2,5.27799579075655));
#202655=CARTESIAN_POINT('Ctrl Pts',(10.0448743801167,12.2,5.28084779416948));
#202656=CARTESIAN_POINT('Ctrl Pts',(10.0470982781459,12.2,5.28370783632999));
#202657=CARTESIAN_POINT('Ctrl Pts',(10.0493230827316,12.2,5.2865759065997));
#202658=CARTESIAN_POINT('Ctrl Pts',(10.0515478877215,12.2,5.28944397739043));
#202659=CARTESIAN_POINT('Ctrl Pts',(10.0537735983283,12.2,5.29232007740844));
#202660=CARTESIAN_POINT('Ctrl Pts',(10.056000174277,12.2,5.29520419466202));
#202661=CARTESIAN_POINT('Ctrl Pts',(10.0582267498212,12.2,5.29808831139165));
#202662=CARTESIAN_POINT('Ctrl Pts',(10.060454188907,12.2,5.30098044535419));
#202663=CARTESIAN_POINT('Ctrl Pts',(10.0626824524928,12.2,5.30388058849952));
#202664=CARTESIAN_POINT('Ctrl Pts',(10.0649107160786,12.2,5.30678073164485));
#202665=CARTESIAN_POINT('Ctrl Pts',(10.0671398026062,12.2,5.30968888257857));
#202666=CARTESIAN_POINT('Ctrl Pts',(10.0693696722853,12.2,5.31260503077759));
#202667=CARTESIAN_POINT('Ctrl Pts',(10.0715995419644,12.2,5.3155211789766));
#202668=CARTESIAN_POINT('Ctrl Pts',(10.0738301953189,12.2,5.31844532504053));
#202669=CARTESIAN_POINT('Ctrl Pts',(10.0760615894979,12.2,5.32137745823894));
#202670=CARTESIAN_POINT('Ctrl Pts',(10.078292983677,12.2,5.32430959143735));
#202671=CARTESIAN_POINT('Ctrl Pts',(10.0805251189044,12.2,5.32724971145321));
#202672=CARTESIAN_POINT('Ctrl Pts',(10.0827579565316,12.2,5.33019780817872));
#202673=CARTESIAN_POINT('Ctrl Pts',(10.0849907941587,12.2,5.33314590490424));
#202674=CARTESIAN_POINT('Ctrl Pts',(10.0872243328275,12.2,5.33610197891256));
#202675=CARTESIAN_POINT('Ctrl Pts',(10.0894585339962,12.2,5.33906601909544));
#202676=CARTESIAN_POINT('Ctrl Pts',(10.0916927355708,12.2,5.3420300598168));
#202677=CARTESIAN_POINT('Ctrl Pts',(10.0939275994623,12.2,5.34500206646539));
#202678=CARTESIAN_POINT('Ctrl Pts',(10.0961630849956,12.2,5.34798202964957));
#202679=CARTESIAN_POINT('Ctrl Pts',(10.0983985701228,12.2,5.35096199229238));
#202680=CARTESIAN_POINT('Ctrl Pts',(10.1006346761188,12.2,5.35394991028789));
#202681=CARTESIAN_POINT('Ctrl Pts',(10.1028713623994,12.2,5.35694577403797));
#202682=CARTESIAN_POINT('Ctrl Pts',(10.1051080486799,12.2,5.35994163778804));
#202683=CARTESIAN_POINT('Ctrl Pts',(10.1073453144585,12.2,5.36294544515376));
#202684=CARTESIAN_POINT('Ctrl Pts',(10.1095831227522,12.2,5.36595718783667));
#202685=CARTESIAN_POINT('Ctrl Pts',(10.1118209310459,12.2,5.36896893051959));
#202686=CARTESIAN_POINT('Ctrl Pts',(10.1140592831646,12.2,5.3719886079766));
#202687=CARTESIAN_POINT('Ctrl Pts',(10.1162981414999,12.2,5.37501621019992));
#202688=CARTESIAN_POINT('Ctrl Pts',(10.1185369998353,12.2,5.37804381242326));
#202689=CARTESIAN_POINT('Ctrl Pts',(10.1207763667872,12.2,5.3810793403296));
#202690=CARTESIAN_POINT('Ctrl Pts',(10.1230161954141,12.2,5.38412278142666));
#202691=CARTESIAN_POINT('Ctrl Pts',(10.1252560240411,12.2,5.38716622252373));
#202692=CARTESIAN_POINT('Ctrl Pts',(10.127496314736,12.2,5.39021757578404));
#202693=CARTESIAN_POINT('Ctrl Pts',(10.1297370200581,12.2,5.39327682915812));
#202694=CARTESIAN_POINT('Ctrl Pts',(10.1319777253802,12.2,5.3963360825322));
#202695=CARTESIAN_POINT('Ctrl Pts',(10.1342188448594,12.2,5.39940323605904));
#202696=CARTESIAN_POINT('Ctrl Pts',(10.136460352528,12.2,5.40247828182125));
#202697=CARTESIAN_POINT('Ctrl Pts',(10.1394490296908,12.2,5.40657834320993));
#202698=CARTESIAN_POINT('Ctrl Pts',(10.1424383928518,12.2,5.41069243854174));
#202699=CARTESIAN_POINT('Ctrl Pts',(10.1454284469999,12.2,5.41482055299999));
#202700=CARTESIAN_POINT('Ctrl Pts',(9.95917514599994,15.2,5.75020264099999));
#202701=CARTESIAN_POINT('Ctrl Pts',(9.95917514599994,11.6,5.75020264099999));
#202702=CARTESIAN_POINT('Ctrl Pts',(9.95841243099994,15.2,5.75014920999998));
#202703=CARTESIAN_POINT('Ctrl Pts',(9.95841243099994,11.6,5.75014920999998));
#202704=CARTESIAN_POINT('Ctrl Pts',(9.95688745999994,15.2,5.75004209399999));
#202705=CARTESIAN_POINT('Ctrl Pts',(9.95688745999994,11.6,5.75004209399999));
#202706=CARTESIAN_POINT('Ctrl Pts',(9.95460138399994,15.2,5.74988064799999));
#202707=CARTESIAN_POINT('Ctrl Pts',(9.95460138399994,11.6,5.74988064799999));
#202708=CARTESIAN_POINT('Ctrl Pts',(9.95155604399995,15.2,5.74966384999998));
#202709=CARTESIAN_POINT('Ctrl Pts',(9.95155604399995,11.6,5.74966384999998));
#202710=CARTESIAN_POINT('Ctrl Pts',(9.94775396999995,15.2,5.74939028999999));
#202711=CARTESIAN_POINT('Ctrl Pts',(9.94775396999995,11.6,5.74939028999999));
#202712=CARTESIAN_POINT('Ctrl Pts',(9.94395649899995,15.2,5.74911416799999));
#202713=CARTESIAN_POINT('Ctrl Pts',(9.94395649899995,11.6,5.74911416799999));
#202714=CARTESIAN_POINT('Ctrl Pts',(9.94016363099995,15.2,5.74883548499999));
#202715=CARTESIAN_POINT('Ctrl Pts',(9.94016363099995,11.6,5.74883548499999));
#202716=CARTESIAN_POINT('Ctrl Pts',(9.93637536999995,15.2,5.74855424299999));
#202717=CARTESIAN_POINT('Ctrl Pts',(9.93637536999995,11.6,5.74855424299999));
#202718=CARTESIAN_POINT('Ctrl Pts',(9.93259172199994,15.2,5.74827044899998));
#202719=CARTESIAN_POINT('Ctrl Pts',(9.93259172199994,11.6,5.74827044899998));
#202720=CARTESIAN_POINT('Ctrl Pts',(9.92881268899995,15.2,5.74798410599998));
#202721=CARTESIAN_POINT('Ctrl Pts',(9.92881268899995,11.6,5.74798410599998));
#202722=CARTESIAN_POINT('Ctrl Pts',(9.92503828399995,15.2,5.74769521999999));
#202723=CARTESIAN_POINT('Ctrl Pts',(9.92503828399995,11.6,5.74769521999999));
#202724=CARTESIAN_POINT('Ctrl Pts',(9.92126850899995,15.2,5.74740379999999));
#202725=CARTESIAN_POINT('Ctrl Pts',(9.92126850899995,11.6,5.74740379999999));
#202726=CARTESIAN_POINT('Ctrl Pts',(9.91750337599995,15.2,5.74710985399999));
#202727=CARTESIAN_POINT('Ctrl Pts',(9.91750337599995,11.6,5.74710985399999));
#202728=CARTESIAN_POINT('Ctrl Pts',(9.91374289199995,15.2,5.74681338699998));
#202729=CARTESIAN_POINT('Ctrl Pts',(9.91374289199995,11.6,5.74681338699998));
#202730=CARTESIAN_POINT('Ctrl Pts',(9.90998706399994,15.2,5.74651440899999));
#202731=CARTESIAN_POINT('Ctrl Pts',(9.90998706399994,11.6,5.74651440899999));
#202732=CARTESIAN_POINT('Ctrl Pts',(9.90623589999995,15.2,5.74621292499998));
#202733=CARTESIAN_POINT('Ctrl Pts',(9.90623589999995,11.6,5.74621292499998));
#202734=CARTESIAN_POINT('Ctrl Pts',(9.90248940499994,15.2,5.74590894099998));
#202735=CARTESIAN_POINT('Ctrl Pts',(9.90248940499994,11.6,5.74590894099998));
#202736=CARTESIAN_POINT('Ctrl Pts',(9.89874758699995,15.2,5.74560246199999));
#202737=CARTESIAN_POINT('Ctrl Pts',(9.89874758699995,11.6,5.74560246199999));
#202738=CARTESIAN_POINT('Ctrl Pts',(9.89501044999994,15.2,5.74529349399998));
#202739=CARTESIAN_POINT('Ctrl Pts',(9.89501044999994,11.6,5.74529349399998));
#202740=CARTESIAN_POINT('Ctrl Pts',(9.89127800099994,15.2,5.74498204399998));
#202741=CARTESIAN_POINT('Ctrl Pts',(9.89127800099994,11.6,5.74498204399998));
#202742=CARTESIAN_POINT('Ctrl Pts',(9.88755024699995,15.2,5.74466811599999));
#202743=CARTESIAN_POINT('Ctrl Pts',(9.88755024699995,11.6,5.74466811599999));
#202744=CARTESIAN_POINT('Ctrl Pts',(9.88382719199994,15.2,5.74435171599998));
#202745=CARTESIAN_POINT('Ctrl Pts',(9.88382719199994,11.6,5.74435171599998));
#202746=CARTESIAN_POINT('Ctrl Pts',(9.88010884599994,15.2,5.74403285099999));
#202747=CARTESIAN_POINT('Ctrl Pts',(9.88010884599994,11.6,5.74403285099999));
#202748=CARTESIAN_POINT('Ctrl Pts',(9.87639521399995,15.2,5.74371152899998));
#202749=CARTESIAN_POINT('Ctrl Pts',(9.87639521399995,11.6,5.74371152899998));
#202750=CARTESIAN_POINT('Ctrl Pts',(9.87268630299994,15.2,5.74338775499999));
#202751=CARTESIAN_POINT('Ctrl Pts',(9.87268630299994,11.6,5.74338775499999));
#202752=CARTESIAN_POINT('Ctrl Pts',(9.86898211999995,15.2,5.74306153399998));
#202753=CARTESIAN_POINT('Ctrl Pts',(9.86898211999995,11.6,5.74306153399998));
#202754=CARTESIAN_POINT('Ctrl Pts',(9.86528267199994,15.2,5.74273287599999));
#202755=CARTESIAN_POINT('Ctrl Pts',(9.86528267199994,11.6,5.74273287599999));
#202756=CARTESIAN_POINT('Ctrl Pts',(9.86158796599995,15.2,5.74240178399998));
#202757=CARTESIAN_POINT('Ctrl Pts',(9.86158796599995,11.6,5.74240178399998));
#202758=CARTESIAN_POINT('Ctrl Pts',(9.85789800899994,15.2,5.74206826699999));
#202759=CARTESIAN_POINT('Ctrl Pts',(9.85789800899994,11.6,5.74206826699999));
#202760=CARTESIAN_POINT('Ctrl Pts',(9.85421280599994,15.2,5.74173232999998));
#202761=CARTESIAN_POINT('Ctrl Pts',(9.85421280599994,11.6,5.74173232999998));
#202762=CARTESIAN_POINT('Ctrl Pts',(9.85053236499994,15.2,5.74139397699999));
#202763=CARTESIAN_POINT('Ctrl Pts',(9.85053236499994,11.6,5.74139397699999));
#202764=CARTESIAN_POINT('Ctrl Pts',(9.84685669199994,15.2,5.74105321899999));
#202765=CARTESIAN_POINT('Ctrl Pts',(9.84685669199994,11.6,5.74105321899999));
#202766=CARTESIAN_POINT('Ctrl Pts',(9.84318579299994,15.2,5.74071005899999));
#202767=CARTESIAN_POINT('Ctrl Pts',(9.84318579299994,11.6,5.74071005899999));
#202768=CARTESIAN_POINT('Ctrl Pts',(9.83951967699995,15.2,5.74036450399999));
#202769=CARTESIAN_POINT('Ctrl Pts',(9.83951967699995,11.6,5.74036450399999));
#202770=CARTESIAN_POINT('Ctrl Pts',(9.83585834799995,15.2,5.74001656099998));
#202771=CARTESIAN_POINT('Ctrl Pts',(9.83585834799995,11.6,5.74001656099998));
#202772=CARTESIAN_POINT('Ctrl Pts',(9.83220181499994,15.2,5.73966623599999));
#202773=CARTESIAN_POINT('Ctrl Pts',(9.83220181499994,11.6,5.73966623599999));
#202774=CARTESIAN_POINT('Ctrl Pts',(9.82855008299994,15.2,5.73931353499999));
#202775=CARTESIAN_POINT('Ctrl Pts',(9.82855008299994,11.6,5.73931353499999));
#202776=CARTESIAN_POINT('Ctrl Pts',(9.82490315999994,15.2,5.73895846699998));
#202777=CARTESIAN_POINT('Ctrl Pts',(9.82490315999994,11.6,5.73895846699998));
#202778=CARTESIAN_POINT('Ctrl Pts',(9.82126105299994,15.2,5.73860103599999));
#202779=CARTESIAN_POINT('Ctrl Pts',(9.82126105299994,11.6,5.73860103599999));
#202780=CARTESIAN_POINT('Ctrl Pts',(9.81762376699994,15.2,5.73824124899998));
#202781=CARTESIAN_POINT('Ctrl Pts',(9.81762376699994,11.6,5.73824124899998));
#202782=CARTESIAN_POINT('Ctrl Pts',(9.81399130999994,15.2,5.73787911299998));
#202783=CARTESIAN_POINT('Ctrl Pts',(9.81399130999994,11.6,5.73787911299998));
#202784=CARTESIAN_POINT('Ctrl Pts',(9.81036368999994,15.2,5.73751463399999));
#202785=CARTESIAN_POINT('Ctrl Pts',(9.81036368999994,11.6,5.73751463399999));
#202786=CARTESIAN_POINT('Ctrl Pts',(9.80674090999995,15.2,5.73714781899999));
#202787=CARTESIAN_POINT('Ctrl Pts',(9.80674090999995,11.6,5.73714781899999));
#202788=CARTESIAN_POINT('Ctrl Pts',(9.80312298099994,15.2,5.73677867599999));
#202789=CARTESIAN_POINT('Ctrl Pts',(9.80312298099994,11.6,5.73677867599999));
#202790=CARTESIAN_POINT('Ctrl Pts',(9.79950990699994,15.2,5.73640720799999));
#202791=CARTESIAN_POINT('Ctrl Pts',(9.79950990699994,11.6,5.73640720799999));
#202792=CARTESIAN_POINT('Ctrl Pts',(9.79590169599994,15.2,5.73603342499998));
#202793=CARTESIAN_POINT('Ctrl Pts',(9.79590169599994,11.6,5.73603342499998));
#202794=CARTESIAN_POINT('Ctrl Pts',(9.79229835399994,15.2,5.73565733199998));
#202795=CARTESIAN_POINT('Ctrl Pts',(9.79229835399994,11.6,5.73565733199998));
#202796=CARTESIAN_POINT('Ctrl Pts',(9.78869988999995,15.2,5.73527893499998));
#202797=CARTESIAN_POINT('Ctrl Pts',(9.78869988999995,11.6,5.73527893499998));
#202798=CARTESIAN_POINT('Ctrl Pts',(9.78510630799994,15.2,5.73489824299998));
#202799=CARTESIAN_POINT('Ctrl Pts',(9.78510630799994,11.6,5.73489824299998));
#202800=CARTESIAN_POINT('Ctrl Pts',(9.78151761599995,15.2,5.73451526099999));
#202801=CARTESIAN_POINT('Ctrl Pts',(9.78151761599995,11.6,5.73451526099999));
#202802=CARTESIAN_POINT('Ctrl Pts',(9.77793381999994,15.2,5.73412999599999));
#202803=CARTESIAN_POINT('Ctrl Pts',(9.77793381999994,11.6,5.73412999599999));
#202804=CARTESIAN_POINT('Ctrl Pts',(9.77435492799994,15.2,5.73374245399998));
#202805=CARTESIAN_POINT('Ctrl Pts',(9.77435492799994,11.6,5.73374245399998));
#202806=CARTESIAN_POINT('Ctrl Pts',(9.77078094799994,15.2,5.73335264399999));
#202807=CARTESIAN_POINT('Ctrl Pts',(9.77078094799994,11.6,5.73335264399999));
#202808=CARTESIAN_POINT('Ctrl Pts',(9.76721188399994,15.2,5.73296056999999));
#202809=CARTESIAN_POINT('Ctrl Pts',(9.76721188399994,11.6,5.73296056999999));
#202810=CARTESIAN_POINT('Ctrl Pts',(9.76364774399994,15.2,5.73256623999999));
#202811=CARTESIAN_POINT('Ctrl Pts',(9.76364774399994,11.6,5.73256623999999));
#202812=CARTESIAN_POINT('Ctrl Pts',(9.76008853499994,15.2,5.73216966199999));
#202813=CARTESIAN_POINT('Ctrl Pts',(9.76008853499994,11.6,5.73216966199999));
#202814=CARTESIAN_POINT('Ctrl Pts',(9.75653426499995,15.2,5.73177084099999));
#202815=CARTESIAN_POINT('Ctrl Pts',(9.75653426499995,11.6,5.73177084099999));
#202816=CARTESIAN_POINT('Ctrl Pts',(9.75298493899994,15.2,5.73136978499999));
#202817=CARTESIAN_POINT('Ctrl Pts',(9.75298493899994,11.6,5.73136978499999));
#202818=CARTESIAN_POINT('Ctrl Pts',(9.74944056499995,15.2,5.73096649999999));
#202819=CARTESIAN_POINT('Ctrl Pts',(9.74944056499995,11.6,5.73096649999999));
#202820=CARTESIAN_POINT('Ctrl Pts',(9.74590114799994,15.2,5.73056099299999));
#202821=CARTESIAN_POINT('Ctrl Pts',(9.74590114799994,11.6,5.73056099299999));
#202822=CARTESIAN_POINT('Ctrl Pts',(9.74236669799994,15.2,5.73015327099998));
#202823=CARTESIAN_POINT('Ctrl Pts',(9.74236669799994,11.6,5.73015327099998));
#202824=CARTESIAN_POINT('Ctrl Pts',(9.73883722099995,15.2,5.72974334099998));
#202825=CARTESIAN_POINT('Ctrl Pts',(9.73883722099995,11.6,5.72974334099998));
#202826=CARTESIAN_POINT('Ctrl Pts',(9.73531272199994,15.2,5.72933120999998));
#202827=CARTESIAN_POINT('Ctrl Pts',(9.73531272199994,11.6,5.72933120999998));
#202828=CARTESIAN_POINT('Ctrl Pts',(9.73179320799994,15.2,5.72891688399999));
#202829=CARTESIAN_POINT('Ctrl Pts',(9.73179320799994,11.6,5.72891688399999));
#202830=CARTESIAN_POINT('Ctrl Pts',(9.72827868999994,15.2,5.72850037199998));
#202831=CARTESIAN_POINT('Ctrl Pts',(9.72827868999994,11.6,5.72850037199998));
#202832=CARTESIAN_POINT('Ctrl Pts',(9.72476916999995,15.2,5.72808167999998));
#202833=CARTESIAN_POINT('Ctrl Pts',(9.72476916999995,11.6,5.72808167999998));
#202834=CARTESIAN_POINT('Ctrl Pts',(9.72126465599995,15.2,5.72766081399998));
#202835=CARTESIAN_POINT('Ctrl Pts',(9.72126465599995,11.6,5.72766081399998));
#202836=CARTESIAN_POINT('Ctrl Pts',(9.71776515699995,15.2,5.72723778199999));
#202837=CARTESIAN_POINT('Ctrl Pts',(9.71776515699995,11.6,5.72723778199999));
#202838=CARTESIAN_POINT('Ctrl Pts',(9.71427067999995,15.2,5.72681258999998));
#202839=CARTESIAN_POINT('Ctrl Pts',(9.71427067999995,11.6,5.72681258999998));
#202840=CARTESIAN_POINT('Ctrl Pts',(9.71078122899995,15.2,5.72638524699999));
#202841=CARTESIAN_POINT('Ctrl Pts',(9.71078122899995,11.6,5.72638524699999));
#202842=CARTESIAN_POINT('Ctrl Pts',(9.70729681399994,15.2,5.72595575799999));
#202843=CARTESIAN_POINT('Ctrl Pts',(9.70729681399994,11.6,5.72595575799999));
#202844=CARTESIAN_POINT('Ctrl Pts',(9.70381743999994,15.2,5.72552413199999));
#202845=CARTESIAN_POINT('Ctrl Pts',(9.70381743999994,11.6,5.72552413199999));
#202846=CARTESIAN_POINT('Ctrl Pts',(9.70034311499995,15.2,5.72509037399998));
#202847=CARTESIAN_POINT('Ctrl Pts',(9.70034311499995,11.6,5.72509037399998));
#202848=CARTESIAN_POINT('Ctrl Pts',(9.69687384599995,15.2,5.72465449299998));
#202849=CARTESIAN_POINT('Ctrl Pts',(9.69687384599995,11.6,5.72465449299998));
#202850=CARTESIAN_POINT('Ctrl Pts',(9.69340963899995,15.2,5.72421649499999));
#202851=CARTESIAN_POINT('Ctrl Pts',(9.69340963899995,11.6,5.72421649499999));
#202852=CARTESIAN_POINT('Ctrl Pts',(9.68995050199995,15.2,5.72377638799999));
#202853=CARTESIAN_POINT('Ctrl Pts',(9.68995050199995,11.6,5.72377638799999));
#202854=CARTESIAN_POINT('Ctrl Pts',(9.68649644099994,15.2,5.72333417799998));
#202855=CARTESIAN_POINT('Ctrl Pts',(9.68649644099994,11.6,5.72333417799998));
#202856=CARTESIAN_POINT('Ctrl Pts',(9.68304746299994,15.2,5.72288987399999));
#202857=CARTESIAN_POINT('Ctrl Pts',(9.68304746299994,11.6,5.72288987399999));
#202858=CARTESIAN_POINT('Ctrl Pts',(9.67960357799994,15.2,5.72244348099999));
#202859=CARTESIAN_POINT('Ctrl Pts',(9.67960357799994,11.6,5.72244348099999));
#202860=CARTESIAN_POINT('Ctrl Pts',(9.67616478999994,15.2,5.72199500699998));
#202861=CARTESIAN_POINT('Ctrl Pts',(9.67616478999994,11.6,5.72199500699998));
#202862=CARTESIAN_POINT('Ctrl Pts',(9.67273110599994,15.2,5.72154445999999));
#202863=CARTESIAN_POINT('Ctrl Pts',(9.67273110599994,11.6,5.72154445999999));
#202864=CARTESIAN_POINT('Ctrl Pts',(9.66930253399994,15.2,5.72109184799999));
#202865=CARTESIAN_POINT('Ctrl Pts',(9.66930253399994,11.6,5.72109184799999));
#202866=CARTESIAN_POINT('Ctrl Pts',(9.66587907999994,15.2,5.72063717499999));
#202867=CARTESIAN_POINT('Ctrl Pts',(9.66587907999994,11.6,5.72063717499999));
#202868=CARTESIAN_POINT('Ctrl Pts',(9.66246075399994,15.2,5.72018045199999));
#202869=CARTESIAN_POINT('Ctrl Pts',(9.66246075399994,11.6,5.72018045199999));
#202870=CARTESIAN_POINT('Ctrl Pts',(9.65904755999994,15.2,5.71972168499999));
#202871=CARTESIAN_POINT('Ctrl Pts',(9.65904755999994,11.6,5.71972168499999));
#202872=CARTESIAN_POINT('Ctrl Pts',(9.65563950499994,15.2,5.71926088099998));
#202873=CARTESIAN_POINT('Ctrl Pts',(9.65563950499994,11.6,5.71926088099998));
#202874=CARTESIAN_POINT('Ctrl Pts',(9.65223659799994,15.2,5.71879804699999));
#202875=CARTESIAN_POINT('Ctrl Pts',(9.65223659799994,11.6,5.71879804699999));
#202876=CARTESIAN_POINT('Ctrl Pts',(9.64883884499995,15.2,5.71833318999998));
#202877=CARTESIAN_POINT('Ctrl Pts',(9.64883884499995,11.6,5.71833318999998));
#202878=CARTESIAN_POINT('Ctrl Pts',(9.64544625399995,15.2,5.71786631999998));
#202879=CARTESIAN_POINT('Ctrl Pts',(9.64544625399995,11.6,5.71786631999998));
#202880=CARTESIAN_POINT('Ctrl Pts',(9.64205882999994,15.2,5.71739744199999));
#202881=CARTESIAN_POINT('Ctrl Pts',(9.64205882999994,11.6,5.71739744199999));
#202882=CARTESIAN_POINT('Ctrl Pts',(9.63867658199995,15.2,5.71692656499999));
#202883=CARTESIAN_POINT('Ctrl Pts',(9.63867658199995,11.6,5.71692656499999));
#202884=CARTESIAN_POINT('Ctrl Pts',(9.63529951699994,15.2,5.71645369399998));
#202885=CARTESIAN_POINT('Ctrl Pts',(9.63529951699994,11.6,5.71645369399998));
#202886=CARTESIAN_POINT('Ctrl Pts',(9.63192764199994,15.2,5.71597883899998));
#202887=CARTESIAN_POINT('Ctrl Pts',(9.63192764199994,11.6,5.71597883899998));
#202888=CARTESIAN_POINT('Ctrl Pts',(9.62856096299994,15.2,5.71550200699999));
#202889=CARTESIAN_POINT('Ctrl Pts',(9.62856096299994,11.6,5.71550200699999));
#202890=CARTESIAN_POINT('Ctrl Pts',(9.62519948899994,15.2,5.71502320599999));
#202891=CARTESIAN_POINT('Ctrl Pts',(9.62519948899994,11.6,5.71502320599999));
#202892=CARTESIAN_POINT('Ctrl Pts',(9.62184322499994,15.2,5.71454244099999));
#202893=CARTESIAN_POINT('Ctrl Pts',(9.62184322499994,11.6,5.71454244099999));
#202894=CARTESIAN_POINT('Ctrl Pts',(9.61849217999994,15.2,5.71405972199998));
#202895=CARTESIAN_POINT('Ctrl Pts',(9.61849217999994,11.6,5.71405972199998));
#202896=CARTESIAN_POINT('Ctrl Pts',(9.61514635999994,15.2,5.71357505599998));
#202897=CARTESIAN_POINT('Ctrl Pts',(9.61514635999994,11.6,5.71357505599998));
#202898=CARTESIAN_POINT('Ctrl Pts',(9.61180577299995,15.2,5.71308845099999));
#202899=CARTESIAN_POINT('Ctrl Pts',(9.61180577299995,11.6,5.71308845099999));
#202900=CARTESIAN_POINT('Ctrl Pts',(9.60847042599994,15.2,5.71259991399998));
#202901=CARTESIAN_POINT('Ctrl Pts',(9.60847042599994,11.6,5.71259991399998));
#202902=CARTESIAN_POINT('Ctrl Pts',(9.60514032499994,15.2,5.71210945199999));
#202903=CARTESIAN_POINT('Ctrl Pts',(9.60514032499994,11.6,5.71210945199999));
#202904=CARTESIAN_POINT('Ctrl Pts',(9.60181547999994,15.2,5.71161707499999));
#202905=CARTESIAN_POINT('Ctrl Pts',(9.60181547999994,11.6,5.71161707499999));
#202906=CARTESIAN_POINT('Ctrl Pts',(9.59849589499994,15.2,5.71112278799998));
#202907=CARTESIAN_POINT('Ctrl Pts',(9.59849589499994,11.6,5.71112278799998));
#202908=CARTESIAN_POINT('Ctrl Pts',(9.59518157899995,15.2,5.71062659899999));
#202909=CARTESIAN_POINT('Ctrl Pts',(9.59518157899995,11.6,5.71062659899999));
#202910=CARTESIAN_POINT('Ctrl Pts',(9.59187253899995,15.2,5.71012851899999));
#202911=CARTESIAN_POINT('Ctrl Pts',(9.59187253899995,11.6,5.71012851899999));
#202912=CARTESIAN_POINT('Ctrl Pts',(9.58856878199994,15.2,5.70962855199999));
#202913=CARTESIAN_POINT('Ctrl Pts',(9.58856878199994,11.6,5.70962855199999));
#202914=CARTESIAN_POINT('Ctrl Pts',(9.58527031499995,15.2,5.70912670699999));
#202915=CARTESIAN_POINT('Ctrl Pts',(9.58527031499995,11.6,5.70912670699999));
#202916=CARTESIAN_POINT('Ctrl Pts',(9.58197714599994,15.2,5.70862299299999));
#202917=CARTESIAN_POINT('Ctrl Pts',(9.58197714599994,11.6,5.70862299299999));
#202918=CARTESIAN_POINT('Ctrl Pts',(9.57868928099994,15.2,5.70811741599999));
#202919=CARTESIAN_POINT('Ctrl Pts',(9.57868928099994,11.6,5.70811741599999));
#202920=CARTESIAN_POINT('Ctrl Pts',(9.57540672899994,15.2,5.70760998399999));
#202921=CARTESIAN_POINT('Ctrl Pts',(9.57540672899994,11.6,5.70760998399999));
#202922=CARTESIAN_POINT('Ctrl Pts',(9.57212949599995,15.2,5.70710070699998));
#202923=CARTESIAN_POINT('Ctrl Pts',(9.57212949599995,11.6,5.70710070699998));
#202924=CARTESIAN_POINT('Ctrl Pts',(9.56885758899995,15.2,5.70658958999999));
#202925=CARTESIAN_POINT('Ctrl Pts',(9.56885758899995,11.6,5.70658958999999));
#202926=CARTESIAN_POINT('Ctrl Pts',(9.56559101699994,15.2,5.70607664299998));
#202927=CARTESIAN_POINT('Ctrl Pts',(9.56559101699994,11.6,5.70607664299998));
#202928=CARTESIAN_POINT('Ctrl Pts',(9.56232978499994,15.2,5.70556187299999));
#202929=CARTESIAN_POINT('Ctrl Pts',(9.56232978499994,11.6,5.70556187299999));
#202930=CARTESIAN_POINT('Ctrl Pts',(9.55907390099994,15.2,5.70504528899999));
#202931=CARTESIAN_POINT('Ctrl Pts',(9.55907390099994,11.6,5.70504528899999));
#202932=CARTESIAN_POINT('Ctrl Pts',(9.55582337399994,15.2,5.70452689699999));
#202933=CARTESIAN_POINT('Ctrl Pts',(9.55582337399994,11.6,5.70452689699999));
#202934=CARTESIAN_POINT('Ctrl Pts',(9.55257820899994,15.2,5.70400670599999));
#202935=CARTESIAN_POINT('Ctrl Pts',(9.55257820899994,11.6,5.70400670599999));
#202936=CARTESIAN_POINT('Ctrl Pts',(9.54933841599994,15.2,5.70348472499998));
#202937=CARTESIAN_POINT('Ctrl Pts',(9.54933841599994,11.6,5.70348472499998));
#202938=CARTESIAN_POINT('Ctrl Pts',(9.54610399999994,15.2,5.70296096099998));
#202939=CARTESIAN_POINT('Ctrl Pts',(9.54610399999994,11.6,5.70296096099998));
#202940=CARTESIAN_POINT('Ctrl Pts',(9.54287496799994,15.2,5.70243542199999));
#202941=CARTESIAN_POINT('Ctrl Pts',(9.54287496799994,11.6,5.70243542199999));
#202942=CARTESIAN_POINT('Ctrl Pts',(9.53965132899994,15.2,5.70190811599999));
#202943=CARTESIAN_POINT('Ctrl Pts',(9.53965132899994,11.6,5.70190811599999));
#202944=CARTESIAN_POINT('Ctrl Pts',(9.53643308999995,15.2,5.70137905199999));
#202945=CARTESIAN_POINT('Ctrl Pts',(9.53643308999995,11.6,5.70137905199999));
#202946=CARTESIAN_POINT('Ctrl Pts',(9.53322025799994,15.2,5.70084823799998));
#202947=CARTESIAN_POINT('Ctrl Pts',(9.53322025799994,11.6,5.70084823799998));
#202948=CARTESIAN_POINT('Ctrl Pts',(9.53001284099994,15.2,5.70031568099999));
#202949=CARTESIAN_POINT('Ctrl Pts',(9.53001284099994,11.6,5.70031568099999));
#202950=CARTESIAN_POINT('Ctrl Pts',(9.52681084499994,15.2,5.69978138999998));
#202951=CARTESIAN_POINT('Ctrl Pts',(9.52681084499994,11.6,5.69978138999998));
#202952=CARTESIAN_POINT('Ctrl Pts',(9.52361427899995,15.2,5.69924537299999));
#202953=CARTESIAN_POINT('Ctrl Pts',(9.52361427899995,11.6,5.69924537299999));
#202954=CARTESIAN_POINT('Ctrl Pts',(9.52042314999994,15.2,5.69870763799998));
#202955=CARTESIAN_POINT('Ctrl Pts',(9.52042314999994,11.6,5.69870763799998));
#202956=CARTESIAN_POINT('Ctrl Pts',(9.51723746399994,15.2,5.69816819399998));
#202957=CARTESIAN_POINT('Ctrl Pts',(9.51723746399994,11.6,5.69816819399998));
#202958=CARTESIAN_POINT('Ctrl Pts',(9.51405722999995,15.2,5.69762704899999));
#202959=CARTESIAN_POINT('Ctrl Pts',(9.51405722999995,11.6,5.69762704899999));
#202960=CARTESIAN_POINT('Ctrl Pts',(9.51088245499994,15.2,5.69708421099998));
#202961=CARTESIAN_POINT('Ctrl Pts',(9.51088245499994,11.6,5.69708421099998));
#202962=CARTESIAN_POINT('Ctrl Pts',(9.50771314699994,15.2,5.69653968799999));
#202963=CARTESIAN_POINT('Ctrl Pts',(9.50771314699994,11.6,5.69653968799999));
#202964=CARTESIAN_POINT('Ctrl Pts',(9.50454931099994,15.2,5.69599348799999));
#202965=CARTESIAN_POINT('Ctrl Pts',(9.50454931099994,11.6,5.69599348799999));
#202966=CARTESIAN_POINT('Ctrl Pts',(9.50139095799994,15.2,5.69544562099999));
#202967=CARTESIAN_POINT('Ctrl Pts',(9.50139095799994,11.6,5.69544562099999));
#202968=CARTESIAN_POINT('Ctrl Pts',(9.49823809299994,15.2,5.69489609399999));
#202969=CARTESIAN_POINT('Ctrl Pts',(9.49823809299994,11.6,5.69489609399999));
#202970=CARTESIAN_POINT('Ctrl Pts',(9.49509072499995,15.2,5.69434491599999));
#202971=CARTESIAN_POINT('Ctrl Pts',(9.49509072499995,11.6,5.69434491599999));
#202972=CARTESIAN_POINT('Ctrl Pts',(9.49194885999994,15.2,5.69379209499999));
#202973=CARTESIAN_POINT('Ctrl Pts',(9.49194885999994,11.6,5.69379209499999));
#202974=CARTESIAN_POINT('Ctrl Pts',(9.48881250599995,15.2,5.69323763999999));
#202975=CARTESIAN_POINT('Ctrl Pts',(9.48881250599995,11.6,5.69323763999999));
#202976=CARTESIAN_POINT('Ctrl Pts',(9.48568167099994,15.2,5.69268155999998));
#202977=CARTESIAN_POINT('Ctrl Pts',(9.48568167099994,11.6,5.69268155999998));
#202978=CARTESIAN_POINT('Ctrl Pts',(9.48255636299994,15.2,5.69212386099998));
#202979=CARTESIAN_POINT('Ctrl Pts',(9.48255636299994,11.6,5.69212386099998));
#202980=CARTESIAN_POINT('Ctrl Pts',(9.47943658699995,15.2,5.69156455499999));
#202981=CARTESIAN_POINT('Ctrl Pts',(9.47943658699995,11.6,5.69156455499999));
#202982=CARTESIAN_POINT('Ctrl Pts',(9.47632235299994,15.2,5.69100364699998));
#202983=CARTESIAN_POINT('Ctrl Pts',(9.47632235299994,11.6,5.69100364699998));
#202984=CARTESIAN_POINT('Ctrl Pts',(9.47321366799994,15.2,5.69044114799999));
#202985=CARTESIAN_POINT('Ctrl Pts',(9.47321366799994,11.6,5.69044114799999));
#202986=CARTESIAN_POINT('Ctrl Pts',(9.47011053899995,15.2,5.68987706599999));
#202987=CARTESIAN_POINT('Ctrl Pts',(9.47011053899995,11.6,5.68987706599999));
#202988=CARTESIAN_POINT('Ctrl Pts',(9.46701297399994,15.2,5.68931140899998));
#202989=CARTESIAN_POINT('Ctrl Pts',(9.46701297399994,11.6,5.68931140899998));
#202990=CARTESIAN_POINT('Ctrl Pts',(9.46392097999994,15.2,5.68874418599999));
#202991=CARTESIAN_POINT('Ctrl Pts',(9.46392097999994,11.6,5.68874418599999));
#202992=CARTESIAN_POINT('Ctrl Pts',(9.46083456599995,15.2,5.68817540699998));
#202993=CARTESIAN_POINT('Ctrl Pts',(9.46083456599995,11.6,5.68817540699998));
#202994=CARTESIAN_POINT('Ctrl Pts',(9.45775373799994,15.2,5.68760507899999));
#202995=CARTESIAN_POINT('Ctrl Pts',(9.45775373799994,11.6,5.68760507899999));
#202996=CARTESIAN_POINT('Ctrl Pts',(9.45467850399995,15.2,5.68703321099999));
#202997=CARTESIAN_POINT('Ctrl Pts',(9.45467850399995,11.6,5.68703321099999));
#202998=CARTESIAN_POINT('Ctrl Pts',(9.45160887199994,15.2,5.68645981199998));
#202999=CARTESIAN_POINT('Ctrl Pts',(9.45160887199994,11.6,5.68645981199998));
#203000=CARTESIAN_POINT('Ctrl Pts',(9.44854484899994,15.2,5.68588488999998));
#203001=CARTESIAN_POINT('Ctrl Pts',(9.44854484899994,11.6,5.68588488999998));
#203002=CARTESIAN_POINT('Ctrl Pts',(9.44548644299994,15.2,5.68530845399999));
#203003=CARTESIAN_POINT('Ctrl Pts',(9.44548644299994,11.6,5.68530845399999));
#203004=CARTESIAN_POINT('Ctrl Pts',(9.44243366199995,15.2,5.68473051499998));
#203005=CARTESIAN_POINT('Ctrl Pts',(9.44243366199995,11.6,5.68473051499998));
#203006=CARTESIAN_POINT('Ctrl Pts',(9.43938651299994,15.2,5.68415107899998));
#203007=CARTESIAN_POINT('Ctrl Pts',(9.43938651299994,11.6,5.68415107899998));
#203008=CARTESIAN_POINT('Ctrl Pts',(9.43634500399994,15.2,5.68357015699998));
#203009=CARTESIAN_POINT('Ctrl Pts',(9.43634500399994,11.6,5.68357015699998));
#203010=CARTESIAN_POINT('Ctrl Pts',(9.43330914299995,15.2,5.68298775599998));
#203011=CARTESIAN_POINT('Ctrl Pts',(9.43330914299995,11.6,5.68298775599998));
#203012=CARTESIAN_POINT('Ctrl Pts',(9.43027893599995,15.2,5.68240388599998));
#203013=CARTESIAN_POINT('Ctrl Pts',(9.43027893599995,11.6,5.68240388599998));
#203014=CARTESIAN_POINT('Ctrl Pts',(9.42725439399995,15.2,5.68181855599998));
#203015=CARTESIAN_POINT('Ctrl Pts',(9.42725439399995,11.6,5.68181855599998));
#203016=CARTESIAN_POINT('Ctrl Pts',(9.42423552099994,15.2,5.68123177399999));
#203017=CARTESIAN_POINT('Ctrl Pts',(9.42423552099994,11.6,5.68123177399999));
#203018=CARTESIAN_POINT('Ctrl Pts',(9.42122232599995,15.2,5.68064355099998));
#203019=CARTESIAN_POINT('Ctrl Pts',(9.42122232599995,11.6,5.68064355099998));
#203020=CARTESIAN_POINT('Ctrl Pts',(9.41821481799994,15.2,5.68005389299999));
#203021=CARTESIAN_POINT('Ctrl Pts',(9.41821481799994,11.6,5.68005389299999));
#203022=CARTESIAN_POINT('Ctrl Pts',(9.41521300399994,15.2,5.67946281199998));
#203023=CARTESIAN_POINT('Ctrl Pts',(9.41521300399994,11.6,5.67946281199998));
#203024=CARTESIAN_POINT('Ctrl Pts',(9.41221688999994,15.2,5.67887031499998));
#203025=CARTESIAN_POINT('Ctrl Pts',(9.41221688999994,11.6,5.67887031499998));
#203026=CARTESIAN_POINT('Ctrl Pts',(9.40922648699994,15.2,5.67827641199998));
#203027=CARTESIAN_POINT('Ctrl Pts',(9.40922648699994,11.6,5.67827641199998));
#203028=CARTESIAN_POINT('Ctrl Pts',(9.40624179999995,15.2,5.67768111199998));
#203029=CARTESIAN_POINT('Ctrl Pts',(9.40624179999995,11.6,5.67768111199998));
#203030=CARTESIAN_POINT('Ctrl Pts',(9.40326283699994,15.2,5.67708442399999));
#203031=CARTESIAN_POINT('Ctrl Pts',(9.40326283699994,11.6,5.67708442399999));
#203032=CARTESIAN_POINT('Ctrl Pts',(9.40028960699994,15.2,5.67648635799999));
#203033=CARTESIAN_POINT('Ctrl Pts',(9.40028960699994,11.6,5.67648635799999));
#203034=CARTESIAN_POINT('Ctrl Pts',(9.39732211799994,15.2,5.67588692199998));
#203035=CARTESIAN_POINT('Ctrl Pts',(9.39732211799994,11.6,5.67588692199998));
#203036=CARTESIAN_POINT('Ctrl Pts',(9.39436037699994,15.2,5.67528612499999));
#203037=CARTESIAN_POINT('Ctrl Pts',(9.39436037699994,11.6,5.67528612499999));
#203038=CARTESIAN_POINT('Ctrl Pts',(9.39140439099994,15.2,5.67468397899999));
#203039=CARTESIAN_POINT('Ctrl Pts',(9.39140439099994,11.6,5.67468397899999));
#203040=CARTESIAN_POINT('Ctrl Pts',(9.38845416799994,15.2,5.67408048999998));
#203041=CARTESIAN_POINT('Ctrl Pts',(9.38845416799994,11.6,5.67408048999998));
#203042=CARTESIAN_POINT('Ctrl Pts',(9.38550971799994,15.2,5.67347566799998));
#203043=CARTESIAN_POINT('Ctrl Pts',(9.38550971799994,11.6,5.67347566799998));
#203044=CARTESIAN_POINT('Ctrl Pts',(9.38257104799994,15.2,5.67286952399999));
#203045=CARTESIAN_POINT('Ctrl Pts',(9.38257104799994,11.6,5.67286952399999));
#203046=CARTESIAN_POINT('Ctrl Pts',(9.37963816299994,15.2,5.67226206499999));
#203047=CARTESIAN_POINT('Ctrl Pts',(9.37963816299994,11.6,5.67226206499999));
#203048=CARTESIAN_POINT('Ctrl Pts',(9.37671107399994,15.2,5.67165330199998));
#203049=CARTESIAN_POINT('Ctrl Pts',(9.37671107399994,11.6,5.67165330199998));
#203050=CARTESIAN_POINT('Ctrl Pts',(9.37378978799994,15.2,5.67104324499999));
#203051=CARTESIAN_POINT('Ctrl Pts',(9.37378978799994,11.6,5.67104324499999));
#203052=CARTESIAN_POINT('Ctrl Pts',(9.37087431199994,15.2,5.67043190199998));
#203053=CARTESIAN_POINT('Ctrl Pts',(9.37087431199994,11.6,5.67043190199998));
#203054=CARTESIAN_POINT('Ctrl Pts',(9.36796465499994,15.2,5.66981928199999));
#203055=CARTESIAN_POINT('Ctrl Pts',(9.36796465499994,11.6,5.66981928199999));
#203056=CARTESIAN_POINT('Ctrl Pts',(9.36506082499994,15.2,5.66920539599998));
#203057=CARTESIAN_POINT('Ctrl Pts',(9.36506082499994,11.6,5.66920539599998));
#203058=CARTESIAN_POINT('Ctrl Pts',(9.36216282899995,15.2,5.66859025299999));
#203059=CARTESIAN_POINT('Ctrl Pts',(9.36216282899995,11.6,5.66859025299999));
#203060=CARTESIAN_POINT('Ctrl Pts',(9.35927067599994,15.2,5.66797386399998));
#203061=CARTESIAN_POINT('Ctrl Pts',(9.35927067599994,11.6,5.66797386399998));
#203062=CARTESIAN_POINT('Ctrl Pts',(9.35638437199995,15.2,5.66735623499999));
#203063=CARTESIAN_POINT('Ctrl Pts',(9.35638437199995,11.6,5.66735623499999));
#203064=CARTESIAN_POINT('Ctrl Pts',(9.35350392699995,15.2,5.66673737799999));
#203065=CARTESIAN_POINT('Ctrl Pts',(9.35350392699995,11.6,5.66673737799999));
#203066=CARTESIAN_POINT('Ctrl Pts',(9.35062934799994,15.2,5.66611730299999));
#203067=CARTESIAN_POINT('Ctrl Pts',(9.35062934799994,11.6,5.66611730299999));
#203068=CARTESIAN_POINT('Ctrl Pts',(9.34776064299994,15.2,5.66549601799998));
#203069=CARTESIAN_POINT('Ctrl Pts',(9.34776064299994,11.6,5.66549601799998));
#203070=CARTESIAN_POINT('Ctrl Pts',(9.34489781999994,15.2,5.66487353499999));
#203071=CARTESIAN_POINT('Ctrl Pts',(9.34489781999994,11.6,5.66487353499999));
#203072=CARTESIAN_POINT('Ctrl Pts',(9.34204088699994,15.2,5.66424986199999));
#203073=CARTESIAN_POINT('Ctrl Pts',(9.34204088699994,11.6,5.66424986199999));
#203074=CARTESIAN_POINT('Ctrl Pts',(9.33918985299995,15.2,5.66362500899999));
#203075=CARTESIAN_POINT('Ctrl Pts',(9.33918985299995,11.6,5.66362500899999));
#203076=CARTESIAN_POINT('Ctrl Pts',(9.33634472399994,15.2,5.66299898499998));
#203077=CARTESIAN_POINT('Ctrl Pts',(9.33634472399994,11.6,5.66299898499998));
#203078=CARTESIAN_POINT('Ctrl Pts',(9.33350550899995,15.2,5.66237180199998));
#203079=CARTESIAN_POINT('Ctrl Pts',(9.33350550899995,11.6,5.66237180199998));
#203080=CARTESIAN_POINT('Ctrl Pts',(9.33067221599994,15.2,5.66174346799999));
#203081=CARTESIAN_POINT('Ctrl Pts',(9.33067221599994,11.6,5.66174346799999));
#203082=CARTESIAN_POINT('Ctrl Pts',(9.32784485399995,15.2,5.66111399399999));
#203083=CARTESIAN_POINT('Ctrl Pts',(9.32784485399995,11.6,5.66111399399999));
#203084=CARTESIAN_POINT('Ctrl Pts',(9.32502342999994,15.2,5.66048338899999));
#203085=CARTESIAN_POINT('Ctrl Pts',(9.32502342999994,11.6,5.66048338899999));
#203086=CARTESIAN_POINT('Ctrl Pts',(9.32220795199994,15.2,5.65985166299999));
#203087=CARTESIAN_POINT('Ctrl Pts',(9.32220795199994,11.6,5.65985166299999));
#203088=CARTESIAN_POINT('Ctrl Pts',(9.31939842799994,15.2,5.65921882599999));
#203089=CARTESIAN_POINT('Ctrl Pts',(9.31939842799994,11.6,5.65921882599999));
#203090=CARTESIAN_POINT('Ctrl Pts',(9.31659486699994,15.2,5.65858488899998));
#203091=CARTESIAN_POINT('Ctrl Pts',(9.31659486699994,11.6,5.65858488899998));
#203092=CARTESIAN_POINT('Ctrl Pts',(9.31379727599994,15.2,5.65794985999998));
#203093=CARTESIAN_POINT('Ctrl Pts',(9.31379727599994,11.6,5.65794985999998));
#203094=CARTESIAN_POINT('Ctrl Pts',(9.31100566399994,15.2,5.65731375099999));
#203095=CARTESIAN_POINT('Ctrl Pts',(9.31100566399994,11.6,5.65731375099999));
#203096=CARTESIAN_POINT('Ctrl Pts',(9.30822003899994,15.2,5.65667657099999));
#203097=CARTESIAN_POINT('Ctrl Pts',(9.30822003899994,11.6,5.65667657099999));
#203098=CARTESIAN_POINT('Ctrl Pts',(9.30544040899994,15.2,5.65603833099999));
#203099=CARTESIAN_POINT('Ctrl Pts',(9.30544040899994,11.6,5.65603833099999));
#203100=CARTESIAN_POINT('Ctrl Pts',(9.30266678099994,15.2,5.65539904099998));
#203101=CARTESIAN_POINT('Ctrl Pts',(9.30266678099994,11.6,5.65539904099998));
#203102=CARTESIAN_POINT('Ctrl Pts',(9.29989916399995,15.2,5.65475870899999));
#203103=CARTESIAN_POINT('Ctrl Pts',(9.29989916399995,11.6,5.65475870899999));
#203104=CARTESIAN_POINT('Ctrl Pts',(9.29713756699994,15.2,5.65411734799999));
#203105=CARTESIAN_POINT('Ctrl Pts',(9.29713756699994,11.6,5.65411734799999));
#203106=CARTESIAN_POINT('Ctrl Pts',(9.29438199799994,15.2,5.65347496699999));
#203107=CARTESIAN_POINT('Ctrl Pts',(9.29438199799994,11.6,5.65347496699999));
#203108=CARTESIAN_POINT('Ctrl Pts',(9.29163246399994,15.2,5.65283157699999));
#203109=CARTESIAN_POINT('Ctrl Pts',(9.29163246399994,11.6,5.65283157699999));
#203110=CARTESIAN_POINT('Ctrl Pts',(9.28888897399995,15.2,5.65218718699998));
#203111=CARTESIAN_POINT('Ctrl Pts',(9.28888897399995,11.6,5.65218718699998));
#203112=CARTESIAN_POINT('Ctrl Pts',(9.28615153699995,15.2,5.65154180799999));
#203113=CARTESIAN_POINT('Ctrl Pts',(9.28615153699995,11.6,5.65154180799999));
#203114=CARTESIAN_POINT('Ctrl Pts',(9.28342015899995,15.2,5.65089544999999));
#203115=CARTESIAN_POINT('Ctrl Pts',(9.28342015899995,11.6,5.65089544999999));
#203116=CARTESIAN_POINT('Ctrl Pts',(9.28069484999994,15.2,5.65024812499999));
#203117=CARTESIAN_POINT('Ctrl Pts',(9.28069484999994,11.6,5.65024812499999));
#203118=CARTESIAN_POINT('Ctrl Pts',(9.27797561899995,15.2,5.64959983999999));
#203119=CARTESIAN_POINT('Ctrl Pts',(9.27797561899995,11.6,5.64959983999999));
#203120=CARTESIAN_POINT('Ctrl Pts',(9.27526247199994,15.2,5.64895060899998));
#203121=CARTESIAN_POINT('Ctrl Pts',(9.27526247199994,11.6,5.64895060899998));
#203122=CARTESIAN_POINT('Ctrl Pts',(9.27255541799994,15.2,5.64830044099998));
#203123=CARTESIAN_POINT('Ctrl Pts',(9.27255541799994,11.6,5.64830044099998));
#203124=CARTESIAN_POINT('Ctrl Pts',(9.26985446699994,15.2,5.64764934699999));
#203125=CARTESIAN_POINT('Ctrl Pts',(9.26985446699994,11.6,5.64764934699999));
#203126=CARTESIAN_POINT('Ctrl Pts',(9.26715962499994,15.2,5.64699733499998));
#203127=CARTESIAN_POINT('Ctrl Pts',(9.26715962499994,11.6,5.64699733499998));
#203128=CARTESIAN_POINT('Ctrl Pts',(9.26447090199994,15.2,5.64634441999999));
#203129=CARTESIAN_POINT('Ctrl Pts',(9.26447090199994,11.6,5.64634441999999));
#203130=CARTESIAN_POINT('Ctrl Pts',(9.26178830499994,15.2,5.64569060999998));
#203131=CARTESIAN_POINT('Ctrl Pts',(9.26178830499994,11.6,5.64569060999998));
#203132=CARTESIAN_POINT('Ctrl Pts',(9.25911184299995,15.2,5.64503591499999));
#203133=CARTESIAN_POINT('Ctrl Pts',(9.25911184299995,11.6,5.64503591499999));
#203134=CARTESIAN_POINT('Ctrl Pts',(9.25644152499994,15.2,5.64438034699998));
#203135=CARTESIAN_POINT('Ctrl Pts',(9.25644152499994,11.6,5.64438034699998));
#203136=CARTESIAN_POINT('Ctrl Pts',(9.25377735799995,15.2,5.64372391599999));
#203137=CARTESIAN_POINT('Ctrl Pts',(9.25377735799995,11.6,5.64372391599999));
#203138=CARTESIAN_POINT('Ctrl Pts',(9.25111935099994,15.2,5.64306663299998));
#203139=CARTESIAN_POINT('Ctrl Pts',(9.25111935099994,11.6,5.64306663299998));
#203140=CARTESIAN_POINT('Ctrl Pts',(9.24846751299994,15.2,5.64240850999998));
#203141=CARTESIAN_POINT('Ctrl Pts',(9.24846751299994,11.6,5.64240850999998));
#203142=CARTESIAN_POINT('Ctrl Pts',(9.24582185199995,15.2,5.64174955399999));
#203143=CARTESIAN_POINT('Ctrl Pts',(9.24582185199995,11.6,5.64174955399999));
#203144=CARTESIAN_POINT('Ctrl Pts',(9.24318237599994,15.2,5.64108978099998));
#203145=CARTESIAN_POINT('Ctrl Pts',(9.24318237599994,11.6,5.64108978099998));
#203146=CARTESIAN_POINT('Ctrl Pts',(9.24054909399995,15.2,5.64042919699999));
#203147=CARTESIAN_POINT('Ctrl Pts',(9.24054909399995,11.6,5.64042919699999));
#203148=CARTESIAN_POINT('Ctrl Pts',(9.23792201399994,15.2,5.63976781699999));
#203149=CARTESIAN_POINT('Ctrl Pts',(9.23792201399994,11.6,5.63976781699999));
#203150=CARTESIAN_POINT('Ctrl Pts',(9.23530114399994,15.2,5.63910564999999));
#203151=CARTESIAN_POINT('Ctrl Pts',(9.23530114399994,11.6,5.63910564999999));
#203152=CARTESIAN_POINT('Ctrl Pts',(9.23268649399994,15.2,5.63844270699998));
#203153=CARTESIAN_POINT('Ctrl Pts',(9.23268649399994,11.6,5.63844270699998));
#203154=CARTESIAN_POINT('Ctrl Pts',(9.23007807099994,15.2,5.63777899799998));
#203155=CARTESIAN_POINT('Ctrl Pts',(9.23007807099994,11.6,5.63777899799998));
#203156=CARTESIAN_POINT('Ctrl Pts',(9.22747588499995,15.2,5.63711453599999));
#203157=CARTESIAN_POINT('Ctrl Pts',(9.22747588499995,11.6,5.63711453599999));
#203158=CARTESIAN_POINT('Ctrl Pts',(9.22487994299994,15.2,5.63644933199999));
#203159=CARTESIAN_POINT('Ctrl Pts',(9.22487994299994,11.6,5.63644933199999));
#203160=CARTESIAN_POINT('Ctrl Pts',(9.22229025399995,15.2,5.63578339499998));
#203161=CARTESIAN_POINT('Ctrl Pts',(9.22229025399995,11.6,5.63578339499998));
#203162=CARTESIAN_POINT('Ctrl Pts',(9.21970682699994,15.2,5.63511673799999));
#203163=CARTESIAN_POINT('Ctrl Pts',(9.21970682699994,11.6,5.63511673799999));
#203164=CARTESIAN_POINT('Ctrl Pts',(9.21712967099995,15.2,5.63444937099998));
#203165=CARTESIAN_POINT('Ctrl Pts',(9.21712967099995,11.6,5.63444937099998));
#203166=CARTESIAN_POINT('Ctrl Pts',(9.21455879299995,15.2,5.63378130699999));
#203167=CARTESIAN_POINT('Ctrl Pts',(9.21455879299995,11.6,5.63378130699999));
#203168=CARTESIAN_POINT('Ctrl Pts',(9.21199420199994,15.2,5.63311255599999));
#203169=CARTESIAN_POINT('Ctrl Pts',(9.21199420199994,11.6,5.63311255599999));
#203170=CARTESIAN_POINT('Ctrl Pts',(9.20943590799994,15.2,5.63244312799998));
#203171=CARTESIAN_POINT('Ctrl Pts',(9.20943590799994,11.6,5.63244312799998));
#203172=CARTESIAN_POINT('Ctrl Pts',(9.20688391799995,15.2,5.63177303699998));
#203173=CARTESIAN_POINT('Ctrl Pts',(9.20688391799995,11.6,5.63177303699998));
#203174=CARTESIAN_POINT('Ctrl Pts',(9.20433824099994,15.2,5.63110229299999));
#203175=CARTESIAN_POINT('Ctrl Pts',(9.20433824099994,11.6,5.63110229299999));
#203176=CARTESIAN_POINT('Ctrl Pts',(9.20179888699994,15.2,5.63043090699999));
#203177=CARTESIAN_POINT('Ctrl Pts',(9.20179888699994,11.6,5.63043090699999));
#203178=CARTESIAN_POINT('Ctrl Pts',(9.19926586299994,15.2,5.62975889199999));
#203179=CARTESIAN_POINT('Ctrl Pts',(9.19926586299994,11.6,5.62975889199999));
#203180=CARTESIAN_POINT('Ctrl Pts',(9.19673917799994,15.2,5.62908625699999));
#203181=CARTESIAN_POINT('Ctrl Pts',(9.19673917799994,11.6,5.62908625699999));
#203182=CARTESIAN_POINT('Ctrl Pts',(9.19421883999994,15.2,5.62841301499999));
#203183=CARTESIAN_POINT('Ctrl Pts',(9.19421883999994,11.6,5.62841301499999));
#203184=CARTESIAN_POINT('Ctrl Pts',(9.19170485999994,15.2,5.62773917799999));
#203185=CARTESIAN_POINT('Ctrl Pts',(9.19170485999994,11.6,5.62773917799999));
#203186=CARTESIAN_POINT('Ctrl Pts',(9.18919724499995,15.2,5.62706475599998));
#203187=CARTESIAN_POINT('Ctrl Pts',(9.18919724499995,11.6,5.62706475599998));
#203188=CARTESIAN_POINT('Ctrl Pts',(9.18669600399994,15.2,5.62638976199998));
#203189=CARTESIAN_POINT('Ctrl Pts',(9.18669600399994,11.6,5.62638976199998));
#203190=CARTESIAN_POINT('Ctrl Pts',(9.18420114599994,15.2,5.62571420799999));
#203191=CARTESIAN_POINT('Ctrl Pts',(9.18420114599994,11.6,5.62571420799999));
#203192=CARTESIAN_POINT('Ctrl Pts',(9.18171267899995,15.2,5.62503810399999));
#203193=CARTESIAN_POINT('Ctrl Pts',(9.18171267899995,11.6,5.62503810399999));
#203194=CARTESIAN_POINT('Ctrl Pts',(9.17923061299994,15.2,5.62436146299999));
#203195=CARTESIAN_POINT('Ctrl Pts',(9.17923061299994,11.6,5.62436146299999));
#203196=CARTESIAN_POINT('Ctrl Pts',(9.17675495599994,15.2,5.62368429599999));
#203197=CARTESIAN_POINT('Ctrl Pts',(9.17675495599994,11.6,5.62368429599999));
#203198=CARTESIAN_POINT('Ctrl Pts',(9.17428571599994,15.2,5.62300661499999));
#203199=CARTESIAN_POINT('Ctrl Pts',(9.17428571599994,11.6,5.62300661499999));
#203200=CARTESIAN_POINT('Ctrl Pts',(9.17182290399994,15.2,5.62232843199999));
#203201=CARTESIAN_POINT('Ctrl Pts',(9.17182290399994,11.6,5.62232843199999));
#203202=CARTESIAN_POINT('Ctrl Pts',(9.16936652699994,15.2,5.62164975999998));
#203203=CARTESIAN_POINT('Ctrl Pts',(9.16936652699994,11.6,5.62164975999998));
#203204=CARTESIAN_POINT('Ctrl Pts',(9.16691659499994,15.2,5.62097060899998));
#203205=CARTESIAN_POINT('Ctrl Pts',(9.16691659499994,11.6,5.62097060899998));
#203206=CARTESIAN_POINT('Ctrl Pts',(9.16447311499994,15.2,5.62029099199999));
#203207=CARTESIAN_POINT('Ctrl Pts',(9.16447311499994,11.6,5.62029099199999));
#203208=CARTESIAN_POINT('Ctrl Pts',(9.16203609799994,15.2,5.61961092099998));
#203209=CARTESIAN_POINT('Ctrl Pts',(9.16203609799994,11.6,5.61961092099998));
#203210=CARTESIAN_POINT('Ctrl Pts',(9.15960555199994,15.2,5.61893040699999));
#203211=CARTESIAN_POINT('Ctrl Pts',(9.15960555199994,11.6,5.61893040699999));
#203212=CARTESIAN_POINT('Ctrl Pts',(9.15718148699994,15.2,5.61824946399998));
#203213=CARTESIAN_POINT('Ctrl Pts',(9.15718148699994,11.6,5.61824946399998));
#203214=CARTESIAN_POINT('Ctrl Pts',(9.15476390899994,15.2,5.61756810199999));
#203215=CARTESIAN_POINT('Ctrl Pts',(9.15476390899994,11.6,5.61756810199999));
#203216=CARTESIAN_POINT('Ctrl Pts',(9.15235282999994,15.2,5.61688633399999));
#203217=CARTESIAN_POINT('Ctrl Pts',(9.15235282999994,11.6,5.61688633399999));
#203218=CARTESIAN_POINT('Ctrl Pts',(9.14994825699995,15.2,5.61620417299999));
#203219=CARTESIAN_POINT('Ctrl Pts',(9.14994825699995,11.6,5.61620417299999));
#203220=CARTESIAN_POINT('Ctrl Pts',(9.14755020099994,15.2,5.61552162999998));
#203221=CARTESIAN_POINT('Ctrl Pts',(9.14755020099994,11.6,5.61552162999998));
#203222=CARTESIAN_POINT('Ctrl Pts',(9.14515866899994,15.2,5.61483871699998));
#203223=CARTESIAN_POINT('Ctrl Pts',(9.14515866899994,11.6,5.61483871699998));
#203224=CARTESIAN_POINT('Ctrl Pts',(9.14277367099994,15.2,5.61415544799999));
#203225=CARTESIAN_POINT('Ctrl Pts',(9.14277367099994,11.6,5.61415544799999));
#203226=CARTESIAN_POINT('Ctrl Pts',(9.14039521599994,15.2,5.61347183499999));
#203227=CARTESIAN_POINT('Ctrl Pts',(9.14039521599994,11.6,5.61347183499999));
#203228=CARTESIAN_POINT('Ctrl Pts',(9.13802331299994,15.2,5.61278788899998));
#203229=CARTESIAN_POINT('Ctrl Pts',(9.13802331299994,11.6,5.61278788899998));
#203230=CARTESIAN_POINT('Ctrl Pts',(9.13565796999994,15.2,5.61210362299998));
#203231=CARTESIAN_POINT('Ctrl Pts',(9.13565796999994,11.6,5.61210362299998));
#203232=CARTESIAN_POINT('Ctrl Pts',(9.13329919699994,15.2,5.61141905099999));
#203233=CARTESIAN_POINT('Ctrl Pts',(9.13329919699994,11.6,5.61141905099999));
#203234=CARTESIAN_POINT('Ctrl Pts',(9.13094700399995,15.2,5.61073418299999));
#203235=CARTESIAN_POINT('Ctrl Pts',(9.13094700399995,11.6,5.61073418299999));
#203236=CARTESIAN_POINT('Ctrl Pts',(9.12860139899994,15.2,5.61004903299998));
#203237=CARTESIAN_POINT('Ctrl Pts',(9.12860139899994,11.6,5.61004903299998));
#203238=CARTESIAN_POINT('Ctrl Pts',(9.12626239099994,15.2,5.60936361399998));
#203239=CARTESIAN_POINT('Ctrl Pts',(9.12626239099994,11.6,5.60936361399998));
#203240=CARTESIAN_POINT('Ctrl Pts',(9.12392998999995,15.2,5.60867793699998));
#203241=CARTESIAN_POINT('Ctrl Pts',(9.12392998999995,11.6,5.60867793699998));
#203242=CARTESIAN_POINT('Ctrl Pts',(9.12160420399994,15.2,5.60799201699999));
#203243=CARTESIAN_POINT('Ctrl Pts',(9.12160420399994,11.6,5.60799201699999));
#203244=CARTESIAN_POINT('Ctrl Pts',(9.11928504399994,15.2,5.60730586399998));
#203245=CARTESIAN_POINT('Ctrl Pts',(9.11928504399994,11.6,5.60730586399998));
#203246=CARTESIAN_POINT('Ctrl Pts',(9.11697251599995,15.2,5.60661949299998));
#203247=CARTESIAN_POINT('Ctrl Pts',(9.11697251599995,11.6,5.60661949299998));
#203248=CARTESIAN_POINT('Ctrl Pts',(9.11466663299995,15.2,5.60593291599999));
#203249=CARTESIAN_POINT('Ctrl Pts',(9.11466663299995,11.6,5.60593291599999));
#203250=CARTESIAN_POINT('Ctrl Pts',(9.11236740099995,15.2,5.60524614599998));
#203251=CARTESIAN_POINT('Ctrl Pts',(9.11236740099995,11.6,5.60524614599998));
#203252=CARTESIAN_POINT('Ctrl Pts',(9.11007483199995,15.2,5.60455919599999));
#203253=CARTESIAN_POINT('Ctrl Pts',(9.11007483199995,11.6,5.60455919599999));
#203254=CARTESIAN_POINT('Ctrl Pts',(9.10778893399995,15.2,5.60387207799998));
#203255=CARTESIAN_POINT('Ctrl Pts',(9.10778893399995,11.6,5.60387207799998));
#203256=CARTESIAN_POINT('Ctrl Pts',(9.10550971499994,15.2,5.60318480599998));
#203257=CARTESIAN_POINT('Ctrl Pts',(9.10550971499994,11.6,5.60318480599998));
#203258=CARTESIAN_POINT('Ctrl Pts',(9.10323718599994,15.2,5.60249739199998));
#203259=CARTESIAN_POINT('Ctrl Pts',(9.10323718599994,11.6,5.60249739199998));
#203260=CARTESIAN_POINT('Ctrl Pts',(9.10097135599995,15.2,5.60180985099999));
#203261=CARTESIAN_POINT('Ctrl Pts',(9.10097135599995,11.6,5.60180985099999));
#203262=CARTESIAN_POINT('Ctrl Pts',(9.09871223299995,15.2,5.60112219399999));
#203263=CARTESIAN_POINT('Ctrl Pts',(9.09871223299995,11.6,5.60112219399999));
#203264=CARTESIAN_POINT('Ctrl Pts',(9.09645982899994,15.2,5.60043443499998));
#203265=CARTESIAN_POINT('Ctrl Pts',(9.09645982899994,11.6,5.60043443499998));
#203266=CARTESIAN_POINT('Ctrl Pts',(9.09421415199994,15.2,5.59974658699999));
#203267=CARTESIAN_POINT('Ctrl Pts',(9.09421415199994,11.6,5.59974658699999));
#203268=CARTESIAN_POINT('Ctrl Pts',(9.09197521099994,15.2,5.59905866399999));
#203269=CARTESIAN_POINT('Ctrl Pts',(9.09197521099994,11.6,5.59905866399999));
#203270=CARTESIAN_POINT('Ctrl Pts',(9.08974301599994,15.2,5.59837067899998));
#203271=CARTESIAN_POINT('Ctrl Pts',(9.08974301599994,11.6,5.59837067899998));
#203272=CARTESIAN_POINT('Ctrl Pts',(9.08751757499994,15.2,5.59768264499999));
#203273=CARTESIAN_POINT('Ctrl Pts',(9.08751757499994,11.6,5.59768264499999));
#203274=CARTESIAN_POINT('Ctrl Pts',(9.08529889899994,15.2,5.59699457499998));
#203275=CARTESIAN_POINT('Ctrl Pts',(9.08529889899994,11.6,5.59699457499998));
#203276=CARTESIAN_POINT('Ctrl Pts',(9.08308699699995,15.2,5.59630648299999));
#203277=CARTESIAN_POINT('Ctrl Pts',(9.08308699699995,11.6,5.59630648299999));
#203278=CARTESIAN_POINT('Ctrl Pts',(9.08088187999994,15.2,5.59561838299998));
#203279=CARTESIAN_POINT('Ctrl Pts',(9.08088187999994,11.6,5.59561838299998));
#203280=CARTESIAN_POINT('Ctrl Pts',(9.07868355399994,15.2,5.59493028699999));
#203281=CARTESIAN_POINT('Ctrl Pts',(9.07868355399994,11.6,5.59493028699999));
#203282=CARTESIAN_POINT('Ctrl Pts',(9.07649203099994,15.2,5.59424220999999));
#203283=CARTESIAN_POINT('Ctrl Pts',(9.07649203099994,11.6,5.59424220999999));
#203284=CARTESIAN_POINT('Ctrl Pts',(9.07430732099994,15.2,5.59355416599999));
#203285=CARTESIAN_POINT('Ctrl Pts',(9.07430732099994,11.6,5.59355416599999));
#203286=CARTESIAN_POINT('Ctrl Pts',(9.07212943199994,15.2,5.59286616699998));
#203287=CARTESIAN_POINT('Ctrl Pts',(9.07212943199994,11.6,5.59286616699998));
#203288=CARTESIAN_POINT('Ctrl Pts',(9.06995837399995,15.2,5.59217822799998));
#203289=CARTESIAN_POINT('Ctrl Pts',(9.06995837399995,11.6,5.59217822799998));
#203290=CARTESIAN_POINT('Ctrl Pts',(9.06779415699994,15.2,5.59149036099999));
#203291=CARTESIAN_POINT('Ctrl Pts',(9.06779415699994,11.6,5.59149036099999));
#203292=CARTESIAN_POINT('Ctrl Pts',(9.06563679099994,15.2,5.59080258199998));
#203293=CARTESIAN_POINT('Ctrl Pts',(9.06563679099994,11.6,5.59080258199998));
#203294=CARTESIAN_POINT('Ctrl Pts',(9.06348628499994,15.2,5.59011490399998));
#203295=CARTESIAN_POINT('Ctrl Pts',(9.06348628499994,11.6,5.59011490399998));
#203296=CARTESIAN_POINT('Ctrl Pts',(9.06134264799995,15.2,5.58942733999999));
#203297=CARTESIAN_POINT('Ctrl Pts',(9.06134264799995,11.6,5.58942733999999));
#203298=CARTESIAN_POINT('Ctrl Pts',(9.05920589099994,15.2,5.58873990499999));
#203299=CARTESIAN_POINT('Ctrl Pts',(9.05920589099994,11.6,5.58873990499999));
#203300=CARTESIAN_POINT('Ctrl Pts',(9.05707602299995,15.2,5.58805261299998));
#203301=CARTESIAN_POINT('Ctrl Pts',(9.05707602299995,11.6,5.58805261299998));
#203302=CARTESIAN_POINT('Ctrl Pts',(9.05495305299995,15.2,5.58736547799998));
#203303=CARTESIAN_POINT('Ctrl Pts',(9.05495305299995,11.6,5.58736547799998));
#203304=CARTESIAN_POINT('Ctrl Pts',(9.05283699199994,15.2,5.58667851399999));
#203305=CARTESIAN_POINT('Ctrl Pts',(9.05283699199994,11.6,5.58667851399999));
#203306=CARTESIAN_POINT('Ctrl Pts',(9.05072784999994,15.2,5.58599173499999));
#203307=CARTESIAN_POINT('Ctrl Pts',(9.05072784999994,11.6,5.58599173499999));
#203308=CARTESIAN_POINT('Ctrl Pts',(9.04862563599995,15.2,5.58530515499999));
#203309=CARTESIAN_POINT('Ctrl Pts',(9.04862563599995,11.6,5.58530515499999));
#203310=CARTESIAN_POINT('Ctrl Pts',(9.04653035899995,15.2,5.58461878899998));
#203311=CARTESIAN_POINT('Ctrl Pts',(9.04653035899995,11.6,5.58461878899998));
#203312=CARTESIAN_POINT('Ctrl Pts',(9.04444203099994,15.2,5.58393264999999));
#203313=CARTESIAN_POINT('Ctrl Pts',(9.04444203099994,11.6,5.58393264999999));
#203314=CARTESIAN_POINT('Ctrl Pts',(9.04236065999994,15.2,5.58324675499998));
#203315=CARTESIAN_POINT('Ctrl Pts',(9.04236065999994,11.6,5.58324675499998));
#203316=CARTESIAN_POINT('Ctrl Pts',(9.04028625599994,15.2,5.58256111499999));
#203317=CARTESIAN_POINT('Ctrl Pts',(9.04028625599994,11.6,5.58256111499999));
#203318=CARTESIAN_POINT('Ctrl Pts',(9.03821882999994,15.2,5.58187574599998));
#203319=CARTESIAN_POINT('Ctrl Pts',(9.03821882999994,11.6,5.58187574599998));
#203320=CARTESIAN_POINT('Ctrl Pts',(9.03615839099994,15.2,5.58119066299999));
#203321=CARTESIAN_POINT('Ctrl Pts',(9.03615839099994,11.6,5.58119066299999));
#203322=CARTESIAN_POINT('Ctrl Pts',(9.03410494899994,15.2,5.58050587999999));
#203323=CARTESIAN_POINT('Ctrl Pts',(9.03410494899994,11.6,5.58050587999999));
#203324=CARTESIAN_POINT('Ctrl Pts',(9.03205851499994,15.2,5.57982141199999));
#203325=CARTESIAN_POINT('Ctrl Pts',(9.03205851499994,11.6,5.57982141199999));
#203326=CARTESIAN_POINT('Ctrl Pts',(9.03001909699995,15.2,5.57913727299999));
#203327=CARTESIAN_POINT('Ctrl Pts',(9.03001909699995,11.6,5.57913727299999));
#203328=CARTESIAN_POINT('Ctrl Pts',(9.02798670599994,15.2,5.57845347799999));
#203329=CARTESIAN_POINT('Ctrl Pts',(9.02798670599994,11.6,5.57845347799999));
#203330=CARTESIAN_POINT('Ctrl Pts',(9.02596135199994,15.2,5.57777004299999));
#203331=CARTESIAN_POINT('Ctrl Pts',(9.02596135199994,11.6,5.57777004299999));
#203332=CARTESIAN_POINT('Ctrl Pts',(9.02394304599994,15.2,5.57708698099999));
#203333=CARTESIAN_POINT('Ctrl Pts',(9.02394304599994,11.6,5.57708698099999));
#203334=CARTESIAN_POINT('Ctrl Pts',(9.02193179699994,15.2,5.57640430699998));
#203335=CARTESIAN_POINT('Ctrl Pts',(9.02193179699994,11.6,5.57640430699998));
#203336=CARTESIAN_POINT('Ctrl Pts',(9.01992761499995,15.2,5.57572203699999));
#203337=CARTESIAN_POINT('Ctrl Pts',(9.01992761499995,11.6,5.57572203699999));
#203338=CARTESIAN_POINT('Ctrl Pts',(9.01793051099994,15.2,5.57504018599998));
#203339=CARTESIAN_POINT('Ctrl Pts',(9.01793051099994,11.6,5.57504018599998));
#203340=CARTESIAN_POINT('Ctrl Pts',(9.01594049299994,15.2,5.57435876699999));
#203341=CARTESIAN_POINT('Ctrl Pts',(9.01594049299994,11.6,5.57435876699999));
#203342=CARTESIAN_POINT('Ctrl Pts',(9.01395757299994,15.2,5.57367779799999));
#203343=CARTESIAN_POINT('Ctrl Pts',(9.01395757299994,11.6,5.57367779799999));
#203344=CARTESIAN_POINT('Ctrl Pts',(9.01198176199994,15.2,5.57299729199999));
#203345=CARTESIAN_POINT('Ctrl Pts',(9.01198176199994,11.6,5.57299729199999));
#203346=CARTESIAN_POINT('Ctrl Pts',(9.01001306899994,15.2,5.57231726599999));
#203347=CARTESIAN_POINT('Ctrl Pts',(9.01001306899994,11.6,5.57231726599999));
#203348=CARTESIAN_POINT('Ctrl Pts',(9.00805150299994,15.2,5.57163773399999));
#203349=CARTESIAN_POINT('Ctrl Pts',(9.00805150299994,11.6,5.57163773399999));
#203350=CARTESIAN_POINT('Ctrl Pts',(9.00609707499994,15.2,5.57095871199999));
#203351=CARTESIAN_POINT('Ctrl Pts',(9.00609707499994,11.6,5.57095871199999));
#203352=CARTESIAN_POINT('Ctrl Pts',(9.00414979799995,15.2,5.57028021399999));
#203353=CARTESIAN_POINT('Ctrl Pts',(9.00414979799995,11.6,5.57028021399999));
#203354=CARTESIAN_POINT('Ctrl Pts',(9.00220967899994,15.2,5.56960225599998));
#203355=CARTESIAN_POINT('Ctrl Pts',(9.00220967899994,11.6,5.56960225599998));
#203356=CARTESIAN_POINT('Ctrl Pts',(9.00027672899994,15.2,5.56892485499999));
#203357=CARTESIAN_POINT('Ctrl Pts',(9.00027672899994,11.6,5.56892485499999));
#203358=CARTESIAN_POINT('Ctrl Pts',(8.99835095899994,15.2,5.56824802499998));
#203359=CARTESIAN_POINT('Ctrl Pts',(8.99835095899994,11.6,5.56824802499998));
#203360=CARTESIAN_POINT('Ctrl Pts',(8.99643237899994,15.2,5.56757178299998));
#203361=CARTESIAN_POINT('Ctrl Pts',(8.99643237899994,11.6,5.56757178299998));
#203362=CARTESIAN_POINT('Ctrl Pts',(8.99452099899994,15.2,5.56689614199998));
#203363=CARTESIAN_POINT('Ctrl Pts',(8.99452099899994,11.6,5.56689614199998));
#203364=CARTESIAN_POINT('Ctrl Pts',(8.99261682999994,15.2,5.56622111999998));
#203365=CARTESIAN_POINT('Ctrl Pts',(8.99261682999994,11.6,5.56622111999998));
#203366=CARTESIAN_POINT('Ctrl Pts',(8.99071988199994,15.2,5.56554673199999));
#203367=CARTESIAN_POINT('Ctrl Pts',(8.99071988199994,11.6,5.56554673199999));
#203368=CARTESIAN_POINT('Ctrl Pts',(8.98883016699994,15.2,5.56487299599999));
#203369=CARTESIAN_POINT('Ctrl Pts',(8.98883016699994,11.6,5.56487299599999));
#203370=CARTESIAN_POINT('Ctrl Pts',(8.98694769299994,15.2,5.56419992299999));
#203371=CARTESIAN_POINT('Ctrl Pts',(8.98694769299994,11.6,5.56419992299999));
#203372=CARTESIAN_POINT('Ctrl Pts',(8.98507247199994,15.2,5.56352753399998));
#203373=CARTESIAN_POINT('Ctrl Pts',(8.98507247199994,11.6,5.56352753399998));
#203374=CARTESIAN_POINT('Ctrl Pts',(8.98320451499995,15.2,5.56285584199999));
#203375=CARTESIAN_POINT('Ctrl Pts',(8.98320451499995,11.6,5.56285584199999));
#203376=CARTESIAN_POINT('Ctrl Pts',(8.98134383099995,15.2,5.56218486499999));
#203377=CARTESIAN_POINT('Ctrl Pts',(8.98134383099995,11.6,5.56218486499999));
#203378=CARTESIAN_POINT('Ctrl Pts',(8.97949043199995,15.2,5.56151461699999));
#203379=CARTESIAN_POINT('Ctrl Pts',(8.97949043199995,11.6,5.56151461699999));
#203380=CARTESIAN_POINT('Ctrl Pts',(8.97764432699995,15.2,5.56084511599998));
#203381=CARTESIAN_POINT('Ctrl Pts',(8.97764432699995,11.6,5.56084511599998));
#203382=CARTESIAN_POINT('Ctrl Pts',(8.97580552899995,15.2,5.56017637699998));
#203383=CARTESIAN_POINT('Ctrl Pts',(8.97580552899995,11.6,5.56017637699998));
#203384=CARTESIAN_POINT('Ctrl Pts',(8.97397404599995,15.2,5.55950841699998));
#203385=CARTESIAN_POINT('Ctrl Pts',(8.97397404599995,11.6,5.55950841699998));
#203386=CARTESIAN_POINT('Ctrl Pts',(8.97214989099994,15.2,5.55884125399999));
#203387=CARTESIAN_POINT('Ctrl Pts',(8.97214989099994,11.6,5.55884125399999));
#203388=CARTESIAN_POINT('Ctrl Pts',(8.97033307399994,15.2,5.55817490099999));
#203389=CARTESIAN_POINT('Ctrl Pts',(8.97033307399994,11.6,5.55817490099999));
#203390=CARTESIAN_POINT('Ctrl Pts',(8.96852360399994,15.2,5.55750937699998));
#203391=CARTESIAN_POINT('Ctrl Pts',(8.96852360399994,11.6,5.55750937699998));
#203392=CARTESIAN_POINT('Ctrl Pts',(8.96672149499994,15.2,5.55684469799999));
#203393=CARTESIAN_POINT('Ctrl Pts',(8.96672149499994,11.6,5.55684469799999));
#203394=CARTESIAN_POINT('Ctrl Pts',(8.96492675499994,15.2,5.55618087899998));
#203395=CARTESIAN_POINT('Ctrl Pts',(8.96492675499994,11.6,5.55618087899998));
#203396=CARTESIAN_POINT('Ctrl Pts',(8.96313939599995,15.2,5.55551794099999));
#203397=CARTESIAN_POINT('Ctrl Pts',(8.96313939599995,11.6,5.55551794099999));
#203398=CARTESIAN_POINT('Ctrl Pts',(8.96135942899994,15.2,5.55485589599999));
#203399=CARTESIAN_POINT('Ctrl Pts',(8.96135942899994,11.6,5.55485589599999));
#203400=CARTESIAN_POINT('Ctrl Pts',(8.95958686399995,15.2,5.55419476399998));
#203401=CARTESIAN_POINT('Ctrl Pts',(8.95958686399995,11.6,5.55419476399998));
#203402=CARTESIAN_POINT('Ctrl Pts',(8.95782171299994,15.2,5.55353455899999));
#203403=CARTESIAN_POINT('Ctrl Pts',(8.95782171299994,11.6,5.55353455899999));
#203404=CARTESIAN_POINT('Ctrl Pts',(8.95606398699995,15.2,5.55287530099999));
#203405=CARTESIAN_POINT('Ctrl Pts',(8.95606398699995,11.6,5.55287530099999));
#203406=CARTESIAN_POINT('Ctrl Pts',(8.95431369499994,15.2,5.55221700599999));
#203407=CARTESIAN_POINT('Ctrl Pts',(8.95431369499994,11.6,5.55221700599999));
#203408=CARTESIAN_POINT('Ctrl Pts',(8.95257084999994,15.2,5.55155968999999));
#203409=CARTESIAN_POINT('Ctrl Pts',(8.95257084999994,11.6,5.55155968999999));
#203410=CARTESIAN_POINT('Ctrl Pts',(8.95083546399994,15.2,5.55090337199999));
#203411=CARTESIAN_POINT('Ctrl Pts',(8.95083546399994,11.6,5.55090337199999));
#203412=CARTESIAN_POINT('Ctrl Pts',(8.94910754399995,15.2,5.55024806799998));
#203413=CARTESIAN_POINT('Ctrl Pts',(8.94910754399995,11.6,5.55024806799998));
#203414=CARTESIAN_POINT('Ctrl Pts',(8.94738710499994,15.2,5.54959379599998));
#203415=CARTESIAN_POINT('Ctrl Pts',(8.94738710499994,11.6,5.54959379599998));
#203416=CARTESIAN_POINT('Ctrl Pts',(8.94567415599994,15.2,5.54894057199999));
#203417=CARTESIAN_POINT('Ctrl Pts',(8.94567415599994,11.6,5.54894057199999));
#203418=CARTESIAN_POINT('Ctrl Pts',(8.94396870899994,15.2,5.54828841499998));
#203419=CARTESIAN_POINT('Ctrl Pts',(8.94396870899994,11.6,5.54828841499998));
#203420=CARTESIAN_POINT('Ctrl Pts',(8.94227077499994,15.2,5.54763734099998));
#203421=CARTESIAN_POINT('Ctrl Pts',(8.94227077499994,11.6,5.54763734099998));
#203422=CARTESIAN_POINT('Ctrl Pts',(8.94058036499995,15.2,5.54698736999998));
#203423=CARTESIAN_POINT('Ctrl Pts',(8.94058036499995,11.6,5.54698736999998));
#203424=CARTESIAN_POINT('Ctrl Pts',(8.93889749099994,15.2,5.54633851799998));
#203425=CARTESIAN_POINT('Ctrl Pts',(8.93889749099994,11.6,5.54633851799998));
#203426=CARTESIAN_POINT('Ctrl Pts',(8.93722216299994,15.2,5.54569080199999));
#203427=CARTESIAN_POINT('Ctrl Pts',(8.93722216299994,11.6,5.54569080199999));
#203428=CARTESIAN_POINT('Ctrl Pts',(8.93555439299995,15.2,5.54504424099999));
#203429=CARTESIAN_POINT('Ctrl Pts',(8.93555439299995,11.6,5.54504424099999));
#203430=CARTESIAN_POINT('Ctrl Pts',(8.93389419199995,15.2,5.54439885199999));
#203431=CARTESIAN_POINT('Ctrl Pts',(8.93389419199995,11.6,5.54439885199999));
#203432=CARTESIAN_POINT('Ctrl Pts',(8.93224157199995,15.2,5.54375465399998));
#203433=CARTESIAN_POINT('Ctrl Pts',(8.93224157199995,11.6,5.54375465399998));
#203434=CARTESIAN_POINT('Ctrl Pts',(8.93059654299994,15.2,5.54311166499998));
#203435=CARTESIAN_POINT('Ctrl Pts',(8.93059654299994,11.6,5.54311166499998));
#203436=CARTESIAN_POINT('Ctrl Pts',(8.92895911799994,15.2,5.54246990199999));
#203437=CARTESIAN_POINT('Ctrl Pts',(8.92895911799994,11.6,5.54246990199999));
#203438=CARTESIAN_POINT('Ctrl Pts',(8.92732930899994,15.2,5.54182938399999));
#203439=CARTESIAN_POINT('Ctrl Pts',(8.92732930899994,11.6,5.54182938399999));
#203440=CARTESIAN_POINT('Ctrl Pts',(8.92570712399994,15.2,5.54119012899999));
#203441=CARTESIAN_POINT('Ctrl Pts',(8.92570712399994,11.6,5.54119012899999));
#203442=CARTESIAN_POINT('Ctrl Pts',(8.92409257799994,15.2,5.54055215499999));
#203443=CARTESIAN_POINT('Ctrl Pts',(8.92409257799994,11.6,5.54055215499999));
#203444=CARTESIAN_POINT('Ctrl Pts',(8.92248568099994,15.2,5.53991548099999));
#203445=CARTESIAN_POINT('Ctrl Pts',(8.92248568099994,11.6,5.53991548099999));
#203446=CARTESIAN_POINT('Ctrl Pts',(8.92088644399994,15.2,5.53928012499998));
#203447=CARTESIAN_POINT('Ctrl Pts',(8.92088644399994,11.6,5.53928012499998));
#203448=CARTESIAN_POINT('Ctrl Pts',(8.91929488099995,15.2,5.53864610499998));
#203449=CARTESIAN_POINT('Ctrl Pts',(8.91929488099995,11.6,5.53864610499998));
#203450=CARTESIAN_POINT('Ctrl Pts',(8.91771100199995,15.2,5.53801344099998));
#203451=CARTESIAN_POINT('Ctrl Pts',(8.91771100199995,11.6,5.53801344099998));
#203452=CARTESIAN_POINT('Ctrl Pts',(8.91613481799994,15.2,5.53738214999999));
#203453=CARTESIAN_POINT('Ctrl Pts',(8.91613481799994,11.6,5.53738214999999));
#203454=CARTESIAN_POINT('Ctrl Pts',(8.91456634199994,15.2,5.53675225299998));
#203455=CARTESIAN_POINT('Ctrl Pts',(8.91456634199994,11.6,5.53675225299998));
#203456=CARTESIAN_POINT('Ctrl Pts',(8.91300558499994,15.2,5.53612376599999));
#203457=CARTESIAN_POINT('Ctrl Pts',(8.91300558499994,11.6,5.53612376599999));
#203458=CARTESIAN_POINT('Ctrl Pts',(8.91145255799995,15.2,5.53549671099999));
#203459=CARTESIAN_POINT('Ctrl Pts',(8.91145255799995,11.6,5.53549671099999));
#203460=CARTESIAN_POINT('Ctrl Pts',(8.90990727399994,15.2,5.53487110399999));
#203461=CARTESIAN_POINT('Ctrl Pts',(8.90990727399994,11.6,5.53487110399999));
#203462=CARTESIAN_POINT('Ctrl Pts',(8.90836974499994,15.2,5.53424696699999));
#203463=CARTESIAN_POINT('Ctrl Pts',(8.90836974499994,11.6,5.53424696699999));
#203464=CARTESIAN_POINT('Ctrl Pts',(8.90683998299994,15.2,5.53362431599999));
#203465=CARTESIAN_POINT('Ctrl Pts',(8.90683998299994,11.6,5.53362431599999));
#203466=CARTESIAN_POINT('Ctrl Pts',(8.90531799899994,15.2,5.53300317299998));
#203467=CARTESIAN_POINT('Ctrl Pts',(8.90531799899994,11.6,5.53300317299998));
#203468=CARTESIAN_POINT('Ctrl Pts',(8.90380380499994,15.2,5.53238355599999));
#203469=CARTESIAN_POINT('Ctrl Pts',(8.90380380499994,11.6,5.53238355599999));
#203470=CARTESIAN_POINT('Ctrl Pts',(8.90229741299994,15.2,5.53176548399998));
#203471=CARTESIAN_POINT('Ctrl Pts',(8.90229741299994,11.6,5.53176548399998));
#203472=CARTESIAN_POINT('Ctrl Pts',(8.90079883499994,15.2,5.53114897899999));
#203473=CARTESIAN_POINT('Ctrl Pts',(8.90079883499994,11.6,5.53114897899999));
#203474=CARTESIAN_POINT('Ctrl Pts',(8.89930808499994,15.2,5.53053405699998));
#203475=CARTESIAN_POINT('Ctrl Pts',(8.89930808499994,11.6,5.53053405699998));
#203476=CARTESIAN_POINT('Ctrl Pts',(8.89782517099994,15.2,5.52992073899999));
#203477=CARTESIAN_POINT('Ctrl Pts',(8.89782517099994,11.6,5.52992073899999));
#203478=CARTESIAN_POINT('Ctrl Pts',(8.89635010799994,15.2,5.52930904599998));
#203479=CARTESIAN_POINT('Ctrl Pts',(8.89635010799994,11.6,5.52930904599998));
#203480=CARTESIAN_POINT('Ctrl Pts',(8.89488290799994,15.2,5.52869899699999));
#203481=CARTESIAN_POINT('Ctrl Pts',(8.89488290799994,11.6,5.52869899699999));
#203482=CARTESIAN_POINT('Ctrl Pts',(8.89342358299994,15.2,5.52809061099998));
#203483=CARTESIAN_POINT('Ctrl Pts',(8.89342358299994,11.6,5.52809061099998));
#203484=CARTESIAN_POINT('Ctrl Pts',(8.89197214599994,15.2,5.52748390799999));
#203485=CARTESIAN_POINT('Ctrl Pts',(8.89197214599994,11.6,5.52748390799999));
#203486=CARTESIAN_POINT('Ctrl Pts',(8.89052860699995,15.2,5.52687890999999));
#203487=CARTESIAN_POINT('Ctrl Pts',(8.89052860699995,11.6,5.52687890999999));
#203488=CARTESIAN_POINT('Ctrl Pts',(8.88909297899995,15.2,5.52627563599999));
#203489=CARTESIAN_POINT('Ctrl Pts',(8.88909297899995,11.6,5.52627563599999));
#203490=CARTESIAN_POINT('Ctrl Pts',(8.88766527599994,15.2,5.52567410599998));
#203491=CARTESIAN_POINT('Ctrl Pts',(8.88766527599994,11.6,5.52567410599998));
#203492=CARTESIAN_POINT('Ctrl Pts',(8.88624550899995,15.2,5.52507433999998));
#203493=CARTESIAN_POINT('Ctrl Pts',(8.88624550899995,11.6,5.52507433999998));
#203494=CARTESIAN_POINT('Ctrl Pts',(8.88483369099994,15.2,5.52447635799999));
#203495=CARTESIAN_POINT('Ctrl Pts',(8.88483369099994,11.6,5.52447635799999));
#203496=CARTESIAN_POINT('Ctrl Pts',(8.88342983399994,15.2,5.52388018299999));
#203497=CARTESIAN_POINT('Ctrl Pts',(8.88342983399994,11.6,5.52388018299999));
#203498=CARTESIAN_POINT('Ctrl Pts',(8.88203394899995,15.2,5.52328583399999));
#203499=CARTESIAN_POINT('Ctrl Pts',(8.88203394899995,11.6,5.52328583399999));
#203500=CARTESIAN_POINT('Ctrl Pts',(8.88064605099995,15.2,5.52269333099999));
#203501=CARTESIAN_POINT('Ctrl Pts',(8.88064605099995,11.6,5.52269333099999));
#203502=CARTESIAN_POINT('Ctrl Pts',(8.87926615299994,15.2,5.52210269599998));
#203503=CARTESIAN_POINT('Ctrl Pts',(8.87926615299994,11.6,5.52210269599998));
#203504=CARTESIAN_POINT('Ctrl Pts',(8.87789426599995,15.2,5.52151394899998));
#203505=CARTESIAN_POINT('Ctrl Pts',(8.87789426599995,11.6,5.52151394899998));
#203506=CARTESIAN_POINT('Ctrl Pts',(8.87653040199995,15.2,5.52092711099998));
#203507=CARTESIAN_POINT('Ctrl Pts',(8.87653040199995,11.6,5.52092711099998));
#203508=CARTESIAN_POINT('Ctrl Pts',(8.87517457499994,15.2,5.52034220399998));
#203509=CARTESIAN_POINT('Ctrl Pts',(8.87517457499994,11.6,5.52034220399998));
#203510=CARTESIAN_POINT('Ctrl Pts',(8.87382679799994,15.2,5.51975924799999));
#203511=CARTESIAN_POINT('Ctrl Pts',(8.87382679799994,11.6,5.51975924799999));
#203512=CARTESIAN_POINT('Ctrl Pts',(8.87248708199994,15.2,5.51917826499999));
#203513=CARTESIAN_POINT('Ctrl Pts',(8.87248708199994,11.6,5.51917826499999));
#203514=CARTESIAN_POINT('Ctrl Pts',(8.87115544199995,15.2,5.51859927599998));
#203515=CARTESIAN_POINT('Ctrl Pts',(8.87115544199995,11.6,5.51859927599998));
#203516=CARTESIAN_POINT('Ctrl Pts',(8.86983188899995,15.2,5.51802230299998));
#203517=CARTESIAN_POINT('Ctrl Pts',(8.86983188899995,11.6,5.51802230299998));
#203518=CARTESIAN_POINT('Ctrl Pts',(8.86851643699995,15.2,5.51744736599999));
#203519=CARTESIAN_POINT('Ctrl Pts',(8.86851643699995,11.6,5.51744736599999));
#203520=CARTESIAN_POINT('Ctrl Pts',(8.86720909899994,15.2,5.51687448799999));
#203521=CARTESIAN_POINT('Ctrl Pts',(8.86720909899994,11.6,5.51687448799999));
#203522=CARTESIAN_POINT('Ctrl Pts',(8.86590988599994,15.2,5.51630369099998));
#203523=CARTESIAN_POINT('Ctrl Pts',(8.86590988599994,11.6,5.51630369099998));
#203524=CARTESIAN_POINT('Ctrl Pts',(8.86461881499994,15.2,5.51573499599999));
#203525=CARTESIAN_POINT('Ctrl Pts',(8.86461881499994,11.6,5.51573499599999));
#203526=CARTESIAN_POINT('Ctrl Pts',(8.86333589499994,15.2,5.51516842399998));
#203527=CARTESIAN_POINT('Ctrl Pts',(8.86333589499994,11.6,5.51516842399998));
#203528=CARTESIAN_POINT('Ctrl Pts',(8.86206114199994,15.2,5.51460399899998));
#203529=CARTESIAN_POINT('Ctrl Pts',(8.86206114199994,11.6,5.51460399899998));
#203530=CARTESIAN_POINT('Ctrl Pts',(8.86079456699994,15.2,5.51404174299999));
#203531=CARTESIAN_POINT('Ctrl Pts',(8.86079456699994,11.6,5.51404174299999));
#203532=CARTESIAN_POINT('Ctrl Pts',(8.85953618399994,15.2,5.51348167599999));
#203533=CARTESIAN_POINT('Ctrl Pts',(8.85953618399994,11.6,5.51348167599999));
#203534=CARTESIAN_POINT('Ctrl Pts',(8.85828600699995,15.2,5.51292382299999));
#203535=CARTESIAN_POINT('Ctrl Pts',(8.85828600699995,11.6,5.51292382299999));
#203536=CARTESIAN_POINT('Ctrl Pts',(8.85704404899995,15.2,5.51236820399998));
#203537=CARTESIAN_POINT('Ctrl Pts',(8.85704404899995,11.6,5.51236820399998));
#203538=CARTESIAN_POINT('Ctrl Pts',(8.85581032199994,15.2,5.51181484299998));
#203539=CARTESIAN_POINT('Ctrl Pts',(8.85581032199994,11.6,5.51181484299998));
#203540=CARTESIAN_POINT('Ctrl Pts',(8.85458484099994,15.2,5.51126376199999));
#203541=CARTESIAN_POINT('Ctrl Pts',(8.85458484099994,11.6,5.51126376199999));
#203542=CARTESIAN_POINT('Ctrl Pts',(8.85336761799994,15.2,5.51071498499999));
#203543=CARTESIAN_POINT('Ctrl Pts',(8.85336761799994,11.6,5.51071498499999));
#203544=CARTESIAN_POINT('Ctrl Pts',(8.85215866799994,15.2,5.51016853299998));
#203545=CARTESIAN_POINT('Ctrl Pts',(8.85215866799994,11.6,5.51016853299998));
#203546=CARTESIAN_POINT('Ctrl Pts',(8.85095800299995,15.2,5.50962442999998));
#203547=CARTESIAN_POINT('Ctrl Pts',(8.85095800299995,11.6,5.50962442999998));
#203548=CARTESIAN_POINT('Ctrl Pts',(8.84976563899994,15.2,5.50908269999999));
#203549=CARTESIAN_POINT('Ctrl Pts',(8.84976563899994,11.6,5.50908269999999));
#203550=CARTESIAN_POINT('Ctrl Pts',(8.84858158699994,15.2,5.50854336299999));
#203551=CARTESIAN_POINT('Ctrl Pts',(8.84858158699994,11.6,5.50854336299999));
#203552=CARTESIAN_POINT('Ctrl Pts',(8.84740586099995,15.2,5.50800644699999));
#203553=CARTESIAN_POINT('Ctrl Pts',(8.84740586099995,11.6,5.50800644699999));
#203554=CARTESIAN_POINT('Ctrl Pts',(8.84623847599994,15.2,5.50747196999998));
#203555=CARTESIAN_POINT('Ctrl Pts',(8.84623847599994,11.6,5.50747196999998));
#203556=CARTESIAN_POINT('Ctrl Pts',(8.84507944399994,15.2,5.50693995899999));
#203557=CARTESIAN_POINT('Ctrl Pts',(8.84507944399994,11.6,5.50693995899999));
#203558=CARTESIAN_POINT('Ctrl Pts',(8.84392878099994,15.2,5.50641043699999));
#203559=CARTESIAN_POINT('Ctrl Pts',(8.84392878099994,11.6,5.50641043699999));
#203560=CARTESIAN_POINT('Ctrl Pts',(8.84278649899995,15.2,5.50588342799998));
#203561=CARTESIAN_POINT('Ctrl Pts',(8.84278649899995,11.6,5.50588342799998));
#203562=CARTESIAN_POINT('Ctrl Pts',(8.84165261299995,15.2,5.50535895499999));
#203563=CARTESIAN_POINT('Ctrl Pts',(8.84165261299995,11.6,5.50535895499999));
#203564=CARTESIAN_POINT('Ctrl Pts',(8.84052713599995,15.2,5.50483704199999));
#203565=CARTESIAN_POINT('Ctrl Pts',(8.84052713599995,11.6,5.50483704199999));
#203566=CARTESIAN_POINT('Ctrl Pts',(8.83941008399994,15.2,5.50431771299999));
#203567=CARTESIAN_POINT('Ctrl Pts',(8.83941008399994,11.6,5.50431771299999));
#203568=CARTESIAN_POINT('Ctrl Pts',(8.83830146799994,15.2,5.50380099199998));
#203569=CARTESIAN_POINT('Ctrl Pts',(8.83830146799994,11.6,5.50380099199998));
#203570=CARTESIAN_POINT('Ctrl Pts',(8.83720130399994,15.2,5.50328690399999));
#203571=CARTESIAN_POINT('Ctrl Pts',(8.83720130399994,11.6,5.50328690399999));
#203572=CARTESIAN_POINT('Ctrl Pts',(8.83610960699994,15.2,5.50277547399999));
#203573=CARTESIAN_POINT('Ctrl Pts',(8.83610960699994,11.6,5.50277547399999));
#203574=CARTESIAN_POINT('Ctrl Pts',(8.83502638899994,15.2,5.50226672399998));
#203575=CARTESIAN_POINT('Ctrl Pts',(8.83502638899994,11.6,5.50226672399998));
#203576=CARTESIAN_POINT('Ctrl Pts',(8.83395166499995,15.2,5.50176068099999));
#203577=CARTESIAN_POINT('Ctrl Pts',(8.83395166499995,11.6,5.50176068099999));
#203578=CARTESIAN_POINT('Ctrl Pts',(8.83288545099994,15.2,5.50125736999998));
#203579=CARTESIAN_POINT('Ctrl Pts',(8.83288545099994,11.6,5.50125736999998));
#203580=CARTESIAN_POINT('Ctrl Pts',(8.83182775899994,15.2,5.50075681399999));
#203581=CARTESIAN_POINT('Ctrl Pts',(8.83182775899994,11.6,5.50075681399999));
#203582=CARTESIAN_POINT('Ctrl Pts',(8.83077860499995,15.2,5.50025903799998));
#203583=CARTESIAN_POINT('Ctrl Pts',(8.83077860499995,11.6,5.50025903799998));
#203584=CARTESIAN_POINT('Ctrl Pts',(8.82973800299995,15.2,5.49976406899999));
#203585=CARTESIAN_POINT('Ctrl Pts',(8.82973800299995,11.6,5.49976406899999));
#203586=CARTESIAN_POINT('Ctrl Pts',(8.82870596699994,15.2,5.49927192999998));
#203587=CARTESIAN_POINT('Ctrl Pts',(8.82870596699994,11.6,5.49927192999998));
#203588=CARTESIAN_POINT('Ctrl Pts',(8.82768251199994,15.2,5.49878264899998));
#203589=CARTESIAN_POINT('Ctrl Pts',(8.82768251199994,11.6,5.49878264899998));
#203590=CARTESIAN_POINT('Ctrl Pts',(8.82666765299994,15.2,5.49829624999998));
#203591=CARTESIAN_POINT('Ctrl Pts',(8.82666765299994,11.6,5.49829624999998));
#203592=CARTESIAN_POINT('Ctrl Pts',(8.82566140499994,15.2,5.49781275799998));
#203593=CARTESIAN_POINT('Ctrl Pts',(8.82566140499994,11.6,5.49781275799998));
#203594=CARTESIAN_POINT('Ctrl Pts',(8.82466378099994,15.2,5.49733219899998));
#203595=CARTESIAN_POINT('Ctrl Pts',(8.82466378099994,11.6,5.49733219899998));
#203596=CARTESIAN_POINT('Ctrl Pts',(8.82367479799994,15.2,5.49685459999999));
#203597=CARTESIAN_POINT('Ctrl Pts',(8.82367479799994,11.6,5.49685459999999));
#203598=CARTESIAN_POINT('Ctrl Pts',(8.82269446899994,15.2,5.49637998599999));
#203599=CARTESIAN_POINT('Ctrl Pts',(8.82269446899994,11.6,5.49637998599999));
#203600=CARTESIAN_POINT('Ctrl Pts',(8.82172280999994,15.2,5.49590838499999));
#203601=CARTESIAN_POINT('Ctrl Pts',(8.82172280999994,11.6,5.49590838499999));
#203602=CARTESIAN_POINT('Ctrl Pts',(8.82075983499995,15.2,5.49543981999999));
#203603=CARTESIAN_POINT('Ctrl Pts',(8.82075983499995,11.6,5.49543981999999));
#203604=CARTESIAN_POINT('Ctrl Pts',(8.81980556099995,15.2,5.49497431899999));
#203605=CARTESIAN_POINT('Ctrl Pts',(8.81980556099995,11.6,5.49497431899999));
#203606=CARTESIAN_POINT('Ctrl Pts',(8.81886000299994,15.2,5.49451190899998));
#203607=CARTESIAN_POINT('Ctrl Pts',(8.81886000299994,11.6,5.49451190899998));
#203608=CARTESIAN_POINT('Ctrl Pts',(8.81792317299994,15.2,5.49405261699999));
#203609=CARTESIAN_POINT('Ctrl Pts',(8.81792317299994,11.6,5.49405261699999));
#203610=CARTESIAN_POINT('Ctrl Pts',(8.81699508899995,15.2,5.49359646799999));
#203611=CARTESIAN_POINT('Ctrl Pts',(8.81699508899995,11.6,5.49359646799999));
#203612=CARTESIAN_POINT('Ctrl Pts',(8.81607576599994,15.2,5.49314348999999));
#203613=CARTESIAN_POINT('Ctrl Pts',(8.81607576599994,11.6,5.49314348999999));
#203614=CARTESIAN_POINT('Ctrl Pts',(8.81516521899994,15.2,5.49269370999999));
#203615=CARTESIAN_POINT('Ctrl Pts',(8.81516521899994,11.6,5.49269370999999));
#203616=CARTESIAN_POINT('Ctrl Pts',(8.81426346299994,15.2,5.49224715599999));
#203617=CARTESIAN_POINT('Ctrl Pts',(8.81426346299994,11.6,5.49224715599999));
#203618=CARTESIAN_POINT('Ctrl Pts',(8.81337051299995,15.2,5.49180385399998));
#203619=CARTESIAN_POINT('Ctrl Pts',(8.81337051299995,11.6,5.49180385399998));
#203620=CARTESIAN_POINT('Ctrl Pts',(8.81248638699994,15.2,5.49136383299999));
#203621=CARTESIAN_POINT('Ctrl Pts',(8.81248638699994,11.6,5.49136383299999));
#203622=CARTESIAN_POINT('Ctrl Pts',(8.81161109899994,15.2,5.49092711899998));
#203623=CARTESIAN_POINT('Ctrl Pts',(8.81161109899994,11.6,5.49092711899998));
#203624=CARTESIAN_POINT('Ctrl Pts',(8.81074466299994,15.2,5.49049374099998));
#203625=CARTESIAN_POINT('Ctrl Pts',(8.81074466299994,11.6,5.49049374099998));
#203626=CARTESIAN_POINT('Ctrl Pts',(8.80988709799994,15.2,5.49006372699999));
#203627=CARTESIAN_POINT('Ctrl Pts',(8.80988709799994,11.6,5.49006372699999));
#203628=CARTESIAN_POINT('Ctrl Pts',(8.80903841799995,15.2,5.48963710299999));
#203629=CARTESIAN_POINT('Ctrl Pts',(8.80903841799995,11.6,5.48963710299999));
#203630=CARTESIAN_POINT('Ctrl Pts',(8.80819863999994,15.2,5.48921389999999));
#203631=CARTESIAN_POINT('Ctrl Pts',(8.80819863999994,11.6,5.48921389999999));
#203632=CARTESIAN_POINT('Ctrl Pts',(8.80736777699994,15.2,5.48879414499999));
#203633=CARTESIAN_POINT('Ctrl Pts',(8.80736777699994,11.6,5.48879414499999));
#203634=CARTESIAN_POINT('Ctrl Pts',(8.80655058299994,15.2,5.48838026399999));
#203635=CARTESIAN_POINT('Ctrl Pts',(8.80655058299994,11.6,5.48838026399999));
#203636=CARTESIAN_POINT('Ctrl Pts',(8.80590482999994,15.2,5.48805240199999));
#203637=CARTESIAN_POINT('Ctrl Pts',(8.80590482999994,11.6,5.48805240199999));
#203638=CARTESIAN_POINT('Ctrl Pts',(8.80542564399994,15.2,5.48780866099998));
#203639=CARTESIAN_POINT('Ctrl Pts',(8.80542564399994,11.6,5.48780866099998));
#203640=CARTESIAN_POINT('Ctrl Pts',(8.80510947799995,15.2,5.48764764399999));
#203641=CARTESIAN_POINT('Ctrl Pts',(8.80510947799995,11.6,5.48764764399999));
#203642=CARTESIAN_POINT('Ctrl Pts',(8.80495412799995,15.2,5.48756847999999));
#203643=CARTESIAN_POINT('Ctrl Pts',(8.80495412799995,11.6,5.48756847999999));
#203644=CARTESIAN_POINT('',(8.80495412746567,12.2,5.48756847941583));
#203645=CARTESIAN_POINT('',(8.80495412746567,15.2,5.48756847941583));
#203646=CARTESIAN_POINT('',(8.80495412699995,12.2,5.48756847899998));
#203647=CARTESIAN_POINT('Ctrl Pts',(9.95917514599994,12.2,5.75020264099999));
#203648=CARTESIAN_POINT('Ctrl Pts',(9.95536157030715,12.2,5.74993548595142));
#203649=CARTESIAN_POINT('Ctrl Pts',(9.95155489341636,12.2,5.74966449046052));
#203650=CARTESIAN_POINT('Ctrl Pts',(9.94775512114579,12.2,5.74938964953395));
#203651=CARTESIAN_POINT('Ctrl Pts',(9.94395534887523,12.2,5.74911480860738));
#203652=CARTESIAN_POINT('Ctrl Pts',(9.94016247816818,12.2,5.74883612260804));
#203653=CARTESIAN_POINT('Ctrl Pts',(9.93637652394912,12.2,5.7485536050213));
#203654=CARTESIAN_POINT('Ctrl Pts',(9.93259056973007,12.2,5.74827108743457));
#203655=CARTESIAN_POINT('Ctrl Pts',(9.92881153168612,12.2,5.74798473883553));
#203656=CARTESIAN_POINT('Ctrl Pts',(9.92503944240555,12.2,5.74769458655493));
#203657=CARTESIAN_POINT('Ctrl Pts',(9.92126735243973,12.2,5.74740443422161));
#203658=CARTESIAN_POINT('Ctrl Pts',(9.9175022111092,12.2,5.74711048106222));
#203659=CARTESIAN_POINT('Ctrl Pts',(9.91374405518896,12.2,5.74681275914344));
#203660=CARTESIAN_POINT('Ctrl Pts',(9.90998589995145,12.2,5.74651503727874));
#203661=CARTESIAN_POINT('Ctrl Pts',(9.90623472967193,12.2,5.74621354825591));
#203662=CARTESIAN_POINT('Ctrl Pts',(9.90249057380857,12.2,5.74590831722501));
#203663=CARTESIAN_POINT('Ctrl Pts',(9.89874641794522,12.2,5.74560308619412));
#203664=CARTESIAN_POINT('Ctrl Pts',(9.89500927564456,12.2,5.7452941130898));
#203665=CARTESIAN_POINT('Ctrl Pts',(9.89127917472151,12.2,5.74498142451639));
#203666=CARTESIAN_POINT('Ctrl Pts',(9.88754907379846,12.2,5.74466873594298));
#203667=CARTESIAN_POINT('Ctrl Pts',(9.88382601290183,12.2,5.74435232967344));
#203668=CARTESIAN_POINT('Ctrl Pts',(9.88011002451994,12.2,5.7440322367253));
#203669=CARTESIAN_POINT('Ctrl Pts',(9.87639403613804,12.2,5.74371214377716));
#203670=CARTESIAN_POINT('Ctrl Pts',(9.8726851189363,12.2,5.74338836367343));
#203671=CARTESIAN_POINT('Ctrl Pts',(9.86898330415351,12.2,5.74306092472731));
#203672=CARTESIAN_POINT('Ctrl Pts',(9.86528148937072,12.2,5.74273348578119));
#203673=CARTESIAN_POINT('Ctrl Pts',(9.86158677765411,12.2,5.74240238867699));
#203674=CARTESIAN_POINT('Ctrl Pts',(9.85789919832879,12.2,5.74206766206465));
#203675=CARTESIAN_POINT('Ctrl Pts',(9.85421161833356,12.2,5.7417329353915));
#203676=CARTESIAN_POINT('Ctrl Pts',(9.850531170632,12.2,5.74139457709232));
#203677=CARTESIAN_POINT('Ctrl Pts',(9.84685788472413,12.2,5.7410526184588));
#203678=CARTESIAN_POINT('Ctrl Pts',(9.84196017129248,12.2,5.74059667371764));
#203679=CARTESIAN_POINT('Ctrl Pts',(9.83707519084653,12.2,5.74013432515579));
#203680=CARTESIAN_POINT('Ctrl Pts',(9.83220301527822,12.2,5.73966564202533));
#203681=CARTESIAN_POINT('Ctrl Pts',(9.82854888343602,12.2,5.73931412966153));
#203682=CARTESIAN_POINT('Ctrl Pts',(9.82490195449846,12.2,5.73895905544237));
#203683=CARTESIAN_POINT('Ctrl Pts',(9.82126225867174,12.2,5.73860044703904));
#203684=CARTESIAN_POINT('Ctrl Pts',(9.81762256284502,12.2,5.73824183863572));
#203685=CARTESIAN_POINT('Ctrl Pts',(9.8139901001428,12.2,5.73787969644929));
#203686=CARTESIAN_POINT('Ctrl Pts',(9.81036490085686,12.2,5.73751405008805));
#203687=CARTESIAN_POINT('Ctrl Pts',(9.80553130136988,12.2,5.73702652156212));
#203688=CARTESIAN_POINT('Ctrl Pts',(9.8007106147221,12.2,5.73653276425977));
#203689=CARTESIAN_POINT('Ctrl Pts',(9.79590291327162,12.2,5.736032847508));
#203690=CARTESIAN_POINT('Ctrl Pts',(9.79229713751129,12.2,5.73565790997824));
#203691=CARTESIAN_POINT('Ctrl Pts',(9.78869866678903,12.2,5.73527950700487));
#203692=CARTESIAN_POINT('Ctrl Pts',(9.78510753048649,12.2,5.73489767051702));
#203693=CARTESIAN_POINT('Ctrl Pts',(9.78151639418396,12.2,5.73451583402918));
#203694=CARTESIAN_POINT('Ctrl Pts',(9.77793259172721,12.2,5.73413056244457));
#203695=CARTESIAN_POINT('Ctrl Pts',(9.77435615635651,12.2,5.73374188700065));
#203696=CARTESIAN_POINT('Ctrl Pts',(9.76958757542909,12.2,5.73322365302836));
#203697=CARTESIAN_POINT('Ctrl Pts',(9.76483208820603,12.2,5.73269936653867));
#203698=CARTESIAN_POINT('Ctrl Pts',(9.76008976933733,12.2,5.7321691012316));
#203699=CARTESIAN_POINT('Ctrl Pts',(9.75653303050887,12.2,5.73177140228743));
#203700=CARTESIAN_POINT('Ctrl Pts',(9.75298369903787,12.2,5.73137033990198));
#203701=CARTESIAN_POINT('Ctrl Pts',(9.74944180429156,12.2,5.73096594450001));
#203702=CARTESIAN_POINT('Ctrl Pts',(9.74589990954524,12.2,5.73056154909804));
#203703=CARTESIAN_POINT('Ctrl Pts',(9.74236545327363,12.2,5.73015382072953));
#203704=CARTESIAN_POINT('Ctrl Pts',(9.73883846590113,12.2,5.72974279078642));
#203705=CARTESIAN_POINT('Ctrl Pts',(9.73531147852862,12.2,5.72933176084331));
#203706=CARTESIAN_POINT('Ctrl Pts',(9.7317919588615,12.2,5.72891742858608));
#203707=CARTESIAN_POINT('Ctrl Pts',(9.72827994022945,12.2,5.72849982708077));
#203708=CARTESIAN_POINT('Ctrl Pts',(9.7247679215974,12.2,5.72808222557546));
#203709=CARTESIAN_POINT('Ctrl Pts',(9.72126340065288,12.2,5.72766135347661));
#203710=CARTESIAN_POINT('Ctrl Pts',(9.71776641323724,12.2,5.72723724211746));
#203711=CARTESIAN_POINT('Ctrl Pts',(9.71426942518632,12.2,5.72681313068126));
#203712=CARTESIAN_POINT('Ctrl Pts',(9.71077996797918,12.2,5.72638578060249));
#203713=CARTESIAN_POINT('Ctrl Pts',(9.70729807351585,12.2,5.72595522362281));
#203714=CARTESIAN_POINT('Ctrl Pts',(9.70381617968505,12.2,5.72552466672135));
#203715=CARTESIAN_POINT('Ctrl Pts',(9.70034184842886,12.2,5.72509090262006));
#203716=CARTESIAN_POINT('Ctrl Pts',(9.69687511113881,12.2,5.72465396371899));
#203717=CARTESIAN_POINT('Ctrl Pts',(9.69225279496202,12.2,5.72407137854403));
#203718=CARTESIAN_POINT('Ctrl Pts',(9.68764397794407,12.2,5.72348314911955));
#203719=CARTESIAN_POINT('Ctrl Pts',(9.68304873686676,12.2,5.72288935186114));
#203720=CARTESIAN_POINT('Ctrl Pts',(9.67960230590225,12.2,5.7224440038971));
#203721=CARTESIAN_POINT('Ctrl Pts',(9.67616351202427,12.2,5.72199552279828));
#203722=CARTESIAN_POINT('Ctrl Pts',(9.67273238473122,12.2,5.72154394381512));
#203723=CARTESIAN_POINT('Ctrl Pts',(9.66930125681485,12.2,5.72109236474991));
#203724=CARTESIAN_POINT('Ctrl Pts',(9.66587779631731,12.2,5.72063768543383));
#203725=CARTESIAN_POINT('Ctrl Pts',(9.66246203628026,12.2,5.72017994090855));
#203726=CARTESIAN_POINT('Ctrl Pts',(9.65904627686376,12.2,5.71972219646643));
#203727=CARTESIAN_POINT('Ctrl Pts',(9.65563821543851,12.2,5.71926138599948));
#203728=CARTESIAN_POINT('Ctrl Pts',(9.65223788614605,12.2,5.7187975412244));
#203729=CARTESIAN_POINT('Ctrl Pts',(9.6488375568536,12.2,5.71833369644932));
#203730=CARTESIAN_POINT('Ctrl Pts',(9.64544495920584,12.2,5.71786681911798));
#203731=CARTESIAN_POINT('Ctrl Pts',(9.64206012398015,12.2,5.71739694221625));
#203732=CARTESIAN_POINT('Ctrl Pts',(9.63867528875446,12.2,5.71692706531451));
#203733=CARTESIAN_POINT('Ctrl Pts',(9.63529821729588,12.2,5.71645418761863));
#203734=CARTESIAN_POINT('Ctrl Pts',(9.63192894102795,12.2,5.71597834475877));
#203735=CARTESIAN_POINT('Ctrl Pts',(9.62855966476003,12.2,5.71550250189891));
#203736=CARTESIAN_POINT('Ctrl Pts',(9.6251981838444,12.2,5.71502369380138));
#203737=CARTESIAN_POINT('Ctrl Pts',(9.62184453009057,12.2,5.71454195252747));
#203738=CARTESIAN_POINT('Ctrl Pts',(9.61849087633673,12.2,5.71406021125356));
#203739=CARTESIAN_POINT('Ctrl Pts',(9.61514505005736,12.2,5.71357553850485));
#203740=CARTESIAN_POINT('Ctrl Pts',(9.61180708371924,12.2,5.71308796810629));
#203741=CARTESIAN_POINT('Ctrl Pts',(9.60735646153079,12.2,5.7124378741825));
#203742=CARTESIAN_POINT('Ctrl Pts',(9.60291981226906,12.2,5.71178262884134));
#203743=CARTESIAN_POINT('Ctrl Pts',(9.59849721223022,12.2,5.71112231252456));
#203744=CARTESIAN_POINT('Ctrl Pts',(9.59518026250237,12.2,5.71062707533195));
#203745=CARTESIAN_POINT('Ctrl Pts',(9.59187121578131,12.2,5.71012898773453));
#203746=CARTESIAN_POINT('Ctrl Pts',(9.58857010451123,12.2,5.70962808250046));
#203747=CARTESIAN_POINT('Ctrl Pts',(9.58416862241797,12.2,5.70896020879438));
#203748=CARTESIAN_POINT('Ctrl Pts',(9.57978124755788,12.2,5.70828732780163));
#203749=CARTESIAN_POINT('Ctrl Pts',(9.57540805804321,12.2,5.70760952259752));
#203750=CARTESIAN_POINT('Ctrl Pts',(9.57103486912439,12.2,5.70693171748576));
#203751=CARTESIAN_POINT('Ctrl Pts',(9.56667586506485,12.2,5.70624898797464));
#203752=CARTESIAN_POINT('Ctrl Pts',(9.56233112236354,12.2,5.70556141953117));
#203753=CARTESIAN_POINT('Ctrl Pts',(9.55798637907026,12.2,5.70487385099401));
#203754=CARTESIAN_POINT('Ctrl Pts',(9.55365589875662,12.2,5.70418144173039));
#203755=CARTESIAN_POINT('Ctrl Pts',(9.54933975964033,12.2,5.70348427915715));
#203756=CARTESIAN_POINT('Ctrl Pts',(9.54502362111214,12.2,5.70278711667889));
#203757=CARTESIAN_POINT('Ctrl Pts',(9.54072182159263,12.2,5.70208519899132));
#203758=CARTESIAN_POINT('Ctrl Pts',(9.53643444210885,12.2,5.70137861454939));
#203759=CARTESIAN_POINT('Ctrl Pts',(9.53107521731601,12.2,5.70049538392476));
#203760=CARTESIAN_POINT('Ctrl Pts',(9.52573852258208,12.2,5.69960485878607));
#203761=CARTESIAN_POINT('Ctrl Pts',(9.52042451112256,12.2,5.69870721080033));
#203762=CARTESIAN_POINT('Ctrl Pts',(9.51617330172327,12.2,5.69798909237261));
#203763=CARTESIAN_POINT('Ctrl Pts',(9.51193660998819,12.2,5.69726641640414));
#203764=CARTESIAN_POINT('Ctrl Pts',(9.50771451443732,12.2,5.69653926866113));
#203765=CARTESIAN_POINT('Ctrl Pts',(9.5034924194617,12.2,5.6958121210172));
#203766=CARTESIAN_POINT('Ctrl Pts',(9.49928492198987,12.2,5.6950805036469));
#203767=CARTESIAN_POINT('Ctrl Pts',(9.49509210110946,12.2,5.69434450531846));
#203768=CARTESIAN_POINT('Ctrl Pts',(9.49089927965777,12.2,5.69360850688974));
#203769=CARTESIAN_POINT('Ctrl Pts',(9.48672113442726,12.2,5.69286812822716));
#203770=CARTESIAN_POINT('Ctrl Pts',(9.48255774570133,12.2,5.69212345913075));
#203771=CARTESIAN_POINT('Ctrl Pts',(9.47839435754265,12.2,5.69137879013579));
#203772=CARTESIAN_POINT('Ctrl Pts',(9.47424572562801,12.2,5.69062983073218));
#203773=CARTESIAN_POINT('Ctrl Pts',(9.47011193059148,12.2,5.6898766723676));
#203774=CARTESIAN_POINT('Ctrl Pts',(9.46597813499171,12.2,5.6891235139004));
#203775=CARTESIAN_POINT('Ctrl Pts',(9.46185917683167,12.2,5.68836615697948));
#203776=CARTESIAN_POINT('Ctrl Pts',(9.45775513616452,12.2,5.68760469393771));
#203777=CARTESIAN_POINT('Ctrl Pts',(9.45365109605656,12.2,5.6868432309997));
#203778=CARTESIAN_POINT('Ctrl Pts',(9.44956197340949,12.2,5.68607766065973));
#203779=CARTESIAN_POINT('Ctrl Pts',(9.44548784990768,12.2,5.68530807833416));
#203780=CARTESIAN_POINT('Ctrl Pts',(9.44141372585077,12.2,5.68453849590374));
#203781=CARTESIAN_POINT('Ctrl Pts',(9.4373546011664,12.2,5.6837649017315));
#203782=CARTESIAN_POINT('Ctrl Pts',(9.4333105565388,12.2,5.68298738874114));
#203783=CARTESIAN_POINT('Ctrl Pts',(9.4282555010298,12.2,5.68201549755615));
#203784=CARTESIAN_POINT('Ctrl Pts',(9.4232240085935,12.2,5.68103748499148));
#203785=CARTESIAN_POINT('Ctrl Pts',(9.41821624116419,12.2,5.68005353714395));
#203786=CARTESIAN_POINT('Ctrl Pts',(9.41421002754824,12.2,5.67926637893027));
#203787=CARTESIAN_POINT('Ctrl Pts',(9.41021899705703,12.2,5.67847542268402));
#203788=CARTESIAN_POINT('Ctrl Pts',(9.40624323165826,12.2,5.67768076513826));
#203789=CARTESIAN_POINT('Ctrl Pts',(9.4022674657178,12.2,5.67688610748422));
#203790=CARTESIAN_POINT('Ctrl Pts',(9.39830696647322,12.2,5.6760877487437));
#203791=CARTESIAN_POINT('Ctrl Pts',(9.39436181575821,12.2,5.6752857877));
#203792=CARTESIAN_POINT('Ctrl Pts',(9.3904166650432,12.2,5.6744838266563));
#203793=CARTESIAN_POINT('Ctrl Pts',(9.38648686298276,12.2,5.67367826286216));
#203794=CARTESIAN_POINT('Ctrl Pts',(9.38257249365989,12.2,5.67286919515105));
#203795=CARTESIAN_POINT('Ctrl Pts',(9.37572234814487,12.2,5.67145332682194));
#203796=CARTESIAN_POINT('Ctrl Pts',(9.36891946199662,12.2,5.6700267271161));
#203797=CARTESIAN_POINT('Ctrl Pts',(9.36216429004059,12.2,5.66858994152542));
#203798=CARTESIAN_POINT('Ctrl Pts',(9.3583041913292,12.2,5.667768921092));
#203799=CARTESIAN_POINT('Ctrl Pts',(9.35445967150579,12.2,5.66694457273319));
#203800=CARTESIAN_POINT('Ctrl Pts',(9.35063081618702,12.2,5.66611700046565));
#203801=CARTESIAN_POINT('Ctrl Pts',(9.34680196138996,12.2,5.66528942831087));
#203802=CARTESIAN_POINT('Ctrl Pts',(9.34298877087331,12.2,5.66445863320254));
#203803=CARTESIAN_POINT('Ctrl Pts',(9.339191329826,12.2,5.66362471639599));
#203804=CARTESIAN_POINT('Ctrl Pts',(9.3353938882613,12.2,5.66279079947581));
#203805=CARTESIAN_POINT('Ctrl Pts',(9.33161219490472,12.2,5.66195376284672));
#203806=CARTESIAN_POINT('Ctrl Pts',(9.32784633820051,12.2,5.66111371118963));
#203807=CARTESIAN_POINT('Ctrl Pts',(9.32408048200939,12.2,5.660273659647));
#203808=CARTESIAN_POINT('Ctrl Pts',(9.32033046026789,12.2,5.65943059232441));
#203809=CARTESIAN_POINT('Ctrl Pts',(9.31659636012708,12.2,5.65858461617164));
#203810=CARTESIAN_POINT('Ctrl Pts',(9.3128622594775,12.2,5.65773863990361));
#203811=CARTESIAN_POINT('Ctrl Pts',(9.30914408084367,12.2,5.65688975419971));
#203812=CARTESIAN_POINT('Ctrl Pts',(9.30544190951403,12.2,5.65603806848275));
#203813=CARTESIAN_POINT('Ctrl Pts',(9.30173973868881,12.2,5.65518638288183));
#203814=CARTESIAN_POINT('Ctrl Pts',(9.298053574846,12.2,5.65433189435868));
#203815=CARTESIAN_POINT('Ctrl Pts',(9.29438350736661,12.2,5.65347471487348));
#203816=CARTESIAN_POINT('Ctrl Pts',(9.29071343938716,12.2,5.65261753527149));
#203817=CARTESIAN_POINT('Ctrl Pts',(9.28705946671757,12.2,5.65175766253311));
#203818=CARTESIAN_POINT('Ctrl Pts',(9.28342167624154,12.2,5.65089520820833));
#203819=CARTESIAN_POINT('Ctrl Pts',(9.27978388576551,12.2,5.65003275388355));
#203820=CARTESIAN_POINT('Ctrl Pts',(9.27616227909968,12.2,5.64916771632514));
#203821=CARTESIAN_POINT('Ctrl Pts',(9.27255694312709,12.2,5.64830020933315));
#203822=CARTESIAN_POINT('Ctrl Pts',(9.26895160764571,12.2,5.64743270245938));
#203823=CARTESIAN_POINT('Ctrl Pts',(9.26536254347652,12.2,5.64656272414433));
#203824=CARTESIAN_POINT('Ctrl Pts',(9.26178983875232,12.2,5.64569038876726));
#203825=CARTESIAN_POINT('Ctrl Pts',(9.25821713354134,12.2,5.64481805327132));
#203826=CARTESIAN_POINT('Ctrl Pts',(9.25466078857625,12.2,5.64394335914075));
#203827=CARTESIAN_POINT('Ctrl Pts',(9.25112089266278,12.2,5.64306642281494));
#203828=CARTESIAN_POINT('Ctrl Pts',(9.24758099723162,12.2,5.64218948660863));
#203829=CARTESIAN_POINT('Ctrl Pts',(9.24405755161222,12.2,5.64131030594984));
#203830=CARTESIAN_POINT('Ctrl Pts',(9.24055064478673,12.2,5.64042899802202));
#203831=CARTESIAN_POINT('Ctrl Pts',(9.23704373748341,12.2,5.63954768997413));
#203832=CARTESIAN_POINT('Ctrl Pts',(9.2335533684712,12.2,5.63866425569749));
#203833=CARTESIAN_POINT('Ctrl Pts',(9.2300796297209,12.2,5.63777880960483));
#203834=CARTESIAN_POINT('Ctrl Pts',(9.22660589144391,12.2,5.63689336363281));
#203835=CARTESIAN_POINT('Ctrl Pts',(9.22314878251223,12.2,5.63600590858041));
#203836=CARTESIAN_POINT('Ctrl Pts',(9.21970839501462,12.2,5.63511656059768));
#203837=CARTESIAN_POINT('Ctrl Pts',(9.21626800704825,12.2,5.63422721249378));
#203838=CARTESIAN_POINT('Ctrl Pts',(9.21284433903388,12.2,5.63333597352575));
#203839=CARTESIAN_POINT('Ctrl Pts',(9.2094374837382,12.2,5.63244296214364));
#203840=CARTESIAN_POINT('Ctrl Pts',(9.20603062890669,12.2,5.6315499508832));
#203841=CARTESIAN_POINT('Ctrl Pts',(9.20264058651422,12.2,5.63065516924586));
#203842=CARTESIAN_POINT('Ctrl Pts',(9.1992674482311,12.2,5.6297587371634));
#203843=CARTESIAN_POINT('Ctrl Pts',(9.19589430948839,12.2,5.62886230495879));
#203844=CARTESIAN_POINT('Ctrl Pts',(9.19253807474126,12.2,5.627964222245));
#203845=CARTESIAN_POINT('Ctrl Pts',(9.18919883822704,12.2,5.6270646129181));
#203846=CARTESIAN_POINT('Ctrl Pts',(9.1858596021678,12.2,5.62616500371376));
#203847=CARTESIAN_POINT('Ctrl Pts',(9.18253736329961,12.2,5.62526386897085));
#203848=CARTESIAN_POINT('Ctrl Pts',(9.17923221579028,12.2,5.62436133165589));
#203849=CARTESIAN_POINT('Ctrl Pts',(9.17592706783062,12.2,5.62345879421795));
#203850=CARTESIAN_POINT('Ctrl Pts',(9.17263901013793,12.2,5.62255485438337));
#203851=CARTESIAN_POINT('Ctrl Pts',(9.16936813822266,12.2,5.62164964027437));
#203852=CARTESIAN_POINT('Ctrl Pts',(9.16609726675304,12.2,5.62074442628871));
#203853=CARTESIAN_POINT('Ctrl Pts',(9.16284357892735,12.2,5.6198379364574));
#203854=CARTESIAN_POINT('Ctrl Pts',(9.15960717274571,12.2,5.61893029986506));
#203855=CARTESIAN_POINT('Ctrl Pts',(9.15637076612311,12.2,5.61802266314904));
#203856=CARTESIAN_POINT('Ctrl Pts',(9.15315163805771,12.2,5.6171138789468));
#203857=CARTESIAN_POINT('Ctrl Pts',(9.14994988621654,12.2,5.61620407750832));
#203858=CARTESIAN_POINT('Ctrl Pts',(9.14594769663319,12.2,5.61506682577221));
#203859=CARTESIAN_POINT('Ctrl Pts',(9.14197265678225,12.2,5.61392798380454));
#203860=CARTESIAN_POINT('Ctrl Pts',(9.1380249530144,12.2,5.6127878090077));
#203861=CARTESIAN_POINT('Ctrl Pts',(9.13407724924654,12.2,5.61164763421084));
#203862=CARTESIAN_POINT('Ctrl Pts',(9.13015688206068,12.2,5.61050612765309));
#203863=CARTESIAN_POINT('Ctrl Pts',(9.12626404247878,12.2,5.60936354945859));
#203864=CARTESIAN_POINT('Ctrl Pts',(9.1223712028969,12.2,5.60822097126409));
#203865=CARTESIAN_POINT('Ctrl Pts',(9.11850589013095,12.2,5.60707732170295));
#203866=CARTESIAN_POINT('Ctrl Pts',(9.11466829554906,12.2,5.60593286767514));
#203867=CARTESIAN_POINT('Ctrl Pts',(9.11083070096718,12.2,5.60478841364731));
#203868=CARTESIAN_POINT('Ctrl Pts',(9.10702082514568,12.2,5.60364315416952));
#203869=CARTESIAN_POINT('Ctrl Pts',(9.10323886049437,12.2,5.60249736014171));
#203870=CARTESIAN_POINT('Ctrl Pts',(9.09945689584305,12.2,5.60135156611392));
#203871=CARTESIAN_POINT('Ctrl Pts',(9.09570284265165,12.2,5.60020523661863));
#203872=CARTESIAN_POINT('Ctrl Pts',(9.09197689705078,12.2,5.59905864836688));
#203873=CARTESIAN_POINT('Ctrl Pts',(9.08825095144993,12.2,5.59791206011514));
#203874=CARTESIAN_POINT('Ctrl Pts',(9.08455311190092,12.2,5.59676521199998));
#203875=CARTESIAN_POINT('Ctrl Pts',(9.08088357731991,12.2,5.59561838387498));
#203876=CARTESIAN_POINT('Ctrl Pts',(9.07721404273889,12.2,5.59447155574998));
#203877=CARTESIAN_POINT('Ctrl Pts',(9.07357281155278,12.2,5.59332474893888));
#203878=CARTESIAN_POINT('Ctrl Pts',(9.06996008377734,12.2,5.59217824588336));
#203879=CARTESIAN_POINT('Ctrl Pts',(9.06634735639569,12.2,5.5910317429528));
#203880=CARTESIAN_POINT('Ctrl Pts',(9.06276313291307,12.2,5.5898855446639));
#203881=CARTESIAN_POINT('Ctrl Pts',(9.05920761371494,12.2,5.58873994089983));
#203882=CARTESIAN_POINT('Ctrl Pts',(9.05565209412926,12.2,5.58759433701089));
#203883=CARTESIAN_POINT('Ctrl Pts',(9.05212527844311,12.2,5.58644932835526));
#203884=CARTESIAN_POINT('Ctrl Pts',(9.04862737073241,12.2,5.58530520863297));
#203885=CARTESIAN_POINT('Ctrl Pts',(9.04512946302171,12.2,5.58416108891067));
#203886=CARTESIAN_POINT('Ctrl Pts',(9.04166046351206,12.2,5.5830178590008));
#203887=CARTESIAN_POINT('Ctrl Pts',(9.03822057715763,12.2,5.58187581762423));
#203888=CARTESIAN_POINT('Ctrl Pts',(9.03478069080321,12.2,5.58073377624764));
#203889=CARTESIAN_POINT('Ctrl Pts',(9.03136991818942,12.2,5.57959292436904));
#203890=CARTESIAN_POINT('Ctrl Pts',(9.02798846547953,12.2,5.57845356804951));
#203891=CARTESIAN_POINT('Ctrl Pts',(9.02460701276966,12.2,5.57731421172998));
#203892=CARTESIAN_POINT('Ctrl Pts',(9.02125488303,12.2,5.5761763502966));
#203893=CARTESIAN_POINT('Ctrl Pts',(9.01793228275068,12.2,5.57504029411596));
#203894=CARTESIAN_POINT('Ctrl Pts',(9.01460968247136,12.2,5.57390423793531));
#203895=CARTESIAN_POINT('Ctrl Pts',(9.01131661419989,12.2,5.57276998773909));
#203896=CARTESIAN_POINT('Ctrl Pts',(9.00805328751832,12.2,5.57163786148393));
#203897=CARTESIAN_POINT('Ctrl Pts',(9.00478996083673,12.2,5.57050573522879));
#203898=CARTESIAN_POINT('Ctrl Pts',(9.00155638011096,12.2,5.56937572988331));
#203899=CARTESIAN_POINT('Ctrl Pts',(8.99835275649986,12.2,5.56824817196664));
#203900=CARTESIAN_POINT('Ctrl Pts',(8.99514913288876,12.2,5.56712061404998));
#203901=CARTESIAN_POINT('Ctrl Pts',(8.99197546674013,12.2,5.56599550044891));
#203902=CARTESIAN_POINT('Ctrl Pts',(8.98883197728149,12.2,5.5648731618327));
#203903=CARTESIAN_POINT('Ctrl Pts',(8.98505979006818,12.2,5.56352635554219));
#203904=CARTESIAN_POINT('Ctrl Pts',(8.98133105502724,12.2,5.5621835438745));
#203905=CARTESIAN_POINT('Ctrl Pts',(8.97764615390921,12.2,5.5608453065896));
#203906=CARTESIAN_POINT('Ctrl Pts',(8.97396125245647,12.2,5.55950706918311));
#203907=CARTESIAN_POINT('Ctrl Pts',(8.97032018441751,12.2,5.55817340797722));
#203908=CARTESIAN_POINT('Ctrl Pts',(8.96672333689116,12.2,5.55684491290517));
#203909=CARTESIAN_POINT('Ctrl Pts',(8.96312648969154,12.2,5.5555164179538));
#203910=CARTESIAN_POINT('Ctrl Pts',(8.95957386137946,12.2,5.55419309196341));
#203911=CARTESIAN_POINT('Ctrl Pts',(8.9560658453422,12.2,5.5528755416782));
#203912=CARTESIAN_POINT('Ctrl Pts',(8.95255782930494,12.2,5.55155799139299));
#203913=CARTESIAN_POINT('Ctrl Pts',(8.94909442563911,12.2,5.55024621683233));
#203914=CARTESIAN_POINT('Ctrl Pts',(8.94567603167802,12.2,5.54894083879614));
#203915=CARTESIAN_POINT('Ctrl Pts',(8.94225763771692,12.2,5.54763546075995));
#203916=CARTESIAN_POINT('Ctrl Pts',(8.93888425458646,12.2,5.546336481111));
#203917=CARTESIAN_POINT('Ctrl Pts',(8.93555628562096,12.2,5.54504453415747));
#203918=CARTESIAN_POINT('Ctrl Pts',(8.93222831635318,12.2,5.54375258708658));
#203919=CARTESIAN_POINT('Ctrl Pts',(8.92894576262307,12.2,5.54246767517467));
#203920=CARTESIAN_POINT('Ctrl Pts',(8.92570903353199,12.2,5.54119044918873));
#203921=CARTESIAN_POINT('Ctrl Pts',(8.92247230473491,12.2,5.5399132233188));
#203922=CARTESIAN_POINT('Ctrl Pts',(8.91928140288474,12.2,5.53864368333546));
#203923=CARTESIAN_POINT('Ctrl Pts',(8.91613674498463,12.2,5.53738249845888));
#203924=CARTESIAN_POINT('Ctrl Pts',(8.91299208708452,12.2,5.53612131358229));
#203925=CARTESIAN_POINT('Ctrl Pts',(8.9098936718165,12.2,5.53486848372431));
#203926=CARTESIAN_POINT('Ctrl Pts',(8.90684192784084,12.2,5.53362469310221));
#203927=CARTESIAN_POINT('Ctrl Pts',(8.90379018358799,12.2,5.53238090236713));
#203928=CARTESIAN_POINT('Ctrl Pts',(8.90078510847299,12.2,5.53114615289958));
#203929=CARTESIAN_POINT('Ctrl Pts',(8.89782713356385,12.2,5.52992114516658));
#203930=CARTESIAN_POINT('Ctrl Pts',(8.89486915892338,12.2,5.52869613754485));
#203931=CARTESIAN_POINT('Ctrl Pts',(8.89195828905192,12.2,5.5274808726289));
#203932=CARTESIAN_POINT('Ctrl Pts',(8.88909496022617,12.2,5.52627607200052));
#203933=CARTESIAN_POINT('Ctrl Pts',(8.88623163140042,12.2,5.52507127137212));
#203934=CARTESIAN_POINT('Ctrl Pts',(8.8834158451876,12.2,5.52387693257005));
#203935=CARTESIAN_POINT('Ctrl Pts',(8.8806480512849,12.2,5.52269379811226));
#203936=CARTESIAN_POINT('Ctrl Pts',(8.87788025713077,12.2,5.52151066354701));
#203937=CARTESIAN_POINT('Ctrl Pts',(8.8751604548178,12.2,5.52033873193327));
#203938=CARTESIAN_POINT('Ctrl Pts',(8.87248910070822,12.2,5.51917876339611));
#203939=CARTESIAN_POINT('Ctrl Pts',(8.8698177468413,12.2,5.51801879496433));
#203940=CARTESIAN_POINT('Ctrl Pts',(8.86719484163134,12.2,5.51687078998372));
#203941=CARTESIAN_POINT('Ctrl Pts',(8.86462085280818,12.2,5.51573552677496));
#203942=CARTESIAN_POINT('Ctrl Pts',(8.86204686398504,12.2,5.51460026356621));
#203943=CARTESIAN_POINT('Ctrl Pts',(8.85952178980104,12.2,5.51347774477317));
#203944=CARTESIAN_POINT('Ctrl Pts',(8.85704610701447,12.2,5.51236876859061));
#203945=CARTESIAN_POINT('Ctrl Pts',(8.85457042400302,12.2,5.51125979230731));
#203946=CARTESIAN_POINT('Ctrl Pts',(8.85214413080862,12.2,5.51016436125673));
#203947=CARTESIAN_POINT('Ctrl Pts',(8.84976771676584,12.2,5.5090832981988));
#203948=CARTESIAN_POINT('Ctrl Pts',(8.84699523403973,12.2,5.50782205811184));
#203949=CARTESIAN_POINT('Ctrl Pts',(8.84429063614501,12.2,5.5065803740872));
#203950=CARTESIAN_POINT('Ctrl Pts',(8.84165471549355,12.2,5.50535959510122));
#203951=CARTESIAN_POINT('Ctrl Pts',(8.8393953546713,12.2,5.50431321299104));
#203952=CARTESIAN_POINT('Ctrl Pts',(8.83718645180378,12.2,5.50328218934354));
#203953=CARTESIAN_POINT('Ctrl Pts',(8.83502851227299,12.2,5.50226740062268));
#203954=CARTESIAN_POINT('Ctrl Pts',(8.83251091644776,12.2,5.50108348058661));
#203955=CARTESIAN_POINT('Ctrl Pts',(8.83006269125468,12.2,5.49992165815931));
#203956=CARTESIAN_POINT('Ctrl Pts',(8.82768466119716,12.2,5.49878336960271));
#203957=CARTESIAN_POINT('Ctrl Pts',(8.82564634948126,12.2,5.49780769358313));
#203958=CARTESIAN_POINT('Ctrl Pts',(8.82365961233255,12.2,5.49684930573914));
#203959=CARTESIAN_POINT('Ctrl Pts',(8.82172498081399,12.2,5.49590914393915));
#203960=CARTESIAN_POINT('Ctrl Pts',(8.81946791097259,12.2,5.49481228863392));
#203961=CARTESIAN_POINT('Ctrl Pts',(8.81728176748612,12.2,5.49374023430846));
#203962=CARTESIAN_POINT('Ctrl Pts',(8.8151674169253,12.2,5.49269451657004));
#203963=CARTESIAN_POINT('Ctrl Pts',(8.81335511623294,12.2,5.49179818697529));
#203964=CARTESIAN_POINT('Ctrl Pts',(8.81159556159492,12.2,5.49092120774354));
#203965=CARTESIAN_POINT('Ctrl Pts',(8.80988931908888,12.2,5.49006457444825));
#203966=CARTESIAN_POINT('Ctrl Pts',(8.8081912654558,12.2,5.48921205244499));
#203967=CARTESIAN_POINT('Ctrl Pts',(8.80654600943141,12.2,5.48837967859438));
#203968=CARTESIAN_POINT('Ctrl Pts',(8.80495412799995,12.2,5.48756847999999));
#203969=CARTESIAN_POINT('Ctrl Pts',(8.80495412799995,15.2,5.48756847999999));
#203970=CARTESIAN_POINT('Ctrl Pts',(8.80654600943141,15.2,5.48837967859438));
#203971=CARTESIAN_POINT('Ctrl Pts',(8.8081912654558,15.2,5.48921205244499));
#203972=CARTESIAN_POINT('Ctrl Pts',(8.80988931908889,15.2,5.49006457444825));
#203973=CARTESIAN_POINT('Ctrl Pts',(8.81159556159492,15.2,5.49092120774355));
#203974=CARTESIAN_POINT('Ctrl Pts',(8.81335511623294,15.2,5.49179818697529));
#203975=CARTESIAN_POINT('Ctrl Pts',(8.8151674169253,15.2,5.49269451657004));
#203976=CARTESIAN_POINT('Ctrl Pts',(8.81697971745304,15.2,5.49359084608338));
#203977=CARTESIAN_POINT('Ctrl Pts',(8.81884476396952,15.2,5.4945065246089));
#203978=CARTESIAN_POINT('Ctrl Pts',(8.82076201023318,15.2,5.49544058599162));
#203979=CARTESIAN_POINT('Ctrl Pts',(8.82267925649684,15.2,5.49637464737434));
#203980=CARTESIAN_POINT('Ctrl Pts',(8.82464870084658,15.2,5.4973270899023));
#203981=CARTESIAN_POINT('Ctrl Pts',(8.8266698055378,15.2,5.49829697666451));
#203982=CARTESIAN_POINT('Ctrl Pts',(8.8286909104126,15.2,5.49926686351481));
#203983=CARTESIAN_POINT('Ctrl Pts',(8.8307636779788,15.2,5.5002541958202));
#203984=CARTESIAN_POINT('Ctrl Pts',(8.83288758176471,15.2,5.50125805887605));
#203985=CARTESIAN_POINT('Ctrl Pts',(8.83501148535769,15.2,5.5022619218407));
#203986=CARTESIAN_POINT('Ctrl Pts',(8.83718652736316,15.2,5.50328231912499));
#203987=CARTESIAN_POINT('Ctrl Pts',(8.83941219304253,15.2,5.50431836500876));
#203988=CARTESIAN_POINT('Ctrl Pts',(8.84200880313657,15.2,5.50552708526924));
#203989=CARTESIAN_POINT('Ctrl Pts',(8.84467431955873,15.2,5.50675710279612));
#203990=CARTESIAN_POINT('Ctrl Pts',(8.84740794648027,15.2,5.50800705694175));
#203991=CARTESIAN_POINT('Ctrl Pts',(8.84975105514856,15.2,5.50907844615382));
#203992=CARTESIAN_POINT('Ctrl Pts',(8.85214420385351,15.2,5.5101644837604));
#203993=CARTESIAN_POINT('Ctrl Pts',(8.85458690552597,15.2,5.51126433797546));
#203994=CARTESIAN_POINT('Ctrl Pts',(8.85702960719842,15.2,5.51236419219053));
#203995=CARTESIAN_POINT('Ctrl Pts',(8.85952186056438,15.2,5.51347786371345));
#203996=CARTESIAN_POINT('Ctrl Pts',(8.86206318638656,15.2,5.51460454117194));
#203997=CARTESIAN_POINT('Ctrl Pts',(8.86460451243961,15.2,5.51573121873278));
#203998=CARTESIAN_POINT('Ctrl Pts',(8.86719491163205,15.2,5.51687090567025));
#203999=CARTESIAN_POINT('Ctrl Pts',(8.86983391452919,15.2,5.51802281215052));
#204000=CARTESIAN_POINT('Ctrl Pts',(8.87247291718662,15.2,5.51917471852617));
#204001=CARTESIAN_POINT('Ctrl Pts',(8.8751605231798,15.2,5.52033884494797));
#204002=CARTESIAN_POINT('Ctrl Pts',(8.87789627191583,15.2,5.52151442632241));
#204003=CARTESIAN_POINT('Ctrl Pts',(8.88063202065186,15.2,5.52269000769687));
#204004=CARTESIAN_POINT('Ctrl Pts',(8.88341591327567,15.2,5.52387704158704));
#204005=CARTESIAN_POINT('Ctrl Pts',(8.88624749608741,15.2,5.52507478595973));
#204006=CARTESIAN_POINT('Ctrl Pts',(8.88907907889914,15.2,5.52627253033242));
#204007=CARTESIAN_POINT('Ctrl Pts',(8.8919583536321,15.2,5.52748098092045));
#204008=CARTESIAN_POINT('Ctrl Pts',(8.89488487643921,15.2,5.52869941262549));
#204009=CARTESIAN_POINT('Ctrl Pts',(8.89781139951215,15.2,5.52991784444121));
#204010=CARTESIAN_POINT('Ctrl Pts',(8.90078517149801,15.2,5.53114625669128));
#204011=CARTESIAN_POINT('Ctrl Pts',(8.90380575566468,15.2,5.53238394234246));
#204012=CARTESIAN_POINT('Ctrl Pts',(8.9073297703886,15.2,5.5338279088793));
#204013=CARTESIAN_POINT('Ctrl Pts',(8.91091750233601,15.2,5.53528449469138));
#204014=CARTESIAN_POINT('Ctrl Pts',(8.91456827209096,15.2,5.53675260568714));
#204015=CARTESIAN_POINT('Ctrl Pts',(8.91769750314708,15.2,5.53801098647532));
#204016=CARTESIAN_POINT('Ctrl Pts',(8.920873049299,15.2,5.53927783519046));
#204017=CARTESIAN_POINT('Ctrl Pts',(8.92409449043396,15.2,5.54055248006114));
#204018=CARTESIAN_POINT('Ctrl Pts',(8.92731593156891,15.2,5.54182712493184));
#204019=CARTESIAN_POINT('Ctrl Pts',(8.93058326800852,15.2,5.54310956580188));
#204020=CARTESIAN_POINT('Ctrl Pts',(8.93389608705284,15.2,5.54439914967139));
#204021=CARTESIAN_POINT('Ctrl Pts',(8.93720890609717,15.2,5.54568873354089));
#204022=CARTESIAN_POINT('Ctrl Pts',(8.94056720783897,15.2,5.54698545768905));
#204023=CARTESIAN_POINT('Ctrl Pts',(8.94397058687891,15.2,5.54828868564126));
#204024=CARTESIAN_POINT('Ctrl Pts',(8.94737396622797,15.2,5.54959191371184));
#204025=CARTESIAN_POINT('Ctrl Pts',(8.95082242182309,15.2,5.55090164269141));
#204026=CARTESIAN_POINT('Ctrl Pts',(8.9543155569321,15.2,5.5522172508467));
#204027=CARTESIAN_POINT('Ctrl Pts',(8.95839088074999,15.2,5.55375212684862));
#204028=CARTESIAN_POINT('Ctrl Pts',(8.96252701526716,15.2,5.5552950021688));
#204029=CARTESIAN_POINT('Ctrl Pts',(8.96672333689116,15.2,5.55684491290517));
#204030=CARTESIAN_POINT('Ctrl Pts',(8.97032018441752,15.2,5.55817340797722));
#204031=CARTESIAN_POINT('Ctrl Pts',(8.97396125245646,15.2,5.5595070691831));
#204032=CARTESIAN_POINT('Ctrl Pts',(8.97764615390921,15.2,5.5608453065896));
#204033=CARTESIAN_POINT('Ctrl Pts',(8.98133105502726,15.2,5.56218354387451));
#204034=CARTESIAN_POINT('Ctrl Pts',(8.98505979006818,15.2,5.56352635554219));
#204035=CARTESIAN_POINT('Ctrl Pts',(8.98883197728149,15.2,5.5648731618327));
#204036=CARTESIAN_POINT('Ctrl Pts',(8.99197546674013,15.2,5.56599550044891));
#204037=CARTESIAN_POINT('Ctrl Pts',(8.99514913288874,15.2,5.56712061404997));
#204038=CARTESIAN_POINT('Ctrl Pts',(8.99835275649986,15.2,5.56824817196664));
#204039=CARTESIAN_POINT('Ctrl Pts',(9.00155638011097,15.2,5.56937572988331));
#204040=CARTESIAN_POINT('Ctrl Pts',(9.00478996083675,15.2,5.57050573522879));
#204041=CARTESIAN_POINT('Ctrl Pts',(9.00805328751832,15.2,5.57163786148393));
#204042=CARTESIAN_POINT('Ctrl Pts',(9.01131661419988,15.2,5.57276998773908));
#204043=CARTESIAN_POINT('Ctrl Pts',(9.01460968247137,15.2,5.57390423793531));
#204044=CARTESIAN_POINT('Ctrl Pts',(9.01793228275068,15.2,5.57504029411595));
#204045=CARTESIAN_POINT('Ctrl Pts',(9.02125488302999,15.2,5.5761763502966));
#204046=CARTESIAN_POINT('Ctrl Pts',(9.02460701276966,15.2,5.57731421172998));
#204047=CARTESIAN_POINT('Ctrl Pts',(9.02798846547952,15.2,5.57845356804951));
#204048=CARTESIAN_POINT('Ctrl Pts',(9.0313699181894,15.2,5.57959292436903));
#204049=CARTESIAN_POINT('Ctrl Pts',(9.0347806908032,15.2,5.58073377624764));
#204050=CARTESIAN_POINT('Ctrl Pts',(9.03822057715763,15.2,5.58187581762423));
#204051=CARTESIAN_POINT('Ctrl Pts',(9.04166046351206,15.2,5.5830178590008));
#204052=CARTESIAN_POINT('Ctrl Pts',(9.04512946302171,15.2,5.58416108891067));
#204053=CARTESIAN_POINT('Ctrl Pts',(9.04862737073241,15.2,5.58530520863297));
#204054=CARTESIAN_POINT('Ctrl Pts',(9.05212527844311,15.2,5.58644932835527));
#204055=CARTESIAN_POINT('Ctrl Pts',(9.05565209412926,15.2,5.58759433701089));
#204056=CARTESIAN_POINT('Ctrl Pts',(9.05920761371494,15.2,5.58873994089983));
#204057=CARTESIAN_POINT('Ctrl Pts',(9.06347423706274,15.2,5.59011466551661));
#204058=CARTESIAN_POINT('Ctrl Pts',(9.06778219480995,15.2,5.59149024634994));
#204059=CARTESIAN_POINT('Ctrl Pts',(9.07213113998706,15.2,5.59286618204997));
#204060=CARTESIAN_POINT('Ctrl Pts',(9.07575526109965,15.2,5.59401279517499));
#204061=CARTESIAN_POINT('Ctrl Pts',(9.07940784546153,15.2,5.59515965619721));
#204062=CARTESIAN_POINT('Ctrl Pts',(9.08308869344911,15.2,5.59630648105832));
#204063=CARTESIAN_POINT('Ctrl Pts',(9.08676954143669,15.2,5.59745330591943));
#204064=CARTESIAN_POINT('Ctrl Pts',(9.09047865590627,15.2,5.59860009435916));
#204065=CARTESIAN_POINT('Ctrl Pts',(9.09421583644214,15.2,5.59974656837474));
#204066=CARTESIAN_POINT('Ctrl Pts',(9.09795301697802,15.2,5.60089304239033));
#204067=CARTESIAN_POINT('Ctrl Pts',(9.10171826603263,15.2,5.6020392008832));
#204068=CARTESIAN_POINT('Ctrl Pts',(9.10551138797936,15.2,5.60318477067482));
#204069=CARTESIAN_POINT('Ctrl Pts',(9.10930450992608,15.2,5.60433034046644));
#204070=CARTESIAN_POINT('Ctrl Pts',(9.11312550317881,15.2,5.60547532006082));
#204071=CARTESIAN_POINT('Ctrl Pts',(9.11697417769496,15.2,5.60661944165797));
#204072=CARTESIAN_POINT('Ctrl Pts',(9.12159258694654,15.2,5.60799238752467));
#204073=CARTESIAN_POINT('Ctrl Pts',(9.12625085457627,15.2,5.60936409678583));
#204074=CARTESIAN_POINT('Ctrl Pts',(9.13094865101035,15.2,5.61073411249228));
#204075=CARTESIAN_POINT('Ctrl Pts',(9.13486348151431,15.2,5.61187579228913));
#204076=CARTESIAN_POINT('Ctrl Pts',(9.13880576409157,15.2,5.61301629533011));
#204077=CARTESIAN_POINT('Ctrl Pts',(9.14277530700965,15.2,5.61415536206614));
#204078=CARTESIAN_POINT('Ctrl Pts',(9.14674484992774,15.2,5.61529442880218));
#204079=CARTESIAN_POINT('Ctrl Pts',(9.15074165445623,15.2,5.61643206071325));
#204080=CARTESIAN_POINT('Ctrl Pts',(9.15476553397154,15.2,5.61756800057427));
#204081=CARTESIAN_POINT('Ctrl Pts',(9.15798463732061,15.2,5.61847675238879));
#204082=CARTESIAN_POINT('Ctrl Pts',(9.16122106674667,15.2,5.61938442099994));
#204083=CARTESIAN_POINT('Ctrl Pts',(9.16447473025285,15.2,5.62029087836012));
#204084=CARTESIAN_POINT('Ctrl Pts',(9.16772839420232,15.2,5.6211973358438));
#204085=CARTESIAN_POINT('Ctrl Pts',(9.17099928938852,15.2,5.62210258158859));
#204086=CARTESIAN_POINT('Ctrl Pts',(9.1742873232355,15.2,5.62300648958221));
#204087=CARTESIAN_POINT('Ctrl Pts',(9.17757535663448,15.2,5.62391039745267));
#204088=CARTESIAN_POINT('Ctrl Pts',(9.18088052783003,15.2,5.62481296639561));
#204089=CARTESIAN_POINT('Ctrl Pts',(9.18420274322337,15.2,5.62571407037766));
#204090=CARTESIAN_POINT('Ctrl Pts',(9.18752495906935,15.2,5.62661517448248));
#204091=CARTESIAN_POINT('Ctrl Pts',(9.19086421827063,15.2,5.62751481473648));
#204092=CARTESIAN_POINT('Ctrl Pts',(9.19422042946883,15.2,5.62841286623394));
#204093=CARTESIAN_POINT('Ctrl Pts',(9.19757664020976,15.2,5.62931091760904));
#204094=CARTESIAN_POINT('Ctrl Pts',(9.20094980172726,15.2,5.63020738044334));
#204095=CARTESIAN_POINT('Ctrl Pts',(9.20433982117062,15.2,5.63110213237036));
#204096=CARTESIAN_POINT('Ctrl Pts',(9.20857734582124,15.2,5.63222057237058));
#204097=CARTESIAN_POINT('Ctrl Pts',(9.21284121273534,15.2,5.63333633900974));
#204098=CARTESIAN_POINT('Ctrl Pts',(9.21713123995542,15.2,5.63444919657943));
#204099=CARTESIAN_POINT('Ctrl Pts',(9.22056326191852,15.2,5.63533948268369));
#204100=CARTESIAN_POINT('Ctrl Pts',(9.22401202803647,15.2,5.63622790754271));
#204101=CARTESIAN_POINT('Ctrl Pts',(9.22747744601891,15.2,5.63711435048393));
#204102=CARTESIAN_POINT('Ctrl Pts',(9.23094286352918,15.2,5.63800079330437));
#204103=CARTESIAN_POINT('Ctrl Pts',(9.2344249338989,15.2,5.63888525663876));
#204104=CARTESIAN_POINT('Ctrl Pts',(9.23792356594453,15.2,5.63976762012239));
#204105=CARTESIAN_POINT('Ctrl Pts',(9.24229685635908,15.2,5.64087057456711));
#204106=CARTESIAN_POINT('Ctrl Pts',(9.24669602301209,15.2,5.64197025246743));
#204107=CARTESIAN_POINT('Ctrl Pts',(9.25112089266278,15.2,5.64306642281494));
#204108=CARTESIAN_POINT('Ctrl Pts',(9.25466078857626,15.2,5.64394335914075));
#204109=CARTESIAN_POINT('Ctrl Pts',(9.25821713354134,15.2,5.64481805327132));
#204110=CARTESIAN_POINT('Ctrl Pts',(9.26178983875232,15.2,5.64569038876726));
#204111=CARTESIAN_POINT('Ctrl Pts',(9.26536254347652,15.2,5.64656272414433));
#204112=CARTESIAN_POINT('Ctrl Pts',(9.2689516076457,15.2,5.64743270245938));
#204113=CARTESIAN_POINT('Ctrl Pts',(9.27255694312708,15.2,5.64830020933316));
#204114=CARTESIAN_POINT('Ctrl Pts',(9.27616227909968,15.2,5.64916771632514));
#204115=CARTESIAN_POINT('Ctrl Pts',(9.2797838857655,15.2,5.65003275388355));
#204116=CARTESIAN_POINT('Ctrl Pts',(9.28342167624154,15.2,5.65089520820833));
#204117=CARTESIAN_POINT('Ctrl Pts',(9.28705946671758,15.2,5.65175766253311));
#204118=CARTESIAN_POINT('Ctrl Pts',(9.29071343938716,15.2,5.65261753527149));
#204119=CARTESIAN_POINT('Ctrl Pts',(9.29438350736661,15.2,5.65347471487348));
#204120=CARTESIAN_POINT('Ctrl Pts',(9.29805357484601,15.2,5.65433189435868));
#204121=CARTESIAN_POINT('Ctrl Pts',(9.30173973868881,15.2,5.65518638288183));
#204122=CARTESIAN_POINT('Ctrl Pts',(9.30544190951403,15.2,5.65603806848275));
#204123=CARTESIAN_POINT('Ctrl Pts',(9.30914408084367,15.2,5.65688975419971));
#204124=CARTESIAN_POINT('Ctrl Pts',(9.3128622594775,15.2,5.65773863990362));
#204125=CARTESIAN_POINT('Ctrl Pts',(9.31659636012708,15.2,5.65858461617164));
#204126=CARTESIAN_POINT('Ctrl Pts',(9.32033046026789,15.2,5.65943059232441));
#204127=CARTESIAN_POINT('Ctrl Pts',(9.32408048200939,15.2,5.660273659647));
#204128=CARTESIAN_POINT('Ctrl Pts',(9.32784633820051,15.2,5.66111371118963));
#204129=CARTESIAN_POINT('Ctrl Pts',(9.33161219490472,15.2,5.66195376284672));
#204130=CARTESIAN_POINT('Ctrl Pts',(9.3353938882613,15.2,5.66279079947581));
#204131=CARTESIAN_POINT('Ctrl Pts',(9.339191329826,15.2,5.66362471639599));
#204132=CARTESIAN_POINT('Ctrl Pts',(9.3429887708733,15.2,5.66445863320254));
#204133=CARTESIAN_POINT('Ctrl Pts',(9.34680196138996,15.2,5.66528942831087));
#204134=CARTESIAN_POINT('Ctrl Pts',(9.35063081618702,15.2,5.66611700046565));
#204135=CARTESIAN_POINT('Ctrl Pts',(9.35445967150578,15.2,5.66694457273318));
#204136=CARTESIAN_POINT('Ctrl Pts',(9.3583041913292,15.2,5.667768921092));
#204137=CARTESIAN_POINT('Ctrl Pts',(9.36216429004059,15.2,5.66858994152542));
#204138=CARTESIAN_POINT('Ctrl Pts',(9.36602438822606,15.2,5.66941096184697));
#204139=CARTESIAN_POINT('Ctrl Pts',(9.36990006629928,15.2,5.67022865769353));
#204140=CARTESIAN_POINT('Ctrl Pts',(9.373791239952,15.2,5.67104292339016));
#204141=CARTESIAN_POINT('Ctrl Pts',(9.3776824141349,15.2,5.67185718919773));
#204142=CARTESIAN_POINT('Ctrl Pts',(9.3815890837559,15.2,5.6726680278222));
#204143=CARTESIAN_POINT('Ctrl Pts',(9.38551116330399,15.2,5.67347533753263));
#204144=CARTESIAN_POINT('Ctrl Pts',(9.38943324231771,15.2,5.67428264713306));
#204145=CARTESIAN_POINT('Ctrl Pts',(9.3933707354561,15.2,5.67508642754254));
#204146=CARTESIAN_POINT('Ctrl Pts',(9.3973235543536,15.2,5.67588658164417));
#204147=CARTESIAN_POINT('Ctrl Pts',(9.40127637378968,15.2,5.67668673585482));
#204148=CARTESIAN_POINT('Ctrl Pts',(9.40524452319667,15.2,5.67748326170679));
#204149=CARTESIAN_POINT('Ctrl Pts',(9.40922791602488,15.2,5.67827606275));
#204150=CARTESIAN_POINT('Ctrl Pts',(9.41420715678877,15.2,5.679267064));
#204151=CARTESIAN_POINT('Ctrl Pts',(9.4192102183964,15.2,5.68025224405166));
#204152=CARTESIAN_POINT('Ctrl Pts',(9.42423694050263,15.2,5.68123141370887));
#204153=CARTESIAN_POINT('Ctrl Pts',(9.42825831785886,15.2,5.68201474937059));
#204154=CARTESIAN_POINT('Ctrl Pts',(9.43229483643133,15.2,5.68279423948897));
#204155=CARTESIAN_POINT('Ctrl Pts',(9.43634641532079,15.2,5.68356978714819));
#204156=CARTESIAN_POINT('Ctrl Pts',(9.44141088934664,15.2,5.68453922180148));
#204157=CARTESIAN_POINT('Ctrl Pts',(9.44649889546656,15.2,5.68550249814654));
#204158=CARTESIAN_POINT('Ctrl Pts',(9.45161027358966,15.2,5.68645943113316));
#204159=CARTESIAN_POINT('Ctrl Pts',(9.45876620307341,15.2,5.6877991373353));
#204160=CARTESIAN_POINT('Ctrl Pts',(9.46596794198473,15.2,5.68912640927859));
#204161=CARTESIAN_POINT('Ctrl Pts',(9.4732150570054,15.2,5.69044075224949));
#204162=CARTESIAN_POINT('Ctrl Pts',(9.47942686955785,15.2,5.69156733188036));
#204163=CARTESIAN_POINT('Ctrl Pts',(9.48567201962926,15.2,5.69268441191886));
#204164=CARTESIAN_POINT('Ctrl Pts',(9.49195023706557,15.2,5.69379168637931));
#204165=CARTESIAN_POINT('Ctrl Pts',(9.49613571573661,15.2,5.69452986941999));
#204166=CARTESIAN_POINT('Ctrl Pts',(9.50033588967609,15.2,5.69526369412689));
#204167=CARTESIAN_POINT('Ctrl Pts',(9.50455068170276,15.2,5.6959930712255));
#204168=CARTESIAN_POINT('Ctrl Pts',(9.50981917144896,15.2,5.69690479254907));
#204169=CARTESIAN_POINT('Ctrl Pts',(9.51511049966305,15.2,5.6978095628146));
#204170=CARTESIAN_POINT('Ctrl Pts',(9.52042451112256,15.2,5.69870721080033));
#204171=CARTESIAN_POINT('Ctrl Pts',(9.52467571994265,15.2,5.69942532913022));
#204172=CARTESIAN_POINT('Ctrl Pts',(9.52894144616258,15.2,5.70013888909713));
#204173=CARTESIAN_POINT('Ctrl Pts',(9.53322161103342,15.2,5.70084780215076));
#204174=CARTESIAN_POINT('Ctrl Pts',(9.53750177648744,15.2,5.70155671530098));
#204175=CARTESIAN_POINT('Ctrl Pts',(9.54179638132058,15.2,5.70226098276476));
#204176=CARTESIAN_POINT('Ctrl Pts',(9.54610534601949,15.2,5.70296051725048));
#204177=CARTESIAN_POINT('Ctrl Pts',(9.5504143101313,15.2,5.70366005164089));
#204178=CARTESIAN_POINT('Ctrl Pts',(9.55473763330786,15.2,5.70435485380143));
#204179=CARTESIAN_POINT('Ctrl Pts',(9.55907523950737,15.2,5.70504483691219));
#204180=CARTESIAN_POINT('Ctrl Pts',(9.56449724769998,15.2,5.70590731587114));
#204181=CARTESIAN_POINT('Ctrl Pts',(9.56994157144779,15.2,5.70676226613856));
#204182=CARTESIAN_POINT('Ctrl Pts',(9.57540805804322,15.2,5.70760952259752));
#204183=CARTESIAN_POINT('Ctrl Pts',(9.58087454463863,15.2,5.70845677905648));
#204184=CARTESIAN_POINT('Ctrl Pts',(9.58636319564204,15.2,5.70929634222245));
#204185=CARTESIAN_POINT('Ctrl Pts',(9.59187385911026,15.2,5.7101280471951));
#204186=CARTESIAN_POINT('Ctrl Pts',(9.59628239012511,15.2,5.71079341120949));
#204187=CARTESIAN_POINT('Ctrl Pts',(9.60070500918112,15.2,5.71145374805982));
#204188=CARTESIAN_POINT('Ctrl Pts',(9.60514163931272,15.2,5.71210897326186));
#204189=CARTESIAN_POINT('Ctrl Pts',(9.60957826883983,15.2,5.71276419837462));
#204190=CARTESIAN_POINT('Ctrl Pts',(9.61402891001412,15.2,5.71341431270508));
#204191=CARTESIAN_POINT('Ctrl Pts',(9.61849348553661,15.2,5.71405923515289));
#204192=CARTESIAN_POINT('Ctrl Pts',(9.62407420539593,15.2,5.71486538827856));
#204193=CARTESIAN_POINT('Ctrl Pts',(9.6296766977954,15.2,5.71566342735715));
#204194=CARTESIAN_POINT('Ctrl Pts',(9.63530081383876,15.2,5.7164531978833));
#204195=CARTESIAN_POINT('Ctrl Pts',(9.63867528334217,15.2,5.71692706018177));
#204196=CARTESIAN_POINT('Ctrl Pts',(9.64205753825177,15.2,5.71739794453126));
#204197=CARTESIAN_POINT('Ctrl Pts',(9.64544754504421,15.2,5.71786581793134));
#204198=CARTESIAN_POINT('Ctrl Pts',(9.64883755245251,15.2,5.71833369141641));
#204199=CARTESIAN_POINT('Ctrl Pts',(9.65223531184631,15.2,5.71879855511732));
#204200=CARTESIAN_POINT('Ctrl Pts',(9.65564079271729,15.2,5.71926037360068));
#204201=CARTESIAN_POINT('Ctrl Pts',(9.66018143284749,15.2,5.71987613143868));
#204202=CARTESIAN_POINT('Ctrl Pts',(9.6647357970898,15.2,5.72048647697461));
#204203=CARTESIAN_POINT('Ctrl Pts',(9.66930381315992,15.2,5.72109133275884));
#204204=CARTESIAN_POINT('Ctrl Pts',(9.6727298253681,15.2,5.72154497461763));
#204205=CARTESIAN_POINT('Ctrl Pts',(9.67616351552148,15.2,5.72199552782362));
#204206=CARTESIAN_POINT('Ctrl Pts',(9.67960485160915,15.2,5.72244296066341));
#204207=CARTESIAN_POINT('Ctrl Pts',(9.68304618769682,15.2,5.7228903935032));
#204208=CARTESIAN_POINT('Ctrl Pts',(9.68649517192299,15.2,5.72333470431943));
#204209=CARTESIAN_POINT('Ctrl Pts',(9.68995177025469,15.2,5.72377586217883));
#204210=CARTESIAN_POINT('Ctrl Pts',(9.69340836921434,15.2,5.72421702011838));
#204211=CARTESIAN_POINT('Ctrl Pts',(9.69687258278448,15.2,5.72465502438204));
#204212=CARTESIAN_POINT('Ctrl Pts',(9.70034437974842,15.2,5.72508984331979));
#204213=CARTESIAN_POINT('Ctrl Pts',(9.70381617608165,15.2,5.72552466217856));
#204214=CARTESIAN_POINT('Ctrl Pts',(9.70729555608946,15.2,5.72595629517917));
#204215=CARTESIAN_POINT('Ctrl Pts',(9.71078248833843,15.2,5.72638471057998));
#204216=CARTESIAN_POINT('Ctrl Pts',(9.71426942058739,15.2,5.7268131259808));
#204217=CARTESIAN_POINT('Ctrl Pts',(9.71776390401438,15.2,5.72723832408048));
#204218=CARTESIAN_POINT('Ctrl Pts',(9.72126590973641,15.2,5.72766027248372));
#204219=CARTESIAN_POINT('Ctrl Pts',(9.72593525048706,15.2,5.72822287032915));
#204220=CARTESIAN_POINT('Ctrl Pts',(9.73061796023402,15.2,5.72877969072936));
#204221=CARTESIAN_POINT('Ctrl Pts',(9.73531396751543,15.2,5.72933066118492));
#204222=CARTESIAN_POINT('Ctrl Pts',(9.73883597377628,15.2,5.72974388912042));
#204223=CARTESIAN_POINT('Ctrl Pts',(9.74236545713923,15.2,5.73015382536334));
#204224=CARTESIAN_POINT('Ctrl Pts',(9.74590239048762,15.2,5.73056043933865));
#204225=CARTESIAN_POINT('Ctrl Pts',(9.74943932319346,15.2,5.73096705324009));
#204226=CARTESIAN_POINT('Ctrl Pts',(9.75298370408223,15.2,5.73137034437504));
#204227=CARTESIAN_POINT('Ctrl Pts',(9.75653550141217,15.2,5.73177028227688));
#204228=CARTESIAN_POINT('Ctrl Pts',(9.76127123097032,15.2,5.73230353278845));
#204229=CARTESIAN_POINT('Ctrl Pts',(9.7660201479786,15.2,5.73283082265678));
#204230=CARTESIAN_POINT('Ctrl Pts',(9.77078217625464,15.2,5.73335207794812));
#204231=CARTESIAN_POINT('Ctrl Pts',(9.77435369827269,15.2,5.7337430195054));
#204232=CARTESIAN_POINT('Ctrl Pts',(9.7779325968595,15.2,5.73413056731172));
#204233=CARTESIAN_POINT('Ctrl Pts',(9.78151884079837,15.2,5.73451469032541));
#204234=CARTESIAN_POINT('Ctrl Pts',(9.78510508408574,15.2,5.73489881326932));
#204235=CARTESIAN_POINT('Ctrl Pts',(9.78869867164675,15.2,5.73527951171823));
#204236=CARTESIAN_POINT('Ctrl Pts',(9.79229957415498,15.2,5.73565675609796));
#204237=CARTESIAN_POINT('Ctrl Pts',(9.79710077728126,15.2,5.73615974858144));
#204238=CARTESIAN_POINT('Ctrl Pts',(9.80191498419252,15.2,5.73665659890233));
#204239=CARTESIAN_POINT('Ctrl Pts',(9.80674212229706,15.2,5.73714723691818));
#204240=CARTESIAN_POINT('Ctrl Pts',(9.81036247603989,15.2,5.73751521544678));
#204241=CARTESIAN_POINT('Ctrl Pts',(9.81399010275721,15.2,5.73787970071729));
#204242=CARTESIAN_POINT('Ctrl Pts',(9.8176249734575,15.2,5.73824066166298));
#204243=CARTESIAN_POINT('Ctrl Pts',(9.82247146816477,15.2,5.73872194296763));
#204244=CARTESIAN_POINT('Ctrl Pts',(9.82733083904608,15.2,5.73919695883102));
#204245=CARTESIAN_POINT('Ctrl Pts',(9.83220301527822,15.2,5.73966564202533));
#204246=CARTESIAN_POINT('Ctrl Pts',(9.83585714712041,15.2,5.74001715438914));
#204247=CARTESIAN_POINT('Ctrl Pts',(9.83951848186322,15.2,5.74036510334397));
#204248=CARTESIAN_POINT('Ctrl Pts',(9.8431869887049,15.2,5.7407094602497));
#204249=CARTESIAN_POINT('Ctrl Pts',(9.84685549554658,15.2,5.74105381715544));
#204250=CARTESIAN_POINT('Ctrl Pts',(9.85053117479968,15.2,5.74139458165847));
#204251=CARTESIAN_POINT('Ctrl Pts',(9.85421399608192,15.2,5.74173172602154));
#204252=CARTESIAN_POINT('Ctrl Pts',(9.85789681736415,15.2,5.7420688703846));
#204253=CARTESIAN_POINT('Ctrl Pts',(9.86158678041257,15.2,5.74240239298959));
#204254=CARTESIAN_POINT('Ctrl Pts',(9.86528385669394,15.2,5.7427322674781));
#204255=CARTESIAN_POINT('Ctrl Pts',(9.87021329218351,15.2,5.7431721001694));
#204256=CARTESIAN_POINT('Ctrl Pts',(9.87515537289402,15.2,5.74360544608902));
#204257=CARTESIAN_POINT('Ctrl Pts',(9.88011002451994,15.2,5.7440322367253));
#204258=CARTESIAN_POINT('Ctrl Pts',(9.88382601290184,15.2,5.74435232967344));
#204259=CARTESIAN_POINT('Ctrl Pts',(9.88754907379846,15.2,5.74466873594298));
#204260=CARTESIAN_POINT('Ctrl Pts',(9.89127917472151,15.2,5.74498142451639));
#204261=CARTESIAN_POINT('Ctrl Pts',(9.89500927564456,15.2,5.7452941130898));
#204262=CARTESIAN_POINT('Ctrl Pts',(9.89874641794522,15.2,5.74560308619412));
#204263=CARTESIAN_POINT('Ctrl Pts',(9.90249057380857,15.2,5.74590831722501));
#204264=CARTESIAN_POINT('Ctrl Pts',(9.90623472967192,15.2,5.7462135482559));
#204265=CARTESIAN_POINT('Ctrl Pts',(9.90998589995145,15.2,5.74651503727874));
#204266=CARTESIAN_POINT('Ctrl Pts',(9.91374405518896,15.2,5.74681275914344));
#204267=CARTESIAN_POINT('Ctrl Pts',(9.91750221110919,15.2,5.74711048106222));
#204268=CARTESIAN_POINT('Ctrl Pts',(9.92126735243973,15.2,5.74740443422161));
#204269=CARTESIAN_POINT('Ctrl Pts',(9.92503944240555,15.2,5.74769458655493));
#204270=CARTESIAN_POINT('Ctrl Pts',(9.92881153168611,15.2,5.74798473883553));
#204271=CARTESIAN_POINT('Ctrl Pts',(9.93259056973007,15.2,5.74827108743457));
#204272=CARTESIAN_POINT('Ctrl Pts',(9.93637652394912,15.2,5.74855360502131));
#204273=CARTESIAN_POINT('Ctrl Pts',(9.94016247816818,15.2,5.74883612260804));
#204274=CARTESIAN_POINT('Ctrl Pts',(9.94395534887523,15.2,5.74911480860738));
#204275=CARTESIAN_POINT('Ctrl Pts',(9.94775512114579,15.2,5.74938964953395));
#204276=CARTESIAN_POINT('Ctrl Pts',(9.95155489341636,15.2,5.74966449046052));
#204277=CARTESIAN_POINT('Ctrl Pts',(9.95536157030715,15.2,5.74993548595142));
#204278=CARTESIAN_POINT('Ctrl Pts',(9.95917514599994,15.2,5.75020264099999));
#204279=CARTESIAN_POINT('Origin',(-5.66257110645729E-14,15.2,-1.77635683940025E-14));
#204280=CARTESIAN_POINT('',(8.56667970899995,15.2,5.85257411499998));
#204281=CARTESIAN_POINT('',(8.56667970899995,12.2,5.85257411499998));
#204282=CARTESIAN_POINT('',(8.56667970899995,15.2,5.85257411499998));
#204283=CARTESIAN_POINT('Origin',(-5.66257110645729E-14,12.2,-1.77635683940025E-14));
#204284=CARTESIAN_POINT('Origin',(-5.66257110645729E-14,15.2,-1.77635683940025E-14));
#204285=CARTESIAN_POINT('Origin',(-5.66257110645729E-14,15.2,-1.77635683940025E-14));
#204286=CARTESIAN_POINT('',(9.27155330199994,15.2,6.80355049699998));
#204287=CARTESIAN_POINT('',(9.03946594399994,15.2,7.10901226999999));
#204288=CARTESIAN_POINT('Origin',(-5.66257110645729E-14,15.2,-1.77635683940025E-14));
#204289=CARTESIAN_POINT('',(9.03946594399994,12.2,7.10901226999999));
#204290=CARTESIAN_POINT('',(9.03946594399994,15.2,7.10901226999999));
#204291=CARTESIAN_POINT('',(9.27155330199994,12.2,6.80355049699998));
#204292=CARTESIAN_POINT('Origin',(-5.66257110645729E-14,12.2,-1.77635683940025E-14));
#204293=CARTESIAN_POINT('',(9.27155330199994,15.2,6.80355049699998));
#204294=CARTESIAN_POINT('Ctrl Pts',(9.03946594399994,15.2,7.10901226999999));
#204295=CARTESIAN_POINT('Ctrl Pts',(9.03946594399994,11.6,7.10901226999999));
#204296=CARTESIAN_POINT('Ctrl Pts',(9.03871859599995,15.2,7.10885083699999));
#204297=CARTESIAN_POINT('Ctrl Pts',(9.03871859599995,11.6,7.10885083699999));
#204298=CARTESIAN_POINT('Ctrl Pts',(9.03722439199995,15.2,7.10852778399998));
#204299=CARTESIAN_POINT('Ctrl Pts',(9.03722439199995,11.6,7.10852778399998));
#204300=CARTESIAN_POINT('Ctrl Pts',(9.03498456099994,15.2,7.10804263999999));
#204301=CARTESIAN_POINT('Ctrl Pts',(9.03498456099994,11.6,7.10804263999999));
#204302=CARTESIAN_POINT('Ctrl Pts',(9.03200107099994,15.2,7.10739465099999));
#204303=CARTESIAN_POINT('Ctrl Pts',(9.03200107099994,11.6,7.10739465099999));
#204304=CARTESIAN_POINT('Ctrl Pts',(9.02827662899995,15.2,7.10658278399999));
#204305=CARTESIAN_POINT('Ctrl Pts',(9.02827662899995,11.6,7.10658278399999));
#204306=CARTESIAN_POINT('Ctrl Pts',(9.02455710699994,15.2,7.10576903499998));
#204307=CARTESIAN_POINT('Ctrl Pts',(9.02455710699994,11.6,7.10576903499998));
#204308=CARTESIAN_POINT('Ctrl Pts',(9.02084250599994,15.2,7.10495340799999));
#204309=CARTESIAN_POINT('Ctrl Pts',(9.02084250599994,11.6,7.10495340799999));
#204310=CARTESIAN_POINT('Ctrl Pts',(9.01713282899994,15.2,7.10413590399998));
#204311=CARTESIAN_POINT('Ctrl Pts',(9.01713282899994,11.6,7.10413590399998));
#204312=CARTESIAN_POINT('Ctrl Pts',(9.01342807999994,15.2,7.10331652899999));
#204313=CARTESIAN_POINT('Ctrl Pts',(9.01342807999994,11.6,7.10331652899999));
#204314=CARTESIAN_POINT('Ctrl Pts',(9.00972826499994,15.2,7.10249528799999));
#204315=CARTESIAN_POINT('Ctrl Pts',(9.00972826499994,11.6,7.10249528799999));
#204316=CARTESIAN_POINT('Ctrl Pts',(9.00603338799994,15.2,7.10167218799998));
#204317=CARTESIAN_POINT('Ctrl Pts',(9.00603338799994,11.6,7.10167218799998));
#204318=CARTESIAN_POINT('Ctrl Pts',(9.00234345899994,15.2,7.10084723999999));
#204319=CARTESIAN_POINT('Ctrl Pts',(9.00234345899994,11.6,7.10084723999999));
#204320=CARTESIAN_POINT('Ctrl Pts',(8.99865848199994,15.2,7.10002045099999));
#204321=CARTESIAN_POINT('Ctrl Pts',(8.99865848199994,11.6,7.10002045099999));
#204322=CARTESIAN_POINT('Ctrl Pts',(8.99497846499994,15.2,7.09919182899998));
#204323=CARTESIAN_POINT('Ctrl Pts',(8.99497846499994,11.6,7.09919182899998));
#204324=CARTESIAN_POINT('Ctrl Pts',(8.99130341599994,15.2,7.09836138399999));
#204325=CARTESIAN_POINT('Ctrl Pts',(8.99130341599994,11.6,7.09836138399999));
#204326=CARTESIAN_POINT('Ctrl Pts',(8.98763333799995,15.2,7.09752912199999));
#204327=CARTESIAN_POINT('Ctrl Pts',(8.98763333799995,11.6,7.09752912199999));
#204328=CARTESIAN_POINT('Ctrl Pts',(8.98396823899994,15.2,7.09669505099999));
#204329=CARTESIAN_POINT('Ctrl Pts',(8.98396823899994,11.6,7.09669505099999));
#204330=CARTESIAN_POINT('Ctrl Pts',(8.98030812399995,15.2,7.09585917499999));
#204331=CARTESIAN_POINT('Ctrl Pts',(8.98030812399995,11.6,7.09585917499999));
#204332=CARTESIAN_POINT('Ctrl Pts',(8.97665299699994,15.2,7.09502150199998));
#204333=CARTESIAN_POINT('Ctrl Pts',(8.97665299699994,11.6,7.09502150199998));
#204334=CARTESIAN_POINT('Ctrl Pts',(8.97300286299994,15.2,7.09418203899999));
#204335=CARTESIAN_POINT('Ctrl Pts',(8.97300286299994,11.6,7.09418203899999));
#204336=CARTESIAN_POINT('Ctrl Pts',(8.96935772799995,15.2,7.09334079099998));
#204337=CARTESIAN_POINT('Ctrl Pts',(8.96935772799995,11.6,7.09334079099998));
#204338=CARTESIAN_POINT('Ctrl Pts',(8.96571759699994,15.2,7.09249776699998));
#204339=CARTESIAN_POINT('Ctrl Pts',(8.96571759699994,11.6,7.09249776699998));
#204340=CARTESIAN_POINT('Ctrl Pts',(8.96208247799994,15.2,7.09165297199998));
#204341=CARTESIAN_POINT('Ctrl Pts',(8.96208247799994,11.6,7.09165297199998));
#204342=CARTESIAN_POINT('Ctrl Pts',(8.95845237299995,15.2,7.09080641399999));
#204343=CARTESIAN_POINT('Ctrl Pts',(8.95845237299995,11.6,7.09080641399999));
#204344=CARTESIAN_POINT('Ctrl Pts',(8.95482729199994,15.2,7.08995810299999));
#204345=CARTESIAN_POINT('Ctrl Pts',(8.95482729199994,11.6,7.08995810299999));
#204346=CARTESIAN_POINT('Ctrl Pts',(8.95120723799995,15.2,7.08910804299999));
#204347=CARTESIAN_POINT('Ctrl Pts',(8.95120723799995,11.6,7.08910804299999));
#204348=CARTESIAN_POINT('Ctrl Pts',(8.94759221899994,15.2,7.08825624399999));
#204349=CARTESIAN_POINT('Ctrl Pts',(8.94759221899994,11.6,7.08825624399999));
#204350=CARTESIAN_POINT('Ctrl Pts',(8.94398223899995,15.2,7.08740271099998));
#204351=CARTESIAN_POINT('Ctrl Pts',(8.94398223899995,11.6,7.08740271099998));
#204352=CARTESIAN_POINT('Ctrl Pts',(8.94037730399995,15.2,7.08654745199999));
#204353=CARTESIAN_POINT('Ctrl Pts',(8.94037730399995,11.6,7.08654745199999));
#204354=CARTESIAN_POINT('Ctrl Pts',(8.93677741999995,15.2,7.08569047499999));
#204355=CARTESIAN_POINT('Ctrl Pts',(8.93677741999995,11.6,7.08569047499999));
#204356=CARTESIAN_POINT('Ctrl Pts',(8.93318259299994,15.2,7.08483178599998));
#204357=CARTESIAN_POINT('Ctrl Pts',(8.93318259299994,11.6,7.08483178599998));
#204358=CARTESIAN_POINT('Ctrl Pts',(8.92959282899995,15.2,7.08397139299999));
#204359=CARTESIAN_POINT('Ctrl Pts',(8.92959282899995,11.6,7.08397139299999));
#204360=CARTESIAN_POINT('Ctrl Pts',(8.92600813099994,15.2,7.08310930299999));
#204361=CARTESIAN_POINT('Ctrl Pts',(8.92600813099994,11.6,7.08310930299999));
#204362=CARTESIAN_POINT('Ctrl Pts',(8.92242850799994,15.2,7.08224552199999));
#204363=CARTESIAN_POINT('Ctrl Pts',(8.92242850799994,11.6,7.08224552199999));
#204364=CARTESIAN_POINT('Ctrl Pts',(8.91885396299994,15.2,7.08138005899999));
#204365=CARTESIAN_POINT('Ctrl Pts',(8.91885396299994,11.6,7.08138005899999));
#204366=CARTESIAN_POINT('Ctrl Pts',(8.91528450599994,15.2,7.08051292099999));
#204367=CARTESIAN_POINT('Ctrl Pts',(8.91528450599994,11.6,7.08051292099999));
#204368=CARTESIAN_POINT('Ctrl Pts',(8.91172013699994,15.2,7.07964411399999));
#204369=CARTESIAN_POINT('Ctrl Pts',(8.91172013699994,11.6,7.07964411399999));
#204370=CARTESIAN_POINT('Ctrl Pts',(8.90816086699994,15.2,7.07877364899999));
#204371=CARTESIAN_POINT('Ctrl Pts',(8.90816086699994,11.6,7.07877364899999));
#204372=CARTESIAN_POINT('Ctrl Pts',(8.90460669799995,15.2,7.07790152999999));
#204373=CARTESIAN_POINT('Ctrl Pts',(8.90460669799995,11.6,7.07790152999999));
#204374=CARTESIAN_POINT('Ctrl Pts',(8.90105763799994,15.2,7.07702776599999));
#204375=CARTESIAN_POINT('Ctrl Pts',(8.90105763799994,11.6,7.07702776599999));
#204376=CARTESIAN_POINT('Ctrl Pts',(8.89751369099994,15.2,7.07615236299999));
#204377=CARTESIAN_POINT('Ctrl Pts',(8.89751369099994,11.6,7.07615236299999));
#204378=CARTESIAN_POINT('Ctrl Pts',(8.89397486399995,15.2,7.07527532999999));
#204379=CARTESIAN_POINT('Ctrl Pts',(8.89397486399995,11.6,7.07527532999999));
#204380=CARTESIAN_POINT('Ctrl Pts',(8.89044116399995,15.2,7.07439667399999));
#204381=CARTESIAN_POINT('Ctrl Pts',(8.89044116399995,11.6,7.07439667399999));
#204382=CARTESIAN_POINT('Ctrl Pts',(8.88691259399994,15.2,7.07351640199998));
#204383=CARTESIAN_POINT('Ctrl Pts',(8.88691259399994,11.6,7.07351640199998));
#204384=CARTESIAN_POINT('Ctrl Pts',(8.88338916199995,15.2,7.07263452199999));
#204385=CARTESIAN_POINT('Ctrl Pts',(8.88338916199995,11.6,7.07263452199999));
#204386=CARTESIAN_POINT('Ctrl Pts',(8.87987087299994,15.2,7.07175104099999));
#204387=CARTESIAN_POINT('Ctrl Pts',(8.87987087299994,11.6,7.07175104099999));
#204388=CARTESIAN_POINT('Ctrl Pts',(8.87635773099994,15.2,7.07086596699998));
#204389=CARTESIAN_POINT('Ctrl Pts',(8.87635773099994,11.6,7.07086596699998));
#204390=CARTESIAN_POINT('Ctrl Pts',(8.87284974399994,15.2,7.06997930699998));
#204391=CARTESIAN_POINT('Ctrl Pts',(8.87284974399994,11.6,7.06997930699998));
#204392=CARTESIAN_POINT('Ctrl Pts',(8.86934691799994,15.2,7.06909106899998));
#204393=CARTESIAN_POINT('Ctrl Pts',(8.86934691799994,11.6,7.06909106899998));
#204394=CARTESIAN_POINT('Ctrl Pts',(8.86584925799994,15.2,7.06820126099998));
#204395=CARTESIAN_POINT('Ctrl Pts',(8.86584925799994,11.6,7.06820126099998));
#204396=CARTESIAN_POINT('Ctrl Pts',(8.86235676999994,15.2,7.06730989099999));
#204397=CARTESIAN_POINT('Ctrl Pts',(8.86235676999994,11.6,7.06730989099999));
#204398=CARTESIAN_POINT('Ctrl Pts',(8.85886945899994,15.2,7.06641696499998));
#204399=CARTESIAN_POINT('Ctrl Pts',(8.85886945899994,11.6,7.06641696499998));
#204400=CARTESIAN_POINT('Ctrl Pts',(8.85538733199994,15.2,7.06552249099998));
#204401=CARTESIAN_POINT('Ctrl Pts',(8.85538733199994,11.6,7.06552249099998));
#204402=CARTESIAN_POINT('Ctrl Pts',(8.85191039299994,15.2,7.06462647799999));
#204403=CARTESIAN_POINT('Ctrl Pts',(8.85191039299994,11.6,7.06462647799999));
#204404=CARTESIAN_POINT('Ctrl Pts',(8.84843865099995,15.2,7.06372893099999));
#204405=CARTESIAN_POINT('Ctrl Pts',(8.84843865099995,11.6,7.06372893099999));
#204406=CARTESIAN_POINT('Ctrl Pts',(8.84497210899994,15.2,7.06282986199999));
#204407=CARTESIAN_POINT('Ctrl Pts',(8.84497210899994,11.6,7.06282986199999));
#204408=CARTESIAN_POINT('Ctrl Pts',(8.84151077299994,15.2,7.06192927399999));
#204409=CARTESIAN_POINT('Ctrl Pts',(8.84151077299994,11.6,7.06192927399999));
#204410=CARTESIAN_POINT('Ctrl Pts',(8.83805465099995,15.2,7.06102717799999));
#204411=CARTESIAN_POINT('Ctrl Pts',(8.83805465099995,11.6,7.06102717799999));
#204412=CARTESIAN_POINT('Ctrl Pts',(8.83460374599995,15.2,7.06012358099999));
#204413=CARTESIAN_POINT('Ctrl Pts',(8.83460374599995,11.6,7.06012358099999));
#204414=CARTESIAN_POINT('Ctrl Pts',(8.83115806599994,15.2,7.05921849099998));
#204415=CARTESIAN_POINT('Ctrl Pts',(8.83115806599994,11.6,7.05921849099998));
#204416=CARTESIAN_POINT('Ctrl Pts',(8.82771761599994,15.2,7.05831191399999));
#204417=CARTESIAN_POINT('Ctrl Pts',(8.82771761599994,11.6,7.05831191399999));
#204418=CARTESIAN_POINT('Ctrl Pts',(8.82428240299994,15.2,7.05740385899999));
#204419=CARTESIAN_POINT('Ctrl Pts',(8.82428240299994,11.6,7.05740385899999));
#204420=CARTESIAN_POINT('Ctrl Pts',(8.82085243099995,15.2,7.05649433499998));
#204421=CARTESIAN_POINT('Ctrl Pts',(8.82085243099995,11.6,7.05649433499998));
#204422=CARTESIAN_POINT('Ctrl Pts',(8.81742770599995,15.2,7.05558334799999));
#204423=CARTESIAN_POINT('Ctrl Pts',(8.81742770599995,11.6,7.05558334799999));
#204424=CARTESIAN_POINT('Ctrl Pts',(8.81400823499994,15.2,7.05467090699998));
#204425=CARTESIAN_POINT('Ctrl Pts',(8.81400823499994,11.6,7.05467090699998));
#204426=CARTESIAN_POINT('Ctrl Pts',(8.81059402299995,15.2,7.05375701899998));
#204427=CARTESIAN_POINT('Ctrl Pts',(8.81059402299995,11.6,7.05375701899998));
#204428=CARTESIAN_POINT('Ctrl Pts',(8.80718507599994,15.2,7.05284169299999));
#204429=CARTESIAN_POINT('Ctrl Pts',(8.80718507599994,11.6,7.05284169299999));
#204430=CARTESIAN_POINT('Ctrl Pts',(8.80378140199995,15.2,7.05192493599998));
#204431=CARTESIAN_POINT('Ctrl Pts',(8.80378140199995,11.6,7.05192493599998));
#204432=CARTESIAN_POINT('Ctrl Pts',(8.80038300299994,15.2,7.05100675699998));
#204433=CARTESIAN_POINT('Ctrl Pts',(8.80038300299994,11.6,7.05100675699998));
#204434=CARTESIAN_POINT('Ctrl Pts',(8.79698988899994,15.2,7.05008716199998));
#204435=CARTESIAN_POINT('Ctrl Pts',(8.79698988899994,11.6,7.05008716199998));
#204436=CARTESIAN_POINT('Ctrl Pts',(8.79360206099994,15.2,7.04916616199998));
#204437=CARTESIAN_POINT('Ctrl Pts',(8.79360206099994,11.6,7.04916616199998));
#204438=CARTESIAN_POINT('Ctrl Pts',(8.79021952999994,15.2,7.04824376099998));
#204439=CARTESIAN_POINT('Ctrl Pts',(8.79021952999994,11.6,7.04824376099998));
#204440=CARTESIAN_POINT('Ctrl Pts',(8.78684229799994,15.2,7.04731997099999));
#204441=CARTESIAN_POINT('Ctrl Pts',(8.78684229799994,11.6,7.04731997099999));
#204442=CARTESIAN_POINT('Ctrl Pts',(8.78347037299994,15.2,7.04639479699999));
#204443=CARTESIAN_POINT('Ctrl Pts',(8.78347037299994,11.6,7.04639479699999));
#204444=CARTESIAN_POINT('Ctrl Pts',(8.78010375999994,15.2,7.04546824999999));
#204445=CARTESIAN_POINT('Ctrl Pts',(8.78010375999994,11.6,7.04546824999999));
#204446=CARTESIAN_POINT('Ctrl Pts',(8.77674246599994,15.2,7.04454033599998));
#204447=CARTESIAN_POINT('Ctrl Pts',(8.77674246599994,11.6,7.04454033599998));
#204448=CARTESIAN_POINT('Ctrl Pts',(8.77338649599994,15.2,7.04361106299999));
#204449=CARTESIAN_POINT('Ctrl Pts',(8.77338649599994,11.6,7.04361106299999));
#204450=CARTESIAN_POINT('Ctrl Pts',(8.77003585599994,15.2,7.04268043999999));
#204451=CARTESIAN_POINT('Ctrl Pts',(8.77003585599994,11.6,7.04268043999999));
#204452=CARTESIAN_POINT('Ctrl Pts',(8.76669055199994,15.2,7.04174847499999));
#204453=CARTESIAN_POINT('Ctrl Pts',(8.76669055199994,11.6,7.04174847499999));
#204454=CARTESIAN_POINT('Ctrl Pts',(8.76335058999994,15.2,7.04081517599998));
#204455=CARTESIAN_POINT('Ctrl Pts',(8.76335058999994,11.6,7.04081517599998));
#204456=CARTESIAN_POINT('Ctrl Pts',(8.76001597499994,15.2,7.03988055099998));
#204457=CARTESIAN_POINT('Ctrl Pts',(8.76001597499994,11.6,7.03988055099998));
#204458=CARTESIAN_POINT('Ctrl Pts',(8.75668671499995,15.2,7.03894460699999));
#204459=CARTESIAN_POINT('Ctrl Pts',(8.75668671499995,11.6,7.03894460699999));
#204460=CARTESIAN_POINT('Ctrl Pts',(8.75336281399994,15.2,7.03800735499998));
#204461=CARTESIAN_POINT('Ctrl Pts',(8.75336281399994,11.6,7.03800735499998));
#204462=CARTESIAN_POINT('Ctrl Pts',(8.75004427899994,15.2,7.03706880299999));
#204463=CARTESIAN_POINT('Ctrl Pts',(8.75004427899994,11.6,7.03706880299999));
#204464=CARTESIAN_POINT('Ctrl Pts',(8.74673111599994,15.2,7.03612895699998));
#204465=CARTESIAN_POINT('Ctrl Pts',(8.74673111599994,11.6,7.03612895699998));
#204466=CARTESIAN_POINT('Ctrl Pts',(8.74342332999994,15.2,7.03518782599998));
#204467=CARTESIAN_POINT('Ctrl Pts',(8.74342332999994,11.6,7.03518782599998));
#204468=CARTESIAN_POINT('Ctrl Pts',(8.74012092799994,15.2,7.03424541899999));
#204469=CARTESIAN_POINT('Ctrl Pts',(8.74012092799994,11.6,7.03424541899999));
#204470=CARTESIAN_POINT('Ctrl Pts',(8.73682391499995,15.2,7.03330174299998));
#204471=CARTESIAN_POINT('Ctrl Pts',(8.73682391499995,11.6,7.03330174299998));
#204472=CARTESIAN_POINT('Ctrl Pts',(8.73353229799994,15.2,7.03235680799998));
#204473=CARTESIAN_POINT('Ctrl Pts',(8.73353229799994,11.6,7.03235680799998));
#204474=CARTESIAN_POINT('Ctrl Pts',(8.73024608099995,15.2,7.03141062299999));
#204475=CARTESIAN_POINT('Ctrl Pts',(8.73024608099995,11.6,7.03141062299999));
#204476=CARTESIAN_POINT('Ctrl Pts',(8.72696527299994,15.2,7.03046319399999));
#204477=CARTESIAN_POINT('Ctrl Pts',(8.72696527299994,11.6,7.03046319399999));
#204478=CARTESIAN_POINT('Ctrl Pts',(8.72368987799994,15.2,7.02951452999999));
#204479=CARTESIAN_POINT('Ctrl Pts',(8.72368987799994,11.6,7.02951452999999));
#204480=CARTESIAN_POINT('Ctrl Pts',(8.72041990199994,15.2,7.02856464099998));
#204481=CARTESIAN_POINT('Ctrl Pts',(8.72041990199994,11.6,7.02856464099998));
#204482=CARTESIAN_POINT('Ctrl Pts',(8.71715535199994,15.2,7.02761353499999));
#204483=CARTESIAN_POINT('Ctrl Pts',(8.71715535199994,11.6,7.02761353499999));
#204484=CARTESIAN_POINT('Ctrl Pts',(8.71389623199994,15.2,7.02666121899998));
#204485=CARTESIAN_POINT('Ctrl Pts',(8.71389623199994,11.6,7.02666121899998));
#204486=CARTESIAN_POINT('Ctrl Pts',(8.71064255099994,15.2,7.02570770199999));
#204487=CARTESIAN_POINT('Ctrl Pts',(8.71064255099994,11.6,7.02570770199999));
#204488=CARTESIAN_POINT('Ctrl Pts',(8.70739431399995,15.2,7.02475299199998));
#204489=CARTESIAN_POINT('Ctrl Pts',(8.70739431399995,11.6,7.02475299199998));
#204490=CARTESIAN_POINT('Ctrl Pts',(8.70415152399995,15.2,7.02379709899999));
#204491=CARTESIAN_POINT('Ctrl Pts',(8.70415152399995,11.6,7.02379709899999));
#204492=CARTESIAN_POINT('Ctrl Pts',(8.70091418999994,15.2,7.02284003199999));
#204493=CARTESIAN_POINT('Ctrl Pts',(8.70091418999994,11.6,7.02284003199999));
#204494=CARTESIAN_POINT('Ctrl Pts',(8.69768231899995,15.2,7.02188179799998));
#204495=CARTESIAN_POINT('Ctrl Pts',(8.69768231899995,11.6,7.02188179799998));
#204496=CARTESIAN_POINT('Ctrl Pts',(8.69445591399994,15.2,7.02092240599999));
#204497=CARTESIAN_POINT('Ctrl Pts',(8.69445591399994,11.6,7.02092240599999));
#204498=CARTESIAN_POINT('Ctrl Pts',(8.69123498299994,15.2,7.01996186499999));
#204499=CARTESIAN_POINT('Ctrl Pts',(8.69123498299994,11.6,7.01996186499999));
#204500=CARTESIAN_POINT('Ctrl Pts',(8.68801953099995,15.2,7.01900018299998));
#204501=CARTESIAN_POINT('Ctrl Pts',(8.68801953099995,11.6,7.01900018299998));
#204502=CARTESIAN_POINT('Ctrl Pts',(8.68480956499995,15.2,7.01803736999998));
#204503=CARTESIAN_POINT('Ctrl Pts',(8.68480956499995,11.6,7.01803736999998));
#204504=CARTESIAN_POINT('Ctrl Pts',(8.68160508999994,15.2,7.01707343299999));
#204505=CARTESIAN_POINT('Ctrl Pts',(8.68160508999994,11.6,7.01707343299999));
#204506=CARTESIAN_POINT('Ctrl Pts',(8.67840611299994,15.2,7.01610838099998));
#204507=CARTESIAN_POINT('Ctrl Pts',(8.67840611299994,11.6,7.01610838099998));
#204508=CARTESIAN_POINT('Ctrl Pts',(8.67521263999994,15.2,7.01514222399998));
#204509=CARTESIAN_POINT('Ctrl Pts',(8.67521263999994,11.6,7.01514222399998));
#204510=CARTESIAN_POINT('Ctrl Pts',(8.67202467599994,15.2,7.01417496899998));
#204511=CARTESIAN_POINT('Ctrl Pts',(8.67202467599994,11.6,7.01417496899998));
#204512=CARTESIAN_POINT('Ctrl Pts',(8.66884222899994,15.2,7.01320662699998));
#204513=CARTESIAN_POINT('Ctrl Pts',(8.66884222899994,11.6,7.01320662699998));
#204514=CARTESIAN_POINT('Ctrl Pts',(8.66566530299994,15.2,7.01223720499998));
#204515=CARTESIAN_POINT('Ctrl Pts',(8.66566530299994,11.6,7.01223720499998));
#204516=CARTESIAN_POINT('Ctrl Pts',(8.66249390499994,15.2,7.01126671199999));
#204517=CARTESIAN_POINT('Ctrl Pts',(8.66249390499994,11.6,7.01126671199999));
#204518=CARTESIAN_POINT('Ctrl Pts',(8.65932804199994,15.2,7.01029515699998));
#204519=CARTESIAN_POINT('Ctrl Pts',(8.65932804199994,11.6,7.01029515699998));
#204520=CARTESIAN_POINT('Ctrl Pts',(8.65616771699995,15.2,7.00932254899998));
#204521=CARTESIAN_POINT('Ctrl Pts',(8.65616771699995,11.6,7.00932254899998));
#204522=CARTESIAN_POINT('Ctrl Pts',(8.65301293899994,15.2,7.00834889699999));
#204523=CARTESIAN_POINT('Ctrl Pts',(8.65301293899994,11.6,7.00834889699999));
#204524=CARTESIAN_POINT('Ctrl Pts',(8.64986371499995,15.2,7.00737420999998));
#204525=CARTESIAN_POINT('Ctrl Pts',(8.64986371499995,11.6,7.00737420999998));
#204526=CARTESIAN_POINT('Ctrl Pts',(8.64672004799995,15.2,7.00639849699999));
#204527=CARTESIAN_POINT('Ctrl Pts',(8.64672004799995,11.6,7.00639849699999));
#204528=CARTESIAN_POINT('Ctrl Pts',(8.64358194499994,15.2,7.00542176599999));
#204529=CARTESIAN_POINT('Ctrl Pts',(8.64358194499994,11.6,7.00542176599999));
#204530=CARTESIAN_POINT('Ctrl Pts',(8.64044941299994,15.2,7.00444402599998));
#204531=CARTESIAN_POINT('Ctrl Pts',(8.64044941299994,11.6,7.00444402599998));
#204532=CARTESIAN_POINT('Ctrl Pts',(8.63732245799994,15.2,7.00346528799999));
#204533=CARTESIAN_POINT('Ctrl Pts',(8.63732245799994,11.6,7.00346528799999));
#204534=CARTESIAN_POINT('Ctrl Pts',(8.63420108499995,15.2,7.00248555899999));
#204535=CARTESIAN_POINT('Ctrl Pts',(8.63420108499995,11.6,7.00248555899999));
#204536=CARTESIAN_POINT('Ctrl Pts',(8.63108530199994,15.2,7.00150484999998));
#204537=CARTESIAN_POINT('Ctrl Pts',(8.63108530199994,11.6,7.00150484999998));
#204538=CARTESIAN_POINT('Ctrl Pts',(8.62797511399994,15.2,7.00052316799999));
#204539=CARTESIAN_POINT('Ctrl Pts',(8.62797511399994,11.6,7.00052316799999));
#204540=CARTESIAN_POINT('Ctrl Pts',(8.62487052699995,15.2,6.99954052199999));
#204541=CARTESIAN_POINT('Ctrl Pts',(8.62487052699995,11.6,6.99954052199999));
#204542=CARTESIAN_POINT('Ctrl Pts',(8.62177154699994,15.2,6.99855692299998));
#204543=CARTESIAN_POINT('Ctrl Pts',(8.62177154699994,11.6,6.99855692299998));
#204544=CARTESIAN_POINT('Ctrl Pts',(8.61867818099994,15.2,6.99757237799999));
#204545=CARTESIAN_POINT('Ctrl Pts',(8.61867818099994,11.6,6.99757237799999));
#204546=CARTESIAN_POINT('Ctrl Pts',(8.61559043399994,15.2,6.99658689899999));
#204547=CARTESIAN_POINT('Ctrl Pts',(8.61559043399994,11.6,6.99658689899999));
#204548=CARTESIAN_POINT('Ctrl Pts',(8.61250831399994,15.2,6.99560049199999));
#204549=CARTESIAN_POINT('Ctrl Pts',(8.61250831399994,11.6,6.99560049199999));
#204550=CARTESIAN_POINT('Ctrl Pts',(8.60943182399994,15.2,6.99461316899999));
#204551=CARTESIAN_POINT('Ctrl Pts',(8.60943182399994,11.6,6.99461316899999));
#204552=CARTESIAN_POINT('Ctrl Pts',(8.60636097399994,15.2,6.99362493599998));
#204553=CARTESIAN_POINT('Ctrl Pts',(8.60636097399994,11.6,6.99362493599998));
#204554=CARTESIAN_POINT('Ctrl Pts',(8.60329576799994,15.2,6.99263580599998));
#204555=CARTESIAN_POINT('Ctrl Pts',(8.60329576799994,11.6,6.99263580599998));
#204556=CARTESIAN_POINT('Ctrl Pts',(8.60023621199994,15.2,6.99164578599999));
#204557=CARTESIAN_POINT('Ctrl Pts',(8.60023621199994,11.6,6.99164578599999));
#204558=CARTESIAN_POINT('Ctrl Pts',(8.59718231199994,15.2,6.99065488499999));
#204559=CARTESIAN_POINT('Ctrl Pts',(8.59718231199994,11.6,6.99065488499999));
#204560=CARTESIAN_POINT('Ctrl Pts',(8.59413407599994,15.2,6.98966311399998));
#204561=CARTESIAN_POINT('Ctrl Pts',(8.59413407599994,11.6,6.98966311399998));
#204562=CARTESIAN_POINT('Ctrl Pts',(8.59109150899994,15.2,6.98867048199999));
#204563=CARTESIAN_POINT('Ctrl Pts',(8.59109150899994,11.6,6.98867048199999));
#204564=CARTESIAN_POINT('Ctrl Pts',(8.58805461599994,15.2,6.98767699699999));
#204565=CARTESIAN_POINT('Ctrl Pts',(8.58805461599994,11.6,6.98767699699999));
#204566=CARTESIAN_POINT('Ctrl Pts',(8.58502340499994,15.2,6.98668266799999));
#204567=CARTESIAN_POINT('Ctrl Pts',(8.58502340499994,11.6,6.98668266799999));
#204568=CARTESIAN_POINT('Ctrl Pts',(8.58199788199994,15.2,6.98568750799998));
#204569=CARTESIAN_POINT('Ctrl Pts',(8.58199788199994,11.6,6.98568750799998));
#204570=CARTESIAN_POINT('Ctrl Pts',(8.57897805299995,15.2,6.98469152199999));
#204571=CARTESIAN_POINT('Ctrl Pts',(8.57897805299995,11.6,6.98469152199999));
#204572=CARTESIAN_POINT('Ctrl Pts',(8.57596392399994,15.2,6.98369472299999));
#204573=CARTESIAN_POINT('Ctrl Pts',(8.57596392399994,11.6,6.98369472299999));
#204574=CARTESIAN_POINT('Ctrl Pts',(8.57295550099994,15.2,6.98269711899999));
#204575=CARTESIAN_POINT('Ctrl Pts',(8.57295550099994,11.6,6.98269711899999));
#204576=CARTESIAN_POINT('Ctrl Pts',(8.56995279099995,15.2,6.98169871899999));
#204577=CARTESIAN_POINT('Ctrl Pts',(8.56995279099995,11.6,6.98169871899999));
#204578=CARTESIAN_POINT('Ctrl Pts',(8.56695579999995,15.2,6.98069953299999));
#204579=CARTESIAN_POINT('Ctrl Pts',(8.56695579999995,11.6,6.98069953299999));
#204580=CARTESIAN_POINT('Ctrl Pts',(8.56396453399995,15.2,6.97969957099998));
#204581=CARTESIAN_POINT('Ctrl Pts',(8.56396453399995,11.6,6.97969957099998));
#204582=CARTESIAN_POINT('Ctrl Pts',(8.56097899899994,15.2,6.97869884199999));
#204583=CARTESIAN_POINT('Ctrl Pts',(8.56097899899994,11.6,6.97869884199999));
#204584=CARTESIAN_POINT('Ctrl Pts',(8.55799920199994,15.2,6.97769735699998));
#204585=CARTESIAN_POINT('Ctrl Pts',(8.55799920199994,11.6,6.97769735699998));
#204586=CARTESIAN_POINT('Ctrl Pts',(8.55502514699995,15.2,6.97669512399998));
#204587=CARTESIAN_POINT('Ctrl Pts',(8.55502514699995,11.6,6.97669512399998));
#204588=CARTESIAN_POINT('Ctrl Pts',(8.55205684399994,15.2,6.97569215299998));
#204589=CARTESIAN_POINT('Ctrl Pts',(8.55205684399994,11.6,6.97569215299998));
#204590=CARTESIAN_POINT('Ctrl Pts',(8.54909429799994,15.2,6.97468845499999));
#204591=CARTESIAN_POINT('Ctrl Pts',(8.54909429799994,11.6,6.97468845499999));
#204592=CARTESIAN_POINT('Ctrl Pts',(8.54613751299994,15.2,6.97368403699999));
#204593=CARTESIAN_POINT('Ctrl Pts',(8.54613751299994,11.6,6.97368403699999));
#204594=CARTESIAN_POINT('Ctrl Pts',(8.54318649699995,15.2,6.97267891199999));
#204595=CARTESIAN_POINT('Ctrl Pts',(8.54318649699995,11.6,6.97267891199999));
#204596=CARTESIAN_POINT('Ctrl Pts',(8.54024125699994,15.2,6.97167308799998));
#204597=CARTESIAN_POINT('Ctrl Pts',(8.54024125699994,11.6,6.97167308799998));
#204598=CARTESIAN_POINT('Ctrl Pts',(8.53730179799994,15.2,6.97066657499998));
#204599=CARTESIAN_POINT('Ctrl Pts',(8.53730179799994,11.6,6.97066657499998));
#204600=CARTESIAN_POINT('Ctrl Pts',(8.53436812699995,15.2,6.96965938299999));
#204601=CARTESIAN_POINT('Ctrl Pts',(8.53436812699995,11.6,6.96965938299999));
#204602=CARTESIAN_POINT('Ctrl Pts',(8.53144025099994,15.2,6.96865152099999));
#204603=CARTESIAN_POINT('Ctrl Pts',(8.53144025099994,11.6,6.96865152099999));
#204604=CARTESIAN_POINT('Ctrl Pts',(8.52851817399995,15.2,6.96764299999998));
#204605=CARTESIAN_POINT('Ctrl Pts',(8.52851817399995,11.6,6.96764299999998));
#204606=CARTESIAN_POINT('Ctrl Pts',(8.52560190399995,15.2,6.96663382999999));
#204607=CARTESIAN_POINT('Ctrl Pts',(8.52560190399995,11.6,6.96663382999999));
#204608=CARTESIAN_POINT('Ctrl Pts',(8.52269144699994,15.2,6.96562401999999));
#204609=CARTESIAN_POINT('Ctrl Pts',(8.52269144699994,11.6,6.96562401999999));
#204610=CARTESIAN_POINT('Ctrl Pts',(8.51978681099994,15.2,6.96461358099998));
#204611=CARTESIAN_POINT('Ctrl Pts',(8.51978681099994,11.6,6.96461358099998));
#204612=CARTESIAN_POINT('Ctrl Pts',(8.51688799999994,15.2,6.96360252199998));
#204613=CARTESIAN_POINT('Ctrl Pts',(8.51688799999994,11.6,6.96360252199998));
#204614=CARTESIAN_POINT('Ctrl Pts',(8.51399501999994,15.2,6.96259085299998));
#204615=CARTESIAN_POINT('Ctrl Pts',(8.51399501999994,11.6,6.96259085299998));
#204616=CARTESIAN_POINT('Ctrl Pts',(8.51110787899995,15.2,6.96157858499999));
#204617=CARTESIAN_POINT('Ctrl Pts',(8.51110787899995,11.6,6.96157858499999));
#204618=CARTESIAN_POINT('Ctrl Pts',(8.50822658299995,15.2,6.96056572799999));
#204619=CARTESIAN_POINT('Ctrl Pts',(8.50822658299995,11.6,6.96056572799999));
#204620=CARTESIAN_POINT('Ctrl Pts',(8.50535113799994,15.2,6.95955229099999));
#204621=CARTESIAN_POINT('Ctrl Pts',(8.50535113799994,11.6,6.95955229099999));
#204622=CARTESIAN_POINT('Ctrl Pts',(8.50248155099994,15.2,6.95853828499998));
#204623=CARTESIAN_POINT('Ctrl Pts',(8.50248155099994,11.6,6.95853828499998));
#204624=CARTESIAN_POINT('Ctrl Pts',(8.49961782799994,15.2,6.95752372099999));
#204625=CARTESIAN_POINT('Ctrl Pts',(8.49961782799994,11.6,6.95752372099999));
#204626=CARTESIAN_POINT('Ctrl Pts',(8.49675997499994,15.2,6.95650860699998));
#204627=CARTESIAN_POINT('Ctrl Pts',(8.49675997499994,11.6,6.95650860699998));
#204628=CARTESIAN_POINT('Ctrl Pts',(8.49390799999994,15.2,6.95549295399999));
#204629=CARTESIAN_POINT('Ctrl Pts',(8.49390799999994,11.6,6.95549295399999));
#204630=CARTESIAN_POINT('Ctrl Pts',(8.49106190599995,15.2,6.95447677399999));
#204631=CARTESIAN_POINT('Ctrl Pts',(8.49106190599995,11.6,6.95447677399999));
#204632=CARTESIAN_POINT('Ctrl Pts',(8.48822170299995,15.2,6.95346007399999));
#204633=CARTESIAN_POINT('Ctrl Pts',(8.48822170299995,11.6,6.95346007399999));
#204634=CARTESIAN_POINT('Ctrl Pts',(8.48538739499994,15.2,6.95244286799999));
#204635=CARTESIAN_POINT('Ctrl Pts',(8.48538739499994,11.6,6.95244286799999));
#204636=CARTESIAN_POINT('Ctrl Pts',(8.48255898999994,15.2,6.95142516299998));
#204637=CARTESIAN_POINT('Ctrl Pts',(8.48255898999994,11.6,6.95142516299998));
#204638=CARTESIAN_POINT('Ctrl Pts',(8.47973649299994,15.2,6.95040697199998));
#204639=CARTESIAN_POINT('Ctrl Pts',(8.47973649299994,11.6,6.95040697199998));
#204640=CARTESIAN_POINT('Ctrl Pts',(8.47691991299994,15.2,6.94938830399998));
#204641=CARTESIAN_POINT('Ctrl Pts',(8.47691991299994,11.6,6.94938830399998));
#204642=CARTESIAN_POINT('Ctrl Pts',(8.47410925299994,15.2,6.94836916899998));
#204643=CARTESIAN_POINT('Ctrl Pts',(8.47410925299994,11.6,6.94836916899998));
#204644=CARTESIAN_POINT('Ctrl Pts',(8.47130452199995,15.2,6.94734957899998));
#204645=CARTESIAN_POINT('Ctrl Pts',(8.47130452199995,11.6,6.94734957899998));
#204646=CARTESIAN_POINT('Ctrl Pts',(8.46850572399994,15.2,6.94632954299998));
#204647=CARTESIAN_POINT('Ctrl Pts',(8.46850572399994,11.6,6.94632954299998));
#204648=CARTESIAN_POINT('Ctrl Pts',(8.46571286899995,15.2,6.94530907199999));
#204649=CARTESIAN_POINT('Ctrl Pts',(8.46571286899995,11.6,6.94530907199999));
#204650=CARTESIAN_POINT('Ctrl Pts',(8.46292595999994,15.2,6.94428817699999));
#204651=CARTESIAN_POINT('Ctrl Pts',(8.46292595999994,11.6,6.94428817699999));
#204652=CARTESIAN_POINT('Ctrl Pts',(8.46014500499994,15.2,6.94326686699998));
#204653=CARTESIAN_POINT('Ctrl Pts',(8.46014500499994,11.6,6.94326686699998));
#204654=CARTESIAN_POINT('Ctrl Pts',(8.45737001099995,15.2,6.94224515399998));
#204655=CARTESIAN_POINT('Ctrl Pts',(8.45737001099995,11.6,6.94224515399998));
#204656=CARTESIAN_POINT('Ctrl Pts',(8.45460098399995,15.2,6.94122304799999));
#204657=CARTESIAN_POINT('Ctrl Pts',(8.45460098399995,11.6,6.94122304799999));
#204658=CARTESIAN_POINT('Ctrl Pts',(8.45183793099994,15.2,6.94020056099999));
#204659=CARTESIAN_POINT('Ctrl Pts',(8.45183793099994,11.6,6.94020056099999));
#204660=CARTESIAN_POINT('Ctrl Pts',(8.44908085599995,15.2,6.93917770199998));
#204661=CARTESIAN_POINT('Ctrl Pts',(8.44908085599995,11.6,6.93917770199998));
#204662=CARTESIAN_POINT('Ctrl Pts',(8.44632976799994,15.2,6.93815448199998));
#204663=CARTESIAN_POINT('Ctrl Pts',(8.44632976799994,11.6,6.93815448199998));
#204664=CARTESIAN_POINT('Ctrl Pts',(8.44358467399994,15.2,6.93713091199999));
#204665=CARTESIAN_POINT('Ctrl Pts',(8.44358467399994,11.6,6.93713091199999));
#204666=CARTESIAN_POINT('Ctrl Pts',(8.44084557799994,15.2,6.93610700299998));
#204667=CARTESIAN_POINT('Ctrl Pts',(8.44084557799994,11.6,6.93610700299998));
#204668=CARTESIAN_POINT('Ctrl Pts',(8.43811248799994,15.2,6.93508276499998));
#204669=CARTESIAN_POINT('Ctrl Pts',(8.43811248799994,11.6,6.93508276499998));
#204670=CARTESIAN_POINT('Ctrl Pts',(8.43538541199995,15.2,6.93405821099999));
#204671=CARTESIAN_POINT('Ctrl Pts',(8.43538541199995,11.6,6.93405821099999));
#204672=CARTESIAN_POINT('Ctrl Pts',(8.43266435299994,15.2,6.93303334799998));
#204673=CARTESIAN_POINT('Ctrl Pts',(8.43266435299994,11.6,6.93303334799998));
#204674=CARTESIAN_POINT('Ctrl Pts',(8.42994932099994,15.2,6.93200819099999));
#204675=CARTESIAN_POINT('Ctrl Pts',(8.42994932099994,11.6,6.93200819099999));
#204676=CARTESIAN_POINT('Ctrl Pts',(8.42724032099994,15.2,6.93098274799999));
#204677=CARTESIAN_POINT('Ctrl Pts',(8.42724032099994,11.6,6.93098274799999));
#204678=CARTESIAN_POINT('Ctrl Pts',(8.42453735899995,15.2,6.92995703099999));
#204679=CARTESIAN_POINT('Ctrl Pts',(8.42453735899995,11.6,6.92995703099999));
#204680=CARTESIAN_POINT('Ctrl Pts',(8.42184044199995,15.2,6.92893105099999));
#204681=CARTESIAN_POINT('Ctrl Pts',(8.42184044199995,11.6,6.92893105099999));
#204682=CARTESIAN_POINT('Ctrl Pts',(8.41914957699995,15.2,6.92790481899999));
#204683=CARTESIAN_POINT('Ctrl Pts',(8.41914957699995,11.6,6.92790481899999));
#204684=CARTESIAN_POINT('Ctrl Pts',(8.41646477099994,15.2,6.92687834499999));
#204685=CARTESIAN_POINT('Ctrl Pts',(8.41646477099994,11.6,6.92687834499999));
#204686=CARTESIAN_POINT('Ctrl Pts',(8.41378603099994,15.2,6.92585164199999));
#204687=CARTESIAN_POINT('Ctrl Pts',(8.41378603099994,11.6,6.92585164199999));
#204688=CARTESIAN_POINT('Ctrl Pts',(8.41111335999994,15.2,6.92482471999998));
#204689=CARTESIAN_POINT('Ctrl Pts',(8.41111335999994,11.6,6.92482471999998));
#204690=CARTESIAN_POINT('Ctrl Pts',(8.40844676899994,15.2,6.92379758999999));
#204691=CARTESIAN_POINT('Ctrl Pts',(8.40844676899994,11.6,6.92379758999999));
#204692=CARTESIAN_POINT('Ctrl Pts',(8.40578626199994,15.2,6.92277026299998));
#204693=CARTESIAN_POINT('Ctrl Pts',(8.40578626199994,11.6,6.92277026299998));
#204694=CARTESIAN_POINT('Ctrl Pts',(8.40313184599994,15.2,6.92174275099998));
#204695=CARTESIAN_POINT('Ctrl Pts',(8.40313184599994,11.6,6.92174275099998));
#204696=CARTESIAN_POINT('Ctrl Pts',(8.40048352899995,15.2,6.92071506499998));
#204697=CARTESIAN_POINT('Ctrl Pts',(8.40048352899995,11.6,6.92071506499998));
#204698=CARTESIAN_POINT('Ctrl Pts',(8.39784131599994,15.2,6.91968721599999));
#204699=CARTESIAN_POINT('Ctrl Pts',(8.39784131599994,11.6,6.91968721599999));
#204700=CARTESIAN_POINT('Ctrl Pts',(8.39520521499994,15.2,6.91865921399998));
#204701=CARTESIAN_POINT('Ctrl Pts',(8.39520521499994,11.6,6.91865921399998));
#204702=CARTESIAN_POINT('Ctrl Pts',(8.39257523199995,15.2,6.91763107399999));
#204703=CARTESIAN_POINT('Ctrl Pts',(8.39257523199995,11.6,6.91763107399999));
#204704=CARTESIAN_POINT('Ctrl Pts',(8.38995137299994,15.2,6.91660280399999));
#204705=CARTESIAN_POINT('Ctrl Pts',(8.38995137299994,11.6,6.91660280399999));
#204706=CARTESIAN_POINT('Ctrl Pts',(8.38733364499994,15.2,6.91557441599999));
#204707=CARTESIAN_POINT('Ctrl Pts',(8.38733364499994,11.6,6.91557441599999));
#204708=CARTESIAN_POINT('Ctrl Pts',(8.38472205599994,15.2,6.91454592099999));
#204709=CARTESIAN_POINT('Ctrl Pts',(8.38472205599994,11.6,6.91454592099999));
#204710=CARTESIAN_POINT('Ctrl Pts',(8.38211660999994,15.2,6.91351733199999));
#204711=CARTESIAN_POINT('Ctrl Pts',(8.38211660999994,11.6,6.91351733199999));
#204712=CARTESIAN_POINT('Ctrl Pts',(8.37951731699994,15.2,6.91248865999999));
#204713=CARTESIAN_POINT('Ctrl Pts',(8.37951731699994,11.6,6.91248865999999));
#204714=CARTESIAN_POINT('Ctrl Pts',(8.37692418099994,15.2,6.91145991599999));
#204715=CARTESIAN_POINT('Ctrl Pts',(8.37692418099994,11.6,6.91145991599999));
#204716=CARTESIAN_POINT('Ctrl Pts',(8.37433721099995,15.2,6.91043111099999));
#204717=CARTESIAN_POINT('Ctrl Pts',(8.37433721099995,11.6,6.91043111099999));
#204718=CARTESIAN_POINT('Ctrl Pts',(8.37175641099994,15.2,6.90940225799999));
#204719=CARTESIAN_POINT('Ctrl Pts',(8.37175641099994,11.6,6.90940225799999));
#204720=CARTESIAN_POINT('Ctrl Pts',(8.36918178899994,15.2,6.90837336799999));
#204721=CARTESIAN_POINT('Ctrl Pts',(8.36918178899994,11.6,6.90837336799999));
#204722=CARTESIAN_POINT('Ctrl Pts',(8.36661335299994,15.2,6.90734445299999));
#204723=CARTESIAN_POINT('Ctrl Pts',(8.36661335299994,11.6,6.90734445299999));
#204724=CARTESIAN_POINT('Ctrl Pts',(8.36405110799994,15.2,6.90631552499998));
#204725=CARTESIAN_POINT('Ctrl Pts',(8.36405110799994,11.6,6.90631552499998));
#204726=CARTESIAN_POINT('Ctrl Pts',(8.36149506199994,15.2,6.90528659299999));
#204727=CARTESIAN_POINT('Ctrl Pts',(8.36149506199994,11.6,6.90528659299999));
#204728=CARTESIAN_POINT('Ctrl Pts',(8.35894522099995,15.2,6.90425767199999));
#204729=CARTESIAN_POINT('Ctrl Pts',(8.35894522099995,11.6,6.90425767199999));
#204730=CARTESIAN_POINT('Ctrl Pts',(8.35640158999994,15.2,6.90322877199999));
#204731=CARTESIAN_POINT('Ctrl Pts',(8.35640158999994,11.6,6.90322877199999));
#204732=CARTESIAN_POINT('Ctrl Pts',(8.35386417999995,15.2,6.90219990599999));
#204733=CARTESIAN_POINT('Ctrl Pts',(8.35386417999995,11.6,6.90219990599999));
#204734=CARTESIAN_POINT('Ctrl Pts',(8.35133299399994,15.2,6.90117108499999));
#204735=CARTESIAN_POINT('Ctrl Pts',(8.35133299399994,11.6,6.90117108499999));
#204736=CARTESIAN_POINT('Ctrl Pts',(8.34880804099994,15.2,6.90014232099998));
#204737=CARTESIAN_POINT('Ctrl Pts',(8.34880804099994,11.6,6.90014232099998));
#204738=CARTESIAN_POINT('Ctrl Pts',(8.34628932799994,15.2,6.89911362499998));
#204739=CARTESIAN_POINT('Ctrl Pts',(8.34628932799994,11.6,6.89911362499998));
#204740=CARTESIAN_POINT('Ctrl Pts',(8.34377685899995,15.2,6.89808501099999));
#204741=CARTESIAN_POINT('Ctrl Pts',(8.34377685899995,11.6,6.89808501099999));
#204742=CARTESIAN_POINT('Ctrl Pts',(8.34127064199994,15.2,6.89705648999999));
#204743=CARTESIAN_POINT('Ctrl Pts',(8.34127064199994,11.6,6.89705648999999));
#204744=CARTESIAN_POINT('Ctrl Pts',(8.33877068699995,15.2,6.89602807399999));
#204745=CARTESIAN_POINT('Ctrl Pts',(8.33877068699995,11.6,6.89602807399999));
#204746=CARTESIAN_POINT('Ctrl Pts',(8.33627699599995,15.2,6.89499977499998));
#204747=CARTESIAN_POINT('Ctrl Pts',(8.33627699599995,11.6,6.89499977499998));
#204748=CARTESIAN_POINT('Ctrl Pts',(8.33378957899994,15.2,6.89397160599999));
#204749=CARTESIAN_POINT('Ctrl Pts',(8.33378957899994,11.6,6.89397160599999));
#204750=CARTESIAN_POINT('Ctrl Pts',(8.33130844099994,15.2,6.89294357699998));
#204751=CARTESIAN_POINT('Ctrl Pts',(8.33130844099994,11.6,6.89294357699998));
#204752=CARTESIAN_POINT('Ctrl Pts',(8.32883359199995,15.2,6.89191570199998));
#204753=CARTESIAN_POINT('Ctrl Pts',(8.32883359199995,11.6,6.89191570199998));
#204754=CARTESIAN_POINT('Ctrl Pts',(8.32636503499994,15.2,6.89088799199999));
#204755=CARTESIAN_POINT('Ctrl Pts',(8.32636503499994,11.6,6.89088799199999));
#204756=CARTESIAN_POINT('Ctrl Pts',(8.32390277799994,15.2,6.88986046099998));
#204757=CARTESIAN_POINT('Ctrl Pts',(8.32390277799994,11.6,6.88986046099998));
#204758=CARTESIAN_POINT('Ctrl Pts',(8.32144682899994,15.2,6.88883311999999));
#204759=CARTESIAN_POINT('Ctrl Pts',(8.32144682899994,11.6,6.88883311999999));
#204760=CARTESIAN_POINT('Ctrl Pts',(8.31899719499994,15.2,6.88780598099999));
#204761=CARTESIAN_POINT('Ctrl Pts',(8.31899719499994,11.6,6.88780598099999));
#204762=CARTESIAN_POINT('Ctrl Pts',(8.31655388099995,15.2,6.88677905699999));
#204763=CARTESIAN_POINT('Ctrl Pts',(8.31655388099995,11.6,6.88677905699999));
#204764=CARTESIAN_POINT('Ctrl Pts',(8.31411689599994,15.2,6.88575236099998));
#204765=CARTESIAN_POINT('Ctrl Pts',(8.31411689599994,11.6,6.88575236099998));
#204766=CARTESIAN_POINT('Ctrl Pts',(8.31168624599994,15.2,6.88472590299998));
#204767=CARTESIAN_POINT('Ctrl Pts',(8.31168624599994,11.6,6.88472590299998));
#204768=CARTESIAN_POINT('Ctrl Pts',(8.30926193799994,15.2,6.88369969999999));
#204769=CARTESIAN_POINT('Ctrl Pts',(8.30926193799994,11.6,6.88369969999999));
#204770=CARTESIAN_POINT('Ctrl Pts',(8.30684397799994,15.2,6.88267375999998));
#204771=CARTESIAN_POINT('Ctrl Pts',(8.30684397799994,11.6,6.88267375999998));
#204772=CARTESIAN_POINT('Ctrl Pts',(8.30443237399994,15.2,6.88164809699998));
#204773=CARTESIAN_POINT('Ctrl Pts',(8.30443237399994,11.6,6.88164809699998));
#204774=CARTESIAN_POINT('Ctrl Pts',(8.30202713399994,15.2,6.88062272299998));
#204775=CARTESIAN_POINT('Ctrl Pts',(8.30202713399994,11.6,6.88062272299998));
#204776=CARTESIAN_POINT('Ctrl Pts',(8.29962826099995,15.2,6.87959765299999));
#204777=CARTESIAN_POINT('Ctrl Pts',(8.29962826099995,11.6,6.87959765299999));
#204778=CARTESIAN_POINT('Ctrl Pts',(8.29723576699994,15.2,6.87857289799998));
#204779=CARTESIAN_POINT('Ctrl Pts',(8.29723576699994,11.6,6.87857289799998));
#204780=CARTESIAN_POINT('Ctrl Pts',(8.29484965599995,15.2,6.87754846999999));
#204781=CARTESIAN_POINT('Ctrl Pts',(8.29484965599995,11.6,6.87754846999999));
#204782=CARTESIAN_POINT('Ctrl Pts',(8.29246993599994,15.2,6.87652438299998));
#204783=CARTESIAN_POINT('Ctrl Pts',(8.29246993599994,11.6,6.87652438299998));
#204784=CARTESIAN_POINT('Ctrl Pts',(8.29009661399994,15.2,6.87550064899998));
#204785=CARTESIAN_POINT('Ctrl Pts',(8.29009661399994,11.6,6.87550064899998));
#204786=CARTESIAN_POINT('Ctrl Pts',(8.28772969499994,15.2,6.87447728199999));
#204787=CARTESIAN_POINT('Ctrl Pts',(8.28772969499994,11.6,6.87447728199999));
#204788=CARTESIAN_POINT('Ctrl Pts',(8.28536918899994,15.2,6.87345429299998));
#204789=CARTESIAN_POINT('Ctrl Pts',(8.28536918899994,11.6,6.87345429299998));
#204790=CARTESIAN_POINT('Ctrl Pts',(8.28301510099994,15.2,6.87243169599999));
#204791=CARTESIAN_POINT('Ctrl Pts',(8.28301510099994,11.6,6.87243169599999));
#204792=CARTESIAN_POINT('Ctrl Pts',(8.28066743899995,15.2,6.87140950299998));
#204793=CARTESIAN_POINT('Ctrl Pts',(8.28066743899995,11.6,6.87140950299998));
#204794=CARTESIAN_POINT('Ctrl Pts',(8.27832620999994,15.2,6.87038772899999));
#204795=CARTESIAN_POINT('Ctrl Pts',(8.27832620999994,11.6,6.87038772899999));
#204796=CARTESIAN_POINT('Ctrl Pts',(8.27599141999994,15.2,6.86936638599998));
#204797=CARTESIAN_POINT('Ctrl Pts',(8.27599141999994,11.6,6.86936638599998));
#204798=CARTESIAN_POINT('Ctrl Pts',(8.27366307799995,15.2,6.86834548599998));
#204799=CARTESIAN_POINT('Ctrl Pts',(8.27366307799995,11.6,6.86834548599998));
#204800=CARTESIAN_POINT('Ctrl Pts',(8.27134118899994,15.2,6.86732504299999));
#204801=CARTESIAN_POINT('Ctrl Pts',(8.27134118899994,11.6,6.86732504299999));
#204802=CARTESIAN_POINT('Ctrl Pts',(8.26902576199994,15.2,6.86630506999999));
#204803=CARTESIAN_POINT('Ctrl Pts',(8.26902576199994,11.6,6.86630506999999));
#204804=CARTESIAN_POINT('Ctrl Pts',(8.26671680299994,15.2,6.86528557999999));
#204805=CARTESIAN_POINT('Ctrl Pts',(8.26671680299994,11.6,6.86528557999999));
#204806=CARTESIAN_POINT('Ctrl Pts',(8.26441431799994,15.2,6.86426658699999));
#204807=CARTESIAN_POINT('Ctrl Pts',(8.26441431799994,11.6,6.86426658699999));
#204808=CARTESIAN_POINT('Ctrl Pts',(8.26211831599995,15.2,6.86324810299999));
#204809=CARTESIAN_POINT('Ctrl Pts',(8.26211831599995,11.6,6.86324810299999));
#204810=CARTESIAN_POINT('Ctrl Pts',(8.25982880499994,15.2,6.86223014299999));
#204811=CARTESIAN_POINT('Ctrl Pts',(8.25982880499994,11.6,6.86223014299999));
#204812=CARTESIAN_POINT('Ctrl Pts',(8.25754578899994,15.2,6.86121271799998));
#204813=CARTESIAN_POINT('Ctrl Pts',(8.25754578899994,11.6,6.86121271799998));
#204814=CARTESIAN_POINT('Ctrl Pts',(8.25526927699994,15.2,6.86019584399999));
#204815=CARTESIAN_POINT('Ctrl Pts',(8.25526927699994,11.6,6.86019584399999));
#204816=CARTESIAN_POINT('Ctrl Pts',(8.25299927599995,15.2,6.85917953199999));
#204817=CARTESIAN_POINT('Ctrl Pts',(8.25299927599995,11.6,6.85917953199999));
#204818=CARTESIAN_POINT('Ctrl Pts',(8.25073579299995,15.2,6.85816379699999));
#204819=CARTESIAN_POINT('Ctrl Pts',(8.25073579299995,11.6,6.85816379699999));
#204820=CARTESIAN_POINT('Ctrl Pts',(8.24847883499995,15.2,6.85714865199999));
#204821=CARTESIAN_POINT('Ctrl Pts',(8.24847883499995,11.6,6.85714865199999));
#204822=CARTESIAN_POINT('Ctrl Pts',(8.24622840999995,15.2,6.85613411099999));
#204823=CARTESIAN_POINT('Ctrl Pts',(8.24622840999995,11.6,6.85613411099999));
#204824=CARTESIAN_POINT('Ctrl Pts',(8.24398452499995,15.2,6.85512018699999));
#204825=CARTESIAN_POINT('Ctrl Pts',(8.24398452499995,11.6,6.85512018699999));
#204826=CARTESIAN_POINT('Ctrl Pts',(8.24174718699994,15.2,6.85410689399998));
#204827=CARTESIAN_POINT('Ctrl Pts',(8.24174718699994,11.6,6.85410689399998));
#204828=CARTESIAN_POINT('Ctrl Pts',(8.23951640199994,15.2,6.85309424599998));
#204829=CARTESIAN_POINT('Ctrl Pts',(8.23951640199994,11.6,6.85309424599998));
#204830=CARTESIAN_POINT('Ctrl Pts',(8.23729217799994,15.2,6.85208225499998));
#204831=CARTESIAN_POINT('Ctrl Pts',(8.23729217799994,11.6,6.85208225499998));
#204832=CARTESIAN_POINT('Ctrl Pts',(8.23507452399994,15.2,6.85107093599999));
#204833=CARTESIAN_POINT('Ctrl Pts',(8.23507452399994,11.6,6.85107093599999));
#204834=CARTESIAN_POINT('Ctrl Pts',(8.23286344499994,15.2,6.85006030399999));
#204835=CARTESIAN_POINT('Ctrl Pts',(8.23286344499994,11.6,6.85006030399999));
#204836=CARTESIAN_POINT('Ctrl Pts',(8.23065894899995,15.2,6.84905037099998));
#204837=CARTESIAN_POINT('Ctrl Pts',(8.23065894899995,11.6,6.84905037099998));
#204838=CARTESIAN_POINT('Ctrl Pts',(8.22846104299994,15.2,6.84804115099999));
#204839=CARTESIAN_POINT('Ctrl Pts',(8.22846104299994,11.6,6.84804115099999));
#204840=CARTESIAN_POINT('Ctrl Pts',(8.22626973499995,15.2,6.84703266099999));
#204841=CARTESIAN_POINT('Ctrl Pts',(8.22626973499995,11.6,6.84703266099999));
#204842=CARTESIAN_POINT('Ctrl Pts',(8.22408503299994,15.2,6.84602490999998));
#204843=CARTESIAN_POINT('Ctrl Pts',(8.22408503299994,11.6,6.84602490999998));
#204844=CARTESIAN_POINT('Ctrl Pts',(8.22190694099995,15.2,6.84501791499999));
#204845=CARTESIAN_POINT('Ctrl Pts',(8.22190694099995,11.6,6.84501791499999));
#204846=CARTESIAN_POINT('Ctrl Pts',(8.21973547099994,15.2,6.84401169099999));
#204847=CARTESIAN_POINT('Ctrl Pts',(8.21973547099994,11.6,6.84401169099999));
#204848=CARTESIAN_POINT('Ctrl Pts',(8.21757062599995,15.2,6.84300624899999));
#204849=CARTESIAN_POINT('Ctrl Pts',(8.21757062599995,11.6,6.84300624899999));
#204850=CARTESIAN_POINT('Ctrl Pts',(8.21541241599994,15.2,6.84200160599998));
#204851=CARTESIAN_POINT('Ctrl Pts',(8.21541241599994,11.6,6.84200160599998));
#204852=CARTESIAN_POINT('Ctrl Pts',(8.21326084699994,15.2,6.84099777499998));
#204853=CARTESIAN_POINT('Ctrl Pts',(8.21326084699994,11.6,6.84099777499998));
#204854=CARTESIAN_POINT('Ctrl Pts',(8.21111592699994,15.2,6.83999476999999));
#204855=CARTESIAN_POINT('Ctrl Pts',(8.21111592699994,11.6,6.83999476999999));
#204856=CARTESIAN_POINT('Ctrl Pts',(8.20897766399994,15.2,6.83899260599999));
#204857=CARTESIAN_POINT('Ctrl Pts',(8.20897766399994,11.6,6.83899260599999));
#204858=CARTESIAN_POINT('Ctrl Pts',(8.20684606299995,15.2,6.83799129599999));
#204859=CARTESIAN_POINT('Ctrl Pts',(8.20684606299995,11.6,6.83799129599999));
#204860=CARTESIAN_POINT('Ctrl Pts',(8.20472113499994,15.2,6.83699085699998));
#204861=CARTESIAN_POINT('Ctrl Pts',(8.20472113499994,11.6,6.83699085699998));
#204862=CARTESIAN_POINT('Ctrl Pts',(8.20260288499994,15.2,6.83599130199998));
#204863=CARTESIAN_POINT('Ctrl Pts',(8.20260288499994,11.6,6.83599130199998));
#204864=CARTESIAN_POINT('Ctrl Pts',(8.20049131999994,15.2,6.83499264399998));
#204865=CARTESIAN_POINT('Ctrl Pts',(8.20049131999994,11.6,6.83499264399998));
#204866=CARTESIAN_POINT('Ctrl Pts',(8.19838644899994,15.2,6.83399490099998));
#204867=CARTESIAN_POINT('Ctrl Pts',(8.19838644899994,11.6,6.83399490099998));
#204868=CARTESIAN_POINT('Ctrl Pts',(8.19628827799994,15.2,6.83299808399998));
#204869=CARTESIAN_POINT('Ctrl Pts',(8.19628827799994,11.6,6.83299808399998));
#204870=CARTESIAN_POINT('Ctrl Pts',(8.19419681699994,15.2,6.83200220999999));
#204871=CARTESIAN_POINT('Ctrl Pts',(8.19419681699994,11.6,6.83200220999999));
#204872=CARTESIAN_POINT('Ctrl Pts',(8.19211206999995,15.2,6.83100729199998));
#204873=CARTESIAN_POINT('Ctrl Pts',(8.19211206999995,11.6,6.83100729199998));
#204874=CARTESIAN_POINT('Ctrl Pts',(8.19003404699994,15.2,6.83001334599999));
#204875=CARTESIAN_POINT('Ctrl Pts',(8.19003404699994,11.6,6.83001334599999));
#204876=CARTESIAN_POINT('Ctrl Pts',(8.18796275399994,15.2,6.82902038599998));
#204877=CARTESIAN_POINT('Ctrl Pts',(8.18796275399994,11.6,6.82902038599998));
#204878=CARTESIAN_POINT('Ctrl Pts',(8.18589819999995,15.2,6.82802842899999));
#204879=CARTESIAN_POINT('Ctrl Pts',(8.18589819999995,11.6,6.82802842899999));
#204880=CARTESIAN_POINT('Ctrl Pts',(8.18384039099995,15.2,6.82703748699999));
#204881=CARTESIAN_POINT('Ctrl Pts',(8.18384039099995,11.6,6.82703748699999));
#204882=CARTESIAN_POINT('Ctrl Pts',(8.18178933599994,15.2,6.82604757499998));
#204883=CARTESIAN_POINT('Ctrl Pts',(8.18178933599994,11.6,6.82604757499998));
#204884=CARTESIAN_POINT('Ctrl Pts',(8.17974504099995,15.2,6.82505870999999));
#204885=CARTESIAN_POINT('Ctrl Pts',(8.17974504099995,11.6,6.82505870999999));
#204886=CARTESIAN_POINT('Ctrl Pts',(8.17770751499994,15.2,6.82407090699999));
#204887=CARTESIAN_POINT('Ctrl Pts',(8.17770751499994,11.6,6.82407090699999));
#204888=CARTESIAN_POINT('Ctrl Pts',(8.17567676399995,15.2,6.82308417899999));
#204889=CARTESIAN_POINT('Ctrl Pts',(8.17567676399995,11.6,6.82308417899999));
#204890=CARTESIAN_POINT('Ctrl Pts',(8.17365279699995,15.2,6.82209854299998));
#204891=CARTESIAN_POINT('Ctrl Pts',(8.17365279699995,11.6,6.82209854299998));
#204892=CARTESIAN_POINT('Ctrl Pts',(8.17163562099994,15.2,6.82111401199998));
#204893=CARTESIAN_POINT('Ctrl Pts',(8.17163562099994,11.6,6.82111401199998));
#204894=CARTESIAN_POINT('Ctrl Pts',(8.16962524399995,15.2,6.82013060399999));
#204895=CARTESIAN_POINT('Ctrl Pts',(8.16962524399995,11.6,6.82013060399999));
#204896=CARTESIAN_POINT('Ctrl Pts',(8.16762167299995,15.2,6.81914833299999));
#204897=CARTESIAN_POINT('Ctrl Pts',(8.16762167299995,11.6,6.81914833299999));
#204898=CARTESIAN_POINT('Ctrl Pts',(8.16562491599995,15.2,6.81816721399999));
#204899=CARTESIAN_POINT('Ctrl Pts',(8.16562491599995,11.6,6.81816721399999));
#204900=CARTESIAN_POINT('Ctrl Pts',(8.16363497999994,15.2,6.81718726399998));
#204901=CARTESIAN_POINT('Ctrl Pts',(8.16363497999994,11.6,6.81718726399998));
#204902=CARTESIAN_POINT('Ctrl Pts',(8.16165187399994,15.2,6.81620849599998));
#204903=CARTESIAN_POINT('Ctrl Pts',(8.16165187399994,11.6,6.81620849599998));
#204904=CARTESIAN_POINT('Ctrl Pts',(8.15967560399995,15.2,6.81523092699998));
#204905=CARTESIAN_POINT('Ctrl Pts',(8.15967560399995,11.6,6.81523092699998));
#204906=CARTESIAN_POINT('Ctrl Pts',(8.15770618099994,15.2,6.81425457199998));
#204907=CARTESIAN_POINT('Ctrl Pts',(8.15770618099994,11.6,6.81425457199998));
#204908=CARTESIAN_POINT('Ctrl Pts',(8.15574360699994,15.2,6.81327944699999));
#204909=CARTESIAN_POINT('Ctrl Pts',(8.15574360699994,11.6,6.81327944699999));
#204910=CARTESIAN_POINT('Ctrl Pts',(8.15378789499994,15.2,6.81230556799999));
#204911=CARTESIAN_POINT('Ctrl Pts',(8.15378789499994,11.6,6.81230556799999));
#204912=CARTESIAN_POINT('Ctrl Pts',(8.15183904999994,15.2,6.81133294999999));
#204913=CARTESIAN_POINT('Ctrl Pts',(8.15183904999994,11.6,6.81133294999999));
#204914=CARTESIAN_POINT('Ctrl Pts',(8.14989708099995,15.2,6.81036160899998));
#204915=CARTESIAN_POINT('Ctrl Pts',(8.14989708099995,11.6,6.81036160899998));
#204916=CARTESIAN_POINT('Ctrl Pts',(8.14796199499994,15.2,6.80939156099999));
#204917=CARTESIAN_POINT('Ctrl Pts',(8.14796199499994,11.6,6.80939156099999));
#204918=CARTESIAN_POINT('Ctrl Pts',(8.14603379999994,15.2,6.80842282199999));
#204919=CARTESIAN_POINT('Ctrl Pts',(8.14603379999994,11.6,6.80842282199999));
#204920=CARTESIAN_POINT('Ctrl Pts',(8.14411250399995,15.2,6.80745540699998));
#204921=CARTESIAN_POINT('Ctrl Pts',(8.14411250399995,11.6,6.80745540699998));
#204922=CARTESIAN_POINT('Ctrl Pts',(8.14219811399994,15.2,6.80648933399999));
#204923=CARTESIAN_POINT('Ctrl Pts',(8.14219811399994,11.6,6.80648933399999));
#204924=CARTESIAN_POINT('Ctrl Pts',(8.14029063899994,15.2,6.80552461599999));
#204925=CARTESIAN_POINT('Ctrl Pts',(8.14029063899994,11.6,6.80552461599999));
#204926=CARTESIAN_POINT('Ctrl Pts',(8.13839008599994,15.2,6.80456127199999));
#204927=CARTESIAN_POINT('Ctrl Pts',(8.13839008599994,11.6,6.80456127199999));
#204928=CARTESIAN_POINT('Ctrl Pts',(8.13649646199995,15.2,6.80359931699999));
#204929=CARTESIAN_POINT('Ctrl Pts',(8.13649646199995,11.6,6.80359931699999));
#204930=CARTESIAN_POINT('Ctrl Pts',(8.13460977799994,15.2,6.80263876599999));
#204931=CARTESIAN_POINT('Ctrl Pts',(8.13460977799994,11.6,6.80263876599999));
#204932=CARTESIAN_POINT('Ctrl Pts',(8.13273003799994,15.2,6.80167963699999));
#204933=CARTESIAN_POINT('Ctrl Pts',(8.13273003799994,11.6,6.80167963699999));
#204934=CARTESIAN_POINT('Ctrl Pts',(8.13085725199995,15.2,6.80072194599998));
#204935=CARTESIAN_POINT('Ctrl Pts',(8.13085725199995,11.6,6.80072194599998));
#204936=CARTESIAN_POINT('Ctrl Pts',(8.12899142799994,15.2,6.79976570899999));
#204937=CARTESIAN_POINT('Ctrl Pts',(8.12899142799994,11.6,6.79976570899999));
#204938=CARTESIAN_POINT('Ctrl Pts',(8.12713257399994,15.2,6.79881094299999));
#204939=CARTESIAN_POINT('Ctrl Pts',(8.12713257399994,11.6,6.79881094299999));
#204940=CARTESIAN_POINT('Ctrl Pts',(8.12528069599994,15.2,6.79785766399998));
#204941=CARTESIAN_POINT('Ctrl Pts',(8.12528069599994,11.6,6.79785766399998));
#204942=CARTESIAN_POINT('Ctrl Pts',(8.12343580399994,15.2,6.79690588799998));
#204943=CARTESIAN_POINT('Ctrl Pts',(8.12343580399994,11.6,6.79690588799998));
#204944=CARTESIAN_POINT('Ctrl Pts',(8.12159790499994,15.2,6.79595563299999));
#204945=CARTESIAN_POINT('Ctrl Pts',(8.12159790499994,11.6,6.79595563299999));
#204946=CARTESIAN_POINT('Ctrl Pts',(8.11976700799995,15.2,6.79500691499998));
#204947=CARTESIAN_POINT('Ctrl Pts',(8.11976700799995,11.6,6.79500691499998));
#204948=CARTESIAN_POINT('Ctrl Pts',(8.11794311899994,15.2,6.79405974999998));
#204949=CARTESIAN_POINT('Ctrl Pts',(8.11794311899994,11.6,6.79405974999998));
#204950=CARTESIAN_POINT('Ctrl Pts',(8.11612624899994,15.2,6.79311415699999));
#204951=CARTESIAN_POINT('Ctrl Pts',(8.11612624899994,11.6,6.79311415699999));
#204952=CARTESIAN_POINT('Ctrl Pts',(8.11431640299995,15.2,6.79217015099999));
#204953=CARTESIAN_POINT('Ctrl Pts',(8.11431640299995,11.6,6.79217015099999));
#204954=CARTESIAN_POINT('Ctrl Pts',(8.11251358999994,15.2,6.79122774899999));
#204955=CARTESIAN_POINT('Ctrl Pts',(8.11251358999994,11.6,6.79122774899999));
#204956=CARTESIAN_POINT('Ctrl Pts',(8.11071781999994,15.2,6.79028696799998));
#204957=CARTESIAN_POINT('Ctrl Pts',(8.11071781999994,11.6,6.79028696799998));
#204958=CARTESIAN_POINT('Ctrl Pts',(8.10892909899994,15.2,6.78934782499999));
#204959=CARTESIAN_POINT('Ctrl Pts',(8.10892909899994,11.6,6.78934782499999));
#204960=CARTESIAN_POINT('Ctrl Pts',(8.10714743499994,15.2,6.78841033799999));
#204961=CARTESIAN_POINT('Ctrl Pts',(8.10714743499994,11.6,6.78841033799999));
#204962=CARTESIAN_POINT('Ctrl Pts',(8.10537283599994,15.2,6.78747452299999));
#204963=CARTESIAN_POINT('Ctrl Pts',(8.10537283599994,11.6,6.78747452299999));
#204964=CARTESIAN_POINT('Ctrl Pts',(8.10360531199994,15.2,6.78654039899998));
#204965=CARTESIAN_POINT('Ctrl Pts',(8.10360531199994,11.6,6.78654039899998));
#204966=CARTESIAN_POINT('Ctrl Pts',(8.10184486799994,15.2,6.78560798099999));
#204967=CARTESIAN_POINT('Ctrl Pts',(8.10184486799994,11.6,6.78560798099999));
#204968=CARTESIAN_POINT('Ctrl Pts',(8.10009151599994,15.2,6.78467728899999));
#204969=CARTESIAN_POINT('Ctrl Pts',(8.10009151599994,11.6,6.78467728899999));
#204970=CARTESIAN_POINT('Ctrl Pts',(8.09834526099994,15.2,6.78374833799998));
#204971=CARTESIAN_POINT('Ctrl Pts',(8.09834526099994,11.6,6.78374833799998));
#204972=CARTESIAN_POINT('Ctrl Pts',(8.09660611299994,15.2,6.78282114599998));
#204973=CARTESIAN_POINT('Ctrl Pts',(8.09660611299994,11.6,6.78282114599998));
#204974=CARTESIAN_POINT('Ctrl Pts',(8.09487407999994,15.2,6.78189573099999));
#204975=CARTESIAN_POINT('Ctrl Pts',(8.09487407999994,11.6,6.78189573099999));
#204976=CARTESIAN_POINT('Ctrl Pts',(8.09314916899995,15.2,6.78097211099999));
#204977=CARTESIAN_POINT('Ctrl Pts',(8.09314916899995,11.6,6.78097211099999));
#204978=CARTESIAN_POINT('Ctrl Pts',(8.09143138899995,15.2,6.78005030299998));
#204979=CARTESIAN_POINT('Ctrl Pts',(8.09143138899995,11.6,6.78005030299998));
#204980=CARTESIAN_POINT('Ctrl Pts',(8.08972074799994,15.2,6.77913032599999));
#204981=CARTESIAN_POINT('Ctrl Pts',(8.08972074799994,11.6,6.77913032599999));
#204982=CARTESIAN_POINT('Ctrl Pts',(8.08801725499994,15.2,6.77821219599998));
#204983=CARTESIAN_POINT('Ctrl Pts',(8.08801725499994,11.6,6.77821219599998));
#204984=CARTESIAN_POINT('Ctrl Pts',(8.08632091699995,15.2,6.77729592999999));
#204985=CARTESIAN_POINT('Ctrl Pts',(8.08632091699995,11.6,6.77729592999999));
#204986=CARTESIAN_POINT('Ctrl Pts',(8.08463174399994,15.2,6.77638154999999));
#204987=CARTESIAN_POINT('Ctrl Pts',(8.08463174399994,11.6,6.77638154999999));
#204988=CARTESIAN_POINT('Ctrl Pts',(8.08294974399994,15.2,6.77546907099998));
#204989=CARTESIAN_POINT('Ctrl Pts',(8.08294974399994,11.6,6.77546907099998));
#204990=CARTESIAN_POINT('Ctrl Pts',(8.08127492299995,15.2,6.77455851099998));
#204991=CARTESIAN_POINT('Ctrl Pts',(8.08127492299995,11.6,6.77455851099998));
#204992=CARTESIAN_POINT('Ctrl Pts',(8.07960729299994,15.2,6.77364988999998));
#204993=CARTESIAN_POINT('Ctrl Pts',(8.07960729299994,11.6,6.77364988999998));
#204994=CARTESIAN_POINT('Ctrl Pts',(8.07794685899994,15.2,6.77274322499999));
#204995=CARTESIAN_POINT('Ctrl Pts',(8.07794685899994,11.6,6.77274322499999));
#204996=CARTESIAN_POINT('Ctrl Pts',(8.07629363199995,15.2,6.77183853299999));
#204997=CARTESIAN_POINT('Ctrl Pts',(8.07629363199995,11.6,6.77183853299999));
#204998=CARTESIAN_POINT('Ctrl Pts',(8.07464761799995,15.2,6.77093583499998));
#204999=CARTESIAN_POINT('Ctrl Pts',(8.07464761799995,11.6,6.77093583499998));
#205000=CARTESIAN_POINT('Ctrl Pts',(8.07300882799994,15.2,6.77003514799999));
#205001=CARTESIAN_POINT('Ctrl Pts',(8.07300882799994,11.6,6.77003514799999));
#205002=CARTESIAN_POINT('Ctrl Pts',(8.07137726799994,15.2,6.76913649099999));
#205003=CARTESIAN_POINT('Ctrl Pts',(8.07137726799994,11.6,6.76913649099999));
#205004=CARTESIAN_POINT('Ctrl Pts',(8.06975294899994,15.2,6.76823988099999));
#205005=CARTESIAN_POINT('Ctrl Pts',(8.06975294899994,11.6,6.76823988099999));
#205006=CARTESIAN_POINT('Ctrl Pts',(8.06813587699994,15.2,6.76734533899998));
#205007=CARTESIAN_POINT('Ctrl Pts',(8.06813587699994,11.6,6.76734533899998));
#205008=CARTESIAN_POINT('Ctrl Pts',(8.06652606199994,15.2,6.76645288099999));
#205009=CARTESIAN_POINT('Ctrl Pts',(8.06652606199994,11.6,6.76645288099999));
#205010=CARTESIAN_POINT('Ctrl Pts',(8.06492351199994,15.2,6.76556252899999));
#205011=CARTESIAN_POINT('Ctrl Pts',(8.06492351199994,11.6,6.76556252899999));
#205012=CARTESIAN_POINT('Ctrl Pts',(8.06332823499995,15.2,6.76467429899999));
#205013=CARTESIAN_POINT('Ctrl Pts',(8.06332823499995,11.6,6.76467429899999));
#205014=CARTESIAN_POINT('Ctrl Pts',(8.06174024099995,15.2,6.76378821199999));
#205015=CARTESIAN_POINT('Ctrl Pts',(8.06174024099995,11.6,6.76378821199999));
#205016=CARTESIAN_POINT('Ctrl Pts',(8.06015953799994,15.2,6.76290428499998));
#205017=CARTESIAN_POINT('Ctrl Pts',(8.06015953799994,11.6,6.76290428499998));
#205018=CARTESIAN_POINT('Ctrl Pts',(8.05858613399994,15.2,6.76202253899999));
#205019=CARTESIAN_POINT('Ctrl Pts',(8.05858613399994,11.6,6.76202253899999));
#205020=CARTESIAN_POINT('Ctrl Pts',(8.05702003799994,15.2,6.76114299299999));
#205021=CARTESIAN_POINT('Ctrl Pts',(8.05702003799994,11.6,6.76114299299999));
#205022=CARTESIAN_POINT('Ctrl Pts',(8.05546125799994,15.2,6.76026566499999));
#205023=CARTESIAN_POINT('Ctrl Pts',(8.05546125799994,11.6,6.76026566499999));
#205024=CARTESIAN_POINT('Ctrl Pts',(8.05390980499994,15.2,6.75939057399999));
#205025=CARTESIAN_POINT('Ctrl Pts',(8.05390980499994,11.6,6.75939057399999));
#205026=CARTESIAN_POINT('Ctrl Pts',(8.05236568499994,15.2,6.75851773999998));
#205027=CARTESIAN_POINT('Ctrl Pts',(8.05236568499994,11.6,6.75851773999998));
#205028=CARTESIAN_POINT('Ctrl Pts',(8.05082890799994,15.2,6.75764718399999));
#205029=CARTESIAN_POINT('Ctrl Pts',(8.05082890799994,11.6,6.75764718399999));
#205030=CARTESIAN_POINT('Ctrl Pts',(8.04929948099995,15.2,6.75677892399998));
#205031=CARTESIAN_POINT('Ctrl Pts',(8.04929948099995,11.6,6.75677892399998));
#205032=CARTESIAN_POINT('Ctrl Pts',(8.04777741499995,15.2,6.75591297799999));
#205033=CARTESIAN_POINT('Ctrl Pts',(8.04777741499995,11.6,6.75591297799999));
#205034=CARTESIAN_POINT('Ctrl Pts',(8.04626271799994,15.2,6.75504936999998));
#205035=CARTESIAN_POINT('Ctrl Pts',(8.04626271799994,11.6,6.75504936999998));
#205036=CARTESIAN_POINT('Ctrl Pts',(8.04475539899994,15.2,6.75418811499998));
#205037=CARTESIAN_POINT('Ctrl Pts',(8.04475539899994,11.6,6.75418811499998));
#205038=CARTESIAN_POINT('Ctrl Pts',(8.04325546599994,15.2,6.75332923599999));
#205039=CARTESIAN_POINT('Ctrl Pts',(8.04325546599994,11.6,6.75332923599999));
#205040=CARTESIAN_POINT('Ctrl Pts',(8.04176292899994,15.2,6.75247275199998));
#205041=CARTESIAN_POINT('Ctrl Pts',(8.04176292899994,11.6,6.75247275199998));
#205042=CARTESIAN_POINT('Ctrl Pts',(8.04027779499994,15.2,6.75161868299998));
#205043=CARTESIAN_POINT('Ctrl Pts',(8.04027779499994,11.6,6.75161868299998));
#205044=CARTESIAN_POINT('Ctrl Pts',(8.03880007499994,15.2,6.75076704899999));
#205045=CARTESIAN_POINT('Ctrl Pts',(8.03880007499994,11.6,6.75076704899999));
#205046=CARTESIAN_POINT('Ctrl Pts',(8.03732977699994,15.2,6.74991786899999));
#205047=CARTESIAN_POINT('Ctrl Pts',(8.03732977699994,11.6,6.74991786899999));
#205048=CARTESIAN_POINT('Ctrl Pts',(8.03586690899994,15.2,6.74907116499998));
#205049=CARTESIAN_POINT('Ctrl Pts',(8.03586690899994,11.6,6.74907116499998));
#205050=CARTESIAN_POINT('Ctrl Pts',(8.03441148099994,15.2,6.74822695799998));
#205051=CARTESIAN_POINT('Ctrl Pts',(8.03441148099994,11.6,6.74822695799998));
#205052=CARTESIAN_POINT('Ctrl Pts',(8.03296350099994,15.2,6.74738526499999));
#205053=CARTESIAN_POINT('Ctrl Pts',(8.03296350099994,11.6,6.74738526499999));
#205054=CARTESIAN_POINT('Ctrl Pts',(8.03152297999995,15.2,6.74654610999998));
#205055=CARTESIAN_POINT('Ctrl Pts',(8.03152297999995,11.6,6.74654610999998));
#205056=CARTESIAN_POINT('Ctrl Pts',(8.03008992399995,15.2,6.74570951199998));
#205057=CARTESIAN_POINT('Ctrl Pts',(8.03008992399995,11.6,6.74570951199998));
#205058=CARTESIAN_POINT('Ctrl Pts',(8.02866434499995,15.2,6.74487549099998));
#205059=CARTESIAN_POINT('Ctrl Pts',(8.02866434499995,11.6,6.74487549099998));
#205060=CARTESIAN_POINT('Ctrl Pts',(8.02724624999994,15.2,6.74404406999999));
#205061=CARTESIAN_POINT('Ctrl Pts',(8.02724624999994,11.6,6.74404406999999));
#205062=CARTESIAN_POINT('Ctrl Pts',(8.02583564899994,15.2,6.74321526699998));
#205063=CARTESIAN_POINT('Ctrl Pts',(8.02583564899994,11.6,6.74321526699998));
#205064=CARTESIAN_POINT('Ctrl Pts',(8.02443255099995,15.2,6.74238910499999));
#205065=CARTESIAN_POINT('Ctrl Pts',(8.02443255099995,11.6,6.74238910499999));
#205066=CARTESIAN_POINT('Ctrl Pts',(8.02303696499994,15.2,6.74156560299998));
#205067=CARTESIAN_POINT('Ctrl Pts',(8.02303696499994,11.6,6.74156560299998));
#205068=CARTESIAN_POINT('Ctrl Pts',(8.02164889999995,15.2,6.74074478499998));
#205069=CARTESIAN_POINT('Ctrl Pts',(8.02164889999995,11.6,6.74074478499998));
#205070=CARTESIAN_POINT('Ctrl Pts',(8.02026836499994,15.2,6.73992666999998));
#205071=CARTESIAN_POINT('Ctrl Pts',(8.02026836499994,11.6,6.73992666999998));
#205072=CARTESIAN_POINT('Ctrl Pts',(8.01889536899994,15.2,6.73911127899999));
#205073=CARTESIAN_POINT('Ctrl Pts',(8.01889536899994,11.6,6.73911127899999));
#205074=CARTESIAN_POINT('Ctrl Pts',(8.01752992299994,15.2,6.73829863499999));
#205075=CARTESIAN_POINT('Ctrl Pts',(8.01752992299994,11.6,6.73829863499999));
#205076=CARTESIAN_POINT('Ctrl Pts',(8.01617203399994,15.2,6.73748875799999));
#205077=CARTESIAN_POINT('Ctrl Pts',(8.01617203399994,11.6,6.73748875799999));
#205078=CARTESIAN_POINT('Ctrl Pts',(8.01482171199994,15.2,6.73668166999998));
#205079=CARTESIAN_POINT('Ctrl Pts',(8.01482171199994,11.6,6.73668166999998));
#205080=CARTESIAN_POINT('Ctrl Pts',(8.01347896699994,15.2,6.73587739199998));
#205081=CARTESIAN_POINT('Ctrl Pts',(8.01347896699994,11.6,6.73587739199998));
#205082=CARTESIAN_POINT('Ctrl Pts',(8.01214380699994,15.2,6.73507594799998));
#205083=CARTESIAN_POINT('Ctrl Pts',(8.01214380699994,11.6,6.73507594799998));
#205084=CARTESIAN_POINT('Ctrl Pts',(8.01081624199995,15.2,6.73427735699998));
#205085=CARTESIAN_POINT('Ctrl Pts',(8.01081624199995,11.6,6.73427735699998));
#205086=CARTESIAN_POINT('Ctrl Pts',(8.00949628099995,15.2,6.73348164099998));
#205087=CARTESIAN_POINT('Ctrl Pts',(8.00949628099995,11.6,6.73348164099998));
#205088=CARTESIAN_POINT('Ctrl Pts',(8.00818393499994,15.2,6.73268882499999));
#205089=CARTESIAN_POINT('Ctrl Pts',(8.00818393499994,11.6,6.73268882499999));
#205090=CARTESIAN_POINT('Ctrl Pts',(8.00687921199994,15.2,6.73189892799999));
#205091=CARTESIAN_POINT('Ctrl Pts',(8.00687921199994,11.6,6.73189892799999));
#205092=CARTESIAN_POINT('Ctrl Pts',(8.00558212099994,15.2,6.73111197299999));
#205093=CARTESIAN_POINT('Ctrl Pts',(8.00558212099994,11.6,6.73111197299999));
#205094=CARTESIAN_POINT('Ctrl Pts',(8.00429267199994,15.2,6.73032798199999));
#205095=CARTESIAN_POINT('Ctrl Pts',(8.00429267199994,11.6,6.73032798199999));
#205096=CARTESIAN_POINT('Ctrl Pts',(8.00301087399994,15.2,6.72954697899999));
#205097=CARTESIAN_POINT('Ctrl Pts',(8.00301087399994,11.6,6.72954697899999));
#205098=CARTESIAN_POINT('Ctrl Pts',(8.00173673799994,15.2,6.72876898499998));
#205099=CARTESIAN_POINT('Ctrl Pts',(8.00173673799994,11.6,6.72876898499998));
#205100=CARTESIAN_POINT('Ctrl Pts',(8.00047027299994,15.2,6.72799402299999));
#205101=CARTESIAN_POINT('Ctrl Pts',(8.00047027299994,11.6,6.72799402299999));
#205102=CARTESIAN_POINT('Ctrl Pts',(7.99921148699994,15.2,6.72722211399999));
#205103=CARTESIAN_POINT('Ctrl Pts',(7.99921148699994,11.6,6.72722211399999));
#205104=CARTESIAN_POINT('Ctrl Pts',(7.99796039099994,15.2,6.72645328399998));
#205105=CARTESIAN_POINT('Ctrl Pts',(7.99796039099994,11.6,6.72645328399998));
#205106=CARTESIAN_POINT('Ctrl Pts',(7.99671699399994,15.2,6.72568755299999));
#205107=CARTESIAN_POINT('Ctrl Pts',(7.99671699399994,11.6,6.72568755299999));
#205108=CARTESIAN_POINT('Ctrl Pts',(7.99548130699994,15.2,6.72492494499998));
#205109=CARTESIAN_POINT('Ctrl Pts',(7.99548130699994,11.6,6.72492494499998));
#205110=CARTESIAN_POINT('Ctrl Pts',(7.99425333799994,15.2,6.72416548299999));
#205111=CARTESIAN_POINT('Ctrl Pts',(7.99425333799994,11.6,6.72416548299999));
#205112=CARTESIAN_POINT('Ctrl Pts',(7.99303309699994,15.2,6.72340918999998));
#205113=CARTESIAN_POINT('Ctrl Pts',(7.99303309699994,11.6,6.72340918999998));
#205114=CARTESIAN_POINT('Ctrl Pts',(7.99182059499994,15.2,6.72265608999999));
#205115=CARTESIAN_POINT('Ctrl Pts',(7.99182059499994,11.6,6.72265608999999));
#205116=CARTESIAN_POINT('Ctrl Pts',(7.99061583999995,15.2,6.72190620499999));
#205117=CARTESIAN_POINT('Ctrl Pts',(7.99061583999995,11.6,6.72190620499999));
#205118=CARTESIAN_POINT('Ctrl Pts',(7.98941884299994,15.2,6.72115955999999));
#205119=CARTESIAN_POINT('Ctrl Pts',(7.98941884299994,11.6,6.72115955999999));
#205120=CARTESIAN_POINT('Ctrl Pts',(7.98822961399994,15.2,6.72041617699998));
#205121=CARTESIAN_POINT('Ctrl Pts',(7.98822961399994,11.6,6.72041617699998));
#205122=CARTESIAN_POINT('Ctrl Pts',(7.98704816099994,15.2,6.71967607999999));
#205123=CARTESIAN_POINT('Ctrl Pts',(7.98704816099994,11.6,6.71967607999999));
#205124=CARTESIAN_POINT('Ctrl Pts',(7.98587449499994,15.2,6.71893929399998));
#205125=CARTESIAN_POINT('Ctrl Pts',(7.98587449499994,11.6,6.71893929399998));
#205126=CARTESIAN_POINT('Ctrl Pts',(7.98470862699994,15.2,6.71820584199998));
#205127=CARTESIAN_POINT('Ctrl Pts',(7.98470862699994,11.6,6.71820584199998));
#205128=CARTESIAN_POINT('Ctrl Pts',(7.98355056499994,15.2,6.71747574699998));
#205129=CARTESIAN_POINT('Ctrl Pts',(7.98355056499994,11.6,6.71747574699998));
#205130=CARTESIAN_POINT('Ctrl Pts',(7.98240032199995,15.2,6.71674903499999));
#205131=CARTESIAN_POINT('Ctrl Pts',(7.98240032199995,11.6,6.71674903499999));
#205132=CARTESIAN_POINT('Ctrl Pts',(7.98125790399994,15.2,6.71602572899998));
#205133=CARTESIAN_POINT('Ctrl Pts',(7.98125790399994,11.6,6.71602572899998));
#205134=CARTESIAN_POINT('Ctrl Pts',(7.98012332299994,15.2,6.71530585399999));
#205135=CARTESIAN_POINT('Ctrl Pts',(7.98012332299994,11.6,6.71530585399999));
#205136=CARTESIAN_POINT('Ctrl Pts',(7.97899658999994,15.2,6.71458943299999));
#205137=CARTESIAN_POINT('Ctrl Pts',(7.97899658999994,11.6,6.71458943299999));
#205138=CARTESIAN_POINT('Ctrl Pts',(7.97787771299994,15.2,6.71387649199998));
#205139=CARTESIAN_POINT('Ctrl Pts',(7.97787771299994,11.6,6.71387649199998));
#205140=CARTESIAN_POINT('Ctrl Pts',(7.97676670299994,15.2,6.71316705499999));
#205141=CARTESIAN_POINT('Ctrl Pts',(7.97676670299994,11.6,6.71316705499999));
#205142=CARTESIAN_POINT('Ctrl Pts',(7.97566357099995,15.2,6.71246114699999));
#205143=CARTESIAN_POINT('Ctrl Pts',(7.97566357099995,11.6,6.71246114699999));
#205144=CARTESIAN_POINT('Ctrl Pts',(7.97456832699995,15.2,6.71175879199998));
#205145=CARTESIAN_POINT('Ctrl Pts',(7.97456832699995,11.6,6.71175879199998));
#205146=CARTESIAN_POINT('Ctrl Pts',(7.97348097899994,15.2,6.71106001599998));
#205147=CARTESIAN_POINT('Ctrl Pts',(7.97348097899994,11.6,6.71106001599998));
#205148=CARTESIAN_POINT('Ctrl Pts',(7.97240153999994,15.2,6.71036484399998));
#205149=CARTESIAN_POINT('Ctrl Pts',(7.97240153999994,11.6,6.71036484399998));
#205150=CARTESIAN_POINT('Ctrl Pts',(7.97133001899994,15.2,6.70967330099998));
#205151=CARTESIAN_POINT('Ctrl Pts',(7.97133001899994,11.6,6.70967330099998));
#205152=CARTESIAN_POINT('Ctrl Pts',(7.97026642699994,15.2,6.70898541299999));
#205153=CARTESIAN_POINT('Ctrl Pts',(7.97026642699994,11.6,6.70898541299999));
#205154=CARTESIAN_POINT('Ctrl Pts',(7.96921077299995,15.2,6.70830120399999));
#205155=CARTESIAN_POINT('Ctrl Pts',(7.96921077299995,11.6,6.70830120399999));
#205156=CARTESIAN_POINT('Ctrl Pts',(7.96816306799994,15.2,6.70762069999999));
#205157=CARTESIAN_POINT('Ctrl Pts',(7.96816306799994,11.6,6.70762069999999));
#205158=CARTESIAN_POINT('Ctrl Pts',(7.96712332399995,15.2,6.70694392699998));
#205159=CARTESIAN_POINT('Ctrl Pts',(7.96712332399995,11.6,6.70694392699998));
#205160=CARTESIAN_POINT('Ctrl Pts',(7.96609154999994,15.2,6.70627091099998));
#205161=CARTESIAN_POINT('Ctrl Pts',(7.96609154999994,11.6,6.70627091099998));
#205162=CARTESIAN_POINT('Ctrl Pts',(7.96506775499994,15.2,6.70560167799999));
#205163=CARTESIAN_POINT('Ctrl Pts',(7.96506775499994,11.6,6.70560167799999));
#205164=CARTESIAN_POINT('Ctrl Pts',(7.96405195199994,15.2,6.70493625299999));
#205165=CARTESIAN_POINT('Ctrl Pts',(7.96405195199994,11.6,6.70493625299999));
#205166=CARTESIAN_POINT('Ctrl Pts',(7.96304414999994,15.2,6.70427466299999));
#205167=CARTESIAN_POINT('Ctrl Pts',(7.96304414999994,11.6,6.70427466299999));
#205168=CARTESIAN_POINT('Ctrl Pts',(7.96204436099995,15.2,6.70361693399999));
#205169=CARTESIAN_POINT('Ctrl Pts',(7.96204436099995,11.6,6.70361693399999));
#205170=CARTESIAN_POINT('Ctrl Pts',(7.96105259399994,15.2,6.70296309299999));
#205171=CARTESIAN_POINT('Ctrl Pts',(7.96105259399994,11.6,6.70296309299999));
#205172=CARTESIAN_POINT('Ctrl Pts',(7.96006886099994,15.2,6.70231316599998));
#205173=CARTESIAN_POINT('Ctrl Pts',(7.96006886099994,11.6,6.70231316599998));
#205174=CARTESIAN_POINT('Ctrl Pts',(7.95909317099994,15.2,6.70166717899999));
#205175=CARTESIAN_POINT('Ctrl Pts',(7.95909317099994,11.6,6.70166717899999));
#205176=CARTESIAN_POINT('Ctrl Pts',(7.95812553699994,15.2,6.70102516099998));
#205177=CARTESIAN_POINT('Ctrl Pts',(7.95812553699994,11.6,6.70102516099998));
#205178=CARTESIAN_POINT('Ctrl Pts',(7.95716596799994,15.2,6.70038713599999));
#205179=CARTESIAN_POINT('Ctrl Pts',(7.95716596799994,11.6,6.70038713599999));
#205180=CARTESIAN_POINT('Ctrl Pts',(7.95621447399995,15.2,6.69975313299998));
#205181=CARTESIAN_POINT('Ctrl Pts',(7.95621447399995,11.6,6.69975313299998));
#205182=CARTESIAN_POINT('Ctrl Pts',(7.95527106899995,15.2,6.69912317999999));
#205183=CARTESIAN_POINT('Ctrl Pts',(7.95527106899995,11.6,6.69912317999999));
#205184=CARTESIAN_POINT('Ctrl Pts',(7.95433576199994,15.2,6.69849730199999));
#205185=CARTESIAN_POINT('Ctrl Pts',(7.95433576199994,11.6,6.69849730199999));
#205186=CARTESIAN_POINT('Ctrl Pts',(7.95340856399994,15.2,6.69787552699999));
#205187=CARTESIAN_POINT('Ctrl Pts',(7.95340856399994,11.6,6.69787552699999));
#205188=CARTESIAN_POINT('Ctrl Pts',(7.95248948499995,15.2,6.69725788299999));
#205189=CARTESIAN_POINT('Ctrl Pts',(7.95248948499995,11.6,6.69725788299999));
#205190=CARTESIAN_POINT('Ctrl Pts',(7.95157853699994,15.2,6.69664439899999));
#205191=CARTESIAN_POINT('Ctrl Pts',(7.95157853699994,11.6,6.69664439899999));
#205192=CARTESIAN_POINT('Ctrl Pts',(7.95067573199994,15.2,6.69603509999998));
#205193=CARTESIAN_POINT('Ctrl Pts',(7.95067573199994,11.6,6.69603509999998));
#205194=CARTESIAN_POINT('Ctrl Pts',(7.94978107899994,15.2,6.69543001699999));
#205195=CARTESIAN_POINT('Ctrl Pts',(7.94978107899994,11.6,6.69543001699999));
#205196=CARTESIAN_POINT('Ctrl Pts',(7.94889458999994,15.2,6.69482917499998));
#205197=CARTESIAN_POINT('Ctrl Pts',(7.94889458999994,11.6,6.69482917499998));
#205198=CARTESIAN_POINT('Ctrl Pts',(7.94801627599995,15.2,6.69423260599999));
#205199=CARTESIAN_POINT('Ctrl Pts',(7.94801627599995,11.6,6.69423260599999));
#205200=CARTESIAN_POINT('Ctrl Pts',(7.94714614999994,15.2,6.69364033599999));
#205201=CARTESIAN_POINT('Ctrl Pts',(7.94714614999994,11.6,6.69364033599999));
#205202=CARTESIAN_POINT('Ctrl Pts',(7.94628421999994,15.2,6.69305239299998));
#205203=CARTESIAN_POINT('Ctrl Pts',(7.94628421999994,11.6,6.69305239299998));
#205204=CARTESIAN_POINT('Ctrl Pts',(7.94543049999994,15.2,6.69246880699998));
#205205=CARTESIAN_POINT('Ctrl Pts',(7.94543049999994,11.6,6.69246880699998));
#205206=CARTESIAN_POINT('Ctrl Pts',(7.94458499899994,15.2,6.69188960699999));
#205207=CARTESIAN_POINT('Ctrl Pts',(7.94458499899994,11.6,6.69188960699999));
#205208=CARTESIAN_POINT('Ctrl Pts',(7.94374772999995,15.2,6.69131482099999));
#205209=CARTESIAN_POINT('Ctrl Pts',(7.94374772999995,11.6,6.69131482099999));
#205210=CARTESIAN_POINT('Ctrl Pts',(7.94291870399995,15.2,6.69074447799999));
#205211=CARTESIAN_POINT('Ctrl Pts',(7.94291870399995,11.6,6.69074447799999));
#205212=CARTESIAN_POINT('Ctrl Pts',(7.94209793199995,15.2,6.69017860899999));
#205213=CARTESIAN_POINT('Ctrl Pts',(7.94209793199995,11.6,6.69017860899999));
#205214=CARTESIAN_POINT('Ctrl Pts',(7.94128542699994,15.2,6.68961724199999));
#205215=CARTESIAN_POINT('Ctrl Pts',(7.94128542699994,11.6,6.68961724199999));
#205216=CARTESIAN_POINT('Ctrl Pts',(7.94048119799994,15.2,6.68906040599998));
#205217=CARTESIAN_POINT('Ctrl Pts',(7.94048119799994,11.6,6.68906040599998));
#205218=CARTESIAN_POINT('Ctrl Pts',(7.93968525799994,15.2,6.68850813299999));
#205219=CARTESIAN_POINT('Ctrl Pts',(7.93968525799994,11.6,6.68850813299999));
#205220=CARTESIAN_POINT('Ctrl Pts',(7.93889761899995,15.2,6.68796045099998));
#205221=CARTESIAN_POINT('Ctrl Pts',(7.93889761899995,11.6,6.68796045099998));
#205222=CARTESIAN_POINT('Ctrl Pts',(7.93811829199995,15.2,6.68741739099998));
#205223=CARTESIAN_POINT('Ctrl Pts',(7.93811829199995,11.6,6.68741739099998));
#205224=CARTESIAN_POINT('Ctrl Pts',(7.93734728899994,15.2,6.68687898099999));
#205225=CARTESIAN_POINT('Ctrl Pts',(7.93734728899994,11.6,6.68687898099999));
#205226=CARTESIAN_POINT('Ctrl Pts',(7.93658462199994,15.2,6.68634525499999));
#205227=CARTESIAN_POINT('Ctrl Pts',(7.93658462199994,11.6,6.68634525499999));
#205228=CARTESIAN_POINT('Ctrl Pts',(7.93583464599994,15.2,6.68581928799998));
#205229=CARTESIAN_POINT('Ctrl Pts',(7.93583464599994,11.6,6.68581928799998));
#205230=CARTESIAN_POINT('Ctrl Pts',(7.93524212599995,15.2,6.68540286399999));
#205231=CARTESIAN_POINT('Ctrl Pts',(7.93524212599995,11.6,6.68540286399999));
#205232=CARTESIAN_POINT('Ctrl Pts',(7.93480250499995,15.2,6.68509340799999));
#205233=CARTESIAN_POINT('Ctrl Pts',(7.93480250499995,11.6,6.68509340799999));
#205234=CARTESIAN_POINT('Ctrl Pts',(7.93451247199994,15.2,6.68488903399999));
#205235=CARTESIAN_POINT('Ctrl Pts',(7.93451247199994,11.6,6.68488903399999));
#205236=CARTESIAN_POINT('Ctrl Pts',(7.93436996999994,15.2,6.68478856799998));
#205237=CARTESIAN_POINT('Ctrl Pts',(7.93436996999994,11.6,6.68478856799998));
#205238=CARTESIAN_POINT('',(7.93436996899994,12.2,6.68478856799998));
#205239=CARTESIAN_POINT('',(7.93436996899994,15.2,6.68478856799998));
#205240=CARTESIAN_POINT('',(7.93436996899994,12.2,6.68478856799998));
#205241=CARTESIAN_POINT('Ctrl Pts',(9.03946594399994,12.2,7.10901226999999));
#205242=CARTESIAN_POINT('Ctrl Pts',(9.0357292033211,12.2,7.10820510485334));
#205243=CARTESIAN_POINT('Ctrl Pts',(9.03199984125262,12.2,7.10739512148574));
#205244=CARTESIAN_POINT('Ctrl Pts',(9.02827785941652,12.2,7.10658231363194));
#205245=CARTESIAN_POINT('Ctrl Pts',(9.02455587758041,12.2,7.10576950577814));
#205246=CARTESIAN_POINT('Ctrl Pts',(9.02084127436859,12.2,7.10495387545248));
#205247=CARTESIAN_POINT('Ctrl Pts',(9.01713406173388,12.2,7.10413543639999));
#205248=CARTESIAN_POINT('Ctrl Pts',(9.01342684909918,12.2,7.1033169973475));
#205249=CARTESIAN_POINT('Ctrl Pts',(9.00972702803836,12.2,7.10249574936599));
#205250=CARTESIAN_POINT('Ctrl Pts',(9.00603462575484,12.2,7.10167172614631));
#205251=CARTESIAN_POINT('Ctrl Pts',(9.00234222280054,12.2,7.10084770277693));
#205252=CARTESIAN_POINT('Ctrl Pts',(8.99865723923165,12.2,7.1000209059901));
#205253=CARTESIAN_POINT('Ctrl Pts',(8.99497970615653,12.2,7.09919137303583));
#205254=CARTESIAN_POINT('Ctrl Pts',(8.99007632983651,12.2,7.09808532934797));
#205255=CARTESIAN_POINT('Ctrl Pts',(8.98518619850922,12.2,7.09697442424131));
#205256=CARTESIAN_POINT('Ctrl Pts',(8.98030937140703,12.2,7.09585872583283));
#205257=CARTESIAN_POINT('Ctrl Pts',(8.97665175091428,12.2,7.09502195198847));
#205258=CARTESIAN_POINT('Ctrl Pts',(8.97300161223856,12.2,7.09418248255741));
#205259=CARTESIAN_POINT('Ctrl Pts',(8.96935897972972,12.2,7.09334034712958));
#205260=CARTESIAN_POINT('Ctrl Pts',(8.9657163472209,12.2,7.09249821170174));
#205261=CARTESIAN_POINT('Ctrl Pts',(8.96208122205994,12.2,7.09165340977026));
#205262=CARTESIAN_POINT('Ctrl Pts',(8.95845362973238,12.2,7.09080597588474));
#205263=CARTESIAN_POINT('Ctrl Pts',(8.9548260367458,12.2,7.08995854184528));
#205264=CARTESIAN_POINT('Ctrl Pts',(8.95120597758635,12.2,7.08910847592173));
#205265=CARTESIAN_POINT('Ctrl Pts',(8.94759347797903,12.2,7.08825581033912));
#205266=CARTESIAN_POINT('Ctrl Pts',(8.94398097902799,12.2,7.08740314491141));
#205267=CARTESIAN_POINT('Ctrl Pts',(8.94037603872654,12.2,7.08654787930885));
#205268=CARTESIAN_POINT('Ctrl Pts',(8.93677868385791,12.2,7.08569004692312));
#205269=CARTESIAN_POINT('Ctrl Pts',(8.93318132898928,12.2,7.0848322145374));
#205270=CARTESIAN_POINT('Ctrl Pts',(8.92959155958273,12.2,7.0839718151218));
#205271=CARTESIAN_POINT('Ctrl Pts',(8.92600939969664,12.2,7.08310888027422));
#205272=CARTESIAN_POINT('Ctrl Pts',(8.92242723981055,12.2,7.08224594542665));
#205273=CARTESIAN_POINT('Ctrl Pts',(8.91885269052311,12.2,7.08138047555652));
#205274=CARTESIAN_POINT('Ctrl Pts',(8.9152857780948,12.2,7.08051250379246));
#205275=CARTESIAN_POINT('Ctrl Pts',(8.91171886566649,12.2,7.07964453202839));
#205276=CARTESIAN_POINT('Ctrl Pts',(8.90815958947544,12.2,7.07877405966317));
#205277=CARTESIAN_POINT('Ctrl Pts',(8.90460797560381,12.2,7.07790111882011));
#205278=CARTESIAN_POINT('Ctrl Pts',(8.90105636173218,12.2,7.07702817797704));
#205279=CARTESIAN_POINT('Ctrl Pts',(8.89751240944337,12.2,7.07615276832581));
#205280=CARTESIAN_POINT('Ctrl Pts',(8.89397614648747,12.2,7.07527492444137));
#205281=CARTESIAN_POINT('Ctrl Pts',(8.89043988288915,12.2,7.07439708039746));
#205282=CARTESIAN_POINT('Ctrl Pts',(8.88691130760967,12.2,7.07351680156952));
#205283=CARTESIAN_POINT('Ctrl Pts',(8.88339044697402,12.2,7.07263412156591));
#205284=CARTESIAN_POINT('Ctrl Pts',(8.87986958697799,12.2,7.07175144172265));
#205285=CARTESIAN_POINT('Ctrl Pts',(8.87635643965195,12.2,7.07086636067398));
#205286=CARTESIAN_POINT('Ctrl Pts',(8.87285103356342,12.2,7.06997891232828));
#205287=CARTESIAN_POINT('Ctrl Pts',(8.86934562747489,12.2,7.06909146398258));
#205288=CARTESIAN_POINT('Ctrl Pts',(8.86584796275881,12.2,7.06820164930384));
#205289=CARTESIAN_POINT('Ctrl Pts',(8.86235806388629,12.2,7.06730950191939));
#205290=CARTESIAN_POINT('Ctrl Pts',(8.85886816501376,12.2,7.06641735453493));
#205291=CARTESIAN_POINT('Ctrl Pts',(8.85538603207365,12.2,7.06552287381742));
#205292=CARTESIAN_POINT('Ctrl Pts',(8.85191169219988,12.2,7.06462609455834));
#205293=CARTESIAN_POINT('Ctrl Pts',(8.84843735232612,12.2,7.06372931529925));
#205294=CARTESIAN_POINT('Ctrl Pts',(8.84497080525204,12.2,7.06283023828193));
#205295=CARTESIAN_POINT('Ctrl Pts',(8.84151207683536,12.2,7.06192889706488));
#205296=CARTESIAN_POINT('Ctrl Pts',(8.83805334841867,12.2,7.06102755584782));
#205297=CARTESIAN_POINT('Ctrl Pts',(8.83460243864312,12.2,7.06012395231425));
#205298=CARTESIAN_POINT('Ctrl Pts',(8.83115937426714,12.2,7.05921811947247));
#205299=CARTESIAN_POINT('Ctrl Pts',(8.82771630926568,12.2,7.05831228646613));
#205300=CARTESIAN_POINT('Ctrl Pts',(8.82428109046645,12.2,7.05740422408416));
#205301=CARTESIAN_POINT('Ctrl Pts',(8.82085374201108,12.2,7.05649396907657));
#205302=CARTESIAN_POINT('Ctrl Pts',(8.81742639417834,12.2,7.05558371423434));
#205303=CARTESIAN_POINT('Ctrl Pts',(8.81400691756881,12.2,7.0546712656524));
#205304=CARTESIAN_POINT('Ctrl Pts',(8.81059533860657,12.2,7.05375665930636));
#205305=CARTESIAN_POINT('Ctrl Pts',(8.80718375964434,12.2,7.05284205296031));
#205306=CARTESIAN_POINT('Ctrl Pts',(8.80378007972248,12.2,7.05192528919994));
#205307=CARTESIAN_POINT('Ctrl Pts',(8.80038432380488,12.2,7.05100640294147));
#205308=CARTESIAN_POINT('Ctrl Pts',(8.79698856788729,12.2,7.050087516683));
#205309=CARTESIAN_POINT('Ctrl Pts',(8.79360073576041,12.2,7.04916650844979));
#205310=CARTESIAN_POINT('Ctrl Pts',(8.79022085479989,12.2,7.04824341369167));
#205311=CARTESIAN_POINT('Ctrl Pts',(8.78684097383936,12.2,7.04732031893354));
#205312=CARTESIAN_POINT('Ctrl Pts',(8.7834690429785,12.2,7.0463951382505));
#205313=CARTESIAN_POINT('Ctrl Pts',(8.78010509010003,12.2,7.0454679083677));
#205314=CARTESIAN_POINT('Ctrl Pts',(8.77674113722156,12.2,7.04454067848491));
#205315=CARTESIAN_POINT('Ctrl Pts',(8.77338516219426,12.2,7.04361139802595));
#205316=CARTESIAN_POINT('Ctrl Pts',(8.77003719064772,12.2,7.04268010468016));
#205317=CARTESIAN_POINT('Ctrl Pts',(8.76668921910116,12.2,7.04174881133437));
#205318=CARTESIAN_POINT('Ctrl Pts',(8.76334925132296,12.2,7.04081550520297));
#205319=CARTESIAN_POINT('Ctrl Pts',(8.76001731444292,12.2,7.03988022148722));
#205320=CARTESIAN_POINT('Ctrl Pts',(8.75668537695758,12.2,7.03894493760156));
#205321=CARTESIAN_POINT('Ctrl Pts',(8.75336147029118,12.2,7.03800767783202));
#205322=CARTESIAN_POINT('Ctrl Pts',(8.75004562126871,12.2,7.03706847932025));
#205323=CARTESIAN_POINT('Ctrl Pts',(8.74672977284863,12.2,7.03612928097911));
#205324=CARTESIAN_POINT('Ctrl Pts',(8.74342198178642,12.2,7.03518814242974));
#205325=CARTESIAN_POINT('Ctrl Pts',(8.74012227490702,12.2,7.03424510167217));
#205326=CARTESIAN_POINT('Ctrl Pts',(8.73682256802762,12.2,7.0333020609146));
#205327=CARTESIAN_POINT('Ctrl Pts',(8.73353094505916,12.2,7.03235711836905));
#205328=CARTESIAN_POINT('Ctrl Pts',(8.73024743320524,12.2,7.03141031202414));
#205329=CARTESIAN_POINT('Ctrl Pts',(8.72696392135134,12.2,7.03046350567923));
#205330=CARTESIAN_POINT('Ctrl Pts',(8.72368852091569,12.2,7.0295148335873));
#205331=CARTESIAN_POINT('Ctrl Pts',(8.72042125847786,12.2,7.02856433674253));
#205332=CARTESIAN_POINT('Ctrl Pts',(8.71715399604003,12.2,7.02761383989776));
#205333=CARTESIAN_POINT('Ctrl Pts',(8.71389487088697,12.2,7.02666151658581));
#205334=CARTESIAN_POINT('Ctrl Pts',(8.71064391233771,12.2,7.02570740387063));
#205335=CARTESIAN_POINT('Ctrl Pts',(8.70739295378845,12.2,7.02475329115545));
#205336=CARTESIAN_POINT('Ctrl Pts',(8.70415015838862,12.2,7.02379739027373));
#205337=CARTESIAN_POINT('Ctrl Pts',(8.70091555642171,12.2,7.02283974047543));
#205338=CARTESIAN_POINT('Ctrl Pts',(8.6966027534074,12.2,7.02156287396171));
#205339=CARTESIAN_POINT('Ctrl Pts',(8.69230451406649,12.2,7.02028289602211));
#205340=CARTESIAN_POINT('Ctrl Pts',(8.68802090248032,12.2,7.01899990022412));
#205341=CARTESIAN_POINT('Ctrl Pts',(8.68480819408251,12.2,7.01803765346304));
#205342=CARTESIAN_POINT('Ctrl Pts',(8.68160371343455,12.2,7.01707370848684));
#205343=CARTESIAN_POINT('Ctrl Pts',(8.67840748899446,12.2,7.01610810472587));
#205344=CARTESIAN_POINT('Ctrl Pts',(8.67414585602057,12.2,7.01482063292764));
#205345=CARTESIAN_POINT('Ctrl Pts',(8.6698988997593,12.2,7.01353021277599));
#205346=CARTESIAN_POINT('Ctrl Pts',(8.66566668430793,12.2,7.01223693703855));
#205347=CARTESIAN_POINT('Ctrl Pts',(8.66143446943319,12.2,7.01094366147731));
#205348=CARTESIAN_POINT('Ctrl Pts',(8.65721699491211,12.2,7.00964752991645));
#205349=CARTESIAN_POINT('Ctrl Pts',(8.65301432781026,12.2,7.00834863835615));
#205350=CARTESIAN_POINT('Ctrl Pts',(8.6488116601358,12.2,7.00704974661887));
#205351=CARTESIAN_POINT('Ctrl Pts',(8.64462379779295,12.2,7.00574809408054));
#205352=CARTESIAN_POINT('Ctrl Pts',(8.64045080663611,12.2,7.00444377627738));
#205353=CARTESIAN_POINT('Ctrl Pts',(8.63627781604783,12.2,7.00313945865194));
#205354=CARTESIAN_POINT('Ctrl Pts',(8.63211969691766,12.2,7.00183247790536));
#205355=CARTESIAN_POINT('Ctrl Pts',(8.62797651458873,12.2,7.00052292712369));
#205356=CARTESIAN_POINT('Ctrl Pts',(8.62383333169529,12.2,6.99921337616361));
#205357=CARTESIAN_POINT('Ctrl Pts',(8.61970508465086,12.2,6.99790125668099));
#205358=CARTESIAN_POINT('Ctrl Pts',(8.6155918403721,12.2,6.99658666694251));
#205359=CARTESIAN_POINT('Ctrl Pts',(8.61147859665378,12.2,6.99527207738314));
#205360=CARTESIAN_POINT('Ctrl Pts',(8.60738035496395,12.2,6.99395501611039));
#205361=CARTESIAN_POINT('Ctrl Pts',(8.60329718109246,12.2,6.99263558370811));
#205362=CARTESIAN_POINT('Ctrl Pts',(8.59921400666464,12.2,6.99131615112604));
#205363=CARTESIAN_POINT('Ctrl Pts',(8.59514590002471,12.2,6.98999434577793));
#205364=CARTESIAN_POINT('Ctrl Pts',(8.5910929271937,12.2,6.98867026865006));
#205365=CARTESIAN_POINT('Ctrl Pts',(8.58703995491491,12.2,6.98734619170261));
#205366=CARTESIAN_POINT('Ctrl Pts',(8.58300211633029,12.2,6.98601984098337));
#205367=CARTESIAN_POINT('Ctrl Pts',(8.57897947865759,12.2,6.98469131892554));
#205368=CARTESIAN_POINT('Ctrl Pts',(8.57495684043681,12.2,6.9833627966867));
#205369=CARTESIAN_POINT('Ctrl Pts',(8.57094940214949,12.2,6.98203210334723));
#205370=CARTESIAN_POINT('Ctrl Pts',(8.56695723124717,12.2,6.98069933899075));
#205371=CARTESIAN_POINT('Ctrl Pts',(8.56296506088878,12.2,6.97936657481586));
#205372=CARTESIAN_POINT('Ctrl Pts',(8.5589881564503,12.2,6.9780317411174));
#205373=CARTESIAN_POINT('Ctrl Pts',(8.55502658560594,12.2,6.97669493972689));
#205374=CARTESIAN_POINT('Ctrl Pts',(8.55106501422181,12.2,6.97535813815425));
#205375=CARTESIAN_POINT('Ctrl Pts',(8.54711877786409,12.2,6.97401936900639));
#205376=CARTESIAN_POINT('Ctrl Pts',(8.54318794098321,12.2,6.97267873726666));
#205377=CARTESIAN_POINT('Ctrl Pts',(8.53925710410233,12.2,6.97133810552693));
#205378=CARTESIAN_POINT('Ctrl Pts',(8.53534166835655,12.2,6.96999561026198));
#205379=CARTESIAN_POINT('Ctrl Pts',(8.53144170014558,12.2,6.96865135602187));
#205380=CARTESIAN_POINT('Ctrl Pts',(8.5255917483605,12.2,6.96663497484487));
#205381=CARTESIAN_POINT('Ctrl Pts',(8.51977659904015,12.2,6.96461463830795));
#205382=CARTESIAN_POINT('Ctrl Pts',(8.51399647941834,12.2,6.96259070313133));
#205383=CARTESIAN_POINT('Ctrl Pts',(8.51014306651215,12.2,6.96124141307487));
#205384=CARTESIAN_POINT('Ctrl Pts',(8.50630522331396,12.2,6.95989052452984));
#205385=CARTESIAN_POINT('Ctrl Pts',(8.50248301762482,12.2,6.95853814569611));
#205386=CARTESIAN_POINT('Ctrl Pts',(8.4986608114149,12.2,6.95718576667811));
#205387=CARTESIAN_POINT('Ctrl Pts',(8.49485424279537,12.2,6.95583189629886));
#205388=CARTESIAN_POINT('Ctrl Pts',(8.49106337869988,12.2,6.95447664405833));
#205389=CARTESIAN_POINT('Ctrl Pts',(8.4872725146044,12.2,6.9531213918178));
#205390=CARTESIAN_POINT('Ctrl Pts',(8.4834973557885,12.2,6.95176475755489));
#205391=CARTESIAN_POINT('Ctrl Pts',(8.47973797158523,12.2,6.9504068525363));
#205392=CARTESIAN_POINT('Ctrl Pts',(8.47503874209946,12.2,6.9487094715406));
#205393=CARTESIAN_POINT('Ctrl Pts',(8.4703641582144,12.2,6.9470101029647));
#205394=CARTESIAN_POINT('Ctrl Pts',(8.46571435614975,12.2,6.94530896620584));
#205395=CARTESIAN_POINT('Ctrl Pts',(8.46199451388983,12.2,6.94394805657622));
#205396=CARTESIAN_POINT('Ctrl Pts',(8.4582905303981,12.2,6.94258601363261));
#205397=CARTESIAN_POINT('Ctrl Pts',(8.45460247747488,12.2,6.94122295272499));
#205398=CARTESIAN_POINT('Ctrl Pts',(8.45091442455165,12.2,6.93985989181737));
#205399=CARTESIAN_POINT('Ctrl Pts',(8.44724229913308,12.2,6.9384958119263));
#205400=CARTESIAN_POINT('Ctrl Pts',(8.44358617293545,12.2,6.93713082701848));
#205401=CARTESIAN_POINT('Ctrl Pts',(8.43993004723596,12.2,6.93576584229665));
#205402=CARTESIAN_POINT('Ctrl Pts',(8.43628991926427,12.2,6.93439995305929));
#205403=CARTESIAN_POINT('Ctrl Pts',(8.43266585971069,12.2,6.93303327444259));
#205404=CARTESIAN_POINT('Ctrl Pts',(8.42904179966332,12.2,6.93166659563967));
#205405=CARTESIAN_POINT('Ctrl Pts',(8.42543380849562,12.2,6.93029912800927));
#205406=CARTESIAN_POINT('Ctrl Pts',(8.42184195441262,12.2,6.92893098776797));
#205407=CARTESIAN_POINT('Ctrl Pts',(8.41825010081901,12.2,6.92756284771307));
#205408=CARTESIAN_POINT('Ctrl Pts',(8.41467438710943,12.2,6.92619403477772));
#205409=CARTESIAN_POINT('Ctrl Pts',(8.41111488023269,12.2,6.92482466811193));
#205410=CARTESIAN_POINT('Ctrl Pts',(8.40755537287097,12.2,6.92345530125956));
#205411=CARTESIAN_POINT('Ctrl Pts',(8.40401207415797,12.2,6.92208537968598));
#205412=CARTESIAN_POINT('Ctrl Pts',(8.40048505451318,12.2,6.9207150240428));
#205413=CARTESIAN_POINT('Ctrl Pts',(8.39695803534894,12.2,6.91934466858633));
#205414=CARTESIAN_POINT('Ctrl Pts',(8.39344729625945,12.2,6.91797387854719));
#205415=CARTESIAN_POINT('Ctrl Pts',(8.38995290604404,12.2,6.91660277460374));
#205416=CARTESIAN_POINT('Ctrl Pts',(8.38645851535251,12.2,6.91523167047348));
#205417=CARTESIAN_POINT('Ctrl Pts',(8.3829804748074,12.2,6.91386025140706));
#205418=CARTESIAN_POINT('Ctrl Pts',(8.37951885600872,12.2,6.91248864188786));
#205419=CARTESIAN_POINT('Ctrl Pts',(8.37605723768168,12.2,6.91111703255554));
#205420=CARTESIAN_POINT('Ctrl Pts',(8.37261204047605,12.2,6.9097452305721));
#205421=CARTESIAN_POINT('Ctrl Pts',(8.36918333597249,12.2,6.90837336194905));
#205422=CARTESIAN_POINT('Ctrl Pts',(8.36575463100178,12.2,6.90700149313908));
#205423=CARTESIAN_POINT('Ctrl Pts',(8.36234242056755,12.2,6.90562955662649));
#205424=CARTESIAN_POINT('Ctrl Pts',(8.35894677327244,12.2,6.90425767716284));
#205425=CARTESIAN_POINT('Ctrl Pts',(8.35555112643999,12.2,6.9028857978861));
#205426=CARTESIAN_POINT('Ctrl Pts',(8.35217204464038,12.2,6.90151397674825));
#205427=CARTESIAN_POINT('Ctrl Pts',(8.34880960152466,12.2,6.90014233824925));
#205428=CARTESIAN_POINT('Ctrl Pts',(8.34544715795081,12.2,6.89877069956336));
#205429=CARTESIAN_POINT('Ctrl Pts',(8.34210134992745,12.2,6.89739924528279));
#205430=CARTESIAN_POINT('Ctrl Pts',(8.33877225306428,12.2,6.89602810325738));
#205431=CARTESIAN_POINT('Ctrl Pts',(8.3354431566547,12.2,6.8946569614188));
#205432=CARTESIAN_POINT('Ctrl Pts',(8.33213076870157,12.2,6.89328613199817));
#205433=CARTESIAN_POINT('Ctrl Pts',(8.32883516558038,12.2,6.89191574349904));
#205434=CARTESIAN_POINT('Ctrl Pts',(8.32553956201018,12.2,6.8905453548132));
#205435=CARTESIAN_POINT('Ctrl Pts',(8.32226073976654,12.2,6.88917540871351));
#205436=CARTESIAN_POINT('Ctrl Pts',(8.31899877503321,12.2,6.88780603474999));
#205437=CARTESIAN_POINT('Ctrl Pts',(8.31573681029987,12.2,6.88643666078647));
#205438=CARTESIAN_POINT('Ctrl Pts',(8.31249170255185,12.2,6.88506785976191));
#205439=CARTESIAN_POINT('Ctrl Pts',(8.30926352448875,12.2,6.8836997655763));
#205440=CARTESIAN_POINT('Ctrl Pts',(8.30522830256963,12.2,6.8819896481239));
#205441=CARTESIAN_POINT('Ctrl Pts',(8.30121953287222,12.2,6.88028063049843));
#205442=CARTESIAN_POINT('Ctrl Pts',(8.2972373633041,12.2,6.87857297999002));
#205443=CARTESIAN_POINT('Ctrl Pts',(8.29405162712872,12.2,6.87720685935991));
#205444=CARTESIAN_POINT('Ctrl Pts',(8.2908829142133,12.2,6.87584161254377));
#205445=CARTESIAN_POINT('Ctrl Pts',(8.28773129820821,12.2,6.87447737652498));
#205446=CARTESIAN_POINT('Ctrl Pts',(8.28457968220312,12.2,6.87311314050619));
#205447=CARTESIAN_POINT('Ctrl Pts',(8.28144516460002,12.2,6.87174991326807));
#205448=CARTESIAN_POINT('Ctrl Pts',(8.27832781926519,12.2,6.87038783652728));
#205449=CARTESIAN_POINT('Ctrl Pts',(8.2752104743551,12.2,6.86902575997208));
#205450=CARTESIAN_POINT('Ctrl Pts',(8.27211030209734,12.2,6.86766483115426));
#205451=CARTESIAN_POINT('Ctrl Pts',(8.26902737900198,12.2,6.86630519075924));
#205452=CARTESIAN_POINT('Ctrl Pts',(8.26594445548657,12.2,6.86494555017896));
#205453=CARTESIAN_POINT('Ctrl Pts',(8.26287877906861,12.2,6.86358719847693));
#205454=CARTESIAN_POINT('Ctrl Pts',(8.25983042829315,12.2,6.86223027656979));
#205455=CARTESIAN_POINT('Ctrl Pts',(8.25601999003147,12.2,6.86053412427831));
#205456=CARTESIAN_POINT('Ctrl Pts',(8.25223661920634,12.2,6.8588402058952));
#205457=CARTESIAN_POINT('Ctrl Pts',(8.24848046775025,12.2,6.85714880277041));
#205458=CARTESIAN_POINT('Ctrl Pts',(8.24472431670358,12.2,6.85545739982999));
#205459=CARTESIAN_POINT('Ctrl Pts',(8.24099538457726,12.2,6.85376851262029));
#205460=CARTESIAN_POINT('Ctrl Pts',(8.23729382095071,12.2,6.85208242322052));
#205461=CARTESIAN_POINT('Ctrl Pts',(8.23359225692068,12.2,6.85039633363696));
#205462=CARTESIAN_POINT('Ctrl Pts',(8.22991806111245,12.2,6.84871304506445));
#205463=CARTESIAN_POINT('Ctrl Pts',(8.22627138694354,12.2,6.84703284603642));
#205464=CARTESIAN_POINT('Ctrl Pts',(8.22262471277462,12.2,6.84535264700839));
#205465=CARTESIAN_POINT('Ctrl Pts',(8.21900555826635,12.2,6.84367553568585));
#205466=CARTESIAN_POINT('Ctrl Pts',(8.21541407673632,12.2,6.84200180922724));
#205467=CARTESIAN_POINT('Ctrl Pts',(8.2111042986654,12.2,6.83999333736745));
#205468=CARTESIAN_POINT('Ctrl Pts',(8.20683436996365,12.2,6.83798973672343));
#205469=CARTESIAN_POINT('Ctrl Pts',(8.20260455585746,12.2,6.83599152609835));
#205470=CARTESIAN_POINT('Ctrl Pts',(8.19907971096108,12.2,6.83432635066819));
#205471=CARTESIAN_POINT('Ctrl Pts',(8.19558272439941,12.2,6.83266491934952));
#205472=CARTESIAN_POINT('Ctrl Pts',(8.19211375051281,12.2,6.83100753476652));
#205473=CARTESIAN_POINT('Ctrl Pts',(8.18864477662621,12.2,6.82935015018352));
#205474=CARTESIAN_POINT('Ctrl Pts',(8.1852038162012,12.2,6.82769681512838));
#205475=CARTESIAN_POINT('Ctrl Pts',(8.18179102557851,12.2,6.82604783651763));
#205476=CARTESIAN_POINT('Ctrl Pts',(8.17837823532779,12.2,6.82439885808662));
#205477=CARTESIAN_POINT('Ctrl Pts',(8.17499361394205,12.2,6.82275423969722));
#205478=CARTESIAN_POINT('Ctrl Pts',(8.17163732118055,12.2,6.82111429293114));
#205479=CARTESIAN_POINT('Ctrl Pts',(8.16828102805322,12.2,6.81947434598632));
#205480=CARTESIAN_POINT('Ctrl Pts',(8.1649530622949,12.2,6.81783907455807));
#205481=CARTESIAN_POINT('Ctrl Pts',(8.16165358347312,12.2,6.81620879594654));
#205482=CARTESIAN_POINT('Ctrl Pts',(8.15835410465134,12.2,6.81457851733502));
#205483=CARTESIAN_POINT('Ctrl Pts',(8.15508311341256,12.2,6.81295323313046));
#205484=CARTESIAN_POINT('Ctrl Pts',(8.1518407693597,12.2,6.81133326943805));
#205485=CARTESIAN_POINT('Ctrl Pts',(8.14859842530684,12.2,6.80971330574564));
#205486=CARTESIAN_POINT('Ctrl Pts',(8.14538472933206,12.2,6.8080986631833));
#205487=CARTESIAN_POINT('Ctrl Pts',(8.14219984294167,12.2,6.80648967290524));
#205488=CARTESIAN_POINT('Ctrl Pts',(8.13901495655129,12.2,6.80488068262717));
#205489=CARTESIAN_POINT('Ctrl Pts',(8.13585888043942,12.2,6.80327734438259));
#205490=CARTESIAN_POINT('Ctrl Pts',(8.13273177668789,12.2,6.80167999660448));
#205491=CARTESIAN_POINT('Ctrl Pts',(8.12960467293636,12.2,6.80008264882637));
#205492=CARTESIAN_POINT('Ctrl Pts',(8.12650654367112,12.2,6.7984912917136));
#205493=CARTESIAN_POINT('Ctrl Pts',(8.12343755226821,12.2,6.79690626823416));
#205494=CARTESIAN_POINT('Ctrl Pts',(8.1203685608653,12.2,6.79532124475473));
#205495=CARTESIAN_POINT('Ctrl Pts',(8.11732870910542,12.2,6.79374255630553));
#205496=CARTESIAN_POINT('Ctrl Pts',(8.1143181612582,12.2,6.79217055199997));
#205497=CARTESIAN_POINT('Ctrl Pts',(8.11130761341098,12.2,6.79059854769441));
#205498=CARTESIAN_POINT('Ctrl Pts',(8.10832637284494,12.2,6.78903322586174));
#205499=CARTESIAN_POINT('Ctrl Pts',(8.1053746047066,12.2,6.78747494571579));
#205500=CARTESIAN_POINT('Ctrl Pts',(8.10183248306929,12.2,6.78560500960859));
#205501=CARTESIAN_POINT('Ctrl Pts',(8.09833280324803,12.2,6.78374521185907));
#205502=CARTESIAN_POINT('Ctrl Pts',(8.09487586070512,12.2,6.78189617984245));
#205503=CARTESIAN_POINT('Ctrl Pts',(8.0914189178482,12.2,6.78004714765789));
#205504=CARTESIAN_POINT('Ctrl Pts',(8.08800470887987,12.2,6.77820888142463));
#205505=CARTESIAN_POINT('Ctrl Pts',(8.08463353686576,12.2,6.77638202507584));
#205506=CARTESIAN_POINT('Ctrl Pts',(8.08126236515784,12.2,6.77455516889299));
#205507=CARTESIAN_POINT('Ctrl Pts',(8.07793422624145,12.2,6.77273971960236));
#205508=CARTESIAN_POINT('Ctrl Pts',(8.07464942377936,12.2,6.7709363376684));
#205509=CARTESIAN_POINT('Ctrl Pts',(8.07136462131726,12.2,6.76913295573445));
#205510=CARTESIAN_POINT('Ctrl Pts',(8.06812315582669,12.2,6.76734163849119));
#205511=CARTESIAN_POINT('Ctrl Pts',(8.06492533044098,12.2,6.76556305963861));
#205512=CARTESIAN_POINT('Ctrl Pts',(8.06172750505528,12.2,6.76378448078601));
#205513=CARTESIAN_POINT('Ctrl Pts',(8.05857332152055,12.2,6.76201864013655));
#205514=CARTESIAN_POINT('Ctrl Pts',(8.05546309004723,12.2,6.76026622444931));
#205515=CARTESIAN_POINT('Ctrl Pts',(8.05235285829139,12.2,6.75851380860291));
#205516=CARTESIAN_POINT('Ctrl Pts',(8.04928657707312,12.2,6.7567748181494));
#205517=CARTESIAN_POINT('Ctrl Pts',(8.04626456232702,12.2,6.75504995822268));
#205518=CARTESIAN_POINT('Ctrl Pts',(8.0427388788683,12.2,6.75303762187651));
#205519=CARTESIAN_POINT('Ctrl Pts',(8.03927344600945,12.2,6.75104451508481));
#205520=CARTESIAN_POINT('Ctrl Pts',(8.0358687693013,12.2,6.74907178940094));
#205521=CARTESIAN_POINT('Ctrl Pts',(8.03295047463924,12.2,6.74738088147443));
#205522=CARTESIAN_POINT('Ctrl Pts',(8.03007681790642,12.2,6.74570494512434));
#205523=CARTESIAN_POINT('Ctrl Pts',(8.02724812333756,12.2,6.74404472445121));
#205524=CARTESIAN_POINT('Ctrl Pts',(8.02441942902563,12.2,6.74238450392889));
#205525=CARTESIAN_POINT('Ctrl Pts',(8.02163569701842,12.2,6.74073999717198));
#205526=CARTESIAN_POINT('Ctrl Pts',(8.01889725661596,12.2,6.73911196581375));
#205527=CARTESIAN_POINT('Ctrl Pts',(8.0161588162135,12.2,6.73748393445552));
#205528=CARTESIAN_POINT('Ctrl Pts',(8.0134656675454,12.2,6.73587237897535));
#205529=CARTESIAN_POINT('Ctrl Pts',(8.01081814330513,12.2,6.73427807594874));
#205530=CARTESIAN_POINT('Ctrl Pts',(8.00817061882438,12.2,6.73268377277733));
#205531=CARTESIAN_POINT('Ctrl Pts',(8.00556872181471,12.2,6.73110672459924));
#205532=CARTESIAN_POINT('Ctrl Pts',(8.00301278934409,12.2,6.72954773118173));
#205533=CARTESIAN_POINT('Ctrl Pts',(8.00003086847662,12.2,6.72772890574039));
#205534=CARTESIAN_POINT('Ctrl Pts',(7.99711151305915,12.2,6.72593465157874));
#205535=CARTESIAN_POINT('Ctrl Pts',(7.99425527027506,12.2,6.72416627542351));
#205536=CARTESIAN_POINT('Ctrl Pts',(7.99180706188851,12.2,6.7226505242563));
#205537=CARTESIAN_POINT('Ctrl Pts',(7.98940522491469,12.2,6.7211537867325));
#205538=CARTESIAN_POINT('Ctrl Pts',(7.98705010762171,12.2,6.71967690765288));
#205539=CARTESIAN_POINT('Ctrl Pts',(7.98469499054264,12.2,6.7182000287074));
#205540=CARTESIAN_POINT('Ctrl Pts',(7.9823865973208,12.2,6.71674300939667));
#205541=CARTESIAN_POINT('Ctrl Pts',(7.98012528497589,12.2,6.7153067175256));
#205542=CARTESIAN_POINT('Ctrl Pts',(7.97786397263098,12.2,6.71387042565454));
#205543=CARTESIAN_POINT('Ctrl Pts',(7.97564974154392,12.2,6.71245486093606));
#205544=CARTESIAN_POINT('Ctrl Pts',(7.97348295645272,12.2,6.71106091715189));
#205545=CARTESIAN_POINT('Ctrl Pts',(7.97131617116471,12.2,6.7096669732411));
#205546=CARTESIAN_POINT('Ctrl Pts',(7.96919683301319,12.2,6.70829465092577));
#205547=CARTESIAN_POINT('Ctrl Pts',(7.96712531629959,12.2,6.70694486611943));
#205548=CARTESIAN_POINT('Ctrl Pts',(7.96505379977415,12.2,6.70559508143567));
#205549=CARTESIAN_POINT('Ctrl Pts',(7.96303010065307,12.2,6.70426783511924));
#205550=CARTESIAN_POINT('Ctrl Pts',(7.96105460247486,12.2,6.70296407149994));
#205551=CARTESIAN_POINT('Ctrl Pts',(7.95907910429665,12.2,6.70166030788065));
#205552=CARTESIAN_POINT('Ctrl Pts',(7.95715180406014,12.2,6.70038002549835));
#205553=CARTESIAN_POINT('Ctrl Pts',(7.95527309369839,12.2,6.69912419889649));
#205554=CARTESIAN_POINT('Ctrl Pts',(7.953394383166,12.2,6.69786837218056));
#205555=CARTESIAN_POINT('Ctrl Pts',(7.95156425997445,12.2,6.69663699749083));
#205556=CARTESIAN_POINT('Ctrl Pts',(7.94978311979739,12.2,6.69543107717683));
#205557=CARTESIAN_POINT('Ctrl Pts',(7.94800197978211,12.2,6.69422515697239));
#205558=CARTESIAN_POINT('Ctrl Pts',(7.94626982492883,12.2,6.693044691721));
#205559=CARTESIAN_POINT('Ctrl Pts',(7.94458705698243,12.2,6.69189071050775));
#205560=CARTESIAN_POINT('Ctrl Pts',(7.94290428903604,12.2,6.6907367292945));
#205561=CARTESIAN_POINT('Ctrl Pts',(7.94127091035603,12.2,6.68960923087958));
#205562=CARTESIAN_POINT('Ctrl Pts',(7.93968733332804,12.2,6.688509280835));
#205563=CARTESIAN_POINT('Ctrl Pts',(7.93784742671344,12.2,6.68723128467378));
#205564=CARTESIAN_POINT('Ctrl Pts',(7.93607474793184,12.2,6.68599046144507));
#205565=CARTESIAN_POINT('Ctrl Pts',(7.93436996999994,12.2,6.68478856799998));
#205566=CARTESIAN_POINT('Ctrl Pts',(7.93436996999994,15.2,6.68478856799998));
#205567=CARTESIAN_POINT('Ctrl Pts',(7.93583020217336,15.2,6.68581805309871));
#205568=CARTESIAN_POINT('Ctrl Pts',(7.93734025309804,15.2,6.68687610405595));
#205569=CARTESIAN_POINT('Ctrl Pts',(7.9388996968374,15.2,6.68796160635605));
#205570=CARTESIAN_POINT('Ctrl Pts',(7.94046666100273,15.2,6.68905234349694));
#205571=CARTESIAN_POINT('Ctrl Pts',(7.94208349756759,15.2,6.69017080775629));
#205572=CARTESIAN_POINT('Ctrl Pts',(7.94374979091117,15.2,6.69131593187745));
#205573=CARTESIAN_POINT('Ctrl Pts',(7.9454160841034,15.2,6.69246105589459));
#205574=CARTESIAN_POINT('Ctrl Pts',(7.94713183283063,15.2,6.69363283707676));
#205575=CARTESIAN_POINT('Ctrl Pts',(7.94889663376652,15.2,6.69483024319994));
#205576=CARTESIAN_POINT('Ctrl Pts',(7.95066143470242,15.2,6.69602764932311));
#205577=CARTESIAN_POINT('Ctrl Pts',(7.95247528578891,15.2,6.6972506792804));
#205578=CARTESIAN_POINT('Ctrl Pts',(7.95433778906148,15.2,6.69849832762931));
#205579=CARTESIAN_POINT('Ctrl Pts',(7.9562002925032,15.2,6.69974597609154));
#205580=CARTESIAN_POINT('Ctrl Pts',(7.95811145072005,15.2,6.70101824167729));
#205581=CARTESIAN_POINT('Ctrl Pts',(7.96007087199678,15.2,6.7023141511662));
#205582=CARTESIAN_POINT('Ctrl Pts',(7.96203029309555,15.2,6.70361006053739));
#205583=CARTESIAN_POINT('Ctrl Pts',(7.96403797768271,15.2,6.70492961203486));
#205584=CARTESIAN_POINT('Ctrl Pts',(7.96609354478413,15.2,6.70627185674222));
#205585=CARTESIAN_POINT('Ctrl Pts',(7.96814911188555,15.2,6.70761410144959));
#205586=CARTESIAN_POINT('Ctrl Pts',(7.9702525611464,15.2,6.70897904048412));
#205587=CARTESIAN_POINT('Ctrl Pts',(7.9724035193995,15.2,6.71036575118279));
#205588=CARTESIAN_POINT('Ctrl Pts',(7.97455447784797,15.2,6.71175246200742));
#205589=CARTESIAN_POINT('Ctrl Pts',(7.97675294572737,15.2,6.71316094522642));
#205590=CARTESIAN_POINT('Ctrl Pts',(7.97899855426965,15.2,6.71459030313909));
#205591=CARTESIAN_POINT('Ctrl Pts',(7.98124416260797,15.2,6.71601966092194));
#205592=CARTESIAN_POINT('Ctrl Pts',(7.98353691226888,15.2,6.71746989346604));
#205593=CARTESIAN_POINT('Ctrl Pts',(7.98587644460257,15.2,6.71894012758016));
#205594=CARTESIAN_POINT('Ctrl Pts',(7.98821597693625,15.2,6.72041036169427));
#205595=CARTESIAN_POINT('Ctrl Pts',(7.99060229026621,15.2,6.72190059904011));
#205596=CARTESIAN_POINT('Ctrl Pts',(7.99303503159248,15.2,6.72340998815111));
#205597=CARTESIAN_POINT('Ctrl Pts',(7.99587322995379,15.2,6.72517094220533));
#205598=CARTESIAN_POINT('Ctrl Pts',(7.9987746229845,15.2,6.72695796531665));
#205599=CARTESIAN_POINT('Ctrl Pts',(8.00173865588018,15.2,6.728769743068));
#205600=CARTESIAN_POINT('Ctrl Pts',(8.00427925537319,15.2,6.73032269534568));
#205601=CARTESIAN_POINT('Ctrl Pts',(8.00686587926256,15.2,6.73189383758858));
#205602=CARTESIAN_POINT('Ctrl Pts',(8.0094981845816,15.2,6.73348236586345));
#205603=CARTESIAN_POINT('Ctrl Pts',(8.01213048990063,15.2,6.73507089413831));
#205604=CARTESIAN_POINT('Ctrl Pts',(8.01480847849673,15.2,6.73667680914985));
#205605=CARTESIAN_POINT('Ctrl Pts',(8.01753181197804,15.2,6.73829932658978));
#205606=CARTESIAN_POINT('Ctrl Pts',(8.02025514570673,15.2,6.73992184417708));
#205607=CARTESIAN_POINT('Ctrl Pts',(8.02302382724809,15.2,6.74156096571598));
#205608=CARTESIAN_POINT('Ctrl Pts',(8.0258375249034,15.2,6.74321592730689));
#205609=CARTESIAN_POINT('Ctrl Pts',(8.02865122230314,15.2,6.74487088874745));
#205610=CARTESIAN_POINT('Ctrl Pts',(8.0315099365576,15.2,6.74654168994505));
#205611=CARTESIAN_POINT('Ctrl Pts',(8.03441334286682,15.2,6.74822758646647));
#205612=CARTESIAN_POINT('Ctrl Pts',(8.03731674917604,15.2,6.74991348298789));
#205613=CARTESIAN_POINT('Ctrl Pts',(8.04026484617711,15.2,6.75161447488462));
#205614=CARTESIAN_POINT('Ctrl Pts',(8.0432573146487,15.2,6.75332983457132));
#205615=CARTESIAN_POINT('Ctrl Pts',(8.04674852804677,15.2,6.755331087643));
#205616=CARTESIAN_POINT('Ctrl Pts',(8.05030013778289,15.2,6.75735189628479));
#205617=CARTESIAN_POINT('Ctrl Pts',(8.05391163811468,15.2,6.75939113816309));
#205618=CARTESIAN_POINT('Ctrl Pts',(8.05700720966694,15.2,6.76113905968233));
#205619=CARTESIAN_POINT('Ctrl Pts',(8.06014678600487,15.2,6.76290052075525));
#205620=CARTESIAN_POINT('Ctrl Pts',(8.06333005538623,15.2,6.76467483452324));
#205621=CARTESIAN_POINT('Ctrl Pts',(8.06651332505673,15.2,6.76644914845239));
#205622=CARTESIAN_POINT('Ctrl Pts',(8.0697402869565,15.2,6.76823631448283));
#205623=CARTESIAN_POINT('Ctrl Pts',(8.07301063571995,15.2,6.77003565558141));
#205624=CARTESIAN_POINT('Ctrl Pts',(8.07628098418636,15.2,6.77183499651657));
#205625=CARTESIAN_POINT('Ctrl Pts',(8.07959471940516,15.2,6.77364651499044));
#205626=CARTESIAN_POINT('Ctrl Pts',(8.08295153879835,15.2,6.7754695507658));
#205627=CARTESIAN_POINT('Ctrl Pts',(8.08630835819154,15.2,6.77729258654116));
#205628=CARTESIAN_POINT('Ctrl Pts',(8.08970826191097,15.2,6.77912713888328));
#205629=CARTESIAN_POINT('Ctrl Pts',(8.0931509513663,15.2,6.78097256381548));
#205630=CARTESIAN_POINT('Ctrl Pts',(8.09659364113434,15.2,6.78281798891532));
#205631=CARTESIAN_POINT('Ctrl Pts',(8.10007911544526,15.2,6.78467428644332));
#205632=CARTESIAN_POINT('Ctrl Pts',(8.10360708239959,15.2,6.78654082572222));
#205633=CARTESIAN_POINT('Ctrl Pts',(8.1065470547013,15.2,6.78809627503655));
#205634=CARTESIAN_POINT('Ctrl Pts',(8.10951653305084,15.2,6.78965883764913));
#205635=CARTESIAN_POINT('Ctrl Pts',(8.11251535110879,15.2,6.79122815445524));
#205636=CARTESIAN_POINT('Ctrl Pts',(8.11611393264758,15.2,6.79311133455415));
#205637=CARTESIAN_POINT('Ctrl Pts',(8.11975476271853,15.2,6.79500424012795));
#205638=CARTESIAN_POINT('Ctrl Pts',(8.12343755226821,15.2,6.79690626823417));
#205639=CARTESIAN_POINT('Ctrl Pts',(8.1271203418179,15.2,6.79880829634039));
#205640=CARTESIAN_POINT('Ctrl Pts',(8.13084509115011,15.2,6.80071944428217));
#205641=CARTESIAN_POINT('Ctrl Pts',(8.13461151384478,15.2,6.80263912137872));
#205642=CARTESIAN_POINT('Ctrl Pts',(8.13900567388331,15.2,6.80487874477428));
#205643=CARTESIAN_POINT('Ctrl Pts',(8.14345655804975,15.2,6.80712997304422));
#205644=CARTESIAN_POINT('Ctrl Pts',(8.14796371775163,15.2,6.80939188824252));
#205645=CARTESIAN_POINT('Ctrl Pts',(8.15118311748855,15.2,6.81100754193043));
#205646=CARTESIAN_POINT('Ctrl Pts',(8.15443123042951,15.2,6.81262864849498));
#205647=CARTESIAN_POINT('Ctrl Pts',(8.15770789355601,15.2,6.81425487960636));
#205648=CARTESIAN_POINT('Ctrl Pts',(8.16098455668251,15.2,6.81588111071774));
#205649=CARTESIAN_POINT('Ctrl Pts',(8.16428977108326,15.2,6.81751246501231));
#205650=CARTESIAN_POINT('Ctrl Pts',(8.16762337670973,15.2,6.81914862112368));
#205651=CARTESIAN_POINT('Ctrl Pts',(8.17095698233621,15.2,6.82078477723504));
#205652=CARTESIAN_POINT('Ctrl Pts',(8.17431897920554,15.2,6.82242573547515));
#205653=CARTESIAN_POINT('Ctrl Pts',(8.17770920916852,15.2,6.82407117597433));
#205654=CARTESIAN_POINT('Ctrl Pts',(8.18177748497631,15.2,6.8260457045016));
#205655=CARTESIAN_POINT('Ctrl Pts',(8.18588641492562,15.2,6.82802668918051));
#205656=CARTESIAN_POINT('Ctrl Pts',(8.19003572952487,15.2,6.83001359252497));
#205657=CARTESIAN_POINT('Ctrl Pts',(8.19418504412412,15.2,6.83200049586945));
#205658=CARTESIAN_POINT('Ctrl Pts',(8.19837474213551,15.2,6.83399331565477));
#205659=CARTESIAN_POINT('Ctrl Pts',(8.20260455585746,15.2,6.83599152609835));
#205660=CARTESIAN_POINT('Ctrl Pts',(8.20612940075384,15.2,6.8376567015285));
#205661=CARTESIAN_POINT('Ctrl Pts',(8.20968210262846,15.2,6.8393256200797));
#205662=CARTESIAN_POINT('Ctrl Pts',(8.21326250901588,15.2,6.84099798139896));
#205663=CARTESIAN_POINT('Ctrl Pts',(8.21684291540332,15.2,6.84267034271821));
#205664=CARTESIAN_POINT('Ctrl Pts',(8.22045102477482,15.2,6.8443461460959));
#205665=CARTESIAN_POINT('Ctrl Pts',(8.22408668532894,15.2,6.84602509887353));
#205666=CARTESIAN_POINT('Ctrl Pts',(8.22917661018398,15.2,6.84837563279879));
#205667=CARTESIAN_POINT('Ctrl Pts',(8.23432053330838,15.2,6.85073233402004));
#205668=CARTESIAN_POINT('Ctrl Pts',(8.23951804226024,15.2,6.8530944102759));
#205669=CARTESIAN_POINT('Ctrl Pts',(8.24397304970202,15.2,6.85511904696153));
#205670=CARTESIAN_POINT('Ctrl Pts',(8.24846742258604,15.2,6.85714763152989));
#205671=CARTESIAN_POINT('Ctrl Pts',(8.25300090525296,15.2,6.85917967612258));
#205672=CARTESIAN_POINT('Ctrl Pts',(8.25677880761266,15.2,6.86087304667802));
#205673=CARTESIAN_POINT('Ctrl Pts',(8.26058386717306,15.2,6.86256881853906));
#205674=CARTESIAN_POINT('Ctrl Pts',(8.26441593849109,15.2,6.86426671416395));
#205675=CARTESIAN_POINT('Ctrl Pts',(8.2674815957126,15.2,6.86562503073789));
#205676=CARTESIAN_POINT('Ctrl Pts',(8.27056453818561,15.2,6.86698470646354));
#205677=CARTESIAN_POINT('Ctrl Pts',(8.27366469173316,15.2,6.86834560043913));
#205678=CARTESIAN_POINT('Ctrl Pts',(8.27676484485831,15.2,6.8697064942293));
#205679=CARTESIAN_POINT('Ctrl Pts',(8.27988220832615,15.2,6.87106860519172));
#205680=CARTESIAN_POINT('Ctrl Pts',(8.28301670723546,15.2,6.87243179691355));
#205681=CARTESIAN_POINT('Ctrl Pts',(8.28693483119239,15.2,6.87413578670513));
#205682=CARTESIAN_POINT('Ctrl Pts',(8.29087972869169,15.2,6.87584146109397));
#205683=CARTESIAN_POINT('Ctrl Pts',(8.29485125348197,15.2,6.87754855512168));
#205684=CARTESIAN_POINT('Ctrl Pts',(8.29802847348734,15.2,6.87891423041827));
#205685=CARTESIAN_POINT('Ctrl Pts',(8.30122273636515,15.2,6.8802808128305));
#205686=CARTESIAN_POINT('Ctrl Pts',(8.30443396542428,15.2,6.8816481694734));
#205687=CARTESIAN_POINT('Ctrl Pts',(8.30764519404587,15.2,6.88301552592999));
#205688=CARTESIAN_POINT('Ctrl Pts',(8.31087339048169,15.2,6.88438365272502));
#205689=CARTESIAN_POINT('Ctrl Pts',(8.31411847949309,15.2,6.88575242044642));
#205690=CARTESIAN_POINT('Ctrl Pts',(8.31736356894661,15.2,6.88712118835431));
#205691=CARTESIAN_POINT('Ctrl Pts',(8.32062555191328,15.2,6.88849059515674));
#205692=CARTESIAN_POINT('Ctrl Pts',(8.32390435525974,15.2,6.88986050862031));
#205693=CARTESIAN_POINT('Ctrl Pts',(8.32882255983269,15.2,6.89191537862903));
#205694=CARTESIAN_POINT('Ctrl Pts',(8.33377860822313,15.2,6.8939713904061));
#205695=CARTESIAN_POINT('Ctrl Pts',(8.33877225306428,15.2,6.89602810325738));
#205696=CARTESIAN_POINT('Ctrl Pts',(8.34293362391644,15.2,6.89774203069572));
#205697=CARTESIAN_POINT('Ctrl Pts',(8.34712110417766,15.2,6.89945644667221));
#205698=CARTESIAN_POINT('Ctrl Pts',(8.3513345522332,15.2,6.90117109924165));
#205699=CARTESIAN_POINT('Ctrl Pts',(8.35639068971615,15.2,6.90322868225023));
#205700=CARTESIAN_POINT('Ctrl Pts',(8.36148422029424,15.2,6.90528660824788));
#205701=CARTESIAN_POINT('Ctrl Pts',(8.36661490027864,15.2,6.90734444952591));
#205702=CARTESIAN_POINT('Ctrl Pts',(8.37003535391226,15.2,6.90871634383588));
#205703=CARTESIAN_POINT('Ctrl Pts',(8.37347231927362,15.2,6.91008820280404));
#205704=CARTESIAN_POINT('Ctrl Pts',(8.37692572274069,15.2,6.91145990087879));
#205705=CARTESIAN_POINT('Ctrl Pts',(8.38037912573722,15.2,6.91283159876665));
#205706=CARTESIAN_POINT('Ctrl Pts',(8.38384896876655,15.2,6.91420313515452));
#205707=CARTESIAN_POINT('Ctrl Pts',(8.38733517914656,15.2,6.91557438904245));
#205708=CARTESIAN_POINT('Ctrl Pts',(8.39082139000155,15.2,6.91694564311721));
#205709=CARTESIAN_POINT('Ctrl Pts',(8.39432396855558,15.2,6.91831661176722));
#205710=CARTESIAN_POINT('Ctrl Pts',(8.39784284398562,15.2,6.91968717779259));
#205711=CARTESIAN_POINT('Ctrl Pts',(8.4013617189362,15.2,6.92105774363121));
#205712=CARTESIAN_POINT('Ctrl Pts',(8.40489689168066,15.2,6.92242790392408));
#205713=CARTESIAN_POINT('Ctrl Pts',(8.40844828944424,15.2,6.92379754053439));
#205714=CARTESIAN_POINT('Ctrl Pts',(8.4128875370116,15.2,6.92550958643724));
#205715=CARTESIAN_POINT('Ctrl Pts',(8.41735213705356,15.2,6.92722081255954));
#205716=CARTESIAN_POINT('Ctrl Pts',(8.42184195441262,15.2,6.92893098776796));
#205717=CARTESIAN_POINT('Ctrl Pts',(8.42543380849563,15.2,6.93029912800927));
#205718=CARTESIAN_POINT('Ctrl Pts',(8.42904179966334,15.2,6.93166659563968));
#205719=CARTESIAN_POINT('Ctrl Pts',(8.43266585971069,15.2,6.93303327444259));
#205720=CARTESIAN_POINT('Ctrl Pts',(8.43628991926425,15.2,6.93439995305928));
#205721=CARTESIAN_POINT('Ctrl Pts',(8.43993004723596,15.2,6.93576584229665));
#205722=CARTESIAN_POINT('Ctrl Pts',(8.44358617293545,15.2,6.93713082701848));
#205723=CARTESIAN_POINT('Ctrl Pts',(8.44724229913307,15.2,6.9384958119263));
#205724=CARTESIAN_POINT('Ctrl Pts',(8.45091442455165,15.2,6.93985989181737));
#205725=CARTESIAN_POINT('Ctrl Pts',(8.45460247747488,15.2,6.94122295272499));
#205726=CARTESIAN_POINT('Ctrl Pts',(8.4582905303981,15.2,6.94258601363261));
#205727=CARTESIAN_POINT('Ctrl Pts',(8.46199451388984,15.2,6.94394805657623));
#205728=CARTESIAN_POINT('Ctrl Pts',(8.46571435614975,15.2,6.94530896620583));
#205729=CARTESIAN_POINT('Ctrl Pts',(8.46943419790283,15.2,6.94666987565001));
#205730=CARTESIAN_POINT('Ctrl Pts',(8.47316990067037,15.2,6.9480296532595));
#205731=CARTESIAN_POINT('Ctrl Pts',(8.47692139304733,15.2,6.94938818726573));
#205732=CARTESIAN_POINT('Ctrl Pts',(8.48067288593543,15.2,6.95074672145705));
#205733=CARTESIAN_POINT('Ctrl Pts',(8.4844401705273,15.2,6.95210401142293));
#205734=CARTESIAN_POINT('Ctrl Pts',(8.48822317740175,15.2,6.95345994766336));
#205735=CARTESIAN_POINT('Ctrl Pts',(8.49200618376075,15.2,6.95481588371903));
#205736=CARTESIAN_POINT('Ctrl Pts',(8.4958049122955,15.2,6.95617046591377));
#205737=CARTESIAN_POINT('Ctrl Pts',(8.49961929520487,15.2,6.95752358341436));
#205738=CARTESIAN_POINT('Ctrl Pts',(8.50343367863396,15.2,6.95887670109932));
#205739=CARTESIAN_POINT('Ctrl Pts',(8.5072637163538,15.2,6.96022835550076));
#205740=CARTESIAN_POINT('Ctrl Pts',(8.51110934056441,15.2,6.96157843785201));
#205741=CARTESIAN_POINT('Ctrl Pts',(8.51495496425105,15.2,6.96292852001931));
#205742=CARTESIAN_POINT('Ctrl Pts',(8.51881617377869,15.2,6.96427703102499));
#205743=CARTESIAN_POINT('Ctrl Pts',(8.5226929016541,15.2,6.96562386253788));
#205744=CARTESIAN_POINT('Ctrl Pts',(8.52656963005771,15.2,6.96697069423427));
#205745=CARTESIAN_POINT('Ctrl Pts',(8.53046187844162,15.2,6.96831584733116));
#205746=CARTESIAN_POINT('Ctrl Pts',(8.53436957604449,15.2,6.96965921562646));
#205747=CARTESIAN_POINT('Ctrl Pts',(8.53925419778185,15.2,6.97133842590408));
#205748=CARTESIAN_POINT('Ctrl Pts',(8.54416296360471,15.2,6.97301484654846));
#205749=CARTESIAN_POINT('Ctrl Pts',(8.54909573860597,15.2,6.97468827515942));
#205750=CARTESIAN_POINT('Ctrl Pts',(8.55304195828437,15.2,6.97602701793874));
#205751=CARTESIAN_POINT('Ctrl Pts',(8.55700354563677,15.2,6.97736384454578));
#205752=CARTESIAN_POINT('Ctrl Pts',(8.5609804328979,15.2,6.97869865278129));
#205753=CARTESIAN_POINT('Ctrl Pts',(8.5659515423807,15.2,6.98036716321209));
#205754=CARTESIAN_POINT('Ctrl Pts',(8.57094655775082,15.2,6.98203252032999));
#205755=CARTESIAN_POINT('Ctrl Pts',(8.57596535018013,15.2,6.98369452164961));
#205756=CARTESIAN_POINT('Ctrl Pts',(8.58098414260944,15.2,6.98535652296923));
#205757=CARTESIAN_POINT('Ctrl Pts',(8.58602671143105,15.2,6.98701517233044));
#205758=CARTESIAN_POINT('Ctrl Pts',(8.5910929271937,15.2,6.98867026865006));
#205759=CARTESIAN_POINT('Ctrl Pts',(8.59514590002471,15.2,6.98999434577792));
#205760=CARTESIAN_POINT('Ctrl Pts',(8.59921400666464,15.2,6.99131615112604));
#205761=CARTESIAN_POINT('Ctrl Pts',(8.60329718109246,15.2,6.99263558370811));
#205762=CARTESIAN_POINT('Ctrl Pts',(8.60738035496396,15.2,6.9939550161104));
#205763=CARTESIAN_POINT('Ctrl Pts',(8.61147859665379,15.2,6.99527207738314));
#205764=CARTESIAN_POINT('Ctrl Pts',(8.6155918403721,15.2,6.99658666694251));
#205765=CARTESIAN_POINT('Ctrl Pts',(8.62073339544031,15.2,6.99822990402604));
#205766=CARTESIAN_POINT('Ctrl Pts',(8.62589839201748,15.2,6.99986928193725));
#205767=CARTESIAN_POINT('Ctrl Pts',(8.63108670041905,15.2,7.00150460665969));
#205768=CARTESIAN_POINT('Ctrl Pts',(8.63523734736651,15.2,7.00281286650893));
#205769=CARTESIAN_POINT('Ctrl Pts',(8.63940291529916,15.2,7.00411853426429));
#205770=CARTESIAN_POINT('Ctrl Pts',(8.64358333834824,15.2,7.00542151395572));
#205771=CARTESIAN_POINT('Ctrl Pts',(8.64880886687479,15.2,7.00705023848124));
#205772=CARTESIAN_POINT('Ctrl Pts',(8.65405760473756,15.2,7.00867475937892));
#205773=CARTESIAN_POINT('Ctrl Pts',(8.65932942723945,15.2,7.01029489396191));
#205774=CARTESIAN_POINT('Ctrl Pts',(8.66460124974133,15.2,7.01191502854488));
#205775=CARTESIAN_POINT('Ctrl Pts',(8.66989615470471,15.2,7.01353077432778));
#205776=CARTESIAN_POINT('Ctrl Pts',(8.67521401797047,15.2,7.01514194974407));
#205777=CARTESIAN_POINT('Ctrl Pts',(8.678404735814,15.2,7.01610865495873));
#205778=CARTESIAN_POINT('Ctrl Pts',(8.68160371834249,15.2,7.01707371485678));
#205779=CARTESIAN_POINT('Ctrl Pts',(8.68481093838715,15.2,7.01803708920303));
#205780=CARTESIAN_POINT('Ctrl Pts',(8.69015630532246,15.2,7.01964271317181));
#205781=CARTESIAN_POINT('Ctrl Pts',(8.69552455294763,15.2,7.02124365742027));
#205782=CARTESIAN_POINT('Ctrl Pts',(8.7009155564217,15.2,7.02283974047543));
#205783=CARTESIAN_POINT('Ctrl Pts',(8.70522835884839,15.2,7.02411660681517));
#205784=CARTESIAN_POINT('Ctrl Pts',(8.70955572516209,15.2,7.02539036435254));
#205785=CARTESIAN_POINT('Ctrl Pts',(8.71389759136174,15.2,7.02666091863777));
#205786=CARTESIAN_POINT('Ctrl Pts',(8.71823945815298,15.2,7.02793147309611));
#205787=CARTESIAN_POINT('Ctrl Pts',(8.7225958249986,15.2,7.02919882436553));
#205788=CARTESIAN_POINT('Ctrl Pts',(8.72696662690087,15.2,7.03046288544174));
#205789=CARTESIAN_POINT('Ctrl Pts',(8.73133742820762,15.2,7.03172694634571));
#205790=CARTESIAN_POINT('Ctrl Pts',(8.73572266593428,15.2,7.03298771405252));
#205791=CARTESIAN_POINT('Ctrl Pts',(8.74012227490702,15.2,7.03424510167218));
#205792=CARTESIAN_POINT('Ctrl Pts',(8.74342198178643,15.2,7.03518814242974));
#205793=CARTESIAN_POINT('Ctrl Pts',(8.74672977284861,15.2,7.03612928097911));
#205794=CARTESIAN_POINT('Ctrl Pts',(8.7500456212687,15.2,7.03706847932025));
#205795=CARTESIAN_POINT('Ctrl Pts',(8.75336147029117,15.2,7.03800767783202));
#205796=CARTESIAN_POINT('Ctrl Pts',(8.75668537695759,15.2,7.03894493760156));
#205797=CARTESIAN_POINT('Ctrl Pts',(8.76001731444292,15.2,7.03988022148722));
#205798=CARTESIAN_POINT('Ctrl Pts',(8.76334925132296,15.2,7.04081550520297));
#205799=CARTESIAN_POINT('Ctrl Pts',(8.76668921910117,15.2,7.04174881133438));
#205800=CARTESIAN_POINT('Ctrl Pts',(8.77003719064772,15.2,7.04268010468016));
#205801=CARTESIAN_POINT('Ctrl Pts',(8.77338516219426,15.2,7.04361139802594));
#205802=CARTESIAN_POINT('Ctrl Pts',(8.77674113722156,15.2,7.04454067848491));
#205803=CARTESIAN_POINT('Ctrl Pts',(8.78010509010003,15.2,7.0454679083677));
#205804=CARTESIAN_POINT('Ctrl Pts',(8.78346904297849,15.2,7.0463951382505));
#205805=CARTESIAN_POINT('Ctrl Pts',(8.78684097383936,15.2,7.04732031893354));
#205806=CARTESIAN_POINT('Ctrl Pts',(8.79022085479988,15.2,7.04824341369167));
#205807=CARTESIAN_POINT('Ctrl Pts',(8.79360073576041,15.2,7.04916650844979));
#205808=CARTESIAN_POINT('Ctrl Pts',(8.79698856788729,15.2,7.050087516683));
#205809=CARTESIAN_POINT('Ctrl Pts',(8.80038432380488,15.2,7.05100640294147));
#205810=CARTESIAN_POINT('Ctrl Pts',(8.80378007972247,15.2,7.05192528919994));
#205811=CARTESIAN_POINT('Ctrl Pts',(8.80718375964434,15.2,7.05284205296031));
#205812=CARTESIAN_POINT('Ctrl Pts',(8.81059533860658,15.2,7.05375665930636));
#205813=CARTESIAN_POINT('Ctrl Pts',(8.81514411096941,15.2,7.05497613454518));
#205814=CARTESIAN_POINT('Ctrl Pts',(8.81970692394604,15.2,7.05619177325824));
#205815=CARTESIAN_POINT('Ctrl Pts',(8.82428371364084,15.2,7.05740349182402));
#205816=CARTESIAN_POINT('Ctrl Pts',(8.82771630560014,15.2,7.05831228066581));
#205817=CARTESIAN_POINT('Ctrl Pts',(8.83115676039184,15.2,7.05921886484952));
#205818=CARTESIAN_POINT('Ctrl Pts',(8.83460505222489,15.2,7.06012320773334));
#205819=CARTESIAN_POINT('Ctrl Pts',(8.84035220548878,15.2,7.06163044592778));
#205820=CARTESIAN_POINT('Ctrl Pts',(8.84612112553322,15.2,7.06313146240556));
#205821=CARTESIAN_POINT('Ctrl Pts',(8.85191169219989,15.2,7.06462609455834));
#205822=CARTESIAN_POINT('Ctrl Pts',(8.85538603207365,15.2,7.06552287381742));
#205823=CARTESIAN_POINT('Ctrl Pts',(8.85886816501377,15.2,7.06641735453493));
#205824=CARTESIAN_POINT('Ctrl Pts',(8.86235806388629,15.2,7.06730950191939));
#205825=CARTESIAN_POINT('Ctrl Pts',(8.8658479627588,15.2,7.06820164930383));
#205826=CARTESIAN_POINT('Ctrl Pts',(8.86934562747489,15.2,7.06909146398258));
#205827=CARTESIAN_POINT('Ctrl Pts',(8.87285103356343,15.2,7.06997891232828));
#205828=CARTESIAN_POINT('Ctrl Pts',(8.87635643965195,15.2,7.07086636067398));
#205829=CARTESIAN_POINT('Ctrl Pts',(8.87986958697799,15.2,7.07175144172265));
#205830=CARTESIAN_POINT('Ctrl Pts',(8.88339044697402,15.2,7.07263412156592));
#205831=CARTESIAN_POINT('Ctrl Pts',(8.88691130760967,15.2,7.07351680156952));
#205832=CARTESIAN_POINT('Ctrl Pts',(8.89043988288915,15.2,7.07439708039745));
#205833=CARTESIAN_POINT('Ctrl Pts',(8.89397614648747,15.2,7.07527492444137));
#205834=CARTESIAN_POINT('Ctrl Pts',(8.89751240944337,15.2,7.07615276832581));
#205835=CARTESIAN_POINT('Ctrl Pts',(8.90105636173219,15.2,7.07702817797705));
#205836=CARTESIAN_POINT('Ctrl Pts',(8.90460797560381,15.2,7.07790111882011));
#205837=CARTESIAN_POINT('Ctrl Pts',(8.90815958947543,15.2,7.07877405966317));
#205838=CARTESIAN_POINT('Ctrl Pts',(8.9117188656665,15.2,7.07964453202839));
#205839=CARTESIAN_POINT('Ctrl Pts',(8.9152857780948,15.2,7.08051250379246));
#205840=CARTESIAN_POINT('Ctrl Pts',(8.92004166111654,15.2,7.08166979942532));
#205841=CARTESIAN_POINT('Ctrl Pts',(8.92481112116026,15.2,7.08282264736955));
#205842=CARTESIAN_POINT('Ctrl Pts',(8.92959409476788,15.2,7.08397096855392));
#205843=CARTESIAN_POINT('Ctrl Pts',(8.93318132578819,15.2,7.08483220963776));
#205844=CARTESIAN_POINT('Ctrl Pts',(8.93677615801064,15.2,7.08569090512924));
#205845=CARTESIAN_POINT('Ctrl Pts',(8.94037856753523,15.2,7.08654702266997));
#205846=CARTESIAN_POINT('Ctrl Pts',(8.94518177914394,15.2,7.08768851246506));
#205847=CARTESIAN_POINT('Ctrl Pts',(8.94999845940367,15.2,7.0888254192441));
#205848=CARTESIAN_POINT('Ctrl Pts',(8.95482854839683,15.2,7.0899576657074));
#205849=CARTESIAN_POINT('Ctrl Pts',(8.96086616013184,15.2,7.09137297390223));
#205850=CARTESIAN_POINT('Ctrl Pts',(8.96692472264126,15.2,7.09278100124842));
#205851=CARTESIAN_POINT('Ctrl Pts',(8.97300411273825,15.2,7.09418159278257));
#205852=CARTESIAN_POINT('Ctrl Pts',(8.97665174666391,15.2,7.09502194767254));
#205853=CARTESIAN_POINT('Ctrl Pts',(8.98030687810118,15.2,7.09585962672239));
#205854=CARTESIAN_POINT('Ctrl Pts',(8.98396948459246,15.2,7.09669459969228));
#205855=CARTESIAN_POINT('Ctrl Pts',(8.98763209108373,15.2,7.09752957266218));
#205856=CARTESIAN_POINT('Ctrl Pts',(8.99130217374949,15.2,7.09836184023226));
#205857=CARTESIAN_POINT('Ctrl Pts',(8.99497970615653,15.2,7.09919137303583));
#205858=CARTESIAN_POINT('Ctrl Pts',(8.99865723923164,15.2,7.1000209059901));
#205859=CARTESIAN_POINT('Ctrl Pts',(9.00234222280053,15.2,7.10084770277693));
#205860=CARTESIAN_POINT('Ctrl Pts',(9.00603462575484,15.2,7.10167172614631));
#205861=CARTESIAN_POINT('Ctrl Pts',(9.01218862911353,15.2,7.10304509807931));
#205862=CARTESIAN_POINT('Ctrl Pts',(9.01836323491096,15.2,7.10441075245865));
#205863=CARTESIAN_POINT('Ctrl Pts',(9.02455833645625,15.2,7.1057685652974));
#205864=CARTESIAN_POINT('Ctrl Pts',(9.0295144185028,15.2,7.106854815746));
#205865=CARTESIAN_POINT('Ctrl Pts',(9.03448362264226,15.2,7.1079360497067));
#205866=CARTESIAN_POINT('Ctrl Pts',(9.03946594399994,15.2,7.10901226999999));
#205867=CARTESIAN_POINT('Ctrl Pts',(8.56667970899995,15.2,5.85257411499998));
#205868=CARTESIAN_POINT('Ctrl Pts',(8.56667970899995,11.6,5.85257411499998));
#205869=CARTESIAN_POINT('Ctrl Pts',(8.56681469199994,15.2,5.85268447899999));
#205870=CARTESIAN_POINT('Ctrl Pts',(8.56681469199994,11.6,5.85268447899999));
#205871=CARTESIAN_POINT('Ctrl Pts',(8.56708931799994,15.2,5.85290912899998));
#205872=CARTESIAN_POINT('Ctrl Pts',(8.56708931799994,11.6,5.85290912899998));
#205873=CARTESIAN_POINT('Ctrl Pts',(8.56750527399995,15.2,5.85324973199998));
#205874=CARTESIAN_POINT('Ctrl Pts',(8.56750527399995,11.6,5.85324973199998));
#205875=CARTESIAN_POINT('Ctrl Pts',(8.56806526099994,15.2,5.85370897499998));
#205876=CARTESIAN_POINT('Ctrl Pts',(8.56806526099994,11.6,5.85370897499998));
#205877=CARTESIAN_POINT('Ctrl Pts',(8.56877298299995,15.2,5.85429055399998));
#205878=CARTESIAN_POINT('Ctrl Pts',(8.56877298299995,11.6,5.85429055399998));
#205879=CARTESIAN_POINT('Ctrl Pts',(8.56949158199994,15.2,5.85488228199999));
#205880=CARTESIAN_POINT('Ctrl Pts',(8.56949158199994,11.6,5.85488228199999));
#205881=CARTESIAN_POINT('Ctrl Pts',(8.57021692599995,15.2,5.85548078499999));
#205882=CARTESIAN_POINT('Ctrl Pts',(8.57021692599995,11.6,5.85548078499999));
#205883=CARTESIAN_POINT('Ctrl Pts',(8.57094898299994,15.2,5.85608606099999));
#205884=CARTESIAN_POINT('Ctrl Pts',(8.57094898299994,11.6,5.85608606099999));
#205885=CARTESIAN_POINT('Ctrl Pts',(8.57168771799994,15.2,5.85669810599998));
#205886=CARTESIAN_POINT('Ctrl Pts',(8.57168771799994,11.6,5.85669810599998));
#205887=CARTESIAN_POINT('Ctrl Pts',(8.57243310299994,15.2,5.85731691899999));
#205888=CARTESIAN_POINT('Ctrl Pts',(8.57243310299994,11.6,5.85731691899999));
#205889=CARTESIAN_POINT('Ctrl Pts',(8.57318510299995,15.2,5.85794249299998));
#205890=CARTESIAN_POINT('Ctrl Pts',(8.57318510299995,11.6,5.85794249299998));
#205891=CARTESIAN_POINT('Ctrl Pts',(8.57394368799994,15.2,5.85857482799998));
#205892=CARTESIAN_POINT('Ctrl Pts',(8.57394368799994,11.6,5.85857482799998));
#205893=CARTESIAN_POINT('Ctrl Pts',(8.57470882599995,15.2,5.85921391999998));
#205894=CARTESIAN_POINT('Ctrl Pts',(8.57470882599995,11.6,5.85921391999998));
#205895=CARTESIAN_POINT('Ctrl Pts',(8.57548048599994,15.2,5.85985976499998));
#205896=CARTESIAN_POINT('Ctrl Pts',(8.57548048599994,11.6,5.85985976499998));
#205897=CARTESIAN_POINT('Ctrl Pts',(8.57625863499995,15.2,5.86051236099999));
#205898=CARTESIAN_POINT('Ctrl Pts',(8.57625863499995,11.6,5.86051236099999));
#205899=CARTESIAN_POINT('Ctrl Pts',(8.57704324399995,15.2,5.86117170499998));
#205900=CARTESIAN_POINT('Ctrl Pts',(8.57704324399995,11.6,5.86117170499998));
#205901=CARTESIAN_POINT('Ctrl Pts',(8.57783427999994,15.2,5.86183779199998));
#205902=CARTESIAN_POINT('Ctrl Pts',(8.57783427999994,11.6,5.86183779199998));
#205903=CARTESIAN_POINT('Ctrl Pts',(8.57863171399995,15.2,5.86251061999998));
#205904=CARTESIAN_POINT('Ctrl Pts',(8.57863171399995,11.6,5.86251061999998));
#205905=CARTESIAN_POINT('Ctrl Pts',(8.57943551499995,15.2,5.86319018599998));
#205906=CARTESIAN_POINT('Ctrl Pts',(8.57943551499995,11.6,5.86319018599998));
#205907=CARTESIAN_POINT('Ctrl Pts',(8.58024565199995,15.2,5.86387648699999));
#205908=CARTESIAN_POINT('Ctrl Pts',(8.58024565199995,11.6,5.86387648699999));
#205909=CARTESIAN_POINT('Ctrl Pts',(8.58106209399994,15.2,5.86456951899999));
#205910=CARTESIAN_POINT('Ctrl Pts',(8.58106209399994,11.6,5.86456951899999));
#205911=CARTESIAN_POINT('Ctrl Pts',(8.58188481199995,15.2,5.86526927999999));
#205912=CARTESIAN_POINT('Ctrl Pts',(8.58188481199995,11.6,5.86526927999999));
#205913=CARTESIAN_POINT('Ctrl Pts',(8.58271377499995,15.2,5.86597576499998));
#205914=CARTESIAN_POINT('Ctrl Pts',(8.58271377499995,11.6,5.86597576499998));
#205915=CARTESIAN_POINT('Ctrl Pts',(8.58354895399994,15.2,5.86668897399999));
#205916=CARTESIAN_POINT('Ctrl Pts',(8.58354895399994,11.6,5.86668897399999));
#205917=CARTESIAN_POINT('Ctrl Pts',(8.58439031899995,15.2,5.86740889999999));
#205918=CARTESIAN_POINT('Ctrl Pts',(8.58439031899995,11.6,5.86740889999999));
#205919=CARTESIAN_POINT('Ctrl Pts',(8.58523783999994,15.2,5.86813554199999));
#205920=CARTESIAN_POINT('Ctrl Pts',(8.58523783999994,11.6,5.86813554199999));
#205921=CARTESIAN_POINT('Ctrl Pts',(8.58609148699994,15.2,5.86886889799998));
#205922=CARTESIAN_POINT('Ctrl Pts',(8.58609148699994,11.6,5.86886889799998));
#205923=CARTESIAN_POINT('Ctrl Pts',(8.58695123199994,15.2,5.86960896199999));
#205924=CARTESIAN_POINT('Ctrl Pts',(8.58695123199994,11.6,5.86960896199999));
#205925=CARTESIAN_POINT('Ctrl Pts',(8.58781704399994,15.2,5.87035573299998));
#205926=CARTESIAN_POINT('Ctrl Pts',(8.58781704399994,11.6,5.87035573299998));
#205927=CARTESIAN_POINT('Ctrl Pts',(8.58868889599994,15.2,5.87110920699998));
#205928=CARTESIAN_POINT('Ctrl Pts',(8.58868889599994,11.6,5.87110920699998));
#205929=CARTESIAN_POINT('Ctrl Pts',(8.58956675699994,15.2,5.87186937999999));
#205930=CARTESIAN_POINT('Ctrl Pts',(8.58956675699994,11.6,5.87186937999999));
#205931=CARTESIAN_POINT('Ctrl Pts',(8.59045059999995,15.2,5.87263625099999));
#205932=CARTESIAN_POINT('Ctrl Pts',(8.59045059999995,11.6,5.87263625099999));
#205933=CARTESIAN_POINT('Ctrl Pts',(8.59134039399994,15.2,5.87340981499998));
#205934=CARTESIAN_POINT('Ctrl Pts',(8.59134039399994,11.6,5.87340981499998));
#205935=CARTESIAN_POINT('Ctrl Pts',(8.59223611299995,15.2,5.87419006999998));
#205936=CARTESIAN_POINT('Ctrl Pts',(8.59223611299995,11.6,5.87419006999998));
#205937=CARTESIAN_POINT('Ctrl Pts',(8.59313772599995,15.2,5.87497701299998));
#205938=CARTESIAN_POINT('Ctrl Pts',(8.59313772599995,11.6,5.87497701299998));
#205939=CARTESIAN_POINT('Ctrl Pts',(8.59404520799994,15.2,5.87577063899998));
#205940=CARTESIAN_POINT('Ctrl Pts',(8.59404520799994,11.6,5.87577063899998));
#205941=CARTESIAN_POINT('Ctrl Pts',(8.59495852899994,15.2,5.87657094699999));
#205942=CARTESIAN_POINT('Ctrl Pts',(8.59495852899994,11.6,5.87657094699999));
#205943=CARTESIAN_POINT('Ctrl Pts',(8.59587765999994,15.2,5.87737793199998));
#205944=CARTESIAN_POINT('Ctrl Pts',(8.59587765999994,11.6,5.87737793199998));
#205945=CARTESIAN_POINT('Ctrl Pts',(8.59680257499994,15.2,5.87819159299999));
#205946=CARTESIAN_POINT('Ctrl Pts',(8.59680257499994,11.6,5.87819159299999));
#205947=CARTESIAN_POINT('Ctrl Pts',(8.59773324399994,15.2,5.87901192399999));
#205948=CARTESIAN_POINT('Ctrl Pts',(8.59773324399994,11.6,5.87901192399999));
#205949=CARTESIAN_POINT('Ctrl Pts',(8.59866964199994,15.2,5.87983892599999));
#205950=CARTESIAN_POINT('Ctrl Pts',(8.59866964199994,11.6,5.87983892599999));
#205951=CARTESIAN_POINT('Ctrl Pts',(8.59961173899995,15.2,5.88067259099999));
#205952=CARTESIAN_POINT('Ctrl Pts',(8.59961173899995,11.6,5.88067259099999));
#205953=CARTESIAN_POINT('Ctrl Pts',(8.60055950899994,15.2,5.88151291899998));
#205954=CARTESIAN_POINT('Ctrl Pts',(8.60055950899994,11.6,5.88151291899998));
#205955=CARTESIAN_POINT('Ctrl Pts',(8.60151292399994,15.2,5.88235990599999));
#205956=CARTESIAN_POINT('Ctrl Pts',(8.60151292399994,11.6,5.88235990599999));
#205957=CARTESIAN_POINT('Ctrl Pts',(8.60247195899994,15.2,5.88321354999999));
#205958=CARTESIAN_POINT('Ctrl Pts',(8.60247195899994,11.6,5.88321354999999));
#205959=CARTESIAN_POINT('Ctrl Pts',(8.60343658399995,15.2,5.88407384599999));
#205960=CARTESIAN_POINT('Ctrl Pts',(8.60343658399995,11.6,5.88407384599999));
#205961=CARTESIAN_POINT('Ctrl Pts',(8.60440677399994,15.2,5.88494079199998));
#205962=CARTESIAN_POINT('Ctrl Pts',(8.60440677399994,11.6,5.88494079199998));
#205963=CARTESIAN_POINT('Ctrl Pts',(8.60538250099994,15.2,5.88581438399999));
#205964=CARTESIAN_POINT('Ctrl Pts',(8.60538250099994,11.6,5.88581438399999));
#205965=CARTESIAN_POINT('Ctrl Pts',(8.60636373899995,15.2,5.88669461999999));
#205966=CARTESIAN_POINT('Ctrl Pts',(8.60636373899995,11.6,5.88669461999999));
#205967=CARTESIAN_POINT('Ctrl Pts',(8.60735046099995,15.2,5.88758149599999));
#205968=CARTESIAN_POINT('Ctrl Pts',(8.60735046099995,11.6,5.88758149599999));
#205969=CARTESIAN_POINT('Ctrl Pts',(8.60834264199994,15.2,5.88847500899998));
#205970=CARTESIAN_POINT('Ctrl Pts',(8.60834264199994,11.6,5.88847500899998));
#205971=CARTESIAN_POINT('Ctrl Pts',(8.60934025399994,15.2,5.88937515599999));
#205972=CARTESIAN_POINT('Ctrl Pts',(8.60934025399994,11.6,5.88937515599999));
#205973=CARTESIAN_POINT('Ctrl Pts',(8.61034327099994,15.2,5.89028193299999));
#205974=CARTESIAN_POINT('Ctrl Pts',(8.61034327099994,11.6,5.89028193299999));
#205975=CARTESIAN_POINT('Ctrl Pts',(8.61135166799994,15.2,5.89119533799998));
#205976=CARTESIAN_POINT('Ctrl Pts',(8.61135166799994,11.6,5.89119533799998));
#205977=CARTESIAN_POINT('Ctrl Pts',(8.61236541699994,15.2,5.89211536899998));
#205978=CARTESIAN_POINT('Ctrl Pts',(8.61236541699994,11.6,5.89211536899998));
#205979=CARTESIAN_POINT('Ctrl Pts',(8.61338449399994,15.2,5.89304202099999));
#205980=CARTESIAN_POINT('Ctrl Pts',(8.61338449399994,11.6,5.89304202099999));
#205981=CARTESIAN_POINT('Ctrl Pts',(8.61440887299995,15.2,5.89397528999999));
#205982=CARTESIAN_POINT('Ctrl Pts',(8.61440887299995,11.6,5.89397528999999));
#205983=CARTESIAN_POINT('Ctrl Pts',(8.61543852799995,15.2,5.89491517399999));
#205984=CARTESIAN_POINT('Ctrl Pts',(8.61543852799995,11.6,5.89491517399999));
#205985=CARTESIAN_POINT('Ctrl Pts',(8.61647343299994,15.2,5.89586167199998));
#205986=CARTESIAN_POINT('Ctrl Pts',(8.61647343299994,11.6,5.89586167199998));
#205987=CARTESIAN_POINT('Ctrl Pts',(8.61751356299994,15.2,5.89681477699998));
#205988=CARTESIAN_POINT('Ctrl Pts',(8.61751356299994,11.6,5.89681477699998));
#205989=CARTESIAN_POINT('Ctrl Pts',(8.61855889399994,15.2,5.89777448799998));
#205990=CARTESIAN_POINT('Ctrl Pts',(8.61855889399994,11.6,5.89777448799998));
#205991=CARTESIAN_POINT('Ctrl Pts',(8.61960939799994,15.2,5.89874080299998));
#205992=CARTESIAN_POINT('Ctrl Pts',(8.61960939799994,11.6,5.89874080299998));
#205993=CARTESIAN_POINT('Ctrl Pts',(8.62066505299994,15.2,5.89971371599999));
#205994=CARTESIAN_POINT('Ctrl Pts',(8.62066505299994,11.6,5.89971371599999));
#205995=CARTESIAN_POINT('Ctrl Pts',(8.62172582999994,15.2,5.90069322599999));
#205996=CARTESIAN_POINT('Ctrl Pts',(8.62172582999994,11.6,5.90069322599999));
#205997=CARTESIAN_POINT('Ctrl Pts',(8.62279170899994,15.2,5.90167932799999));
#205998=CARTESIAN_POINT('Ctrl Pts',(8.62279170899994,11.6,5.90167932799999));
#205999=CARTESIAN_POINT('Ctrl Pts',(8.62386266099995,15.2,5.90267202099999));
#206000=CARTESIAN_POINT('Ctrl Pts',(8.62386266099995,11.6,5.90267202099999));
#206001=CARTESIAN_POINT('Ctrl Pts',(8.62493866399995,15.2,5.90367129999999));
#206002=CARTESIAN_POINT('Ctrl Pts',(8.62493866399995,11.6,5.90367129999999));
#206003=CARTESIAN_POINT('Ctrl Pts',(8.62601969299994,15.2,5.90467716399999));
#206004=CARTESIAN_POINT('Ctrl Pts',(8.62601969299994,11.6,5.90467716399999));
#206005=CARTESIAN_POINT('Ctrl Pts',(8.62710572199994,15.2,5.90568960799998));
#206006=CARTESIAN_POINT('Ctrl Pts',(8.62710572199994,11.6,5.90568960799998));
#206007=CARTESIAN_POINT('Ctrl Pts',(8.62819672799995,15.2,5.90670862899999));
#206008=CARTESIAN_POINT('Ctrl Pts',(8.62819672799995,11.6,5.90670862899999));
#206009=CARTESIAN_POINT('Ctrl Pts',(8.62929268599994,15.2,5.90773422499999));
#206010=CARTESIAN_POINT('Ctrl Pts',(8.62929268599994,11.6,5.90773422499999));
#206011=CARTESIAN_POINT('Ctrl Pts',(8.63039357199994,15.2,5.90876639099999));
#206012=CARTESIAN_POINT('Ctrl Pts',(8.63039357199994,11.6,5.90876639099999));
#206013=CARTESIAN_POINT('Ctrl Pts',(8.63149936299994,15.2,5.90980512599998));
#206014=CARTESIAN_POINT('Ctrl Pts',(8.63149936299994,11.6,5.90980512599998));
#206015=CARTESIAN_POINT('Ctrl Pts',(8.63261003299994,15.2,5.91085042599998));
#206016=CARTESIAN_POINT('Ctrl Pts',(8.63261003299994,11.6,5.91085042599998));
#206017=CARTESIAN_POINT('Ctrl Pts',(8.63372555899995,15.2,5.91190228799999));
#206018=CARTESIAN_POINT('Ctrl Pts',(8.63372555899995,11.6,5.91190228799999));
#206019=CARTESIAN_POINT('Ctrl Pts',(8.63484591899994,15.2,5.91296070799999));
#206020=CARTESIAN_POINT('Ctrl Pts',(8.63484591899994,11.6,5.91296070799999));
#206021=CARTESIAN_POINT('Ctrl Pts',(8.63597108699994,15.2,5.91402568299999));
#206022=CARTESIAN_POINT('Ctrl Pts',(8.63597108699994,11.6,5.91402568299999));
#206023=CARTESIAN_POINT('Ctrl Pts',(8.63710103999994,15.2,5.91509721099998));
#206024=CARTESIAN_POINT('Ctrl Pts',(8.63710103999994,11.6,5.91509721099998));
#206025=CARTESIAN_POINT('Ctrl Pts',(8.63823575599995,15.2,5.91617528699998));
#206026=CARTESIAN_POINT('Ctrl Pts',(8.63823575599995,11.6,5.91617528699998));
#206027=CARTESIAN_POINT('Ctrl Pts',(8.63937520799994,15.2,5.91725990999999));
#206028=CARTESIAN_POINT('Ctrl Pts',(8.63937520799994,11.6,5.91725990999999));
#206029=CARTESIAN_POINT('Ctrl Pts',(8.64051937599994,15.2,5.91835107599999));
#206030=CARTESIAN_POINT('Ctrl Pts',(8.64051937599994,11.6,5.91835107599999));
#206031=CARTESIAN_POINT('Ctrl Pts',(8.64166823699994,15.2,5.91944878099999));
#206032=CARTESIAN_POINT('Ctrl Pts',(8.64166823699994,11.6,5.91944878099999));
#206033=CARTESIAN_POINT('Ctrl Pts',(8.64282176499995,15.2,5.92055302299999));
#206034=CARTESIAN_POINT('Ctrl Pts',(8.64282176499995,11.6,5.92055302299999));
#206035=CARTESIAN_POINT('Ctrl Pts',(8.64397993899994,15.2,5.92166379699999));
#206036=CARTESIAN_POINT('Ctrl Pts',(8.64397993899994,11.6,5.92166379699999));
#206037=CARTESIAN_POINT('Ctrl Pts',(8.64514273599994,15.2,5.92278110299999));
#206038=CARTESIAN_POINT('Ctrl Pts',(8.64514273599994,11.6,5.92278110299999));
#206039=CARTESIAN_POINT('Ctrl Pts',(8.64631013299994,15.2,5.92390493599999));
#206040=CARTESIAN_POINT('Ctrl Pts',(8.64631013299994,11.6,5.92390493599999));
#206041=CARTESIAN_POINT('Ctrl Pts',(8.64748210699995,15.2,5.92503529199998));
#206042=CARTESIAN_POINT('Ctrl Pts',(8.64748210699995,11.6,5.92503529199998));
#206043=CARTESIAN_POINT('Ctrl Pts',(8.64865863499995,15.2,5.92617216999999));
#206044=CARTESIAN_POINT('Ctrl Pts',(8.64865863499995,11.6,5.92617216999999));
#206045=CARTESIAN_POINT('Ctrl Pts',(8.64983969599994,15.2,5.92731556399999));
#206046=CARTESIAN_POINT('Ctrl Pts',(8.64983969599994,11.6,5.92731556399999));
#206047=CARTESIAN_POINT('Ctrl Pts',(8.65102526499994,15.2,5.92846547399999));
#206048=CARTESIAN_POINT('Ctrl Pts',(8.65102526499994,11.6,5.92846547399999));
#206049=CARTESIAN_POINT('Ctrl Pts',(8.65221532199994,15.2,5.92962189399999));
#206050=CARTESIAN_POINT('Ctrl Pts',(8.65221532199994,11.6,5.92962189399999));
#206051=CARTESIAN_POINT('Ctrl Pts',(8.65340984299995,15.2,5.93078482399999));
#206052=CARTESIAN_POINT('Ctrl Pts',(8.65340984299995,11.6,5.93078482399999));
#206053=CARTESIAN_POINT('Ctrl Pts',(8.65460880699995,15.2,5.93195425699999));
#206054=CARTESIAN_POINT('Ctrl Pts',(8.65460880699995,11.6,5.93195425699999));
#206055=CARTESIAN_POINT('Ctrl Pts',(8.65581219099994,15.2,5.93313019299998));
#206056=CARTESIAN_POINT('Ctrl Pts',(8.65581219099994,11.6,5.93313019299998));
#206057=CARTESIAN_POINT('Ctrl Pts',(8.65701997299994,15.2,5.93431262699998));
#206058=CARTESIAN_POINT('Ctrl Pts',(8.65701997299994,11.6,5.93431262699998));
#206059=CARTESIAN_POINT('Ctrl Pts',(8.65823213199995,15.2,5.93550155699998));
#206060=CARTESIAN_POINT('Ctrl Pts',(8.65823213199995,11.6,5.93550155699998));
#206061=CARTESIAN_POINT('Ctrl Pts',(8.65944864499994,15.2,5.93669697899998));
#206062=CARTESIAN_POINT('Ctrl Pts',(8.65944864499994,11.6,5.93669697899998));
#206063=CARTESIAN_POINT('Ctrl Pts',(8.66066948999995,15.2,5.93789889099998));
#206064=CARTESIAN_POINT('Ctrl Pts',(8.66066948999995,11.6,5.93789889099998));
#206065=CARTESIAN_POINT('Ctrl Pts',(8.66189464699995,15.2,5.93910728899999));
#206066=CARTESIAN_POINT('Ctrl Pts',(8.66189464699995,11.6,5.93910728899999));
#206067=CARTESIAN_POINT('Ctrl Pts',(8.66312409299994,15.2,5.94032216899999));
#206068=CARTESIAN_POINT('Ctrl Pts',(8.66312409299994,11.6,5.94032216899999));
#206069=CARTESIAN_POINT('Ctrl Pts',(8.66435780599994,15.2,5.94154352899999));
#206070=CARTESIAN_POINT('Ctrl Pts',(8.66435780599994,11.6,5.94154352899999));
#206071=CARTESIAN_POINT('Ctrl Pts',(8.66559576699995,15.2,5.94277136599998));
#206072=CARTESIAN_POINT('Ctrl Pts',(8.66559576699995,11.6,5.94277136599998));
#206073=CARTESIAN_POINT('Ctrl Pts',(8.66683795199994,15.2,5.94400567599998));
#206074=CARTESIAN_POINT('Ctrl Pts',(8.66683795199994,11.6,5.94400567599998));
#206075=CARTESIAN_POINT('Ctrl Pts',(8.66808433999994,15.2,5.94524645699998));
#206076=CARTESIAN_POINT('Ctrl Pts',(8.66808433999994,11.6,5.94524645699998));
#206077=CARTESIAN_POINT('Ctrl Pts',(8.66933491099994,15.2,5.94649370499998));
#206078=CARTESIAN_POINT('Ctrl Pts',(8.66933491099994,11.6,5.94649370499998));
#206079=CARTESIAN_POINT('Ctrl Pts',(8.67058964199994,15.2,5.94774741499998));
#206080=CARTESIAN_POINT('Ctrl Pts',(8.67058964199994,11.6,5.94774741499998));
#206081=CARTESIAN_POINT('Ctrl Pts',(8.67184851399994,15.2,5.94900758799999));
#206082=CARTESIAN_POINT('Ctrl Pts',(8.67184851399994,11.6,5.94900758799999));
#206083=CARTESIAN_POINT('Ctrl Pts',(8.67311150499994,15.2,5.95027421799998));
#206084=CARTESIAN_POINT('Ctrl Pts',(8.67311150499994,11.6,5.95027421799998));
#206085=CARTESIAN_POINT('Ctrl Pts',(8.67437859499994,15.2,5.95154730199998));
#206086=CARTESIAN_POINT('Ctrl Pts',(8.67437859499994,11.6,5.95154730199998));
#206087=CARTESIAN_POINT('Ctrl Pts',(8.67564976199995,15.2,5.95282683799999));
#206088=CARTESIAN_POINT('Ctrl Pts',(8.67564976199995,11.6,5.95282683799999));
#206089=CARTESIAN_POINT('Ctrl Pts',(8.67692498499994,15.2,5.95411282099998));
#206090=CARTESIAN_POINT('Ctrl Pts',(8.67692498499994,11.6,5.95411282099998));
#206091=CARTESIAN_POINT('Ctrl Pts',(8.67820424499994,15.2,5.95540524999999));
#206092=CARTESIAN_POINT('Ctrl Pts',(8.67820424499994,11.6,5.95540524999999));
#206093=CARTESIAN_POINT('Ctrl Pts',(8.67948751899995,15.2,5.95670411999999));
#206094=CARTESIAN_POINT('Ctrl Pts',(8.67948751899995,11.6,5.95670411999999));
#206095=CARTESIAN_POINT('Ctrl Pts',(8.68077478899994,15.2,5.95800942899999));
#206096=CARTESIAN_POINT('Ctrl Pts',(8.68077478899994,11.6,5.95800942899999));
#206097=CARTESIAN_POINT('Ctrl Pts',(8.68206603399994,15.2,5.95932117299999));
#206098=CARTESIAN_POINT('Ctrl Pts',(8.68206603399994,11.6,5.95932117299999));
#206099=CARTESIAN_POINT('Ctrl Pts',(8.68336123199994,15.2,5.96063934899998));
#206100=CARTESIAN_POINT('Ctrl Pts',(8.68336123199994,11.6,5.96063934899998));
#206101=CARTESIAN_POINT('Ctrl Pts',(8.68466036399994,15.2,5.96196395499998));
#206102=CARTESIAN_POINT('Ctrl Pts',(8.68466036399994,11.6,5.96196395499998));
#206103=CARTESIAN_POINT('Ctrl Pts',(8.68596340899994,15.2,5.96329498599999));
#206104=CARTESIAN_POINT('Ctrl Pts',(8.68596340899994,11.6,5.96329498599999));
#206105=CARTESIAN_POINT('Ctrl Pts',(8.68727034799995,15.2,5.96463243999998));
#206106=CARTESIAN_POINT('Ctrl Pts',(8.68727034799995,11.6,5.96463243999998));
#206107=CARTESIAN_POINT('Ctrl Pts',(8.68858115999994,15.2,5.96597631299999));
#206108=CARTESIAN_POINT('Ctrl Pts',(8.68858115999994,11.6,5.96597631299999));
#206109=CARTESIAN_POINT('Ctrl Pts',(8.68989582599994,15.2,5.96732660299998));
#206110=CARTESIAN_POINT('Ctrl Pts',(8.68989582599994,11.6,5.96732660299998));
#206111=CARTESIAN_POINT('Ctrl Pts',(8.69121432399995,15.2,5.96868330599998));
#206112=CARTESIAN_POINT('Ctrl Pts',(8.69121432399995,11.6,5.96868330599998));
#206113=CARTESIAN_POINT('Ctrl Pts',(8.69253663599994,15.2,5.97004641899999));
#206114=CARTESIAN_POINT('Ctrl Pts',(8.69253663599994,11.6,5.97004641899999));
#206115=CARTESIAN_POINT('Ctrl Pts',(8.69386274199995,15.2,5.97141593799999));
#206116=CARTESIAN_POINT('Ctrl Pts',(8.69386274199995,11.6,5.97141593799999));
#206117=CARTESIAN_POINT('Ctrl Pts',(8.69519262199994,15.2,5.97279186099998));
#206118=CARTESIAN_POINT('Ctrl Pts',(8.69519262199994,11.6,5.97279186099998));
#206119=CARTESIAN_POINT('Ctrl Pts',(8.69652625699995,15.2,5.97417418499998));
#206120=CARTESIAN_POINT('Ctrl Pts',(8.69652625699995,11.6,5.97417418499998));
#206121=CARTESIAN_POINT('Ctrl Pts',(8.69786362599994,15.2,5.97556290499998));
#206122=CARTESIAN_POINT('Ctrl Pts',(8.69786362599994,11.6,5.97556290499998));
#206123=CARTESIAN_POINT('Ctrl Pts',(8.69920470899994,15.2,5.97695802099998));
#206124=CARTESIAN_POINT('Ctrl Pts',(8.69920470899994,11.6,5.97695802099998));
#206125=CARTESIAN_POINT('Ctrl Pts',(8.70054948899995,15.2,5.97835952599999));
#206126=CARTESIAN_POINT('Ctrl Pts',(8.70054948899995,11.6,5.97835952599999));
#206127=CARTESIAN_POINT('Ctrl Pts',(8.70189794499994,15.2,5.97976741899998));
#206128=CARTESIAN_POINT('Ctrl Pts',(8.70189794499994,11.6,5.97976741899998));
#206129=CARTESIAN_POINT('Ctrl Pts',(8.70325005799994,15.2,5.98118169699998));
#206130=CARTESIAN_POINT('Ctrl Pts',(8.70325005799994,11.6,5.98118169699998));
#206131=CARTESIAN_POINT('Ctrl Pts',(8.70460580899995,15.2,5.98260235599999));
#206132=CARTESIAN_POINT('Ctrl Pts',(8.70460580899995,11.6,5.98260235599999));
#206133=CARTESIAN_POINT('Ctrl Pts',(8.70596517899994,15.2,5.98402939299999));
#206134=CARTESIAN_POINT('Ctrl Pts',(8.70596517899994,11.6,5.98402939299999));
#206135=CARTESIAN_POINT('Ctrl Pts',(8.70732814799995,15.2,5.98546280499999));
#206136=CARTESIAN_POINT('Ctrl Pts',(8.70732814799995,11.6,5.98546280499999));
#206137=CARTESIAN_POINT('Ctrl Pts',(8.70869469799995,15.2,5.98690258799999));
#206138=CARTESIAN_POINT('Ctrl Pts',(8.70869469799995,11.6,5.98690258799999));
#206139=CARTESIAN_POINT('Ctrl Pts',(8.71006480999995,15.2,5.98834873999999));
#206140=CARTESIAN_POINT('Ctrl Pts',(8.71006480999995,11.6,5.98834873999999));
#206141=CARTESIAN_POINT('Ctrl Pts',(8.71143846399994,15.2,5.98980125699998));
#206142=CARTESIAN_POINT('Ctrl Pts',(8.71143846399994,11.6,5.98980125699998));
#206143=CARTESIAN_POINT('Ctrl Pts',(8.71281564199995,15.2,5.99126013699999));
#206144=CARTESIAN_POINT('Ctrl Pts',(8.71281564199995,11.6,5.99126013699999));
#206145=CARTESIAN_POINT('Ctrl Pts',(8.71419632499994,15.2,5.99272537499999));
#206146=CARTESIAN_POINT('Ctrl Pts',(8.71419632499994,11.6,5.99272537499999));
#206147=CARTESIAN_POINT('Ctrl Pts',(8.71558049399994,15.2,5.99419696999998));
#206148=CARTESIAN_POINT('Ctrl Pts',(8.71558049399994,11.6,5.99419696999998));
#206149=CARTESIAN_POINT('Ctrl Pts',(8.71696813099994,15.2,5.99567491599998));
#206150=CARTESIAN_POINT('Ctrl Pts',(8.71696813099994,11.6,5.99567491599998));
#206151=CARTESIAN_POINT('Ctrl Pts',(8.71835921699994,15.2,5.99715921099998));
#206152=CARTESIAN_POINT('Ctrl Pts',(8.71835921699994,11.6,5.99715921099998));
#206153=CARTESIAN_POINT('Ctrl Pts',(8.71975373299994,15.2,5.99864985399999));
#206154=CARTESIAN_POINT('Ctrl Pts',(8.71975373299994,11.6,5.99864985399999));
#206155=CARTESIAN_POINT('Ctrl Pts',(8.72115166199994,15.2,6.00014683799999));
#206156=CARTESIAN_POINT('Ctrl Pts',(8.72115166199994,11.6,6.00014683799999));
#206157=CARTESIAN_POINT('Ctrl Pts',(8.72255298499995,15.2,6.00165016199998));
#206158=CARTESIAN_POINT('Ctrl Pts',(8.72255298499995,11.6,6.00165016199998));
#206159=CARTESIAN_POINT('Ctrl Pts',(8.72395768199994,15.2,6.00315982299998));
#206160=CARTESIAN_POINT('Ctrl Pts',(8.72395768199994,11.6,6.00315982299998));
#206161=CARTESIAN_POINT('Ctrl Pts',(8.72536573799995,15.2,6.00467581699998));
#206162=CARTESIAN_POINT('Ctrl Pts',(8.72536573799995,11.6,6.00467581699998));
#206163=CARTESIAN_POINT('Ctrl Pts',(8.72677713199994,15.2,6.00619814099999));
#206164=CARTESIAN_POINT('Ctrl Pts',(8.72677713199994,11.6,6.00619814099999));
#206165=CARTESIAN_POINT('Ctrl Pts',(8.72819184599994,15.2,6.00772679099999));
#206166=CARTESIAN_POINT('Ctrl Pts',(8.72819184599994,11.6,6.00772679099999));
#206167=CARTESIAN_POINT('Ctrl Pts',(8.72960986399994,15.2,6.00926176599998));
#206168=CARTESIAN_POINT('Ctrl Pts',(8.72960986399994,11.6,6.00926176599998));
#206169=CARTESIAN_POINT('Ctrl Pts',(8.73103116499994,15.2,6.01080305999999));
#206170=CARTESIAN_POINT('Ctrl Pts',(8.73103116499994,11.6,6.01080305999999));
#206171=CARTESIAN_POINT('Ctrl Pts',(8.73245573399995,15.2,6.01235067199998));
#206172=CARTESIAN_POINT('Ctrl Pts',(8.73245573399995,11.6,6.01235067199998));
#206173=CARTESIAN_POINT('Ctrl Pts',(8.73388355099994,15.2,6.01390459899999));
#206174=CARTESIAN_POINT('Ctrl Pts',(8.73388355099994,11.6,6.01390459899999));
#206175=CARTESIAN_POINT('Ctrl Pts',(8.73531459999995,15.2,6.01546483499998));
#206176=CARTESIAN_POINT('Ctrl Pts',(8.73531459999995,11.6,6.01546483499998));
#206177=CARTESIAN_POINT('Ctrl Pts',(8.73674886199994,15.2,6.01703137999999));
#206178=CARTESIAN_POINT('Ctrl Pts',(8.73674886199994,11.6,6.01703137999999));
#206179=CARTESIAN_POINT('Ctrl Pts',(8.73818631899994,15.2,6.01860422699998));
#206180=CARTESIAN_POINT('Ctrl Pts',(8.73818631899994,11.6,6.01860422699998));
#206181=CARTESIAN_POINT('Ctrl Pts',(8.73962695399995,15.2,6.02018337699998));
#206182=CARTESIAN_POINT('Ctrl Pts',(8.73962695399995,11.6,6.02018337699998));
#206183=CARTESIAN_POINT('Ctrl Pts',(8.74107074799995,15.2,6.02176882399998));
#206184=CARTESIAN_POINT('Ctrl Pts',(8.74107074799995,11.6,6.02176882399998));
#206185=CARTESIAN_POINT('Ctrl Pts',(8.74251768599994,15.2,6.02336056599999));
#206186=CARTESIAN_POINT('Ctrl Pts',(8.74251768599994,11.6,6.02336056599999));
#206187=CARTESIAN_POINT('Ctrl Pts',(8.74396774799994,15.2,6.02495859899999));
#206188=CARTESIAN_POINT('Ctrl Pts',(8.74396774799994,11.6,6.02495859899999));
#206189=CARTESIAN_POINT('Ctrl Pts',(8.74542091899994,15.2,6.02656292099999));
#206190=CARTESIAN_POINT('Ctrl Pts',(8.74542091899994,11.6,6.02656292099999));
#206191=CARTESIAN_POINT('Ctrl Pts',(8.74687717899995,15.2,6.02817352699999));
#206192=CARTESIAN_POINT('Ctrl Pts',(8.74687717899995,11.6,6.02817352699999));
#206193=CARTESIAN_POINT('Ctrl Pts',(8.74833651199994,15.2,6.02979041499999));
#206194=CARTESIAN_POINT('Ctrl Pts',(8.74833651199994,11.6,6.02979041499999));
#206195=CARTESIAN_POINT('Ctrl Pts',(8.74979890299995,15.2,6.03141358199998));
#206196=CARTESIAN_POINT('Ctrl Pts',(8.74979890299995,11.6,6.03141358199998));
#206197=CARTESIAN_POINT('Ctrl Pts',(8.75126432999994,15.2,6.03304302299998));
#206198=CARTESIAN_POINT('Ctrl Pts',(8.75126432999994,11.6,6.03304302299998));
#206199=CARTESIAN_POINT('Ctrl Pts',(8.75273277899994,15.2,6.03467873699999));
#206200=CARTESIAN_POINT('Ctrl Pts',(8.75273277899994,11.6,6.03467873699999));
#206201=CARTESIAN_POINT('Ctrl Pts',(8.75420423299994,15.2,6.03632071999999));
#206202=CARTESIAN_POINT('Ctrl Pts',(8.75420423299994,11.6,6.03632071999999));
#206203=CARTESIAN_POINT('Ctrl Pts',(8.75567867299995,15.2,6.03796896799999));
#206204=CARTESIAN_POINT('Ctrl Pts',(8.75567867299995,11.6,6.03796896799999));
#206205=CARTESIAN_POINT('Ctrl Pts',(8.75715608399994,15.2,6.03962347899999));
#206206=CARTESIAN_POINT('Ctrl Pts',(8.75715608399994,11.6,6.03962347899999));
#206207=CARTESIAN_POINT('Ctrl Pts',(8.75863644699994,15.2,6.04128424799999));
#206208=CARTESIAN_POINT('Ctrl Pts',(8.75863644699994,11.6,6.04128424799999));
#206209=CARTESIAN_POINT('Ctrl Pts',(8.76011974799994,15.2,6.04295127299999));
#206210=CARTESIAN_POINT('Ctrl Pts',(8.76011974799994,11.6,6.04295127299999));
#206211=CARTESIAN_POINT('Ctrl Pts',(8.76160596799994,15.2,6.04462455099998));
#206212=CARTESIAN_POINT('Ctrl Pts',(8.76160596799994,11.6,6.04462455099998));
#206213=CARTESIAN_POINT('Ctrl Pts',(8.76309508999995,15.2,6.04630407799998));
#206214=CARTESIAN_POINT('Ctrl Pts',(8.76309508999995,11.6,6.04630407799998));
#206215=CARTESIAN_POINT('Ctrl Pts',(8.76458709899994,15.2,6.04798985099999));
#206216=CARTESIAN_POINT('Ctrl Pts',(8.76458709899994,11.6,6.04798985099999));
#206217=CARTESIAN_POINT('Ctrl Pts',(8.76608197799994,15.2,6.04968186699999));
#206218=CARTESIAN_POINT('Ctrl Pts',(8.76608197799994,11.6,6.04968186699999));
#206219=CARTESIAN_POINT('Ctrl Pts',(8.76757970799994,15.2,6.05138012299999));
#206220=CARTESIAN_POINT('Ctrl Pts',(8.76757970799994,11.6,6.05138012299999));
#206221=CARTESIAN_POINT('Ctrl Pts',(8.76908027599994,15.2,6.05308461599999));
#206222=CARTESIAN_POINT('Ctrl Pts',(8.76908027599994,11.6,6.05308461599999));
#206223=CARTESIAN_POINT('Ctrl Pts',(8.77058366299994,15.2,6.05479533999999));
#206224=CARTESIAN_POINT('Ctrl Pts',(8.77058366299994,11.6,6.05479533999999));
#206225=CARTESIAN_POINT('Ctrl Pts',(8.77208985199994,15.2,6.05651229599999));
#206226=CARTESIAN_POINT('Ctrl Pts',(8.77208985199994,11.6,6.05651229599999));
#206227=CARTESIAN_POINT('Ctrl Pts',(8.77359882999994,15.2,6.05823547699998));
#206228=CARTESIAN_POINT('Ctrl Pts',(8.77359882999994,11.6,6.05823547699998));
#206229=CARTESIAN_POINT('Ctrl Pts',(8.77511057699994,15.2,6.05996488199998));
#206230=CARTESIAN_POINT('Ctrl Pts',(8.77511057699994,11.6,6.05996488199998));
#206231=CARTESIAN_POINT('Ctrl Pts',(8.77662507799995,15.2,6.06170050699999));
#206232=CARTESIAN_POINT('Ctrl Pts',(8.77662507799995,11.6,6.06170050699999));
#206233=CARTESIAN_POINT('Ctrl Pts',(8.77814231699995,15.2,6.06344234899999));
#206234=CARTESIAN_POINT('Ctrl Pts',(8.77814231699995,11.6,6.06344234899999));
#206235=CARTESIAN_POINT('Ctrl Pts',(8.77966227899995,15.2,6.06519040399998));
#206236=CARTESIAN_POINT('Ctrl Pts',(8.77966227899995,11.6,6.06519040399998));
#206237=CARTESIAN_POINT('Ctrl Pts',(8.78118494499994,15.2,6.06694466999999));
#206238=CARTESIAN_POINT('Ctrl Pts',(8.78118494499994,11.6,6.06694466999999));
#206239=CARTESIAN_POINT('Ctrl Pts',(8.78271030099994,15.2,6.06870514299998));
#206240=CARTESIAN_POINT('Ctrl Pts',(8.78271030099994,11.6,6.06870514299998));
#206241=CARTESIAN_POINT('Ctrl Pts',(8.78423832999994,15.2,6.07047181899999));
#206242=CARTESIAN_POINT('Ctrl Pts',(8.78423832999994,11.6,6.07047181899999));
#206243=CARTESIAN_POINT('Ctrl Pts',(8.78576901699994,15.2,6.07224469699998));
#206244=CARTESIAN_POINT('Ctrl Pts',(8.78576901699994,11.6,6.07224469699998));
#206245=CARTESIAN_POINT('Ctrl Pts',(8.78730234599994,15.2,6.07402377099999));
#206246=CARTESIAN_POINT('Ctrl Pts',(8.78730234599994,11.6,6.07402377099999));
#206247=CARTESIAN_POINT('Ctrl Pts',(8.78883829999995,15.2,6.07580903899999));
#206248=CARTESIAN_POINT('Ctrl Pts',(8.78883829999995,11.6,6.07580903899999));
#206249=CARTESIAN_POINT('Ctrl Pts',(8.79037686299995,15.2,6.07760049799998));
#206250=CARTESIAN_POINT('Ctrl Pts',(8.79037686299995,11.6,6.07760049799998));
#206251=CARTESIAN_POINT('Ctrl Pts',(8.79191802099994,15.2,6.07939814499999));
#206252=CARTESIAN_POINT('Ctrl Pts',(8.79191802099994,11.6,6.07939814499999));
#206253=CARTESIAN_POINT('Ctrl Pts',(8.79346175599995,15.2,6.08120197499999));
#206254=CARTESIAN_POINT('Ctrl Pts',(8.79346175599995,11.6,6.08120197499999));
#206255=CARTESIAN_POINT('Ctrl Pts',(8.79500805399994,15.2,6.08301198699999));
#206256=CARTESIAN_POINT('Ctrl Pts',(8.79500805399994,11.6,6.08301198699999));
#206257=CARTESIAN_POINT('Ctrl Pts',(8.79655689899994,15.2,6.08482817699999));
#206258=CARTESIAN_POINT('Ctrl Pts',(8.79655689899994,11.6,6.08482817699999));
#206259=CARTESIAN_POINT('Ctrl Pts',(8.79810827499995,15.2,6.08665054099998));
#206260=CARTESIAN_POINT('Ctrl Pts',(8.79810827499995,11.6,6.08665054099998));
#206261=CARTESIAN_POINT('Ctrl Pts',(8.79966216599994,15.2,6.08847907499998));
#206262=CARTESIAN_POINT('Ctrl Pts',(8.79966216599994,11.6,6.08847907499998));
#206263=CARTESIAN_POINT('Ctrl Pts',(8.80121855799995,15.2,6.09031377899999));
#206264=CARTESIAN_POINT('Ctrl Pts',(8.80121855799995,11.6,6.09031377899999));
#206265=CARTESIAN_POINT('Ctrl Pts',(8.80277743299994,15.2,6.09215464499999));
#206266=CARTESIAN_POINT('Ctrl Pts',(8.80277743299994,11.6,6.09215464499999));
#206267=CARTESIAN_POINT('Ctrl Pts',(8.80433877799994,15.2,6.09400167399999));
#206268=CARTESIAN_POINT('Ctrl Pts',(8.80433877799994,11.6,6.09400167399999));
#206269=CARTESIAN_POINT('Ctrl Pts',(8.80590257699994,15.2,6.09585486099999));
#206270=CARTESIAN_POINT('Ctrl Pts',(8.80590257699994,11.6,6.09585486099999));
#206271=CARTESIAN_POINT('Ctrl Pts',(8.80746881299994,15.2,6.09771420199999));
#206272=CARTESIAN_POINT('Ctrl Pts',(8.80746881299994,11.6,6.09771420199999));
#206273=CARTESIAN_POINT('Ctrl Pts',(8.80903747399995,15.2,6.09957969499998));
#206274=CARTESIAN_POINT('Ctrl Pts',(8.80903747399995,11.6,6.09957969499998));
#206275=CARTESIAN_POINT('Ctrl Pts',(8.81060854099994,15.2,6.10145133499999));
#206276=CARTESIAN_POINT('Ctrl Pts',(8.81060854099994,11.6,6.10145133499999));
#206277=CARTESIAN_POINT('Ctrl Pts',(8.81218200199994,15.2,6.10332912099998));
#206278=CARTESIAN_POINT('Ctrl Pts',(8.81218200199994,11.6,6.10332912099998));
#206279=CARTESIAN_POINT('Ctrl Pts',(8.81375783899994,15.2,6.10521304799998));
#206280=CARTESIAN_POINT('Ctrl Pts',(8.81375783899994,11.6,6.10521304799998));
#206281=CARTESIAN_POINT('Ctrl Pts',(8.81533603999994,15.2,6.10710311399998));
#206282=CARTESIAN_POINT('Ctrl Pts',(8.81533603999994,11.6,6.10710311399998));
#206283=CARTESIAN_POINT('Ctrl Pts',(8.81691658799994,15.2,6.10899931499999));
#206284=CARTESIAN_POINT('Ctrl Pts',(8.81691658799994,11.6,6.10899931499999));
#206285=CARTESIAN_POINT('Ctrl Pts',(8.81849946799995,15.2,6.11090164599998));
#206286=CARTESIAN_POINT('Ctrl Pts',(8.81849946799995,11.6,6.11090164599998));
#206287=CARTESIAN_POINT('Ctrl Pts',(8.82008466499994,15.2,6.11281010699999));
#206288=CARTESIAN_POINT('Ctrl Pts',(8.82008466499994,11.6,6.11281010699999));
#206289=CARTESIAN_POINT('Ctrl Pts',(8.82167216399995,15.2,6.11472469299999));
#206290=CARTESIAN_POINT('Ctrl Pts',(8.82167216399995,11.6,6.11472469299999));
#206291=CARTESIAN_POINT('Ctrl Pts',(8.82326195199994,15.2,6.11664540099999));
#206292=CARTESIAN_POINT('Ctrl Pts',(8.82326195199994,11.6,6.11664540099999));
#206293=CARTESIAN_POINT('Ctrl Pts',(8.82485401099995,15.2,6.11857222699999));
#206294=CARTESIAN_POINT('Ctrl Pts',(8.82485401099995,11.6,6.11857222699999));
#206295=CARTESIAN_POINT('Ctrl Pts',(8.82644832899994,15.2,6.12050516799999));
#206296=CARTESIAN_POINT('Ctrl Pts',(8.82644832899994,11.6,6.12050516799999));
#206297=CARTESIAN_POINT('Ctrl Pts',(8.82804488899994,15.2,6.12244422099998));
#206298=CARTESIAN_POINT('Ctrl Pts',(8.82804488899994,11.6,6.12244422099998));
#206299=CARTESIAN_POINT('Ctrl Pts',(8.82964367799994,15.2,6.12438938399999));
#206300=CARTESIAN_POINT('Ctrl Pts',(8.82964367799994,11.6,6.12438938399999));
#206301=CARTESIAN_POINT('Ctrl Pts',(8.83124467999994,15.2,6.12634065099999));
#206302=CARTESIAN_POINT('Ctrl Pts',(8.83124467999994,11.6,6.12634065099999));
#206303=CARTESIAN_POINT('Ctrl Pts',(8.83284788199994,15.2,6.12829801999998));
#206304=CARTESIAN_POINT('Ctrl Pts',(8.83284788199994,11.6,6.12829801999998));
#206305=CARTESIAN_POINT('Ctrl Pts',(8.83445326699994,15.2,6.13026148799998));
#206306=CARTESIAN_POINT('Ctrl Pts',(8.83445326699994,11.6,6.13026148799998));
#206307=CARTESIAN_POINT('Ctrl Pts',(8.83606082299995,15.2,6.13223105099999));
#206308=CARTESIAN_POINT('Ctrl Pts',(8.83606082299995,11.6,6.13223105099999));
#206309=CARTESIAN_POINT('Ctrl Pts',(8.83767053399995,15.2,6.13420670699998));
#206310=CARTESIAN_POINT('Ctrl Pts',(8.83767053399995,11.6,6.13420670699998));
#206311=CARTESIAN_POINT('Ctrl Pts',(8.83928238599994,15.2,6.13618845099998));
#206312=CARTESIAN_POINT('Ctrl Pts',(8.83928238599994,11.6,6.13618845099998));
#206313=CARTESIAN_POINT('Ctrl Pts',(8.84089636399995,15.2,6.13817628099999));
#206314=CARTESIAN_POINT('Ctrl Pts',(8.84089636399995,11.6,6.13817628099999));
#206315=CARTESIAN_POINT('Ctrl Pts',(8.84251245399994,15.2,6.14017019299999));
#206316=CARTESIAN_POINT('Ctrl Pts',(8.84251245399994,11.6,6.14017019299999));
#206317=CARTESIAN_POINT('Ctrl Pts',(8.84413064299994,15.2,6.14217018399999));
#206318=CARTESIAN_POINT('Ctrl Pts',(8.84413064299994,11.6,6.14217018399999));
#206319=CARTESIAN_POINT('Ctrl Pts',(8.84575091399994,15.2,6.14417624999999));
#206320=CARTESIAN_POINT('Ctrl Pts',(8.84575091399994,11.6,6.14417624999999));
#206321=CARTESIAN_POINT('Ctrl Pts',(8.84737325499995,15.2,6.14618838899998));
#206322=CARTESIAN_POINT('Ctrl Pts',(8.84737325499995,11.6,6.14618838899998));
#206323=CARTESIAN_POINT('Ctrl Pts',(8.84899765099994,15.2,6.14820659599999));
#206324=CARTESIAN_POINT('Ctrl Pts',(8.84899765099994,11.6,6.14820659599999));
#206325=CARTESIAN_POINT('Ctrl Pts',(8.85062408799994,15.2,6.15023086999999));
#206326=CARTESIAN_POINT('Ctrl Pts',(8.85062408799994,11.6,6.15023086999999));
#206327=CARTESIAN_POINT('Ctrl Pts',(8.85225254999994,15.2,6.15226120499998));
#206328=CARTESIAN_POINT('Ctrl Pts',(8.85225254999994,11.6,6.15226120499998));
#206329=CARTESIAN_POINT('Ctrl Pts',(8.85388302599995,15.2,6.15429759899998));
#206330=CARTESIAN_POINT('Ctrl Pts',(8.85388302599995,11.6,6.15429759899998));
#206331=CARTESIAN_POINT('Ctrl Pts',(8.85551549999994,15.2,6.15634004899999));
#206332=CARTESIAN_POINT('Ctrl Pts',(8.85551549999994,11.6,6.15634004899999));
#206333=CARTESIAN_POINT('Ctrl Pts',(8.85714995899994,15.2,6.15838855199998));
#206334=CARTESIAN_POINT('Ctrl Pts',(8.85714995899994,11.6,6.15838855199998));
#206335=CARTESIAN_POINT('Ctrl Pts',(8.85878638799995,15.2,6.16044310299999));
#206336=CARTESIAN_POINT('Ctrl Pts',(8.85878638799995,11.6,6.16044310299999));
#206337=CARTESIAN_POINT('Ctrl Pts',(8.86042477299995,15.2,6.16250369999998));
#206338=CARTESIAN_POINT('Ctrl Pts',(8.86042477299995,11.6,6.16250369999998));
#206339=CARTESIAN_POINT('Ctrl Pts',(8.86206510099995,15.2,6.16457033999998));
#206340=CARTESIAN_POINT('Ctrl Pts',(8.86206510099995,11.6,6.16457033999998));
#206341=CARTESIAN_POINT('Ctrl Pts',(8.86370735799994,15.2,6.16664301699998));
#206342=CARTESIAN_POINT('Ctrl Pts',(8.86370735799994,11.6,6.16664301699998));
#206343=CARTESIAN_POINT('Ctrl Pts',(8.86535153099994,15.2,6.16872173199998));
#206344=CARTESIAN_POINT('Ctrl Pts',(8.86535153099994,11.6,6.16872173199998));
#206345=CARTESIAN_POINT('Ctrl Pts',(8.86699760299994,15.2,6.17080647799998));
#206346=CARTESIAN_POINT('Ctrl Pts',(8.86699760299994,11.6,6.17080647799998));
#206347=CARTESIAN_POINT('Ctrl Pts',(8.86864556399994,15.2,6.17289725399999));
#206348=CARTESIAN_POINT('Ctrl Pts',(8.86864556399994,11.6,6.17289725399999));
#206349=CARTESIAN_POINT('Ctrl Pts',(8.87029539799994,15.2,6.17499405499998));
#206350=CARTESIAN_POINT('Ctrl Pts',(8.87029539799994,11.6,6.17499405499998));
#206351=CARTESIAN_POINT('Ctrl Pts',(8.87194709099994,15.2,6.17709687799999));
#206352=CARTESIAN_POINT('Ctrl Pts',(8.87194709099994,11.6,6.17709687799999));
#206353=CARTESIAN_POINT('Ctrl Pts',(8.87360063099995,15.2,6.17920572099998));
#206354=CARTESIAN_POINT('Ctrl Pts',(8.87360063099995,11.6,6.17920572099998));
#206355=CARTESIAN_POINT('Ctrl Pts',(8.87525600399995,15.2,6.18132057799999));
#206356=CARTESIAN_POINT('Ctrl Pts',(8.87525600399995,11.6,6.18132057799999));
#206357=CARTESIAN_POINT('Ctrl Pts',(8.87691319699995,15.2,6.18344144999998));
#206358=CARTESIAN_POINT('Ctrl Pts',(8.87691319699995,11.6,6.18344144999998));
#206359=CARTESIAN_POINT('Ctrl Pts',(8.87857219499995,15.2,6.18556832899999));
#206360=CARTESIAN_POINT('Ctrl Pts',(8.87857219499995,11.6,6.18556832899999));
#206361=CARTESIAN_POINT('Ctrl Pts',(8.88023298399995,15.2,6.18770121299999));
#206362=CARTESIAN_POINT('Ctrl Pts',(8.88023298399995,11.6,6.18770121299999));
#206363=CARTESIAN_POINT('Ctrl Pts',(8.88189555299994,15.2,6.18984010099998));
#206364=CARTESIAN_POINT('Ctrl Pts',(8.88189555299994,11.6,6.18984010099998));
#206365=CARTESIAN_POINT('Ctrl Pts',(8.88355988699994,15.2,6.19198498699999));
#206366=CARTESIAN_POINT('Ctrl Pts',(8.88355988699994,11.6,6.19198498699999));
#206367=CARTESIAN_POINT('Ctrl Pts',(8.88522597299995,15.2,6.19413586899999));
#206368=CARTESIAN_POINT('Ctrl Pts',(8.88522597299995,11.6,6.19413586899999));
#206369=CARTESIAN_POINT('Ctrl Pts',(8.88689379699995,15.2,6.19629274299999));
#206370=CARTESIAN_POINT('Ctrl Pts',(8.88689379699995,11.6,6.19629274299999));
#206371=CARTESIAN_POINT('Ctrl Pts',(8.88856334799994,15.2,6.19845560599998));
#206372=CARTESIAN_POINT('Ctrl Pts',(8.88856334799994,11.6,6.19845560599998));
#206373=CARTESIAN_POINT('Ctrl Pts',(8.89023460899995,15.2,6.20062445499999));
#206374=CARTESIAN_POINT('Ctrl Pts',(8.89023460899995,11.6,6.20062445499999));
#206375=CARTESIAN_POINT('Ctrl Pts',(8.89190756899995,15.2,6.20279928499999));
#206376=CARTESIAN_POINT('Ctrl Pts',(8.89190756899995,11.6,6.20279928499999));
#206377=CARTESIAN_POINT('Ctrl Pts',(8.89358221599995,15.2,6.20498009499999));
#206378=CARTESIAN_POINT('Ctrl Pts',(8.89358221599995,11.6,6.20498009499999));
#206379=CARTESIAN_POINT('Ctrl Pts',(8.89525853299994,15.2,6.20716688099999));
#206380=CARTESIAN_POINT('Ctrl Pts',(8.89525853299994,11.6,6.20716688099999));
#206381=CARTESIAN_POINT('Ctrl Pts',(8.89693651199994,15.2,6.20935963799998));
#206382=CARTESIAN_POINT('Ctrl Pts',(8.89693651199994,11.6,6.20935963799998));
#206383=CARTESIAN_POINT('Ctrl Pts',(8.89861613499994,15.2,6.21155836399998));
#206384=CARTESIAN_POINT('Ctrl Pts',(8.89861613499994,11.6,6.21155836399998));
#206385=CARTESIAN_POINT('Ctrl Pts',(8.90029739199995,15.2,6.21376305599998));
#206386=CARTESIAN_POINT('Ctrl Pts',(8.90029739199995,11.6,6.21376305599998));
#206387=CARTESIAN_POINT('Ctrl Pts',(8.90198026899995,15.2,6.21597370999999));
#206388=CARTESIAN_POINT('Ctrl Pts',(8.90198026899995,11.6,6.21597370999999));
#206389=CARTESIAN_POINT('Ctrl Pts',(8.90366475299994,15.2,6.21819032099998));
#206390=CARTESIAN_POINT('Ctrl Pts',(8.90366475299994,11.6,6.21819032099998));
#206391=CARTESIAN_POINT('Ctrl Pts',(8.90535083099994,15.2,6.22041288899998));
#206392=CARTESIAN_POINT('Ctrl Pts',(8.90535083099994,11.6,6.22041288899998));
#206393=CARTESIAN_POINT('Ctrl Pts',(8.90703848999994,15.2,6.22264140899999));
#206394=CARTESIAN_POINT('Ctrl Pts',(8.90703848999994,11.6,6.22264140899999));
#206395=CARTESIAN_POINT('Ctrl Pts',(8.90872771799994,15.2,6.22487587699998));
#206396=CARTESIAN_POINT('Ctrl Pts',(8.90872771799994,11.6,6.22487587699998));
#206397=CARTESIAN_POINT('Ctrl Pts',(8.91041850099995,15.2,6.22711629099998));
#206398=CARTESIAN_POINT('Ctrl Pts',(8.91041850099995,11.6,6.22711629099998));
#206399=CARTESIAN_POINT('Ctrl Pts',(8.91211082699994,15.2,6.22936264599999));
#206400=CARTESIAN_POINT('Ctrl Pts',(8.91211082699994,11.6,6.22936264599999));
#206401=CARTESIAN_POINT('Ctrl Pts',(8.91380468299995,15.2,6.23161493999999));
#206402=CARTESIAN_POINT('Ctrl Pts',(8.91380468299995,11.6,6.23161493999999));
#206403=CARTESIAN_POINT('Ctrl Pts',(8.91550005599994,15.2,6.23387316899999));
#206404=CARTESIAN_POINT('Ctrl Pts',(8.91550005599994,11.6,6.23387316899999));
#206405=CARTESIAN_POINT('Ctrl Pts',(8.91719693299994,15.2,6.23613732899998));
#206406=CARTESIAN_POINT('Ctrl Pts',(8.91719693299994,11.6,6.23613732899998));
#206407=CARTESIAN_POINT('Ctrl Pts',(8.91889530199995,15.2,6.23840741899999));
#206408=CARTESIAN_POINT('Ctrl Pts',(8.91889530199995,11.6,6.23840741899999));
#206409=CARTESIAN_POINT('Ctrl Pts',(8.92059514999995,15.2,6.24068343399999));
#206410=CARTESIAN_POINT('Ctrl Pts',(8.92059514999995,11.6,6.24068343399999));
#206411=CARTESIAN_POINT('Ctrl Pts',(8.92229646399995,15.2,6.24296536899998));
#206412=CARTESIAN_POINT('Ctrl Pts',(8.92229646399995,11.6,6.24296536899998));
#206413=CARTESIAN_POINT('Ctrl Pts',(8.92399923199994,15.2,6.24525322299998));
#206414=CARTESIAN_POINT('Ctrl Pts',(8.92399923199994,11.6,6.24525322299998));
#206415=CARTESIAN_POINT('Ctrl Pts',(8.92570344199994,15.2,6.24754699299999));
#206416=CARTESIAN_POINT('Ctrl Pts',(8.92570344199994,11.6,6.24754699299999));
#206417=CARTESIAN_POINT('Ctrl Pts',(8.92740908099995,15.2,6.24984667299999));
#206418=CARTESIAN_POINT('Ctrl Pts',(8.92740908099995,11.6,6.24984667299999));
#206419=CARTESIAN_POINT('Ctrl Pts',(8.92911613499994,15.2,6.25215226099999));
#206420=CARTESIAN_POINT('Ctrl Pts',(8.92911613499994,11.6,6.25215226099999));
#206421=CARTESIAN_POINT('Ctrl Pts',(8.93082459399994,15.2,6.25446375399999));
#206422=CARTESIAN_POINT('Ctrl Pts',(8.93082459399994,11.6,6.25446375399999));
#206423=CARTESIAN_POINT('Ctrl Pts',(8.93253444299994,15.2,6.25678114999998));
#206424=CARTESIAN_POINT('Ctrl Pts',(8.93253444299994,11.6,6.25678114999998));
#206425=CARTESIAN_POINT('Ctrl Pts',(8.93424567199995,15.2,6.25910444199998));
#206426=CARTESIAN_POINT('Ctrl Pts',(8.93424567199995,11.6,6.25910444199998));
#206427=CARTESIAN_POINT('Ctrl Pts',(8.93595826799995,15.2,6.26143362999999));
#206428=CARTESIAN_POINT('Ctrl Pts',(8.93595826799995,11.6,6.26143362999999));
#206429=CARTESIAN_POINT('Ctrl Pts',(8.93767221799994,15.2,6.26376870799999));
#206430=CARTESIAN_POINT('Ctrl Pts',(8.93767221799994,11.6,6.26376870799999));
#206431=CARTESIAN_POINT('Ctrl Pts',(8.93938750999994,15.2,6.26610967499998));
#206432=CARTESIAN_POINT('Ctrl Pts',(8.93938750999994,11.6,6.26610967499998));
#206433=CARTESIAN_POINT('Ctrl Pts',(8.94110413199994,15.2,6.26845652599999));
#206434=CARTESIAN_POINT('Ctrl Pts',(8.94110413199994,11.6,6.26845652599999));
#206435=CARTESIAN_POINT('Ctrl Pts',(8.94282207099995,15.2,6.27080925799999));
#206436=CARTESIAN_POINT('Ctrl Pts',(8.94282207099995,11.6,6.27080925799999));
#206437=CARTESIAN_POINT('Ctrl Pts',(8.94454131499994,15.2,6.27316786599999));
#206438=CARTESIAN_POINT('Ctrl Pts',(8.94454131499994,11.6,6.27316786599999));
#206439=CARTESIAN_POINT('Ctrl Pts',(8.94626185299994,15.2,6.27553235099998));
#206440=CARTESIAN_POINT('Ctrl Pts',(8.94626185299994,11.6,6.27553235099998));
#206441=CARTESIAN_POINT('Ctrl Pts',(8.94798367199994,15.2,6.27790270599998));
#206442=CARTESIAN_POINT('Ctrl Pts',(8.94798367199994,11.6,6.27790270599998));
#206443=CARTESIAN_POINT('Ctrl Pts',(8.94970675999994,15.2,6.28027892699999));
#206444=CARTESIAN_POINT('Ctrl Pts',(8.94970675999994,11.6,6.28027892699999));
#206445=CARTESIAN_POINT('Ctrl Pts',(8.95143110399994,15.2,6.28266101399999));
#206446=CARTESIAN_POINT('Ctrl Pts',(8.95143110399994,11.6,6.28266101399999));
#206447=CARTESIAN_POINT('Ctrl Pts',(8.95315669399994,15.2,6.28504895999999));
#206448=CARTESIAN_POINT('Ctrl Pts',(8.95315669399994,11.6,6.28504895999999));
#206449=CARTESIAN_POINT('Ctrl Pts',(8.95488351599995,15.2,6.28744276399999));
#206450=CARTESIAN_POINT('Ctrl Pts',(8.95488351599995,11.6,6.28744276399999));
#206451=CARTESIAN_POINT('Ctrl Pts',(8.95661155799995,15.2,6.28984242199999));
#206452=CARTESIAN_POINT('Ctrl Pts',(8.95661155799995,11.6,6.28984242199999));
#206453=CARTESIAN_POINT('Ctrl Pts',(8.95834080899995,15.2,6.29224792999998));
#206454=CARTESIAN_POINT('Ctrl Pts',(8.95834080899995,11.6,6.29224792999998));
#206455=CARTESIAN_POINT('Ctrl Pts',(8.96007125799994,15.2,6.29465928599998));
#206456=CARTESIAN_POINT('Ctrl Pts',(8.96007125799994,11.6,6.29465928599998));
#206457=CARTESIAN_POINT('Ctrl Pts',(8.96180289099994,15.2,6.29707648499998));
#206458=CARTESIAN_POINT('Ctrl Pts',(8.96180289099994,11.6,6.29707648499998));
#206459=CARTESIAN_POINT('Ctrl Pts',(8.96353569799994,15.2,6.29949952399999));
#206460=CARTESIAN_POINT('Ctrl Pts',(8.96353569799994,11.6,6.29949952399999));
#206461=CARTESIAN_POINT('Ctrl Pts',(8.96526966599994,15.2,6.30192839999999));
#206462=CARTESIAN_POINT('Ctrl Pts',(8.96526966599994,11.6,6.30192839999999));
#206463=CARTESIAN_POINT('Ctrl Pts',(8.96700478399995,15.2,6.30436310899999));
#206464=CARTESIAN_POINT('Ctrl Pts',(8.96700478399995,11.6,6.30436310899999));
#206465=CARTESIAN_POINT('Ctrl Pts',(8.96874103899994,15.2,6.30680364899998));
#206466=CARTESIAN_POINT('Ctrl Pts',(8.96874103899994,11.6,6.30680364899998));
#206467=CARTESIAN_POINT('Ctrl Pts',(8.97047841899994,15.2,6.30925001499998));
#206468=CARTESIAN_POINT('Ctrl Pts',(8.97047841899994,11.6,6.30925001499998));
#206469=CARTESIAN_POINT('Ctrl Pts',(8.97221691399994,15.2,6.31170220499998));
#206470=CARTESIAN_POINT('Ctrl Pts',(8.97221691399994,11.6,6.31170220499998));
#206471=CARTESIAN_POINT('Ctrl Pts',(8.97395651199994,15.2,6.31416021399998));
#206472=CARTESIAN_POINT('Ctrl Pts',(8.97395651199994,11.6,6.31416021399998));
#206473=CARTESIAN_POINT('Ctrl Pts',(8.97569719999994,15.2,6.31662403999999));
#206474=CARTESIAN_POINT('Ctrl Pts',(8.97569719999994,11.6,6.31662403999999));
#206475=CARTESIAN_POINT('Ctrl Pts',(8.97743896899994,15.2,6.31909367799998));
#206476=CARTESIAN_POINT('Ctrl Pts',(8.97743896899994,11.6,6.31909367799998));
#206477=CARTESIAN_POINT('Ctrl Pts',(8.97918180399994,15.2,6.32156912499998));
#206478=CARTESIAN_POINT('Ctrl Pts',(8.97918180399994,11.6,6.32156912499998));
#206479=CARTESIAN_POINT('Ctrl Pts',(8.98092569499994,15.2,6.32405037899999));
#206480=CARTESIAN_POINT('Ctrl Pts',(8.98092569499994,11.6,6.32405037899999));
#206481=CARTESIAN_POINT('Ctrl Pts',(8.98267063099994,15.2,6.32653743699999));
#206482=CARTESIAN_POINT('Ctrl Pts',(8.98267063099994,11.6,6.32653743699999));
#206483=CARTESIAN_POINT('Ctrl Pts',(8.98441659999994,15.2,6.32903029299998));
#206484=CARTESIAN_POINT('Ctrl Pts',(8.98441659999994,11.6,6.32903029299998));
#206485=CARTESIAN_POINT('Ctrl Pts',(8.98616358999995,15.2,6.33152894399998));
#206486=CARTESIAN_POINT('Ctrl Pts',(8.98616358999995,11.6,6.33152894399998));
#206487=CARTESIAN_POINT('Ctrl Pts',(8.98791159099994,15.2,6.33403338899999));
#206488=CARTESIAN_POINT('Ctrl Pts',(8.98791159099994,11.6,6.33403338899999));
#206489=CARTESIAN_POINT('Ctrl Pts',(8.98966059099994,15.2,6.33654362099998));
#206490=CARTESIAN_POINT('Ctrl Pts',(8.98966059099994,11.6,6.33654362099998));
#206491=CARTESIAN_POINT('Ctrl Pts',(8.99141057699994,15.2,6.33905963999998));
#206492=CARTESIAN_POINT('Ctrl Pts',(8.99141057699994,11.6,6.33905963999998));
#206493=CARTESIAN_POINT('Ctrl Pts',(8.99316153799995,15.2,6.34158143999999));
#206494=CARTESIAN_POINT('Ctrl Pts',(8.99316153799995,11.6,6.34158143999999));
#206495=CARTESIAN_POINT('Ctrl Pts',(8.99491346499994,15.2,6.34410901999999));
#206496=CARTESIAN_POINT('Ctrl Pts',(8.99491346499994,11.6,6.34410901999999));
#206497=CARTESIAN_POINT('Ctrl Pts',(8.99666634399994,15.2,6.34664237499998));
#206498=CARTESIAN_POINT('Ctrl Pts',(8.99666634399994,11.6,6.34664237499998));
#206499=CARTESIAN_POINT('Ctrl Pts',(8.99842016599995,15.2,6.34918150199999));
#206500=CARTESIAN_POINT('Ctrl Pts',(8.99842016599995,11.6,6.34918150199999));
#206501=CARTESIAN_POINT('Ctrl Pts',(9.00017491699994,15.2,6.35172639699999));
#206502=CARTESIAN_POINT('Ctrl Pts',(9.00017491699994,11.6,6.35172639699999));
#206503=CARTESIAN_POINT('Ctrl Pts',(9.00193058899994,15.2,6.35427705699998));
#206504=CARTESIAN_POINT('Ctrl Pts',(9.00193058899994,11.6,6.35427705699998));
#206505=CARTESIAN_POINT('Ctrl Pts',(9.00368716799994,15.2,6.35683347799999));
#206506=CARTESIAN_POINT('Ctrl Pts',(9.00368716799994,11.6,6.35683347799999));
#206507=CARTESIAN_POINT('Ctrl Pts',(9.00544464399994,15.2,6.35939565799998));
#206508=CARTESIAN_POINT('Ctrl Pts',(9.00544464399994,11.6,6.35939565799998));
#206509=CARTESIAN_POINT('Ctrl Pts',(9.00720300599994,15.2,6.36196359199998));
#206510=CARTESIAN_POINT('Ctrl Pts',(9.00720300599994,11.6,6.36196359199998));
#206511=CARTESIAN_POINT('Ctrl Pts',(9.00896224199995,15.2,6.36453727799999));
#206512=CARTESIAN_POINT('Ctrl Pts',(9.00896224199995,11.6,6.36453727799999));
#206513=CARTESIAN_POINT('Ctrl Pts',(9.01072234199994,15.2,6.36711671099999));
#206514=CARTESIAN_POINT('Ctrl Pts',(9.01072234199994,11.6,6.36711671099999));
#206515=CARTESIAN_POINT('Ctrl Pts',(9.01248329499994,15.2,6.36970188899999));
#206516=CARTESIAN_POINT('Ctrl Pts',(9.01248329499994,11.6,6.36970188899999));
#206517=CARTESIAN_POINT('Ctrl Pts',(9.01424508899994,15.2,6.37229280699999));
#206518=CARTESIAN_POINT('Ctrl Pts',(9.01424508899994,11.6,6.37229280699999));
#206519=CARTESIAN_POINT('Ctrl Pts',(9.01600771199995,15.2,6.37488946299998));
#206520=CARTESIAN_POINT('Ctrl Pts',(9.01600771199995,11.6,6.37488946299998));
#206521=CARTESIAN_POINT('Ctrl Pts',(9.01777115599995,15.2,6.37749185299998));
#206522=CARTESIAN_POINT('Ctrl Pts',(9.01777115599995,11.6,6.37749185299998));
#206523=CARTESIAN_POINT('Ctrl Pts',(9.01953540799994,15.2,6.38009997399998));
#206524=CARTESIAN_POINT('Ctrl Pts',(9.01953540799994,11.6,6.38009997399998));
#206525=CARTESIAN_POINT('Ctrl Pts',(9.02130045699994,15.2,6.38271382099998));
#206526=CARTESIAN_POINT('Ctrl Pts',(9.02130045699994,11.6,6.38271382099998));
#206527=CARTESIAN_POINT('Ctrl Pts',(9.02306629199994,15.2,6.38533339199999));
#206528=CARTESIAN_POINT('Ctrl Pts',(9.02306629199994,11.6,6.38533339199999));
#206529=CARTESIAN_POINT('Ctrl Pts',(9.02483290299994,15.2,6.38795868399999));
#206530=CARTESIAN_POINT('Ctrl Pts',(9.02483290299994,11.6,6.38795868399999));
#206531=CARTESIAN_POINT('Ctrl Pts',(9.02660027799995,15.2,6.39058969199999));
#206532=CARTESIAN_POINT('Ctrl Pts',(9.02660027799995,11.6,6.39058969199999));
#206533=CARTESIAN_POINT('Ctrl Pts',(9.02836840899995,15.2,6.39322641399998));
#206534=CARTESIAN_POINT('Ctrl Pts',(9.02836840899995,11.6,6.39322641399998));
#206535=CARTESIAN_POINT('Ctrl Pts',(9.03013728099994,15.2,6.39586884499998));
#206536=CARTESIAN_POINT('Ctrl Pts',(9.03013728099994,11.6,6.39586884499998));
#206537=CARTESIAN_POINT('Ctrl Pts',(9.03190688599994,15.2,6.39851698299999));
#206538=CARTESIAN_POINT('Ctrl Pts',(9.03190688599994,11.6,6.39851698299999));
#206539=CARTESIAN_POINT('Ctrl Pts',(9.03367721299994,15.2,6.40117082399998));
#206540=CARTESIAN_POINT('Ctrl Pts',(9.03367721299994,11.6,6.40117082399998));
#206541=CARTESIAN_POINT('Ctrl Pts',(9.03544824899994,15.2,6.40383036399999));
#206542=CARTESIAN_POINT('Ctrl Pts',(9.03544824899994,11.6,6.40383036399999));
#206543=CARTESIAN_POINT('Ctrl Pts',(9.03721998599995,15.2,6.40649559999999));
#206544=CARTESIAN_POINT('Ctrl Pts',(9.03721998599995,11.6,6.40649559999999));
#206545=CARTESIAN_POINT('Ctrl Pts',(9.03899241199994,15.2,6.40916652899998));
#206546=CARTESIAN_POINT('Ctrl Pts',(9.03899241199994,11.6,6.40916652899998));
#206547=CARTESIAN_POINT('Ctrl Pts',(9.04076551699994,15.2,6.41184314699998));
#206548=CARTESIAN_POINT('Ctrl Pts',(9.04076551699994,11.6,6.41184314699998));
#206549=CARTESIAN_POINT('Ctrl Pts',(9.04253928999994,15.2,6.41452544999999));
#206550=CARTESIAN_POINT('Ctrl Pts',(9.04253928999994,11.6,6.41452544999999));
#206551=CARTESIAN_POINT('Ctrl Pts',(9.04431372099994,15.2,6.41721343699999));
#206552=CARTESIAN_POINT('Ctrl Pts',(9.04431372099994,11.6,6.41721343699999));
#206553=CARTESIAN_POINT('Ctrl Pts',(9.04608879799994,15.2,6.41990710099999));
#206554=CARTESIAN_POINT('Ctrl Pts',(9.04608879799994,11.6,6.41990710099999));
#206555=CARTESIAN_POINT('Ctrl Pts',(9.04786451099995,15.2,6.42260643999998));
#206556=CARTESIAN_POINT('Ctrl Pts',(9.04786451099995,11.6,6.42260643999998));
#206557=CARTESIAN_POINT('Ctrl Pts',(9.04964084999994,15.2,6.42531145199998));
#206558=CARTESIAN_POINT('Ctrl Pts',(9.04964084999994,11.6,6.42531145199998));
#206559=CARTESIAN_POINT('Ctrl Pts',(9.05141780299994,15.2,6.42802213199998));
#206560=CARTESIAN_POINT('Ctrl Pts',(9.05141780299994,11.6,6.42802213199998));
#206561=CARTESIAN_POINT('Ctrl Pts',(9.05319536099995,15.2,6.43073847599998));
#206562=CARTESIAN_POINT('Ctrl Pts',(9.05319536099995,11.6,6.43073847599998));
#206563=CARTESIAN_POINT('Ctrl Pts',(9.05497351399994,15.2,6.43346048299998));
#206564=CARTESIAN_POINT('Ctrl Pts',(9.05497351399994,11.6,6.43346048299998));
#206565=CARTESIAN_POINT('Ctrl Pts',(9.05675225099994,15.2,6.43618814699998));
#206566=CARTESIAN_POINT('Ctrl Pts',(9.05675225099994,11.6,6.43618814699998));
#206567=CARTESIAN_POINT('Ctrl Pts',(9.05853155999995,15.2,6.43892146399998));
#206568=CARTESIAN_POINT('Ctrl Pts',(9.05853155999995,11.6,6.43892146399998));
#206569=CARTESIAN_POINT('Ctrl Pts',(9.06031143299994,15.2,6.44166043399999));
#206570=CARTESIAN_POINT('Ctrl Pts',(9.06031143299994,11.6,6.44166043399999));
#206571=CARTESIAN_POINT('Ctrl Pts',(9.06209185699994,15.2,6.44440504999999));
#206572=CARTESIAN_POINT('Ctrl Pts',(9.06209185699994,11.6,6.44440504999999));
#206573=CARTESIAN_POINT('Ctrl Pts',(9.06387282499994,15.2,6.44715531099998));
#206574=CARTESIAN_POINT('Ctrl Pts',(9.06387282499994,11.6,6.44715531099998));
#206575=CARTESIAN_POINT('Ctrl Pts',(9.06565432399994,15.2,6.44991121299999));
#206576=CARTESIAN_POINT('Ctrl Pts',(9.06565432399994,11.6,6.44991121299999));
#206577=CARTESIAN_POINT('Ctrl Pts',(9.06743634399995,15.2,6.45267275099998));
#206578=CARTESIAN_POINT('Ctrl Pts',(9.06743634399995,11.6,6.45267275099998));
#206579=CARTESIAN_POINT('Ctrl Pts',(9.06921887499994,15.2,6.45543992199999));
#206580=CARTESIAN_POINT('Ctrl Pts',(9.06921887499994,11.6,6.45543992199999));
#206581=CARTESIAN_POINT('Ctrl Pts',(9.07100190699994,15.2,6.45821272499998));
#206582=CARTESIAN_POINT('Ctrl Pts',(9.07100190699994,11.6,6.45821272499998));
#206583=CARTESIAN_POINT('Ctrl Pts',(9.07278542999994,15.2,6.46099115299998));
#206584=CARTESIAN_POINT('Ctrl Pts',(9.07278542999994,11.6,6.46099115299998));
#206585=CARTESIAN_POINT('Ctrl Pts',(9.07456943399995,15.2,6.46377520499998));
#206586=CARTESIAN_POINT('Ctrl Pts',(9.07456943399995,11.6,6.46377520499998));
#206587=CARTESIAN_POINT('Ctrl Pts',(9.07635390799994,15.2,6.46656487599999));
#206588=CARTESIAN_POINT('Ctrl Pts',(9.07635390799994,11.6,6.46656487599999));
#206589=CARTESIAN_POINT('Ctrl Pts',(9.07813884099994,15.2,6.46936016399999));
#206590=CARTESIAN_POINT('Ctrl Pts',(9.07813884099994,11.6,6.46936016399999));
#206591=CARTESIAN_POINT('Ctrl Pts',(9.07992422599994,15.2,6.47216106399998));
#206592=CARTESIAN_POINT('Ctrl Pts',(9.07992422599994,11.6,6.47216106399998));
#206593=CARTESIAN_POINT('Ctrl Pts',(9.08171004899994,15.2,6.47496757299999));
#206594=CARTESIAN_POINT('Ctrl Pts',(9.08171004899994,11.6,6.47496757299999));
#206595=CARTESIAN_POINT('Ctrl Pts',(9.08349630299995,15.2,6.47777968799998));
#206596=CARTESIAN_POINT('Ctrl Pts',(9.08349630299995,11.6,6.47777968799998));
#206597=CARTESIAN_POINT('Ctrl Pts',(9.08528297599995,15.2,6.48059740499999));
#206598=CARTESIAN_POINT('Ctrl Pts',(9.08528297599995,11.6,6.48059740499999));
#206599=CARTESIAN_POINT('Ctrl Pts',(9.08707005899995,15.2,6.48342072099998));
#206600=CARTESIAN_POINT('Ctrl Pts',(9.08707005899995,11.6,6.48342072099998));
#206601=CARTESIAN_POINT('Ctrl Pts',(9.08885754099994,15.2,6.48624963299999));
#206602=CARTESIAN_POINT('Ctrl Pts',(9.08885754099994,11.6,6.48624963299999));
#206603=CARTESIAN_POINT('Ctrl Pts',(9.09064541299994,15.2,6.48908413499999));
#206604=CARTESIAN_POINT('Ctrl Pts',(9.09064541299994,11.6,6.48908413499999));
#206605=CARTESIAN_POINT('Ctrl Pts',(9.09243366399994,15.2,6.49192422699999));
#206606=CARTESIAN_POINT('Ctrl Pts',(9.09243366399994,11.6,6.49192422699999));
#206607=CARTESIAN_POINT('Ctrl Pts',(9.09422228599994,15.2,6.49476990299998));
#206608=CARTESIAN_POINT('Ctrl Pts',(9.09422228599994,11.6,6.49476990299998));
#206609=CARTESIAN_POINT('Ctrl Pts',(9.09601126799994,15.2,6.49762115899998));
#206610=CARTESIAN_POINT('Ctrl Pts',(9.09601126799994,11.6,6.49762115899998));
#206611=CARTESIAN_POINT('Ctrl Pts',(9.09780059799994,15.2,6.50047799499998));
#206612=CARTESIAN_POINT('Ctrl Pts',(9.09780059799994,11.6,6.50047799499998));
#206613=CARTESIAN_POINT('Ctrl Pts',(9.09959026799994,15.2,6.50334040299998));
#206614=CARTESIAN_POINT('Ctrl Pts',(9.09959026799994,11.6,6.50334040299998));
#206615=CARTESIAN_POINT('Ctrl Pts',(9.10138026999994,15.2,6.50620838299999));
#206616=CARTESIAN_POINT('Ctrl Pts',(9.10138026999994,11.6,6.50620838299999));
#206617=CARTESIAN_POINT('Ctrl Pts',(9.10317058999994,15.2,6.50908192999999));
#206618=CARTESIAN_POINT('Ctrl Pts',(9.10317058999994,11.6,6.50908192999999));
#206619=CARTESIAN_POINT('Ctrl Pts',(9.10496121999994,15.2,6.51196104099999));
#206620=CARTESIAN_POINT('Ctrl Pts',(9.10496121999994,11.6,6.51196104099999));
#206621=CARTESIAN_POINT('Ctrl Pts',(9.10675215199995,15.2,6.51484571199998));
#206622=CARTESIAN_POINT('Ctrl Pts',(9.10675215199995,11.6,6.51484571199998));
#206623=CARTESIAN_POINT('Ctrl Pts',(9.10854337499994,15.2,6.51773593999999));
#206624=CARTESIAN_POINT('Ctrl Pts',(9.10854337499994,11.6,6.51773593999999));
#206625=CARTESIAN_POINT('Ctrl Pts',(9.11033487799994,15.2,6.52063171999998));
#206626=CARTESIAN_POINT('Ctrl Pts',(9.11033487799994,11.6,6.52063171999998));
#206627=CARTESIAN_POINT('Ctrl Pts',(9.11212665199994,15.2,6.52353305199998));
#206628=CARTESIAN_POINT('Ctrl Pts',(9.11212665199994,11.6,6.52353305199998));
#206629=CARTESIAN_POINT('Ctrl Pts',(9.11391868799994,15.2,6.52643992799998));
#206630=CARTESIAN_POINT('Ctrl Pts',(9.11391868799994,11.6,6.52643992799998));
#206631=CARTESIAN_POINT('Ctrl Pts',(9.11571097599994,15.2,6.52935234799998));
#206632=CARTESIAN_POINT('Ctrl Pts',(9.11571097599994,11.6,6.52935234799998));
#206633=CARTESIAN_POINT('Ctrl Pts',(9.11750350599995,15.2,6.53227030699998));
#206634=CARTESIAN_POINT('Ctrl Pts',(9.11750350599995,11.6,6.53227030699998));
#206635=CARTESIAN_POINT('Ctrl Pts',(9.11929626799994,15.2,6.53519380099999));
#206636=CARTESIAN_POINT('Ctrl Pts',(9.11929626799994,11.6,6.53519380099999));
#206637=CARTESIAN_POINT('Ctrl Pts',(9.12108925299994,15.2,6.53812282799999));
#206638=CARTESIAN_POINT('Ctrl Pts',(9.12108925299994,11.6,6.53812282799999));
#206639=CARTESIAN_POINT('Ctrl Pts',(9.12288245099995,15.2,6.54105738299998));
#206640=CARTESIAN_POINT('Ctrl Pts',(9.12288245099995,11.6,6.54105738299998));
#206641=CARTESIAN_POINT('Ctrl Pts',(9.12467585299994,15.2,6.54399746299998));
#206642=CARTESIAN_POINT('Ctrl Pts',(9.12467585299994,11.6,6.54399746299998));
#206643=CARTESIAN_POINT('Ctrl Pts',(9.12646944899994,15.2,6.54694306399998));
#206644=CARTESIAN_POINT('Ctrl Pts',(9.12646944899994,11.6,6.54694306399998));
#206645=CARTESIAN_POINT('Ctrl Pts',(9.12826322899994,15.2,6.54989418499999));
#206646=CARTESIAN_POINT('Ctrl Pts',(9.12826322899994,11.6,6.54989418499999));
#206647=CARTESIAN_POINT('Ctrl Pts',(9.13005718399994,15.2,6.55285081999998));
#206648=CARTESIAN_POINT('Ctrl Pts',(9.13005718399994,11.6,6.55285081999998));
#206649=CARTESIAN_POINT('Ctrl Pts',(9.13185130399994,15.2,6.55581296599999));
#206650=CARTESIAN_POINT('Ctrl Pts',(9.13185130399994,11.6,6.55581296599999));
#206651=CARTESIAN_POINT('Ctrl Pts',(9.13364558099994,15.2,6.55878061899998));
#206652=CARTESIAN_POINT('Ctrl Pts',(9.13364558099994,11.6,6.55878061899998));
#206653=CARTESIAN_POINT('Ctrl Pts',(9.13544000399994,15.2,6.56175377599999));
#206654=CARTESIAN_POINT('Ctrl Pts',(9.13544000399994,11.6,6.56175377599999));
#206655=CARTESIAN_POINT('Ctrl Pts',(9.13723456499994,15.2,6.56473243399999));
#206656=CARTESIAN_POINT('Ctrl Pts',(9.13723456499994,11.6,6.56473243399999));
#206657=CARTESIAN_POINT('Ctrl Pts',(9.13902925199995,15.2,6.56771658899999));
#206658=CARTESIAN_POINT('Ctrl Pts',(9.13902925199995,11.6,6.56771658899999));
#206659=CARTESIAN_POINT('Ctrl Pts',(9.14082405799994,15.2,6.57070623799999));
#206660=CARTESIAN_POINT('Ctrl Pts',(9.14082405799994,11.6,6.57070623799999));
#206661=CARTESIAN_POINT('Ctrl Pts',(9.14261897099994,15.2,6.57370137599998));
#206662=CARTESIAN_POINT('Ctrl Pts',(9.14261897099994,11.6,6.57370137599998));
#206663=CARTESIAN_POINT('Ctrl Pts',(9.14441398599994,15.2,6.57670200099999));
#206664=CARTESIAN_POINT('Ctrl Pts',(9.14441398599994,11.6,6.57670200099999));
#206665=CARTESIAN_POINT('Ctrl Pts',(9.14620908999994,15.2,6.57970810799998));
#206666=CARTESIAN_POINT('Ctrl Pts',(9.14620908999994,11.6,6.57970810799998));
#206667=CARTESIAN_POINT('Ctrl Pts',(9.14800427399994,15.2,6.58271969499998));
#206668=CARTESIAN_POINT('Ctrl Pts',(9.14800427399994,11.6,6.58271969499998));
#206669=CARTESIAN_POINT('Ctrl Pts',(9.14979952999994,15.2,6.58573675799998));
#206670=CARTESIAN_POINT('Ctrl Pts',(9.14979952999994,11.6,6.58573675799998));
#206671=CARTESIAN_POINT('Ctrl Pts',(9.15159484799995,15.2,6.58875929299998));
#206672=CARTESIAN_POINT('Ctrl Pts',(9.15159484799995,11.6,6.58875929299998));
#206673=CARTESIAN_POINT('Ctrl Pts',(9.15339021899995,15.2,6.59178729599999));
#206674=CARTESIAN_POINT('Ctrl Pts',(9.15339021899995,11.6,6.59178729599999));
#206675=CARTESIAN_POINT('Ctrl Pts',(9.15518563399995,15.2,6.59482076599998));
#206676=CARTESIAN_POINT('Ctrl Pts',(9.15518563399995,11.6,6.59482076599998));
#206677=CARTESIAN_POINT('Ctrl Pts',(9.15698108299994,15.2,6.59785969599999));
#206678=CARTESIAN_POINT('Ctrl Pts',(9.15698108299994,11.6,6.59785969599999));
#206679=CARTESIAN_POINT('Ctrl Pts',(9.15877655699994,15.2,6.60090408599999));
#206680=CARTESIAN_POINT('Ctrl Pts',(9.15877655699994,11.6,6.60090408599999));
#206681=CARTESIAN_POINT('Ctrl Pts',(9.16057204699994,15.2,6.60395392999998));
#206682=CARTESIAN_POINT('Ctrl Pts',(9.16057204699994,11.6,6.60395392999998));
#206683=CARTESIAN_POINT('Ctrl Pts',(9.16236754399994,15.2,6.60700922399998));
#206684=CARTESIAN_POINT('Ctrl Pts',(9.16236754399994,11.6,6.60700922399998));
#206685=CARTESIAN_POINT('Ctrl Pts',(9.16416303799994,15.2,6.61006996599999));
#206686=CARTESIAN_POINT('Ctrl Pts',(9.16416303799994,11.6,6.61006996599999));
#206687=CARTESIAN_POINT('Ctrl Pts',(9.16595852199995,15.2,6.61313615199998));
#206688=CARTESIAN_POINT('Ctrl Pts',(9.16595852199995,11.6,6.61313615199998));
#206689=CARTESIAN_POINT('Ctrl Pts',(9.16775398399994,15.2,6.61620777999998));
#206690=CARTESIAN_POINT('Ctrl Pts',(9.16775398399994,11.6,6.61620777999998));
#206691=CARTESIAN_POINT('Ctrl Pts',(9.16954941699995,15.2,6.61928484299998));
#206692=CARTESIAN_POINT('Ctrl Pts',(9.16954941699995,11.6,6.61928484299998));
#206693=CARTESIAN_POINT('Ctrl Pts',(9.17134480999995,15.2,6.62236733999999));
#206694=CARTESIAN_POINT('Ctrl Pts',(9.17134480999995,11.6,6.62236733999999));
#206695=CARTESIAN_POINT('Ctrl Pts',(9.17314015699995,15.2,6.62545526799998));
#206696=CARTESIAN_POINT('Ctrl Pts',(9.17314015699995,11.6,6.62545526799998));
#206697=CARTESIAN_POINT('Ctrl Pts',(9.17493544599994,15.2,6.62854862099999));
#206698=CARTESIAN_POINT('Ctrl Pts',(9.17493544599994,11.6,6.62854862099999));
#206699=CARTESIAN_POINT('Ctrl Pts',(9.17673066899994,15.2,6.63164739699998));
#206700=CARTESIAN_POINT('Ctrl Pts',(9.17673066899994,11.6,6.63164739699998));
#206701=CARTESIAN_POINT('Ctrl Pts',(9.17852581699995,15.2,6.63475159199999));
#206702=CARTESIAN_POINT('Ctrl Pts',(9.17852581699995,11.6,6.63475159199999));
#206703=CARTESIAN_POINT('Ctrl Pts',(9.18032088299995,15.2,6.63786120299999));
#206704=CARTESIAN_POINT('Ctrl Pts',(9.18032088299995,11.6,6.63786120299999));
#206705=CARTESIAN_POINT('Ctrl Pts',(9.18211585399994,15.2,6.64097622599999));
#206706=CARTESIAN_POINT('Ctrl Pts',(9.18211585399994,11.6,6.64097622599999));
#206707=CARTESIAN_POINT('Ctrl Pts',(9.18391072399994,15.2,6.64409665799998));
#206708=CARTESIAN_POINT('Ctrl Pts',(9.18391072399994,11.6,6.64409665799998));
#206709=CARTESIAN_POINT('Ctrl Pts',(9.18570548299994,15.2,6.64722249499999));
#206710=CARTESIAN_POINT('Ctrl Pts',(9.18570548299994,11.6,6.64722249499999));
#206711=CARTESIAN_POINT('Ctrl Pts',(9.18750012399994,15.2,6.65035373299999));
#206712=CARTESIAN_POINT('Ctrl Pts',(9.18750012399994,11.6,6.65035373299999));
#206713=CARTESIAN_POINT('Ctrl Pts',(9.18929463499994,15.2,6.65349036999999));
#206714=CARTESIAN_POINT('Ctrl Pts',(9.18929463499994,11.6,6.65349036999999));
#206715=CARTESIAN_POINT('Ctrl Pts',(9.19108900999994,15.2,6.65663239999999));
#206716=CARTESIAN_POINT('Ctrl Pts',(9.19108900999994,11.6,6.65663239999999));
#206717=CARTESIAN_POINT('Ctrl Pts',(9.19288323699995,15.2,6.65977982199998));
#206718=CARTESIAN_POINT('Ctrl Pts',(9.19288323699995,11.6,6.65977982199998));
#206719=CARTESIAN_POINT('Ctrl Pts',(9.19467730999994,15.2,6.66293263099998));
#206720=CARTESIAN_POINT('Ctrl Pts',(9.19467730999994,11.6,6.66293263099998));
#206721=CARTESIAN_POINT('Ctrl Pts',(9.19647121899994,15.2,6.66609082299999));
#206722=CARTESIAN_POINT('Ctrl Pts',(9.19647121899994,11.6,6.66609082299999));
#206723=CARTESIAN_POINT('Ctrl Pts',(9.19826495499994,15.2,6.66925439599999));
#206724=CARTESIAN_POINT('Ctrl Pts',(9.19826495499994,11.6,6.66925439599999));
#206725=CARTESIAN_POINT('Ctrl Pts',(9.20005851099994,15.2,6.67242334499999));
#206726=CARTESIAN_POINT('Ctrl Pts',(9.20005851099994,11.6,6.67242334499999));
#206727=CARTESIAN_POINT('Ctrl Pts',(9.20185187499994,15.2,6.67559766799998));
#206728=CARTESIAN_POINT('Ctrl Pts',(9.20185187499994,11.6,6.67559766799998));
#206729=CARTESIAN_POINT('Ctrl Pts',(9.20364504099994,15.2,6.67877735899999));
#206730=CARTESIAN_POINT('Ctrl Pts',(9.20364504099994,11.6,6.67877735899999));
#206731=CARTESIAN_POINT('Ctrl Pts',(9.20543799999994,15.2,6.68196241699999));
#206732=CARTESIAN_POINT('Ctrl Pts',(9.20543799999994,11.6,6.68196241699999));
#206733=CARTESIAN_POINT('Ctrl Pts',(9.20723074199995,15.2,6.68515283699998));
#206734=CARTESIAN_POINT('Ctrl Pts',(9.20723074199995,11.6,6.68515283699998));
#206735=CARTESIAN_POINT('Ctrl Pts',(9.20902325999995,15.2,6.68834861599999));
#206736=CARTESIAN_POINT('Ctrl Pts',(9.20902325999995,11.6,6.68834861599999));
#206737=CARTESIAN_POINT('Ctrl Pts',(9.21081554299995,15.2,6.69154974999999));
#206738=CARTESIAN_POINT('Ctrl Pts',(9.21081554299995,11.6,6.69154974999999));
#206739=CARTESIAN_POINT('Ctrl Pts',(9.21260758499994,15.2,6.69475623599999));
#206740=CARTESIAN_POINT('Ctrl Pts',(9.21260758499994,11.6,6.69475623599999));
#206741=CARTESIAN_POINT('Ctrl Pts',(9.21439937499994,15.2,6.69796807099999));
#206742=CARTESIAN_POINT('Ctrl Pts',(9.21439937499994,11.6,6.69796807099999));
#206743=CARTESIAN_POINT('Ctrl Pts',(9.21619090599994,15.2,6.70118524899999));
#206744=CARTESIAN_POINT('Ctrl Pts',(9.21619090599994,11.6,6.70118524899999));
#206745=CARTESIAN_POINT('Ctrl Pts',(9.21798216799995,15.2,6.70440776899999));
#206746=CARTESIAN_POINT('Ctrl Pts',(9.21798216799995,11.6,6.70440776899999));
#206747=CARTESIAN_POINT('Ctrl Pts',(9.21977315299995,15.2,6.70763562499998));
#206748=CARTESIAN_POINT('Ctrl Pts',(9.21977315299995,11.6,6.70763562499998));
#206749=CARTESIAN_POINT('Ctrl Pts',(9.22156385299994,15.2,6.71086881599999));
#206750=CARTESIAN_POINT('Ctrl Pts',(9.22156385299994,11.6,6.71086881599999));
#206751=CARTESIAN_POINT('Ctrl Pts',(9.22335425899995,15.2,6.71410733599998));
#206752=CARTESIAN_POINT('Ctrl Pts',(9.22335425899995,11.6,6.71410733599998));
#206753=CARTESIAN_POINT('Ctrl Pts',(9.22514436299995,15.2,6.71735118499999));
#206754=CARTESIAN_POINT('Ctrl Pts',(9.22514436299995,11.6,6.71735118499999));
#206755=CARTESIAN_POINT('Ctrl Pts',(9.22693415699994,15.2,6.72060035599999));
#206756=CARTESIAN_POINT('Ctrl Pts',(9.22693415699994,11.6,6.72060035599999));
#206757=CARTESIAN_POINT('Ctrl Pts',(9.22872363199994,15.2,6.72385484699999));
#206758=CARTESIAN_POINT('Ctrl Pts',(9.22872363199994,11.6,6.72385484699999));
#206759=CARTESIAN_POINT('Ctrl Pts',(9.23051277899994,15.2,6.72711465399999));
#206760=CARTESIAN_POINT('Ctrl Pts',(9.23051277899994,11.6,6.72711465399999));
#206761=CARTESIAN_POINT('Ctrl Pts',(9.23230158999995,15.2,6.73037977299998));
#206762=CARTESIAN_POINT('Ctrl Pts',(9.23230158999995,11.6,6.73037977299998));
#206763=CARTESIAN_POINT('Ctrl Pts',(9.23409005699994,15.2,6.73365020099999));
#206764=CARTESIAN_POINT('Ctrl Pts',(9.23409005699994,11.6,6.73365020099999));
#206765=CARTESIAN_POINT('Ctrl Pts',(9.23587816899994,15.2,6.73692593499998));
#206766=CARTESIAN_POINT('Ctrl Pts',(9.23587816899994,11.6,6.73692593499998));
#206767=CARTESIAN_POINT('Ctrl Pts',(9.23766591999994,15.2,6.74020696899999));
#206768=CARTESIAN_POINT('Ctrl Pts',(9.23766591999994,11.6,6.74020696899999));
#206769=CARTESIAN_POINT('Ctrl Pts',(9.23945329899994,15.2,6.74349330199998));
#206770=CARTESIAN_POINT('Ctrl Pts',(9.23945329899994,11.6,6.74349330199998));
#206771=CARTESIAN_POINT('Ctrl Pts',(9.24124029999994,15.2,6.74678492799998));
#206772=CARTESIAN_POINT('Ctrl Pts',(9.24124029999994,11.6,6.74678492799998));
#206773=CARTESIAN_POINT('Ctrl Pts',(9.24302691299994,15.2,6.75008184599999));
#206774=CARTESIAN_POINT('Ctrl Pts',(9.24302691299994,11.6,6.75008184599999));
#206775=CARTESIAN_POINT('Ctrl Pts',(9.24481313099994,15.2,6.75338405099998));
#206776=CARTESIAN_POINT('Ctrl Pts',(9.24481313099994,11.6,6.75338405099998));
#206777=CARTESIAN_POINT('Ctrl Pts',(9.24659894799994,15.2,6.75669153999999));
#206778=CARTESIAN_POINT('Ctrl Pts',(9.24659894799994,11.6,6.75669153999999));
#206779=CARTESIAN_POINT('Ctrl Pts',(9.24838435499994,15.2,6.76000431099999));
#206780=CARTESIAN_POINT('Ctrl Pts',(9.24838435499994,11.6,6.76000431099999));
#206781=CARTESIAN_POINT('Ctrl Pts',(9.25016934499994,15.2,6.76332235799999));
#206782=CARTESIAN_POINT('Ctrl Pts',(9.25016934499994,11.6,6.76332235799999));
#206783=CARTESIAN_POINT('Ctrl Pts',(9.25195390799994,15.2,6.76664567999998));
#206784=CARTESIAN_POINT('Ctrl Pts',(9.25195390799994,11.6,6.76664567999998));
#206785=CARTESIAN_POINT('Ctrl Pts',(9.25373803599994,15.2,6.76997427199999));
#206786=CARTESIAN_POINT('Ctrl Pts',(9.25373803599994,11.6,6.76997427199999));
#206787=CARTESIAN_POINT('Ctrl Pts',(9.25552171699995,15.2,6.77330812899999));
#206788=CARTESIAN_POINT('Ctrl Pts',(9.25552171699995,11.6,6.77330812899999));
#206789=CARTESIAN_POINT('Ctrl Pts',(9.25730494299994,15.2,6.77664724599998));
#206790=CARTESIAN_POINT('Ctrl Pts',(9.25730494299994,11.6,6.77664724599998));
#206791=CARTESIAN_POINT('Ctrl Pts',(9.25908770199994,15.2,6.77999162099999));
#206792=CARTESIAN_POINT('Ctrl Pts',(9.25908770199994,11.6,6.77999162099999));
#206793=CARTESIAN_POINT('Ctrl Pts',(9.26086998599994,15.2,6.78334124699998));
#206794=CARTESIAN_POINT('Ctrl Pts',(9.26086998599994,11.6,6.78334124699998));
#206795=CARTESIAN_POINT('Ctrl Pts',(9.26265178899994,15.2,6.78669612499998));
#206796=CARTESIAN_POINT('Ctrl Pts',(9.26265178899994,11.6,6.78669612499998));
#206797=CARTESIAN_POINT('Ctrl Pts',(9.26443310199994,15.2,6.79005624799998));
#206798=CARTESIAN_POINT('Ctrl Pts',(9.26443310199994,11.6,6.79005624799998));
#206799=CARTESIAN_POINT('Ctrl Pts',(9.26621392399994,15.2,6.79342161599998));
#206800=CARTESIAN_POINT('Ctrl Pts',(9.26621392399994,11.6,6.79342161599998));
#206801=CARTESIAN_POINT('Ctrl Pts',(9.26799425299994,15.2,6.79679222999999));
#206802=CARTESIAN_POINT('Ctrl Pts',(9.26799425299994,11.6,6.79679222999999));
#206803=CARTESIAN_POINT('Ctrl Pts',(9.26941811999994,15.2,6.79949291499998));
#206804=CARTESIAN_POINT('Ctrl Pts',(9.26941811999994,11.6,6.79949291499998));
#206805=CARTESIAN_POINT('Ctrl Pts',(9.27048579799994,15.2,6.80152078799999));
#206806=CARTESIAN_POINT('Ctrl Pts',(9.27048579799994,11.6,6.80152078799999));
#206807=CARTESIAN_POINT('Ctrl Pts',(9.27119748299994,15.2,6.80287375299999));
#206808=CARTESIAN_POINT('Ctrl Pts',(9.27119748299994,11.6,6.80287375299999));
#206809=CARTESIAN_POINT('Ctrl Pts',(9.27155330199994,15.2,6.80355049599999));
#206810=CARTESIAN_POINT('Ctrl Pts',(9.27155330199994,11.6,6.80355049599999));
#206811=CARTESIAN_POINT('Ctrl Pts',(8.56667970899995,15.2,5.85257411499998));
#206812=CARTESIAN_POINT('Ctrl Pts',(8.5680628930964,15.2,5.85370502577855));
#206813=CARTESIAN_POINT('Ctrl Pts',(8.5694869244067,15.2,5.85487627485597));
#206814=CARTESIAN_POINT('Ctrl Pts',(8.5709506523979,15.2,5.85608775314224));
#206815=CARTESIAN_POINT('Ctrl Pts',(8.57242143922536,15.2,5.85730507378917));
#206816=CARTESIAN_POINT('Ctrl Pts',(8.57393230443574,15.2,5.85856301214596));
#206817=CARTESIAN_POINT('Ctrl Pts',(8.57548210843323,15.2,5.85986145286728));
#206818=CARTESIAN_POINT('Ctrl Pts',(8.57703191228994,15.2,5.86115989347067));
#206819=CARTESIAN_POINT('Ctrl Pts',(8.57862065432565,15.2,5.8624988373167));
#206820=CARTESIAN_POINT('Ctrl Pts',(8.58024722826654,15.2,5.86387816976658));
#206821=CARTESIAN_POINT('Ctrl Pts',(8.58187380220742,15.2,5.86525750221645));
#206822=CARTESIAN_POINT('Ctrl Pts',(8.58353820816439,15.2,5.86667722297458));
#206823=CARTESIAN_POINT('Ctrl Pts',(8.58523937135207,15.2,5.86813722032544));
#206824=CARTESIAN_POINT('Ctrl Pts',(8.58694053469429,15.2,5.86959721780893));
#206825=CARTESIAN_POINT('Ctrl Pts',(8.58867845563581,15.2,5.87109748993948));
#206826=CARTESIAN_POINT('Ctrl Pts',(8.59045208798488,15.2,5.87263792444283));
#206827=CARTESIAN_POINT('Ctrl Pts',(8.59252132548382,15.2,5.87443509782017));
#206828=CARTESIAN_POINT('Ctrl Pts',(8.59463917073834,15.2,5.87628693691257));
#206829=CARTESIAN_POINT('Ctrl Pts',(8.59680401336214,15.2,5.87819326040028));
#206830=CARTESIAN_POINT('Ctrl Pts',(8.59865959297066,15.2,5.87982725215201));
#206831=CARTESIAN_POINT('Ctrl Pts',(8.60054970122744,15.2,5.88150127369895));
#206832=CARTESIAN_POINT('Ctrl Pts',(8.60247335675124,15.2,5.88321521321174));
#206833=CARTESIAN_POINT('Ctrl Pts',(8.6043970121003,15.2,5.88492915256886));
#206834=CARTESIAN_POINT('Ctrl Pts',(8.60635421133064,15.2,5.88668300813266));
#206835=CARTESIAN_POINT('Ctrl Pts',(8.60834399976746,15.2,5.8884766674924));
#206836=CARTESIAN_POINT('Ctrl Pts',(8.61033378820427,15.2,5.89027032685213));
#206837=CARTESIAN_POINT('Ctrl Pts',(8.61235616229743,15.2,5.89210379097614));
#206838=CARTESIAN_POINT('Ctrl Pts',(8.61441019188808,15.2,5.89397694365633));
#206839=CARTESIAN_POINT('Ctrl Pts',(8.6164642216653,15.2,5.89585009650669));
#206840=CARTESIAN_POINT('Ctrl Pts',(8.61854990577146,15.2,5.89776294282028));
#206841=CARTESIAN_POINT('Ctrl Pts',(8.62066633380559,15.2,5.89971536542941));
#206842=CARTESIAN_POINT('Ctrl Pts',(8.62278276164747,15.2,5.90166778786119));
#206843=CARTESIAN_POINT('Ctrl Pts',(8.62492993542981,15.2,5.9036597878579));
#206844=CARTESIAN_POINT('Ctrl Pts',(8.627106966352,15.2,5.90569125236913));
#206845=CARTESIAN_POINT('Ctrl Pts',(8.62928399727419,15.2,5.90772271688036));
#206846=CARTESIAN_POINT('Ctrl Pts',(8.63149088542733,15.2,5.90979364605512));
#206847=CARTESIAN_POINT('Ctrl Pts',(8.63372676734483,15.2,5.91190392739341));
#206848=CARTESIAN_POINT('Ctrl Pts',(8.63596264926232,15.2,5.91401420873169));
#206849=CARTESIAN_POINT('Ctrl Pts',(8.63822752414354,15.2,5.91616384011022));
#206850=CARTESIAN_POINT('Ctrl Pts',(8.64052054897496,15.2,5.91835271052801));
#206851=CARTESIAN_POINT('Ctrl Pts',(8.64281357401467,15.2,5.92054158114462));
#206852=CARTESIAN_POINT('Ctrl Pts',(8.64513474718215,15.2,5.92276968904004));
#206853=CARTESIAN_POINT('Ctrl Pts',(8.64748324564467,15.2,5.92503692258198));
#206854=CARTESIAN_POINT('Ctrl Pts',(8.64983174389386,15.2,5.92730415591797));
#206855=CARTESIAN_POINT('Ctrl Pts',(8.65220756771585,15.2,5.92961051408417));
#206856=CARTESIAN_POINT('Ctrl Pts',(8.65460991187742,15.2,5.9319558825806));
#206857=CARTESIAN_POINT('Ctrl Pts',(8.65701225603899,15.2,5.93430125107702));
#206858=CARTESIAN_POINT('Ctrl Pts',(8.65944111983161,15.2,5.93668563184312));
#206859=CARTESIAN_POINT('Ctrl Pts',(8.66189571899069,15.2,5.93910890925246));
#206860=CARTESIAN_POINT('Ctrl Pts',(8.66435031837273,15.2,5.9415321868819));
#206861=CARTESIAN_POINT('Ctrl Pts',(8.66683065253225,15.2,5.94399436288172));
#206862=CARTESIAN_POINT('Ctrl Pts',(8.66933595116988,15.2,5.94649532068638));
#206863=CARTESIAN_POINT('Ctrl Pts',(8.67225879923911,15.2,5.94941310445107));
#206864=CARTESIAN_POINT('Ctrl Pts',(8.67521562943652,15.2,5.95238367869775));
#206865=CARTESIAN_POINT('Ctrl Pts',(8.67820524826226,15.2,5.95540685999247));
#206866=CARTESIAN_POINT('Ctrl Pts',(8.68076777898359,15.2,5.95799815854772));
#206867=CARTESIAN_POINT('Ctrl Pts',(8.68335440181564,15.2,5.96062810723174));
#206868=CARTESIAN_POINT('Ctrl Pts',(8.68596438262558,15.2,5.96329659187885));
#206869=CARTESIAN_POINT('Ctrl Pts',(8.68857436319844,15.2,5.96596507628358));
#206870=CARTESIAN_POINT('Ctrl Pts',(8.69120770284151,15.2,5.96867209749437));
#206871=CARTESIAN_POINT('Ctrl Pts',(8.69386368550703,15.2,5.97141753899034));
#206872=CARTESIAN_POINT('Ctrl Pts',(8.69651966817254,15.2,5.9741629804863));
#206873=CARTESIAN_POINT('Ctrl Pts',(8.69919829322183,15.2,5.97694684462246));
#206874=CARTESIAN_POINT('Ctrl Pts',(8.70189885895555,15.2,5.97976901493398));
#206875=CARTESIAN_POINT('Ctrl Pts',(8.70459942493457,15.2,5.98259118550184));
#206876=CARTESIAN_POINT('Ctrl Pts',(8.70732193266089,15.2,5.9854516627421));
#206877=CARTESIAN_POINT('Ctrl Pts',(8.71006569578205,15.2,5.98835033154708));
#206878=CARTESIAN_POINT('Ctrl Pts',(8.71235216492506,15.2,5.99076588875292));
#206879=CARTESIAN_POINT('Ctrl Pts',(8.71465339369052,15.2,5.99320796962066));
#206880=CARTESIAN_POINT('Ctrl Pts',(8.7169689935528,15.2,5.99567650358114));
#206881=CARTESIAN_POINT('Ctrl Pts',(8.71928459341506,15.2,5.99814503754163));
#206882=CARTESIAN_POINT('Ctrl Pts',(8.72161456367202,15.2,6.00064002790532));
#206883=CARTESIAN_POINT('Ctrl Pts',(8.7239585220065,15.2,6.00316140658806));
#206884=CARTESIAN_POINT('Ctrl Pts',(8.72677127190571,15.2,6.00618706089739));
#206885=CARTESIAN_POINT('Ctrl Pts',(8.72960416329157,15.2,6.00925071275516));
#206886=CARTESIAN_POINT('Ctrl Pts',(8.73245654618878,15.2,6.01235225089412));
#206887=CARTESIAN_POINT('Ctrl Pts',(8.73483353202283,15.2,6.01493686610382));
#206888=CARTESIAN_POINT('Ctrl Pts',(8.7372240554676,15.2,6.01754778784338));
#206889=CARTESIAN_POINT('Ctrl Pts',(8.73962774394052,15.2,6.02018495145588));
#206890=CARTESIAN_POINT('Ctrl Pts',(8.74203143241346,15.2,6.02282211506838));
#206891=CARTESIAN_POINT('Ctrl Pts',(8.74444828873749,15.2,6.02548551968159));
#206892=CARTESIAN_POINT('Ctrl Pts',(8.74687794754034,15.2,6.02817509780391));
#206893=CARTESIAN_POINT('Ctrl Pts',(8.74930760634317,15.2,6.03086467592622));
#206894=CARTESIAN_POINT('Ctrl Pts',(8.75175007054779,15.2,6.03358042787311));
#206895=CARTESIAN_POINT('Ctrl Pts',(8.75420497985435,15.2,6.03632228662523));
#206896=CARTESIAN_POINT('Ctrl Pts',(8.75665988916092,15.2,6.03906414537735));
#206897=CARTESIAN_POINT('Ctrl Pts',(8.75912724439545,15.2,6.04183210994103));
#206898=CARTESIAN_POINT('Ctrl Pts',(8.7616066938409,15.2,6.04462611362372));
#206899=CARTESIAN_POINT('Ctrl Pts',(8.76408614301609,15.2,6.04742011700186));
#206900=CARTESIAN_POINT('Ctrl Pts',(8.76657768737967,15.2,6.05024015992893));
#206901=CARTESIAN_POINT('Ctrl Pts',(8.76908098043915,15.2,6.05308617343601));
#206902=CARTESIAN_POINT('Ctrl Pts',(8.77208493260169,15.2,6.05650139020287));
#206903=CARTESIAN_POINT('Ctrl Pts',(8.77510579954927,15.2,6.05995400576511));
#206904=CARTESIAN_POINT('Ctrl Pts',(8.77814299788217,15.2,6.06344390245694));
#206905=CARTESIAN_POINT('Ctrl Pts',(8.78067399635499,15.2,6.06635214954162));
#206906=CARTESIAN_POINT('Ctrl Pts',(8.7832163332847,15.2,6.06928628678283));
#206907=CARTESIAN_POINT('Ctrl Pts',(8.78576967778803,15.2,6.07224624637696));
#206908=CARTESIAN_POINT('Ctrl Pts',(8.7888336910807,15.2,6.07579819776084));
#206909=CARTESIAN_POINT('Ctrl Pts',(8.79191355052904,15.2,6.07938733029834));
#206910=CARTESIAN_POINT('Ctrl Pts',(8.79500869074992,15.2,6.08301353149992));
#206911=CARTESIAN_POINT('Ctrl Pts',(8.79758797436103,15.2,6.08603536594437));
#206912=CARTESIAN_POINT('Ctrl Pts',(8.80017786915547,15.2,6.08908294014436));
#206913=CARTESIAN_POINT('Ctrl Pts',(8.80277805047492,15.2,6.09215618569992));
#206914=CARTESIAN_POINT('Ctrl Pts',(8.80589826794488,15.2,6.09584408023259));
#206915=CARTESIAN_POINT('Ctrl Pts',(8.80903330020322,15.2,6.09956894344534));
#206916=CARTESIAN_POINT('Ctrl Pts',(8.8121825957453,15.2,6.10333065591111));
#206917=CARTESIAN_POINT('Ctrl Pts',(8.81480700879237,15.2,6.10646541641316));
#206918=CARTESIAN_POINT('Ctrl Pts',(8.81744132895533,15.2,6.10962576611528));
#206919=CARTESIAN_POINT('Ctrl Pts',(8.82008524034373,15.2,6.11281163805839));
#206920=CARTESIAN_POINT('Ctrl Pts',(8.82272915173212,15.2,6.11599751000151));
#206921=CARTESIAN_POINT('Ctrl Pts',(8.82538265723187,15.2,6.11920890214527));
#206922=CARTESIAN_POINT('Ctrl Pts',(8.82804544605083,15.2,6.12244574825506));
#206923=CARTESIAN_POINT('Ctrl Pts',(8.83017567722211,15.2,6.12503522528401));
#206924=CARTESIAN_POINT('Ctrl Pts',(8.83231185069209,15.2,6.12764099153853));
#206925=CARTESIAN_POINT('Ctrl Pts',(8.83445381002743,15.2,6.13026301214715));
#206926=CARTESIAN_POINT('Ctrl Pts',(8.83659576907094,15.2,6.13288503239852));
#206927=CARTESIAN_POINT('Ctrl Pts',(8.83874351484201,15.2,6.13552330723169));
#206928=CARTESIAN_POINT('Ctrl Pts',(8.84089689183227,15.2,6.1381778012914));
#206929=CARTESIAN_POINT('Ctrl Pts',(8.84358861329014,15.2,6.14149591913729));
#206930=CARTESIAN_POINT('Ctrl Pts',(8.8462891356399,15.2,6.14483937880884));
#206931=CARTESIAN_POINT('Ctrl Pts',(8.84899816105614,15.2,6.1482081124881));
#206932=CARTESIAN_POINT('Ctrl Pts',(8.85116538150725,15.2,6.15090309957838));
#206933=CARTESIAN_POINT('Ctrl Pts',(8.8533380425436,15.2,6.15361426078727));
#206934=CARTESIAN_POINT('Ctrl Pts',(8.85551599654933,15.2,6.15634156262911));
#206935=CARTESIAN_POINT('Ctrl Pts',(8.85769395025832,15.2,6.15906886409935));
#206936=CARTESIAN_POINT('Ctrl Pts',(8.85987719475863,15.2,6.16181230492056));
#206937=CARTESIAN_POINT('Ctrl Pts',(8.86206558307941,15.2,6.16457184908281));
#206938=CARTESIAN_POINT('Ctrl Pts',(8.86425397169834,15.2,6.16733139362106));
#206939=CARTESIAN_POINT('Ctrl Pts',(8.8664475039929,15.2,6.17010704278621));
#206940=CARTESIAN_POINT('Ctrl Pts',(8.86864603244637,15.2,6.17289876049496));
#206941=CARTESIAN_POINT('Ctrl Pts',(8.87084456060029,15.2,6.17569047782334));
#206942=CARTESIAN_POINT('Ctrl Pts',(8.87304808295569,15.2,6.17849826241198));
#206943=CARTESIAN_POINT('Ctrl Pts',(8.87525645866284,15.2,6.18132208126526));
#206944=CARTESIAN_POINT('Ctrl Pts',(8.87746483467088,15.2,6.18414590050328));
#206945=CARTESIAN_POINT('Ctrl Pts',(8.879678060549,15.2,6.1869857517213));
#206946=CARTESIAN_POINT('Ctrl Pts',(8.88189599444795,15.2,6.18984160076687));
#206947=CARTESIAN_POINT('Ctrl Pts',(8.88411392804472,15.2,6.19269744942335));
#206948=CARTESIAN_POINT('Ctrl Pts',(8.88633656892387,15.2,6.19556929469327));
#206949=CARTESIAN_POINT('Ctrl Pts',(8.88856377518578,15.2,6.1984571020111));
#206950=CARTESIAN_POINT('Ctrl Pts',(8.89079098175113,15.2,6.20134490972241));
#206951=CARTESIAN_POINT('Ctrl Pts',(8.89302275239719,15.2,6.20424867866005));
#206952=CARTESIAN_POINT('Ctrl Pts',(8.89525894841812,15.2,6.20716837377692));
#206953=CARTESIAN_POINT('Ctrl Pts',(8.89749514413435,15.2,6.21008806849597));
#206954=CARTESIAN_POINT('Ctrl Pts',(8.89973576467797,15.2,6.21302368932974));
#206955=CARTESIAN_POINT('Ctrl Pts',(8.90198067038289,15.2,6.21597519880903));
#206956=CARTESIAN_POINT('Ctrl Pts',(8.90422557639367,15.2,6.21892670869046));
#206957=CARTESIAN_POINT('Ctrl Pts',(8.90647476742156,15.2,6.22189410903455));
#206958=CARTESIAN_POINT('Ctrl Pts',(8.9087281067666,15.2,6.22487736347492));
#206959=CARTESIAN_POINT('Ctrl Pts',(8.91098144611163,15.2,6.22786061791528));
#206960=CARTESIAN_POINT('Ctrl Pts',(8.91323893364324,15.2,6.23085972637972));
#206961=CARTESIAN_POINT('Ctrl Pts',(8.91550043237802,15.2,6.23387465226788));
#206962=CARTESIAN_POINT('Ctrl Pts',(8.91945805470169,15.2,6.23915077195598));
#206963=CARTESIAN_POINT('Ctrl Pts',(8.92342796201238,15.2,6.24447533789665));
#206964=CARTESIAN_POINT('Ctrl Pts',(8.92740943459731,15.2,6.24984814974075));
#206965=CARTESIAN_POINT('Ctrl Pts',(8.92968456205439,15.2,6.25291832829594));
#206966=CARTESIAN_POINT('Ctrl Pts',(8.93196346525637,15.2,6.25600426303358));
#206967=CARTESIAN_POINT('Ctrl Pts',(8.93424601393656,15.2,6.25910591620363));
#206968=CARTESIAN_POINT('Ctrl Pts',(8.93652856230575,15.2,6.26220756895108));
#206969=CARTESIAN_POINT('Ctrl Pts',(8.93881475505471,15.2,6.26532494099083));
#206970=CARTESIAN_POINT('Ctrl Pts',(8.94110446092603,15.2,6.26845799577872));
#206971=CARTESIAN_POINT('Ctrl Pts',(8.94396659349916,15.2,6.27237431458373));
#206972=CARTESIAN_POINT('Ctrl Pts',(8.94683421543458,15.2,6.27631513700315));
#206973=CARTESIAN_POINT('Ctrl Pts',(8.94970707383708,15.2,6.28028039318241));
#206974=CARTESIAN_POINT('Ctrl Pts',(8.95200536068434,15.2,6.28345259829872));
#206975=CARTESIAN_POINT('Ctrl Pts',(8.95430699953477,15.2,6.28664044093633));
#206976=CARTESIAN_POINT('Ctrl Pts',(8.95661186043839,15.2,6.28984388477862));
#206977=CARTESIAN_POINT('Ctrl Pts',(8.95891672102797,15.2,6.29304732818445));
#206978=CARTESIAN_POINT('Ctrl Pts',(8.96122480600498,15.2,6.29626637326537));
#206979=CARTESIAN_POINT('Ctrl Pts',(8.96353598793125,15.2,6.29950098277232));
#206980=CARTESIAN_POINT('Ctrl Pts',(8.96584717017242,15.2,6.30273559271998));
#206981=CARTESIAN_POINT('Ctrl Pts',(8.96816144901848,15.2,6.30598576745194));
#206982=CARTESIAN_POINT('Ctrl Pts',(8.97047869792273,15.2,6.30925147124204));
#206983=CARTESIAN_POINT('Ctrl Pts',(8.97395457096337,15.2,6.31415002648222));
#206984=CARTESIAN_POINT('Ctrl Pts',(8.97743713109518,15.2,6.31908351863633));
#206985=CARTESIAN_POINT('Ctrl Pts',(8.98092595605148,15.2,6.3240518297043));
#206986=CARTESIAN_POINT('Ctrl Pts',(8.98383331028737,15.2,6.32819208907803));
#206987=CARTESIAN_POINT('Ctrl Pts',(8.98674501732613,15.2,6.33235652534406));
#206988=CARTESIAN_POINT('Ctrl Pts',(8.98966083732594,15.2,6.33654506742614));
#206989=CARTESIAN_POINT('Ctrl Pts',(8.9919934934529,15.2,6.33989590127442));
#206990=CARTESIAN_POINT('Ctrl Pts',(8.9943287804142,15.2,6.34326216385));
#206991=CARTESIAN_POINT('Ctrl Pts',(8.99666658004752,15.2,6.34664381848238));
#206992=CARTESIAN_POINT('Ctrl Pts',(8.99900437936231,15.2,6.35002547265401));
#206993=CARTESIAN_POINT('Ctrl Pts',(9.00134469007511,15.2,6.3534225174483));
#206994=CARTESIAN_POINT('Ctrl Pts',(9.00368739205011,15.2,6.35683491744611));
#206995=CARTESIAN_POINT('Ctrl Pts',(9.0072014454914,15.2,6.36195351814023));
#206996=CARTESIAN_POINT('Ctrl Pts',(9.01072088114167,15.2,6.36710666826365));
#206997=CARTESIAN_POINT('Ctrl Pts',(9.01424529666743,15.2,6.37229424204872));
#206998=CARTESIAN_POINT('Ctrl Pts',(9.0165949066978,15.2,6.37575262410089));
#206999=CARTESIAN_POINT('Ctrl Pts',(9.01894673218841,15.2,6.37922630720309));
#207000=CARTESIAN_POINT('Ctrl Pts',(9.02130065350667,15.2,6.38271525198922));
#207001=CARTESIAN_POINT('Ctrl Pts',(9.02365457514564,15.2,6.38620419725072));
#207002=CARTESIAN_POINT('Ctrl Pts',(9.02601059384287,15.2,6.38970840671256));
#207003=CARTESIAN_POINT('Ctrl Pts',(9.02836859469381,15.2,6.39322784185036));
#207004=CARTESIAN_POINT('Ctrl Pts',(9.03072659522346,15.2,6.39674727650864));
#207005=CARTESIAN_POINT('Ctrl Pts',(9.0330865766612,15.2,6.40028193766774));
#207006=CARTESIAN_POINT('Ctrl Pts',(9.03544842402354,15.2,6.40383178770987));
#207007=CARTESIAN_POINT('Ctrl Pts',(9.03840073346781,15.2,6.40826910062526));
#207008=CARTESIAN_POINT('Ctrl Pts',(9.041355960696,15.2,6.41273014772717));
#207009=CARTESIAN_POINT('Ctrl Pts',(9.04431388251499,15.2,6.41721485628915));
#207010=CARTESIAN_POINT('Ctrl Pts',(9.04668022009914,15.2,6.42080262333426));
#207011=CARTESIAN_POINT('Ctrl Pts',(9.04904828155528,15.2,6.42440553269552));
#207012=CARTESIAN_POINT('Ctrl Pts',(9.05141795462904,15.2,6.42802354861647));
#207013=CARTESIAN_POINT('Ctrl Pts',(9.05378762737993,15.2,6.43164156404447));
#207014=CARTESIAN_POINT('Ctrl Pts',(9.05615891412505,15.2,6.43527468624827));
#207015=CARTESIAN_POINT('Ctrl Pts',(9.05853170076431,15.2,6.4389228768935));
#207016=CARTESIAN_POINT('Ctrl Pts',(9.06090448772687,15.2,6.44257106803579));
#207017=CARTESIAN_POINT('Ctrl Pts',(9.06327877612417,15.2,6.446234329276));
#207018=CARTESIAN_POINT('Ctrl Pts',(9.06565445459468,15.2,6.44991262255042));
#207019=CARTESIAN_POINT('Ctrl Pts',(9.06803013274149,15.2,6.45359091532368));
#207020=CARTESIAN_POINT('Ctrl Pts',(9.07040720007505,15.2,6.45728423930107));
#207021=CARTESIAN_POINT('Ctrl Pts',(9.07278555004719,15.2,6.46099255866358));
#207022=CARTESIAN_POINT('Ctrl Pts',(9.07516390034338,15.2,6.46470087853134));
#207023=CARTESIAN_POINT('Ctrl Pts',(9.07754353145642,15.2,6.46842419401763));
#207024=CARTESIAN_POINT('Ctrl Pts',(9.07992433575292,15.2,6.47216246655567));
#207025=CARTESIAN_POINT('Ctrl Pts',(9.08230513972502,15.2,6.47590073858438));
#207026=CARTESIAN_POINT('Ctrl Pts',(9.08468711627447,15.2,6.47965396804934));
#207027=CARTESIAN_POINT('Ctrl Pts',(9.08707015842082,15.2,6.48342211942823));
#207028=CARTESIAN_POINT('Ctrl Pts',(9.08945320089187,15.2,6.48719027132053));
#207029=CARTESIAN_POINT('Ctrl Pts',(9.09183730800098,15.2,6.49097334369148));
#207030=CARTESIAN_POINT('Ctrl Pts',(9.0942223761866,15.2,6.49477129834389));
#207031=CARTESIAN_POINT('Ctrl Pts',(9.09660744404725,15.2,6.49856925247883));
#207032=CARTESIAN_POINT('Ctrl Pts',(9.09899346924379,15.2,6.50238209023299));
#207033=CARTESIAN_POINT('Ctrl Pts',(9.10138034915968,15.2,6.50620977414077));
#207034=CARTESIAN_POINT('Ctrl Pts',(9.10317050950312,15.2,6.50908053772351));
#207035=CARTESIAN_POINT('Ctrl Pts',(9.1049611482967,15.2,6.51195965227528));
#207036=CARTESIAN_POINT('Ctrl Pts',(9.1067522251404,15.2,6.51484710186274));
#207037=CARTESIAN_POINT('Ctrl Pts',(9.10914032705637,15.2,6.51869703377174));
#207038=CARTESIAN_POINT('Ctrl Pts',(9.11152920296059,15.2,6.52256178386632));
#207039=CARTESIAN_POINT('Ctrl Pts',(9.11391875099831,15.2,6.52644131395562));
#207040=CARTESIAN_POINT('Ctrl Pts',(9.115710912108,15.2,6.52935096165473));
#207041=CARTESIAN_POINT('Ctrl Pts',(9.11750345090304,15.2,6.53226892380484));
#207042=CARTESIAN_POINT('Ctrl Pts',(9.11929632354619,15.2,6.5351951839061));
#207043=CARTESIAN_POINT('Ctrl Pts',(9.12108919618934,15.2,6.53812144400736));
#207044=CARTESIAN_POINT('Ctrl Pts',(9.12288240300749,15.2,6.54105600244977));
#207045=CARTESIAN_POINT('Ctrl Pts',(9.12467590110896,15.2,6.54399884263339));
#207046=CARTESIAN_POINT('Ctrl Pts',(9.12766506472,15.2,6.54890357645096));
#207047=CARTESIAN_POINT('Ctrl Pts',(9.13065503501453,15.2,6.55383131959625));
#207048=CARTESIAN_POINT('Ctrl Pts',(9.13364561717778,15.2,6.55878199442531));
#207049=CARTESIAN_POINT('Ctrl Pts',(9.13543996641054,15.2,6.56175239921482));
#207050=CARTESIAN_POINT('Ctrl Pts',(9.13723453567392,15.2,6.5647310602751));
#207051=CARTESIAN_POINT('Ctrl Pts',(9.13902928131702,15.2,6.56771796183212));
#207052=CARTESIAN_POINT('Ctrl Pts',(9.14142227572519,15.2,6.57170049760323));
#207053=CARTESIAN_POINT('Ctrl Pts',(9.14381558548893,15.2,6.57569768209795));
#207054=CARTESIAN_POINT('Ctrl Pts',(9.14620911000829,15.2,6.57970947798327));
#207055=CARTESIAN_POINT('Ctrl Pts',(9.14800425323474,15.2,6.58271832462396));
#207056=CARTESIAN_POINT('Ctrl Pts',(9.14979951736951,15.2,6.5857353910143));
#207057=CARTESIAN_POINT('Ctrl Pts',(9.15159486105425,15.2,6.58876065969531));
#207058=CARTESIAN_POINT('Ctrl Pts',(9.15398865285136,15.2,6.59279435163639));
#207059=CARTESIAN_POINT('Ctrl Pts',(9.15638258609726,15.2,6.59684262756945));
#207060=CARTESIAN_POINT('Ctrl Pts',(9.15877656134733,15.2,6.60090545010622));
#207061=CARTESIAN_POINT('Ctrl Pts',(9.16057204262179,15.2,6.60395256673202));
#207062=CARTESIAN_POINT('Ctrl Pts',(9.16236754751089,15.2,6.60700786371125));
#207063=CARTESIAN_POINT('Ctrl Pts',(9.16416303565399,15.2,6.61007132735065));
#207064=CARTESIAN_POINT('Ctrl Pts',(9.16595852379709,15.2,6.61313479099006));
#207065=CARTESIAN_POINT('Ctrl Pts',(9.16775399481517,15.2,6.6162064217618));
#207066=CARTESIAN_POINT('Ctrl Pts',(9.16954940704161,15.2,6.61928620148326));
#207067=CARTESIAN_POINT('Ctrl Pts',(9.17134481926806,15.2,6.62236598120472));
#207068=CARTESIAN_POINT('Ctrl Pts',(9.17314017406947,15.2,6.62545391225912));
#207069=CARTESIAN_POINT('Ctrl Pts',(9.17493542929593,15.2,6.62854997639593));
#207070=CARTESIAN_POINT('Ctrl Pts',(9.17732910314862,15.2,6.63267806228663));
#207071=CARTESIAN_POINT('Ctrl Pts',(9.17972260233739,15.2,6.63682060874297));
#207072=CARTESIAN_POINT('Ctrl Pts',(9.18211582891226,15.2,6.64097757858157));
#207073=CARTESIAN_POINT('Ctrl Pts',(9.18391074868036,15.2,6.64409530567733));
#207074=CARTESIAN_POINT('Ctrl Pts',(9.18570551635863,15.2,6.64722114565239));
#207075=CARTESIAN_POINT('Ctrl Pts',(9.18750009155158,15.2,6.65035508271944));
#207076=CARTESIAN_POINT('Ctrl Pts',(9.18929466674451,15.2,6.65348901978649));
#207077=CARTESIAN_POINT('Ctrl Pts',(9.19108904918869,15.2,6.65663105373059));
#207078=CARTESIAN_POINT('Ctrl Pts',(9.19288319846499,15.2,6.65978116875541));
#207079=CARTESIAN_POINT('Ctrl Pts',(9.19467734774129,15.2,6.66293128378023));
#207080=CARTESIAN_POINT('Ctrl Pts',(9.19647126461958,15.2,6.66608947908735));
#207081=CARTESIAN_POINT('Ctrl Pts',(9.19826490976277,15.2,6.66925573967994));
#207082=CARTESIAN_POINT('Ctrl Pts',(9.20065643683758,15.2,6.67347742085352));
#207083=CARTESIAN_POINT('Ctrl Pts',(9.20304747945122,15.2,6.67771343940939));
#207084=CARTESIAN_POINT('Ctrl Pts',(9.20543794597036,15.2,6.6819637578642));
#207085=CARTESIAN_POINT('Ctrl Pts',(9.2078284121638,15.2,6.6862140757399));
#207086=CARTESIAN_POINT('Ctrl Pts',(9.21021830142914,15.2,6.6904786925747));
#207087=CARTESIAN_POINT('Ctrl Pts',(9.21260752168658,15.2,6.69475757260411));
#207088=CARTESIAN_POINT('Ctrl Pts',(9.21559404725254,15.2,6.70010617307812));
#207089=CARTESIAN_POINT('Ctrl Pts',(9.21857952549361,15.2,6.70547705586522));
#207090=CARTESIAN_POINT('Ctrl Pts',(9.2215637793131,15.2,6.71087014794735));
#207091=CARTESIAN_POINT('Ctrl Pts',(9.22335433153973,15.2,6.71410600307905));
#207092=CARTESIAN_POINT('Ctrl Pts',(9.22514444317476,15.2,6.71734985464361));
#207093=CARTESIAN_POINT('Ctrl Pts',(9.22693407685981,15.2,6.72060168527437));
#207094=CARTESIAN_POINT('Ctrl Pts',(9.22872371086996,15.2,6.72385351649587));
#207095=CARTESIAN_POINT('Ctrl Pts',(9.23051286589665,15.2,6.7271133272363));
#207096=CARTESIAN_POINT('Ctrl Pts',(9.23230150436487,15.2,6.73038110096231));
#207097=CARTESIAN_POINT('Ctrl Pts',(9.23468635511427,15.2,6.73473813160759));
#207098=CARTESIAN_POINT('Ctrl Pts',(9.23707028553785,15.2,6.73910932001612));
#207099=CARTESIAN_POINT('Ctrl Pts',(9.239453204465,15.2,6.74349462528861));
#207100=CARTESIAN_POINT('Ctrl Pts',(9.24124039374151,15.2,6.74678360439236));
#207101=CARTESIAN_POINT('Ctrl Pts',(9.2430270137201,15.2,6.75008052497727));
#207102=CARTESIAN_POINT('Ctrl Pts',(9.24481303053026,15.2,6.75338537164817));
#207103=CARTESIAN_POINT('Ctrl Pts',(9.24778972532201,15.2,6.75889344963311));
#207104=CARTESIAN_POINT('Ctrl Pts',(9.25076475131095,15.2,6.76442354774921));
#207105=CARTESIAN_POINT('Ctrl Pts',(9.25373792408882,15.2,6.76997558788695));
#207106=CARTESIAN_POINT('Ctrl Pts',(9.2567110968667,15.2,6.77552762802469));
#207107=CARTESIAN_POINT('Ctrl Pts',(9.25968240391261,15.2,6.78110160259929));
#207108=CARTESIAN_POINT('Ctrl Pts',(9.262651666565,15.2,6.78669743630521));
#207109=CARTESIAN_POINT('Ctrl Pts',(9.26562092921739,15.2,6.79229327001113));
#207110=CARTESIAN_POINT('Ctrl Pts',(9.2685881416477,15.2,6.79791096716016));
#207111=CARTESIAN_POINT('Ctrl Pts',(9.27155330199994,15.2,6.80355049599999));
#207112=CARTESIAN_POINT('Ctrl Pts',(8.56667970899995,12.2,5.85257411499998));
#207113=CARTESIAN_POINT('Ctrl Pts',(8.5680628930964,12.2,5.85370502577855));
#207114=CARTESIAN_POINT('Ctrl Pts',(8.5694869244067,12.2,5.85487627485597));
#207115=CARTESIAN_POINT('Ctrl Pts',(8.5709506523979,12.2,5.85608775314224));
#207116=CARTESIAN_POINT('Ctrl Pts',(8.57242143922536,12.2,5.85730507378917));
#207117=CARTESIAN_POINT('Ctrl Pts',(8.57393230443574,12.2,5.85856301214596));
#207118=CARTESIAN_POINT('Ctrl Pts',(8.57548210843323,12.2,5.85986145286728));
#207119=CARTESIAN_POINT('Ctrl Pts',(8.57703191228994,12.2,5.86115989347067));
#207120=CARTESIAN_POINT('Ctrl Pts',(8.57862065432565,12.2,5.8624988373167));
#207121=CARTESIAN_POINT('Ctrl Pts',(8.58024722826654,12.2,5.86387816976658));
#207122=CARTESIAN_POINT('Ctrl Pts',(8.58187380220742,12.2,5.86525750221645));
#207123=CARTESIAN_POINT('Ctrl Pts',(8.58353820816439,12.2,5.86667722297458));
#207124=CARTESIAN_POINT('Ctrl Pts',(8.58523937135207,12.2,5.86813722032544));
#207125=CARTESIAN_POINT('Ctrl Pts',(8.58694053469429,12.2,5.86959721780893));
#207126=CARTESIAN_POINT('Ctrl Pts',(8.58867845563581,12.2,5.87109748993948));
#207127=CARTESIAN_POINT('Ctrl Pts',(8.59045208798488,12.2,5.87263792444283));
#207128=CARTESIAN_POINT('Ctrl Pts',(8.59252132548382,12.2,5.87443509782017));
#207129=CARTESIAN_POINT('Ctrl Pts',(8.59463917073834,12.2,5.87628693691257));
#207130=CARTESIAN_POINT('Ctrl Pts',(8.59680401336214,12.2,5.87819326040028));
#207131=CARTESIAN_POINT('Ctrl Pts',(8.59865959297066,12.2,5.87982725215201));
#207132=CARTESIAN_POINT('Ctrl Pts',(8.60054970122744,12.2,5.88150127369895));
#207133=CARTESIAN_POINT('Ctrl Pts',(8.60247335675124,12.2,5.88321521321174));
#207134=CARTESIAN_POINT('Ctrl Pts',(8.6043970121003,12.2,5.88492915256886));
#207135=CARTESIAN_POINT('Ctrl Pts',(8.60635421133066,12.2,5.88668300813268));
#207136=CARTESIAN_POINT('Ctrl Pts',(8.60834399976748,12.2,5.88847666749242));
#207137=CARTESIAN_POINT('Ctrl Pts',(8.61033378820429,12.2,5.89027032685214));
#207138=CARTESIAN_POINT('Ctrl Pts',(8.61235616229743,12.2,5.89210379097614));
#207139=CARTESIAN_POINT('Ctrl Pts',(8.61441019188808,12.2,5.89397694365633));
#207140=CARTESIAN_POINT('Ctrl Pts',(8.6164642216653,12.2,5.89585009650669));
#207141=CARTESIAN_POINT('Ctrl Pts',(8.61854990577146,12.2,5.89776294282028));
#207142=CARTESIAN_POINT('Ctrl Pts',(8.62066633380559,12.2,5.89971536542941));
#207143=CARTESIAN_POINT('Ctrl Pts',(8.62278276164747,12.2,5.90166778786119));
#207144=CARTESIAN_POINT('Ctrl Pts',(8.62492993542981,12.2,5.9036597878579));
#207145=CARTESIAN_POINT('Ctrl Pts',(8.627106966352,12.2,5.90569125236913));
#207146=CARTESIAN_POINT('Ctrl Pts',(8.62928399727419,12.2,5.90772271688036));
#207147=CARTESIAN_POINT('Ctrl Pts',(8.63149088542733,12.2,5.90979364605512));
#207148=CARTESIAN_POINT('Ctrl Pts',(8.63372676734483,12.2,5.91190392739341));
#207149=CARTESIAN_POINT('Ctrl Pts',(8.63596264926232,12.2,5.91401420873169));
#207150=CARTESIAN_POINT('Ctrl Pts',(8.63822752414355,12.2,5.91616384011022));
#207151=CARTESIAN_POINT('Ctrl Pts',(8.64052054897496,12.2,5.91835271052801));
#207152=CARTESIAN_POINT('Ctrl Pts',(8.64281357401468,12.2,5.92054158114462));
#207153=CARTESIAN_POINT('Ctrl Pts',(8.64513474718216,12.2,5.92276968904004));
#207154=CARTESIAN_POINT('Ctrl Pts',(8.64748324564467,12.2,5.92503692258198));
#207155=CARTESIAN_POINT('Ctrl Pts',(8.64983174389386,12.2,5.92730415591797));
#207156=CARTESIAN_POINT('Ctrl Pts',(8.65220756771584,12.2,5.92961051408416));
#207157=CARTESIAN_POINT('Ctrl Pts',(8.65460991187741,12.2,5.93195588258059));
#207158=CARTESIAN_POINT('Ctrl Pts',(8.65701225603898,12.2,5.93430125107701));
#207159=CARTESIAN_POINT('Ctrl Pts',(8.65944111983161,12.2,5.93668563184312));
#207160=CARTESIAN_POINT('Ctrl Pts',(8.66189571899069,12.2,5.93910890925246));
#207161=CARTESIAN_POINT('Ctrl Pts',(8.66435031837273,12.2,5.9415321868819));
#207162=CARTESIAN_POINT('Ctrl Pts',(8.66683065253225,12.2,5.94399436288172));
#207163=CARTESIAN_POINT('Ctrl Pts',(8.66933595116988,12.2,5.94649532068638));
#207164=CARTESIAN_POINT('Ctrl Pts',(8.67225879923911,12.2,5.94941310445107));
#207165=CARTESIAN_POINT('Ctrl Pts',(8.67521562943652,12.2,5.95238367869775));
#207166=CARTESIAN_POINT('Ctrl Pts',(8.67820524826226,12.2,5.95540685999247));
#207167=CARTESIAN_POINT('Ctrl Pts',(8.68076777898359,12.2,5.95799815854772));
#207168=CARTESIAN_POINT('Ctrl Pts',(8.68335440181564,12.2,5.96062810723174));
#207169=CARTESIAN_POINT('Ctrl Pts',(8.68596438262558,12.2,5.96329659187885));
#207170=CARTESIAN_POINT('Ctrl Pts',(8.68857436319844,12.2,5.96596507628358));
#207171=CARTESIAN_POINT('Ctrl Pts',(8.69120770284151,12.2,5.96867209749437));
#207172=CARTESIAN_POINT('Ctrl Pts',(8.69386368550703,12.2,5.97141753899034));
#207173=CARTESIAN_POINT('Ctrl Pts',(8.69651966817254,12.2,5.9741629804863));
#207174=CARTESIAN_POINT('Ctrl Pts',(8.69919829322183,12.2,5.97694684462246));
#207175=CARTESIAN_POINT('Ctrl Pts',(8.70189885895555,12.2,5.97976901493398));
#207176=CARTESIAN_POINT('Ctrl Pts',(8.70459942493458,12.2,5.98259118550184));
#207177=CARTESIAN_POINT('Ctrl Pts',(8.70732193266089,12.2,5.98545166274211));
#207178=CARTESIAN_POINT('Ctrl Pts',(8.71006569578205,12.2,5.98835033154709));
#207179=CARTESIAN_POINT('Ctrl Pts',(8.71235216492507,12.2,5.99076588875293));
#207180=CARTESIAN_POINT('Ctrl Pts',(8.71465339369052,12.2,5.99320796962066));
#207181=CARTESIAN_POINT('Ctrl Pts',(8.7169689935528,12.2,5.99567650358115));
#207182=CARTESIAN_POINT('Ctrl Pts',(8.71928459341506,12.2,5.99814503754163));
#207183=CARTESIAN_POINT('Ctrl Pts',(8.72161456367202,12.2,6.00064002790533));
#207184=CARTESIAN_POINT('Ctrl Pts',(8.72395852200651,12.2,6.00316140658807));
#207185=CARTESIAN_POINT('Ctrl Pts',(8.72677127190572,12.2,6.0061870608974));
#207186=CARTESIAN_POINT('Ctrl Pts',(8.72960416329157,12.2,6.00925071275516));
#207187=CARTESIAN_POINT('Ctrl Pts',(8.73245654618878,12.2,6.01235225089412));
#207188=CARTESIAN_POINT('Ctrl Pts',(8.73483353202283,12.2,6.01493686610382));
#207189=CARTESIAN_POINT('Ctrl Pts',(8.7372240554676,12.2,6.01754778784338));
#207190=CARTESIAN_POINT('Ctrl Pts',(8.73962774394052,12.2,6.02018495145588));
#207191=CARTESIAN_POINT('Ctrl Pts',(8.74203143241346,12.2,6.02282211506838));
#207192=CARTESIAN_POINT('Ctrl Pts',(8.74444828873749,12.2,6.02548551968159));
#207193=CARTESIAN_POINT('Ctrl Pts',(8.74687794754034,12.2,6.02817509780391));
#207194=CARTESIAN_POINT('Ctrl Pts',(8.74930760634317,12.2,6.03086467592622));
#207195=CARTESIAN_POINT('Ctrl Pts',(8.75175007054779,12.2,6.03358042787311));
#207196=CARTESIAN_POINT('Ctrl Pts',(8.75420497985435,12.2,6.03632228662523));
#207197=CARTESIAN_POINT('Ctrl Pts',(8.75665988916092,12.2,6.03906414537735));
#207198=CARTESIAN_POINT('Ctrl Pts',(8.75912724439545,12.2,6.04183210994103));
#207199=CARTESIAN_POINT('Ctrl Pts',(8.7616066938409,12.2,6.04462611362372));
#207200=CARTESIAN_POINT('Ctrl Pts',(8.76408614301609,12.2,6.04742011700186));
#207201=CARTESIAN_POINT('Ctrl Pts',(8.76657768737967,12.2,6.05024015992893));
#207202=CARTESIAN_POINT('Ctrl Pts',(8.76908098043915,12.2,6.05308617343601));
#207203=CARTESIAN_POINT('Ctrl Pts',(8.77158427377151,12.2,6.05593218725329));
#207204=CARTESIAN_POINT('Ctrl Pts',(8.7740993143315,12.2,6.05880417218411));
#207205=CARTESIAN_POINT('Ctrl Pts',(8.77662576217779,12.2,6.06170206086255));
#207206=CARTESIAN_POINT('Ctrl Pts',(8.77965749975856,12.2,6.06517952746619));
#207207=CARTESIAN_POINT('Ctrl Pts',(8.78270566421705,12.2,6.06869429467042));
#207208=CARTESIAN_POINT('Ctrl Pts',(8.78576967778803,12.2,6.07224624637696));
#207209=CARTESIAN_POINT('Ctrl Pts',(8.78832302229136,12.2,6.07520620597107));
#207210=CARTESIAN_POINT('Ctrl Pts',(8.79088737165252,12.2,6.07819198621395));
#207211=CARTESIAN_POINT('Ctrl Pts',(8.79346239707007,12.2,6.08120352086885));
#207212=CARTESIAN_POINT('Ctrl Pts',(8.79603742248763,12.2,6.08421505552374));
#207213=CARTESIAN_POINT('Ctrl Pts',(8.79862312544976,12.2,6.08725234545957));
#207214=CARTESIAN_POINT('Ctrl Pts',(8.80121917913115,12.2,6.09031531997557));
#207215=CARTESIAN_POINT('Ctrl Pts',(8.80381523281255,12.2,6.09337829449155));
#207216=CARTESIAN_POINT('Ctrl Pts',(8.80642163805244,12.2,6.09646695510517));
#207217=CARTESIAN_POINT('Ctrl Pts',(8.80903807590049,12.2,6.09958123219062));
#207218=CARTESIAN_POINT('Ctrl Pts',(8.81165451346335,12.2,6.1026955089366));
#207219=CARTESIAN_POINT('Ctrl Pts',(8.81428098302658,12.2,6.10583540448858));
#207220=CARTESIAN_POINT('Ctrl Pts',(8.81691717065511,12.2,6.10900084712756));
#207221=CARTESIAN_POINT('Ctrl Pts',(8.81955335857098,12.2,6.11216629011157));
#207222=CARTESIAN_POINT('Ctrl Pts',(8.82219926320895,12.2,6.11535728324798));
#207223=CARTESIAN_POINT('Ctrl Pts',(8.82485457536094,12.2,6.11857375532921));
#207224=CARTESIAN_POINT('Ctrl Pts',(8.8269788251983,12.2,6.12114693313444));
#207225=CARTESIAN_POINT('Ctrl Pts',(8.82910909550858,12.2,6.12373641928392));
#207226=CARTESIAN_POINT('Ctrl Pts',(8.83124522996804,12.2,6.12634217649336));
#207227=CARTESIAN_POINT('Ctrl Pts',(8.83338136413645,12.2,6.12894793334777));
#207228=CARTESIAN_POINT('Ctrl Pts',(8.83552336201105,12.2,6.13156996253314));
#207229=CARTESIAN_POINT('Ctrl Pts',(8.83767106889044,12.2,6.13420822859357));
#207230=CARTESIAN_POINT('Ctrl Pts',(8.83981877606245,12.2,6.13684649501346));
#207231=CARTESIAN_POINT('Ctrl Pts',(8.84197219170171,12.2,6.1395009982877));
#207232=CARTESIAN_POINT('Ctrl Pts',(8.84413116354159,12.2,6.14217170276659));
#207233=CARTESIAN_POINT('Ctrl Pts',(8.84629013538147,12.2,6.14484240724548));
#207234=CARTESIAN_POINT('Ctrl Pts',(8.84845466336088,12.2,6.14752931335402));
#207235=CARTESIAN_POINT('Ctrl Pts',(8.85062459464638,12.2,6.15023238572522));
#207236=CARTESIAN_POINT('Ctrl Pts',(8.85279452563623,12.2,6.15293545772814));
#207237=CARTESIAN_POINT('Ctrl Pts',(8.85496986128625,12.2,6.15565469528987));
#207238=CARTESIAN_POINT('Ctrl Pts',(8.85715045150677,12.2,6.15839006402306));
#207239=CARTESIAN_POINT('Ctrl Pts',(8.85933104202439,12.2,6.16112543312895));
#207240=CARTESIAN_POINT('Ctrl Pts',(8.86151688553822,12.2,6.16387693239996));
#207241=CARTESIAN_POINT('Ctrl Pts',(8.86370783732481,12.2,6.16664452688576));
#207242=CARTESIAN_POINT('Ctrl Pts',(8.86589878881288,12.2,6.16941212099449));
#207243=CARTESIAN_POINT('Ctrl Pts',(8.86809484621139,12.2,6.17219581145388));
#207244=CARTESIAN_POINT('Ctrl Pts',(8.87029586258671,12.2,6.17499556027953));
#207245=CARTESIAN_POINT('Ctrl Pts',(8.8724968792619,12.2,6.17779530948664));
#207246=CARTESIAN_POINT('Ctrl Pts',(8.87470285595884,12.2,6.18061111846928));
#207247=CARTESIAN_POINT('Ctrl Pts',(8.87691364857909,12.2,6.18344295221093));
#207248=CARTESIAN_POINT('Ctrl Pts',(8.87912444089812,12.2,6.18627478556674));
#207249=CARTESIAN_POINT('Ctrl Pts',(8.88134004649194,12.2,6.18912264098444));
#207250=CARTESIAN_POINT('Ctrl Pts',(8.88356032481013,12.2,6.19198648574929));
#207251=CARTESIAN_POINT('Ctrl Pts',(8.88578060343083,12.2,6.19485033090434));
#207252=CARTESIAN_POINT('Ctrl Pts',(8.88800555441322,12.2,6.19773016469463));
#207253=CARTESIAN_POINT('Ctrl Pts',(8.8902350339239,12.2,6.20062595052014));
#207254=CARTESIAN_POINT('Ctrl Pts',(8.89246451313081,12.2,6.2035217359511));
#207255=CARTESIAN_POINT('Ctrl Pts',(8.8946985230356,12.2,6.20643347485579));
#207256=CARTESIAN_POINT('Ctrl Pts',(8.89693692274181,12.2,6.20936112981685));
#207257=CARTESIAN_POINT('Ctrl Pts',(8.899175322753,12.2,6.2122887851768));
#207258=CARTESIAN_POINT('Ctrl Pts',(8.90141811167205,12.2,6.21523235789914));
#207259=CARTESIAN_POINT('Ctrl Pts',(8.90366515168366,12.2,6.21819181045034));
#207260=CARTESIAN_POINT('Ctrl Pts',(8.90591219138912,12.2,6.22115126259831));
#207261=CARTESIAN_POINT('Ctrl Pts',(8.90816348194653,12.2,6.22412659708759));
#207262=CARTESIAN_POINT('Ctrl Pts',(8.91041888637284,12.2,6.22711777578587));
#207263=CARTESIAN_POINT('Ctrl Pts',(8.91267429110643,12.2,6.23010895489169));
#207264=CARTESIAN_POINT('Ctrl Pts',(8.91493380991504,12.2,6.23311597829012));
#207265=CARTESIAN_POINT('Ctrl Pts',(8.91719730599314,12.2,6.23613881146865));
#207266=CARTESIAN_POINT('Ctrl Pts',(8.91946080176284,12.2,6.23916164423531));
#207267=CARTESIAN_POINT('Ctrl Pts',(8.92172827502853,12.2,6.24220028622684));
#207268=CARTESIAN_POINT('Ctrl Pts',(8.92399959212024,12.2,6.24525470147553));
#207269=CARTESIAN_POINT('Ctrl Pts',(8.92627090952141,12.2,6.2483091171404));
#207270=CARTESIAN_POINT('Ctrl Pts',(8.92854607080627,12.2,6.25137930404005));
#207271=CARTESIAN_POINT('Ctrl Pts',(8.9308249415416,12.2,6.25446522970826));
#207272=CARTESIAN_POINT('Ctrl Pts',(8.93310381227694,12.2,6.25755115537647));
#207273=CARTESIAN_POINT('Ctrl Pts',(8.93538639374878,12.2,6.26065281755481));
#207274=CARTESIAN_POINT('Ctrl Pts',(8.93767255387372,12.2,6.26377018072629));
#207275=CARTESIAN_POINT('Ctrl Pts',(8.94053025356266,12.2,6.26766688405352));
#207276=CARTESIAN_POINT('Ctrl Pts',(8.94339354409894,12.2,6.2715881192048));
#207277=CARTESIAN_POINT('Ctrl Pts',(8.94626217288305,12.2,6.27553381800883));
#207278=CARTESIAN_POINT('Ctrl Pts',(8.94855707628554,12.2,6.27869037756814));
#207279=CARTESIAN_POINT('Ctrl Pts',(8.95085539533558,12.2,6.2818625912456));
#207280=CARTESIAN_POINT('Ctrl Pts',(8.9531570020166,12.2,6.28505042447492));
#207281=CARTESIAN_POINT('Ctrl Pts',(8.95545860869761,12.2,6.28823825770425));
#207282=CARTESIAN_POINT('Ctrl Pts',(8.95776350095119,12.2,6.29144171089366));
#207283=CARTESIAN_POINT('Ctrl Pts',(8.96007155441063,12.2,6.29466074729291));
#207284=CARTESIAN_POINT('Ctrl Pts',(8.9623796075556,12.2,6.29787978325357));
#207285=CARTESIAN_POINT('Ctrl Pts',(8.9646908211576,12.2,6.3011144013626));
#207286=CARTESIAN_POINT('Ctrl Pts',(8.96700506825669,12.2,6.30436456672271));
#207287=CARTESIAN_POINT('Ctrl Pts',(8.9693193156711,12.2,6.30761473252566));
#207288=CARTESIAN_POINT('Ctrl Pts',(8.97163659534144,12.2,6.31088044563656));
#207289=CARTESIAN_POINT('Ctrl Pts',(8.97395678491262,12.2,6.31416166876141));
#207290=CARTESIAN_POINT('Ctrl Pts',(8.97627697416767,12.2,6.3174428914392));
#207291=CARTESIAN_POINT('Ctrl Pts',(8.97860007285292,12.2,6.32073962247608));
#207292=CARTESIAN_POINT('Ctrl Pts',(8.98092595605148,12.2,6.3240518297043));
#207293=CARTESIAN_POINT('Ctrl Pts',(8.98383331028737,12.2,6.32819208907803));
#207294=CARTESIAN_POINT('Ctrl Pts',(8.98674501732613,12.2,6.33235652534406));
#207295=CARTESIAN_POINT('Ctrl Pts',(8.98966083732594,12.2,6.33654506742614));
#207296=CARTESIAN_POINT('Ctrl Pts',(8.9919934934529,12.2,6.33989590127442));
#207297=CARTESIAN_POINT('Ctrl Pts',(8.9943287804142,12.2,6.34326216385));
#207298=CARTESIAN_POINT('Ctrl Pts',(8.99666658004752,12.2,6.34664381848238));
#207299=CARTESIAN_POINT('Ctrl Pts',(8.99900437936231,12.2,6.35002547265401));
#207300=CARTESIAN_POINT('Ctrl Pts',(9.00134469007511,12.2,6.3534225174483));
#207301=CARTESIAN_POINT('Ctrl Pts',(9.00368739205011,12.2,6.35683491744611));
#207302=CARTESIAN_POINT('Ctrl Pts',(9.00661576975825,12.2,6.36110041779207));
#207303=CARTESIAN_POINT('Ctrl Pts',(9.00954788422482,12.2,6.365389910897));
#207304=CARTESIAN_POINT('Ctrl Pts',(9.01248350505796,12.2,6.36970332374297));
#207305=CARTESIAN_POINT('Ctrl Pts',(9.01483200185247,12.2,6.37315405420781));
#207306=CARTESIAN_POINT('Ctrl Pts',(9.0171827412343,12.2,6.37662009405408));
#207307=CARTESIAN_POINT('Ctrl Pts',(9.01953560759136,12.2,6.38010140603017));
#207308=CARTESIAN_POINT('Ctrl Pts',(9.02188847362786,12.2,6.38358271753192));
#207309=CARTESIAN_POINT('Ctrl Pts',(9.02424346421952,12.2,6.38707930086493));
#207310=CARTESIAN_POINT('Ctrl Pts',(9.02660046674894,12.2,6.39059112018799));
#207311=CARTESIAN_POINT('Ctrl Pts',(9.02895746959952,12.2,6.39410293998952));
#207312=CARTESIAN_POINT('Ctrl Pts',(9.03131648285582,12.2,6.39762999524281));
#207313=CARTESIAN_POINT('Ctrl Pts',(9.03367739048463,12.2,6.40117224904799));
#207314=CARTESIAN_POINT('Ctrl Pts',(9.03603829779177,12.2,6.40471450237054));
#207315=CARTESIAN_POINT('Ctrl Pts',(9.03840109957382,12.2,6.40827195414927));
#207316=CARTESIAN_POINT('Ctrl Pts',(9.04076568366516,12.2,6.41184456775659));
#207317=CARTESIAN_POINT('Ctrl Pts',(9.04372141402097,12.2,6.41631033513083));
#207318=CARTESIAN_POINT('Ctrl Pts',(9.04667992812311,12.2,6.42079979267283));
#207319=CARTESIAN_POINT('Ctrl Pts',(9.0496410033313,12.2,6.42531286871324));
#207320=CARTESIAN_POINT('Ctrl Pts',(9.05200986362695,12.2,6.42892332974235));
#207321=CARTESIAN_POINT('Ctrl Pts',(9.05438036454227,12.2,6.43254890660384));
#207322=CARTESIAN_POINT('Ctrl Pts',(9.0567523942272,12.2,6.43618956058103));
#207323=CARTESIAN_POINT('Ctrl Pts',(9.05912442358895,12.2,6.43983021406218));
#207324=CARTESIAN_POINT('Ctrl Pts',(9.06149798078373,12.2,6.4434859459937));
#207325=CARTESIAN_POINT('Ctrl Pts',(9.06387295743032,12.2,6.44715672070901));
#207326=CARTESIAN_POINT('Ctrl Pts',(9.0662479344005,12.2,6.45082749592447));
#207327=CARTESIAN_POINT('Ctrl Pts',(9.06862432759243,12.2,6.45451331117771));
#207328=CARTESIAN_POINT('Ctrl Pts',(9.07100202994432,12.2,6.4582141316026));
#207329=CARTESIAN_POINT('Ctrl Pts',(9.0739741577222,12.2,6.46284015688159));
#207330=CARTESIAN_POINT('Ctrl Pts',(9.07694833054449,12.2,6.46748962613779));
#207331=CARTESIAN_POINT('Ctrl Pts',(9.07992433575292,12.2,6.47216246655567));
#207332=CARTESIAN_POINT('Ctrl Pts',(9.08230513972502,12.2,6.47590073858438));
#207333=CARTESIAN_POINT('Ctrl Pts',(9.08468711627447,12.2,6.47965396804934));
#207334=CARTESIAN_POINT('Ctrl Pts',(9.08707015842082,12.2,6.48342211942823));
#207335=CARTESIAN_POINT('Ctrl Pts',(9.08885744011176,12.2,6.48624823309075));
#207336=CARTESIAN_POINT('Ctrl Pts',(9.0906453206918,12.2,6.48908273891798));
#207337=CARTESIAN_POINT('Ctrl Pts',(9.09243375633506,12.2,6.49192562239685));
#207338=CARTESIAN_POINT('Ctrl Pts',(9.09422219230321,12.2,6.49476850639217));
#207339=CARTESIAN_POINT('Ctrl Pts',(9.09601118379659,12.2,6.49761976660661));
#207340=CARTESIAN_POINT('Ctrl Pts',(9.09780068339006,12.2,6.50047938869001));
#207341=CARTESIAN_POINT('Ctrl Pts',(9.09959018265844,12.2,6.50333901025391));
#207342=CARTESIAN_POINT('Ctrl Pts',(9.1013801934268,12.2,6.50620699270071));
#207343=CARTESIAN_POINT('Ctrl Pts',(9.10317066769511,12.2,6.50908332130526));
#207344=CARTESIAN_POINT('Ctrl Pts',(9.10555796661112,12.2,6.51291842593714));
#207345=CARTESIAN_POINT('Ctrl Pts',(9.10794609514599,12.2,6.51676836660781));
#207346=CARTESIAN_POINT('Ctrl Pts',(9.11033494540331,12.2,6.52063310737255));
#207347=CARTESIAN_POINT('Ctrl Pts',(9.11212658317767,12.2,6.52353166307774));
#207348=CARTESIAN_POINT('Ctrl Pts',(9.1139186280077,12.2,6.52643854310479));
#207349=CARTESIAN_POINT('Ctrl Pts',(9.11571103610919,12.2,6.52935373212275));
#207350=CARTESIAN_POINT('Ctrl Pts',(9.11750344453632,12.2,6.5322689216703));
#207351=CARTESIAN_POINT('Ctrl Pts',(9.11929621568019,12.2,6.53519241956185));
#207352=CARTESIAN_POINT('Ctrl Pts',(9.12108930664917,12.2,6.53812421065574));
#207353=CARTESIAN_POINT('Ctrl Pts',(9.12288239729241,12.2,6.54105600121702));
#207354=CARTESIAN_POINT('Ctrl Pts',(9.1246758080606,12.2,6.54399608367784));
#207355=CARTESIAN_POINT('Ctrl Pts',(9.12646949520379,12.2,6.54694444427977));
#207356=CARTESIAN_POINT('Ctrl Pts',(9.12826318234698,12.2,6.54989280488171));
#207357=CARTESIAN_POINT('Ctrl Pts',(9.13005714557528,12.2,6.55284944364684));
#207358=CARTESIAN_POINT('Ctrl Pts',(9.13185134322657,12.2,6.55581434276096));
#207359=CARTESIAN_POINT('Ctrl Pts',(9.13364554087788,12.2,6.55877924187508));
#207360=CARTESIAN_POINT('Ctrl Pts',(9.13543997338869,12.2,6.56175240214204));
#207361=CARTESIAN_POINT('Ctrl Pts',(9.13723459653998,12.2,6.56473380825556));
#207362=CARTESIAN_POINT('Ctrl Pts',(9.13902921969127,12.2,6.56771521436908));
#207363=CARTESIAN_POINT('Ctrl Pts',(9.14082403305286,12.2,6.5707048662996));
#207364=CARTESIAN_POINT('Ctrl Pts',(9.14261899623763,12.2,6.5737027473983));
#207365=CARTESIAN_POINT('Ctrl Pts',(9.14441395942239,12.2,6.57670062849698));
#207366=CARTESIAN_POINT('Ctrl Pts',(9.14620907240715,12.2,6.57970673878677));
#207367=CARTESIAN_POINT('Ctrl Pts',(9.14800429159192,12.2,6.5827210633428));
#207368=CARTESIAN_POINT('Ctrl Pts',(9.14979951110281,12.2,6.58573538844643));
#207369=CARTESIAN_POINT('Ctrl Pts',(9.15159483791374,12.2,6.58875792675239));
#207370=CARTESIAN_POINT('Ctrl Pts',(9.15339023038301,12.2,6.59178866336064));
#207371=CARTESIAN_POINT('Ctrl Pts',(9.15518562252611,12.2,6.5948193994183));
#207372=CARTESIAN_POINT('Ctrl Pts',(9.15698108007287,12.2,6.59785833348042));
#207373=CARTESIAN_POINT('Ctrl Pts',(9.15877656134733,12.2,6.60090545010622));
#207374=CARTESIAN_POINT('Ctrl Pts',(9.16057204262179,12.2,6.60395256673202));
#207375=CARTESIAN_POINT('Ctrl Pts',(9.16236754751089,12.2,6.60700786371125));
#207376=CARTESIAN_POINT('Ctrl Pts',(9.16416303565399,12.2,6.61007132735065));
#207377=CARTESIAN_POINT('Ctrl Pts',(9.16595852379709,12.2,6.61313479099006));
#207378=CARTESIAN_POINT('Ctrl Pts',(9.16775399481517,12.2,6.6162064217618));
#207379=CARTESIAN_POINT('Ctrl Pts',(9.16954940704161,12.2,6.61928620148326));
#207380=CARTESIAN_POINT('Ctrl Pts',(9.17134481926806,12.2,6.62236598120472));
#207381=CARTESIAN_POINT('Ctrl Pts',(9.17314017406947,12.2,6.62545391225912));
#207382=CARTESIAN_POINT('Ctrl Pts',(9.17493542929593,12.2,6.62854997639593));
#207383=CARTESIAN_POINT('Ctrl Pts',(9.17673068452238,12.2,6.63164604053273));
#207384=CARTESIAN_POINT('Ctrl Pts',(9.17852584127383,12.2,6.63475023873564));
#207385=CARTESIAN_POINT('Ctrl Pts',(9.18032085891697,12.2,6.63786255532979));
#207386=CARTESIAN_POINT('Ctrl Pts',(9.1821158768862,12.2,6.64097487248934));
#207387=CARTESIAN_POINT('Ctrl Pts',(9.18391075438039,12.2,6.64409530824285));
#207388=CARTESIAN_POINT('Ctrl Pts',(9.18570545384953,12.2,6.64722384594863));
#207389=CARTESIAN_POINT('Ctrl Pts',(9.18750015299263,12.2,6.65035238308606));
#207390=CARTESIAN_POINT('Ctrl Pts',(9.18929467312268,12.2,6.65348902278134));
#207391=CARTESIAN_POINT('Ctrl Pts',(9.1910889733971,12.2,6.6566337485751));
#207392=CARTESIAN_POINT('Ctrl Pts',(9.19348137365433,12.2,6.6608267161097));
#207393=CARTESIAN_POINT('Ctrl Pts',(9.1958733830138,12.2,6.66503405908155));
#207394=CARTESIAN_POINT('Ctrl Pts',(9.19826490976277,12.2,6.66925573967994));
#207395=CARTESIAN_POINT('Ctrl Pts',(9.20005855490596,12.2,6.67242200027252));
#207396=CARTESIAN_POINT('Ctrl Pts',(9.20185192720749,12.2,6.67559632588957));
#207397=CARTESIAN_POINT('Ctrl Pts',(9.20364498885073,12.2,6.67877870002285));
#207398=CARTESIAN_POINT('Ctrl Pts',(9.20603573792553,12.2,6.68302186591932));
#207399=CARTESIAN_POINT('Ctrl Pts',(9.20842593351326,12.2,6.68727934141724));
#207400=CARTESIAN_POINT('Ctrl Pts',(9.21081548270991,12.2,6.69155108800285));
#207401=CARTESIAN_POINT('Ctrl Pts',(9.21260764444461,12.2,6.69475489765105));
#207402=CARTESIAN_POINT('Ctrl Pts',(9.21439944307193,12.2,6.6979667358494));
#207403=CARTESIAN_POINT('Ctrl Pts',(9.21619083876499,12.2,6.70118658445535));
#207404=CARTESIAN_POINT('Ctrl Pts',(9.21798223445805,12.2,6.7044064330613));
#207405=CARTESIAN_POINT('Ctrl Pts',(9.21977322708646,12.2,6.70763429281564));
#207406=CARTESIAN_POINT('Ctrl Pts',(9.2215637793131,12.2,6.71087014794735));
#207407=CARTESIAN_POINT('Ctrl Pts',(9.22335433153973,12.2,6.71410600307905));
#207408=CARTESIAN_POINT('Ctrl Pts',(9.22514444317476,12.2,6.71734985464361));
#207409=CARTESIAN_POINT('Ctrl Pts',(9.22693407685981,12.2,6.72060168527437));
#207410=CARTESIAN_POINT('Ctrl Pts',(9.22872371086996,12.2,6.72385351649587));
#207411=CARTESIAN_POINT('Ctrl Pts',(9.23051286589665,12.2,6.7271133272363));
#207412=CARTESIAN_POINT('Ctrl Pts',(9.23230150436487,12.2,6.73038110096231));
#207413=CARTESIAN_POINT('Ctrl Pts',(9.23468635511427,12.2,6.73473813160759));
#207414=CARTESIAN_POINT('Ctrl Pts',(9.23707028553785,12.2,6.73910932001612));
#207415=CARTESIAN_POINT('Ctrl Pts',(9.239453204465,12.2,6.74349462528861));
#207416=CARTESIAN_POINT('Ctrl Pts',(9.24124039374151,12.2,6.74678360439236));
#207417=CARTESIAN_POINT('Ctrl Pts',(9.2430270137201,12.2,6.75008052497727));
#207418=CARTESIAN_POINT('Ctrl Pts',(9.24481303053026,12.2,6.75338537164817));
#207419=CARTESIAN_POINT('Ctrl Pts',(9.24659904734042,12.2,6.75669021831906));
#207420=CARTESIAN_POINT('Ctrl Pts',(9.24838446219229,12.2,6.76000299186442));
#207421=CARTESIAN_POINT('Ctrl Pts',(9.25016923787753,12.2,6.7633236759927));
#207422=CARTESIAN_POINT('Ctrl Pts',(9.25195401388701,12.2,6.76664436072422));
#207423=CARTESIAN_POINT('Ctrl Pts',(9.25373815067964,12.2,6.76997295755798));
#207424=CARTESIAN_POINT('Ctrl Pts',(9.25552160360541,12.2,6.77330944475229));
#207425=CARTESIAN_POINT('Ctrl Pts',(9.25789954029976,12.2,6.77775809333448));
#207426=CARTESIAN_POINT('Ctrl Pts',(9.26027625663727,12.2,6.78222076970644));
#207427=CARTESIAN_POINT('Ctrl Pts',(9.262651666565,12.2,6.78669743630522));
#207428=CARTESIAN_POINT('Ctrl Pts',(9.26562092921739,12.2,6.79229327001113));
#207429=CARTESIAN_POINT('Ctrl Pts',(9.2685881416477,12.2,6.79791096716016));
#207430=CARTESIAN_POINT('Ctrl Pts',(9.27155330199994,12.2,6.80355049599999));
#207431=CARTESIAN_POINT('Origin',(-5.66257110645729E-14,15.2,-1.77635683940025E-14));
#207432=CARTESIAN_POINT('',(7.6465751230011,15.2,7.01216898633437));
#207433=CARTESIAN_POINT('',(7.6465751230011,12.2,7.01216898633437));
#207434=CARTESIAN_POINT('',(7.64657512299994,15.2,7.01216898599998));
#207435=CARTESIAN_POINT('Origin',(-5.66257110645729E-14,12.2,-1.77635683940025E-14));
#207436=CARTESIAN_POINT('Origin',(-5.66257110645729E-14,15.2,-1.77635683940025E-14));
#207437=CARTESIAN_POINT('Origin',(-5.66257110645729E-14,15.2,-1.77635683940025E-14));
#207438=CARTESIAN_POINT('',(8.20893606999994,15.2,8.05377977099998));
#207439=CARTESIAN_POINT('',(7.93573928265107,15.2,8.32310290898369));
#207440=CARTESIAN_POINT('Origin',(-5.66257110645729E-14,15.2,-1.77635683940025E-14));
#207441=CARTESIAN_POINT('',(7.93573928265107,12.2,8.32310290898369));
#207442=CARTESIAN_POINT('',(7.93573928299995,15.2,8.32310290899999));
#207443=CARTESIAN_POINT('',(8.20893606999994,12.2,8.05377977099998));
#207444=CARTESIAN_POINT('Origin',(-5.66257110645729E-14,12.2,-1.77635683940025E-14));
#207445=CARTESIAN_POINT('',(8.20893606999994,15.2,8.05377977099998));
#207446=CARTESIAN_POINT('Ctrl Pts',(7.64657512299994,15.2,7.01216898699998));
#207447=CARTESIAN_POINT('Ctrl Pts',(7.64657512299994,11.6,7.01216898699998));
#207448=CARTESIAN_POINT('Ctrl Pts',(7.64669302599994,15.2,7.01229743699999));
#207449=CARTESIAN_POINT('Ctrl Pts',(7.64669302599994,11.6,7.01229743699999));
#207450=CARTESIAN_POINT('Ctrl Pts',(7.64693288599994,15.2,7.01255888399999));
#207451=CARTESIAN_POINT('Ctrl Pts',(7.64693288599994,11.6,7.01255888399999));
#207452=CARTESIAN_POINT('Ctrl Pts',(7.64729613399994,15.2,7.01295521799998));
#207453=CARTESIAN_POINT('Ctrl Pts',(7.64729613399994,11.6,7.01295521799998));
#207454=CARTESIAN_POINT('Ctrl Pts',(7.64778506499994,15.2,7.01348947999998));
#207455=CARTESIAN_POINT('Ctrl Pts',(7.64778506499994,11.6,7.01348947999998));
#207456=CARTESIAN_POINT('Ctrl Pts',(7.64840281599994,15.2,7.01416585899998));
#207457=CARTESIAN_POINT('Ctrl Pts',(7.64840281599994,11.6,7.01416585899998));
#207458=CARTESIAN_POINT('Ctrl Pts',(7.64902988999994,15.2,7.01485383099998));
#207459=CARTESIAN_POINT('Ctrl Pts',(7.64902988999994,11.6,7.01485383099998));
#207460=CARTESIAN_POINT('Ctrl Pts',(7.64966267399994,15.2,7.01554946999998));
#207461=CARTESIAN_POINT('Ctrl Pts',(7.64966267399994,11.6,7.01554946999998));
#207462=CARTESIAN_POINT('Ctrl Pts',(7.65030113899994,15.2,7.01625276699998));
#207463=CARTESIAN_POINT('Ctrl Pts',(7.65030113899994,11.6,7.01625276699998));
#207464=CARTESIAN_POINT('Ctrl Pts',(7.65094525299994,15.2,7.01696371599999));
#207465=CARTESIAN_POINT('Ctrl Pts',(7.65094525299994,11.6,7.01696371599999));
#207466=CARTESIAN_POINT('Ctrl Pts',(7.65159498499994,15.2,7.01768230799999));
#207467=CARTESIAN_POINT('Ctrl Pts',(7.65159498499994,11.6,7.01768230799999));
#207468=CARTESIAN_POINT('Ctrl Pts',(7.65225030199994,15.2,7.01840853699998));
#207469=CARTESIAN_POINT('Ctrl Pts',(7.65225030199994,11.6,7.01840853699998));
#207470=CARTESIAN_POINT('Ctrl Pts',(7.65291117499994,15.2,7.01914239299998));
#207471=CARTESIAN_POINT('Ctrl Pts',(7.65291117499994,11.6,7.01914239299998));
#207472=CARTESIAN_POINT('Ctrl Pts',(7.65357757199994,15.2,7.01988386999999));
#207473=CARTESIAN_POINT('Ctrl Pts',(7.65357757199994,11.6,7.01988386999999));
#207474=CARTESIAN_POINT('Ctrl Pts',(7.65424946499994,15.2,7.02063296099999));
#207475=CARTESIAN_POINT('Ctrl Pts',(7.65424946499994,11.6,7.02063296099999));
#207476=CARTESIAN_POINT('Ctrl Pts',(7.65492681899994,15.2,7.02138965599998));
#207477=CARTESIAN_POINT('Ctrl Pts',(7.65492681899994,11.6,7.02138965599998));
#207478=CARTESIAN_POINT('Ctrl Pts',(7.65560960699994,15.2,7.02215394999998));
#207479=CARTESIAN_POINT('Ctrl Pts',(7.65560960699994,11.6,7.02215394999998));
#207480=CARTESIAN_POINT('Ctrl Pts',(7.65629779899994,15.2,7.02292583299998));
#207481=CARTESIAN_POINT('Ctrl Pts',(7.65629779899994,11.6,7.02292583299998));
#207482=CARTESIAN_POINT('Ctrl Pts',(7.65699136199994,15.2,7.02370529999998));
#207483=CARTESIAN_POINT('Ctrl Pts',(7.65699136199994,11.6,7.02370529999998));
#207484=CARTESIAN_POINT('Ctrl Pts',(7.65769026799994,15.2,7.02449234199998));
#207485=CARTESIAN_POINT('Ctrl Pts',(7.65769026799994,11.6,7.02449234199998));
#207486=CARTESIAN_POINT('Ctrl Pts',(7.65839448899994,15.2,7.02528695099998));
#207487=CARTESIAN_POINT('Ctrl Pts',(7.65839448899994,11.6,7.02528695099998));
#207488=CARTESIAN_POINT('Ctrl Pts',(7.65910399199995,15.2,7.02608912199998));
#207489=CARTESIAN_POINT('Ctrl Pts',(7.65910399199995,11.6,7.02608912199998));
#207490=CARTESIAN_POINT('Ctrl Pts',(7.65981874999994,15.2,7.02689884499998));
#207491=CARTESIAN_POINT('Ctrl Pts',(7.65981874999994,11.6,7.02689884499998));
#207492=CARTESIAN_POINT('Ctrl Pts',(7.66053873199994,15.2,7.02771611299998));
#207493=CARTESIAN_POINT('Ctrl Pts',(7.66053873199994,11.6,7.02771611299998));
#207494=CARTESIAN_POINT('Ctrl Pts',(7.66126390999994,15.2,7.02854091999999));
#207495=CARTESIAN_POINT('Ctrl Pts',(7.66126390999994,11.6,7.02854091999999));
#207496=CARTESIAN_POINT('Ctrl Pts',(7.66199425499994,15.2,7.02937325699998));
#207497=CARTESIAN_POINT('Ctrl Pts',(7.66199425499994,11.6,7.02937325699998));
#207498=CARTESIAN_POINT('Ctrl Pts',(7.66272973699994,15.2,7.03021311899998));
#207499=CARTESIAN_POINT('Ctrl Pts',(7.66272973699994,11.6,7.03021311899998));
#207500=CARTESIAN_POINT('Ctrl Pts',(7.66347032799994,15.2,7.03106049599998));
#207501=CARTESIAN_POINT('Ctrl Pts',(7.66347032799994,11.6,7.03106049599998));
#207502=CARTESIAN_POINT('Ctrl Pts',(7.66421599899994,15.2,7.03191538099999));
#207503=CARTESIAN_POINT('Ctrl Pts',(7.66421599899994,11.6,7.03191538099999));
#207504=CARTESIAN_POINT('Ctrl Pts',(7.66496672199994,15.2,7.03277776899998));
#207505=CARTESIAN_POINT('Ctrl Pts',(7.66496672199994,11.6,7.03277776899998));
#207506=CARTESIAN_POINT('Ctrl Pts',(7.66572246899995,15.2,7.03364765099998));
#207507=CARTESIAN_POINT('Ctrl Pts',(7.66572246899995,11.6,7.03364765099998));
#207508=CARTESIAN_POINT('Ctrl Pts',(7.66648321099995,15.2,7.03452502099999));
#207509=CARTESIAN_POINT('Ctrl Pts',(7.66648321099995,11.6,7.03452502099999));
#207510=CARTESIAN_POINT('Ctrl Pts',(7.66724891999995,15.2,7.03540986999998));
#207511=CARTESIAN_POINT('Ctrl Pts',(7.66724891999995,11.6,7.03540986999998));
#207512=CARTESIAN_POINT('Ctrl Pts',(7.66801956799994,15.2,7.03630219099999));
#207513=CARTESIAN_POINT('Ctrl Pts',(7.66801956799994,11.6,7.03630219099999));
#207514=CARTESIAN_POINT('Ctrl Pts',(7.66879512799994,15.2,7.03720197899998));
#207515=CARTESIAN_POINT('Ctrl Pts',(7.66879512799994,11.6,7.03720197899998));
#207516=CARTESIAN_POINT('Ctrl Pts',(7.66957557199994,15.2,7.03810922399998));
#207517=CARTESIAN_POINT('Ctrl Pts',(7.66957557199994,11.6,7.03810922399998));
#207518=CARTESIAN_POINT('Ctrl Pts',(7.67036087199994,15.2,7.03902391999998));
#207519=CARTESIAN_POINT('Ctrl Pts',(7.67036087199994,11.6,7.03902391999998));
#207520=CARTESIAN_POINT('Ctrl Pts',(7.67115099999994,15.2,7.03994606099998));
#207521=CARTESIAN_POINT('Ctrl Pts',(7.67115099999994,11.6,7.03994606099998));
#207522=CARTESIAN_POINT('Ctrl Pts',(7.67194592999994,15.2,7.04087563799998));
#207523=CARTESIAN_POINT('Ctrl Pts',(7.67194592999994,11.6,7.04087563799998));
#207524=CARTESIAN_POINT('Ctrl Pts',(7.67274563399994,15.2,7.04181264599999));
#207525=CARTESIAN_POINT('Ctrl Pts',(7.67274563399994,11.6,7.04181264599999));
#207526=CARTESIAN_POINT('Ctrl Pts',(7.67355008499995,15.2,7.04275707599999));
#207527=CARTESIAN_POINT('Ctrl Pts',(7.67355008499995,11.6,7.04275707599999));
#207528=CARTESIAN_POINT('Ctrl Pts',(7.67435925699994,15.2,7.04370892199999));
#207529=CARTESIAN_POINT('Ctrl Pts',(7.67435925699994,11.6,7.04370892199999));
#207530=CARTESIAN_POINT('Ctrl Pts',(7.67517312199994,15.2,7.04466817699998));
#207531=CARTESIAN_POINT('Ctrl Pts',(7.67517312199994,11.6,7.04466817699998));
#207532=CARTESIAN_POINT('Ctrl Pts',(7.67599165499995,15.2,7.04563483399999));
#207533=CARTESIAN_POINT('Ctrl Pts',(7.67599165499995,11.6,7.04563483399999));
#207534=CARTESIAN_POINT('Ctrl Pts',(7.67681482699994,15.2,7.04660888499999));
#207535=CARTESIAN_POINT('Ctrl Pts',(7.67681482699994,11.6,7.04660888499999));
#207536=CARTESIAN_POINT('Ctrl Pts',(7.67764261399994,15.2,7.04759032499998));
#207537=CARTESIAN_POINT('Ctrl Pts',(7.67764261399994,11.6,7.04759032499998));
#207538=CARTESIAN_POINT('Ctrl Pts',(7.67847498699994,15.2,7.04857914399999));
#207539=CARTESIAN_POINT('Ctrl Pts',(7.67847498699994,11.6,7.04857914399999));
#207540=CARTESIAN_POINT('Ctrl Pts',(7.67931192299995,15.2,7.04957533799998));
#207541=CARTESIAN_POINT('Ctrl Pts',(7.67931192299995,11.6,7.04957533799998));
#207542=CARTESIAN_POINT('Ctrl Pts',(7.68015339199994,15.2,7.05057889899999));
#207543=CARTESIAN_POINT('Ctrl Pts',(7.68015339199994,11.6,7.05057889899999));
#207544=CARTESIAN_POINT('Ctrl Pts',(7.68099937299994,15.2,7.05158981999999));
#207545=CARTESIAN_POINT('Ctrl Pts',(7.68099937299994,11.6,7.05158981999999));
#207546=CARTESIAN_POINT('Ctrl Pts',(7.68184983599994,15.2,7.05260809399999));
#207547=CARTESIAN_POINT('Ctrl Pts',(7.68184983599994,11.6,7.05260809399999));
#207548=CARTESIAN_POINT('Ctrl Pts',(7.68270475699994,15.2,7.05363371399999));
#207549=CARTESIAN_POINT('Ctrl Pts',(7.68270475699994,11.6,7.05363371399999));
#207550=CARTESIAN_POINT('Ctrl Pts',(7.68356410999995,15.2,7.05466667399998));
#207551=CARTESIAN_POINT('Ctrl Pts',(7.68356410999995,11.6,7.05466667399998));
#207552=CARTESIAN_POINT('Ctrl Pts',(7.68442787099994,15.2,7.05570696599998));
#207553=CARTESIAN_POINT('Ctrl Pts',(7.68442787099994,11.6,7.05570696599998));
#207554=CARTESIAN_POINT('Ctrl Pts',(7.68529601099995,15.2,7.05675458499999));
#207555=CARTESIAN_POINT('Ctrl Pts',(7.68529601099995,11.6,7.05675458499999));
#207556=CARTESIAN_POINT('Ctrl Pts',(7.68616850899994,15.2,7.05780952199999));
#207557=CARTESIAN_POINT('Ctrl Pts',(7.68616850899994,11.6,7.05780952199999));
#207558=CARTESIAN_POINT('Ctrl Pts',(7.68704533799994,15.2,7.05887176999998));
#207559=CARTESIAN_POINT('Ctrl Pts',(7.68704533799994,11.6,7.05887176999998));
#207560=CARTESIAN_POINT('Ctrl Pts',(7.68792647099994,15.2,7.05994132599999));
#207561=CARTESIAN_POINT('Ctrl Pts',(7.68792647099994,11.6,7.05994132599999));
#207562=CARTESIAN_POINT('Ctrl Pts',(7.68881188699994,15.2,7.06101817899999));
#207563=CARTESIAN_POINT('Ctrl Pts',(7.68881188699994,11.6,7.06101817899999));
#207564=CARTESIAN_POINT('Ctrl Pts',(7.68970155799994,15.2,7.06210232399999));
#207565=CARTESIAN_POINT('Ctrl Pts',(7.68970155799994,11.6,7.06210232399999));
#207566=CARTESIAN_POINT('Ctrl Pts',(7.69059545999994,15.2,7.06319375399998));
#207567=CARTESIAN_POINT('Ctrl Pts',(7.69059545999994,11.6,7.06319375399998));
#207568=CARTESIAN_POINT('Ctrl Pts',(7.69149356799995,15.2,7.06429246399999));
#207569=CARTESIAN_POINT('Ctrl Pts',(7.69149356799995,11.6,7.06429246399999));
#207570=CARTESIAN_POINT('Ctrl Pts',(7.69239585999994,15.2,7.06539844399998));
#207571=CARTESIAN_POINT('Ctrl Pts',(7.69239585999994,11.6,7.06539844399998));
#207572=CARTESIAN_POINT('Ctrl Pts',(7.69330230899994,15.2,7.06651168999999));
#207573=CARTESIAN_POINT('Ctrl Pts',(7.69330230899994,11.6,7.06651168999999));
#207574=CARTESIAN_POINT('Ctrl Pts',(7.69421289099995,15.2,7.06763219399999));
#207575=CARTESIAN_POINT('Ctrl Pts',(7.69421289099995,11.6,7.06763219399999));
#207576=CARTESIAN_POINT('Ctrl Pts',(7.69512758299994,15.2,7.06875994999999));
#207577=CARTESIAN_POINT('Ctrl Pts',(7.69512758299994,11.6,7.06875994999999));
#207578=CARTESIAN_POINT('Ctrl Pts',(7.69604635999994,15.2,7.06989494999998));
#207579=CARTESIAN_POINT('Ctrl Pts',(7.69604635999994,11.6,7.06989494999998));
#207580=CARTESIAN_POINT('Ctrl Pts',(7.69696919799994,15.2,7.07103718999999));
#207581=CARTESIAN_POINT('Ctrl Pts',(7.69696919799994,11.6,7.07103718999999));
#207582=CARTESIAN_POINT('Ctrl Pts',(7.69789607399994,15.2,7.07218666199999));
#207583=CARTESIAN_POINT('Ctrl Pts',(7.69789607399994,11.6,7.07218666199999));
#207584=CARTESIAN_POINT('Ctrl Pts',(7.69882696299995,15.2,7.07334335899999));
#207585=CARTESIAN_POINT('Ctrl Pts',(7.69882696299995,11.6,7.07334335899999));
#207586=CARTESIAN_POINT('Ctrl Pts',(7.69976184199994,15.2,7.07450727399999));
#207587=CARTESIAN_POINT('Ctrl Pts',(7.69976184199994,11.6,7.07450727399999));
#207588=CARTESIAN_POINT('Ctrl Pts',(7.70070068699994,15.2,7.07567840199999));
#207589=CARTESIAN_POINT('Ctrl Pts',(7.70070068699994,11.6,7.07567840199999));
#207590=CARTESIAN_POINT('Ctrl Pts',(7.70164347599994,15.2,7.07685673499999));
#207591=CARTESIAN_POINT('Ctrl Pts',(7.70164347599994,11.6,7.07685673499999));
#207592=CARTESIAN_POINT('Ctrl Pts',(7.70259018299994,15.2,7.07804226699999));
#207593=CARTESIAN_POINT('Ctrl Pts',(7.70259018299994,11.6,7.07804226699999));
#207594=CARTESIAN_POINT('Ctrl Pts',(7.70354078799994,15.2,7.07923499199998));
#207595=CARTESIAN_POINT('Ctrl Pts',(7.70354078799994,11.6,7.07923499199998));
#207596=CARTESIAN_POINT('Ctrl Pts',(7.70449526399994,15.2,7.08043490399999));
#207597=CARTESIAN_POINT('Ctrl Pts',(7.70449526399994,11.6,7.08043490399999));
#207598=CARTESIAN_POINT('Ctrl Pts',(7.70545359099994,15.2,7.08164199399998));
#207599=CARTESIAN_POINT('Ctrl Pts',(7.70545359099994,11.6,7.08164199399998));
#207600=CARTESIAN_POINT('Ctrl Pts',(7.70641574499995,15.2,7.08285625699999));
#207601=CARTESIAN_POINT('Ctrl Pts',(7.70641574499995,11.6,7.08285625699999));
#207602=CARTESIAN_POINT('Ctrl Pts',(7.70738170299994,15.2,7.08407768799999));
#207603=CARTESIAN_POINT('Ctrl Pts',(7.70738170299994,11.6,7.08407768799999));
#207604=CARTESIAN_POINT('Ctrl Pts',(7.70835144199994,15.2,7.08530627799998));
#207605=CARTESIAN_POINT('Ctrl Pts',(7.70835144199994,11.6,7.08530627799998));
#207606=CARTESIAN_POINT('Ctrl Pts',(7.70932493799994,15.2,7.08654202199998));
#207607=CARTESIAN_POINT('Ctrl Pts',(7.70932493799994,11.6,7.08654202199998));
#207608=CARTESIAN_POINT('Ctrl Pts',(7.71030217199994,15.2,7.08778491299999));
#207609=CARTESIAN_POINT('Ctrl Pts',(7.71030217199994,11.6,7.08778491299999));
#207610=CARTESIAN_POINT('Ctrl Pts',(7.71128311799994,15.2,7.08903494499998));
#207611=CARTESIAN_POINT('Ctrl Pts',(7.71128311799994,11.6,7.08903494499998));
#207612=CARTESIAN_POINT('Ctrl Pts',(7.71226775599994,15.2,7.09029211199999));
#207613=CARTESIAN_POINT('Ctrl Pts',(7.71226775599994,11.6,7.09029211199999));
#207614=CARTESIAN_POINT('Ctrl Pts',(7.71325606199994,15.2,7.09155640599998));
#207615=CARTESIAN_POINT('Ctrl Pts',(7.71325606199994,11.6,7.09155640599998));
#207616=CARTESIAN_POINT('Ctrl Pts',(7.71424801399994,15.2,7.09282782199999));
#207617=CARTESIAN_POINT('Ctrl Pts',(7.71424801399994,11.6,7.09282782199999));
#207618=CARTESIAN_POINT('Ctrl Pts',(7.71524358999994,15.2,7.09410635399998));
#207619=CARTESIAN_POINT('Ctrl Pts',(7.71524358999994,11.6,7.09410635399998));
#207620=CARTESIAN_POINT('Ctrl Pts',(7.71624276799994,15.2,7.09539199399998));
#207621=CARTESIAN_POINT('Ctrl Pts',(7.71624276799994,11.6,7.09539199399998));
#207622=CARTESIAN_POINT('Ctrl Pts',(7.71724552699995,15.2,7.09668473599999));
#207623=CARTESIAN_POINT('Ctrl Pts',(7.71724552699995,11.6,7.09668473599999));
#207624=CARTESIAN_POINT('Ctrl Pts',(7.71825184399995,15.2,7.09798457599998));
#207625=CARTESIAN_POINT('Ctrl Pts',(7.71825184399995,11.6,7.09798457599998));
#207626=CARTESIAN_POINT('Ctrl Pts',(7.71926169599995,15.2,7.09929150499998));
#207627=CARTESIAN_POINT('Ctrl Pts',(7.71926169599995,11.6,7.09929150499998));
#207628=CARTESIAN_POINT('Ctrl Pts',(7.72027506399994,15.2,7.10060551799998));
#207629=CARTESIAN_POINT('Ctrl Pts',(7.72027506399994,11.6,7.10060551799998));
#207630=CARTESIAN_POINT('Ctrl Pts',(7.72129192499994,15.2,7.10192660699998));
#207631=CARTESIAN_POINT('Ctrl Pts',(7.72129192499994,11.6,7.10192660699998));
#207632=CARTESIAN_POINT('Ctrl Pts',(7.72231225799994,15.2,7.10325476899998));
#207633=CARTESIAN_POINT('Ctrl Pts',(7.72231225799994,11.6,7.10325476899998));
#207634=CARTESIAN_POINT('Ctrl Pts',(7.72333603899994,15.2,7.10458999399999));
#207635=CARTESIAN_POINT('Ctrl Pts',(7.72333603899994,11.6,7.10458999399999));
#207636=CARTESIAN_POINT('Ctrl Pts',(7.72436324999994,15.2,7.10593227899999));
#207637=CARTESIAN_POINT('Ctrl Pts',(7.72436324999994,11.6,7.10593227899999));
#207638=CARTESIAN_POINT('Ctrl Pts',(7.72539386899994,15.2,7.10728161499999));
#207639=CARTESIAN_POINT('Ctrl Pts',(7.72539386899994,11.6,7.10728161499999));
#207640=CARTESIAN_POINT('Ctrl Pts',(7.72642787299994,15.2,7.10863799699998));
#207641=CARTESIAN_POINT('Ctrl Pts',(7.72642787299994,11.6,7.10863799699998));
#207642=CARTESIAN_POINT('Ctrl Pts',(7.72746524199994,15.2,7.11000141999998));
#207643=CARTESIAN_POINT('Ctrl Pts',(7.72746524199994,11.6,7.11000141999998));
#207644=CARTESIAN_POINT('Ctrl Pts',(7.72850595599994,15.2,7.11137187599999));
#207645=CARTESIAN_POINT('Ctrl Pts',(7.72850595599994,11.6,7.11137187599999));
#207646=CARTESIAN_POINT('Ctrl Pts',(7.72954999199994,15.2,7.11274935899999));
#207647=CARTESIAN_POINT('Ctrl Pts',(7.72954999199994,11.6,7.11274935899999));
#207648=CARTESIAN_POINT('Ctrl Pts',(7.73059733099994,15.2,7.11413386299999));
#207649=CARTESIAN_POINT('Ctrl Pts',(7.73059733099994,11.6,7.11413386299999));
#207650=CARTESIAN_POINT('Ctrl Pts',(7.73164795099994,15.2,7.11552538199999));
#207651=CARTESIAN_POINT('Ctrl Pts',(7.73164795099994,11.6,7.11552538199999));
#207652=CARTESIAN_POINT('Ctrl Pts',(7.73270183099994,15.2,7.11692390999998));
#207653=CARTESIAN_POINT('Ctrl Pts',(7.73270183099994,11.6,7.11692390999998));
#207654=CARTESIAN_POINT('Ctrl Pts',(7.73375895099995,15.2,7.11832944099999));
#207655=CARTESIAN_POINT('Ctrl Pts',(7.73375895099995,11.6,7.11832944099999));
#207656=CARTESIAN_POINT('Ctrl Pts',(7.73481929099994,15.2,7.11974196899998));
#207657=CARTESIAN_POINT('Ctrl Pts',(7.73481929099994,11.6,7.11974196899998));
#207658=CARTESIAN_POINT('Ctrl Pts',(7.73588282999994,15.2,7.12116148599998));
#207659=CARTESIAN_POINT('Ctrl Pts',(7.73588282999994,11.6,7.12116148599998));
#207660=CARTESIAN_POINT('Ctrl Pts',(7.73694954799995,15.2,7.12258798699998));
#207661=CARTESIAN_POINT('Ctrl Pts',(7.73694954799995,11.6,7.12258798699998));
#207662=CARTESIAN_POINT('Ctrl Pts',(7.73801942299994,15.2,7.12402146799998));
#207663=CARTESIAN_POINT('Ctrl Pts',(7.73801942299994,11.6,7.12402146799998));
#207664=CARTESIAN_POINT('Ctrl Pts',(7.73909243699994,15.2,7.12546191899998));
#207665=CARTESIAN_POINT('Ctrl Pts',(7.73909243699994,11.6,7.12546191899998));
#207666=CARTESIAN_POINT('Ctrl Pts',(7.74016856799994,15.2,7.12690933699999));
#207667=CARTESIAN_POINT('Ctrl Pts',(7.74016856799994,11.6,7.12690933699999));
#207668=CARTESIAN_POINT('Ctrl Pts',(7.74124779699994,15.2,7.12836371399998));
#207669=CARTESIAN_POINT('Ctrl Pts',(7.74124779699994,11.6,7.12836371399998));
#207670=CARTESIAN_POINT('Ctrl Pts',(7.74233010399994,15.2,7.12982504499998));
#207671=CARTESIAN_POINT('Ctrl Pts',(7.74233010399994,11.6,7.12982504499998));
#207672=CARTESIAN_POINT('Ctrl Pts',(7.74341546799994,15.2,7.13129332399999));
#207673=CARTESIAN_POINT('Ctrl Pts',(7.74341546799994,11.6,7.13129332399999));
#207674=CARTESIAN_POINT('Ctrl Pts',(7.74450387099994,15.2,7.13276854399999));
#207675=CARTESIAN_POINT('Ctrl Pts',(7.74450387099994,11.6,7.13276854399999));
#207676=CARTESIAN_POINT('Ctrl Pts',(7.74559529099994,15.2,7.13425069899999));
#207677=CARTESIAN_POINT('Ctrl Pts',(7.74559529099994,11.6,7.13425069899999));
#207678=CARTESIAN_POINT('Ctrl Pts',(7.74668970999994,15.2,7.13573978499999));
#207679=CARTESIAN_POINT('Ctrl Pts',(7.74668970999994,11.6,7.13573978499999));
#207680=CARTESIAN_POINT('Ctrl Pts',(7.74778710799994,15.2,7.13723579299998));
#207681=CARTESIAN_POINT('Ctrl Pts',(7.74778710799994,11.6,7.13723579299998));
#207682=CARTESIAN_POINT('Ctrl Pts',(7.74888746499995,15.2,7.13873871999999));
#207683=CARTESIAN_POINT('Ctrl Pts',(7.74888746499995,11.6,7.13873871999999));
#207684=CARTESIAN_POINT('Ctrl Pts',(7.74999076099995,15.2,7.14024855699999));
#207685=CARTESIAN_POINT('Ctrl Pts',(7.74999076099995,11.6,7.14024855699999));
#207686=CARTESIAN_POINT('Ctrl Pts',(7.75109697799994,15.2,7.14176529899999));
#207687=CARTESIAN_POINT('Ctrl Pts',(7.75109697799994,11.6,7.14176529899999));
#207688=CARTESIAN_POINT('Ctrl Pts',(7.75220609499994,15.2,7.14328894099998));
#207689=CARTESIAN_POINT('Ctrl Pts',(7.75220609499994,11.6,7.14328894099998));
#207690=CARTESIAN_POINT('Ctrl Pts',(7.75331809499994,15.2,7.14481947699999));
#207691=CARTESIAN_POINT('Ctrl Pts',(7.75331809499994,11.6,7.14481947699999));
#207692=CARTESIAN_POINT('Ctrl Pts',(7.75443295699994,15.2,7.14635689999999));
#207693=CARTESIAN_POINT('Ctrl Pts',(7.75443295699994,11.6,7.14635689999999));
#207694=CARTESIAN_POINT('Ctrl Pts',(7.75555066199995,15.2,7.14790120399999));
#207695=CARTESIAN_POINT('Ctrl Pts',(7.75555066199995,11.6,7.14790120399999));
#207696=CARTESIAN_POINT('Ctrl Pts',(7.75667119099994,15.2,7.14945238399999));
#207697=CARTESIAN_POINT('Ctrl Pts',(7.75667119099994,11.6,7.14945238399999));
#207698=CARTESIAN_POINT('Ctrl Pts',(7.75779452599994,15.2,7.15101043399999));
#207699=CARTESIAN_POINT('Ctrl Pts',(7.75779452599994,11.6,7.15101043399999));
#207700=CARTESIAN_POINT('Ctrl Pts',(7.75892064599994,15.2,7.15257534699998));
#207701=CARTESIAN_POINT('Ctrl Pts',(7.75892064599994,11.6,7.15257534699998));
#207702=CARTESIAN_POINT('Ctrl Pts',(7.76004953399994,15.2,7.15414711799998));
#207703=CARTESIAN_POINT('Ctrl Pts',(7.76004953399994,11.6,7.15414711799998));
#207704=CARTESIAN_POINT('Ctrl Pts',(7.76118117099994,15.2,7.15572573999999));
#207705=CARTESIAN_POINT('Ctrl Pts',(7.76118117099994,11.6,7.15572573999999));
#207706=CARTESIAN_POINT('Ctrl Pts',(7.76231553799994,15.2,7.15731120699999));
#207707=CARTESIAN_POINT('Ctrl Pts',(7.76231553799994,11.6,7.15731120699999));
#207708=CARTESIAN_POINT('Ctrl Pts',(7.76345261599995,15.2,7.15890351599998));
#207709=CARTESIAN_POINT('Ctrl Pts',(7.76345261599995,11.6,7.15890351599998));
#207710=CARTESIAN_POINT('Ctrl Pts',(7.76459238699994,15.2,7.16050265899998));
#207711=CARTESIAN_POINT('Ctrl Pts',(7.76459238699994,11.6,7.16050265899998));
#207712=CARTESIAN_POINT('Ctrl Pts',(7.76573483199994,15.2,7.16210862899998));
#207713=CARTESIAN_POINT('Ctrl Pts',(7.76573483199994,11.6,7.16210862899998));
#207714=CARTESIAN_POINT('Ctrl Pts',(7.76687993199995,15.2,7.16372142099999));
#207715=CARTESIAN_POINT('Ctrl Pts',(7.76687993199995,11.6,7.16372142099999));
#207716=CARTESIAN_POINT('Ctrl Pts',(7.76802766899995,15.2,7.16534102999999));
#207717=CARTESIAN_POINT('Ctrl Pts',(7.76802766899995,11.6,7.16534102999999));
#207718=CARTESIAN_POINT('Ctrl Pts',(7.76917802599994,15.2,7.16696744899998));
#207719=CARTESIAN_POINT('Ctrl Pts',(7.76917802599994,11.6,7.16696744899998));
#207720=CARTESIAN_POINT('Ctrl Pts',(7.77033098399994,15.2,7.16860067399999));
#207721=CARTESIAN_POINT('Ctrl Pts',(7.77033098399994,11.6,7.16860067399999));
#207722=CARTESIAN_POINT('Ctrl Pts',(7.77148652399994,15.2,7.17024069699999));
#207723=CARTESIAN_POINT('Ctrl Pts',(7.77148652399994,11.6,7.17024069699999));
#207724=CARTESIAN_POINT('Ctrl Pts',(7.77264462799995,15.2,7.17188751199998));
#207725=CARTESIAN_POINT('Ctrl Pts',(7.77264462799995,11.6,7.17188751199998));
#207726=CARTESIAN_POINT('Ctrl Pts',(7.77380527899994,15.2,7.17354111599998));
#207727=CARTESIAN_POINT('Ctrl Pts',(7.77380527899994,11.6,7.17354111599998));
#207728=CARTESIAN_POINT('Ctrl Pts',(7.77496845899995,15.2,7.17520149999999));
#207729=CARTESIAN_POINT('Ctrl Pts',(7.77496845899995,11.6,7.17520149999999));
#207730=CARTESIAN_POINT('Ctrl Pts',(7.77613414799994,15.2,7.17686865999998));
#207731=CARTESIAN_POINT('Ctrl Pts',(7.77613414799994,11.6,7.17686865999998));
#207732=CARTESIAN_POINT('Ctrl Pts',(7.77730232999994,15.2,7.17854258899998));
#207733=CARTESIAN_POINT('Ctrl Pts',(7.77730232999994,11.6,7.17854258899998));
#207734=CARTESIAN_POINT('Ctrl Pts',(7.77847298599994,15.2,7.18022328399999));
#207735=CARTESIAN_POINT('Ctrl Pts',(7.77847298599994,11.6,7.18022328399999));
#207736=CARTESIAN_POINT('Ctrl Pts',(7.77964609999994,15.2,7.18191073499998));
#207737=CARTESIAN_POINT('Ctrl Pts',(7.77964609999994,11.6,7.18191073499998));
#207738=CARTESIAN_POINT('Ctrl Pts',(7.78082165299995,15.2,7.18360493899999));
#207739=CARTESIAN_POINT('Ctrl Pts',(7.78082165299995,11.6,7.18360493899999));
#207740=CARTESIAN_POINT('Ctrl Pts',(7.78199962799994,15.2,7.18530588799998));
#207741=CARTESIAN_POINT('Ctrl Pts',(7.78199962799994,11.6,7.18530588799998));
#207742=CARTESIAN_POINT('Ctrl Pts',(7.78318000599994,15.2,7.18701357999999));
#207743=CARTESIAN_POINT('Ctrl Pts',(7.78318000599994,11.6,7.18701357999999));
#207744=CARTESIAN_POINT('Ctrl Pts',(7.78436277199994,15.2,7.18872800599998));
#207745=CARTESIAN_POINT('Ctrl Pts',(7.78436277199994,11.6,7.18872800599998));
#207746=CARTESIAN_POINT('Ctrl Pts',(7.78554790599994,15.2,7.19044916099998));
#207747=CARTESIAN_POINT('Ctrl Pts',(7.78554790599994,11.6,7.19044916099998));
#207748=CARTESIAN_POINT('Ctrl Pts',(7.78673539199994,15.2,7.19217703999998));
#207749=CARTESIAN_POINT('Ctrl Pts',(7.78673539199994,11.6,7.19217703999998));
#207750=CARTESIAN_POINT('Ctrl Pts',(7.78792521299994,15.2,7.19391163699999));
#207751=CARTESIAN_POINT('Ctrl Pts',(7.78792521299994,11.6,7.19391163699999));
#207752=CARTESIAN_POINT('Ctrl Pts',(7.78911734999994,15.2,7.19565294599998));
#207753=CARTESIAN_POINT('Ctrl Pts',(7.78911734999994,11.6,7.19565294599998));
#207754=CARTESIAN_POINT('Ctrl Pts',(7.79031178799995,15.2,7.19740096099999));
#207755=CARTESIAN_POINT('Ctrl Pts',(7.79031178799995,11.6,7.19740096099999));
#207756=CARTESIAN_POINT('Ctrl Pts',(7.79150850799994,15.2,7.19915567599998));
#207757=CARTESIAN_POINT('Ctrl Pts',(7.79150850799994,11.6,7.19915567599998));
#207758=CARTESIAN_POINT('Ctrl Pts',(7.79270749399994,15.2,7.20091708699999));
#207759=CARTESIAN_POINT('Ctrl Pts',(7.79270749399994,11.6,7.20091708699999));
#207760=CARTESIAN_POINT('Ctrl Pts',(7.79390872899994,15.2,7.20268518699999));
#207761=CARTESIAN_POINT('Ctrl Pts',(7.79390872899994,11.6,7.20268518699999));
#207762=CARTESIAN_POINT('Ctrl Pts',(7.79511219599994,15.2,7.20445996999998));
#207763=CARTESIAN_POINT('Ctrl Pts',(7.79511219599994,11.6,7.20445996999998));
#207764=CARTESIAN_POINT('Ctrl Pts',(7.79631787699994,15.2,7.20624143099998));
#207765=CARTESIAN_POINT('Ctrl Pts',(7.79631787699994,11.6,7.20624143099998));
#207766=CARTESIAN_POINT('Ctrl Pts',(7.79752575599994,15.2,7.20802956399999));
#207767=CARTESIAN_POINT('Ctrl Pts',(7.79752575599994,11.6,7.20802956399999));
#207768=CARTESIAN_POINT('Ctrl Pts',(7.79873581599994,15.2,7.20982436299998));
#207769=CARTESIAN_POINT('Ctrl Pts',(7.79873581599994,11.6,7.20982436299998));
#207770=CARTESIAN_POINT('Ctrl Pts',(7.79994804099994,15.2,7.21162582399998));
#207771=CARTESIAN_POINT('Ctrl Pts',(7.79994804099994,11.6,7.21162582399998));
#207772=CARTESIAN_POINT('Ctrl Pts',(7.80116241299995,15.2,7.21343393899998));
#207773=CARTESIAN_POINT('Ctrl Pts',(7.80116241299995,11.6,7.21343393899998));
#207774=CARTESIAN_POINT('Ctrl Pts',(7.80237891699994,15.2,7.21524870399998));
#207775=CARTESIAN_POINT('Ctrl Pts',(7.80237891699994,11.6,7.21524870399998));
#207776=CARTESIAN_POINT('Ctrl Pts',(7.80359753599994,15.2,7.21707011199998));
#207777=CARTESIAN_POINT('Ctrl Pts',(7.80359753599994,11.6,7.21707011199998));
#207778=CARTESIAN_POINT('Ctrl Pts',(7.80481825099994,15.2,7.21889815899999));
#207779=CARTESIAN_POINT('Ctrl Pts',(7.80481825099994,11.6,7.21889815899999));
#207780=CARTESIAN_POINT('Ctrl Pts',(7.80604104899994,15.2,7.22073283799999));
#207781=CARTESIAN_POINT('Ctrl Pts',(7.80604104899994,11.6,7.22073283799999));
#207782=CARTESIAN_POINT('Ctrl Pts',(7.80726591199994,15.2,7.22257414399999));
#207783=CARTESIAN_POINT('Ctrl Pts',(7.80726591199994,11.6,7.22257414399999));
#207784=CARTESIAN_POINT('Ctrl Pts',(7.80849282299994,15.2,7.22442207199999));
#207785=CARTESIAN_POINT('Ctrl Pts',(7.80849282299994,11.6,7.22442207199999));
#207786=CARTESIAN_POINT('Ctrl Pts',(7.80972176699994,15.2,7.22627661499998));
#207787=CARTESIAN_POINT('Ctrl Pts',(7.80972176699994,11.6,7.22627661499998));
#207788=CARTESIAN_POINT('Ctrl Pts',(7.81095272699995,15.2,7.22813776799998));
#207789=CARTESIAN_POINT('Ctrl Pts',(7.81095272699995,11.6,7.22813776799998));
#207790=CARTESIAN_POINT('Ctrl Pts',(7.81218568699995,15.2,7.23000552499999));
#207791=CARTESIAN_POINT('Ctrl Pts',(7.81218568699995,11.6,7.23000552499999));
#207792=CARTESIAN_POINT('Ctrl Pts',(7.81342063099994,15.2,7.23187988099999));
#207793=CARTESIAN_POINT('Ctrl Pts',(7.81342063099994,11.6,7.23187988099999));
#207794=CARTESIAN_POINT('Ctrl Pts',(7.81465754299994,15.2,7.23376083099998));
#207795=CARTESIAN_POINT('Ctrl Pts',(7.81465754299994,11.6,7.23376083099998));
#207796=CARTESIAN_POINT('Ctrl Pts',(7.81589640599995,15.2,7.23564836699998));
#207797=CARTESIAN_POINT('Ctrl Pts',(7.81589640599995,11.6,7.23564836699998));
#207798=CARTESIAN_POINT('Ctrl Pts',(7.81713720499994,15.2,7.23754248699999));
#207799=CARTESIAN_POINT('Ctrl Pts',(7.81713720499994,11.6,7.23754248699999));
#207800=CARTESIAN_POINT('Ctrl Pts',(7.81837992399995,15.2,7.23944318299999));
#207801=CARTESIAN_POINT('Ctrl Pts',(7.81837992399995,11.6,7.23944318299999));
#207802=CARTESIAN_POINT('Ctrl Pts',(7.81962454699995,15.2,7.24135044899998));
#207803=CARTESIAN_POINT('Ctrl Pts',(7.81962454699995,11.6,7.24135044899998));
#207804=CARTESIAN_POINT('Ctrl Pts',(7.82087105799994,15.2,7.24326428099998));
#207805=CARTESIAN_POINT('Ctrl Pts',(7.82087105799994,11.6,7.24326428099998));
#207806=CARTESIAN_POINT('Ctrl Pts',(7.82211944199994,15.2,7.24518467399999));
#207807=CARTESIAN_POINT('Ctrl Pts',(7.82211944199994,11.6,7.24518467399999));
#207808=CARTESIAN_POINT('Ctrl Pts',(7.82336968099994,15.2,7.24711161999998));
#207809=CARTESIAN_POINT('Ctrl Pts',(7.82336968099994,11.6,7.24711161999998));
#207810=CARTESIAN_POINT('Ctrl Pts',(7.82462176299994,15.2,7.24904511499999));
#207811=CARTESIAN_POINT('Ctrl Pts',(7.82462176299994,11.6,7.24904511499999));
#207812=CARTESIAN_POINT('Ctrl Pts',(7.82587566799994,15.2,7.25098515199999));
#207813=CARTESIAN_POINT('Ctrl Pts',(7.82587566799994,11.6,7.25098515199999));
#207814=CARTESIAN_POINT('Ctrl Pts',(7.82713138399994,15.2,7.25293172799999));
#207815=CARTESIAN_POINT('Ctrl Pts',(7.82713138399994,11.6,7.25293172799999));
#207816=CARTESIAN_POINT('Ctrl Pts',(7.82838889399994,15.2,7.25488483599998));
#207817=CARTESIAN_POINT('Ctrl Pts',(7.82838889399994,11.6,7.25488483599998));
#207818=CARTESIAN_POINT('Ctrl Pts',(7.82964818299994,15.2,7.25684447099999));
#207819=CARTESIAN_POINT('Ctrl Pts',(7.82964818299994,11.6,7.25684447099999));
#207820=CARTESIAN_POINT('Ctrl Pts',(7.83090923499994,15.2,7.25881062599999));
#207821=CARTESIAN_POINT('Ctrl Pts',(7.83090923499994,11.6,7.25881062599999));
#207822=CARTESIAN_POINT('Ctrl Pts',(7.83217203599994,15.2,7.26078329699998));
#207823=CARTESIAN_POINT('Ctrl Pts',(7.83217203599994,11.6,7.26078329699998));
#207824=CARTESIAN_POINT('Ctrl Pts',(7.83343656799994,15.2,7.26276247899998));
#207825=CARTESIAN_POINT('Ctrl Pts',(7.83343656799994,11.6,7.26276247899998));
#207826=CARTESIAN_POINT('Ctrl Pts',(7.83470281799994,15.2,7.26474816499999));
#207827=CARTESIAN_POINT('Ctrl Pts',(7.83470281799994,11.6,7.26474816499999));
#207828=CARTESIAN_POINT('Ctrl Pts',(7.83597076999994,15.2,7.26674034999998));
#207829=CARTESIAN_POINT('Ctrl Pts',(7.83597076999994,11.6,7.26674034999998));
#207830=CARTESIAN_POINT('Ctrl Pts',(7.83724040899994,15.2,7.26873902899998));
#207831=CARTESIAN_POINT('Ctrl Pts',(7.83724040899994,11.6,7.26873902899998));
#207832=CARTESIAN_POINT('Ctrl Pts',(7.83851171999994,15.2,7.27074419599998));
#207833=CARTESIAN_POINT('Ctrl Pts',(7.83851171999994,11.6,7.27074419599998));
#207834=CARTESIAN_POINT('Ctrl Pts',(7.83978468599994,15.2,7.27275584499999));
#207835=CARTESIAN_POINT('Ctrl Pts',(7.83978468599994,11.6,7.27275584499999));
#207836=CARTESIAN_POINT('Ctrl Pts',(7.84105929599995,15.2,7.27477397199999));
#207837=CARTESIAN_POINT('Ctrl Pts',(7.84105929599995,11.6,7.27477397199999));
#207838=CARTESIAN_POINT('Ctrl Pts',(7.84233553099994,15.2,7.27679857099999));
#207839=CARTESIAN_POINT('Ctrl Pts',(7.84233553099994,11.6,7.27679857099999));
#207840=CARTESIAN_POINT('Ctrl Pts',(7.84361337799995,15.2,7.27882963499999));
#207841=CARTESIAN_POINT('Ctrl Pts',(7.84361337799995,11.6,7.27882963499999));
#207842=CARTESIAN_POINT('Ctrl Pts',(7.84489282199995,15.2,7.28086716099998));
#207843=CARTESIAN_POINT('Ctrl Pts',(7.84489282199995,11.6,7.28086716099998));
#207844=CARTESIAN_POINT('Ctrl Pts',(7.84617384799994,15.2,7.28291114199998));
#207845=CARTESIAN_POINT('Ctrl Pts',(7.84617384799994,11.6,7.28291114199998));
#207846=CARTESIAN_POINT('Ctrl Pts',(7.84745644099995,15.2,7.28496157299999));
#207847=CARTESIAN_POINT('Ctrl Pts',(7.84745644099995,11.6,7.28496157299999));
#207848=CARTESIAN_POINT('Ctrl Pts',(7.84874058699994,15.2,7.28701844899999));
#207849=CARTESIAN_POINT('Ctrl Pts',(7.84874058699994,11.6,7.28701844899999));
#207850=CARTESIAN_POINT('Ctrl Pts',(7.85002626999994,15.2,7.28908176299999));
#207851=CARTESIAN_POINT('Ctrl Pts',(7.85002626999994,11.6,7.28908176299999));
#207852=CARTESIAN_POINT('Ctrl Pts',(7.85131347599994,15.2,7.29115151199998));
#207853=CARTESIAN_POINT('Ctrl Pts',(7.85131347599994,11.6,7.29115151199998));
#207854=CARTESIAN_POINT('Ctrl Pts',(7.85260218999994,15.2,7.29322768799998));
#207855=CARTESIAN_POINT('Ctrl Pts',(7.85260218999994,11.6,7.29322768799998));
#207856=CARTESIAN_POINT('Ctrl Pts',(7.85389239799994,15.2,7.29531028699999));
#207857=CARTESIAN_POINT('Ctrl Pts',(7.85389239799994,11.6,7.29531028699999));
#207858=CARTESIAN_POINT('Ctrl Pts',(7.85518408499994,15.2,7.29739930399998));
#207859=CARTESIAN_POINT('Ctrl Pts',(7.85518408499994,11.6,7.29739930399998));
#207860=CARTESIAN_POINT('Ctrl Pts',(7.85647723799995,15.2,7.29949473199999));
#207861=CARTESIAN_POINT('Ctrl Pts',(7.85647723799995,11.6,7.29949473199999));
#207862=CARTESIAN_POINT('Ctrl Pts',(7.85777184099994,15.2,7.30159656799999));
#207863=CARTESIAN_POINT('Ctrl Pts',(7.85777184099994,11.6,7.30159656799999));
#207864=CARTESIAN_POINT('Ctrl Pts',(7.85906787899994,15.2,7.30370480499998));
#207865=CARTESIAN_POINT('Ctrl Pts',(7.85906787899994,11.6,7.30370480499998));
#207866=CARTESIAN_POINT('Ctrl Pts',(7.86036533899995,15.2,7.30581943799999));
#207867=CARTESIAN_POINT('Ctrl Pts',(7.86036533899995,11.6,7.30581943799999));
#207868=CARTESIAN_POINT('Ctrl Pts',(7.86166420599994,15.2,7.30794045999998));
#207869=CARTESIAN_POINT('Ctrl Pts',(7.86166420599994,11.6,7.30794045999998));
#207870=CARTESIAN_POINT('Ctrl Pts',(7.86296446599994,15.2,7.31006786799998));
#207871=CARTESIAN_POINT('Ctrl Pts',(7.86296446599994,11.6,7.31006786799998));
#207872=CARTESIAN_POINT('Ctrl Pts',(7.86426610499994,15.2,7.31220165499998));
#207873=CARTESIAN_POINT('Ctrl Pts',(7.86426610499994,11.6,7.31220165499998));
#207874=CARTESIAN_POINT('Ctrl Pts',(7.86556910799994,15.2,7.31434181699999));
#207875=CARTESIAN_POINT('Ctrl Pts',(7.86556910799994,11.6,7.31434181699999));
#207876=CARTESIAN_POINT('Ctrl Pts',(7.86687346199994,15.2,7.31648834799999));
#207877=CARTESIAN_POINT('Ctrl Pts',(7.86687346199994,11.6,7.31648834799999));
#207878=CARTESIAN_POINT('Ctrl Pts',(7.86817915099994,15.2,7.31864124199999));
#207879=CARTESIAN_POINT('Ctrl Pts',(7.86817915099994,11.6,7.31864124199999));
#207880=CARTESIAN_POINT('Ctrl Pts',(7.86948616399994,15.2,7.32080049499999));
#207881=CARTESIAN_POINT('Ctrl Pts',(7.86948616399994,11.6,7.32080049499999));
#207882=CARTESIAN_POINT('Ctrl Pts',(7.87079448499994,15.2,7.32296609999998));
#207883=CARTESIAN_POINT('Ctrl Pts',(7.87079448499994,11.6,7.32296609999998));
#207884=CARTESIAN_POINT('Ctrl Pts',(7.87210409899994,15.2,7.32513805299998));
#207885=CARTESIAN_POINT('Ctrl Pts',(7.87210409899994,11.6,7.32513805299998));
#207886=CARTESIAN_POINT('Ctrl Pts',(7.87341499399994,15.2,7.32731634799999));
#207887=CARTESIAN_POINT('Ctrl Pts',(7.87341499399994,11.6,7.32731634799999));
#207888=CARTESIAN_POINT('Ctrl Pts',(7.87472715499994,15.2,7.32950097999999));
#207889=CARTESIAN_POINT('Ctrl Pts',(7.87472715499994,11.6,7.32950097999999));
#207890=CARTESIAN_POINT('Ctrl Pts',(7.87604056899994,15.2,7.33169194399999));
#207891=CARTESIAN_POINT('Ctrl Pts',(7.87604056899994,11.6,7.33169194399999));
#207892=CARTESIAN_POINT('Ctrl Pts',(7.87735522199994,15.2,7.33388923399998));
#207893=CARTESIAN_POINT('Ctrl Pts',(7.87735522199994,11.6,7.33388923399998));
#207894=CARTESIAN_POINT('Ctrl Pts',(7.87867109999994,15.2,7.33609284399999));
#207895=CARTESIAN_POINT('Ctrl Pts',(7.87867109999994,11.6,7.33609284399999));
#207896=CARTESIAN_POINT('Ctrl Pts',(7.87998818899994,15.2,7.33830276999999));
#207897=CARTESIAN_POINT('Ctrl Pts',(7.87998818899994,11.6,7.33830276999999));
#207898=CARTESIAN_POINT('Ctrl Pts',(7.88130647599995,15.2,7.34051900599999));
#207899=CARTESIAN_POINT('Ctrl Pts',(7.88130647599995,11.6,7.34051900599999));
#207900=CARTESIAN_POINT('Ctrl Pts',(7.88262594599995,15.2,7.34274154699998));
#207901=CARTESIAN_POINT('Ctrl Pts',(7.88262594599995,11.6,7.34274154699998));
#207902=CARTESIAN_POINT('Ctrl Pts',(7.88394658699994,15.2,7.34497038799999));
#207903=CARTESIAN_POINT('Ctrl Pts',(7.88394658699994,11.6,7.34497038799999));
#207904=CARTESIAN_POINT('Ctrl Pts',(7.88526838499994,15.2,7.34720552299999));
#207905=CARTESIAN_POINT('Ctrl Pts',(7.88526838499994,11.6,7.34720552299999));
#207906=CARTESIAN_POINT('Ctrl Pts',(7.88659132599994,15.2,7.34944694699998));
#207907=CARTESIAN_POINT('Ctrl Pts',(7.88659132599994,11.6,7.34944694699998));
#207908=CARTESIAN_POINT('Ctrl Pts',(7.88791539499995,15.2,7.35169465499999));
#207909=CARTESIAN_POINT('Ctrl Pts',(7.88791539499995,11.6,7.35169465499999));
#207910=CARTESIAN_POINT('Ctrl Pts',(7.88924058199994,15.2,7.35394864099998));
#207911=CARTESIAN_POINT('Ctrl Pts',(7.88924058199994,11.6,7.35394864099998));
#207912=CARTESIAN_POINT('Ctrl Pts',(7.89056687199994,15.2,7.35620889999999));
#207913=CARTESIAN_POINT('Ctrl Pts',(7.89056687199994,11.6,7.35620889999999));
#207914=CARTESIAN_POINT('Ctrl Pts',(7.89189425199995,15.2,7.35847542799998));
#207915=CARTESIAN_POINT('Ctrl Pts',(7.89189425199995,11.6,7.35847542799998));
#207916=CARTESIAN_POINT('Ctrl Pts',(7.89322270799994,15.2,7.36074821699999));
#207917=CARTESIAN_POINT('Ctrl Pts',(7.89322270799994,11.6,7.36074821699999));
#207918=CARTESIAN_POINT('Ctrl Pts',(7.89455222599994,15.2,7.36302726399998));
#207919=CARTESIAN_POINT('Ctrl Pts',(7.89455222599994,11.6,7.36302726399998));
#207920=CARTESIAN_POINT('Ctrl Pts',(7.89588279399994,15.2,7.36531256299998));
#207921=CARTESIAN_POINT('Ctrl Pts',(7.89588279399994,11.6,7.36531256299998));
#207922=CARTESIAN_POINT('Ctrl Pts',(7.89721439899994,15.2,7.36760410899999));
#207923=CARTESIAN_POINT('Ctrl Pts',(7.89721439899994,11.6,7.36760410899999));
#207924=CARTESIAN_POINT('Ctrl Pts',(7.89854702699994,15.2,7.36990189599998));
#207925=CARTESIAN_POINT('Ctrl Pts',(7.89854702699994,11.6,7.36990189599998));
#207926=CARTESIAN_POINT('Ctrl Pts',(7.89988066499994,15.2,7.37220591999999));
#207927=CARTESIAN_POINT('Ctrl Pts',(7.89988066499994,11.6,7.37220591999999));
#207928=CARTESIAN_POINT('Ctrl Pts',(7.90121529899994,15.2,7.37451617399999));
#207929=CARTESIAN_POINT('Ctrl Pts',(7.90121529899994,11.6,7.37451617399999));
#207930=CARTESIAN_POINT('Ctrl Pts',(7.90255091899994,15.2,7.37683265399999));
#207931=CARTESIAN_POINT('Ctrl Pts',(7.90255091899994,11.6,7.37683265399999));
#207932=CARTESIAN_POINT('Ctrl Pts',(7.90388750899995,15.2,7.37915535499998));
#207933=CARTESIAN_POINT('Ctrl Pts',(7.90388750899995,11.6,7.37915535499998));
#207934=CARTESIAN_POINT('Ctrl Pts',(7.90522505699994,15.2,7.38148427099999));
#207935=CARTESIAN_POINT('Ctrl Pts',(7.90522505699994,11.6,7.38148427099999));
#207936=CARTESIAN_POINT('Ctrl Pts',(7.90656354999994,15.2,7.38381939599999));
#207937=CARTESIAN_POINT('Ctrl Pts',(7.90656354999994,11.6,7.38381939599999));
#207938=CARTESIAN_POINT('Ctrl Pts',(7.90790297499995,15.2,7.38616072699998));
#207939=CARTESIAN_POINT('Ctrl Pts',(7.90790297499995,11.6,7.38616072699998));
#207940=CARTESIAN_POINT('Ctrl Pts',(7.90924331999994,15.2,7.38850825899998));
#207941=CARTESIAN_POINT('Ctrl Pts',(7.90924331999994,11.6,7.38850825899998));
#207942=CARTESIAN_POINT('Ctrl Pts',(7.91058456999994,15.2,7.39086198299999));
#207943=CARTESIAN_POINT('Ctrl Pts',(7.91058456999994,11.6,7.39086198299999));
#207944=CARTESIAN_POINT('Ctrl Pts',(7.91192671499994,15.2,7.39322189699998));
#207945=CARTESIAN_POINT('Ctrl Pts',(7.91192671499994,11.6,7.39322189699998));
#207946=CARTESIAN_POINT('Ctrl Pts',(7.91326973899994,15.2,7.39558799399998));
#207947=CARTESIAN_POINT('Ctrl Pts',(7.91326973899994,11.6,7.39558799399998));
#207948=CARTESIAN_POINT('Ctrl Pts',(7.91461363199994,15.2,7.39796027099998));
#207949=CARTESIAN_POINT('Ctrl Pts',(7.91461363199994,11.6,7.39796027099998));
#207950=CARTESIAN_POINT('Ctrl Pts',(7.91595838099994,15.2,7.40033872099998));
#207951=CARTESIAN_POINT('Ctrl Pts',(7.91595838099994,11.6,7.40033872099998));
#207952=CARTESIAN_POINT('Ctrl Pts',(7.91730397199994,15.2,7.40272333899998));
#207953=CARTESIAN_POINT('Ctrl Pts',(7.91730397199994,11.6,7.40272333899998));
#207954=CARTESIAN_POINT('Ctrl Pts',(7.91865039399994,15.2,7.40511412099998));
#207955=CARTESIAN_POINT('Ctrl Pts',(7.91865039399994,11.6,7.40511412099998));
#207956=CARTESIAN_POINT('Ctrl Pts',(7.91999763299994,15.2,7.40751105999998));
#207957=CARTESIAN_POINT('Ctrl Pts',(7.91999763299994,11.6,7.40751105999998));
#207958=CARTESIAN_POINT('Ctrl Pts',(7.92134567599994,15.2,7.40991415199999));
#207959=CARTESIAN_POINT('Ctrl Pts',(7.92134567599994,11.6,7.40991415199999));
#207960=CARTESIAN_POINT('Ctrl Pts',(7.92269451299994,15.2,7.41232339099999));
#207961=CARTESIAN_POINT('Ctrl Pts',(7.92269451299994,11.6,7.41232339099999));
#207962=CARTESIAN_POINT('Ctrl Pts',(7.92404412999994,15.2,7.41473877199999));
#207963=CARTESIAN_POINT('Ctrl Pts',(7.92404412999994,11.6,7.41473877199999));
#207964=CARTESIAN_POINT('Ctrl Pts',(7.92539451299994,15.2,7.41716029099998));
#207965=CARTESIAN_POINT('Ctrl Pts',(7.92539451299994,11.6,7.41716029099998));
#207966=CARTESIAN_POINT('Ctrl Pts',(7.92674565299994,15.2,7.41958794199999));
#207967=CARTESIAN_POINT('Ctrl Pts',(7.92674565299994,11.6,7.41958794199999));
#207968=CARTESIAN_POINT('Ctrl Pts',(7.92809753399994,15.2,7.42202171999998));
#207969=CARTESIAN_POINT('Ctrl Pts',(7.92809753399994,11.6,7.42202171999998));
#207970=CARTESIAN_POINT('Ctrl Pts',(7.92945014599994,15.2,7.42446161799998));
#207971=CARTESIAN_POINT('Ctrl Pts',(7.92945014599994,11.6,7.42446161799998));
#207972=CARTESIAN_POINT('Ctrl Pts',(7.93080347599994,15.2,7.42690763399998));
#207973=CARTESIAN_POINT('Ctrl Pts',(7.93080347599994,11.6,7.42690763399998));
#207974=CARTESIAN_POINT('Ctrl Pts',(7.93215751199994,15.2,7.42935976099999));
#207975=CARTESIAN_POINT('Ctrl Pts',(7.93215751199994,11.6,7.42935976099999));
#207976=CARTESIAN_POINT('Ctrl Pts',(7.93351224099994,15.2,7.43181799299999));
#207977=CARTESIAN_POINT('Ctrl Pts',(7.93351224099994,11.6,7.43181799299999));
#207978=CARTESIAN_POINT('Ctrl Pts',(7.93486765099995,15.2,7.43428232699999));
#207979=CARTESIAN_POINT('Ctrl Pts',(7.93486765099995,11.6,7.43428232699999));
#207980=CARTESIAN_POINT('Ctrl Pts',(7.93622373099995,15.2,7.43675275699999));
#207981=CARTESIAN_POINT('Ctrl Pts',(7.93622373099995,11.6,7.43675275699999));
#207982=CARTESIAN_POINT('Ctrl Pts',(7.93758046899995,15.2,7.43922927699998));
#207983=CARTESIAN_POINT('Ctrl Pts',(7.93758046899995,11.6,7.43922927699998));
#207984=CARTESIAN_POINT('Ctrl Pts',(7.93893784999994,15.2,7.44171188299998));
#207985=CARTESIAN_POINT('Ctrl Pts',(7.93893784999994,11.6,7.44171188299998));
#207986=CARTESIAN_POINT('Ctrl Pts',(7.94029586499994,15.2,7.44420056899998));
#207987=CARTESIAN_POINT('Ctrl Pts',(7.94029586499994,11.6,7.44420056899998));
#207988=CARTESIAN_POINT('Ctrl Pts',(7.94165449999995,15.2,7.44669532999998));
#207989=CARTESIAN_POINT('Ctrl Pts',(7.94165449999995,11.6,7.44669532999998));
#207990=CARTESIAN_POINT('Ctrl Pts',(7.94301374399994,15.2,7.44919616099998));
#207991=CARTESIAN_POINT('Ctrl Pts',(7.94301374399994,11.6,7.44919616099998));
#207992=CARTESIAN_POINT('Ctrl Pts',(7.94437358499994,15.2,7.45170305799999));
#207993=CARTESIAN_POINT('Ctrl Pts',(7.94437358499994,11.6,7.45170305799999));
#207994=CARTESIAN_POINT('Ctrl Pts',(7.94573401199994,15.2,7.45421601399999));
#207995=CARTESIAN_POINT('Ctrl Pts',(7.94573401199994,11.6,7.45421601399999));
#207996=CARTESIAN_POINT('Ctrl Pts',(7.94709500999994,15.2,7.45673502499999));
#207997=CARTESIAN_POINT('Ctrl Pts',(7.94709500999994,11.6,7.45673502499999));
#207998=CARTESIAN_POINT('Ctrl Pts',(7.94845656999994,15.2,7.45926008499998));
#207999=CARTESIAN_POINT('Ctrl Pts',(7.94845656999994,11.6,7.45926008499998));
#208000=CARTESIAN_POINT('Ctrl Pts',(7.94981867799994,15.2,7.46179118999999));
#208001=CARTESIAN_POINT('Ctrl Pts',(7.94981867799994,11.6,7.46179118999999));
#208002=CARTESIAN_POINT('Ctrl Pts',(7.95118132499994,15.2,7.46432833399999));
#208003=CARTESIAN_POINT('Ctrl Pts',(7.95118132499994,11.6,7.46432833399999));
#208004=CARTESIAN_POINT('Ctrl Pts',(7.95254449699994,15.2,7.46687151199998));
#208005=CARTESIAN_POINT('Ctrl Pts',(7.95254449699994,11.6,7.46687151199998));
#208006=CARTESIAN_POINT('Ctrl Pts',(7.95390818299994,15.2,7.46942071899999));
#208007=CARTESIAN_POINT('Ctrl Pts',(7.95390818299994,11.6,7.46942071899999));
#208008=CARTESIAN_POINT('Ctrl Pts',(7.95527237099995,15.2,7.47197595099999));
#208009=CARTESIAN_POINT('Ctrl Pts',(7.95527237099995,11.6,7.47197595099999));
#208010=CARTESIAN_POINT('Ctrl Pts',(7.95663704999995,15.2,7.47453720099998));
#208011=CARTESIAN_POINT('Ctrl Pts',(7.95663704999995,11.6,7.47453720099998));
#208012=CARTESIAN_POINT('Ctrl Pts',(7.95800220699994,15.2,7.47710446499998));
#208013=CARTESIAN_POINT('Ctrl Pts',(7.95800220699994,11.6,7.47710446499998));
#208014=CARTESIAN_POINT('Ctrl Pts',(7.95936783099994,15.2,7.47967773799999));
#208015=CARTESIAN_POINT('Ctrl Pts',(7.95936783099994,11.6,7.47967773799999));
#208016=CARTESIAN_POINT('Ctrl Pts',(7.96073391099994,15.2,7.48225701399999));
#208017=CARTESIAN_POINT('Ctrl Pts',(7.96073391099994,11.6,7.48225701399999));
#208018=CARTESIAN_POINT('Ctrl Pts',(7.96210043599994,15.2,7.48484228899999));
#208019=CARTESIAN_POINT('Ctrl Pts',(7.96210043599994,11.6,7.48484228899999));
#208020=CARTESIAN_POINT('Ctrl Pts',(7.96346739099994,15.2,7.48743355699999));
#208021=CARTESIAN_POINT('Ctrl Pts',(7.96346739099994,11.6,7.48743355699999));
#208022=CARTESIAN_POINT('Ctrl Pts',(7.96483476899994,15.2,7.49003081299998));
#208023=CARTESIAN_POINT('Ctrl Pts',(7.96483476899994,11.6,7.49003081299998));
#208024=CARTESIAN_POINT('Ctrl Pts',(7.96620255699994,15.2,7.49263405299998));
#208025=CARTESIAN_POINT('Ctrl Pts',(7.96620255699994,11.6,7.49263405299998));
#208026=CARTESIAN_POINT('Ctrl Pts',(7.96757074099994,15.2,7.49524327099999));
#208027=CARTESIAN_POINT('Ctrl Pts',(7.96757074099994,11.6,7.49524327099999));
#208028=CARTESIAN_POINT('Ctrl Pts',(7.96893931299994,15.2,7.49785846199998));
#208029=CARTESIAN_POINT('Ctrl Pts',(7.96893931299994,11.6,7.49785846199998));
#208030=CARTESIAN_POINT('Ctrl Pts',(7.97030825999994,15.2,7.50047962099998));
#208031=CARTESIAN_POINT('Ctrl Pts',(7.97030825999994,11.6,7.50047962099998));
#208032=CARTESIAN_POINT('Ctrl Pts',(7.97167756999994,15.2,7.50310674299998));
#208033=CARTESIAN_POINT('Ctrl Pts',(7.97167756999994,11.6,7.50310674299998));
#208034=CARTESIAN_POINT('Ctrl Pts',(7.97304723399994,15.2,7.50573982299999));
#208035=CARTESIAN_POINT('Ctrl Pts',(7.97304723399994,11.6,7.50573982299999));
#208036=CARTESIAN_POINT('Ctrl Pts',(7.97441723799994,15.2,7.50837885499998));
#208037=CARTESIAN_POINT('Ctrl Pts',(7.97441723799994,11.6,7.50837885499998));
#208038=CARTESIAN_POINT('Ctrl Pts',(7.97578757299994,15.2,7.51102383499998));
#208039=CARTESIAN_POINT('Ctrl Pts',(7.97578757299994,11.6,7.51102383499998));
#208040=CARTESIAN_POINT('Ctrl Pts',(7.97715822599995,15.2,7.51367475799999));
#208041=CARTESIAN_POINT('Ctrl Pts',(7.97715822599995,11.6,7.51367475799999));
#208042=CARTESIAN_POINT('Ctrl Pts',(7.97852918799994,15.2,7.51633161899999));
#208043=CARTESIAN_POINT('Ctrl Pts',(7.97852918799994,11.6,7.51633161899999));
#208044=CARTESIAN_POINT('Ctrl Pts',(7.97990044399994,15.2,7.51899441299998));
#208045=CARTESIAN_POINT('Ctrl Pts',(7.97990044399994,11.6,7.51899441299998));
#208046=CARTESIAN_POINT('Ctrl Pts',(7.98127198699994,15.2,7.52166313299998));
#208047=CARTESIAN_POINT('Ctrl Pts',(7.98127198699994,11.6,7.52166313299998));
#208048=CARTESIAN_POINT('Ctrl Pts',(7.98264380399995,15.2,7.52433777599999));
#208049=CARTESIAN_POINT('Ctrl Pts',(7.98264380399995,11.6,7.52433777599999));
#208050=CARTESIAN_POINT('Ctrl Pts',(7.98401588399994,15.2,7.52701833699999));
#208051=CARTESIAN_POINT('Ctrl Pts',(7.98401588399994,11.6,7.52701833699999));
#208052=CARTESIAN_POINT('Ctrl Pts',(7.98538821699994,15.2,7.52970480999998));
#208053=CARTESIAN_POINT('Ctrl Pts',(7.98538821699994,11.6,7.52970480999998));
#208054=CARTESIAN_POINT('Ctrl Pts',(7.98676078999994,15.2,7.53239718999998));
#208055=CARTESIAN_POINT('Ctrl Pts',(7.98676078999994,11.6,7.53239718999998));
#208056=CARTESIAN_POINT('Ctrl Pts',(7.98813359199994,15.2,7.53509547299998));
#208057=CARTESIAN_POINT('Ctrl Pts',(7.98813359199994,11.6,7.53509547299998));
#208058=CARTESIAN_POINT('Ctrl Pts',(7.98950661399994,15.2,7.53779965299999));
#208059=CARTESIAN_POINT('Ctrl Pts',(7.98950661399994,11.6,7.53779965299999));
#208060=CARTESIAN_POINT('Ctrl Pts',(7.99087984399995,15.2,7.54050972499999));
#208061=CARTESIAN_POINT('Ctrl Pts',(7.99087984399995,11.6,7.54050972499999));
#208062=CARTESIAN_POINT('Ctrl Pts',(7.99225327199995,15.2,7.54322568499998));
#208063=CARTESIAN_POINT('Ctrl Pts',(7.99225327199995,11.6,7.54322568499998));
#208064=CARTESIAN_POINT('Ctrl Pts',(7.99362688499994,15.2,7.54594752699998));
#208065=CARTESIAN_POINT('Ctrl Pts',(7.99362688499994,11.6,7.54594752699998));
#208066=CARTESIAN_POINT('Ctrl Pts',(7.99500067299994,15.2,7.54867524499998));
#208067=CARTESIAN_POINT('Ctrl Pts',(7.99500067299994,11.6,7.54867524499998));
#208068=CARTESIAN_POINT('Ctrl Pts',(7.99637462599994,15.2,7.55140883699998));
#208069=CARTESIAN_POINT('Ctrl Pts',(7.99637462599994,11.6,7.55140883699998));
#208070=CARTESIAN_POINT('Ctrl Pts',(7.99774873399994,15.2,7.55414829599999));
#208071=CARTESIAN_POINT('Ctrl Pts',(7.99774873399994,11.6,7.55414829599999));
#208072=CARTESIAN_POINT('Ctrl Pts',(7.99912298399994,15.2,7.55689361599998));
#208073=CARTESIAN_POINT('Ctrl Pts',(7.99912298399994,11.6,7.55689361599998));
#208074=CARTESIAN_POINT('Ctrl Pts',(8.00049736599994,15.2,7.55964479299998));
#208075=CARTESIAN_POINT('Ctrl Pts',(8.00049736599994,11.6,7.55964479299998));
#208076=CARTESIAN_POINT('Ctrl Pts',(8.00187186999995,15.2,7.56240182299998));
#208077=CARTESIAN_POINT('Ctrl Pts',(8.00187186999995,11.6,7.56240182299998));
#208078=CARTESIAN_POINT('Ctrl Pts',(8.00324648399994,15.2,7.56516469899999));
#208079=CARTESIAN_POINT('Ctrl Pts',(8.00324648399994,11.6,7.56516469899999));
#208080=CARTESIAN_POINT('Ctrl Pts',(8.00462119899995,15.2,7.56793341899999));
#208081=CARTESIAN_POINT('Ctrl Pts',(8.00462119899995,11.6,7.56793341899999));
#208082=CARTESIAN_POINT('Ctrl Pts',(8.00599600299994,15.2,7.57070797499999));
#208083=CARTESIAN_POINT('Ctrl Pts',(8.00599600299994,11.6,7.57070797499999));
#208084=CARTESIAN_POINT('Ctrl Pts',(8.00737088599995,15.2,7.57348836199998));
#208085=CARTESIAN_POINT('Ctrl Pts',(8.00737088599995,11.6,7.57348836199998));
#208086=CARTESIAN_POINT('Ctrl Pts',(8.00874583699994,15.2,7.57627457799998));
#208087=CARTESIAN_POINT('Ctrl Pts',(8.00874583699994,11.6,7.57627457799998));
#208088=CARTESIAN_POINT('Ctrl Pts',(8.01012084599994,15.2,7.57906661499998));
#208089=CARTESIAN_POINT('Ctrl Pts',(8.01012084599994,11.6,7.57906661499998));
#208090=CARTESIAN_POINT('Ctrl Pts',(8.01149590299995,15.2,7.58186446999999));
#208091=CARTESIAN_POINT('Ctrl Pts',(8.01149590299995,11.6,7.58186446999999));
#208092=CARTESIAN_POINT('Ctrl Pts',(8.01287099699995,15.2,7.58466813699999));
#208093=CARTESIAN_POINT('Ctrl Pts',(8.01287099699995,11.6,7.58466813699999));
#208094=CARTESIAN_POINT('Ctrl Pts',(8.01424611599994,15.2,7.58747760999999));
#208095=CARTESIAN_POINT('Ctrl Pts',(8.01424611599994,11.6,7.58747760999999));
#208096=CARTESIAN_POINT('Ctrl Pts',(8.01562124999995,15.2,7.59029288699999));
#208097=CARTESIAN_POINT('Ctrl Pts',(8.01562124999995,11.6,7.59029288699999));
#208098=CARTESIAN_POINT('Ctrl Pts',(8.01699639099994,15.2,7.59311395999998));
#208099=CARTESIAN_POINT('Ctrl Pts',(8.01699639099994,11.6,7.59311395999998));
#208100=CARTESIAN_POINT('Ctrl Pts',(8.01837152699994,15.2,7.59594082499999));
#208101=CARTESIAN_POINT('Ctrl Pts',(8.01837152699994,11.6,7.59594082499999));
#208102=CARTESIAN_POINT('Ctrl Pts',(8.01974664599994,15.2,7.59877347799998));
#208103=CARTESIAN_POINT('Ctrl Pts',(8.01974664599994,11.6,7.59877347799998));
#208104=CARTESIAN_POINT('Ctrl Pts',(8.02112173999994,15.2,7.60161191299999));
#208105=CARTESIAN_POINT('Ctrl Pts',(8.02112173999994,11.6,7.60161191299999));
#208106=CARTESIAN_POINT('Ctrl Pts',(8.02249679899995,15.2,7.60445612599998));
#208107=CARTESIAN_POINT('Ctrl Pts',(8.02249679899995,11.6,7.60445612599998));
#208108=CARTESIAN_POINT('Ctrl Pts',(8.02387180999995,15.2,7.60730610999998));
#208109=CARTESIAN_POINT('Ctrl Pts',(8.02387180999995,11.6,7.60730610999998));
#208110=CARTESIAN_POINT('Ctrl Pts',(8.02524676499995,15.2,7.61016186299998));
#208111=CARTESIAN_POINT('Ctrl Pts',(8.02524676499995,11.6,7.61016186299998));
#208112=CARTESIAN_POINT('Ctrl Pts',(8.02662165299994,15.2,7.61302337699998));
#208113=CARTESIAN_POINT('Ctrl Pts',(8.02662165299994,11.6,7.61302337699998));
#208114=CARTESIAN_POINT('Ctrl Pts',(8.02799646399994,15.2,7.61589064899999));
#208115=CARTESIAN_POINT('Ctrl Pts',(8.02799646399994,11.6,7.61589064899999));
#208116=CARTESIAN_POINT('Ctrl Pts',(8.02937118699995,15.2,7.61876367399999));
#208117=CARTESIAN_POINT('Ctrl Pts',(8.02937118699995,11.6,7.61876367399999));
#208118=CARTESIAN_POINT('Ctrl Pts',(8.03074581299994,15.2,7.62164244599998));
#208119=CARTESIAN_POINT('Ctrl Pts',(8.03074581299994,11.6,7.62164244599998));
#208120=CARTESIAN_POINT('Ctrl Pts',(8.03212033199994,15.2,7.62452696099999));
#208121=CARTESIAN_POINT('Ctrl Pts',(8.03212033199994,11.6,7.62452696099999));
#208122=CARTESIAN_POINT('Ctrl Pts',(8.03349473299994,15.2,7.62741721399999));
#208123=CARTESIAN_POINT('Ctrl Pts',(8.03349473299994,11.6,7.62741721399999));
#208124=CARTESIAN_POINT('Ctrl Pts',(8.03486900499994,15.2,7.63031319899999));
#208125=CARTESIAN_POINT('Ctrl Pts',(8.03486900499994,11.6,7.63031319899999));
#208126=CARTESIAN_POINT('Ctrl Pts',(8.03624313899994,15.2,7.63321491099998));
#208127=CARTESIAN_POINT('Ctrl Pts',(8.03624313899994,11.6,7.63321491099998));
#208128=CARTESIAN_POINT('Ctrl Pts',(8.03761712599995,15.2,7.63612234699998));
#208129=CARTESIAN_POINT('Ctrl Pts',(8.03761712599995,11.6,7.63612234699998));
#208130=CARTESIAN_POINT('Ctrl Pts',(8.03899095499995,15.2,7.63903550099998));
#208131=CARTESIAN_POINT('Ctrl Pts',(8.03899095499995,11.6,7.63903550099998));
#208132=CARTESIAN_POINT('Ctrl Pts',(8.04036461599994,15.2,7.64195436799999));
#208133=CARTESIAN_POINT('Ctrl Pts',(8.04036461599994,11.6,7.64195436799999));
#208134=CARTESIAN_POINT('Ctrl Pts',(8.04173809999994,15.2,7.64487894199998));
#208135=CARTESIAN_POINT('Ctrl Pts',(8.04173809999994,11.6,7.64487894199998));
#208136=CARTESIAN_POINT('Ctrl Pts',(8.04311139399994,15.2,7.64780921999999));
#208137=CARTESIAN_POINT('Ctrl Pts',(8.04311139399994,11.6,7.64780921999999));
#208138=CARTESIAN_POINT('Ctrl Pts',(8.04448449099995,15.2,7.65074519599998));
#208139=CARTESIAN_POINT('Ctrl Pts',(8.04448449099995,11.6,7.65074519599998));
#208140=CARTESIAN_POINT('Ctrl Pts',(8.04585738099994,15.2,7.65368686499999));
#208141=CARTESIAN_POINT('Ctrl Pts',(8.04585738099994,11.6,7.65368686499999));
#208142=CARTESIAN_POINT('Ctrl Pts',(8.04723005199994,15.2,7.65663422199999));
#208143=CARTESIAN_POINT('Ctrl Pts',(8.04723005199994,11.6,7.65663422199999));
#208144=CARTESIAN_POINT('Ctrl Pts',(8.04860249599994,15.2,7.65958726299999));
#208145=CARTESIAN_POINT('Ctrl Pts',(8.04860249599994,11.6,7.65958726299999));
#208146=CARTESIAN_POINT('Ctrl Pts',(8.04997470299995,15.2,7.66254598199998));
#208147=CARTESIAN_POINT('Ctrl Pts',(8.04997470299995,11.6,7.66254598199998));
#208148=CARTESIAN_POINT('Ctrl Pts',(8.05134666299994,15.2,7.66551037499998));
#208149=CARTESIAN_POINT('Ctrl Pts',(8.05134666299994,11.6,7.66551037499998));
#208150=CARTESIAN_POINT('Ctrl Pts',(8.05271836599994,15.2,7.66848043599998));
#208151=CARTESIAN_POINT('Ctrl Pts',(8.05271836599994,11.6,7.66848043599998));
#208152=CARTESIAN_POINT('Ctrl Pts',(8.05408980299994,15.2,7.67145616099998));
#208153=CARTESIAN_POINT('Ctrl Pts',(8.05408980299994,11.6,7.67145616099998));
#208154=CARTESIAN_POINT('Ctrl Pts',(8.05546096299994,15.2,7.67443754599999));
#208155=CARTESIAN_POINT('Ctrl Pts',(8.05546096299994,11.6,7.67443754599999));
#208156=CARTESIAN_POINT('Ctrl Pts',(8.05683183699994,15.2,7.67742458299999));
#208157=CARTESIAN_POINT('Ctrl Pts',(8.05683183699994,11.6,7.67742458299999));
#208158=CARTESIAN_POINT('Ctrl Pts',(8.05820241499994,15.2,7.68041726999999));
#208159=CARTESIAN_POINT('Ctrl Pts',(8.05820241499994,11.6,7.68041726999999));
#208160=CARTESIAN_POINT('Ctrl Pts',(8.05957268699995,15.2,7.68341559999998));
#208161=CARTESIAN_POINT('Ctrl Pts',(8.05957268699995,11.6,7.68341559999998));
#208162=CARTESIAN_POINT('Ctrl Pts',(8.06094264599994,15.2,7.68641956999998));
#208163=CARTESIAN_POINT('Ctrl Pts',(8.06094264599994,11.6,7.68641956999998));
#208164=CARTESIAN_POINT('Ctrl Pts',(8.06231227799995,15.2,7.68942917499999));
#208165=CARTESIAN_POINT('Ctrl Pts',(8.06231227799995,11.6,7.68942917499999));
#208166=CARTESIAN_POINT('Ctrl Pts',(8.06368157799995,15.2,7.69244440799999));
#208167=CARTESIAN_POINT('Ctrl Pts',(8.06368157799995,11.6,7.69244440799999));
#208168=CARTESIAN_POINT('Ctrl Pts',(8.06505053199994,15.2,7.69546526699998));
#208169=CARTESIAN_POINT('Ctrl Pts',(8.06505053199994,11.6,7.69546526699998));
#208170=CARTESIAN_POINT('Ctrl Pts',(8.06641913399995,15.2,7.69849174399998));
#208171=CARTESIAN_POINT('Ctrl Pts',(8.06641913399995,11.6,7.69849174399998));
#208172=CARTESIAN_POINT('Ctrl Pts',(8.06778737299994,15.2,7.70152383699998));
#208173=CARTESIAN_POINT('Ctrl Pts',(8.06778737299994,11.6,7.70152383699998));
#208174=CARTESIAN_POINT('Ctrl Pts',(8.06915523899994,15.2,7.70456153799999));
#208175=CARTESIAN_POINT('Ctrl Pts',(8.06915523899994,11.6,7.70456153799999));
#208176=CARTESIAN_POINT('Ctrl Pts',(8.07052272299994,15.2,7.70760484499998));
#208177=CARTESIAN_POINT('Ctrl Pts',(8.07052272299994,11.6,7.70760484499998));
#208178=CARTESIAN_POINT('Ctrl Pts',(8.07188981699994,15.2,7.71065375199999));
#208179=CARTESIAN_POINT('Ctrl Pts',(8.07188981699994,11.6,7.71065375199999));
#208180=CARTESIAN_POINT('Ctrl Pts',(8.07325650899994,15.2,7.71370825499999));
#208181=CARTESIAN_POINT('Ctrl Pts',(8.07325650899994,11.6,7.71370825499999));
#208182=CARTESIAN_POINT('Ctrl Pts',(8.07462279199994,15.2,7.71676834699999));
#208183=CARTESIAN_POINT('Ctrl Pts',(8.07462279199994,11.6,7.71676834699999));
#208184=CARTESIAN_POINT('Ctrl Pts',(8.07598865399994,15.2,7.71983402599999));
#208185=CARTESIAN_POINT('Ctrl Pts',(8.07598865399994,11.6,7.71983402599999));
#208186=CARTESIAN_POINT('Ctrl Pts',(8.07735408799994,15.2,7.72290528399999));
#208187=CARTESIAN_POINT('Ctrl Pts',(8.07735408799994,11.6,7.72290528399999));
#208188=CARTESIAN_POINT('Ctrl Pts',(8.07871908299994,15.2,7.72598211799998));
#208189=CARTESIAN_POINT('Ctrl Pts',(8.07871908299994,11.6,7.72598211799998));
#208190=CARTESIAN_POINT('Ctrl Pts',(8.08008363099994,15.2,7.72906452199998));
#208191=CARTESIAN_POINT('Ctrl Pts',(8.08008363099994,11.6,7.72906452199998));
#208192=CARTESIAN_POINT('Ctrl Pts',(8.08144772299995,15.2,7.73215249199998));
#208193=CARTESIAN_POINT('Ctrl Pts',(8.08144772299995,11.6,7.73215249199998));
#208194=CARTESIAN_POINT('Ctrl Pts',(8.08281134699994,15.2,7.73524602399998));
#208195=CARTESIAN_POINT('Ctrl Pts',(8.08281134699994,11.6,7.73524602399998));
#208196=CARTESIAN_POINT('Ctrl Pts',(8.08417449699995,15.2,7.73834511199999));
#208197=CARTESIAN_POINT('Ctrl Pts',(8.08417449699995,11.6,7.73834511199999));
#208198=CARTESIAN_POINT('Ctrl Pts',(8.08553716199994,15.2,7.74144974999999));
#208199=CARTESIAN_POINT('Ctrl Pts',(8.08553716199994,11.6,7.74144974999999));
#208200=CARTESIAN_POINT('Ctrl Pts',(8.08689933199994,15.2,7.74455993599998));
#208201=CARTESIAN_POINT('Ctrl Pts',(8.08689933199994,11.6,7.74455993599998));
#208202=CARTESIAN_POINT('Ctrl Pts',(8.08826100099994,15.2,7.74767566199999));
#208203=CARTESIAN_POINT('Ctrl Pts',(8.08826100099994,11.6,7.74767566199999));
#208204=CARTESIAN_POINT('Ctrl Pts',(8.08962215599994,15.2,7.75079692599999));
#208205=CARTESIAN_POINT('Ctrl Pts',(8.08962215599994,11.6,7.75079692599999));
#208206=CARTESIAN_POINT('Ctrl Pts',(8.09098279099994,15.2,7.75392372099999));
#208207=CARTESIAN_POINT('Ctrl Pts',(8.09098279099994,11.6,7.75392372099999));
#208208=CARTESIAN_POINT('Ctrl Pts',(8.09234289399994,15.2,7.75705604499999));
#208209=CARTESIAN_POINT('Ctrl Pts',(8.09234289399994,11.6,7.75705604499999));
#208210=CARTESIAN_POINT('Ctrl Pts',(8.09370245799995,15.2,7.76019388899999));
#208211=CARTESIAN_POINT('Ctrl Pts',(8.09370245799995,11.6,7.76019388899999));
#208212=CARTESIAN_POINT('Ctrl Pts',(8.09506147399994,15.2,7.76333725099998));
#208213=CARTESIAN_POINT('Ctrl Pts',(8.09506147399994,11.6,7.76333725099998));
#208214=CARTESIAN_POINT('Ctrl Pts',(8.09641993199994,15.2,7.76648612399998));
#208215=CARTESIAN_POINT('Ctrl Pts',(8.09641993199994,11.6,7.76648612399998));
#208216=CARTESIAN_POINT('Ctrl Pts',(8.09777782299994,15.2,7.76964050699998));
#208217=CARTESIAN_POINT('Ctrl Pts',(8.09777782299994,11.6,7.76964050699998));
#208218=CARTESIAN_POINT('Ctrl Pts',(8.09913513899994,15.2,7.77280038999999));
#208219=CARTESIAN_POINT('Ctrl Pts',(8.09913513899994,11.6,7.77280038999999));
#208220=CARTESIAN_POINT('Ctrl Pts',(8.10049186899995,15.2,7.77596577299998));
#208221=CARTESIAN_POINT('Ctrl Pts',(8.10049186899995,11.6,7.77596577299998));
#208222=CARTESIAN_POINT('Ctrl Pts',(8.10184800599994,15.2,7.77913664799998));
#208223=CARTESIAN_POINT('Ctrl Pts',(8.10184800599994,11.6,7.77913664799998));
#208224=CARTESIAN_POINT('Ctrl Pts',(8.10320353999994,15.2,7.78231301199998));
#208225=CARTESIAN_POINT('Ctrl Pts',(8.10320353999994,11.6,7.78231301199998));
#208226=CARTESIAN_POINT('Ctrl Pts',(8.10455846199994,15.2,7.78549485899998));
#208227=CARTESIAN_POINT('Ctrl Pts',(8.10455846199994,11.6,7.78549485899998));
#208228=CARTESIAN_POINT('Ctrl Pts',(8.10591276399995,15.2,7.78868218399998));
#208229=CARTESIAN_POINT('Ctrl Pts',(8.10591276399995,11.6,7.78868218399998));
#208230=CARTESIAN_POINT('Ctrl Pts',(8.10726643599994,15.2,7.79187498299999));
#208231=CARTESIAN_POINT('Ctrl Pts',(8.10726643599994,11.6,7.79187498299999));
#208232=CARTESIAN_POINT('Ctrl Pts',(8.10861946999994,15.2,7.79507325099999));
#208233=CARTESIAN_POINT('Ctrl Pts',(8.10861946999994,11.6,7.79507325099999));
#208234=CARTESIAN_POINT('Ctrl Pts',(8.10997185699994,15.2,7.79827698299999));
#208235=CARTESIAN_POINT('Ctrl Pts',(8.10997185699994,11.6,7.79827698299999));
#208236=CARTESIAN_POINT('Ctrl Pts',(8.11132358699994,15.2,7.80148617399998));
#208237=CARTESIAN_POINT('Ctrl Pts',(8.11132358699994,11.6,7.80148617399998));
#208238=CARTESIAN_POINT('Ctrl Pts',(8.11267465299995,15.2,7.80470081999999));
#208239=CARTESIAN_POINT('Ctrl Pts',(8.11267465299995,11.6,7.80470081999999));
#208240=CARTESIAN_POINT('Ctrl Pts',(8.11402504499994,15.2,7.80792091499999));
#208241=CARTESIAN_POINT('Ctrl Pts',(8.11402504499994,11.6,7.80792091499999));
#208242=CARTESIAN_POINT('Ctrl Pts',(8.11537475499994,15.2,7.81114645499999));
#208243=CARTESIAN_POINT('Ctrl Pts',(8.11537475499994,11.6,7.81114645499999));
#208244=CARTESIAN_POINT('Ctrl Pts',(8.11672377399994,15.2,7.81437743399999));
#208245=CARTESIAN_POINT('Ctrl Pts',(8.11672377399994,11.6,7.81437743399999));
#208246=CARTESIAN_POINT('Ctrl Pts',(8.11807209199995,15.2,7.81761384899998));
#208247=CARTESIAN_POINT('Ctrl Pts',(8.11807209199995,11.6,7.81761384899998));
#208248=CARTESIAN_POINT('Ctrl Pts',(8.11941970299995,15.2,7.82085569399998));
#208249=CARTESIAN_POINT('Ctrl Pts',(8.11941970299995,11.6,7.82085569399998));
#208250=CARTESIAN_POINT('Ctrl Pts',(8.12076659499994,15.2,7.82410296499998));
#208251=CARTESIAN_POINT('Ctrl Pts',(8.12076659499994,11.6,7.82410296499998));
#208252=CARTESIAN_POINT('Ctrl Pts',(8.12211276199994,15.2,7.82735565499999));
#208253=CARTESIAN_POINT('Ctrl Pts',(8.12211276199994,11.6,7.82735565499999));
#208254=CARTESIAN_POINT('Ctrl Pts',(8.12345819499994,15.2,7.83061376199999));
#208255=CARTESIAN_POINT('Ctrl Pts',(8.12345819499994,11.6,7.83061376199999));
#208256=CARTESIAN_POINT('Ctrl Pts',(8.12480288299994,15.2,7.83387727999998));
#208257=CARTESIAN_POINT('Ctrl Pts',(8.12480288299994,11.6,7.83387727999998));
#208258=CARTESIAN_POINT('Ctrl Pts',(8.12614681999994,15.2,7.83714620399999));
#208259=CARTESIAN_POINT('Ctrl Pts',(8.12614681999994,11.6,7.83714620399999));
#208260=CARTESIAN_POINT('Ctrl Pts',(8.12748999699994,15.2,7.84042052999999));
#208261=CARTESIAN_POINT('Ctrl Pts',(8.12748999699994,11.6,7.84042052999999));
#208262=CARTESIAN_POINT('Ctrl Pts',(8.12883240399995,15.2,7.84370025199999));
#208263=CARTESIAN_POINT('Ctrl Pts',(8.12883240399995,11.6,7.84370025199999));
#208264=CARTESIAN_POINT('Ctrl Pts',(8.13017403399994,15.2,7.84698536599999));
#208265=CARTESIAN_POINT('Ctrl Pts',(8.13017403399994,11.6,7.84698536599999));
#208266=CARTESIAN_POINT('Ctrl Pts',(8.13151487799994,15.2,7.85027586699999));
#208267=CARTESIAN_POINT('Ctrl Pts',(8.13151487799994,11.6,7.85027586699999));
#208268=CARTESIAN_POINT('Ctrl Pts',(8.13285492699995,15.2,7.85357174999999));
#208269=CARTESIAN_POINT('Ctrl Pts',(8.13285492699995,11.6,7.85357174999999));
#208270=CARTESIAN_POINT('Ctrl Pts',(8.13419417199994,15.2,7.85687300999999));
#208271=CARTESIAN_POINT('Ctrl Pts',(8.13419417199994,11.6,7.85687300999999));
#208272=CARTESIAN_POINT('Ctrl Pts',(8.13553260699994,15.2,7.86017964299998));
#208273=CARTESIAN_POINT('Ctrl Pts',(8.13553260699994,11.6,7.86017964299998));
#208274=CARTESIAN_POINT('Ctrl Pts',(8.13687022199994,15.2,7.86349164399999));
#208275=CARTESIAN_POINT('Ctrl Pts',(8.13687022199994,11.6,7.86349164399999));
#208276=CARTESIAN_POINT('Ctrl Pts',(8.13820700799995,15.2,7.86680900799999));
#208277=CARTESIAN_POINT('Ctrl Pts',(8.13820700799995,11.6,7.86680900799999));
#208278=CARTESIAN_POINT('Ctrl Pts',(8.13954295599994,15.2,7.87013172999998));
#208279=CARTESIAN_POINT('Ctrl Pts',(8.13954295599994,11.6,7.87013172999998));
#208280=CARTESIAN_POINT('Ctrl Pts',(8.14087805899994,15.2,7.87345980499998));
#208281=CARTESIAN_POINT('Ctrl Pts',(8.14087805899994,11.6,7.87345980499998));
#208282=CARTESIAN_POINT('Ctrl Pts',(8.14221230899994,15.2,7.87679322899999));
#208283=CARTESIAN_POINT('Ctrl Pts',(8.14221230899994,11.6,7.87679322899999));
#208284=CARTESIAN_POINT('Ctrl Pts',(8.14354569599994,15.2,7.88013199699999));
#208285=CARTESIAN_POINT('Ctrl Pts',(8.14354569599994,11.6,7.88013199699999));
#208286=CARTESIAN_POINT('Ctrl Pts',(8.14487821399995,15.2,7.88347610399998));
#208287=CARTESIAN_POINT('Ctrl Pts',(8.14487821399995,11.6,7.88347610399998));
#208288=CARTESIAN_POINT('Ctrl Pts',(8.14620985199995,15.2,7.88682554499999));
#208289=CARTESIAN_POINT('Ctrl Pts',(8.14620985199995,11.6,7.88682554499999));
#208290=CARTESIAN_POINT('Ctrl Pts',(8.14754060299994,15.2,7.89018031599999));
#208291=CARTESIAN_POINT('Ctrl Pts',(8.14754060299994,11.6,7.89018031599999));
#208292=CARTESIAN_POINT('Ctrl Pts',(8.14887045999994,15.2,7.89354041099998));
#208293=CARTESIAN_POINT('Ctrl Pts',(8.14887045999994,11.6,7.89354041099998));
#208294=CARTESIAN_POINT('Ctrl Pts',(8.15019941199994,15.2,7.89690582699999));
#208295=CARTESIAN_POINT('Ctrl Pts',(8.15019941199994,11.6,7.89690582699999));
#208296=CARTESIAN_POINT('Ctrl Pts',(8.15152745299994,15.2,7.90027655699999));
#208297=CARTESIAN_POINT('Ctrl Pts',(8.15152745299994,11.6,7.90027655699999));
#208298=CARTESIAN_POINT('Ctrl Pts',(8.15285457299994,15.2,7.90365259799999));
#208299=CARTESIAN_POINT('Ctrl Pts',(8.15285457299994,11.6,7.90365259799999));
#208300=CARTESIAN_POINT('Ctrl Pts',(8.15418076399994,15.2,7.90703394499998));
#208301=CARTESIAN_POINT('Ctrl Pts',(8.15418076399994,11.6,7.90703394499998));
#208302=CARTESIAN_POINT('Ctrl Pts',(8.15550602099994,15.2,7.91042059199999));
#208303=CARTESIAN_POINT('Ctrl Pts',(8.15550602099994,11.6,7.91042059199999));
#208304=CARTESIAN_POINT('Ctrl Pts',(8.15683033099995,15.2,7.91381253499999));
#208305=CARTESIAN_POINT('Ctrl Pts',(8.15683033099995,11.6,7.91381253499999));
#208306=CARTESIAN_POINT('Ctrl Pts',(8.15815368899995,15.2,7.91720976999999));
#208307=CARTESIAN_POINT('Ctrl Pts',(8.15815368899995,11.6,7.91720976999999));
#208308=CARTESIAN_POINT('Ctrl Pts',(8.15947608599994,15.2,7.92061229099998));
#208309=CARTESIAN_POINT('Ctrl Pts',(8.15947608599994,11.6,7.92061229099998));
#208310=CARTESIAN_POINT('Ctrl Pts',(8.16079751299995,15.2,7.92402009399999));
#208311=CARTESIAN_POINT('Ctrl Pts',(8.16079751299995,11.6,7.92402009399999));
#208312=CARTESIAN_POINT('Ctrl Pts',(8.16211796399994,15.2,7.92743317399999));
#208313=CARTESIAN_POINT('Ctrl Pts',(8.16211796399994,11.6,7.92743317399999));
#208314=CARTESIAN_POINT('Ctrl Pts',(8.16343742899994,15.2,7.93085152599998));
#208315=CARTESIAN_POINT('Ctrl Pts',(8.16343742899994,11.6,7.93085152599998));
#208316=CARTESIAN_POINT('Ctrl Pts',(8.16475590099994,15.2,7.93427514699999));
#208317=CARTESIAN_POINT('Ctrl Pts',(8.16475590099994,11.6,7.93427514699999));
#208318=CARTESIAN_POINT('Ctrl Pts',(8.16607337199994,15.2,7.93770402899998));
#208319=CARTESIAN_POINT('Ctrl Pts',(8.16607337199994,11.6,7.93770402899998));
#208320=CARTESIAN_POINT('Ctrl Pts',(8.16738983299994,15.2,7.94113816999998));
#208321=CARTESIAN_POINT('Ctrl Pts',(8.16738983299994,11.6,7.94113816999998));
#208322=CARTESIAN_POINT('Ctrl Pts',(8.16870527599994,15.2,7.94457756299998));
#208323=CARTESIAN_POINT('Ctrl Pts',(8.16870527599994,11.6,7.94457756299998));
#208324=CARTESIAN_POINT('Ctrl Pts',(8.17001969299995,15.2,7.94802220599998));
#208325=CARTESIAN_POINT('Ctrl Pts',(8.17001969299995,11.6,7.94802220599998));
#208326=CARTESIAN_POINT('Ctrl Pts',(8.17133307699994,15.2,7.95147209099999));
#208327=CARTESIAN_POINT('Ctrl Pts',(8.17133307699994,11.6,7.95147209099999));
#208328=CARTESIAN_POINT('Ctrl Pts',(8.17264541999995,15.2,7.95492721699999));
#208329=CARTESIAN_POINT('Ctrl Pts',(8.17264541999995,11.6,7.95492721699999));
#208330=CARTESIAN_POINT('Ctrl Pts',(8.17395671199994,15.2,7.95838757499999));
#208331=CARTESIAN_POINT('Ctrl Pts',(8.17395671199994,11.6,7.95838757499999));
#208332=CARTESIAN_POINT('Ctrl Pts',(8.17526694799995,15.2,7.96185316399999));
#208333=CARTESIAN_POINT('Ctrl Pts',(8.17526694799995,11.6,7.96185316399999));
#208334=CARTESIAN_POINT('Ctrl Pts',(8.17657611899994,15.2,7.96532397699998));
#208335=CARTESIAN_POINT('Ctrl Pts',(8.17657611899994,11.6,7.96532397699998));
#208336=CARTESIAN_POINT('Ctrl Pts',(8.17788421699994,15.2,7.96880001099999));
#208337=CARTESIAN_POINT('Ctrl Pts',(8.17788421699994,11.6,7.96880001099999));
#208338=CARTESIAN_POINT('Ctrl Pts',(8.17919123399994,15.2,7.97228125999998));
#208339=CARTESIAN_POINT('Ctrl Pts',(8.17919123399994,11.6,7.97228125999998));
#208340=CARTESIAN_POINT('Ctrl Pts',(8.18049716299995,15.2,7.97576771899998));
#208341=CARTESIAN_POINT('Ctrl Pts',(8.18049716299995,11.6,7.97576771899998));
#208342=CARTESIAN_POINT('Ctrl Pts',(8.18180199499994,15.2,7.97925938399998));
#208343=CARTESIAN_POINT('Ctrl Pts',(8.18180199499994,11.6,7.97925938399998));
#208344=CARTESIAN_POINT('Ctrl Pts',(8.18310572199995,15.2,7.98275625099999));
#208345=CARTESIAN_POINT('Ctrl Pts',(8.18310572199995,11.6,7.98275625099999));
#208346=CARTESIAN_POINT('Ctrl Pts',(8.18440833599994,15.2,7.98625831199999));
#208347=CARTESIAN_POINT('Ctrl Pts',(8.18440833599994,11.6,7.98625831199999));
#208348=CARTESIAN_POINT('Ctrl Pts',(8.18570982799995,15.2,7.98976556499999));
#208349=CARTESIAN_POINT('Ctrl Pts',(8.18570982799995,11.6,7.98976556499999));
#208350=CARTESIAN_POINT('Ctrl Pts',(8.18701019199995,15.2,7.99327800499999));
#208351=CARTESIAN_POINT('Ctrl Pts',(8.18701019199995,11.6,7.99327800499999));
#208352=CARTESIAN_POINT('Ctrl Pts',(8.18830941999994,15.2,7.99679562499998));
#208353=CARTESIAN_POINT('Ctrl Pts',(8.18830941999994,11.6,7.99679562499998));
#208354=CARTESIAN_POINT('Ctrl Pts',(8.18960750499994,15.2,8.00031842399999));
#208355=CARTESIAN_POINT('Ctrl Pts',(8.18960750499994,11.6,8.00031842399999));
#208356=CARTESIAN_POINT('Ctrl Pts',(8.19090443899994,15.2,8.00384639699999));
#208357=CARTESIAN_POINT('Ctrl Pts',(8.19090443899994,11.6,8.00384639699999));
#208358=CARTESIAN_POINT('Ctrl Pts',(8.19220021699994,15.2,8.00737953699999));
#208359=CARTESIAN_POINT('Ctrl Pts',(8.19220021699994,11.6,8.00737953699999));
#208360=CARTESIAN_POINT('Ctrl Pts',(8.19349483099994,15.2,8.01091784299999));
#208361=CARTESIAN_POINT('Ctrl Pts',(8.19349483099994,11.6,8.01091784299999));
#208362=CARTESIAN_POINT('Ctrl Pts',(8.19478827199994,15.2,8.01446130799999));
#208363=CARTESIAN_POINT('Ctrl Pts',(8.19478827199994,11.6,8.01446130799999));
#208364=CARTESIAN_POINT('Ctrl Pts',(8.19608053199994,15.2,8.01800992699999));
#208365=CARTESIAN_POINT('Ctrl Pts',(8.19608053199994,11.6,8.01800992699999));
#208366=CARTESIAN_POINT('Ctrl Pts',(8.19737160099994,15.2,8.02156369499999));
#208367=CARTESIAN_POINT('Ctrl Pts',(8.19737160099994,11.6,8.02156369499999));
#208368=CARTESIAN_POINT('Ctrl Pts',(8.19866146999994,15.2,8.02512260499999));
#208369=CARTESIAN_POINT('Ctrl Pts',(8.19866146999994,11.6,8.02512260499999));
#208370=CARTESIAN_POINT('Ctrl Pts',(8.19995012899994,15.2,8.02868665099999));
#208371=CARTESIAN_POINT('Ctrl Pts',(8.19995012899994,11.6,8.02868665099999));
#208372=CARTESIAN_POINT('Ctrl Pts',(8.20123756999994,15.2,8.03225582899999));
#208373=CARTESIAN_POINT('Ctrl Pts',(8.20123756999994,11.6,8.03225582899999));
#208374=CARTESIAN_POINT('Ctrl Pts',(8.20252378699994,15.2,8.03583013499999));
#208375=CARTESIAN_POINT('Ctrl Pts',(8.20252378699994,11.6,8.03583013499999));
#208376=CARTESIAN_POINT('Ctrl Pts',(8.20380877399994,15.2,8.03940956399998));
#208377=CARTESIAN_POINT('Ctrl Pts',(8.20380877399994,11.6,8.03940956399998));
#208378=CARTESIAN_POINT('Ctrl Pts',(8.20509252799994,15.2,8.04299411599998));
#208379=CARTESIAN_POINT('Ctrl Pts',(8.20509252799994,11.6,8.04299411599998));
#208380=CARTESIAN_POINT('Ctrl Pts',(8.20637504799994,15.2,8.04658378899998));
#208381=CARTESIAN_POINT('Ctrl Pts',(8.20637504799994,11.6,8.04658378899998));
#208382=CARTESIAN_POINT('Ctrl Pts',(8.20740007499994,15.2,8.04945962199999));
#208383=CARTESIAN_POINT('Ctrl Pts',(8.20740007499994,11.6,8.04945962199999));
#208384=CARTESIAN_POINT('Ctrl Pts',(8.20816828899994,15.2,8.05161879999999));
#208385=CARTESIAN_POINT('Ctrl Pts',(8.20816828899994,11.6,8.05161879999999));
#208386=CARTESIAN_POINT('Ctrl Pts',(8.20868018299995,15.2,8.05305927699998));
#208387=CARTESIAN_POINT('Ctrl Pts',(8.20868018299995,11.6,8.05305927699998));
#208388=CARTESIAN_POINT('Ctrl Pts',(8.20893606999994,15.2,8.05377977099998));
#208389=CARTESIAN_POINT('Ctrl Pts',(8.20893606999994,11.6,8.05377977099998));
#208390=CARTESIAN_POINT('Ctrl Pts',(7.64657512299994,15.2,7.01216898699998));
#208391=CARTESIAN_POINT('Ctrl Pts',(7.64778328654791,15.2,7.01348522668636));
#208392=CARTESIAN_POINT('Ctrl Pts',(7.64902613283499,15.2,7.0148472224676));
#208393=CARTESIAN_POINT('Ctrl Pts',(7.65030255111842,15.2,7.01625467982076));
#208394=CARTESIAN_POINT('Ctrl Pts',(7.651585124936,15.2,7.01766892464472));
#208395=CARTESIAN_POINT('Ctrl Pts',(7.65290158847099,15.2,7.01912907727743));
#208396=CARTESIAN_POINT('Ctrl Pts',(7.65425083044716,15.2,7.02063486218735));
#208397=CARTESIAN_POINT('Ctrl Pts',(7.65560007230076,15.2,7.0221406469605));
#208398=CARTESIAN_POINT('Ctrl Pts',(7.65698209060125,15.2,7.02369206276625));
#208399=CARTESIAN_POINT('Ctrl Pts',(7.65839580954989,15.2,7.02528884145824));
#208400=CARTESIAN_POINT('Ctrl Pts',(7.65980952849853,15.2,7.02688562015022));
#208401=CARTESIAN_POINT('Ctrl Pts',(7.6612549458305,15.2,7.02852776000807));
#208402=CARTESIAN_POINT('Ctrl Pts',(7.66273101409884,15.2,7.0302149976118));
#208403=CARTESIAN_POINT('Ctrl Pts',(7.66420708250127,15.2,7.03190223536877));
#208404=CARTESIAN_POINT('Ctrl Pts',(7.66571380242329,15.2,7.03363456911039));
#208405=CARTESIAN_POINT('Ctrl Pts',(7.6672501549257,15.2,7.03541173821029));
#208406=CARTESIAN_POINT('Ctrl Pts',(7.66904256596918,15.2,7.03748510191804));
#208407=CARTESIAN_POINT('Ctrl Pts',(7.67087531161421,15.2,7.03961949183139));
#208408=CARTESIAN_POINT('Ctrl Pts',(7.67274682060312,15.2,7.04181450134301));
#208409=CARTESIAN_POINT('Ctrl Pts',(7.67435097135238,15.2,7.04369593828699));
#208410=CARTESIAN_POINT('Ctrl Pts',(7.67598360497184,15.2,7.04562191207094));
#208411=CARTESIAN_POINT('Ctrl Pts',(7.67764376073086,15.2,7.04759217001468));
#208412=CARTESIAN_POINT('Ctrl Pts',(7.67930391633907,15.2,7.04956242777943));
#208413=CARTESIAN_POINT('Ctrl Pts',(7.68099159523845,15.2,7.05157697021619));
#208414=CARTESIAN_POINT('Ctrl Pts',(7.68270586501735,15.2,7.05363554898419));
#208415=CARTESIAN_POINT('Ctrl Pts',(7.68442013479623,15.2,7.05569412775218));
#208416=CARTESIAN_POINT('Ctrl Pts',(7.68616099674403,15.2,7.05779674259635));
#208417=CARTESIAN_POINT('Ctrl Pts',(7.6879275415954,15.2,7.05994315018312));
#208418=CARTESIAN_POINT('Ctrl Pts',(7.68969408660722,15.2,7.06208955796485));
#208419=CARTESIAN_POINT('Ctrl Pts',(7.69148631527225,15.2,7.06427975580202));
#208420=CARTESIAN_POINT('Ctrl Pts',(7.69330334245629,15.2,7.06651350476006));
#208421=CARTESIAN_POINT('Ctrl Pts',(7.6951203694753,15.2,7.06874725351521));
#208422=CARTESIAN_POINT('Ctrl Pts',(7.69696219657678,15.2,7.07102455272568));
#208423=CARTESIAN_POINT('Ctrl Pts',(7.69882796059335,15.2,7.07334516364323));
#208424=CARTESIAN_POINT('Ctrl Pts',(7.70069372460993,15.2,7.07566577456079));
#208425=CARTESIAN_POINT('Ctrl Pts',(7.70258342734961,15.2,7.07802969765826));
#208426=CARTESIAN_POINT('Ctrl Pts',(7.70449622661242,15.2,7.08043669840224));
#208427=CARTESIAN_POINT('Ctrl Pts',(7.70640902587525,15.2,7.08284369914623));
#208428=CARTESIAN_POINT('Ctrl Pts',(7.70834492374246,15.2,7.08529377607167));
#208429=CARTESIAN_POINT('Ctrl Pts',(7.71030309983647,15.2,7.08778669797819));
#208430=CARTESIAN_POINT('Ctrl Pts',(7.71226127610836,15.2,7.09027962011115));
#208431=CARTESIAN_POINT('Ctrl Pts',(7.71424172989907,15.2,7.09281538834824));
#208432=CARTESIAN_POINT('Ctrl Pts',(7.71624366334244,15.2,7.09539376965728));
#208433=CARTESIAN_POINT('Ctrl Pts',(7.71824559660397,15.2,7.09797215073212));
#208434=CARTESIAN_POINT('Ctrl Pts',(7.72026900951376,15.2,7.10059314884522));
#208435=CARTESIAN_POINT('Ctrl Pts',(7.72231311993859,15.2,7.10325653466326));
#208436=CARTESIAN_POINT('Ctrl Pts',(7.7243572303634,15.2,7.10591992048131));
#208437=CARTESIAN_POINT('Ctrl Pts',(7.72642203988311,15.2,7.1086256945531));
#208438=CARTESIAN_POINT('Ctrl Pts',(7.72850678630601,15.2,7.1113736324504));
#208439=CARTESIAN_POINT('Ctrl Pts',(7.73059153291828,15.2,7.1141215705973));
#208440=CARTESIAN_POINT('Ctrl Pts',(7.73269621517416,15.2,7.1169116723566));
#208441=CARTESIAN_POINT('Ctrl Pts',(7.73482009087407,15.2,7.11974371642943));
#208442=CARTESIAN_POINT('Ctrl Pts',(7.73694396638108,15.2,7.12257576024503));
#208443=CARTESIAN_POINT('Ctrl Pts',(7.73908703397603,15.2,7.12544974549974));
#208444=CARTESIAN_POINT('Ctrl Pts',(7.7412485664906,15.2,7.12836545249026));
#208445=CARTESIAN_POINT('Ctrl Pts',(7.74341009900516,15.2,7.13128115948078));
#208446=CARTESIAN_POINT('Ctrl Pts',(7.74559009592475,15.2,7.13423858848483));
#208447=CARTESIAN_POINT('Ctrl Pts',(7.74778784751036,15.2,7.13723752237304));
#208448=CARTESIAN_POINT('Ctrl Pts',(7.7499855992956,15.2,7.14023645653366));
#208449=CARTESIAN_POINT('Ctrl Pts',(7.7522011038984,15.2,7.14327689414883));
#208450=CARTESIAN_POINT('Ctrl Pts',(7.75443366796593,15.2,7.14635862055647));
#208451=CARTESIAN_POINT('Ctrl Pts',(7.75666623183067,15.2,7.14944034668418));
#208452=CARTESIAN_POINT('Ctrl Pts',(7.7589158527489,15.2,7.15256336313987));
#208453=CARTESIAN_POINT('Ctrl Pts',(7.76118185349991,15.2,7.15572745127491));
#208454=CARTESIAN_POINT('Ctrl Pts',(7.76344785425091,15.2,7.15889153940994));
#208455=CARTESIAN_POINT('Ctrl Pts',(7.76573023273056,15.2,7.16209670508579));
#208456=CARTESIAN_POINT('Ctrl Pts',(7.76802832376098,15.2,7.16534273221101));
#208457=CARTESIAN_POINT('Ctrl Pts',(7.76994339968924,15.2,7.16804775491364));
#208458=CARTESIAN_POINT('Ctrl Pts',(7.77186938791277,15.2,7.17078115509872));
#208459=CARTESIAN_POINT('Ctrl Pts',(7.77380591110667,15.2,7.17354281086114));
#208460=CARTESIAN_POINT('Ctrl Pts',(7.77574243430056,15.2,7.17630446662355));
#208461=CARTESIAN_POINT('Ctrl Pts',(7.77768948963916,15.2,7.17909437795613));
#208462=CARTESIAN_POINT('Ctrl Pts',(7.77964670963864,15.2,7.18191242302411));
#208463=CARTESIAN_POINT('Ctrl Pts',(7.78160392963811,15.2,7.18473046809209));
#208464=CARTESIAN_POINT('Ctrl Pts',(7.78357131293987,15.2,7.18757664774091));
#208465=CARTESIAN_POINT('Ctrl Pts',(7.78554849399051,15.2,7.19045084199002));
#208466=CARTESIAN_POINT('Ctrl Pts',(7.78792111116508,15.2,7.19389987496365));
#208467=CARTESIAN_POINT('Ctrl Pts',(7.79030783790979,15.2,7.19738924908786));
#208468=CARTESIAN_POINT('Ctrl Pts',(7.7927080559883,15.2,7.20091875887354));
#208469=CARTESIAN_POINT('Ctrl Pts',(7.79470823779308,15.2,7.20386001713514));
#208470=CARTESIAN_POINT('Ctrl Pts',(7.79671778842654,15.2,7.20682914547103));
#208471=CARTESIAN_POINT('Ctrl Pts',(7.79873635699896,15.2,7.20982602811878));
#208472=CARTESIAN_POINT('Ctrl Pts',(7.80115863941788,15.2,7.21342228749208));
#208473=CARTESIAN_POINT('Ctrl Pts',(7.80359390730747,15.2,7.21705851078088));
#208474=CARTESIAN_POINT('Ctrl Pts',(7.80604156552505,15.2,7.22073449515061));
#208475=CARTESIAN_POINT('Ctrl Pts',(7.80808128059522,15.2,7.22379781529177));
#208476=CARTESIAN_POINT('Ctrl Pts',(7.81012959882382,15.2,7.22688874835002));
#208477=CARTESIAN_POINT('Ctrl Pts',(7.81218618326893,15.2,7.23000717515781));
#208478=CARTESIAN_POINT('Ctrl Pts',(7.81424276748988,15.2,7.23312560162571));
#208479=CARTESIAN_POINT('Ctrl Pts',(7.81630761717762,15.2,7.23627152447745));
#208480=CARTESIAN_POINT('Ctrl Pts',(7.81838039972881,15.2,7.23944482510153));
#208481=CARTESIAN_POINT('Ctrl Pts',(7.82045318250593,15.2,7.2426181260715));
#208482=CARTESIAN_POINT('Ctrl Pts',(7.82253389826626,15.2,7.24581880747434));
#208483=CARTESIAN_POINT('Ctrl Pts',(7.82462221854344,15.2,7.24904675011104));
#208484=CARTESIAN_POINT('Ctrl Pts',(7.82671053882061,15.2,7.25227469274774));
#208485=CARTESIAN_POINT('Ctrl Pts',(7.82880646325679,15.2,7.25552990007356));
#208486=CARTESIAN_POINT('Ctrl Pts',(7.83090967197247,15.2,7.25881225461065));
#208487=CARTESIAN_POINT('Ctrl Pts',(7.83301288068813,15.2,7.26209460914773));
#208488=CARTESIAN_POINT('Ctrl Pts',(7.83512337073404,15.2,7.26540411328326));
#208489=CARTESIAN_POINT('Ctrl Pts',(7.83724082684483,15.2,7.26874065078187));
#208490=CARTESIAN_POINT('Ctrl Pts',(7.83935828295559,15.2,7.2720771882805));
#208491=CARTESIAN_POINT('Ctrl Pts',(7.84148270336094,15.2,7.27544075927419));
#208492=CARTESIAN_POINT('Ctrl Pts',(7.8436137771106,15.2,7.27883125024501));
#208493=CARTESIAN_POINT('Ctrl Pts',(7.84617106574955,15.2,7.28289983963172));
#208494=CARTESIAN_POINT('Ctrl Pts',(7.8487379355647,15.2,7.28700719500659));
#208495=CARTESIAN_POINT('Ctrl Pts',(7.85131385328905,15.2,7.29115311923518));
#208496=CARTESIAN_POINT('Ctrl Pts',(7.8534604510417,15.2,7.29460805552745));
#208497=CARTESIAN_POINT('Ctrl Pts',(7.85561333416446,15.2,7.29808977485895));
#208498=CARTESIAN_POINT('Ctrl Pts',(7.85777219948422,15.2,7.3015981678077));
#208499=CARTESIAN_POINT('Ctrl Pts',(7.8599310650393,15.2,7.30510656113886));
#208500=CARTESIAN_POINT('Ctrl Pts',(7.86209591267761,15.2,7.30864162479734));
#208501=CARTESIAN_POINT('Ctrl Pts',(7.86426644573269,15.2,7.3122032482674));
#208502=CARTESIAN_POINT('Ctrl Pts',(7.8660028722714,15.2,7.31505254719872));
#208503=CARTESIAN_POINT('Ctrl Pts',(7.86774293662873,15.2,7.31791884480106));
#208504=CARTESIAN_POINT('Ctrl Pts',(7.86948649100946,15.2,7.32080208302689));
#208505=CARTESIAN_POINT('Ctrl Pts',(7.87210182234299,15.2,7.3251269399728));
#208506=CARTESIAN_POINT('Ctrl Pts',(7.87472499953583,15.2,7.32948991477177));
#208507=CARTESIAN_POINT('Ctrl Pts',(7.8773555281066,15.2,7.3338908137769));
#208508=CARTESIAN_POINT('Ctrl Pts',(7.87954763532857,15.2,7.33755822974776));
#208509=CARTESIAN_POINT('Ctrl Pts',(7.88174484555065,15.2,7.34125198203039));
#208510=CARTESIAN_POINT('Ctrl Pts',(7.88394687610595,15.2,7.34497196126512));
#208511=CARTESIAN_POINT('Ctrl Pts',(7.88570850064619,15.2,7.3479479448151));
#208512=CARTESIAN_POINT('Ctrl Pts',(7.88747320806044,15.2,7.35094071321255));
#208513=CARTESIAN_POINT('Ctrl Pts',(7.88924085802311,15.2,7.35395020969504));
#208514=CARTESIAN_POINT('Ctrl Pts',(7.89100850774494,15.2,7.35695970576748));
#208515=CARTESIAN_POINT('Ctrl Pts',(7.89277909921404,15.2,7.35998593028729));
#208516=CARTESIAN_POINT('Ctrl Pts',(7.89455248834665,15.2,7.36302882675965));
#208517=CARTESIAN_POINT('Ctrl Pts',(7.89632587772089,15.2,7.3660717236466));
#208518=CARTESIAN_POINT('Ctrl Pts',(7.89810206741491,15.2,7.36913129288557));
#208519=CARTESIAN_POINT('Ctrl Pts',(7.89988091417871,15.2,7.37220747777655));
#208520=CARTESIAN_POINT('Ctrl Pts',(7.90165976070015,15.2,7.37528366224841));
#208521=CARTESIAN_POINT('Ctrl Pts',(7.90344126715913,15.2,7.37837646275746));
#208522=CARTESIAN_POINT('Ctrl Pts',(7.90522529299107,15.2,7.38148582282382));
#208523=CARTESIAN_POINT('Ctrl Pts',(7.9074553254633,15.2,7.38537252322448));
#208524=CARTESIAN_POINT('Ctrl Pts',(7.90968929562603,15.2,7.38928510072164));
#208525=CARTESIAN_POINT('Ctrl Pts',(7.91192693465361,15.2,7.39322344252584));
#208526=CARTESIAN_POINT('Ctrl Pts',(7.91371704597325,15.2,7.39637411614091));
#208527=CARTESIAN_POINT('Ctrl Pts',(7.91550950582929,15.2,7.39954128067188));
#208528=CARTESIAN_POINT('Ctrl Pts',(7.91730417987167,15.2,7.40272488023533));
#208529=CARTESIAN_POINT('Ctrl Pts',(7.91909885366954,15.2,7.40590847936502));
#208530=CARTESIAN_POINT('Ctrl Pts',(7.9208957400185,15.2,7.40910851331197));
#208531=CARTESIAN_POINT('Ctrl Pts',(7.9226947077389,15.2,7.41232492604162));
#208532=CARTESIAN_POINT('Ctrl Pts',(7.92494341757323,15.2,7.41634544228235));
#208533=CARTESIAN_POINT('Ctrl Pts',(7.92719537543041,15.2,7.42039155281845));
#208534=CARTESIAN_POINT('Ctrl Pts',(7.92945032536082,15.2,7.42446314719213));
#208535=CARTESIAN_POINT('Ctrl Pts',(7.93125428540345,15.2,7.42772042286859));
#208536=CARTESIAN_POINT('Ctrl Pts',(7.93306015981854,15.2,7.43099400908866));
#208537=CARTESIAN_POINT('Ctrl Pts',(7.9348678186394,15.2,7.43428385126902));
#208538=CARTESIAN_POINT('Ctrl Pts',(7.93667547721397,15.2,7.43757369300114));
#208539=CARTESIAN_POINT('Ctrl Pts',(7.93848492120874,15.2,7.44087978993051));
#208540=CARTESIAN_POINT('Ctrl Pts',(7.94029601976215,15.2,7.44420208726793));
#208541=CARTESIAN_POINT('Ctrl Pts',(7.94210711856231,15.2,7.44752438505801));
#208542=CARTESIAN_POINT('Ctrl Pts',(7.94391987284929,15.2,7.45086288371266));
#208543=CARTESIAN_POINT('Ctrl Pts',(7.94573415494827,15.2,7.45421752800765));
#208544=CARTESIAN_POINT('Ctrl Pts',(7.94754843680006,15.2,7.45757217184558));
#208545=CARTESIAN_POINT('Ctrl Pts',(7.94936424484875,15.2,7.46094296144694));
#208546=CARTESIAN_POINT('Ctrl Pts',(7.95118145597783,15.2,7.46432984194618));
#208547=CARTESIAN_POINT('Ctrl Pts',(7.95299866735449,15.2,7.46771672290688));
#208548=CARTESIAN_POINT('Ctrl Pts',(7.95481728007706,15.2,7.47111969545868));
#208549=CARTESIAN_POINT('Ctrl Pts',(7.95663716951785,15.2,7.47453870449392));
#208550=CARTESIAN_POINT('Ctrl Pts',(7.95845705871067,15.2,7.47795771306332));
#208551=CARTESIAN_POINT('Ctrl Pts',(7.96027822463998,15.2,7.48139275892224));
#208552=CARTESIAN_POINT('Ctrl Pts',(7.96210054326866,15.2,7.48484378669402));
#208553=CARTESIAN_POINT('Ctrl Pts',(7.96437844174071,15.2,7.48915757176139));
#208554=CARTESIAN_POINT('Ctrl Pts',(7.96665814236277,15.2,7.49349632912564));
#208555=CARTESIAN_POINT('Ctrl Pts',(7.96893940645989,15.2,7.49785995342917));
#208556=CARTESIAN_POINT('Ctrl Pts',(7.97076441783703,15.2,7.50135085306225));
#208557=CARTESIAN_POINT('Ctrl Pts',(7.97259042916554,15.2,7.50485766761928));
#208558=CARTESIAN_POINT('Ctrl Pts',(7.97441732071785,15.2,7.508380341994));
#208559=CARTESIAN_POINT('Ctrl Pts',(7.97624421202125,15.2,7.51190301588875));
#208560=CARTESIAN_POINT('Ctrl Pts',(7.97807198399497,15.2,7.51544155213318));
#208561=CARTESIAN_POINT('Ctrl Pts',(7.97990051540098,15.2,7.51899589395213));
#208562=CARTESIAN_POINT('Ctrl Pts',(7.98218617984534,15.2,7.52343882158902));
#208563=CARTESIAN_POINT('Ctrl Pts',(7.98447303585634,15.2,7.52790644667549));
#208564=CARTESIAN_POINT('Ctrl Pts',(7.98676084696736,15.2,7.53239866514568));
#208565=CARTESIAN_POINT('Ctrl Pts',(7.98859109595593,15.2,7.53599244011769));
#208566=CARTESIAN_POINT('Ctrl Pts',(7.99042195878624,15.2,7.53960195463566));
#208567=CARTESIAN_POINT('Ctrl Pts',(7.99225331827494,15.2,7.54322715549992));
#208568=CARTESIAN_POINT('Ctrl Pts',(7.99454251751107,15.2,7.54775865633328));
#208569=CARTESIAN_POINT('Ctrl Pts',(7.99683249171299,15.2,7.55231466662041));
#208570=CARTESIAN_POINT('Ctrl Pts',(7.99912301700119,15.2,7.55689508025243));
#208571=CARTESIAN_POINT('Ctrl Pts',(8.00095543708196,15.2,7.56055941085848));
#208572=CARTESIAN_POINT('Ctrl Pts',(8.00278820967234,15.2,7.56423936111329));
#208573=CARTESIAN_POINT('Ctrl Pts',(8.00462122096691,15.2,7.56793487742072));
#208574=CARTESIAN_POINT('Ctrl Pts',(8.00645423251124,15.2,7.57163039423166));
#208575=CARTESIAN_POINT('Ctrl Pts',(8.00828748172504,15.2,7.57534147510519));
#208576=CARTESIAN_POINT('Ctrl Pts',(8.01012085799161,15.2,7.57906806947492));
#208577=CARTESIAN_POINT('Ctrl Pts',(8.01195423425818,15.2,7.58279466384465));
#208578=CARTESIAN_POINT('Ctrl Pts',(8.01378773636091,15.2,7.58653677044127));
#208579=CARTESIAN_POINT('Ctrl Pts',(8.01562125201639,15.2,7.59029433664763));
#208580=CARTESIAN_POINT('Ctrl Pts',(8.0183715252498,15.2,7.59593068544521));
#208581=CARTESIAN_POINT('Ctrl Pts',(8.02112183180807,15.2,7.60160181655014));
#208582=CARTESIAN_POINT('Ctrl Pts',(8.02387179612482,15.2,7.60730755251103));
#208583=CARTESIAN_POINT('Ctrl Pts',(8.0261634331387,15.2,7.6120623326512));
#208584=CARTESIAN_POINT('Ctrl Pts',(8.02845483368311,15.2,7.61684114351289));
#208585=CARTESIAN_POINT('Ctrl Pts',(8.03074578639144,15.2,7.62164388205583));
#208586=CARTESIAN_POINT('Ctrl Pts',(8.03303673909975,15.2,7.62644662059878));
#208587=CARTESIAN_POINT('Ctrl Pts',(8.03532724145141,15.2,7.63127328592465));
#208588=CARTESIAN_POINT('Ctrl Pts',(8.03761708677409,15.2,7.63612377707141));
#208589=CARTESIAN_POINT('Ctrl Pts',(8.03944896288249,15.2,7.64000416967159));
#208590=CARTESIAN_POINT('Ctrl Pts',(8.04128041833601,15.2,7.6438998091205));
#208591=CARTESIAN_POINT('Ctrl Pts',(8.04311134457526,15.2,7.64781064418869));
#208592=CARTESIAN_POINT('Ctrl Pts',(8.04494227106398,15.2,7.65172147978973));
#208593=CARTESIAN_POINT('Ctrl Pts',(8.04677267057764,15.2,7.65564750984538));
#208594=CARTESIAN_POINT('Ctrl Pts',(8.04860243689952,15.2,7.65958868283892));
#208595=CARTESIAN_POINT('Ctrl Pts',(8.05134708613306,15.2,7.66550044179226));
#208596=CARTESIAN_POINT('Ctrl Pts',(8.05409031275252,15.2,7.67144627239573));
#208597=CARTESIAN_POINT('Ctrl Pts',(8.0568317629987,15.2,7.67742599545555));
#208598=CARTESIAN_POINT('Ctrl Pts',(8.05865939666216,15.2,7.68141247785753));
#208599=CARTESIAN_POINT('Ctrl Pts',(8.06048624151297,15.2,7.68541402431124));
#208600=CARTESIAN_POINT('Ctrl Pts',(8.06231219522349,15.2,7.68943058269832));
#208601=CARTESIAN_POINT('Ctrl Pts',(8.06413814868524,15.2,7.69344714053815));
#208602=CARTESIAN_POINT('Ctrl Pts',(8.06596321081376,15.2,7.69747871027327));
#208603=CARTESIAN_POINT('Ctrl Pts',(8.06778727960916,15.2,7.70152523871927));
#208604=CARTESIAN_POINT('Ctrl Pts',(8.06915533126784,15.2,7.7045601351916));
#208605=CARTESIAN_POINT('Ctrl Pts',(8.07052282405012,15.2,7.70760344580231));
#208606=CARTESIAN_POINT('Ctrl Pts',(8.07188971627715,15.2,7.71065515038458));
#208607=CARTESIAN_POINT('Ctrl Pts',(8.07371223941205,15.2,7.7147240901972));
#208608=CARTESIAN_POINT('Ctrl Pts',(8.07553369338018,15.2,7.71880795058581));
#208609=CARTESIAN_POINT('Ctrl Pts',(8.07735397842375,15.2,7.72290667831014));
#208610=CARTESIAN_POINT('Ctrl Pts',(8.07871919208242,15.2,7.72598072382416));
#208611=CARTESIAN_POINT('Ctrl Pts',(8.08008374884951,15.2,7.72906313201222));
#208612=CARTESIAN_POINT('Ctrl Pts',(8.08144760604995,15.2,7.73215388248325));
#208613=CARTESIAN_POINT('Ctrl Pts',(8.0828114632504,15.2,7.73524463295429));
#208614=CARTESIAN_POINT('Ctrl Pts',(8.08417462135087,15.2,7.73834372514165));
#208615=CARTESIAN_POINT('Ctrl Pts',(8.08553703813477,15.2,7.74145113661136));
#208616=CARTESIAN_POINT('Ctrl Pts',(8.08735359401163,15.2,7.74559435228064));
#208617=CARTESIAN_POINT('Ctrl Pts',(8.08916883383769,15.2,7.74975235797114));
#208618=CARTESIAN_POINT('Ctrl Pts',(8.0909826583048,15.2,7.75392510379717));
#208619=CARTESIAN_POINT('Ctrl Pts',(8.09234302653157,15.2,7.75705466288243));
#208620=CARTESIAN_POINT('Ctrl Pts',(8.09370259849747,15.2,7.7601925120899));
#208621=CARTESIAN_POINT('Ctrl Pts',(8.09506133465637,15.2,7.76333862914299));
#208622=CARTESIAN_POINT('Ctrl Pts',(8.09642007081527,15.2,7.76648474619608));
#208623=CARTESIAN_POINT('Ctrl Pts',(8.09777797033258,15.2,7.76963913238148));
#208624=CARTESIAN_POINT('Ctrl Pts',(8.09913499253328,15.2,7.77280176493325));
#208625=CARTESIAN_POINT('Ctrl Pts',(8.10139669628329,15.2,7.77807281937772));
#208626=CARTESIAN_POINT('Ctrl Pts',(8.10365596275761,15.2,7.78336678309528));
#208627=CARTESIAN_POINT('Ctrl Pts',(8.10591260651785,15.2,7.78868355249449));
#208628=CARTESIAN_POINT('Ctrl Pts',(8.1072665927248,15.2,7.79187361401812));
#208629=CARTESIAN_POINT('Ctrl Pts',(8.10861963502502,15.2,7.79507188673231));
#208630=CARTESIAN_POINT('Ctrl Pts',(8.10997169277373,15.2,7.79827834775536));
#208631=CARTESIAN_POINT('Ctrl Pts',(8.11132375052243,15.2,7.80148480877841));
#208632=CARTESIAN_POINT('Ctrl Pts',(8.11267482410175,15.2,7.80469945891659));
#208633=CARTESIAN_POINT('Ctrl Pts',(8.11402487434444,15.2,7.80792227588211));
#208634=CARTESIAN_POINT('Ctrl Pts',(8.11537492458714,15.2,7.81114509284762));
#208635=CARTESIAN_POINT('Ctrl Pts',(8.11672395120493,15.2,7.81437607634594));
#208636=CARTESIAN_POINT('Ctrl Pts',(8.1180719149061,15.2,7.81761520581047));
#208637=CARTESIAN_POINT('Ctrl Pts',(8.11941987885214,15.2,7.82085433586344));
#208638=CARTESIAN_POINT('Ctrl Pts',(8.12076677941457,15.2,7.8241016112854));
#208639=CARTESIAN_POINT('Ctrl Pts',(8.12211257877667,15.2,7.82735700992628));
#208640=CARTESIAN_POINT('Ctrl Pts',(8.12345837789428,15.2,7.83061240797576));
#208641=CARTESIAN_POINT('Ctrl Pts',(8.12480307402504,15.2,7.83387593048748));
#208642=CARTESIAN_POINT('Ctrl Pts',(8.12614663025155,15.2,7.83714755511632));
#208643=CARTESIAN_POINT('Ctrl Pts',(8.12749018647806,15.2,7.84041917974517));
#208644=CARTESIAN_POINT('Ctrl Pts',(8.12883260144497,15.2,7.84369890614386));
#208645=CARTESIAN_POINT('Ctrl Pts',(8.13017383764613,15.2,7.84698671310843));
#208646=CARTESIAN_POINT('Ctrl Pts',(8.13151507384729,15.2,7.850274520073));
#208647=CARTESIAN_POINT('Ctrl Pts',(8.13285513018193,15.2,7.85357040723663));
#208648=CARTESIAN_POINT('Ctrl Pts',(8.13419396946662,15.2,7.8568743532416));
#208649=CARTESIAN_POINT('Ctrl Pts',(8.13597908867503,15.2,7.86127961498171));
#208650=CARTESIAN_POINT('Ctrl Pts',(8.13776204510261,15.2,7.86569920457345));
#208651=CARTESIAN_POINT('Ctrl Pts',(8.13954274503276,15.2,7.8701330689832));
#208652=CARTESIAN_POINT('Ctrl Pts',(8.14087826985906,15.2,7.87345846698845));
#208653=CARTESIAN_POINT('Ctrl Pts',(8.14221252711043,15.2,7.87679189515166));
#208654=CARTESIAN_POINT('Ctrl Pts',(8.14354547885356,15.2,7.8801333321143));
#208655=CARTESIAN_POINT('Ctrl Pts',(8.1448784305967,15.2,7.88347476907694));
#208656=CARTESIAN_POINT('Ctrl Pts',(8.14621007626013,15.2,7.88682421450968));
#208657=CARTESIAN_POINT('Ctrl Pts',(8.14754037946783,15.2,7.89018164702799));
#208658=CARTESIAN_POINT('Ctrl Pts',(8.14931411699755,15.2,7.89465822351574));
#208659=CARTESIAN_POINT('Ctrl Pts',(8.15108546735234,15.2,7.89914899940261));
#208660=CARTESIAN_POINT('Ctrl Pts',(8.15285434048574,15.2,7.90365392375505));
#208661=CARTESIAN_POINT('Ctrl Pts',(8.15418099563705,15.2,7.90703261778661));
#208662=CARTESIAN_POINT('Ctrl Pts',(8.15550625964635,15.2,7.91041926964552));
#208663=CARTESIAN_POINT('Ctrl Pts',(8.15683009325522,15.2,7.9138138587233));
#208664=CARTESIAN_POINT('Ctrl Pts',(8.1581539266236,15.2,7.91720844718438));
#208665=CARTESIAN_POINT('Ctrl Pts',(8.15947633082536,15.2,7.92061097266167));
#208666=CARTESIAN_POINT('Ctrl Pts',(8.16079726911058,15.2,7.92402141362181));
#208667=CARTESIAN_POINT('Ctrl Pts',(8.1621182073958,15.2,7.92743185458195));
#208668=CARTESIAN_POINT('Ctrl Pts',(8.16343767999306,15.2,7.9308502113286));
#208669=CARTESIAN_POINT('Ctrl Pts',(8.16475565074282,15.2,7.93427646230306));
#208670=CARTESIAN_POINT('Ctrl Pts',(8.16607362149259,15.2,7.93770271327752));
#208671=CARTESIAN_POINT('Ctrl Pts',(8.16739009017389,15.2,7.94113685797293));
#208672=CARTESIAN_POINT('Ctrl Pts',(8.16870501950709,15.2,7.94457887544681));
#208673=CARTESIAN_POINT('Ctrl Pts',(8.1700199488403,15.2,7.94802089292069));
#208674=CARTESIAN_POINT('Ctrl Pts',(8.17133334032114,15.2,7.95147078323282));
#208675=CARTESIAN_POINT('Ctrl Pts',(8.17264515714861,15.2,7.95492852468983));
#208676=CARTESIAN_POINT('Ctrl Pts',(8.17395697397607,15.2,7.95838626614683));
#208677=CARTESIAN_POINT('Ctrl Pts',(8.17526721667867,15.2,7.96185185847002));
#208678=CARTESIAN_POINT('Ctrl Pts',(8.17657585046467,15.2,7.96532528146773));
#208679=CARTESIAN_POINT('Ctrl Pts',(8.1778844844884,15.2,7.96879870509643));
#208680=CARTESIAN_POINT('Ctrl Pts',(8.17919150906171,15.2,7.97227995908574));
#208681=CARTESIAN_POINT('Ctrl Pts',(8.18049688904286,15.2,7.97576902126055));
#208682=CARTESIAN_POINT('Ctrl Pts',(8.18180226878687,15.2,7.97925808280151));
#208683=CARTESIAN_POINT('Ctrl Pts',(8.18310600338431,15.2,7.98275495389608));
#208684=CARTESIAN_POINT('Ctrl Pts',(8.18440805577685,15.2,7.98625961065307));
#208685=CARTESIAN_POINT('Ctrl Pts',(8.1857101081694,15.2,7.98976426741006));
#208686=CARTESIAN_POINT('Ctrl Pts',(8.18701047855548,15.2,7.99327671097764));
#208687=CARTESIAN_POINT('Ctrl Pts',(8.18830913438315,15.2,7.99679692010043));
#208688=CARTESIAN_POINT('Ctrl Pts',(8.18960779021083,15.2,8.00031712922324));
#208689=CARTESIAN_POINT('Ctrl Pts',(8.19090473074702,15.2,8.00384510591173));
#208690=CARTESIAN_POINT('Ctrl Pts',(8.19219992599163,15.2,8.00738082844994));
#208691=CARTESIAN_POINT('Ctrl Pts',(8.19349512123624,15.2,8.01091655098815));
#208692=CARTESIAN_POINT('Ctrl Pts',(8.1947885704559,15.2,8.01446002097602));
#208693=CARTESIAN_POINT('Ctrl Pts',(8.19608023411747,15.2,8.01801121384631));
#208694=CARTESIAN_POINT('Ctrl Pts',(8.19737189777903,15.2,8.02156240671661));
#208695=CARTESIAN_POINT('Ctrl Pts',(8.19866177483297,15.2,8.0251213215956));
#208696=CARTESIAN_POINT('Ctrl Pts',(8.1999498242674,15.2,8.02868793330996));
#208697=CARTESIAN_POINT('Ctrl Pts',(8.20123787370183,15.2,8.03225454502431));
#208698=CARTESIAN_POINT('Ctrl Pts',(8.20252409519971,15.2,8.03582885366694));
#208699=CARTESIAN_POINT('Ctrl Pts',(8.20380846548663,15.2,8.03941084395239));
#208700=CARTESIAN_POINT('Ctrl Pts',(8.20552095935807,15.2,8.04418683143348));
#208701=CARTESIAN_POINT('Ctrl Pts',(8.20723015620175,15.2,8.04897647635775));
#208702=CARTESIAN_POINT('Ctrl Pts',(8.20893606999994,15.2,8.05377977099998));
#208703=CARTESIAN_POINT('Ctrl Pts',(7.64657512299994,12.2,7.01216898699998));
#208704=CARTESIAN_POINT('Ctrl Pts',(7.64778328654791,12.2,7.01348522668636));
#208705=CARTESIAN_POINT('Ctrl Pts',(7.64902613283499,12.2,7.0148472224676));
#208706=CARTESIAN_POINT('Ctrl Pts',(7.65030255111842,12.2,7.01625467982076));
#208707=CARTESIAN_POINT('Ctrl Pts',(7.651585124936,12.2,7.01766892464472));
#208708=CARTESIAN_POINT('Ctrl Pts',(7.65290158847099,12.2,7.01912907727743));
#208709=CARTESIAN_POINT('Ctrl Pts',(7.65425083044716,12.2,7.02063486218735));
#208710=CARTESIAN_POINT('Ctrl Pts',(7.65560007230076,12.2,7.0221406469605));
#208711=CARTESIAN_POINT('Ctrl Pts',(7.65698209060125,12.2,7.02369206276625));
#208712=CARTESIAN_POINT('Ctrl Pts',(7.65839580954989,12.2,7.02528884145824));
#208713=CARTESIAN_POINT('Ctrl Pts',(7.65980952849853,12.2,7.02688562015022));
#208714=CARTESIAN_POINT('Ctrl Pts',(7.6612549458305,12.2,7.02852776000807));
#208715=CARTESIAN_POINT('Ctrl Pts',(7.66273101409884,12.2,7.0302149976118));
#208716=CARTESIAN_POINT('Ctrl Pts',(7.66420708250127,12.2,7.03190223536877));
#208717=CARTESIAN_POINT('Ctrl Pts',(7.66571380242329,12.2,7.03363456911039));
#208718=CARTESIAN_POINT('Ctrl Pts',(7.6672501549257,12.2,7.0354117382103));
#208719=CARTESIAN_POINT('Ctrl Pts',(7.66904256596918,12.2,7.03748510191804));
#208720=CARTESIAN_POINT('Ctrl Pts',(7.67087531161421,12.2,7.03961949183139));
#208721=CARTESIAN_POINT('Ctrl Pts',(7.67274682060312,12.2,7.04181450134301));
#208722=CARTESIAN_POINT('Ctrl Pts',(7.67435097135238,12.2,7.04369593828699));
#208723=CARTESIAN_POINT('Ctrl Pts',(7.67598360497184,12.2,7.04562191207094));
#208724=CARTESIAN_POINT('Ctrl Pts',(7.67764376073086,12.2,7.04759217001468));
#208725=CARTESIAN_POINT('Ctrl Pts',(7.67930391633907,12.2,7.04956242777943));
#208726=CARTESIAN_POINT('Ctrl Pts',(7.68099159523845,12.2,7.0515769702162));
#208727=CARTESIAN_POINT('Ctrl Pts',(7.68270586501735,12.2,7.05363554898419));
#208728=CARTESIAN_POINT('Ctrl Pts',(7.68442013479623,12.2,7.05569412775218));
#208729=CARTESIAN_POINT('Ctrl Pts',(7.68616099674403,12.2,7.05779674259634));
#208730=CARTESIAN_POINT('Ctrl Pts',(7.6879275415954,12.2,7.05994315018311));
#208731=CARTESIAN_POINT('Ctrl Pts',(7.68969408660721,12.2,7.06208955796484));
#208732=CARTESIAN_POINT('Ctrl Pts',(7.69148631527225,12.2,7.06427975580202));
#208733=CARTESIAN_POINT('Ctrl Pts',(7.69330334245629,12.2,7.06651350476006));
#208734=CARTESIAN_POINT('Ctrl Pts',(7.6951203694753,12.2,7.06874725351521));
#208735=CARTESIAN_POINT('Ctrl Pts',(7.69696219657678,12.2,7.07102455272568));
#208736=CARTESIAN_POINT('Ctrl Pts',(7.69882796059335,12.2,7.07334516364323));
#208737=CARTESIAN_POINT('Ctrl Pts',(7.70069372460993,12.2,7.07566577456079));
#208738=CARTESIAN_POINT('Ctrl Pts',(7.7025834273496,12.2,7.07802969765826));
#208739=CARTESIAN_POINT('Ctrl Pts',(7.70449622661242,12.2,7.08043669840224));
#208740=CARTESIAN_POINT('Ctrl Pts',(7.70640902587524,12.2,7.08284369914623));
#208741=CARTESIAN_POINT('Ctrl Pts',(7.70834492374246,12.2,7.08529377607167));
#208742=CARTESIAN_POINT('Ctrl Pts',(7.71030309983647,12.2,7.08778669797819));
#208743=CARTESIAN_POINT('Ctrl Pts',(7.71226127610836,12.2,7.09027962011115));
#208744=CARTESIAN_POINT('Ctrl Pts',(7.71424172989907,12.2,7.09281538834824));
#208745=CARTESIAN_POINT('Ctrl Pts',(7.71624366334244,12.2,7.09539376965728));
#208746=CARTESIAN_POINT('Ctrl Pts',(7.71824559660397,12.2,7.09797215073212));
#208747=CARTESIAN_POINT('Ctrl Pts',(7.72026900951376,12.2,7.10059314884521));
#208748=CARTESIAN_POINT('Ctrl Pts',(7.72231311993858,12.2,7.10325653466326));
#208749=CARTESIAN_POINT('Ctrl Pts',(7.72435723036339,12.2,7.1059199204813));
#208750=CARTESIAN_POINT('Ctrl Pts',(7.7264220398831,12.2,7.1086256945531));
#208751=CARTESIAN_POINT('Ctrl Pts',(7.72850678630601,12.2,7.1113736324504));
#208752=CARTESIAN_POINT('Ctrl Pts',(7.73059153291827,12.2,7.1141215705973));
#208753=CARTESIAN_POINT('Ctrl Pts',(7.73269621517416,12.2,7.1169116723566));
#208754=CARTESIAN_POINT('Ctrl Pts',(7.73482009087407,12.2,7.11974371642943));
#208755=CARTESIAN_POINT('Ctrl Pts',(7.73694396638108,12.2,7.12257576024503));
#208756=CARTESIAN_POINT('Ctrl Pts',(7.73908703397603,12.2,7.12544974549974));
#208757=CARTESIAN_POINT('Ctrl Pts',(7.7412485664906,12.2,7.12836545249026));
#208758=CARTESIAN_POINT('Ctrl Pts',(7.74341009900516,12.2,7.13128115948078));
#208759=CARTESIAN_POINT('Ctrl Pts',(7.74559009592475,12.2,7.13423858848483));
#208760=CARTESIAN_POINT('Ctrl Pts',(7.74778784751036,12.2,7.13723752237304));
#208761=CARTESIAN_POINT('Ctrl Pts',(7.7499855992956,12.2,7.14023645653366));
#208762=CARTESIAN_POINT('Ctrl Pts',(7.7522011038984,12.2,7.14327689414883));
#208763=CARTESIAN_POINT('Ctrl Pts',(7.75443366796593,12.2,7.14635862055647));
#208764=CARTESIAN_POINT('Ctrl Pts',(7.75666623183067,12.2,7.14944034668418));
#208765=CARTESIAN_POINT('Ctrl Pts',(7.75891585274889,12.2,7.15256336313986));
#208766=CARTESIAN_POINT('Ctrl Pts',(7.76118185349991,12.2,7.1557274512749));
#208767=CARTESIAN_POINT('Ctrl Pts',(7.76344785425091,12.2,7.15889153940993));
#208768=CARTESIAN_POINT('Ctrl Pts',(7.76573023273056,12.2,7.16209670508579));
#208769=CARTESIAN_POINT('Ctrl Pts',(7.76802832376098,12.2,7.16534273221101));
#208770=CARTESIAN_POINT('Ctrl Pts',(7.76994339968924,12.2,7.16804775491364));
#208771=CARTESIAN_POINT('Ctrl Pts',(7.77186938791277,12.2,7.17078115509872));
#208772=CARTESIAN_POINT('Ctrl Pts',(7.77380591110667,12.2,7.17354281086114));
#208773=CARTESIAN_POINT('Ctrl Pts',(7.77574243430056,12.2,7.17630446662355));
#208774=CARTESIAN_POINT('Ctrl Pts',(7.77768948963916,12.2,7.17909437795613));
#208775=CARTESIAN_POINT('Ctrl Pts',(7.77964670963864,12.2,7.18191242302411));
#208776=CARTESIAN_POINT('Ctrl Pts',(7.78160392963811,12.2,7.18473046809209));
#208777=CARTESIAN_POINT('Ctrl Pts',(7.78357131293986,12.2,7.1875766477409));
#208778=CARTESIAN_POINT('Ctrl Pts',(7.7855484939905,12.2,7.19045084199001));
#208779=CARTESIAN_POINT('Ctrl Pts',(7.78752567504114,12.2,7.19332503623913));
#208780=CARTESIAN_POINT('Ctrl Pts',(7.78951265511659,12.2,7.19622724573881));
#208781=CARTESIAN_POINT('Ctrl Pts',(7.79150907449159,12.2,7.19915734997492));
#208782=CARTESIAN_POINT('Ctrl Pts',(7.79350549386659,12.2,7.20208745421102));
#208783=CARTESIAN_POINT('Ctrl Pts',(7.79551135437518,12.2,7.20504545453235));
#208784=CARTESIAN_POINT('Ctrl Pts',(7.79752630125935,12.2,7.20803123051821));
#208785=CARTESIAN_POINT('Ctrl Pts',(7.79954124814353,12.2,7.21101700650407));
#208786=CARTESIAN_POINT('Ctrl Pts',(7.80156528407135,12.2,7.21403056018642));
#208787=CARTESIAN_POINT('Ctrl Pts',(7.80359806018291,12.2,7.21707177192397));
#208788=CARTESIAN_POINT('Ctrl Pts',(7.80563083629447,12.2,7.22011298366151));
#208789=CARTESIAN_POINT('Ctrl Pts',(7.8076723534336,12.2,7.22318185512338));
#208790=CARTESIAN_POINT('Ctrl Pts',(7.80972227114237,12.2,7.22627826769426));
#208791=CARTESIAN_POINT('Ctrl Pts',(7.81177218885114,12.2,7.22937468026514));
#208792=CARTESIAN_POINT('Ctrl Pts',(7.81383050728048,12.2,7.23249863385094));
#208793=CARTESIAN_POINT('Ctrl Pts',(7.8158968902315,12.2,7.23565001331584));
#208794=CARTESIAN_POINT('Ctrl Pts',(7.81796327318252,12.2,7.23880139278073));
#208795=CARTESIAN_POINT('Ctrl Pts',(7.82003772232163,12.2,7.24198019770035));
#208796=CARTESIAN_POINT('Ctrl Pts',(7.82211990607227,12.2,7.24518631270261));
#208797=CARTESIAN_POINT('Ctrl Pts',(7.82420208982293,12.2,7.24839242770487));
#208798=CARTESIAN_POINT('Ctrl Pts',(7.82629200866811,12.2,7.25162584982421));
#208799=CARTESIAN_POINT('Ctrl Pts',(7.82838933901592,12.2,7.25488646815974));
#208800=CARTESIAN_POINT('Ctrl Pts',(7.83048666913513,12.2,7.25814708613988));
#208801=CARTESIAN_POINT('Ctrl Pts',(7.83259141061558,12.2,7.26143489787432));
#208802=CARTESIAN_POINT('Ctrl Pts',(7.83470324323203,12.2,7.26474978931634));
#208803=CARTESIAN_POINT('Ctrl Pts',(7.83681507607868,12.2,7.26806468111968));
#208804=CARTESIAN_POINT('Ctrl Pts',(7.838934000078,12.2,7.27140665212259));
#208805=CARTESIAN_POINT('Ctrl Pts',(7.84105970202189,12.2,7.27477558955094));
#208806=CARTESIAN_POINT('Ctrl Pts',(7.84318540396578,12.2,7.2781445269793));
#208807=CARTESIAN_POINT('Ctrl Pts',(7.84531788187068,12.2,7.28154042878775));
#208808=CARTESIAN_POINT('Ctrl Pts',(7.84745682895349,12.2,7.28496318378556));
#208809=CARTESIAN_POINT('Ctrl Pts',(7.84959577603629,12.2,7.28838593878337));
#208810=CARTESIAN_POINT('Ctrl Pts',(7.85174119018754,12.2,7.29183554507461));
#208811=CARTESIAN_POINT('Ctrl Pts',(7.85389276751685,12.2,7.29531189107979));
#208812=CARTESIAN_POINT('Ctrl Pts',(7.85604434484615,12.2,7.29878823708496));
#208813=CARTESIAN_POINT('Ctrl Pts',(7.85820208679766,12.2,7.30229132324841));
#208814=CARTESIAN_POINT('Ctrl Pts',(7.8603656906168,12.2,7.30582103505257));
#208815=CARTESIAN_POINT('Ctrl Pts',(7.86252929443594,12.2,7.30935074685673));
#208816=CARTESIAN_POINT('Ctrl Pts',(7.86469876169133,12.2,7.31290708506158));
#208817=CARTESIAN_POINT('Ctrl Pts',(7.86687379564938,12.2,7.31648993853243));
#208818=CARTESIAN_POINT('Ctrl Pts',(7.86861382291065,12.2,7.31935622146531));
#208819=CARTESIAN_POINT('Ctrl Pts',(7.87035741479566,12.2,7.32223947390253));
#208820=CARTESIAN_POINT('Ctrl Pts',(7.87210441947845,12.2,7.32513963892918));
#208821=CARTESIAN_POINT('Ctrl Pts',(7.87385142392321,12.2,7.32803980356069));
#208822=CARTESIAN_POINT('Ctrl Pts',(7.8756018424724,12.2,7.33095688124006));
#208823=CARTESIAN_POINT('Ctrl Pts',(7.8773555281066,12.2,7.3338908137769));
#208824=CARTESIAN_POINT('Ctrl Pts',(7.87954763532857,12.2,7.33755822974776));
#208825=CARTESIAN_POINT('Ctrl Pts',(7.88174484555065,12.2,7.34125198203039));
#208826=CARTESIAN_POINT('Ctrl Pts',(7.88394687610595,12.2,7.34497196126512));
#208827=CARTESIAN_POINT('Ctrl Pts',(7.88570850064619,12.2,7.3479479448151));
#208828=CARTESIAN_POINT('Ctrl Pts',(7.88747320806044,12.2,7.35094071321255));
#208829=CARTESIAN_POINT('Ctrl Pts',(7.88924085802311,12.2,7.35395020969504));
#208830=CARTESIAN_POINT('Ctrl Pts',(7.89100850774494,12.2,7.35695970576748));
#208831=CARTESIAN_POINT('Ctrl Pts',(7.89277909921404,12.2,7.35998593028729));
#208832=CARTESIAN_POINT('Ctrl Pts',(7.89455248834665,12.2,7.36302882675965));
#208833=CARTESIAN_POINT('Ctrl Pts',(7.89632587772089,12.2,7.3660717236466));
#208834=CARTESIAN_POINT('Ctrl Pts',(7.89810206741491,12.2,7.36913129288557));
#208835=CARTESIAN_POINT('Ctrl Pts',(7.89988091417871,12.2,7.37220747777655));
#208836=CARTESIAN_POINT('Ctrl Pts',(7.90165976070015,12.2,7.37528366224841));
#208837=CARTESIAN_POINT('Ctrl Pts',(7.90344126715913,12.2,7.37837646275746));
#208838=CARTESIAN_POINT('Ctrl Pts',(7.90522529299107,12.2,7.38148582282382));
#208839=CARTESIAN_POINT('Ctrl Pts',(7.9074553254633,12.2,7.38537252322448));
#208840=CARTESIAN_POINT('Ctrl Pts',(7.90968929562603,12.2,7.38928510072164));
#208841=CARTESIAN_POINT('Ctrl Pts',(7.91192693465361,12.2,7.39322344252584));
#208842=CARTESIAN_POINT('Ctrl Pts',(7.91371704597325,12.2,7.39637411614091));
#208843=CARTESIAN_POINT('Ctrl Pts',(7.91550950582929,12.2,7.39954128067188));
#208844=CARTESIAN_POINT('Ctrl Pts',(7.91730417987167,12.2,7.40272488023534));
#208845=CARTESIAN_POINT('Ctrl Pts',(7.91909885366954,12.2,7.40590847936502));
#208846=CARTESIAN_POINT('Ctrl Pts',(7.9208957400185,12.2,7.40910851331197));
#208847=CARTESIAN_POINT('Ctrl Pts',(7.9226947077389,12.2,7.41232492604162));
#208848=CARTESIAN_POINT('Ctrl Pts',(7.92449367570441,12.2,7.4155413392095));
#208849=CARTESIAN_POINT('Ctrl Pts',(7.92629472271841,12.2,7.41877413329589));
#208850=CARTESIAN_POINT('Ctrl Pts',(7.92809771687235,12.2,7.42202325030735));
#208851=CARTESIAN_POINT('Ctrl Pts',(7.92990071078063,12.2,7.42527236687613));
#208852=CARTESIAN_POINT('Ctrl Pts',(7.93170565305519,12.2,7.42853780804164));
#208853=CARTESIAN_POINT('Ctrl Pts',(7.93351241096287,12.2,7.43181951793837));
#208854=CARTESIAN_POINT('Ctrl Pts',(7.9353191691167,12.2,7.43510122828223));
#208855=CARTESIAN_POINT('Ctrl Pts',(7.93712774563038,12.2,7.4383992087592));
#208856=CARTESIAN_POINT('Ctrl Pts',(7.93893800845951,12.2,7.44171340301052));
#208857=CARTESIAN_POINT('Ctrl Pts',(7.94074827104199,12.2,7.44502759681029));
#208858=CARTESIAN_POINT('Ctrl Pts',(7.94256022076295,12.2,7.44835800444743));
#208859=CARTESIAN_POINT('Ctrl Pts',(7.94437373117009,12.2,7.45170457222776));
#208860=CARTESIAN_POINT('Ctrl Pts',(7.94618724182433,12.2,7.45505114046406));
#208861=CARTESIAN_POINT('Ctrl Pts',(7.94800231055372,12.2,7.45841386751855));
#208862=CARTESIAN_POINT('Ctrl Pts',(7.94981881270827,12.2,7.46179269975825));
#208863=CARTESIAN_POINT('Ctrl Pts',(7.95163531486283,12.2,7.46517153199795));
#208864=CARTESIAN_POINT('Ctrl Pts',(7.95345325059811,12.2,7.46856646850622));
#208865=CARTESIAN_POINT('Ctrl Pts',(7.95527249403072,12.2,7.47197745608263));
#208866=CARTESIAN_POINT('Ctrl Pts',(7.95754654794967,12.2,7.47624118985601));
#208867=CARTESIAN_POINT('Ctrl Pts',(7.95982264504489,12.2,7.48053000209685));
#208868=CARTESIAN_POINT('Ctrl Pts',(7.96210054326866,12.2,7.48484378669403));
#208869=CARTESIAN_POINT('Ctrl Pts',(7.96392286214562,12.2,7.488294814936));
#208870=CARTESIAN_POINT('Ctrl Pts',(7.96574633502549,12.2,7.49176182528228));
#208871=CARTESIAN_POINT('Ctrl Pts',(7.96757083795827,12.2,7.49524476424992));
#208872=CARTESIAN_POINT('Ctrl Pts',(7.96939534089106,12.2,7.49872770321755));
#208873=CARTESIAN_POINT('Ctrl Pts',(7.97122087518504,12.2,7.5022265706203));
#208874=CARTESIAN_POINT('Ctrl Pts',(7.97304731934023,12.2,7.50574131159126));
#208875=CARTESIAN_POINT('Ctrl Pts',(7.97487376324658,12.2,7.50925605208334));
#208876=CARTESIAN_POINT('Ctrl Pts',(7.97670111759539,12.2,7.51278666650468));
#208877=CARTESIAN_POINT('Ctrl Pts',(7.97852926156537,12.2,7.51633310223085));
#208878=CARTESIAN_POINT('Ctrl Pts',(7.98035740578443,12.2,7.51987953844023));
#208879=CARTESIAN_POINT('Ctrl Pts',(7.98218634003541,12.2,7.5234417933411));
#208880=CARTESIAN_POINT('Ctrl Pts',(7.98401594752408,12.2,7.52701981559327));
#208881=CARTESIAN_POINT('Ctrl Pts',(7.98584555476348,12.2,7.53059783735794));
#208882=CARTESIAN_POINT('Ctrl Pts',(7.98767583257221,12.2,7.5341916251761));
#208883=CARTESIAN_POINT('Ctrl Pts',(7.98950666586694,12.2,7.53780112571333));
#208884=CARTESIAN_POINT('Ctrl Pts',(7.99133749941114,12.2,7.54141062674235));
#208885=CARTESIAN_POINT('Ctrl Pts',(7.99316888807762,12.2,7.54503584072326));
#208886=CARTESIAN_POINT('Ctrl Pts',(7.9950007143997,12.2,7.54867671375605));
#208887=CARTESIAN_POINT('Ctrl Pts',(7.9968325404722,12.2,7.55231758629278));
#208888=CARTESIAN_POINT('Ctrl Pts',(7.99866480683119,12.2,7.55597411842136));
#208889=CARTESIAN_POINT('Ctrl Pts',(8.00049739621736,12.2,7.55964625569216));
#208890=CARTESIAN_POINT('Ctrl Pts',(8.00232998585321,12.2,7.56331839346329));
#208891=CARTESIAN_POINT('Ctrl Pts',(8.00416289929155,12.2,7.56700613793053));
#208892=CARTESIAN_POINT('Ctrl Pts',(8.00599602289147,12.2,7.57070943307782));
#208893=CARTESIAN_POINT('Ctrl Pts',(8.00782914624163,12.2,7.57441272772054));
#208894=CARTESIAN_POINT('Ctrl Pts',(8.00966247936952,12.2,7.57813157536289));
#208895=CARTESIAN_POINT('Ctrl Pts',(8.01149591194184,12.2,7.58186592238936));
#208896=CARTESIAN_POINT('Ctrl Pts',(8.01332934476397,12.2,7.58560026992463));
#208897=CARTESIAN_POINT('Ctrl Pts',(8.01516287297628,12.2,7.58935011622459));
#208898=CARTESIAN_POINT('Ctrl Pts',(8.01699638975119,12.2,7.59311540800249));
#208899=CARTESIAN_POINT('Ctrl Pts',(8.01882990627629,12.2,7.59688069926738));
#208900=CARTESIAN_POINT('Ctrl Pts',(8.0206634080584,12.2,7.60066143764954));
#208901=CARTESIAN_POINT('Ctrl Pts',(8.02249678674186,12.2,7.60445756817093));
#208902=CARTESIAN_POINT('Ctrl Pts',(8.0243301656751,12.2,7.60825369920954));
#208903=CARTESIAN_POINT('Ctrl Pts',(8.02616342036114,12.2,7.61206522297743));
#208904=CARTESIAN_POINT('Ctrl Pts',(8.02799644201661,12.2,7.61589208724159));
#208905=CARTESIAN_POINT('Ctrl Pts',(8.02982946367209,12.2,7.61971895150575));
#208906=CARTESIAN_POINT('Ctrl Pts',(8.03166225341084,12.2,7.6235611560383));
#208907=CARTESIAN_POINT('Ctrl Pts',(8.03349470106622,12.2,7.62741864763897));
#208908=CARTESIAN_POINT('Ctrl Pts',(8.03532714847193,12.2,7.63127613871406));
#208909=CARTESIAN_POINT('Ctrl Pts',(8.03715925420401,12.2,7.63514891615031));
#208910=CARTESIAN_POINT('Ctrl Pts',(8.03899091300703,12.2,7.63903692923895));
#208911=CARTESIAN_POINT('Ctrl Pts',(8.04082257205961,12.2,7.64292494285733));
#208912=CARTESIAN_POINT('Ctrl Pts',(8.04265378265511,12.2,7.64682819023105));
#208913=CARTESIAN_POINT('Ctrl Pts',(8.04448443953259,12.2,7.6507466198906));
#208914=CARTESIAN_POINT('Ctrl Pts',(8.04631509616065,12.2,7.65466504901625));
#208915=CARTESIAN_POINT('Ctrl Pts',(8.04814519769434,12.2,7.65859865970659));
#208916=CARTESIAN_POINT('Ctrl Pts',(8.04997464110038,12.2,7.66254740016059));
#208917=CARTESIAN_POINT('Ctrl Pts',(8.05180408475569,12.2,7.6664961411526));
#208918=CARTESIAN_POINT('Ctrl Pts',(8.05363286995487,12.2,7.67046001176599));
#208919=CARTESIAN_POINT('Ctrl Pts',(8.05546089175687,12.2,7.67443895962738));
#208920=CARTESIAN_POINT('Ctrl Pts',(8.05728891330979,12.2,7.67841790694665));
#208921=CARTESIAN_POINT('Ctrl Pts',(8.05911617138044,12.2,7.68241192940106));
#208922=CARTESIAN_POINT('Ctrl Pts',(8.06094256417563,12.2,7.68642097840566));
#208923=CARTESIAN_POINT('Ctrl Pts',(8.06322555535625,12.2,7.69143229007108));
#208924=CARTESIAN_POINT('Ctrl Pts',(8.06550719342852,12.2,7.69646707774827));
#208925=CARTESIAN_POINT('Ctrl Pts',(8.06778727960916,12.2,7.70152523871927));
#208926=CARTESIAN_POINT('Ctrl Pts',(8.06915533126784,12.2,7.7045601351916));
#208927=CARTESIAN_POINT('Ctrl Pts',(8.07052282405012,12.2,7.70760344580231));
#208928=CARTESIAN_POINT('Ctrl Pts',(8.07188971627715,12.2,7.71065515038458));
#208929=CARTESIAN_POINT('Ctrl Pts',(8.07325660850417,12.2,7.71370685496685));
#208930=CARTESIAN_POINT('Ctrl Pts',(8.07462289946845,12.2,7.71676695219367));
#208931=CARTESIAN_POINT('Ctrl Pts',(8.07598854666891,12.2,7.71983542012268));
#208932=CARTESIAN_POINT('Ctrl Pts',(8.07735419411745,12.2,7.72290388860913));
#208933=CARTESIAN_POINT('Ctrl Pts',(8.07871919794917,12.2,7.72598072705629));
#208934=CARTESIAN_POINT('Ctrl Pts',(8.08008351727237,12.2,7.7290659141725));
#208935=CARTESIAN_POINT('Ctrl Pts',(8.08144783634771,12.2,7.73215110072822));
#208936=CARTESIAN_POINT('Ctrl Pts',(8.08281146933141,12.2,7.73524463731681));
#208937=CARTESIAN_POINT('Ctrl Pts',(8.08417437590682,12.2,7.7383464998715));
#208938=CARTESIAN_POINT('Ctrl Pts',(8.08553728248225,12.2,7.74144836242619));
#208939=CARTESIAN_POINT('Ctrl Pts',(8.08689946139447,12.2,7.74455855193521));
#208940=CARTESIAN_POINT('Ctrl Pts',(8.08826087255952,12.2,7.7476770464611));
#208941=CARTESIAN_POINT('Ctrl Pts',(8.08962228372457,12.2,7.750795540987));
#208942=CARTESIAN_POINT('Ctrl Pts',(8.09098292644194,12.2,7.75392234161348));
#208943=CARTESIAN_POINT('Ctrl Pts',(8.09234275923205,12.2,7.75705742505541));
#208944=CARTESIAN_POINT('Ctrl Pts',(8.09370259202214,12.2,7.76019250849735));
#208945=CARTESIAN_POINT('Ctrl Pts',(8.09506161636783,12.2,7.7633358736551));
#208946=CARTESIAN_POINT('Ctrl Pts',(8.09641979011023,12.2,7.76648750108154));
#208947=CARTESIAN_POINT('Ctrl Pts',(8.09777796385263,12.2,7.76963912850798));
#208948=CARTESIAN_POINT('Ctrl Pts',(8.09913528768675,12.2,7.77279901692553));
#208949=CARTESIAN_POINT('Ctrl Pts',(8.10049172042925,12.2,7.77596714535094));
#208950=CARTESIAN_POINT('Ctrl Pts',(8.10184815341816,12.2,7.7791352743519));
#208951=CARTESIAN_POINT('Ctrl Pts',(8.10320369583185,12.2,7.78231164311356));
#208952=CARTESIAN_POINT('Ctrl Pts',(8.10455830727859,12.2,7.78549622920251));
#208953=CARTESIAN_POINT('Ctrl Pts',(8.10591291847924,12.2,7.78868081471293));
#208954=CARTESIAN_POINT('Ctrl Pts',(8.10726659877667,12.2,7.79187361799144));
#208955=CARTESIAN_POINT('Ctrl Pts',(8.10861930850333,12.2,7.79507461761933));
#208956=CARTESIAN_POINT('Ctrl Pts',(8.10997201822998,12.2,7.79827561724721));
#208957=CARTESIAN_POINT('Ctrl Pts',(8.111323756463,12.2,7.80148481265029));
#208958=CARTESIAN_POINT('Ctrl Pts',(8.11267448466383,12.2,7.80470218261743));
#208959=CARTESIAN_POINT('Ctrl Pts',(8.11402521286466,12.2,7.80791955258457));
#208960=CARTESIAN_POINT('Ctrl Pts',(8.11537493099896,12.2,7.81114509646744));
#208961=CARTESIAN_POINT('Ctrl Pts',(8.11672359878329,12.2,7.81437879297494));
#208962=CARTESIAN_POINT('Ctrl Pts',(8.11807226656762,12.2,7.81761248948244));
#208963=CARTESIAN_POINT('Ctrl Pts',(8.11941988475199,12.2,7.82085433943129));
#208964=CARTESIAN_POINT('Ctrl Pts',(8.12076641357816,12.2,7.82410431943747));
#208965=CARTESIAN_POINT('Ctrl Pts',(8.12211294240431,12.2,7.82735429944365));
#208966=CARTESIAN_POINT('Ctrl Pts',(8.12345838307142,12.2,7.83061241020787));
#208967=CARTESIAN_POINT('Ctrl Pts',(8.12480269496485,12.2,7.83387863087641));
#208968=CARTESIAN_POINT('Ctrl Pts',(8.12614700685828,12.2,7.83714485154495));
#208969=CARTESIAN_POINT('Ctrl Pts',(8.127490191656,12.2,7.84041918177142));
#208970=CARTESIAN_POINT('Ctrl Pts',(8.12883220944072,12.2,7.84370159927603));
#208971=CARTESIAN_POINT('Ctrl Pts',(8.13017422746924,12.2,7.84698401737694));
#208972=CARTESIAN_POINT('Ctrl Pts',(8.13151507974747,12.2,7.85027452337188));
#208973=CARTESIAN_POINT('Ctrl Pts',(8.132854726317,12.2,7.85357309497736));
#208974=CARTESIAN_POINT('Ctrl Pts',(8.13419437264315,12.2,7.85687166598359));
#208975=CARTESIAN_POINT('Ctrl Pts',(8.13553281519438,12.2,7.86017830314777));
#208976=CARTESIAN_POINT('Ctrl Pts',(8.13687001489569,12.2,7.86349298511137));
#208977=CARTESIAN_POINT('Ctrl Pts',(8.13820721459699,12.2,7.86680766707496));
#208978=CARTESIAN_POINT('Ctrl Pts',(8.13954317003178,12.2,7.8701303932376));
#208979=CARTESIAN_POINT('Ctrl Pts',(8.14087784573329,12.2,7.87346114224159));
#208980=CARTESIAN_POINT('Ctrl Pts',(8.1422125214348,12.2,7.87679189124558));
#208981=CARTESIAN_POINT('Ctrl Pts',(8.14354591668635,12.2,7.8801306636409));
#208982=CARTESIAN_POINT('Ctrl Pts',(8.14487799388807,12.2,7.8834774371436));
#208983=CARTESIAN_POINT('Ctrl Pts',(8.14621007108978,12.2,7.88682421064629));
#208984=CARTESIAN_POINT('Ctrl Pts',(8.14754082972447,12.2,7.89017898543784));
#208985=CARTESIAN_POINT('Ctrl Pts',(8.1488702335344,12.2,7.89354174056606));
#208986=CARTESIAN_POINT('Ctrl Pts',(8.15019963734433,12.2,7.89690449569427));
#208987=CARTESIAN_POINT('Ctrl Pts',(8.15152768557544,12.2,7.90027523033727));
#208988=CARTESIAN_POINT('Ctrl Pts',(8.15285434048574,12.2,7.90365392375505));
#208989=CARTESIAN_POINT('Ctrl Pts',(8.15418099563705,12.2,7.90703261778662));
#208990=CARTESIAN_POINT('Ctrl Pts',(8.15550625964635,12.2,7.91041926964552));
#208991=CARTESIAN_POINT('Ctrl Pts',(8.15683009325522,12.2,7.9138138587233));
#208992=CARTESIAN_POINT('Ctrl Pts',(8.15859520433289,12.2,7.91833997646585));
#208993=CARTESIAN_POINT('Ctrl Pts',(8.1603577744692,12.2,7.92288020446209));
#208994=CARTESIAN_POINT('Ctrl Pts',(8.16211771738106,12.2,7.92743449164442));
#208995=CARTESIAN_POINT('Ctrl Pts',(8.1634376746249,12.2,7.9308502071863));
#208996=CARTESIAN_POINT('Ctrl Pts',(8.16475615394368,12.2,7.93427383187358));
#208997=CARTESIAN_POINT('Ctrl Pts',(8.16607311925348,12.2,7.93770534304443));
#208998=CARTESIAN_POINT('Ctrl Pts',(8.16739008456327,12.2,7.94113685421527));
#208999=CARTESIAN_POINT('Ctrl Pts',(8.16870553462772,12.2,7.9445762523081));
#209000=CARTESIAN_POINT('Ctrl Pts',(8.17001943445519,12.2,7.94802351580676));
#209001=CARTESIAN_POINT('Ctrl Pts',(8.17133333452135,12.2,7.95147077993168));
#209002=CARTESIAN_POINT('Ctrl Pts',(8.17264568464542,12.2,7.95492590978386));
#209003=CARTESIAN_POINT('Ctrl Pts',(8.17395644825237,12.2,7.95838888345486));
#209004=CARTESIAN_POINT('Ctrl Pts',(8.17526721162119,12.2,7.96185185649677));
#209005=CARTESIAN_POINT('Ctrl Pts',(8.17657639007345,12.2,7.96532267422163));
#209006=CARTESIAN_POINT('Ctrl Pts',(8.17788394690078,12.2,7.96880131513757));
#209007=CARTESIAN_POINT('Ctrl Pts',(8.17919150372813,12.2,7.9722799560535));
#209008=CARTESIAN_POINT('Ctrl Pts',(8.18049743995927,12.2,7.97576641908082));
#209009=CARTESIAN_POINT('Ctrl Pts',(8.18180171875114,12.2,7.97926068446977));
#209010=CARTESIAN_POINT('Ctrl Pts',(8.1835407570613,12.2,7.98391970477677));
#209011=CARTESIAN_POINT('Ctrl Pts',(8.18527684736629,12.2,7.98859259344596));
#209012=CARTESIAN_POINT('Ctrl Pts',(8.18700990772493,12.2,7.99327929928366));
#209013=CARTESIAN_POINT('Ctrl Pts',(8.18830970328908,12.2,7.99679432946014));
#209014=CARTESIAN_POINT('Ctrl Pts',(8.18960779461107,12.2,8.00031713288879));
#209015=CARTESIAN_POINT('Ctrl Pts',(8.19090415025756,12.2,8.0038476895696));
#209016=CARTESIAN_POINT('Ctrl Pts',(8.19220050566854,12.2,8.00737824560902));
#209017=CARTESIAN_POINT('Ctrl Pts',(8.19349512717131,12.2,8.01091655543141));
#209018=CARTESIAN_POINT('Ctrl Pts',(8.19478797687418,12.2,8.01446259688659));
#209019=CARTESIAN_POINT('Ctrl Pts',(8.19608082657705,12.2,8.01800863834176));
#209020=CARTESIAN_POINT('Ctrl Pts',(8.1973719043088,12.2,8.02156241154971));
#209021=CARTESIAN_POINT('Ctrl Pts',(8.19866116751779,12.2,8.02512388901984));
#209022=CARTESIAN_POINT('Ctrl Pts',(8.20038018505172,12.2,8.029872525431));
#209023=CARTESIAN_POINT('Ctrl Pts',(8.20209597184851,12.2,8.03463485712204));
#209024=CARTESIAN_POINT('Ctrl Pts',(8.20380846548663,12.2,8.0394108439524));
#209025=CARTESIAN_POINT('Ctrl Pts',(8.20552095935807,12.2,8.04418683143348));
#209026=CARTESIAN_POINT('Ctrl Pts',(8.20723015620175,12.2,8.04897647635775));
#209027=CARTESIAN_POINT('Ctrl Pts',(8.20893606999994,12.2,8.05377977099998));
#209028=CARTESIAN_POINT('Ctrl Pts',(7.93573928199995,15.2,8.32310290899999));
#209029=CARTESIAN_POINT('Ctrl Pts',(7.93573928199995,11.6,8.32310290899999));
#209030=CARTESIAN_POINT('Ctrl Pts',(7.93502251599994,15.2,8.32283676099999));
#209031=CARTESIAN_POINT('Ctrl Pts',(7.93502251599994,11.6,8.32283676099999));
#209032=CARTESIAN_POINT('Ctrl Pts',(7.93358949599994,15.2,8.32230434799998));
#209033=CARTESIAN_POINT('Ctrl Pts',(7.93358949599994,11.6,8.32230434799998));
#209034=CARTESIAN_POINT('Ctrl Pts',(7.93144150699994,15.2,8.32150538099998));
#209035=CARTESIAN_POINT('Ctrl Pts',(7.93144150699994,11.6,8.32150538099998));
#209036=CARTESIAN_POINT('Ctrl Pts',(7.92858060299995,15.2,8.32043939299999));
#209037=CARTESIAN_POINT('Ctrl Pts',(7.92858060299995,11.6,8.32043939299999));
#209038=CARTESIAN_POINT('Ctrl Pts',(7.92500961099995,15.2,8.31910574599998));
#209039=CARTESIAN_POINT('Ctrl Pts',(7.92500961099995,11.6,8.31910574599998));
#209040=CARTESIAN_POINT('Ctrl Pts',(7.92144375599995,15.2,8.31777093699999));
#209041=CARTESIAN_POINT('Ctrl Pts',(7.92144375599995,11.6,8.31777093699999));
#209042=CARTESIAN_POINT('Ctrl Pts',(7.91788303999994,15.2,8.31643496899999));
#209043=CARTESIAN_POINT('Ctrl Pts',(7.91788303999994,11.6,8.31643496899999));
#209044=CARTESIAN_POINT('Ctrl Pts',(7.91432746599994,15.2,8.31509784499998));
#209045=CARTESIAN_POINT('Ctrl Pts',(7.91432746599994,11.6,8.31509784499998));
#209046=CARTESIAN_POINT('Ctrl Pts',(7.91077703599995,15.2,8.31375956799998));
#209047=CARTESIAN_POINT('Ctrl Pts',(7.91077703599995,11.6,8.31375956799998));
#209048=CARTESIAN_POINT('Ctrl Pts',(7.90723175399994,15.2,8.31242014699999));
#209049=CARTESIAN_POINT('Ctrl Pts',(7.90723175399994,11.6,8.31242014699999));
#209050=CARTESIAN_POINT('Ctrl Pts',(7.90369162499994,15.2,8.31107958999999));
#209051=CARTESIAN_POINT('Ctrl Pts',(7.90369162499994,11.6,8.31107958999999));
#209052=CARTESIAN_POINT('Ctrl Pts',(7.90015665599994,15.2,8.30973790699998));
#209053=CARTESIAN_POINT('Ctrl Pts',(7.90015665599994,11.6,8.30973790699998));
#209054=CARTESIAN_POINT('Ctrl Pts',(7.89662685099994,15.2,8.30839510599999));
#209055=CARTESIAN_POINT('Ctrl Pts',(7.89662685099994,11.6,8.30839510599999));
#209056=CARTESIAN_POINT('Ctrl Pts',(7.89310221699994,15.2,8.30705119899999));
#209057=CARTESIAN_POINT('Ctrl Pts',(7.89310221699994,11.6,8.30705119899999));
#209058=CARTESIAN_POINT('Ctrl Pts',(7.88958275899994,15.2,8.30570619199998));
#209059=CARTESIAN_POINT('Ctrl Pts',(7.88958275899994,11.6,8.30570619199998));
#209060=CARTESIAN_POINT('Ctrl Pts',(7.88606848099994,15.2,8.30436009499999));
#209061=CARTESIAN_POINT('Ctrl Pts',(7.88606848099994,11.6,8.30436009499999));
#209062=CARTESIAN_POINT('Ctrl Pts',(7.88255938799994,15.2,8.30301291499998));
#209063=CARTESIAN_POINT('Ctrl Pts',(7.88255938799994,11.6,8.30301291499998));
#209064=CARTESIAN_POINT('Ctrl Pts',(7.87905548499995,15.2,8.30166465799999));
#209065=CARTESIAN_POINT('Ctrl Pts',(7.87905548499995,11.6,8.30166465799999));
#209066=CARTESIAN_POINT('Ctrl Pts',(7.87555677499994,15.2,8.30031533399998));
#209067=CARTESIAN_POINT('Ctrl Pts',(7.87555677499994,11.6,8.30031533399998));
#209068=CARTESIAN_POINT('Ctrl Pts',(7.87206326199994,15.2,8.29896494699998));
#209069=CARTESIAN_POINT('Ctrl Pts',(7.87206326199994,11.6,8.29896494699998));
#209070=CARTESIAN_POINT('Ctrl Pts',(7.86857495099994,15.2,8.29761350399998));
#209071=CARTESIAN_POINT('Ctrl Pts',(7.86857495099994,11.6,8.29761350399998));
#209072=CARTESIAN_POINT('Ctrl Pts',(7.86509184699994,15.2,8.29626101599998));
#209073=CARTESIAN_POINT('Ctrl Pts',(7.86509184699994,11.6,8.29626101599998));
#209074=CARTESIAN_POINT('Ctrl Pts',(7.86161395399994,15.2,8.29490748799999));
#209075=CARTESIAN_POINT('Ctrl Pts',(7.86161395399994,11.6,8.29490748799999));
#209076=CARTESIAN_POINT('Ctrl Pts',(7.85814127699994,15.2,8.29355293099999));
#209077=CARTESIAN_POINT('Ctrl Pts',(7.85814127699994,11.6,8.29355293099999));
#209078=CARTESIAN_POINT('Ctrl Pts',(7.85467382099994,15.2,8.29219735099999));
#209079=CARTESIAN_POINT('Ctrl Pts',(7.85467382099994,11.6,8.29219735099999));
#209080=CARTESIAN_POINT('Ctrl Pts',(7.85121158999995,15.2,8.29084075499999));
#209081=CARTESIAN_POINT('Ctrl Pts',(7.85121158999995,11.6,8.29084075499999));
#209082=CARTESIAN_POINT('Ctrl Pts',(7.84775458999994,15.2,8.28948315499999));
#209083=CARTESIAN_POINT('Ctrl Pts',(7.84775458999994,11.6,8.28948315499999));
#209084=CARTESIAN_POINT('Ctrl Pts',(7.84430282499994,15.2,8.28812455699998));
#209085=CARTESIAN_POINT('Ctrl Pts',(7.84430282499994,11.6,8.28812455699998));
#209086=CARTESIAN_POINT('Ctrl Pts',(7.84085629899994,15.2,8.28676496699998));
#209087=CARTESIAN_POINT('Ctrl Pts',(7.84085629899994,11.6,8.28676496699998));
#209088=CARTESIAN_POINT('Ctrl Pts',(7.83741501799994,15.2,8.28540439599998));
#209089=CARTESIAN_POINT('Ctrl Pts',(7.83741501799994,11.6,8.28540439599998));
#209090=CARTESIAN_POINT('Ctrl Pts',(7.83397898499994,15.2,8.28404284999999));
#209091=CARTESIAN_POINT('Ctrl Pts',(7.83397898499994,11.6,8.28404284999999));
#209092=CARTESIAN_POINT('Ctrl Pts',(7.83054820599994,15.2,8.28268033699998));
#209093=CARTESIAN_POINT('Ctrl Pts',(7.83054820599994,11.6,8.28268033699998));
#209094=CARTESIAN_POINT('Ctrl Pts',(7.82712268399994,15.2,8.28131686599999));
#209095=CARTESIAN_POINT('Ctrl Pts',(7.82712268399994,11.6,8.28131686599999));
#209096=CARTESIAN_POINT('Ctrl Pts',(7.82370242499994,15.2,8.27995244399998));
#209097=CARTESIAN_POINT('Ctrl Pts',(7.82370242499994,11.6,8.27995244399998));
#209098=CARTESIAN_POINT('Ctrl Pts',(7.82028743299994,15.2,8.27858707999999));
#209099=CARTESIAN_POINT('Ctrl Pts',(7.82028743299994,11.6,8.27858707999999));
#209100=CARTESIAN_POINT('Ctrl Pts',(7.81687771299994,15.2,8.27722078099999));
#209101=CARTESIAN_POINT('Ctrl Pts',(7.81687771299994,11.6,8.27722078099999));
#209102=CARTESIAN_POINT('Ctrl Pts',(7.81347326899994,15.2,8.27585355599999));
#209103=CARTESIAN_POINT('Ctrl Pts',(7.81347326899994,11.6,8.27585355599999));
#209104=CARTESIAN_POINT('Ctrl Pts',(7.81007410599995,15.2,8.27448541299999));
#209105=CARTESIAN_POINT('Ctrl Pts',(7.81007410599995,11.6,8.27448541299999));
#209106=CARTESIAN_POINT('Ctrl Pts',(7.80668022999994,15.2,8.27311635999998));
#209107=CARTESIAN_POINT('Ctrl Pts',(7.80668022999994,11.6,8.27311635999998));
#209108=CARTESIAN_POINT('Ctrl Pts',(7.80329164299994,15.2,8.27174640599999));
#209109=CARTESIAN_POINT('Ctrl Pts',(7.80329164299994,11.6,8.27174640599999));
#209110=CARTESIAN_POINT('Ctrl Pts',(7.79990835199994,15.2,8.27037555699999));
#209111=CARTESIAN_POINT('Ctrl Pts',(7.79990835199994,11.6,8.27037555699999));
#209112=CARTESIAN_POINT('Ctrl Pts',(7.79653035999995,15.2,8.26900382299998));
#209113=CARTESIAN_POINT('Ctrl Pts',(7.79653035999995,11.6,8.26900382299998));
#209114=CARTESIAN_POINT('Ctrl Pts',(7.79315767399994,15.2,8.26763121299999));
#209115=CARTESIAN_POINT('Ctrl Pts',(7.79315767399994,11.6,8.26763121299999));
#209116=CARTESIAN_POINT('Ctrl Pts',(7.78979029499994,15.2,8.26625773199999));
#209117=CARTESIAN_POINT('Ctrl Pts',(7.78979029499994,11.6,8.26625773199999));
#209118=CARTESIAN_POINT('Ctrl Pts',(7.78642823099994,15.2,8.26488339199998));
#209119=CARTESIAN_POINT('Ctrl Pts',(7.78642823099994,11.6,8.26488339199998));
#209120=CARTESIAN_POINT('Ctrl Pts',(7.78307148499994,15.2,8.26350819899999));
#209121=CARTESIAN_POINT('Ctrl Pts',(7.78307148499994,11.6,8.26350819899999));
#209122=CARTESIAN_POINT('Ctrl Pts',(7.77972006199994,15.2,8.26213216099998));
#209123=CARTESIAN_POINT('Ctrl Pts',(7.77972006199994,11.6,8.26213216099998));
#209124=CARTESIAN_POINT('Ctrl Pts',(7.77637396599994,15.2,8.26075528899998));
#209125=CARTESIAN_POINT('Ctrl Pts',(7.77637396599994,11.6,8.26075528899998));
#209126=CARTESIAN_POINT('Ctrl Pts',(7.77303320299994,15.2,8.25937758799999));
#209127=CARTESIAN_POINT('Ctrl Pts',(7.77303320299994,11.6,8.25937758799999));
#209128=CARTESIAN_POINT('Ctrl Pts',(7.76969777599994,15.2,8.25799906799999));
#209129=CARTESIAN_POINT('Ctrl Pts',(7.76969777599994,11.6,8.25799906799999));
#209130=CARTESIAN_POINT('Ctrl Pts',(7.76636769199994,15.2,8.25661973599999));
#209131=CARTESIAN_POINT('Ctrl Pts',(7.76636769199994,11.6,8.25661973599999));
#209132=CARTESIAN_POINT('Ctrl Pts',(7.76304295399994,15.2,8.25523960299999));
#209133=CARTESIAN_POINT('Ctrl Pts',(7.76304295399994,11.6,8.25523960299999));
#209134=CARTESIAN_POINT('Ctrl Pts',(7.75972356599994,15.2,8.25385867599999));
#209135=CARTESIAN_POINT('Ctrl Pts',(7.75972356599994,11.6,8.25385867599999));
#209136=CARTESIAN_POINT('Ctrl Pts',(7.75640953399995,15.2,8.25247696299999));
#209137=CARTESIAN_POINT('Ctrl Pts',(7.75640953399995,11.6,8.25247696299999));
#209138=CARTESIAN_POINT('Ctrl Pts',(7.75310086299994,15.2,8.25109447199999));
#209139=CARTESIAN_POINT('Ctrl Pts',(7.75310086299994,11.6,8.25109447199999));
#209140=CARTESIAN_POINT('Ctrl Pts',(7.74979755699994,15.2,8.24971121299999));
#209141=CARTESIAN_POINT('Ctrl Pts',(7.74979755699994,11.6,8.24971121299999));
#209142=CARTESIAN_POINT('Ctrl Pts',(7.74649961999994,15.2,8.24832719199998));
#209143=CARTESIAN_POINT('Ctrl Pts',(7.74649961999994,11.6,8.24832719199998));
#209144=CARTESIAN_POINT('Ctrl Pts',(7.74320705699994,15.2,8.24694242099999));
#209145=CARTESIAN_POINT('Ctrl Pts',(7.74320705699994,11.6,8.24694242099999));
#209146=CARTESIAN_POINT('Ctrl Pts',(7.73991987299994,15.2,8.24555690599999));
#209147=CARTESIAN_POINT('Ctrl Pts',(7.73991987299994,11.6,8.24555690599999));
#209148=CARTESIAN_POINT('Ctrl Pts',(7.73663807299994,15.2,8.24417065699999));
#209149=CARTESIAN_POINT('Ctrl Pts',(7.73663807299994,11.6,8.24417065699999));
#209150=CARTESIAN_POINT('Ctrl Pts',(7.73336166099994,15.2,8.24278367999998));
#209151=CARTESIAN_POINT('Ctrl Pts',(7.73336166099994,11.6,8.24278367999998));
#209152=CARTESIAN_POINT('Ctrl Pts',(7.73009064199995,15.2,8.24139598699999));
#209153=CARTESIAN_POINT('Ctrl Pts',(7.73009064199995,11.6,8.24139598699999));
#209154=CARTESIAN_POINT('Ctrl Pts',(7.72682502199994,15.2,8.24000758399999));
#209155=CARTESIAN_POINT('Ctrl Pts',(7.72682502199994,11.6,8.24000758399999));
#209156=CARTESIAN_POINT('Ctrl Pts',(7.72356480299995,15.2,8.23861848099998));
#209157=CARTESIAN_POINT('Ctrl Pts',(7.72356480299995,11.6,8.23861848099998));
#209158=CARTESIAN_POINT('Ctrl Pts',(7.72030999099995,15.2,8.23722868499999));
#209159=CARTESIAN_POINT('Ctrl Pts',(7.72030999099995,11.6,8.23722868499999));
#209160=CARTESIAN_POINT('Ctrl Pts',(7.71706059099994,15.2,8.23583820699999));
#209161=CARTESIAN_POINT('Ctrl Pts',(7.71706059099994,11.6,8.23583820699999));
#209162=CARTESIAN_POINT('Ctrl Pts',(7.71381660699994,15.2,8.23444705399999));
#209163=CARTESIAN_POINT('Ctrl Pts',(7.71381660699994,11.6,8.23444705399999));
#209164=CARTESIAN_POINT('Ctrl Pts',(7.71057804499995,15.2,8.23305523499998));
#209165=CARTESIAN_POINT('Ctrl Pts',(7.71057804499995,11.6,8.23305523499998));
#209166=CARTESIAN_POINT('Ctrl Pts',(7.70734490699994,15.2,8.23166275899998));
#209167=CARTESIAN_POINT('Ctrl Pts',(7.70734490699994,11.6,8.23166275899998));
#209168=CARTESIAN_POINT('Ctrl Pts',(7.70411720099994,15.2,8.23026963299998));
#209169=CARTESIAN_POINT('Ctrl Pts',(7.70411720099994,11.6,8.23026963299998));
#209170=CARTESIAN_POINT('Ctrl Pts',(7.70089492999994,15.2,8.22887586899999));
#209171=CARTESIAN_POINT('Ctrl Pts',(7.70089492999994,11.6,8.22887586899999));
#209172=CARTESIAN_POINT('Ctrl Pts',(7.69767809799994,15.2,8.22748147299999));
#209173=CARTESIAN_POINT('Ctrl Pts',(7.69767809799994,11.6,8.22748147299999));
#209174=CARTESIAN_POINT('Ctrl Pts',(7.69446671099994,15.2,8.22608645599999));
#209175=CARTESIAN_POINT('Ctrl Pts',(7.69446671099994,11.6,8.22608645599999));
#209176=CARTESIAN_POINT('Ctrl Pts',(7.69126077299994,15.2,8.22469082499998));
#209177=CARTESIAN_POINT('Ctrl Pts',(7.69126077299994,11.6,8.22469082499998));
#209178=CARTESIAN_POINT('Ctrl Pts',(7.68806028899994,15.2,8.22329458899999));
#209179=CARTESIAN_POINT('Ctrl Pts',(7.68806028899994,11.6,8.22329458899999));
#209180=CARTESIAN_POINT('Ctrl Pts',(7.68486526399994,15.2,8.22189775699999));
#209181=CARTESIAN_POINT('Ctrl Pts',(7.68486526399994,11.6,8.22189775699999));
#209182=CARTESIAN_POINT('Ctrl Pts',(7.68167570299994,15.2,8.22050033799999));
#209183=CARTESIAN_POINT('Ctrl Pts',(7.68167570299994,11.6,8.22050033799999));
#209184=CARTESIAN_POINT('Ctrl Pts',(7.67849160799994,15.2,8.21910234199999));
#209185=CARTESIAN_POINT('Ctrl Pts',(7.67849160799994,11.6,8.21910234199999));
#209186=CARTESIAN_POINT('Ctrl Pts',(7.67531298699994,15.2,8.21770377599999));
#209187=CARTESIAN_POINT('Ctrl Pts',(7.67531298699994,11.6,8.21770377599999));
#209188=CARTESIAN_POINT('Ctrl Pts',(7.67213984399994,15.2,8.21630465099998));
#209189=CARTESIAN_POINT('Ctrl Pts',(7.67213984399994,11.6,8.21630465099998));
#209190=CARTESIAN_POINT('Ctrl Pts',(7.66897218199994,15.2,8.21490497399999));
#209191=CARTESIAN_POINT('Ctrl Pts',(7.66897218199994,11.6,8.21490497399999));
#209192=CARTESIAN_POINT('Ctrl Pts',(7.66581000699994,15.2,8.21350475499998));
#209193=CARTESIAN_POINT('Ctrl Pts',(7.66581000699994,11.6,8.21350475499998));
#209194=CARTESIAN_POINT('Ctrl Pts',(7.66265332399994,15.2,8.21210400299999));
#209195=CARTESIAN_POINT('Ctrl Pts',(7.66265332399994,11.6,8.21210400299999));
#209196=CARTESIAN_POINT('Ctrl Pts',(7.65950213599995,15.2,8.21070272499998));
#209197=CARTESIAN_POINT('Ctrl Pts',(7.65950213599995,11.6,8.21070272499998));
#209198=CARTESIAN_POINT('Ctrl Pts',(7.65635644999994,15.2,8.20930093299998));
#209199=CARTESIAN_POINT('Ctrl Pts',(7.65635644999994,11.6,8.20930093299998));
#209200=CARTESIAN_POINT('Ctrl Pts',(7.65321626899994,15.2,8.20789863399998));
#209201=CARTESIAN_POINT('Ctrl Pts',(7.65321626899994,11.6,8.20789863399998));
#209202=CARTESIAN_POINT('Ctrl Pts',(7.65008159999994,15.2,8.20649583899998));
#209203=CARTESIAN_POINT('Ctrl Pts',(7.65008159999994,11.6,8.20649583899998));
#209204=CARTESIAN_POINT('Ctrl Pts',(7.64695244399995,15.2,8.20509255599998));
#209205=CARTESIAN_POINT('Ctrl Pts',(7.64695244399995,11.6,8.20509255599998));
#209206=CARTESIAN_POINT('Ctrl Pts',(7.64382880899994,15.2,8.20368879199999));
#209207=CARTESIAN_POINT('Ctrl Pts',(7.64382880899994,11.6,8.20368879199999));
#209208=CARTESIAN_POINT('Ctrl Pts',(7.64071069899994,15.2,8.20228455999998));
#209209=CARTESIAN_POINT('Ctrl Pts',(7.64071069899994,11.6,8.20228455999998));
#209210=CARTESIAN_POINT('Ctrl Pts',(7.63759811699994,15.2,8.20087986699999));
#209211=CARTESIAN_POINT('Ctrl Pts',(7.63759811699994,11.6,8.20087986699999));
#209212=CARTESIAN_POINT('Ctrl Pts',(7.63449106999994,15.2,8.19947472299998));
#209213=CARTESIAN_POINT('Ctrl Pts',(7.63449106999994,11.6,8.19947472299998));
#209214=CARTESIAN_POINT('Ctrl Pts',(7.63138956099994,15.2,8.19806913599999));
#209215=CARTESIAN_POINT('Ctrl Pts',(7.63138956099994,11.6,8.19806913599999));
#209216=CARTESIAN_POINT('Ctrl Pts',(7.62829359599994,15.2,8.19666311499999));
#209217=CARTESIAN_POINT('Ctrl Pts',(7.62829359599994,11.6,8.19666311499999));
#209218=CARTESIAN_POINT('Ctrl Pts',(7.62520317899994,15.2,8.19525667199999));
#209219=CARTESIAN_POINT('Ctrl Pts',(7.62520317899994,11.6,8.19525667199999));
#209220=CARTESIAN_POINT('Ctrl Pts',(7.62211831399994,15.2,8.19384981299999));
#209221=CARTESIAN_POINT('Ctrl Pts',(7.62211831399994,11.6,8.19384981299999));
#209222=CARTESIAN_POINT('Ctrl Pts',(7.61903900799994,15.2,8.19244254899999));
#209223=CARTESIAN_POINT('Ctrl Pts',(7.61903900799994,11.6,8.19244254899999));
#209224=CARTESIAN_POINT('Ctrl Pts',(7.61596526299994,15.2,8.19103488999998));
#209225=CARTESIAN_POINT('Ctrl Pts',(7.61596526299994,11.6,8.19103488999998));
#209226=CARTESIAN_POINT('Ctrl Pts',(7.61289708699994,15.2,8.18962684299999));
#209227=CARTESIAN_POINT('Ctrl Pts',(7.61289708699994,11.6,8.18962684299999));
#209228=CARTESIAN_POINT('Ctrl Pts',(7.60983448199994,15.2,8.18821841899998));
#209229=CARTESIAN_POINT('Ctrl Pts',(7.60983448199994,11.6,8.18821841899998));
#209230=CARTESIAN_POINT('Ctrl Pts',(7.60677745199994,15.2,8.18680962699998));
#209231=CARTESIAN_POINT('Ctrl Pts',(7.60677745199994,11.6,8.18680962699998));
#209232=CARTESIAN_POINT('Ctrl Pts',(7.60372600499994,15.2,8.18540047599999));
#209233=CARTESIAN_POINT('Ctrl Pts',(7.60372600499994,11.6,8.18540047599999));
#209234=CARTESIAN_POINT('Ctrl Pts',(7.60068014399994,15.2,8.18399097699999));
#209235=CARTESIAN_POINT('Ctrl Pts',(7.60068014399994,11.6,8.18399097699999));
#209236=CARTESIAN_POINT('Ctrl Pts',(7.59763987299994,15.2,8.18258113699999));
#209237=CARTESIAN_POINT('Ctrl Pts',(7.59763987299994,11.6,8.18258113699999));
#209238=CARTESIAN_POINT('Ctrl Pts',(7.59460519799994,15.2,8.18117096799998));
#209239=CARTESIAN_POINT('Ctrl Pts',(7.59460519799994,11.6,8.18117096799998));
#209240=CARTESIAN_POINT('Ctrl Pts',(7.59157612299994,15.2,8.17976047699998));
#209241=CARTESIAN_POINT('Ctrl Pts',(7.59157612299994,11.6,8.17976047699998));
#209242=CARTESIAN_POINT('Ctrl Pts',(7.58855265399994,15.2,8.17834967499999));
#209243=CARTESIAN_POINT('Ctrl Pts',(7.58855265399994,11.6,8.17834967499999));
#209244=CARTESIAN_POINT('Ctrl Pts',(7.58553479299994,15.2,8.17693857099999));
#209245=CARTESIAN_POINT('Ctrl Pts',(7.58553479299994,11.6,8.17693857099999));
#209246=CARTESIAN_POINT('Ctrl Pts',(7.58252254699994,15.2,8.17552717499998));
#209247=CARTESIAN_POINT('Ctrl Pts',(7.58252254699994,11.6,8.17552717499998));
#209248=CARTESIAN_POINT('Ctrl Pts',(7.57951592099994,15.2,8.17411549599999));
#209249=CARTESIAN_POINT('Ctrl Pts',(7.57951592099994,11.6,8.17411549599999));
#209250=CARTESIAN_POINT('Ctrl Pts',(7.57651491899995,15.2,8.17270354499998));
#209251=CARTESIAN_POINT('Ctrl Pts',(7.57651491899995,11.6,8.17270354499998));
#209252=CARTESIAN_POINT('Ctrl Pts',(7.57351954599994,15.2,8.17129132999998));
#209253=CARTESIAN_POINT('Ctrl Pts',(7.57351954599994,11.6,8.17129132999998));
#209254=CARTESIAN_POINT('Ctrl Pts',(7.57052980599994,15.2,8.16987885999998));
#209255=CARTESIAN_POINT('Ctrl Pts',(7.57052980599994,11.6,8.16987885999998));
#209256=CARTESIAN_POINT('Ctrl Pts',(7.56754570499995,15.2,8.16846614799999));
#209257=CARTESIAN_POINT('Ctrl Pts',(7.56754570499995,11.6,8.16846614799999));
#209258=CARTESIAN_POINT('Ctrl Pts',(7.56456724699994,15.2,8.16705319999999));
#209259=CARTESIAN_POINT('Ctrl Pts',(7.56456724699994,11.6,8.16705319999999));
#209260=CARTESIAN_POINT('Ctrl Pts',(7.56159443699994,15.2,8.16564002699998));
#209261=CARTESIAN_POINT('Ctrl Pts',(7.56159443699994,11.6,8.16564002699998));
#209262=CARTESIAN_POINT('Ctrl Pts',(7.55862727799994,15.2,8.16422663899999));
#209263=CARTESIAN_POINT('Ctrl Pts',(7.55862727799994,11.6,8.16422663899999));
#209264=CARTESIAN_POINT('Ctrl Pts',(7.55566577799994,15.2,8.16281304699999));
#209265=CARTESIAN_POINT('Ctrl Pts',(7.55566577799994,11.6,8.16281304699999));
#209266=CARTESIAN_POINT('Ctrl Pts',(7.55270993899994,15.2,8.16139925799998));
#209267=CARTESIAN_POINT('Ctrl Pts',(7.55270993899994,11.6,8.16139925799998));
#209268=CARTESIAN_POINT('Ctrl Pts',(7.54975976799994,15.2,8.15998528399999));
#209269=CARTESIAN_POINT('Ctrl Pts',(7.54975976799994,11.6,8.15998528399999));
#209270=CARTESIAN_POINT('Ctrl Pts',(7.54681526799994,15.2,8.15857113399998));
#209271=CARTESIAN_POINT('Ctrl Pts',(7.54681526799994,11.6,8.15857113399998));
#209272=CARTESIAN_POINT('Ctrl Pts',(7.54387644499994,15.2,8.15715681799999));
#209273=CARTESIAN_POINT('Ctrl Pts',(7.54387644499994,11.6,8.15715681799999));
#209274=CARTESIAN_POINT('Ctrl Pts',(7.54094330299995,15.2,8.15574234599998));
#209275=CARTESIAN_POINT('Ctrl Pts',(7.54094330299995,11.6,8.15574234599998));
#209276=CARTESIAN_POINT('Ctrl Pts',(7.53801584799994,15.2,8.15432772799999));
#209277=CARTESIAN_POINT('Ctrl Pts',(7.53801584799994,11.6,8.15432772799999));
#209278=CARTESIAN_POINT('Ctrl Pts',(7.53509408299994,15.2,8.15291297299999));
#209279=CARTESIAN_POINT('Ctrl Pts',(7.53509408299994,11.6,8.15291297299999));
#209280=CARTESIAN_POINT('Ctrl Pts',(7.53217801299995,15.2,8.15149809199998));
#209281=CARTESIAN_POINT('Ctrl Pts',(7.53217801299995,11.6,8.15149809199998));
#209282=CARTESIAN_POINT('Ctrl Pts',(7.52926764399994,15.2,8.15008309399998));
#209283=CARTESIAN_POINT('Ctrl Pts',(7.52926764399994,11.6,8.15008309399998));
#209284=CARTESIAN_POINT('Ctrl Pts',(7.52636298099994,15.2,8.14866798899999));
#209285=CARTESIAN_POINT('Ctrl Pts',(7.52636298099994,11.6,8.14866798899999));
#209286=CARTESIAN_POINT('Ctrl Pts',(7.52346402699994,15.2,8.14725278899999));
#209287=CARTESIAN_POINT('Ctrl Pts',(7.52346402699994,11.6,8.14725278899999));
#209288=CARTESIAN_POINT('Ctrl Pts',(7.52057078699995,15.2,8.14583750199999));
#209289=CARTESIAN_POINT('Ctrl Pts',(7.52057078699995,11.6,8.14583750199999));
#209290=CARTESIAN_POINT('Ctrl Pts',(7.51768326699994,15.2,8.14442213799998));
#209291=CARTESIAN_POINT('Ctrl Pts',(7.51768326699994,11.6,8.14442213799998));
#209292=CARTESIAN_POINT('Ctrl Pts',(7.51480147199994,15.2,8.14300670899998));
#209293=CARTESIAN_POINT('Ctrl Pts',(7.51480147199994,11.6,8.14300670899998));
#209294=CARTESIAN_POINT('Ctrl Pts',(7.51192540699994,15.2,8.14159122299999));
#209295=CARTESIAN_POINT('Ctrl Pts',(7.51192540699994,11.6,8.14159122299999));
#209296=CARTESIAN_POINT('Ctrl Pts',(7.50905507399994,15.2,8.14017569099999));
#209297=CARTESIAN_POINT('Ctrl Pts',(7.50905507399994,11.6,8.14017569099999));
#209298=CARTESIAN_POINT('Ctrl Pts',(7.50619048199994,15.2,8.13876012399999));
#209299=CARTESIAN_POINT('Ctrl Pts',(7.50619048199994,11.6,8.13876012399999));
#209300=CARTESIAN_POINT('Ctrl Pts',(7.50333163099994,15.2,8.13734453099999));
#209301=CARTESIAN_POINT('Ctrl Pts',(7.50333163099994,11.6,8.13734453099999));
#209302=CARTESIAN_POINT('Ctrl Pts',(7.50047852999994,15.2,8.13592892199999));
#209303=CARTESIAN_POINT('Ctrl Pts',(7.50047852999994,11.6,8.13592892199999));
#209304=CARTESIAN_POINT('Ctrl Pts',(7.49763118199994,15.2,8.13451330799998));
#209305=CARTESIAN_POINT('Ctrl Pts',(7.49763118199994,11.6,8.13451330799998));
#209306=CARTESIAN_POINT('Ctrl Pts',(7.49478959199994,15.2,8.13309769899998));
#209307=CARTESIAN_POINT('Ctrl Pts',(7.49478959199994,11.6,8.13309769899998));
#209308=CARTESIAN_POINT('Ctrl Pts',(7.49195376399994,15.2,8.13168210599999));
#209309=CARTESIAN_POINT('Ctrl Pts',(7.49195376399994,11.6,8.13168210599999));
#209310=CARTESIAN_POINT('Ctrl Pts',(7.48912370499994,15.2,8.13026653799999));
#209311=CARTESIAN_POINT('Ctrl Pts',(7.48912370499994,11.6,8.13026653799999));
#209312=CARTESIAN_POINT('Ctrl Pts',(7.48629941799994,15.2,8.12885100599999));
#209313=CARTESIAN_POINT('Ctrl Pts',(7.48629941799994,11.6,8.12885100599999));
#209314=CARTESIAN_POINT('Ctrl Pts',(7.48348090699994,15.2,8.12743552099998));
#209315=CARTESIAN_POINT('Ctrl Pts',(7.48348090699994,11.6,8.12743552099998));
#209316=CARTESIAN_POINT('Ctrl Pts',(7.48066817999994,15.2,8.12602009299999));
#209317=CARTESIAN_POINT('Ctrl Pts',(7.48066817999994,11.6,8.12602009299999));
#209318=CARTESIAN_POINT('Ctrl Pts',(7.47786123899994,15.2,8.12460473199998));
#209319=CARTESIAN_POINT('Ctrl Pts',(7.47786123899994,11.6,8.12460473199998));
#209320=CARTESIAN_POINT('Ctrl Pts',(7.47506008899994,15.2,8.12318944799999));
#209321=CARTESIAN_POINT('Ctrl Pts',(7.47506008899994,11.6,8.12318944799999));
#209322=CARTESIAN_POINT('Ctrl Pts',(7.47226473599994,15.2,8.12177425199998));
#209323=CARTESIAN_POINT('Ctrl Pts',(7.47226473599994,11.6,8.12177425199998));
#209324=CARTESIAN_POINT('Ctrl Pts',(7.46947518499994,15.2,8.12035915499998));
#209325=CARTESIAN_POINT('Ctrl Pts',(7.46947518499994,11.6,8.12035915499998));
#209326=CARTESIAN_POINT('Ctrl Pts',(7.46669143899994,15.2,8.11894416699998));
#209327=CARTESIAN_POINT('Ctrl Pts',(7.46669143899994,11.6,8.11894416699998));
#209328=CARTESIAN_POINT('Ctrl Pts',(7.46391350599994,15.2,8.11752929899999));
#209329=CARTESIAN_POINT('Ctrl Pts',(7.46391350599994,11.6,8.11752929899999));
#209330=CARTESIAN_POINT('Ctrl Pts',(7.46114138699994,15.2,8.11611456199999));
#209331=CARTESIAN_POINT('Ctrl Pts',(7.46114138699994,11.6,8.11611456199999));
#209332=CARTESIAN_POINT('Ctrl Pts',(7.45837508999994,15.2,8.11469996499999));
#209333=CARTESIAN_POINT('Ctrl Pts',(7.45837508999994,11.6,8.11469996499999));
#209334=CARTESIAN_POINT('Ctrl Pts',(7.45561461799994,15.2,8.11328551899998));
#209335=CARTESIAN_POINT('Ctrl Pts',(7.45561461799994,11.6,8.11328551899998));
#209336=CARTESIAN_POINT('Ctrl Pts',(7.45285997599994,15.2,8.11187123599998));
#209337=CARTESIAN_POINT('Ctrl Pts',(7.45285997599994,11.6,8.11187123599998));
#209338=CARTESIAN_POINT('Ctrl Pts',(7.45011116899994,15.2,8.11045712599999));
#209339=CARTESIAN_POINT('Ctrl Pts',(7.45011116899994,11.6,8.11045712599999));
#209340=CARTESIAN_POINT('Ctrl Pts',(7.44736820299994,15.2,8.10904319899999));
#209341=CARTESIAN_POINT('Ctrl Pts',(7.44736820299994,11.6,8.10904319899999));
#209342=CARTESIAN_POINT('Ctrl Pts',(7.44463108199994,15.2,8.10762946599999));
#209343=CARTESIAN_POINT('Ctrl Pts',(7.44463108199994,11.6,8.10762946599999));
#209344=CARTESIAN_POINT('Ctrl Pts',(7.44189980999994,15.2,8.10621593899998));
#209345=CARTESIAN_POINT('Ctrl Pts',(7.44189980999994,11.6,8.10621593899998));
#209346=CARTESIAN_POINT('Ctrl Pts',(7.43917439299994,15.2,8.10480262699999));
#209347=CARTESIAN_POINT('Ctrl Pts',(7.43917439299994,11.6,8.10480262699999));
#209348=CARTESIAN_POINT('Ctrl Pts',(7.43645483599994,15.2,8.10338954199998));
#209349=CARTESIAN_POINT('Ctrl Pts',(7.43645483599994,11.6,8.10338954199998));
#209350=CARTESIAN_POINT('Ctrl Pts',(7.43374114299994,15.2,8.10197669399999));
#209351=CARTESIAN_POINT('Ctrl Pts',(7.43374114299994,11.6,8.10197669399999));
#209352=CARTESIAN_POINT('Ctrl Pts',(7.43103331899994,15.2,8.10056409499998));
#209353=CARTESIAN_POINT('Ctrl Pts',(7.43103331899994,11.6,8.10056409499998));
#209354=CARTESIAN_POINT('Ctrl Pts',(7.42833136999994,15.2,8.09915175499999));
#209355=CARTESIAN_POINT('Ctrl Pts',(7.42833136999994,11.6,8.09915175499999));
#209356=CARTESIAN_POINT('Ctrl Pts',(7.42563529899994,15.2,8.09773968699999));
#209357=CARTESIAN_POINT('Ctrl Pts',(7.42563529899994,11.6,8.09773968699999));
#209358=CARTESIAN_POINT('Ctrl Pts',(7.42294511199994,15.2,8.09632789799998));
#209359=CARTESIAN_POINT('Ctrl Pts',(7.42294511199994,11.6,8.09632789799998));
#209360=CARTESIAN_POINT('Ctrl Pts',(7.42026081299994,15.2,8.09491640099999));
#209361=CARTESIAN_POINT('Ctrl Pts',(7.42026081299994,11.6,8.09491640099999));
#209362=CARTESIAN_POINT('Ctrl Pts',(7.41758240899994,15.2,8.09350520899999));
#209363=CARTESIAN_POINT('Ctrl Pts',(7.41758240899994,11.6,8.09350520899999));
#209364=CARTESIAN_POINT('Ctrl Pts',(7.41490990199994,15.2,8.09209432899999));
#209365=CARTESIAN_POINT('Ctrl Pts',(7.41490990199994,11.6,8.09209432899999));
#209366=CARTESIAN_POINT('Ctrl Pts',(7.41224329899994,15.2,8.09068377599999));
#209367=CARTESIAN_POINT('Ctrl Pts',(7.41224329899994,11.6,8.09068377599999));
#209368=CARTESIAN_POINT('Ctrl Pts',(7.40958260399994,15.2,8.08927355899998));
#209369=CARTESIAN_POINT('Ctrl Pts',(7.40958260399994,11.6,8.08927355899998));
#209370=CARTESIAN_POINT('Ctrl Pts',(7.40692782299995,15.2,8.08786368999998));
#209371=CARTESIAN_POINT('Ctrl Pts',(7.40692782299995,11.6,8.08786368999998));
#209372=CARTESIAN_POINT('Ctrl Pts',(7.40427895899994,15.2,8.08645417899999));
#209373=CARTESIAN_POINT('Ctrl Pts',(7.40427895899994,11.6,8.08645417899999));
#209374=CARTESIAN_POINT('Ctrl Pts',(7.40163601799994,15.2,8.08504503799998));
#209375=CARTESIAN_POINT('Ctrl Pts',(7.40163601799994,11.6,8.08504503799998));
#209376=CARTESIAN_POINT('Ctrl Pts',(7.39899900399994,15.2,8.08363627799999));
#209377=CARTESIAN_POINT('Ctrl Pts',(7.39899900399994,11.6,8.08363627799999));
#209378=CARTESIAN_POINT('Ctrl Pts',(7.39636792399994,15.2,8.08222790999999));
#209379=CARTESIAN_POINT('Ctrl Pts',(7.39636792399994,11.6,8.08222790999999));
#209380=CARTESIAN_POINT('Ctrl Pts',(7.39374278199994,15.2,8.08081994599998));
#209381=CARTESIAN_POINT('Ctrl Pts',(7.39374278199994,11.6,8.08081994599998));
#209382=CARTESIAN_POINT('Ctrl Pts',(7.39112357999994,15.2,8.07941239699998));
#209383=CARTESIAN_POINT('Ctrl Pts',(7.39112357999994,11.6,8.07941239699998));
#209384=CARTESIAN_POINT('Ctrl Pts',(7.38851032699994,15.2,8.07800527499998));
#209385=CARTESIAN_POINT('Ctrl Pts',(7.38851032699994,11.6,8.07800527499998));
#209386=CARTESIAN_POINT('Ctrl Pts',(7.38590302599994,15.2,8.07659858999998));
#209387=CARTESIAN_POINT('Ctrl Pts',(7.38590302599994,11.6,8.07659858999998));
#209388=CARTESIAN_POINT('Ctrl Pts',(7.38330168299994,15.2,8.07519235399998));
#209389=CARTESIAN_POINT('Ctrl Pts',(7.38330168299994,11.6,8.07519235399998));
#209390=CARTESIAN_POINT('Ctrl Pts',(7.38070630099994,15.2,8.07378657799998));
#209391=CARTESIAN_POINT('Ctrl Pts',(7.38070630099994,11.6,8.07378657799998));
#209392=CARTESIAN_POINT('Ctrl Pts',(7.37811688699994,15.2,8.07238127399999));
#209393=CARTESIAN_POINT('Ctrl Pts',(7.37811688699994,11.6,8.07238127399999));
#209394=CARTESIAN_POINT('Ctrl Pts',(7.37553344299994,15.2,8.07097645399999));
#209395=CARTESIAN_POINT('Ctrl Pts',(7.37553344299994,11.6,8.07097645399999));
#209396=CARTESIAN_POINT('Ctrl Pts',(7.37295597699994,15.2,8.06957212899999));
#209397=CARTESIAN_POINT('Ctrl Pts',(7.37295597699994,11.6,8.06957212899999));
#209398=CARTESIAN_POINT('Ctrl Pts',(7.37038449199994,15.2,8.06816830999999));
#209399=CARTESIAN_POINT('Ctrl Pts',(7.37038449199994,11.6,8.06816830999999));
#209400=CARTESIAN_POINT('Ctrl Pts',(7.36781899499994,15.2,8.06676500799998));
#209401=CARTESIAN_POINT('Ctrl Pts',(7.36781899499994,11.6,8.06676500799998));
#209402=CARTESIAN_POINT('Ctrl Pts',(7.36525948799994,15.2,8.06536223699998));
#209403=CARTESIAN_POINT('Ctrl Pts',(7.36525948799994,11.6,8.06536223699998));
#209404=CARTESIAN_POINT('Ctrl Pts',(7.36270597799995,15.2,8.06396000599998));
#209405=CARTESIAN_POINT('Ctrl Pts',(7.36270597799995,11.6,8.06396000599998));
#209406=CARTESIAN_POINT('Ctrl Pts',(7.36015846899994,15.2,8.06255832999998));
#209407=CARTESIAN_POINT('Ctrl Pts',(7.36015846899994,11.6,8.06255832999998));
#209408=CARTESIAN_POINT('Ctrl Pts',(7.35761696699995,15.2,8.06115721599999));
#209409=CARTESIAN_POINT('Ctrl Pts',(7.35761696699995,11.6,8.06115721599999));
#209410=CARTESIAN_POINT('Ctrl Pts',(7.35508147699995,15.2,8.05975668099999));
#209411=CARTESIAN_POINT('Ctrl Pts',(7.35508147699995,11.6,8.05975668099999));
#209412=CARTESIAN_POINT('Ctrl Pts',(7.35255200199994,15.2,8.05835673199999));
#209413=CARTESIAN_POINT('Ctrl Pts',(7.35255200199994,11.6,8.05835673199999));
#209414=CARTESIAN_POINT('Ctrl Pts',(7.35002854799994,15.2,8.05695738399999));
#209415=CARTESIAN_POINT('Ctrl Pts',(7.35002854799994,11.6,8.05695738399999));
#209416=CARTESIAN_POINT('Ctrl Pts',(7.34751111999994,15.2,8.05555864699999));
#209417=CARTESIAN_POINT('Ctrl Pts',(7.34751111999994,11.6,8.05555864699999));
#209418=CARTESIAN_POINT('Ctrl Pts',(7.34499972399994,15.2,8.05416053399998));
#209419=CARTESIAN_POINT('Ctrl Pts',(7.34499972399994,11.6,8.05416053399998));
#209420=CARTESIAN_POINT('Ctrl Pts',(7.34249436399995,15.2,8.05276305699999));
#209421=CARTESIAN_POINT('Ctrl Pts',(7.34249436399995,11.6,8.05276305699999));
#209422=CARTESIAN_POINT('Ctrl Pts',(7.33999504399995,15.2,8.05136622699998));
#209423=CARTESIAN_POINT('Ctrl Pts',(7.33999504399995,11.6,8.05136622699998));
#209424=CARTESIAN_POINT('Ctrl Pts',(7.33750177099994,15.2,8.04997005499999));
#209425=CARTESIAN_POINT('Ctrl Pts',(7.33750177099994,11.6,8.04997005499999));
#209426=CARTESIAN_POINT('Ctrl Pts',(7.33501454799995,15.2,8.04857455599999));
#209427=CARTESIAN_POINT('Ctrl Pts',(7.33501454799995,11.6,8.04857455599999));
#209428=CARTESIAN_POINT('Ctrl Pts',(7.33253337999995,15.2,8.04717973999999));
#209429=CARTESIAN_POINT('Ctrl Pts',(7.33253337999995,11.6,8.04717973999999));
#209430=CARTESIAN_POINT('Ctrl Pts',(7.33005827399994,15.2,8.04578561899999));
#209431=CARTESIAN_POINT('Ctrl Pts',(7.33005827399994,11.6,8.04578561899999));
#209432=CARTESIAN_POINT('Ctrl Pts',(7.32758923299994,15.2,8.04439220599999));
#209433=CARTESIAN_POINT('Ctrl Pts',(7.32758923299994,11.6,8.04439220599999));
#209434=CARTESIAN_POINT('Ctrl Pts',(7.32512626299994,15.2,8.04299951299999));
#209435=CARTESIAN_POINT('Ctrl Pts',(7.32512626299994,11.6,8.04299951299999));
#209436=CARTESIAN_POINT('Ctrl Pts',(7.32266936899994,15.2,8.04160755099998));
#209437=CARTESIAN_POINT('Ctrl Pts',(7.32266936899994,11.6,8.04160755099998));
#209438=CARTESIAN_POINT('Ctrl Pts',(7.32021855599994,15.2,8.04021633199999));
#209439=CARTESIAN_POINT('Ctrl Pts',(7.32021855599994,11.6,8.04021633199999));
#209440=CARTESIAN_POINT('Ctrl Pts',(7.31777382799994,15.2,8.03882586999999));
#209441=CARTESIAN_POINT('Ctrl Pts',(7.31777382799994,11.6,8.03882586999999));
#209442=CARTESIAN_POINT('Ctrl Pts',(7.31533518999994,15.2,8.03743617699999));
#209443=CARTESIAN_POINT('Ctrl Pts',(7.31533518999994,11.6,8.03743617699999));
#209444=CARTESIAN_POINT('Ctrl Pts',(7.31290264799994,15.2,8.03604726399998));
#209445=CARTESIAN_POINT('Ctrl Pts',(7.31290264799994,11.6,8.03604726399998));
#209446=CARTESIAN_POINT('Ctrl Pts',(7.31047620699995,15.2,8.03465914399998));
#209447=CARTESIAN_POINT('Ctrl Pts',(7.31047620699995,11.6,8.03465914399998));
#209448=CARTESIAN_POINT('Ctrl Pts',(7.30805587099994,15.2,8.03327182999999));
#209449=CARTESIAN_POINT('Ctrl Pts',(7.30805587099994,11.6,8.03327182999999));
#209450=CARTESIAN_POINT('Ctrl Pts',(7.30564164599994,15.2,8.03188533299998));
#209451=CARTESIAN_POINT('Ctrl Pts',(7.30564164599994,11.6,8.03188533299998));
#209452=CARTESIAN_POINT('Ctrl Pts',(7.30323353699994,15.2,8.03049966599998));
#209453=CARTESIAN_POINT('Ctrl Pts',(7.30323353699994,11.6,8.03049966599998));
#209454=CARTESIAN_POINT('Ctrl Pts',(7.30083154799994,15.2,8.02911484099998));
#209455=CARTESIAN_POINT('Ctrl Pts',(7.30083154799994,11.6,8.02911484099998));
#209456=CARTESIAN_POINT('Ctrl Pts',(7.29843568399994,15.2,8.02773087199999));
#209457=CARTESIAN_POINT('Ctrl Pts',(7.29843568399994,11.6,8.02773087199999));
#209458=CARTESIAN_POINT('Ctrl Pts',(7.29604595099994,15.2,8.02634777099998));
#209459=CARTESIAN_POINT('Ctrl Pts',(7.29604595099994,11.6,8.02634777099998));
#209460=CARTESIAN_POINT('Ctrl Pts',(7.29366235399994,15.2,8.02496554999999));
#209461=CARTESIAN_POINT('Ctrl Pts',(7.29366235399994,11.6,8.02496554999999));
#209462=CARTESIAN_POINT('Ctrl Pts',(7.29128489699994,15.2,8.02358422099999));
#209463=CARTESIAN_POINT('Ctrl Pts',(7.29128489699994,11.6,8.02358422099999));
#209464=CARTESIAN_POINT('Ctrl Pts',(7.28891358599994,15.2,8.02220379799999));
#209465=CARTESIAN_POINT('Ctrl Pts',(7.28891358599994,11.6,8.02220379799999));
#209466=CARTESIAN_POINT('Ctrl Pts',(7.28654842499994,15.2,8.02082429199999));
#209467=CARTESIAN_POINT('Ctrl Pts',(7.28654842499994,11.6,8.02082429199999));
#209468=CARTESIAN_POINT('Ctrl Pts',(7.28418941999994,15.2,8.01944571799999));
#209469=CARTESIAN_POINT('Ctrl Pts',(7.28418941999994,11.6,8.01944571799999));
#209470=CARTESIAN_POINT('Ctrl Pts',(7.28183657499994,15.2,8.01806808699999));
#209471=CARTESIAN_POINT('Ctrl Pts',(7.28183657499994,11.6,8.01806808699999));
#209472=CARTESIAN_POINT('Ctrl Pts',(7.27948989599994,15.2,8.01669141199999));
#209473=CARTESIAN_POINT('Ctrl Pts',(7.27948989599994,11.6,8.01669141199999));
#209474=CARTESIAN_POINT('Ctrl Pts',(7.27714938799994,15.2,8.01531570599998));
#209475=CARTESIAN_POINT('Ctrl Pts',(7.27714938799994,11.6,8.01531570599998));
#209476=CARTESIAN_POINT('Ctrl Pts',(7.27481505599994,15.2,8.01394098199999));
#209477=CARTESIAN_POINT('Ctrl Pts',(7.27481505599994,11.6,8.01394098199999));
#209478=CARTESIAN_POINT('Ctrl Pts',(7.27248690399994,15.2,8.01256725399998));
#209479=CARTESIAN_POINT('Ctrl Pts',(7.27248690399994,11.6,8.01256725399998));
#209480=CARTESIAN_POINT('Ctrl Pts',(7.27016493799994,15.2,8.01119453199998));
#209481=CARTESIAN_POINT('Ctrl Pts',(7.27016493799994,11.6,8.01119453199998));
#209482=CARTESIAN_POINT('Ctrl Pts',(7.26784916299994,15.2,8.00982283099999));
#209483=CARTESIAN_POINT('Ctrl Pts',(7.26784916299994,11.6,8.00982283099999));
#209484=CARTESIAN_POINT('Ctrl Pts',(7.26553958399994,15.2,8.00845216399999));
#209485=CARTESIAN_POINT('Ctrl Pts',(7.26553958399994,11.6,8.00845216399999));
#209486=CARTESIAN_POINT('Ctrl Pts',(7.26323620599994,15.2,8.00708254299998));
#209487=CARTESIAN_POINT('Ctrl Pts',(7.26323620599994,11.6,8.00708254299998));
#209488=CARTESIAN_POINT('Ctrl Pts',(7.26093903399994,15.2,8.00571398199999));
#209489=CARTESIAN_POINT('Ctrl Pts',(7.26093903399994,11.6,8.00571398199999));
#209490=CARTESIAN_POINT('Ctrl Pts',(7.25864807299994,15.2,8.00434649299999));
#209491=CARTESIAN_POINT('Ctrl Pts',(7.25864807299994,11.6,8.00434649299999));
#209492=CARTESIAN_POINT('Ctrl Pts',(7.25636332799994,15.2,8.00298009099999));
#209493=CARTESIAN_POINT('Ctrl Pts',(7.25636332799994,11.6,8.00298009099999));
#209494=CARTESIAN_POINT('Ctrl Pts',(7.25408480399994,15.2,8.00161478799998));
#209495=CARTESIAN_POINT('Ctrl Pts',(7.25408480399994,11.6,8.00161478799998));
#209496=CARTESIAN_POINT('Ctrl Pts',(7.25181250699994,15.2,8.00025059699998));
#209497=CARTESIAN_POINT('Ctrl Pts',(7.25181250699994,11.6,8.00025059699998));
#209498=CARTESIAN_POINT('Ctrl Pts',(7.24954643999994,15.2,7.99888753199999));
#209499=CARTESIAN_POINT('Ctrl Pts',(7.24954643999994,11.6,7.99888753199999));
#209500=CARTESIAN_POINT('Ctrl Pts',(7.24728661099994,15.2,7.99752560499999));
#209501=CARTESIAN_POINT('Ctrl Pts',(7.24728661099994,11.6,7.99752560499999));
#209502=CARTESIAN_POINT('Ctrl Pts',(7.24503302199994,15.2,7.99616483099998));
#209503=CARTESIAN_POINT('Ctrl Pts',(7.24503302199994,11.6,7.99616483099998));
#209504=CARTESIAN_POINT('Ctrl Pts',(7.24278568099994,15.2,7.99480522099999));
#209505=CARTESIAN_POINT('Ctrl Pts',(7.24278568099994,11.6,7.99480522099999));
#209506=CARTESIAN_POINT('Ctrl Pts',(7.24054459099994,15.2,7.99344679199999));
#209507=CARTESIAN_POINT('Ctrl Pts',(7.24054459099994,11.6,7.99344679199999));
#209508=CARTESIAN_POINT('Ctrl Pts',(7.23830975699994,15.2,7.99208955499999));
#209509=CARTESIAN_POINT('Ctrl Pts',(7.23830975699994,11.6,7.99208955499999));
#209510=CARTESIAN_POINT('Ctrl Pts',(7.23608118499994,15.2,7.99073352199999));
#209511=CARTESIAN_POINT('Ctrl Pts',(7.23608118499994,11.6,7.99073352199999));
#209512=CARTESIAN_POINT('Ctrl Pts',(7.23385888099994,15.2,7.98937870999998));
#209513=CARTESIAN_POINT('Ctrl Pts',(7.23385888099994,11.6,7.98937870999998));
#209514=CARTESIAN_POINT('Ctrl Pts',(7.23164284799994,15.2,7.98802513099999));
#209515=CARTESIAN_POINT('Ctrl Pts',(7.23164284799994,11.6,7.98802513099999));
#209516=CARTESIAN_POINT('Ctrl Pts',(7.22943309299994,15.2,7.98667279799999));
#209517=CARTESIAN_POINT('Ctrl Pts',(7.22943309299994,11.6,7.98667279799999));
#209518=CARTESIAN_POINT('Ctrl Pts',(7.22722961999994,15.2,7.98532172499999));
#209519=CARTESIAN_POINT('Ctrl Pts',(7.22722961999994,11.6,7.98532172499999));
#209520=CARTESIAN_POINT('Ctrl Pts',(7.22503243399994,15.2,7.98397192599998));
#209521=CARTESIAN_POINT('Ctrl Pts',(7.22503243399994,11.6,7.98397192599998));
#209522=CARTESIAN_POINT('Ctrl Pts',(7.22284154099994,15.2,7.98262341499999));
#209523=CARTESIAN_POINT('Ctrl Pts',(7.22284154099994,11.6,7.98262341499999));
#209524=CARTESIAN_POINT('Ctrl Pts',(7.22065694499994,15.2,7.98127620399999));
#209525=CARTESIAN_POINT('Ctrl Pts',(7.22065694499994,11.6,7.98127620399999));
#209526=CARTESIAN_POINT('Ctrl Pts',(7.21847865199994,15.2,7.97993030999999));
#209527=CARTESIAN_POINT('Ctrl Pts',(7.21847865199994,11.6,7.97993030999999));
#209528=CARTESIAN_POINT('Ctrl Pts',(7.21630666699994,15.2,7.97858574399999));
#209529=CARTESIAN_POINT('Ctrl Pts',(7.21630666699994,11.6,7.97858574399999));
#209530=CARTESIAN_POINT('Ctrl Pts',(7.21414099399994,15.2,7.97724252099999));
#209531=CARTESIAN_POINT('Ctrl Pts',(7.21414099399994,11.6,7.97724252099999));
#209532=CARTESIAN_POINT('Ctrl Pts',(7.21198163999994,15.2,7.97590065499998));
#209533=CARTESIAN_POINT('Ctrl Pts',(7.21198163999994,11.6,7.97590065499998));
#209534=CARTESIAN_POINT('Ctrl Pts',(7.20982860899994,15.2,7.97456015899999));
#209535=CARTESIAN_POINT('Ctrl Pts',(7.20982860899994,11.6,7.97456015899999));
#209536=CARTESIAN_POINT('Ctrl Pts',(7.20768190699994,15.2,7.97322104899998));
#209537=CARTESIAN_POINT('Ctrl Pts',(7.20768190699994,11.6,7.97322104899998));
#209538=CARTESIAN_POINT('Ctrl Pts',(7.20554153899994,15.2,7.97188333699999));
#209539=CARTESIAN_POINT('Ctrl Pts',(7.20554153899994,11.6,7.97188333699999));
#209540=CARTESIAN_POINT('Ctrl Pts',(7.20340750799994,15.2,7.97054703799999));
#209541=CARTESIAN_POINT('Ctrl Pts',(7.20340750799994,11.6,7.97054703799999));
#209542=CARTESIAN_POINT('Ctrl Pts',(7.20127982199994,15.2,7.96921216499998));
#209543=CARTESIAN_POINT('Ctrl Pts',(7.20127982199994,11.6,7.96921216499998));
#209544=CARTESIAN_POINT('Ctrl Pts',(7.19915848399994,15.2,7.96787873399998));
#209545=CARTESIAN_POINT('Ctrl Pts',(7.19915848399994,11.6,7.96787873399998));
#209546=CARTESIAN_POINT('Ctrl Pts',(7.19704350099994,15.2,7.96654675999999));
#209547=CARTESIAN_POINT('Ctrl Pts',(7.19704350099994,11.6,7.96654675999999));
#209548=CARTESIAN_POINT('Ctrl Pts',(7.19493487699994,15.2,7.96521625399999));
#209549=CARTESIAN_POINT('Ctrl Pts',(7.19493487699994,11.6,7.96521625399999));
#209550=CARTESIAN_POINT('Ctrl Pts',(7.19283261799994,15.2,7.96388723199998));
#209551=CARTESIAN_POINT('Ctrl Pts',(7.19283261799994,11.6,7.96388723199998));
#209552=CARTESIAN_POINT('Ctrl Pts',(7.19073672799994,15.2,7.96255970899999));
#209553=CARTESIAN_POINT('Ctrl Pts',(7.19073672799994,11.6,7.96255970899999));
#209554=CARTESIAN_POINT('Ctrl Pts',(7.18864721299994,15.2,7.96123369799999));
#209555=CARTESIAN_POINT('Ctrl Pts',(7.18864721299994,11.6,7.96123369799999));
#209556=CARTESIAN_POINT('Ctrl Pts',(7.18656407799994,15.2,7.95990921399999));
#209557=CARTESIAN_POINT('Ctrl Pts',(7.18656407799994,11.6,7.95990921399999));
#209558=CARTESIAN_POINT('Ctrl Pts',(7.18448732799994,15.2,7.95858627199999));
#209559=CARTESIAN_POINT('Ctrl Pts',(7.18448732799994,11.6,7.95858627199999));
#209560=CARTESIAN_POINT('Ctrl Pts',(7.18241696999994,15.2,7.95726488699999));
#209561=CARTESIAN_POINT('Ctrl Pts',(7.18241696999994,11.6,7.95726488699999));
#209562=CARTESIAN_POINT('Ctrl Pts',(7.18035300599994,15.2,7.95594507099998));
#209563=CARTESIAN_POINT('Ctrl Pts',(7.18035300599994,11.6,7.95594507099998));
#209564=CARTESIAN_POINT('Ctrl Pts',(7.17829544299994,15.2,7.95462684099999));
#209565=CARTESIAN_POINT('Ctrl Pts',(7.17829544299994,11.6,7.95462684099999));
#209566=CARTESIAN_POINT('Ctrl Pts',(7.17624428699994,15.2,7.95331021199999));
#209567=CARTESIAN_POINT('Ctrl Pts',(7.17624428699994,11.6,7.95331021199999));
#209568=CARTESIAN_POINT('Ctrl Pts',(7.17419954099995,15.2,7.95199519699998));
#209569=CARTESIAN_POINT('Ctrl Pts',(7.17419954099995,11.6,7.95199519699998));
#209570=CARTESIAN_POINT('Ctrl Pts',(7.17216121199994,15.2,7.95068181099998));
#209571=CARTESIAN_POINT('Ctrl Pts',(7.17216121199994,11.6,7.95068181099998));
#209572=CARTESIAN_POINT('Ctrl Pts',(7.17012930499994,15.2,7.94937006899998));
#209573=CARTESIAN_POINT('Ctrl Pts',(7.17012930499994,11.6,7.94937006899998));
#209574=CARTESIAN_POINT('Ctrl Pts',(7.16810382499995,15.2,7.94805998799998));
#209575=CARTESIAN_POINT('Ctrl Pts',(7.16810382499995,11.6,7.94805998799998));
#209576=CARTESIAN_POINT('Ctrl Pts',(7.16608477699994,15.2,7.94675157899999));
#209577=CARTESIAN_POINT('Ctrl Pts',(7.16608477699994,11.6,7.94675157899999));
#209578=CARTESIAN_POINT('Ctrl Pts',(7.16407216599994,15.2,7.94544485999998));
#209579=CARTESIAN_POINT('Ctrl Pts',(7.16407216599994,11.6,7.94544485999998));
#209580=CARTESIAN_POINT('Ctrl Pts',(7.16206599799994,15.2,7.94413984399998));
#209581=CARTESIAN_POINT('Ctrl Pts',(7.16206599799994,11.6,7.94413984399998));
#209582=CARTESIAN_POINT('Ctrl Pts',(7.16006627799994,15.2,7.94283654699999));
#209583=CARTESIAN_POINT('Ctrl Pts',(7.16006627799994,11.6,7.94283654699999));
#209584=CARTESIAN_POINT('Ctrl Pts',(7.15807301099994,15.2,7.94153498399999));
#209585=CARTESIAN_POINT('Ctrl Pts',(7.15807301099994,11.6,7.94153498399999));
#209586=CARTESIAN_POINT('Ctrl Pts',(7.15608620199994,15.2,7.94023516999999));
#209587=CARTESIAN_POINT('Ctrl Pts',(7.15608620199994,11.6,7.94023516999999));
#209588=CARTESIAN_POINT('Ctrl Pts',(7.15410585699994,15.2,7.93893712099998));
#209589=CARTESIAN_POINT('Ctrl Pts',(7.15410585699994,11.6,7.93893712099998));
#209590=CARTESIAN_POINT('Ctrl Pts',(7.15213198099995,15.2,7.93764085199999));
#209591=CARTESIAN_POINT('Ctrl Pts',(7.15213198099995,11.6,7.93764085199999));
#209592=CARTESIAN_POINT('Ctrl Pts',(7.15016457899995,15.2,7.93634637599999));
#209593=CARTESIAN_POINT('Ctrl Pts',(7.15016457899995,11.6,7.93634637599999));
#209594=CARTESIAN_POINT('Ctrl Pts',(7.14820365499994,15.2,7.93505370999998));
#209595=CARTESIAN_POINT('Ctrl Pts',(7.14820365499994,11.6,7.93505370999998));
#209596=CARTESIAN_POINT('Ctrl Pts',(7.14624921799994,15.2,7.93376286999998));
#209597=CARTESIAN_POINT('Ctrl Pts',(7.14624921799994,11.6,7.93376286999998));
#209598=CARTESIAN_POINT('Ctrl Pts',(7.14430126899994,15.2,7.93247387099999));
#209599=CARTESIAN_POINT('Ctrl Pts',(7.14430126899994,11.6,7.93247387099999));
#209600=CARTESIAN_POINT('Ctrl Pts',(7.14235981699994,15.2,7.93118672899999));
#209601=CARTESIAN_POINT('Ctrl Pts',(7.14235981699994,11.6,7.93118672899999));
#209602=CARTESIAN_POINT('Ctrl Pts',(7.14042486499994,15.2,7.92990145699999));
#209603=CARTESIAN_POINT('Ctrl Pts',(7.14042486499994,11.6,7.92990145699999));
#209604=CARTESIAN_POINT('Ctrl Pts',(7.13849641899994,15.2,7.92861807299998));
#209605=CARTESIAN_POINT('Ctrl Pts',(7.13849641899994,11.6,7.92861807299998));
#209606=CARTESIAN_POINT('Ctrl Pts',(7.13657448299994,15.2,7.92733659199998));
#209607=CARTESIAN_POINT('Ctrl Pts',(7.13657448299994,11.6,7.92733659199998));
#209608=CARTESIAN_POINT('Ctrl Pts',(7.13465906499994,15.2,7.92605702899999));
#209609=CARTESIAN_POINT('Ctrl Pts',(7.13465906499994,11.6,7.92605702899999));
#209610=CARTESIAN_POINT('Ctrl Pts',(7.13275016799994,15.2,7.92477940099998));
#209611=CARTESIAN_POINT('Ctrl Pts',(7.13275016799994,11.6,7.92477940099998));
#209612=CARTESIAN_POINT('Ctrl Pts',(7.13084779799994,15.2,7.92350372299998));
#209613=CARTESIAN_POINT('Ctrl Pts',(7.13084779799994,11.6,7.92350372299998));
#209614=CARTESIAN_POINT('Ctrl Pts',(7.12895196099994,15.2,7.92223000999999));
#209615=CARTESIAN_POINT('Ctrl Pts',(7.12895196099994,11.6,7.92223000999999));
#209616=CARTESIAN_POINT('Ctrl Pts',(7.12706265999994,15.2,7.92095827999999));
#209617=CARTESIAN_POINT('Ctrl Pts',(7.12706265999994,11.6,7.92095827999999));
#209618=CARTESIAN_POINT('Ctrl Pts',(7.12517990499994,15.2,7.91968854599999));
#209619=CARTESIAN_POINT('Ctrl Pts',(7.12517990499994,11.6,7.91968854599999));
#209620=CARTESIAN_POINT('Ctrl Pts',(7.12330369599994,15.2,7.91842082699999));
#209621=CARTESIAN_POINT('Ctrl Pts',(7.12330369599994,11.6,7.91842082699999));
#209622=CARTESIAN_POINT('Ctrl Pts',(7.12143404199994,15.2,7.91715513599998));
#209623=CARTESIAN_POINT('Ctrl Pts',(7.12143404199994,11.6,7.91715513599998));
#209624=CARTESIAN_POINT('Ctrl Pts',(7.11957094599994,15.2,7.91589149199999));
#209625=CARTESIAN_POINT('Ctrl Pts',(7.11957094599994,11.6,7.91589149199999));
#209626=CARTESIAN_POINT('Ctrl Pts',(7.11771441499994,15.2,7.91462990899999));
#209627=CARTESIAN_POINT('Ctrl Pts',(7.11771441499994,11.6,7.91462990899999));
#209628=CARTESIAN_POINT('Ctrl Pts',(7.11586445399995,15.2,7.91337040399998));
#209629=CARTESIAN_POINT('Ctrl Pts',(7.11586445399995,11.6,7.91337040399998));
#209630=CARTESIAN_POINT('Ctrl Pts',(7.11402106899994,15.2,7.91211299399999));
#209631=CARTESIAN_POINT('Ctrl Pts',(7.11402106899994,11.6,7.91211299399999));
#209632=CARTESIAN_POINT('Ctrl Pts',(7.11218426399994,15.2,7.91085769199999));
#209633=CARTESIAN_POINT('Ctrl Pts',(7.11218426399994,11.6,7.91085769199999));
#209634=CARTESIAN_POINT('Ctrl Pts',(7.11035404399994,15.2,7.90960451899998));
#209635=CARTESIAN_POINT('Ctrl Pts',(7.11035404399994,11.6,7.90960451899998));
#209636=CARTESIAN_POINT('Ctrl Pts',(7.10853041699994,15.2,7.90835348799998));
#209637=CARTESIAN_POINT('Ctrl Pts',(7.10853041699994,11.6,7.90835348799998));
#209638=CARTESIAN_POINT('Ctrl Pts',(7.10671338599994,15.2,7.90710461699998));
#209639=CARTESIAN_POINT('Ctrl Pts',(7.10671338599994,11.6,7.90710461699998));
#209640=CARTESIAN_POINT('Ctrl Pts',(7.10490295599994,15.2,7.90585792199998));
#209641=CARTESIAN_POINT('Ctrl Pts',(7.10490295599994,11.6,7.90585792199998));
#209642=CARTESIAN_POINT('Ctrl Pts',(7.10309913399994,15.2,7.90461341899999));
#209643=CARTESIAN_POINT('Ctrl Pts',(7.10309913399994,11.6,7.90461341899999));
#209644=CARTESIAN_POINT('Ctrl Pts',(7.10130192599994,15.2,7.90337112599998));
#209645=CARTESIAN_POINT('Ctrl Pts',(7.10130192599994,11.6,7.90337112599998));
#209646=CARTESIAN_POINT('Ctrl Pts',(7.09951133499994,15.2,7.90213105799998));
#209647=CARTESIAN_POINT('Ctrl Pts',(7.09951133499994,11.6,7.90213105799998));
#209648=CARTESIAN_POINT('Ctrl Pts',(7.09772736899994,15.2,7.90089323299998));
#209649=CARTESIAN_POINT('Ctrl Pts',(7.09772736899994,11.6,7.90089323299998));
#209650=CARTESIAN_POINT('Ctrl Pts',(7.09595003199994,15.2,7.89965766699999));
#209651=CARTESIAN_POINT('Ctrl Pts',(7.09595003199994,11.6,7.89965766699999));
#209652=CARTESIAN_POINT('Ctrl Pts',(7.09417932799994,15.2,7.89842437699999));
#209653=CARTESIAN_POINT('Ctrl Pts',(7.09417932799994,11.6,7.89842437699999));
#209654=CARTESIAN_POINT('Ctrl Pts',(7.09241526599994,15.2,7.89719338099999));
#209655=CARTESIAN_POINT('Ctrl Pts',(7.09241526599994,11.6,7.89719338099999));
#209656=CARTESIAN_POINT('Ctrl Pts',(7.09065784799995,15.2,7.89596469399999));
#209657=CARTESIAN_POINT('Ctrl Pts',(7.09065784799995,11.6,7.89596469399999));
#209658=CARTESIAN_POINT('Ctrl Pts',(7.08890708199994,15.2,7.89473833399998));
#209659=CARTESIAN_POINT('Ctrl Pts',(7.08890708199994,11.6,7.89473833399998));
#209660=CARTESIAN_POINT('Ctrl Pts',(7.08716297199994,15.2,7.89351431799999));
#209661=CARTESIAN_POINT('Ctrl Pts',(7.08716297199994,11.6,7.89351431799999));
#209662=CARTESIAN_POINT('Ctrl Pts',(7.08542552399994,15.2,7.89229266299999));
#209663=CARTESIAN_POINT('Ctrl Pts',(7.08542552399994,11.6,7.89229266299999));
#209664=CARTESIAN_POINT('Ctrl Pts',(7.08369474299994,15.2,7.89107338699999));
#209665=CARTESIAN_POINT('Ctrl Pts',(7.08369474299994,11.6,7.89107338699999));
#209666=CARTESIAN_POINT('Ctrl Pts',(7.08197063499994,15.2,7.88985650499999));
#209667=CARTESIAN_POINT('Ctrl Pts',(7.08197063499994,11.6,7.88985650499999));
#209668=CARTESIAN_POINT('Ctrl Pts',(7.08025320599995,15.2,7.88864203699998));
#209669=CARTESIAN_POINT('Ctrl Pts',(7.08025320599995,11.6,7.88864203699998));
#209670=CARTESIAN_POINT('Ctrl Pts',(7.07854245999994,15.2,7.88742999899998));
#209671=CARTESIAN_POINT('Ctrl Pts',(7.07854245999994,11.6,7.88742999899998));
#209672=CARTESIAN_POINT('Ctrl Pts',(7.07683840299994,15.2,7.88622040899998));
#209673=CARTESIAN_POINT('Ctrl Pts',(7.07683840299994,11.6,7.88622040899998));
#209674=CARTESIAN_POINT('Ctrl Pts',(7.07514103999995,15.2,7.88501328299999));
#209675=CARTESIAN_POINT('Ctrl Pts',(7.07514103999995,11.6,7.88501328299999));
#209676=CARTESIAN_POINT('Ctrl Pts',(7.07345037799994,15.2,7.88380863999999));
#209677=CARTESIAN_POINT('Ctrl Pts',(7.07345037799994,11.6,7.88380863999999));
#209678=CARTESIAN_POINT('Ctrl Pts',(7.07176642199994,15.2,7.88260649699998));
#209679=CARTESIAN_POINT('Ctrl Pts',(7.07176642199994,11.6,7.88260649699998));
#209680=CARTESIAN_POINT('Ctrl Pts',(7.07008917699994,15.2,7.88140687099999));
#209681=CARTESIAN_POINT('Ctrl Pts',(7.07008917699994,11.6,7.88140687099999));
#209682=CARTESIAN_POINT('Ctrl Pts',(7.06841864899994,15.2,7.88020978099999));
#209683=CARTESIAN_POINT('Ctrl Pts',(7.06841864899994,11.6,7.88020978099999));
#209684=CARTESIAN_POINT('Ctrl Pts',(7.06675484399995,15.2,7.87901524399999));
#209685=CARTESIAN_POINT('Ctrl Pts',(7.06675484399995,11.6,7.87901524399999));
#209686=CARTESIAN_POINT('Ctrl Pts',(7.06509776499994,15.2,7.87782327899999));
#209687=CARTESIAN_POINT('Ctrl Pts',(7.06509776499994,11.6,7.87782327899999));
#209688=CARTESIAN_POINT('Ctrl Pts',(7.06344742099994,15.2,7.87663390099999));
#209689=CARTESIAN_POINT('Ctrl Pts',(7.06344742099994,11.6,7.87663390099999));
#209690=CARTESIAN_POINT('Ctrl Pts',(7.06180381599994,15.2,7.87544713199999));
#209691=CARTESIAN_POINT('Ctrl Pts',(7.06180381599994,11.6,7.87544713199999));
#209692=CARTESIAN_POINT('Ctrl Pts',(7.06016695399994,15.2,7.87426298699998));
#209693=CARTESIAN_POINT('Ctrl Pts',(7.06016695399994,11.6,7.87426298699998));
#209694=CARTESIAN_POINT('Ctrl Pts',(7.05853684399994,15.2,7.87308148499999));
#209695=CARTESIAN_POINT('Ctrl Pts',(7.05853684399994,11.6,7.87308148499999));
#209696=CARTESIAN_POINT('Ctrl Pts',(7.05691348799995,15.2,7.87190264399998));
#209697=CARTESIAN_POINT('Ctrl Pts',(7.05691348799995,11.6,7.87190264399998));
#209698=CARTESIAN_POINT('Ctrl Pts',(7.05529689499994,15.2,7.87072648199998));
#209699=CARTESIAN_POINT('Ctrl Pts',(7.05529689499994,11.6,7.87072648199998));
#209700=CARTESIAN_POINT('Ctrl Pts',(7.05368706799994,15.2,7.86955301799999));
#209701=CARTESIAN_POINT('Ctrl Pts',(7.05368706799994,11.6,7.86955301799999));
#209702=CARTESIAN_POINT('Ctrl Pts',(7.05208401299994,15.2,7.86838227099998));
#209703=CARTESIAN_POINT('Ctrl Pts',(7.05208401299994,11.6,7.86838227099998));
#209704=CARTESIAN_POINT('Ctrl Pts',(7.05048773599994,15.2,7.86721425699999));
#209705=CARTESIAN_POINT('Ctrl Pts',(7.05048773599994,11.6,7.86721425699999));
#209706=CARTESIAN_POINT('Ctrl Pts',(7.04889824299994,15.2,7.86604899699999));
#209707=CARTESIAN_POINT('Ctrl Pts',(7.04889824299994,11.6,7.86604899699999));
#209708=CARTESIAN_POINT('Ctrl Pts',(7.04731553899994,15.2,7.86488650699999));
#209709=CARTESIAN_POINT('Ctrl Pts',(7.04731553899994,11.6,7.86488650699999));
#209710=CARTESIAN_POINT('Ctrl Pts',(7.04573962999994,15.2,7.86372680699999));
#209711=CARTESIAN_POINT('Ctrl Pts',(7.04573962999994,11.6,7.86372680699999));
#209712=CARTESIAN_POINT('Ctrl Pts',(7.04417052199994,15.2,7.86256991699998));
#209713=CARTESIAN_POINT('Ctrl Pts',(7.04417052199994,11.6,7.86256991699998));
#209714=CARTESIAN_POINT('Ctrl Pts',(7.04260821999994,15.2,7.86141585299998));
#209715=CARTESIAN_POINT('Ctrl Pts',(7.04260821999994,11.6,7.86141585299998));
#209716=CARTESIAN_POINT('Ctrl Pts',(7.04105272899994,15.2,7.86026463599999));
#209717=CARTESIAN_POINT('Ctrl Pts',(7.04105272899994,11.6,7.86026463599999));
#209718=CARTESIAN_POINT('Ctrl Pts',(7.03950405599994,15.2,7.85911628399998));
#209719=CARTESIAN_POINT('Ctrl Pts',(7.03950405599994,11.6,7.85911628399998));
#209720=CARTESIAN_POINT('Ctrl Pts',(7.03796220599994,15.2,7.85797081599998));
#209721=CARTESIAN_POINT('Ctrl Pts',(7.03796220599994,11.6,7.85797081599998));
#209722=CARTESIAN_POINT('Ctrl Pts',(7.03642718499994,15.2,7.85682825099999));
#209723=CARTESIAN_POINT('Ctrl Pts',(7.03642718499994,11.6,7.85682825099999));
#209724=CARTESIAN_POINT('Ctrl Pts',(7.03489899799994,15.2,7.85568860799999));
#209725=CARTESIAN_POINT('Ctrl Pts',(7.03489899799994,11.6,7.85568860799999));
#209726=CARTESIAN_POINT('Ctrl Pts',(7.03337765099994,15.2,7.85455190599999));
#209727=CARTESIAN_POINT('Ctrl Pts',(7.03337765099994,11.6,7.85455190599999));
#209728=CARTESIAN_POINT('Ctrl Pts',(7.03186315099994,15.2,7.85341816499999));
#209729=CARTESIAN_POINT('Ctrl Pts',(7.03186315099994,11.6,7.85341816499999));
#209730=CARTESIAN_POINT('Ctrl Pts',(7.03035550199994,15.2,7.85228740399998));
#209731=CARTESIAN_POINT('Ctrl Pts',(7.03035550199994,11.6,7.85228740399998));
#209732=CARTESIAN_POINT('Ctrl Pts',(7.02885470999994,15.2,7.85115964099998));
#209733=CARTESIAN_POINT('Ctrl Pts',(7.02885470999994,11.6,7.85115964099998));
#209734=CARTESIAN_POINT('Ctrl Pts',(7.02736078099995,15.2,7.85003489699999));
#209735=CARTESIAN_POINT('Ctrl Pts',(7.02736078099995,11.6,7.85003489699999));
#209736=CARTESIAN_POINT('Ctrl Pts',(7.02587372099994,15.2,7.84891319199998));
#209737=CARTESIAN_POINT('Ctrl Pts',(7.02587372099994,11.6,7.84891319199998));
#209738=CARTESIAN_POINT('Ctrl Pts',(7.02439353499994,15.2,7.84779454399998));
#209739=CARTESIAN_POINT('Ctrl Pts',(7.02439353499994,11.6,7.84779454399998));
#209740=CARTESIAN_POINT('Ctrl Pts',(7.02292022899995,15.2,7.84667897299999));
#209741=CARTESIAN_POINT('Ctrl Pts',(7.02292022899995,11.6,7.84667897299999));
#209742=CARTESIAN_POINT('Ctrl Pts',(7.02145380999994,15.2,7.84556649999999));
#209743=CARTESIAN_POINT('Ctrl Pts',(7.02145380999994,11.6,7.84556649999999));
#209744=CARTESIAN_POINT('Ctrl Pts',(7.01999428199994,15.2,7.84445714299999));
#209745=CARTESIAN_POINT('Ctrl Pts',(7.01999428199994,11.6,7.84445714299999));
#209746=CARTESIAN_POINT('Ctrl Pts',(7.01854165099994,15.2,7.84335092199999));
#209747=CARTESIAN_POINT('Ctrl Pts',(7.01854165099994,11.6,7.84335092199999));
#209748=CARTESIAN_POINT('Ctrl Pts',(7.01709592399994,15.2,7.84224785999999));
#209749=CARTESIAN_POINT('Ctrl Pts',(7.01709592399994,11.6,7.84224785999999));
#209750=CARTESIAN_POINT('Ctrl Pts',(7.01565710599994,15.2,7.84114797299999));
#209751=CARTESIAN_POINT('Ctrl Pts',(7.01565710599994,11.6,7.84114797299999));
#209752=CARTESIAN_POINT('Ctrl Pts',(7.01422520299994,15.2,7.84005128199999));
#209753=CARTESIAN_POINT('Ctrl Pts',(7.01422520299994,11.6,7.84005128199999));
#209754=CARTESIAN_POINT('Ctrl Pts',(7.01280021999994,15.2,7.83895780899999));
#209755=CARTESIAN_POINT('Ctrl Pts',(7.01280021999994,11.6,7.83895780899999));
#209756=CARTESIAN_POINT('Ctrl Pts',(7.01138216299994,15.2,7.83786757399999));
#209757=CARTESIAN_POINT('Ctrl Pts',(7.01138216299994,11.6,7.83786757399999));
#209758=CARTESIAN_POINT('Ctrl Pts',(7.00997103899994,15.2,7.83678059499999));
#209759=CARTESIAN_POINT('Ctrl Pts',(7.00997103899994,11.6,7.83678059499999));
#209760=CARTESIAN_POINT('Ctrl Pts',(7.00856685299994,15.2,7.83569689499998));
#209761=CARTESIAN_POINT('Ctrl Pts',(7.00856685299994,11.6,7.83569689499998));
#209762=CARTESIAN_POINT('Ctrl Pts',(7.00716961099995,15.2,7.83461649299999));
#209763=CARTESIAN_POINT('Ctrl Pts',(7.00716961099995,11.6,7.83461649299999));
#209764=CARTESIAN_POINT('Ctrl Pts',(7.00577931899995,15.2,7.83353940999999));
#209765=CARTESIAN_POINT('Ctrl Pts',(7.00577931899995,11.6,7.83353940999999));
#209766=CARTESIAN_POINT('Ctrl Pts',(7.00439598299995,15.2,7.83246566699999));
#209767=CARTESIAN_POINT('Ctrl Pts',(7.00439598299995,11.6,7.83246566699999));
#209768=CARTESIAN_POINT('Ctrl Pts',(7.00301960699995,15.2,7.83139528399998));
#209769=CARTESIAN_POINT('Ctrl Pts',(7.00301960699995,11.6,7.83139528399998));
#209770=CARTESIAN_POINT('Ctrl Pts',(7.00165019899995,15.2,7.83032828199998));
#209771=CARTESIAN_POINT('Ctrl Pts',(7.00165019899995,11.6,7.83032828199998));
#209772=CARTESIAN_POINT('Ctrl Pts',(7.00028776499994,15.2,7.82926468199998));
#209773=CARTESIAN_POINT('Ctrl Pts',(7.00028776499994,11.6,7.82926468199998));
#209774=CARTESIAN_POINT('Ctrl Pts',(6.99893230999994,15.2,7.82820450599999));
#209775=CARTESIAN_POINT('Ctrl Pts',(6.99893230999994,11.6,7.82820450599999));
#209776=CARTESIAN_POINT('Ctrl Pts',(6.99758383999994,15.2,7.82714777299999));
#209777=CARTESIAN_POINT('Ctrl Pts',(6.99758383999994,11.6,7.82714777299999));
#209778=CARTESIAN_POINT('Ctrl Pts',(6.99624235999995,15.2,7.82609450599999));
#209779=CARTESIAN_POINT('Ctrl Pts',(6.99624235999995,11.6,7.82609450599999));
#209780=CARTESIAN_POINT('Ctrl Pts',(6.99490787799994,15.2,7.82504472499999));
#209781=CARTESIAN_POINT('Ctrl Pts',(6.99490787799994,11.6,7.82504472499999));
#209782=CARTESIAN_POINT('Ctrl Pts',(6.99358039899994,15.2,7.82399845199999));
#209783=CARTESIAN_POINT('Ctrl Pts',(6.99358039899994,11.6,7.82399845199999));
#209784=CARTESIAN_POINT('Ctrl Pts',(6.99225992899994,15.2,7.82295570799998));
#209785=CARTESIAN_POINT('Ctrl Pts',(6.99225992899994,11.6,7.82295570799998));
#209786=CARTESIAN_POINT('Ctrl Pts',(6.99094647299995,15.2,7.82191651399998));
#209787=CARTESIAN_POINT('Ctrl Pts',(6.99094647299995,11.6,7.82191651399998));
#209788=CARTESIAN_POINT('Ctrl Pts',(6.98964003699994,15.2,7.82088089299998));
#209789=CARTESIAN_POINT('Ctrl Pts',(6.98964003699994,11.6,7.82088089299998));
#209790=CARTESIAN_POINT('Ctrl Pts',(6.98834062899994,15.2,7.81984886499998));
#209791=CARTESIAN_POINT('Ctrl Pts',(6.98834062899994,11.6,7.81984886499998));
#209792=CARTESIAN_POINT('Ctrl Pts',(6.98704825399994,15.2,7.81882045299999));
#209793=CARTESIAN_POINT('Ctrl Pts',(6.98704825399994,11.6,7.81882045299999));
#209794=CARTESIAN_POINT('Ctrl Pts',(6.98576291599994,15.2,7.81779567699999));
#209795=CARTESIAN_POINT('Ctrl Pts',(6.98576291599994,11.6,7.81779567699999));
#209796=CARTESIAN_POINT('Ctrl Pts',(6.98448462399995,15.2,7.81677456099998));
#209797=CARTESIAN_POINT('Ctrl Pts',(6.98448462399995,11.6,7.81677456099998));
#209798=CARTESIAN_POINT('Ctrl Pts',(6.98321338299994,15.2,7.81575712599999));
#209799=CARTESIAN_POINT('Ctrl Pts',(6.98321338299994,11.6,7.81575712599999));
#209800=CARTESIAN_POINT('Ctrl Pts',(6.98194919799994,15.2,7.81474339399999));
#209801=CARTESIAN_POINT('Ctrl Pts',(6.98194919799994,11.6,7.81474339399999));
#209802=CARTESIAN_POINT('Ctrl Pts',(6.98069207699994,15.2,7.81373338899999));
#209803=CARTESIAN_POINT('Ctrl Pts',(6.98069207699994,11.6,7.81373338899999));
#209804=CARTESIAN_POINT('Ctrl Pts',(6.97944202299994,15.2,7.81272712999999));
#209805=CARTESIAN_POINT('Ctrl Pts',(6.97944202299994,11.6,7.81272712999999));
#209806=CARTESIAN_POINT('Ctrl Pts',(6.97819904499994,15.2,7.81172464099999));
#209807=CARTESIAN_POINT('Ctrl Pts',(6.97819904499994,11.6,7.81172464099999));
#209808=CARTESIAN_POINT('Ctrl Pts',(6.97696314799994,15.2,7.81072594499998));
#209809=CARTESIAN_POINT('Ctrl Pts',(6.97696314799994,11.6,7.81072594499998));
#209810=CARTESIAN_POINT('Ctrl Pts',(6.97573433799994,15.2,7.80973106299999));
#209811=CARTESIAN_POINT('Ctrl Pts',(6.97573433799994,11.6,7.80973106299999));
#209812=CARTESIAN_POINT('Ctrl Pts',(6.97451262099994,15.2,7.80874001999998));
#209813=CARTESIAN_POINT('Ctrl Pts',(6.97451262099994,11.6,7.80874001999998));
#209814=CARTESIAN_POINT('Ctrl Pts',(6.97329800299994,15.2,7.80775283599999));
#209815=CARTESIAN_POINT('Ctrl Pts',(6.97329800299994,11.6,7.80775283599999));
#209816=CARTESIAN_POINT('Ctrl Pts',(6.97209049099994,15.2,7.80676953499999));
#209817=CARTESIAN_POINT('Ctrl Pts',(6.97209049099994,11.6,7.80676953499999));
#209818=CARTESIAN_POINT('Ctrl Pts',(6.97089008999995,15.2,7.80579014099998));
#209819=CARTESIAN_POINT('Ctrl Pts',(6.97089008999995,11.6,7.80579014099998));
#209820=CARTESIAN_POINT('Ctrl Pts',(6.96969680699994,15.2,7.80481467599999));
#209821=CARTESIAN_POINT('Ctrl Pts',(6.96969680699994,11.6,7.80481467599999));
#209822=CARTESIAN_POINT('Ctrl Pts',(6.96851064799994,15.2,7.80384316199999));
#209823=CARTESIAN_POINT('Ctrl Pts',(6.96851064799994,11.6,7.80384316199999));
#209824=CARTESIAN_POINT('Ctrl Pts',(6.96733161899994,15.2,7.80287562399998));
#209825=CARTESIAN_POINT('Ctrl Pts',(6.96733161899994,11.6,7.80287562399998));
#209826=CARTESIAN_POINT('Ctrl Pts',(6.96615972599994,15.2,7.80191208299998));
#209827=CARTESIAN_POINT('Ctrl Pts',(6.96615972599994,11.6,7.80191208299998));
#209828=CARTESIAN_POINT('Ctrl Pts',(6.96499497599994,15.2,7.80095256499998));
#209829=CARTESIAN_POINT('Ctrl Pts',(6.96499497599994,11.6,7.80095256499998));
#209830=CARTESIAN_POINT('Ctrl Pts',(6.96383737299994,15.2,7.79999709199998));
#209831=CARTESIAN_POINT('Ctrl Pts',(6.96383737299994,11.6,7.79999709199998));
#209832=CARTESIAN_POINT('Ctrl Pts',(6.96268692599994,15.2,7.79904568799999));
#209833=CARTESIAN_POINT('Ctrl Pts',(6.96268692599994,11.6,7.79904568799999));
#209834=CARTESIAN_POINT('Ctrl Pts',(6.96154363999994,15.2,7.79809837699998));
#209835=CARTESIAN_POINT('Ctrl Pts',(6.96154363999994,11.6,7.79809837699998));
#209836=CARTESIAN_POINT('Ctrl Pts',(6.96040752099995,15.2,7.79715518299999));
#209837=CARTESIAN_POINT('Ctrl Pts',(6.96040752099995,11.6,7.79715518299999));
#209838=CARTESIAN_POINT('Ctrl Pts',(6.95927857499994,15.2,7.79621612699999));
#209839=CARTESIAN_POINT('Ctrl Pts',(6.95927857499994,11.6,7.79621612699999));
#209840=CARTESIAN_POINT('Ctrl Pts',(6.95815680999995,15.2,7.79528123599999));
#209841=CARTESIAN_POINT('Ctrl Pts',(6.95815680999995,11.6,7.79528123599999));
#209842=CARTESIAN_POINT('Ctrl Pts',(6.95704222999994,15.2,7.79435053399999));
#209843=CARTESIAN_POINT('Ctrl Pts',(6.95704222999994,11.6,7.79435053399999));
#209844=CARTESIAN_POINT('Ctrl Pts',(6.95593484299994,15.2,7.79342404499998));
#209845=CARTESIAN_POINT('Ctrl Pts',(6.95593484299994,11.6,7.79342404499998));
#209846=CARTESIAN_POINT('Ctrl Pts',(6.95483465399994,15.2,7.79250179099999));
#209847=CARTESIAN_POINT('Ctrl Pts',(6.95483465399994,11.6,7.79250179099999));
#209848=CARTESIAN_POINT('Ctrl Pts',(6.95374166999994,15.2,7.79158379899999));
#209849=CARTESIAN_POINT('Ctrl Pts',(6.95374166999994,11.6,7.79158379899999));
#209850=CARTESIAN_POINT('Ctrl Pts',(6.95265589799994,15.2,7.79067009299999));
#209851=CARTESIAN_POINT('Ctrl Pts',(6.95265589799994,11.6,7.79067009299999));
#209852=CARTESIAN_POINT('Ctrl Pts',(6.95157734299994,15.2,7.78976069699999));
#209853=CARTESIAN_POINT('Ctrl Pts',(6.95157734299994,11.6,7.78976069699999));
#209854=CARTESIAN_POINT('Ctrl Pts',(6.95050601299994,15.2,7.78885563599999));
#209855=CARTESIAN_POINT('Ctrl Pts',(6.95050601299994,11.6,7.78885563599999));
#209856=CARTESIAN_POINT('Ctrl Pts',(6.94944191299994,15.2,7.78795493399999));
#209857=CARTESIAN_POINT('Ctrl Pts',(6.94944191299994,11.6,7.78795493399999));
#209858=CARTESIAN_POINT('Ctrl Pts',(6.94838504899994,15.2,7.78705861699999));
#209859=CARTESIAN_POINT('Ctrl Pts',(6.94838504899994,11.6,7.78705861699999));
#209860=CARTESIAN_POINT('Ctrl Pts',(6.94733542899994,15.2,7.78616670999998));
#209861=CARTESIAN_POINT('Ctrl Pts',(6.94733542899994,11.6,7.78616670999998));
#209862=CARTESIAN_POINT('Ctrl Pts',(6.94629305799995,15.2,7.78527923799999));
#209863=CARTESIAN_POINT('Ctrl Pts',(6.94629305799995,11.6,7.78527923799999));
#209864=CARTESIAN_POINT('Ctrl Pts',(6.94525794399994,15.2,7.78439622599999));
#209865=CARTESIAN_POINT('Ctrl Pts',(6.94525794399994,11.6,7.78439622599999));
#209866=CARTESIAN_POINT('Ctrl Pts',(6.94423009099994,15.2,7.78351769899999));
#209867=CARTESIAN_POINT('Ctrl Pts',(6.94423009099994,11.6,7.78351769899999));
#209868=CARTESIAN_POINT('Ctrl Pts',(6.94320950799994,15.2,7.78264368299999));
#209869=CARTESIAN_POINT('Ctrl Pts',(6.94320950799994,11.6,7.78264368299999));
#209870=CARTESIAN_POINT('Ctrl Pts',(6.94219619899994,15.2,7.78177420299999));
#209871=CARTESIAN_POINT('Ctrl Pts',(6.94219619899994,11.6,7.78177420299999));
#209872=CARTESIAN_POINT('Ctrl Pts',(6.94119017399994,15.2,7.78090928599998));
#209873=CARTESIAN_POINT('Ctrl Pts',(6.94119017399994,11.6,7.78090928599998));
#209874=CARTESIAN_POINT('Ctrl Pts',(6.94019143599995,15.2,7.78004895699999));
#209875=CARTESIAN_POINT('Ctrl Pts',(6.94019143599995,11.6,7.78004895699999));
#209876=CARTESIAN_POINT('Ctrl Pts',(6.93919999399994,15.2,7.77919324299998));
#209877=CARTESIAN_POINT('Ctrl Pts',(6.93919999399994,11.6,7.77919324299998));
#209878=CARTESIAN_POINT('Ctrl Pts',(6.93821585199994,15.2,7.77834216699999));
#209879=CARTESIAN_POINT('Ctrl Pts',(6.93821585199994,11.6,7.77834216699999));
#209880=CARTESIAN_POINT('Ctrl Pts',(6.93723901899994,15.2,7.77749575799999));
#209881=CARTESIAN_POINT('Ctrl Pts',(6.93723901899994,11.6,7.77749575799999));
#209882=CARTESIAN_POINT('Ctrl Pts',(6.93626949999994,15.2,7.77665404199999));
#209883=CARTESIAN_POINT('Ctrl Pts',(6.93626949999994,11.6,7.77665404199999));
#209884=CARTESIAN_POINT('Ctrl Pts',(6.93530730199994,15.2,7.77581704399999));
#209885=CARTESIAN_POINT('Ctrl Pts',(6.93530730199994,11.6,7.77581704399999));
#209886=CARTESIAN_POINT('Ctrl Pts',(6.93435243299994,15.2,7.77498479299998));
#209887=CARTESIAN_POINT('Ctrl Pts',(6.93435243299994,11.6,7.77498479299998));
#209888=CARTESIAN_POINT('Ctrl Pts',(6.93340489699994,15.2,7.77415731199999));
#209889=CARTESIAN_POINT('Ctrl Pts',(6.93340489699994,11.6,7.77415731199999));
#209890=CARTESIAN_POINT('Ctrl Pts',(6.93246470299994,15.2,7.77333463099998));
#209891=CARTESIAN_POINT('Ctrl Pts',(6.93246470299994,11.6,7.77333463099998));
#209892=CARTESIAN_POINT('Ctrl Pts',(6.93153185599994,15.2,7.77251677599998));
#209893=CARTESIAN_POINT('Ctrl Pts',(6.93153185599994,11.6,7.77251677599998));
#209894=CARTESIAN_POINT('Ctrl Pts',(6.93060636299994,15.2,7.77170377399998));
#209895=CARTESIAN_POINT('Ctrl Pts',(6.93060636299994,11.6,7.77170377399998));
#209896=CARTESIAN_POINT('Ctrl Pts',(6.92968823199994,15.2,7.77089565099998));
#209897=CARTESIAN_POINT('Ctrl Pts',(6.92968823199994,11.6,7.77089565099998));
#209898=CARTESIAN_POINT('Ctrl Pts',(6.92877746799994,15.2,7.77009243499998));
#209899=CARTESIAN_POINT('Ctrl Pts',(6.92877746799994,11.6,7.77009243499998));
#209900=CARTESIAN_POINT('Ctrl Pts',(6.92787407799995,15.2,7.76929415399999));
#209901=CARTESIAN_POINT('Ctrl Pts',(6.92787407799995,11.6,7.76929415399999));
#209902=CARTESIAN_POINT('Ctrl Pts',(6.92697806899995,15.2,7.76850083499999));
#209903=CARTESIAN_POINT('Ctrl Pts',(6.92697806899995,11.6,7.76850083499999));
#209904=CARTESIAN_POINT('Ctrl Pts',(6.92608944799994,15.2,7.76771250599998));
#209905=CARTESIAN_POINT('Ctrl Pts',(6.92608944799994,11.6,7.76771250599998));
#209906=CARTESIAN_POINT('Ctrl Pts',(6.92520822199994,15.2,7.76692919399999));
#209907=CARTESIAN_POINT('Ctrl Pts',(6.92520822199994,11.6,7.76692919399999));
#209908=CARTESIAN_POINT('Ctrl Pts',(6.92433439799994,15.2,7.76615092899998));
#209909=CARTESIAN_POINT('Ctrl Pts',(6.92433439799994,11.6,7.76615092899998));
#209910=CARTESIAN_POINT('Ctrl Pts',(6.92346798099994,15.2,7.76537773499999));
#209911=CARTESIAN_POINT('Ctrl Pts',(6.92346798099994,11.6,7.76537773499999));
#209912=CARTESIAN_POINT('Ctrl Pts',(6.92260897899994,15.2,7.76460964399998));
#209913=CARTESIAN_POINT('Ctrl Pts',(6.92260897899994,11.6,7.76460964399998));
#209914=CARTESIAN_POINT('Ctrl Pts',(6.92175739999994,15.2,7.76384668399999));
#209915=CARTESIAN_POINT('Ctrl Pts',(6.92175739999994,11.6,7.76384668399999));
#209916=CARTESIAN_POINT('Ctrl Pts',(6.92091324799994,15.2,7.76308888099998));
#209917=CARTESIAN_POINT('Ctrl Pts',(6.92091324799994,11.6,7.76308888099998));
#209918=CARTESIAN_POINT('Ctrl Pts',(6.92007653299994,15.2,7.76233626499998));
#209919=CARTESIAN_POINT('Ctrl Pts',(6.92007653299994,11.6,7.76233626499998));
#209920=CARTESIAN_POINT('Ctrl Pts',(6.91924725999994,15.2,7.76158886499999));
#209921=CARTESIAN_POINT('Ctrl Pts',(6.91924725999994,11.6,7.76158886499999));
#209922=CARTESIAN_POINT('Ctrl Pts',(6.91842543599994,15.2,7.76084670899999));
#209923=CARTESIAN_POINT('Ctrl Pts',(6.91842543599994,11.6,7.76084670899999));
#209924=CARTESIAN_POINT('Ctrl Pts',(6.91761106799994,15.2,7.76010982799999));
#209925=CARTESIAN_POINT('Ctrl Pts',(6.91761106799994,11.6,7.76010982799999));
#209926=CARTESIAN_POINT('Ctrl Pts',(6.91680416399994,15.2,7.75937824799998));
#209927=CARTESIAN_POINT('Ctrl Pts',(6.91680416399994,11.6,7.75937824799998));
#209928=CARTESIAN_POINT('Ctrl Pts',(6.91600472999994,15.2,7.75865200199998));
#209929=CARTESIAN_POINT('Ctrl Pts',(6.91600472999994,11.6,7.75865200199998));
#209930=CARTESIAN_POINT('Ctrl Pts',(6.91521277299994,15.2,7.75793111599998));
#209931=CARTESIAN_POINT('Ctrl Pts',(6.91521277299994,11.6,7.75793111599998));
#209932=CARTESIAN_POINT('Ctrl Pts',(6.91442829999994,15.2,7.75721562099999));
#209933=CARTESIAN_POINT('Ctrl Pts',(6.91442829999994,11.6,7.75721562099999));
#209934=CARTESIAN_POINT('Ctrl Pts',(6.91365131899994,15.2,7.75650554699999));
#209935=CARTESIAN_POINT('Ctrl Pts',(6.91365131899994,11.6,7.75650554699999));
#209936=CARTESIAN_POINT('Ctrl Pts',(6.91288183599994,15.2,7.75580092399998));
#209937=CARTESIAN_POINT('Ctrl Pts',(6.91288183599994,11.6,7.75580092399998));
#209938=CARTESIAN_POINT('Ctrl Pts',(6.91211985799994,15.2,7.75510178099999));
#209939=CARTESIAN_POINT('Ctrl Pts',(6.91211985799994,11.6,7.75510178099999));
#209940=CARTESIAN_POINT('Ctrl Pts',(6.91136539199994,15.2,7.75440814799998));
#209941=CARTESIAN_POINT('Ctrl Pts',(6.91136539199994,11.6,7.75440814799998));
#209942=CARTESIAN_POINT('Ctrl Pts',(6.91061844599994,15.2,7.75372005799999));
#209943=CARTESIAN_POINT('Ctrl Pts',(6.91061844599994,11.6,7.75372005799999));
#209944=CARTESIAN_POINT('Ctrl Pts',(6.90987902599994,15.2,7.75303753699998));
#209945=CARTESIAN_POINT('Ctrl Pts',(6.90987902599994,11.6,7.75303753699998));
#209946=CARTESIAN_POINT('Ctrl Pts',(6.90914713999994,15.2,7.75236061999999));
#209947=CARTESIAN_POINT('Ctrl Pts',(6.90914713999994,11.6,7.75236061999999));
#209948=CARTESIAN_POINT('Ctrl Pts',(6.90842279599994,15.2,7.75168933599998));
#209949=CARTESIAN_POINT('Ctrl Pts',(6.90842279599994,11.6,7.75168933599998));
#209950=CARTESIAN_POINT('Ctrl Pts',(6.90770599799994,15.2,7.75102371499998));
#209951=CARTESIAN_POINT('Ctrl Pts',(6.90770599799994,11.6,7.75102371499998));
#209952=CARTESIAN_POINT('Ctrl Pts',(6.90699675699994,15.2,7.75036378799999));
#209953=CARTESIAN_POINT('Ctrl Pts',(6.90699675699994,11.6,7.75036378799999));
#209954=CARTESIAN_POINT('Ctrl Pts',(6.90629507799994,15.2,7.74970958799998));
#209955=CARTESIAN_POINT('Ctrl Pts',(6.90629507799994,11.6,7.74970958799998));
#209956=CARTESIAN_POINT('Ctrl Pts',(6.90560096999994,15.2,7.74906114499998));
#209957=CARTESIAN_POINT('Ctrl Pts',(6.90560096999994,11.6,7.74906114499998));
#209958=CARTESIAN_POINT('Ctrl Pts',(6.90491443699995,15.2,7.74841849099998));
#209959=CARTESIAN_POINT('Ctrl Pts',(6.90491443699995,11.6,7.74841849099998));
#209960=CARTESIAN_POINT('Ctrl Pts',(6.90423548999994,15.2,7.74778165899999));
#209961=CARTESIAN_POINT('Ctrl Pts',(6.90423548999994,11.6,7.74778165899999));
#209962=CARTESIAN_POINT('Ctrl Pts',(6.90356800099994,15.2,7.74715431199999));
#209963=CARTESIAN_POINT('Ctrl Pts',(6.90356800099994,11.6,7.74715431199999));
#209964=CARTESIAN_POINT('Ctrl Pts',(6.90304077499994,15.2,7.74665780099999));
#209965=CARTESIAN_POINT('Ctrl Pts',(6.90304077499994,11.6,7.74665780099999));
#209966=CARTESIAN_POINT('Ctrl Pts',(6.90264966999995,15.2,7.74628893099998));
#209967=CARTESIAN_POINT('Ctrl Pts',(6.90264966999995,11.6,7.74628893099998));
#209968=CARTESIAN_POINT('Ctrl Pts',(6.90239167399994,15.2,7.74604536199998));
#209969=CARTESIAN_POINT('Ctrl Pts',(6.90239167399994,11.6,7.74604536199998));
#209970=CARTESIAN_POINT('Ctrl Pts',(6.90226491999994,15.2,7.74592563799998));
#209971=CARTESIAN_POINT('Ctrl Pts',(6.90226491999994,11.6,7.74592563799998));
#209972=CARTESIAN_POINT('',(6.90226491999994,12.2,7.74592563699999));
#209973=CARTESIAN_POINT('',(6.90226491999994,15.2,7.74592563699999));
#209974=CARTESIAN_POINT('',(6.90226491999994,12.2,7.74592563799998));
#209975=CARTESIAN_POINT('Ctrl Pts',(7.93573928199995,12.2,8.32310290899999));
#209976=CARTESIAN_POINT('Ctrl Pts',(7.93215544959198,12.2,8.32177216810586));
#209977=CARTESIAN_POINT('Ctrl Pts',(7.92857931898359,12.2,8.32043968349314));
#209978=CARTESIAN_POINT('Ctrl Pts',(7.92501089566235,12.2,8.31910545566979));
#209979=CARTESIAN_POINT('Ctrl Pts',(7.92144247234111,12.2,8.31777122784644));
#209980=CARTESIAN_POINT('Ctrl Pts',(7.91788175450335,12.2,8.31643525707682));
#209981=CARTESIAN_POINT('Ctrl Pts',(7.91432875270405,12.2,8.31509755705879));
#209982=CARTESIAN_POINT('Ctrl Pts',(7.91077575090475,12.2,8.31375985704076));
#209983=CARTESIAN_POINT('Ctrl Pts',(7.90723046416027,12.2,8.31242042797674));
#209984=CARTESIAN_POINT('Ctrl Pts',(7.90369291574608,12.2,8.3110793087757));
#209985=CARTESIAN_POINT('Ctrl Pts',(7.90015536668924,12.2,8.30973818933102));
#209986=CARTESIAN_POINT('Ctrl Pts',(7.89662555635958,12.2,8.3083953802692));
#209987=CARTESIAN_POINT('Ctrl Pts',(7.89310351022376,12.2,8.30705092374024));
#209988=CARTESIAN_POINT('Ctrl Pts',(7.88958146472777,12.2,8.30570646745552));
#209989=CARTESIAN_POINT('Ctrl Pts',(7.88606718263972,12.2,8.3043603634209));
#209990=CARTESIAN_POINT('Ctrl Pts',(7.88256068510114,12.2,8.3030126456364));
#209991=CARTESIAN_POINT('Ctrl Pts',(7.87905418756256,12.2,8.30166492785189));
#209992=CARTESIAN_POINT('Ctrl Pts',(7.87555547396904,12.2,8.30031559723916));
#209993=CARTESIAN_POINT('Ctrl Pts',(7.87206456249672,12.2,8.2989646830321));
#209994=CARTESIAN_POINT('Ctrl Pts',(7.8685736510244,12.2,8.29761376882504));
#209995=CARTESIAN_POINT('Ctrl Pts',(7.86509054247593,12.2,8.29626127245817));
#209996=CARTESIAN_POINT('Ctrl Pts',(7.86161525800305,12.2,8.29490723070956));
#209997=CARTESIAN_POINT('Ctrl Pts',(7.85813997353015,12.2,8.29355318896095));
#209998=CARTESIAN_POINT('Ctrl Pts',(7.85467251306878,12.2,8.29219760129846));
#209999=CARTESIAN_POINT('Ctrl Pts',(7.85121289811045,12.2,8.2908405040979));
#210000=CARTESIAN_POINT('Ctrl Pts',(7.84775328315213,12.2,8.28948340689733));
#210001=CARTESIAN_POINT('Ctrl Pts',(7.84430151397661,12.2,8.28812480174687));
#210002=CARTESIAN_POINT('Ctrl Pts',(7.84085761097567,12.2,8.28676472200483));
#210003=CARTESIAN_POINT('Ctrl Pts',(7.83741370734909,12.2,8.28540464201569));
#210004=CARTESIAN_POINT('Ctrl Pts',(7.83397767014971,12.2,8.28404308871781));
#210005=CARTESIAN_POINT('Ctrl Pts',(7.83054951952756,12.2,8.2826800971862));
#210006=CARTESIAN_POINT('Ctrl Pts',(7.82597865306934,12.2,8.28086277555672));
#210007=CARTESIAN_POINT('Ctrl Pts',(7.82142180716063,12.2,8.27904289774109));
#210008=CARTESIAN_POINT('Ctrl Pts',(7.81687903201132,12.2,8.2772205494929));
#210009=CARTESIAN_POINT('Ctrl Pts',(7.8134719504946,12.2,8.2758537882447));
#210010=CARTESIAN_POINT('Ctrl Pts',(7.81007278366381,12.2,8.27448563769937));
#210011=CARTESIAN_POINT('Ctrl Pts',(7.80668155266133,12.2,8.27311613487425));
#210012=CARTESIAN_POINT('Ctrl Pts',(7.80329032165885,12.2,8.27174663204912));
#210013=CARTESIAN_POINT('Ctrl Pts',(7.79990702573084,12.2,8.27037577563242));
#210014=CARTESIAN_POINT('Ctrl Pts',(7.79653168718572,12.2,8.2690036042658));
#210015=CARTESIAN_POINT('Ctrl Pts',(7.79203123538343,12.2,8.26717404227743));
#210016=CARTESIAN_POINT('Ctrl Pts',(7.78754492816917,12.2,8.26534214082649));
#210017=CARTESIAN_POINT('Ctrl Pts',(7.78307281573851,12.2,8.26350798777374));
#210018=CARTESIAN_POINT('Ctrl Pts',(7.77971873172017,12.2,8.26213237310913));
#210019=CARTESIAN_POINT('Ctrl Pts',(7.7763726315135,12.2,8.26075549297409));
#210020=CARTESIAN_POINT('Ctrl Pts',(7.77303453703626,12.2,8.25937738322624));
#210021=CARTESIAN_POINT('Ctrl Pts',(7.76969644255901,12.2,8.2579992734784));
#210022=CARTESIAN_POINT('Ctrl Pts',(7.76636635434213,12.2,8.25661993398352));
#210023=CARTESIAN_POINT('Ctrl Pts',(7.76304429187879,12.2,8.25523940465878));
#210024=CARTESIAN_POINT('Ctrl Pts',(7.75972222941546,12.2,8.25385887533405));
#210025=CARTESIAN_POINT('Ctrl Pts',(7.75640819301825,12.2,8.25247715455105));
#210026=CARTESIAN_POINT('Ctrl Pts',(7.7531022049706,12.2,8.25109428026813));
#210027=CARTESIAN_POINT('Ctrl Pts',(7.74979621632237,12.2,8.24971140573397));
#210028=CARTESIAN_POINT('Ctrl Pts',(7.74649827459306,12.2,8.24832737726616));
#210029=CARTESIAN_POINT('Ctrl Pts',(7.74320840103271,12.2,8.24694223473137));
#210030=CARTESIAN_POINT('Ctrl Pts',(7.73882190394833,12.2,8.24509537843771));
#210031=CARTESIAN_POINT('Ctrl Pts',(7.73444975060651,12.2,8.24324653931095));
#210032=CARTESIAN_POINT('Ctrl Pts',(7.73009199207294,12.2,8.2413958096846));
#210033=CARTESIAN_POINT('Ctrl Pts',(7.72682367302432,12.2,8.2400077624018));
#210034=CARTESIAN_POINT('Ctrl Pts',(7.72356345029108,12.2,8.23861865100442));
#210035=CARTESIAN_POINT('Ctrl Pts',(7.72031134462083,12.2,8.23722851473561));
#210036=CARTESIAN_POINT('Ctrl Pts',(7.71705923895058,12.2,8.23583837846679));
#210037=CARTESIAN_POINT('Ctrl Pts',(7.71381525122218,12.2,8.23444721781943));
#210038=CARTESIAN_POINT('Ctrl Pts',(7.71057940175531,12.2,8.23305507103681));
#210039=CARTESIAN_POINT('Ctrl Pts',(7.70734355170059,12.2,8.23166292400128));
#210040=CARTESIAN_POINT('Ctrl Pts',(7.70411584061482,12.2,8.23026979023215));
#210041=CARTESIAN_POINT('Ctrl Pts',(7.7008962890647,12.2,8.22887571073775));
#210042=CARTESIAN_POINT('Ctrl Pts',(7.69767673809946,12.2,8.22748163149661));
#210043=CARTESIAN_POINT('Ctrl Pts',(7.69446534661711,12.2,8.22608660629718));
#210044=CARTESIAN_POINT('Ctrl Pts',(7.69126213615087,12.2,8.22469067359782));
#210045=CARTESIAN_POINT('Ctrl Pts',(7.68805892568464,12.2,8.22329474089846));
#210046=CARTESIAN_POINT('Ctrl Pts',(7.68486389702898,12.2,8.22189790047096));
#210047=CARTESIAN_POINT('Ctrl Pts',(7.681677069547,12.2,8.22050019372372));
#210048=CARTESIAN_POINT('Ctrl Pts',(7.67849024206501,12.2,8.21910248697649));
#210049=CARTESIAN_POINT('Ctrl Pts',(7.67531161630202,12.2,8.21770391327344));
#210050=CARTESIAN_POINT('Ctrl Pts',(7.67214121427777,12.2,8.21630451302626));
#210051=CARTESIAN_POINT('Ctrl Pts',(7.66897081225352,12.2,8.21490511277908));
#210052=CARTESIAN_POINT('Ctrl Pts',(7.6658086330966,12.2,8.21350488585172));
#210053=CARTESIAN_POINT('Ctrl Pts',(7.66265469812714,12.2,8.21210387169435));
#210054=CARTESIAN_POINT('Ctrl Pts',(7.65950076315769,12.2,8.210702857537));
#210055=CARTESIAN_POINT('Ctrl Pts',(7.65635507218765,12.2,8.20930105643801));
#210056=CARTESIAN_POINT('Ctrl Pts',(7.65321764763385,12.2,8.20789851028074));
#210057=CARTESIAN_POINT('Ctrl Pts',(7.6500802225101,12.2,8.20649596386868));
#210058=CARTESIAN_POINT('Ctrl Pts',(7.64695106222198,12.2,8.20509267201473));
#210059=CARTESIAN_POINT('Ctrl Pts',(7.64383018956121,12.2,8.20368867464392));
#210060=CARTESIAN_POINT('Ctrl Pts',(7.6407093174674,12.2,8.20228467752817));
#210061=CARTESIAN_POINT('Ctrl Pts',(7.63759673159069,12.2,8.2008799767973));
#210062=CARTESIAN_POINT('Ctrl Pts',(7.63449245392437,12.2,8.19947461198641));
#210063=CARTESIAN_POINT('Ctrl Pts',(7.63138817625805,12.2,8.19806924717553));
#210064=CARTESIAN_POINT('Ctrl Pts',(7.62829220711722,12.2,8.19666321812894));
#210065=CARTESIAN_POINT('Ctrl Pts',(7.62520456668847,12.2,8.19525656788832));
#210066=CARTESIAN_POINT('Ctrl Pts',(7.62211692625973,12.2,8.19384991764772));
#210067=CARTESIAN_POINT('Ctrl Pts',(7.61903761517164,12.2,8.19244264523217));
#210068=CARTESIAN_POINT('Ctrl Pts',(7.61596665519988,12.2,8.19103479303333));
#210069=CARTESIAN_POINT('Ctrl Pts',(7.61289569522812,12.2,8.18962694083447));
#210070=CARTESIAN_POINT('Ctrl Pts',(7.60983308597269,12.2,8.18821850803565));
#210071=CARTESIAN_POINT('Ctrl Pts',(7.60677884804128,12.2,8.18680953742023));
#210072=CARTESIAN_POINT('Ctrl Pts',(7.60372461010986,12.2,8.18540056680481));
#210073=CARTESIAN_POINT('Ctrl Pts',(7.60067874519667,12.2,8.18399105870861));
#210074=CARTESIAN_POINT('Ctrl Pts',(7.59764127257098,12.2,8.18258105498112));
#210075=CARTESIAN_POINT('Ctrl Pts',(7.59460379994529,12.2,8.18117105125363));
#210076=CARTESIAN_POINT('Ctrl Pts',(7.59157472121646,12.2,8.17976055197292));
#210077=CARTESIAN_POINT('Ctrl Pts',(7.58855405670006,12.2,8.17834959981591));
#210078=CARTESIAN_POINT('Ctrl Pts',(7.58452650364569,12.2,8.17646833010235));
#210079=CARTESIAN_POINT('Ctrl Pts',(7.58051390929275,12.2,8.17458625549982));
#210080=CARTESIAN_POINT('Ctrl Pts',(7.57651632624155,12.2,8.17270347900832));
#210081=CARTESIAN_POINT('Ctrl Pts',(7.57251874319034,12.2,8.17082070251681));
#210082=CARTESIAN_POINT('Ctrl Pts',(7.56853617010479,12.2,8.16893722303636));
#210083=CARTESIAN_POINT('Ctrl Pts',(7.56456865833454,12.2,8.16705314343361));
#210084=CARTESIAN_POINT('Ctrl Pts',(7.56060114710487,12.2,8.16516906408757));
#210085=CARTESIAN_POINT('Ctrl Pts',(7.55664869510975,12.2,8.16328438574739));
#210086=CARTESIAN_POINT('Ctrl Pts',(7.55271135596924,12.2,8.16139921172627));
#210087=CARTESIAN_POINT('Ctrl Pts',(7.54778968164126,12.2,8.15904274400723));
#210088=CARTESIAN_POINT('Ctrl Pts',(7.542891619961,12.2,8.1566855032111));
#210089=CARTESIAN_POINT('Ctrl Pts',(7.53801727051655,12.2,8.15432769376665));
#210090=CARTESIAN_POINT('Ctrl Pts',(7.53411779074846,12.2,8.1524414461083));
#210091=CARTESIAN_POINT('Ctrl Pts',(7.53023348539883,12.2,8.1505548338999));
#210092=CARTESIAN_POINT('Ctrl Pts',(7.52636440763396,12.2,8.14866796490815));
#210093=CARTESIAN_POINT('Ctrl Pts',(7.52249533039625,12.2,8.14678109617349));
#210094=CARTESIAN_POINT('Ctrl Pts',(7.51864147712563,12.2,8.14489397024166));
#210095=CARTESIAN_POINT('Ctrl Pts',(7.5148029044775,12.2,8.14300669477627));
#210096=CARTESIAN_POINT('Ctrl Pts',(7.51096433130638,12.2,8.14111941905374));
#210097=CARTESIAN_POINT('Ctrl Pts',(7.50714103536659,12.2,8.13923199363592));
#210098=CARTESIAN_POINT('Ctrl Pts',(7.50333306782729,12.2,8.13734452669972));
#210099=CARTESIAN_POINT('Ctrl Pts',(7.49952510080683,12.2,8.13545706002067));
#210100=CARTESIAN_POINT('Ctrl Pts',(7.49573246366214,12.2,8.1335695518222));
#210101=CARTESIAN_POINT('Ctrl Pts',(7.49195520652549,12.2,8.13168211242095));
#210102=CARTESIAN_POINT('Ctrl Pts',(7.48817794887418,12.2,8.12979467276254));
#210103=CARTESIAN_POINT('Ctrl Pts',(7.4844160713158,12.2,8.12790730122882));
#210104=CARTESIAN_POINT('Ctrl Pts',(7.48066962598134,12.2,8.12602010947614));
#210105=CARTESIAN_POINT('Ctrl Pts',(7.47692318115733,12.2,8.12413291798059));
#210106=CARTESIAN_POINT('Ctrl Pts',(7.47319216701493,12.2,8.122245904425));
#210107=CARTESIAN_POINT('Ctrl Pts',(7.46947663659545,12.2,8.12035918241256));
#210108=CARTESIAN_POINT('Ctrl Pts',(7.46576110566972,12.2,8.11847246014305));
#210109=CARTESIAN_POINT('Ctrl Pts',(7.4620610583875,12.2,8.11658603009579));
#210110=CARTESIAN_POINT('Ctrl Pts',(7.45837654596549,12.2,8.11470000260414));
#210111=CARTESIAN_POINT('Ctrl Pts',(7.4546920340455,12.2,8.11281397536946));
#210112=CARTESIAN_POINT('Ctrl Pts',(7.45102305555418,12.2,8.11092835311085));
#210113=CARTESIAN_POINT('Ctrl Pts',(7.4473696647801,12.2,8.10904324778186));
#210114=CARTESIAN_POINT('Ctrl Pts',(7.44280292593917,12.2,8.10668686592799));
#210115=CARTESIAN_POINT('Ctrl Pts',(7.43826054062456,12.2,8.10433129402626));
#210116=CARTESIAN_POINT('Ctrl Pts',(7.43374261055384,12.2,8.10197675638731));
#210117=CARTESIAN_POINT('Ctrl Pts',(7.42922468048313,12.2,8.09962221874837));
#210118=CARTESIAN_POINT('Ctrl Pts',(7.42473120554358,12.2,8.09726871679834));
#210119=CARTESIAN_POINT('Ctrl Pts',(7.42026228700063,12.2,8.09491647735383));
#210120=CARTESIAN_POINT('Ctrl Pts',(7.41668715197141,12.2,8.09303468569566));
#210121=CARTESIAN_POINT('Ctrl Pts',(7.41312773254409,12.2,8.09115370204313));
#210122=CARTESIAN_POINT('Ctrl Pts',(7.40958408218534,12.2,8.08927364582963));
#210123=CARTESIAN_POINT('Ctrl Pts',(7.40604043230941,12.2,8.08739358987228));
#210124=CARTESIAN_POINT('Ctrl Pts',(7.40251254992986,12.2,8.08551446027678));
#210125=CARTESIAN_POINT('Ctrl Pts',(7.39900048798459,12.2,8.08363637628084));
#210126=CARTESIAN_POINT('Ctrl Pts',(7.3954884255608,12.2,8.08175829202902));
#210127=CARTESIAN_POINT('Ctrl Pts',(7.39199218376249,12.2,8.07988125432658));
#210128=CARTESIAN_POINT('Ctrl Pts',(7.38851181474051,12.2,8.0780053841133));
#210129=CARTESIAN_POINT('Ctrl Pts',(7.38503144619273,12.2,8.07612951415561));
#210130=CARTESIAN_POINT('Ctrl Pts',(7.38156695127788,12.2,8.07425480986715));
#210131=CARTESIAN_POINT('Ctrl Pts',(7.37811838011373,12.2,8.07238139529795));
#210132=CARTESIAN_POINT('Ctrl Pts',(7.37466980847971,12.2,8.0705079804735));
#210133=CARTESIAN_POINT('Ctrl Pts',(7.37123716157424,12.2,8.06863585487305));
#210134=CARTESIAN_POINT('Ctrl Pts',(7.36782049253923,12.2,8.06676514070704));
#210135=CARTESIAN_POINT('Ctrl Pts',(7.36440382396974,12.2,8.06489442679591));
#210136=CARTESIAN_POINT('Ctrl Pts',(7.36100313115045,12.2,8.06302512548616));
#210137=CARTESIAN_POINT('Ctrl Pts',(7.35761847053661,12.2,8.06115736097203));
#210138=CARTESIAN_POINT('Ctrl Pts',(7.35423380946162,12.2,8.05928959620341));
#210139=CARTESIAN_POINT('Ctrl Pts',(7.3508651769437,12.2,8.05742336837106));
#210140=CARTESIAN_POINT('Ctrl Pts',(7.34751262798321,12.2,8.05555880299165));
#210141=CARTESIAN_POINT('Ctrl Pts',(7.34416007902272,12.2,8.05369423761223));
#210142=CARTESIAN_POINT('Ctrl Pts',(7.34082361337521,12.2,8.05183133561638));
#210143=CARTESIAN_POINT('Ctrl Pts',(7.33750328297369,12.2,8.04997022290402));
#210144=CARTESIAN_POINT('Ctrl Pts',(7.33418295302456,12.2,8.04810911044525));
#210145=CARTESIAN_POINT('Ctrl Pts',(7.3308787572122,12.2,8.04624978857173));
#210146=CARTESIAN_POINT('Ctrl Pts',(7.32759075074379,12.2,8.04439238599291));
#210147=CARTESIAN_POINT('Ctrl Pts',(7.32430274382739,12.2,8.04253498316102));
#210148=CARTESIAN_POINT('Ctrl Pts',(7.32103092687394,12.2,8.0406794974283));
#210149=CARTESIAN_POINT('Ctrl Pts',(7.31777534997593,12.2,8.03882606193861));
#210150=CARTESIAN_POINT('Ctrl Pts',(7.3145197735215,12.2,8.03697262670143));
#210151=CARTESIAN_POINT('Ctrl Pts',(7.31128043879833,12.2,8.03512124026681));
#210152=CARTESIAN_POINT('Ctrl Pts',(7.30805739900519,12.2,8.03327203441784));
#210153=CARTESIAN_POINT('Ctrl Pts',(7.3048343587729,12.2,8.0314228283169));
#210154=CARTESIAN_POINT('Ctrl Pts',(7.30162761399941,12.2,8.02957580092479));
#210155=CARTESIAN_POINT('Ctrl Pts',(7.29843721627869,12.2,8.02773108873231));
#210156=CARTESIAN_POINT('Ctrl Pts',(7.29524681899266,12.2,8.02588637679116));
#210157=CARTESIAN_POINT('Ctrl Pts',(7.29207277096222,12.2,8.02404397850571));
#210158=CARTESIAN_POINT('Ctrl Pts',(7.28891512377484,12.2,8.02220402743375));
#210159=CARTESIAN_POINT('Ctrl Pts',(7.28496806446794,12.2,8.01990408840578));
#210160=CARTESIAN_POINT('Ctrl Pts',(7.28104663162282,12.2,8.01760797478344));
#210161=CARTESIAN_POINT('Ctrl Pts',(7.27715093224648,12.2,8.01531595165823));
#210162=CARTESIAN_POINT('Ctrl Pts',(7.27403437257556,12.2,8.01348233305813));
#210163=CARTESIAN_POINT('Ctrl Pts',(7.27093428065097,12.2,8.01165133336154));
#210164=CARTESIAN_POINT('Ctrl Pts',(7.26785071155252,12.2,8.00982308922637));
#210165=CARTESIAN_POINT('Ctrl Pts',(7.26476714287421,12.2,8.00799484534028));
#210166=CARTESIAN_POINT('Ctrl Pts',(7.26170009711222,12.2,8.00616935722518));
#210167=CARTESIAN_POINT('Ctrl Pts',(7.25864962724941,12.2,8.004346764874));
#210168=CARTESIAN_POINT('Ctrl Pts',(7.25559915697098,12.2,8.00252417227449));
#210169=CARTESIAN_POINT('Ctrl Pts',(7.25256526281118,12.2,8.00070447630863));
#210170=CARTESIAN_POINT('Ctrl Pts',(7.24954799920337,12.2,7.99888781637649));
#210171=CARTESIAN_POINT('Ctrl Pts',(7.24653073600668,12.2,7.99707115669187));
#210172=CARTESIAN_POINT('Ctrl Pts',(7.24353010407009,12.2,7.99525753293597));
#210173=CARTESIAN_POINT('Ctrl Pts',(7.24054615544128,12.2,7.99344709027103));
#210174=CARTESIAN_POINT('Ctrl Pts',(7.23756220640591,12.2,7.99163664735941));
#210175=CARTESIAN_POINT('Ctrl Pts',(7.23459494211575,12.2,7.98982938229229));
#210176=CARTESIAN_POINT('Ctrl Pts',(7.23164441723382,12.2,7.98802544236086));
#210177=CARTESIAN_POINT('Ctrl Pts',(7.2286938927539,12.2,7.98622150267522));
#210178=CARTESIAN_POINT('Ctrl Pts',(7.22576010761784,12.2,7.9844208865778));
#210179=CARTESIAN_POINT('Ctrl Pts',(7.22284311574349,12.2,7.98262374033548));
#210180=CARTESIAN_POINT('Ctrl Pts',(7.21992612347169,12.2,7.98082659384829));
#210181=CARTESIAN_POINT('Ctrl Pts',(7.21702592461531,12.2,7.97903291817943));
#210182=CARTESIAN_POINT('Ctrl Pts',(7.21414257372292,12.2,7.97724286024042));
#210183=CARTESIAN_POINT('Ctrl Pts',(7.21125922322339,12.2,7.97545280254531));
#210184=CARTESIAN_POINT('Ctrl Pts',(7.20839272224845,12.2,7.97366636282386));
#210185=CARTESIAN_POINT('Ctrl Pts',(7.20554312375747,12.2,7.97188369052478));
#210186=CARTESIAN_POINT('Ctrl Pts',(7.20269352487822,12.2,7.9701010179828));
#210187=CARTESIAN_POINT('Ctrl Pts',(7.19986082836445,12.2,7.96832211230504));
#210188=CARTESIAN_POINT('Ctrl Pts',(7.19704509076654,12.2,7.96654712704164));
#210189=CARTESIAN_POINT('Ctrl Pts',(7.19352541896098,12.2,7.9643283955833));
#210190=CARTESIAN_POINT('Ctrl Pts',(7.19003224428033,12.2,7.96211578575877));
#210191=CARTESIAN_POINT('Ctrl Pts',(7.18656567426466,12.2,7.95990959949877));
#210192=CARTESIAN_POINT('Ctrl Pts',(7.18309910424899,12.2,7.95770341323877));
#210193=CARTESIAN_POINT('Ctrl Pts',(7.17965914028098,12.2,7.95550365009514));
#210194=CARTESIAN_POINT('Ctrl Pts',(7.17624588931015,12.2,7.95331061537325));
#210195=CARTESIAN_POINT('Ctrl Pts',(7.17283263833932,12.2,7.95111758065137));
#210196=CARTESIAN_POINT('Ctrl Pts',(7.1694461011067,12.2,7.94893127249602));
#210197=CARTESIAN_POINT('Ctrl Pts',(7.16608638603865,12.2,7.94675200131582));
#210198=CARTESIAN_POINT('Ctrl Pts',(7.16272667097059,12.2,7.94457273013561));
#210199=CARTESIAN_POINT('Ctrl Pts',(7.15939377867686,12.2,7.94240049478027));
#210200=CARTESIAN_POINT('Ctrl Pts',(7.1560878177755,12.2,7.9402356111001));
#210201=CARTESIAN_POINT('Ctrl Pts',(7.15278185687413,12.2,7.93807072741993));
#210202=CARTESIAN_POINT('Ctrl Pts',(7.14950282748861,12.2,7.93591319379618));
#210203=CARTESIAN_POINT('Ctrl Pts',(7.14625083968913,12.2,7.93376333000876));
#210204=CARTESIAN_POINT('Ctrl Pts',(7.14299885188964,12.2,7.93161346622133));
#210205=CARTESIAN_POINT('Ctrl Pts',(7.13977390627385,12.2,7.92947127234795));
#210206=CARTESIAN_POINT('Ctrl Pts',(7.13657611203995,12.2,7.92733707123748));
#210207=CARTESIAN_POINT('Ctrl Pts',(7.13337831780604,12.2,7.92520287012701));
#210208=CARTESIAN_POINT('Ctrl Pts',(7.13020767530872,12.2,7.9230766632167));
#210209=CARTESIAN_POINT('Ctrl Pts',(7.12706429600539,12.2,7.92095877877295));
#210210=CARTESIAN_POINT('Ctrl Pts',(7.12392091704471,12.2,7.91884089456003));
#210211=CARTESIAN_POINT('Ctrl Pts',(7.12080480014722,12.2,7.91673133285203));
#210212=CARTESIAN_POINT('Ctrl Pts',(7.11771605791223,12.2,7.91463042877477));
#210213=CARTESIAN_POINT('Ctrl Pts',(7.11462731534056,12.2,7.91252952446851));
#210214=CARTESIAN_POINT('Ctrl Pts',(7.11156594752674,12.2,7.91043727756208));
#210215=CARTESIAN_POINT('Ctrl Pts',(7.10853206641338,12.2,7.90835402825578));
#210216=CARTESIAN_POINT('Ctrl Pts',(7.10549818530004,12.2,7.9062707789495));
#210217=CARTESIAN_POINT('Ctrl Pts',(7.10249178837982,12.2,7.90419652754905));
#210218=CARTESIAN_POINT('Ctrl Pts',(7.09951299156243,12.2,7.90213161897303));
#210219=CARTESIAN_POINT('Ctrl Pts',(7.09653419474505,12.2,7.90006671039701));
#210220=CARTESIAN_POINT('Ctrl Pts',(7.09358299699269,12.2,7.89801114594546));
#210221=CARTESIAN_POINT('Ctrl Pts',(7.0906595111579,12.2,7.89596527587549));
#210222=CARTESIAN_POINT('Ctrl Pts',(7.08773602532311,12.2,7.89391940580553));
#210223=CARTESIAN_POINT('Ctrl Pts',(7.08484025172794,12.2,7.89188323109972));
#210224=CARTESIAN_POINT('Ctrl Pts',(7.08197230492094,12.2,7.8898571085992));
#210225=CARTESIAN_POINT('Ctrl Pts',(7.07910435811394,12.2,7.88783098609868));
#210226=CARTESIAN_POINT('Ctrl Pts',(7.0762642354865,12.2,7.8858149176491));
#210227=CARTESIAN_POINT('Ctrl Pts',(7.07345205450141,12.2,7.88380926500105));
#210228=CARTESIAN_POINT('Ctrl Pts',(7.0700774374419,12.2,7.88140248191085));
#210229=CARTESIAN_POINT('Ctrl Pts',(7.06674305432533,12.2,7.87901069728202));
#210230=CARTESIAN_POINT('Ctrl Pts',(7.06344910610892,12.2,7.87663455345063));
#210231=CARTESIAN_POINT('Ctrl Pts',(7.06070414916219,12.2,7.87465443351919));
#210232=CARTESIAN_POINT('Ctrl Pts',(7.05798726968171,12.2,7.87268517585367));
#210233=CARTESIAN_POINT('Ctrl Pts',(7.05529858683709,12.2,7.87072715672729));
#210234=CARTESIAN_POINT('Ctrl Pts',(7.0520721672477,12.2,7.86837753364757));
#210235=CARTESIAN_POINT('Ctrl Pts',(7.04888634615096,12.2,7.86604409633942));
#210236=CARTESIAN_POINT('Ctrl Pts',(7.04574132989866,12.2,7.86372750921406));
#210237=CARTESIAN_POINT('Ctrl Pts',(7.04259631393203,12.2,7.86141092229912));
#210238=CARTESIAN_POINT('Ctrl Pts',(7.03949210049268,12.2,7.85911118625966));
#210239=CARTESIAN_POINT('Ctrl Pts',(7.03642889350682,12.2,7.85682898149892));
#210240=CARTESIAN_POINT('Ctrl Pts',(7.03336568652096,12.2,7.85454677673819));
#210241=CARTESIAN_POINT('Ctrl Pts',(7.030343486381,12.2,7.8522821026083));
#210242=CARTESIAN_POINT('Ctrl Pts',(7.02736249840418,12.2,7.8500356568558));
#210243=CARTESIAN_POINT('Ctrl Pts',(7.02438151015659,12.2,7.84778921089926));
#210244=CARTESIAN_POINT('Ctrl Pts',(7.02144173382242,12.2,7.84556099131991));
#210245=CARTESIAN_POINT('Ctrl Pts',(7.0185433766673,12.2,7.84335171145081));
#210246=CARTESIAN_POINT('Ctrl Pts',(7.01564501977544,12.2,7.84114243178239));
#210247=CARTESIAN_POINT('Ctrl Pts',(7.0127880823342,12.2,7.8389520900187));
#210248=CARTESIAN_POINT('Ctrl Pts',(7.00997277335495,12.2,7.8367814145984));
#210249=CARTESIAN_POINT('Ctrl Pts',(7.00715746437569,12.2,7.83461073917812));
#210250=CARTESIAN_POINT('Ctrl Pts',(7.00438378362651,12.2,7.83245973096464));
#210251=CARTESIAN_POINT('Ctrl Pts',(7.0016519426406,12.2,7.83032913262448));
#210252=CARTESIAN_POINT('Ctrl Pts',(6.99892010165468,12.2,7.82819853428435));
#210253=CARTESIAN_POINT('Ctrl Pts',(6.99623009952015,12.2,7.82608834790319));
#210254=CARTESIAN_POINT('Ctrl Pts',(6.99358215153017,12.2,7.82399933447765));
#210255=CARTESIAN_POINT('Ctrl Pts',(6.99093420329967,12.2,7.82191032086237));
#210256=CARTESIAN_POINT('Ctrl Pts',(6.98832830629821,12.2,7.8198424802241));
#210257=CARTESIAN_POINT('Ctrl Pts',(6.98576467732702,12.2,7.81779659186356));
#210258=CARTESIAN_POINT('Ctrl Pts',(6.98320104858868,12.2,7.81575070368886));
#210259=CARTESIAN_POINT('Ctrl Pts',(6.98067968938863,12.2,7.81372677060407));
#210260=CARTESIAN_POINT('Ctrl Pts',(6.97820081539348,12.2,7.81172558934244));
#210261=CARTESIAN_POINT('Ctrl Pts',(6.97572194139835,12.2,7.80972440808081));
#210262=CARTESIAN_POINT('Ctrl Pts',(6.97328555258509,12.2,7.80774597872696));
#210263=CARTESIAN_POINT('Ctrl Pts',(6.97089186975247,12.2,7.80579112346304));
#210264=CARTESIAN_POINT('Ctrl Pts',(6.96849818670243,12.2,7.80383626802155));
#210265=CARTESIAN_POINT('Ctrl Pts',(6.96614721079818,12.2,7.80190498224898));
#210266=CARTESIAN_POINT('Ctrl Pts',(6.96383916184092,12.2,7.79999810914611));
#210267=CARTESIAN_POINT('Ctrl Pts',(6.96153111309331,12.2,7.79809123621645));
#210268=CARTESIAN_POINT('Ctrl Pts',(6.95926599407201,12.2,7.7962087743418));
#210269=CARTESIAN_POINT('Ctrl Pts',(6.95704402822588,12.2,7.79435158723412));
#210270=CARTESIAN_POINT('Ctrl Pts',(6.95482206237975,12.2,7.79249440012643));
#210271=CARTESIAN_POINT('Ctrl Pts',(6.95264324974966,12.2,7.79066248473294));
#210272=CARTESIAN_POINT('Ctrl Pts',(6.95050782074098,12.2,7.78885672596344));
#210273=CARTESIAN_POINT('Ctrl Pts',(6.94837239153831,12.2,7.78705096702992));
#210274=CARTESIAN_POINT('Ctrl Pts',(6.94628034338827,12.2,7.78527136550364));
#210275=CARTESIAN_POINT('Ctrl Pts',(6.94423190826015,12.2,7.78351882657214));
#210276=CARTESIAN_POINT('Ctrl Pts',(6.9421834733181,12.2,7.78176628779983));
#210277=CARTESIAN_POINT('Ctrl Pts',(6.94017865297863,12.2,7.78004081407993));
#210278=CARTESIAN_POINT('Ctrl Pts',(6.93821767921653,12.2,7.77834333372493));
#210279=CARTESIAN_POINT('Ctrl Pts',(6.93625670545443,12.2,7.77664585336993));
#210280=CARTESIAN_POINT('Ctrl Pts',(6.93433957997591,12.2,7.77497636927441));
#210281=CARTESIAN_POINT('Ctrl Pts',(6.93246653994784,12.2,7.77333583766704));
#210282=CARTESIAN_POINT('Ctrl Pts',(6.93059349974963,12.2,7.77169530591067));
#210283=CARTESIAN_POINT('Ctrl Pts',(6.92876454473291,12.2,7.77008372582003));
#210284=CARTESIAN_POINT('Ctrl Pts',(6.92697991580536,12.2,7.76850208231921));
#210285=CARTESIAN_POINT('Ctrl Pts',(6.92519528703991,12.2,7.76692043896207));
#210286=CARTESIAN_POINT('Ctrl Pts',(6.92345498657842,12.2,7.76536873156749));
#210287=CARTESIAN_POINT('Ctrl Pts',(6.92175925679911,12.2,7.76384797328258));
#210288=CARTESIAN_POINT('Ctrl Pts',(6.9200635270198,12.2,7.76232721499769));
#210289=CARTESIAN_POINT('Ctrl Pts',(6.91841236845617,12.2,7.76083740255294));
#210290=CARTESIAN_POINT('Ctrl Pts',(6.91680603159594,12.2,7.75937958152118));
#210291=CARTESIAN_POINT('Ctrl Pts',(6.91519969458979,12.2,7.75792176035702));
#210292=CARTESIAN_POINT('Ctrl Pts',(6.91363817867246,12.2,7.75649592919676));
#210293=CARTESIAN_POINT('Ctrl Pts',(6.91212173584292,12.2,7.75510315837313));
#210294=CARTESIAN_POINT('Ctrl Pts',(6.91060529315112,12.2,7.75371038767601));
#210295=CARTESIAN_POINT('Ctrl Pts',(6.90913392473523,12.2,7.75235068106152));
#210296=CARTESIAN_POINT('Ctrl Pts',(6.90770788712233,12.2,7.75102513844449));
#210297=CARTESIAN_POINT('Ctrl Pts',(6.90581334753501,12.2,7.74926410988541));
#210298=CARTESIAN_POINT('Ctrl Pts',(6.90399882477399,12.2,7.74756337736256));
#210299=CARTESIAN_POINT('Ctrl Pts',(6.90226491999994,12.2,7.74592563799998));
#210300=CARTESIAN_POINT('Ctrl Pts',(6.90226491999994,15.2,7.74592563799998));
#210301=CARTESIAN_POINT('Ctrl Pts',(6.90356378263743,15.2,7.74715246342883));
#210302=CARTESIAN_POINT('Ctrl Pts',(6.90490788344662,15.2,7.74841464105156));
#210303=CARTESIAN_POINT('Ctrl Pts',(6.90629697055607,15.2,7.74971102712461));
#210304=CARTESIAN_POINT('Ctrl Pts',(6.90769275654571,15.2,7.75101366502659));
#210305=CARTESIAN_POINT('Ctrl Pts',(6.90913396266922,15.2,7.75235084439584));
#210306=CARTESIAN_POINT('Ctrl Pts',(6.91062032766044,15.2,7.7537214504576));
#210307=CARTESIAN_POINT('Ctrl Pts',(6.91210669251663,15.2,7.75509205639487));
#210308=CARTESIAN_POINT('Ctrl Pts',(6.91363821531548,15.2,7.75649608787712));
#210309=CARTESIAN_POINT('Ctrl Pts',(6.9152146440082,15.2,7.75793246374159));
#210310=CARTESIAN_POINT('Ctrl Pts',(6.91679107270092,15.2,7.75936883960606));
#210311=CARTESIAN_POINT('Ctrl Pts',(6.91841240633538,15.2,7.76083755757795));
#210312=CARTESIAN_POINT('Ctrl Pts',(6.92007839335548,15.2,7.76233756884657));
#210313=CARTESIAN_POINT('Ctrl Pts',(6.92174438052691,15.2,7.76383758025143));
#210314=CARTESIAN_POINT('Ctrl Pts',(6.92345502357584,15.2,7.76536888328299));
#210315=CARTESIAN_POINT('Ctrl Pts',(6.92521007267451,15.2,7.76693045587015));
#210316=CARTESIAN_POINT('Ctrl Pts',(6.92696512161377,15.2,7.76849202831548));
#210317=CARTESIAN_POINT('Ctrl Pts',(6.92876458061756,15.2,7.77008387331881));
#210318=CARTESIAN_POINT('Ctrl Pts',(6.93060820347571,15.2,7.77170499376734));
#210319=CARTESIAN_POINT('Ctrl Pts',(6.93245182633386,15.2,7.77332611421586));
#210320=CARTESIAN_POINT('Ctrl Pts',(6.93433961447518,15.2,7.77497651200411));
#210321=CARTESIAN_POINT('Ctrl Pts',(6.93627133015311,15.2,7.7766552214419));
#210322=CARTESIAN_POINT('Ctrl Pts',(6.93820304600649,15.2,7.77833393103218));
#210323=CARTESIAN_POINT('Ctrl Pts',(6.94017868713198,15.2,7.78004095115929));
#210324=CARTESIAN_POINT('Ctrl Pts',(6.94219802016165,15.2,7.78177534392233));
#210325=CARTESIAN_POINT('Ctrl Pts',(6.9442173530079,15.2,7.78350973652782));
#210326=CARTESIAN_POINT('Ctrl Pts',(6.94628037724782,15.2,7.78527149982797));
#210327=CARTESIAN_POINT('Ctrl Pts',(6.94838686008986,15.2,7.78705971959751));
#210328=CARTESIAN_POINT('Ctrl Pts',(6.95049334293191,15.2,7.78884793936704));
#210329=CARTESIAN_POINT('Ctrl Pts',(6.95264328337871,15.2,7.79066261469271));
#210330=CARTESIAN_POINT('Ctrl Pts',(6.95483645513052,15.2,7.79250285637475));
#210331=CARTESIAN_POINT('Ctrl Pts',(6.95702962688232,15.2,7.79434309805681));
#210332=CARTESIAN_POINT('Ctrl Pts',(6.95926602758718,15.2,7.79620890483925));
#210333=CARTESIAN_POINT('Ctrl Pts',(6.96154543150143,15.2,7.79809940601888));
#210334=CARTESIAN_POINT('Ctrl Pts',(6.96382483562273,15.2,7.79998990737024));
#210335=CARTESIAN_POINT('Ctrl Pts',(6.9661472434982,15.2,7.80190510779901));
#210336=CARTESIAN_POINT('Ctrl Pts',(6.96851243062895,15.2,7.80384415607239));
#210337=CARTESIAN_POINT('Ctrl Pts',(6.97127181529257,15.2,7.80610637879379));
#210338=CARTESIAN_POINT('Ctrl Pts',(6.97408942933038,15.2,7.80840106193489));
#210339=CARTESIAN_POINT('Ctrl Pts',(6.97696491948123,15.2,7.81072689831598));
#210340=CARTESIAN_POINT('Ctrl Pts',(6.97942962561266,15.2,7.81272047258974));
#210341=CARTESIAN_POINT('Ctrl Pts',(6.98193685458154,15.2,7.81473693384074));
#210342=CARTESIAN_POINT('Ctrl Pts',(6.984486386889,15.2,7.81677548136947));
#210343=CARTESIAN_POINT('Ctrl Pts',(6.98746084113191,15.2,7.81915378672707));
#210344=CARTESIAN_POINT('Ctrl Pts',(6.99049287871483,15.2,7.82156215202135));
#210345=CARTESIAN_POINT('Ctrl Pts',(6.99358215153017,15.2,7.82399933447766));
#210346=CARTESIAN_POINT('Ctrl Pts',(6.99623009952018,15.2,7.8260883479032));
#210347=CARTESIAN_POINT('Ctrl Pts',(6.99892010165468,15.2,7.82819853428434));
#210348=CARTESIAN_POINT('Ctrl Pts',(7.0016519426406,15.2,7.83032913262448));
#210349=CARTESIAN_POINT('Ctrl Pts',(7.00438378362652,15.2,7.83245973096464));
#210350=CARTESIAN_POINT('Ctrl Pts',(7.00715746437572,15.2,7.83461073917814));
#210351=CARTESIAN_POINT('Ctrl Pts',(7.00997277335495,15.2,7.8367814145984));
#210352=CARTESIAN_POINT('Ctrl Pts',(7.01278808233417,15.2,7.83895209001868));
#210353=CARTESIAN_POINT('Ctrl Pts',(7.01564501977542,15.2,7.84114243178237));
#210354=CARTESIAN_POINT('Ctrl Pts',(7.01854337666729,15.2,7.84335171145081));
#210355=CARTESIAN_POINT('Ctrl Pts',(7.02144173382244,15.2,7.84556099131992));
#210356=CARTESIAN_POINT('Ctrl Pts',(7.02438151015657,15.2,7.84778921089924));
#210357=CARTESIAN_POINT('Ctrl Pts',(7.02736249840418,15.2,7.8500356568558));
#210358=CARTESIAN_POINT('Ctrl Pts',(7.03034348638102,15.2,7.85228210260832));
#210359=CARTESIAN_POINT('Ctrl Pts',(7.03336568652096,15.2,7.85454677673819));
#210360=CARTESIAN_POINT('Ctrl Pts',(7.03642889350682,15.2,7.85682898149892));
#210361=CARTESIAN_POINT('Ctrl Pts',(7.03949210049268,15.2,7.85911118625966));
#210362=CARTESIAN_POINT('Ctrl Pts',(7.04259631393244,15.2,7.86141092229942));
#210363=CARTESIAN_POINT('Ctrl Pts',(7.04574132989874,15.2,7.86372750921412));
#210364=CARTESIAN_POINT('Ctrl Pts',(7.04888634615073,15.2,7.86604409633925));
#210365=CARTESIAN_POINT('Ctrl Pts',(7.05207216724769,15.2,7.86837753364757));
#210366=CARTESIAN_POINT('Ctrl Pts',(7.05529858683709,15.2,7.87072715672729));
#210367=CARTESIAN_POINT('Ctrl Pts',(7.05798726968171,15.2,7.87268517585368));
#210368=CARTESIAN_POINT('Ctrl Pts',(7.0607041491622,15.2,7.87465443351919));
#210369=CARTESIAN_POINT('Ctrl Pts',(7.06344910610893,15.2,7.87663455345063));
#210370=CARTESIAN_POINT('Ctrl Pts',(7.06619406305566,15.2,7.87861467338206));
#210371=CARTESIAN_POINT('Ctrl Pts',(7.06896710005286,15.2,7.88060565486091));
#210372=CARTESIAN_POINT('Ctrl Pts',(7.07176810012459,15.2,7.88260712652842));
#210373=CARTESIAN_POINT('Ctrl Pts',(7.07456909989099,15.2,7.88460859797777));
#210374=CARTESIAN_POINT('Ctrl Pts',(7.077398064901,15.2,7.88662055850115));
#210375=CARTESIAN_POINT('Ctrl Pts',(7.08025487639288,15.2,7.88864264425214));
#210376=CARTESIAN_POINT('Ctrl Pts',(7.08311168819617,15.2,7.89066473022354));
#210377=CARTESIAN_POINT('Ctrl Pts',(7.08599634966565,15.2,7.89269694209479));
#210378=CARTESIAN_POINT('Ctrl Pts',(7.08890874563561,15.2,7.89473891973287));
#210379=CARTESIAN_POINT('Ctrl Pts',(7.09182114160556,15.2,7.89678089737096));
#210380=CARTESIAN_POINT('Ctrl Pts',(7.09476127381467,15.2,7.89883264054175));
#210381=CARTESIAN_POINT('Ctrl Pts',(7.09772902590546,15.2,7.90089379751906));
#210382=CARTESIAN_POINT('Ctrl Pts',(7.10069677799626,15.2,7.90295495449638));
#210383=CARTESIAN_POINT('Ctrl Pts',(7.10369215273713,15.2,7.90502552475338));
#210384=CARTESIAN_POINT('Ctrl Pts',(7.10671503606901,15.2,7.90710516086401));
#210385=CARTESIAN_POINT('Ctrl Pts',(7.11034249626498,15.2,7.90960072433278));
#210386=CARTESIAN_POINT('Ctrl Pts',(7.11400956662419,15.2,7.91210934346984));
#210387=CARTESIAN_POINT('Ctrl Pts',(7.11771605791223,15.2,7.91463042877477));
#210388=CARTESIAN_POINT('Ctrl Pts',(7.12080480014725,15.2,7.91673133285204));
#210389=CARTESIAN_POINT('Ctrl Pts',(7.12392091704472,15.2,7.91884089456004));
#210390=CARTESIAN_POINT('Ctrl Pts',(7.1270642960054,15.2,7.92095877877295));
#210391=CARTESIAN_POINT('Ctrl Pts',(7.13020767530871,15.2,7.9230766632167));
#210392=CARTESIAN_POINT('Ctrl Pts',(7.13337831780605,15.2,7.92520287012702));
#210393=CARTESIAN_POINT('Ctrl Pts',(7.13657611203995,15.2,7.92733707123748));
#210394=CARTESIAN_POINT('Ctrl Pts',(7.13977390627383,15.2,7.92947127234794));
#210395=CARTESIAN_POINT('Ctrl Pts',(7.14299885188965,15.2,7.93161346622134));
#210396=CARTESIAN_POINT('Ctrl Pts',(7.14625083968913,15.2,7.93376333000876));
#210397=CARTESIAN_POINT('Ctrl Pts',(7.1495028274886,15.2,7.93591319379618));
#210398=CARTESIAN_POINT('Ctrl Pts',(7.15278185687412,15.2,7.93807072741992));
#210399=CARTESIAN_POINT('Ctrl Pts',(7.1560878177755,15.2,7.9402356111001));
#210400=CARTESIAN_POINT('Ctrl Pts',(7.15939377867686,15.2,7.94240049478027));
#210401=CARTESIAN_POINT('Ctrl Pts',(7.1627266709706,15.2,7.94457273013562));
#210402=CARTESIAN_POINT('Ctrl Pts',(7.16608638603865,15.2,7.94675200131582));
#210403=CARTESIAN_POINT('Ctrl Pts',(7.16944610110669,15.2,7.94893127249602));
#210404=CARTESIAN_POINT('Ctrl Pts',(7.17283263833933,15.2,7.95111758065138));
#210405=CARTESIAN_POINT('Ctrl Pts',(7.17624588931015,15.2,7.95331061537325));
#210406=CARTESIAN_POINT('Ctrl Pts',(7.17965914028097,15.2,7.95550365009513));
#210407=CARTESIAN_POINT('Ctrl Pts',(7.183099104249,15.2,7.95770341323877));
#210408=CARTESIAN_POINT('Ctrl Pts',(7.18656567426466,15.2,7.95990959949877));
#210409=CARTESIAN_POINT('Ctrl Pts',(7.19003224428033,15.2,7.96211578575877));
#210410=CARTESIAN_POINT('Ctrl Pts',(7.19352541896098,15.2,7.9643283955833));
#210411=CARTESIAN_POINT('Ctrl Pts',(7.19704509076654,15.2,7.96654712704164));
#210412=CARTESIAN_POINT('Ctrl Pts',(7.19986082836445,15.2,7.96832211230504));
#210413=CARTESIAN_POINT('Ctrl Pts',(7.2026935248782,15.2,7.97010101798279));
#210414=CARTESIAN_POINT('Ctrl Pts',(7.20554312375746,15.2,7.97188369052478));
#210415=CARTESIAN_POINT('Ctrl Pts',(7.20839272224847,15.2,7.97366636282387));
#210416=CARTESIAN_POINT('Ctrl Pts',(7.21125922322337,15.2,7.9754528025453));
#210417=CARTESIAN_POINT('Ctrl Pts',(7.21414257372292,15.2,7.97724286024042));
#210418=CARTESIAN_POINT('Ctrl Pts',(7.21702592461532,15.2,7.97903291817944));
#210419=CARTESIAN_POINT('Ctrl Pts',(7.21992612347168,15.2,7.98082659384829));
#210420=CARTESIAN_POINT('Ctrl Pts',(7.22284311574349,15.2,7.98262374033548));
#210421=CARTESIAN_POINT('Ctrl Pts',(7.22576010761785,15.2,7.9844208865778));
#210422=CARTESIAN_POINT('Ctrl Pts',(7.22869389275389,15.2,7.98622150267522));
#210423=CARTESIAN_POINT('Ctrl Pts',(7.23164441723383,15.2,7.98802544236086));
#210424=CARTESIAN_POINT('Ctrl Pts',(7.23459494211577,15.2,7.9898293822923));
#210425=CARTESIAN_POINT('Ctrl Pts',(7.23756220640593,15.2,7.99163664735943));
#210426=CARTESIAN_POINT('Ctrl Pts',(7.2405461554413,15.2,7.99344709027103));
#210427=CARTESIAN_POINT('Ctrl Pts',(7.24427609153222,15.2,7.99571014378721));
#210428=CARTESIAN_POINT('Ctrl Pts',(7.24803209579799,15.2,7.99797816725241));
#210429=CARTESIAN_POINT('Ctrl Pts',(7.25181406503624,15.2,8.00025087878058));
#210430=CARTESIAN_POINT('Ctrl Pts',(7.2548396401795,15.2,8.00206904785448));
#210431=CARTESIAN_POINT('Ctrl Pts',(7.25788183197334,15.2,8.00389021819185));
#210432=CARTESIAN_POINT('Ctrl Pts',(7.26094058649998,15.2,8.00571424987588));
#210433=CARTESIAN_POINT('Ctrl Pts',(7.26399934144337,15.2,8.00753828180843));
#210434=CARTESIAN_POINT('Ctrl Pts',(7.26707465909644,15.2,8.00936517352968));
#210435=CARTESIAN_POINT('Ctrl Pts',(7.27016648619862,15.2,8.01119478749881));
#210436=CARTESIAN_POINT('Ctrl Pts',(7.2740312698657,15.2,8.01348180483557));
#210437=CARTESIAN_POINT('Ctrl Pts',(7.27792184776561,15.2,8.01577307310544));
#210438=CARTESIAN_POINT('Ctrl Pts',(7.2818381170038,15.2,8.0180683263002));
#210439=CARTESIAN_POINT('Ctrl Pts',(7.28497113213824,15.2,8.01990452870589));
#210440=CARTESIAN_POINT('Ctrl Pts',(7.28812058870667,15.2,8.02174328086405));
#210441=CARTESIAN_POINT('Ctrl Pts',(7.29128643322456,15.2,8.02358444732448));
#210442=CARTESIAN_POINT('Ctrl Pts',(7.2944522781738,15.2,8.02542561403577));
#210443=CARTESIAN_POINT('Ctrl Pts',(7.29763451133135,15.2,8.02726919383593));
#210444=CARTESIAN_POINT('Ctrl Pts',(7.30083307972244,15.2,8.02911505525117));
#210445=CARTESIAN_POINT('Ctrl Pts',(7.30403164767773,15.2,8.03096091641491));
#210446=CARTESIAN_POINT('Ctrl Pts',(7.30724654915665,15.2,8.03280905748347));
#210447=CARTESIAN_POINT('Ctrl Pts',(7.31047773300255,15.2,8.03465934533207));
#210448=CARTESIAN_POINT('Ctrl Pts',(7.3137089172887,15.2,8.03650963343278));
#210449=CARTESIAN_POINT('Ctrl Pts',(7.31695638384625,15.2,8.03836206872818));
#210450=CARTESIAN_POINT('Ctrl Pts',(7.32022007752517,15.2,8.04021652138493));
#210451=CARTESIAN_POINT('Ctrl Pts',(7.32511561759888,15.2,8.04299820011739));
#210452=CARTESIAN_POINT('Ctrl Pts',(7.33004767192233,15.2,8.04578441368743));
#210453=CARTESIAN_POINT('Ctrl Pts',(7.33501606176429,15.2,8.04857472676538));
#210454=CARTESIAN_POINT('Ctrl Pts',(7.3383283219598,15.2,8.05043493565298));
#210455=CARTESIAN_POINT('Ctrl Pts',(7.34165672980724,15.2,8.05229696780573));
#210456=CARTESIAN_POINT('Ctrl Pts',(7.34500123354672,15.2,8.05416069329637));
#210457=CARTESIAN_POINT('Ctrl Pts',(7.34918186299321,15.2,8.05649035003269));
#210458=CARTESIAN_POINT('Ctrl Pts',(7.35338764442345,15.2,8.0588226551385));
#210459=CARTESIAN_POINT('Ctrl Pts',(7.35761847053662,15.2,8.06115736097203));
#210460=CARTESIAN_POINT('Ctrl Pts',(7.36100313115045,15.2,8.06302512548616));
#210461=CARTESIAN_POINT('Ctrl Pts',(7.36440382396975,15.2,8.06489442679592));
#210462=CARTESIAN_POINT('Ctrl Pts',(7.36782049253922,15.2,8.06676514070704));
#210463=CARTESIAN_POINT('Ctrl Pts',(7.37209132860021,15.2,8.06910353328709));
#210464=CARTESIAN_POINT('Ctrl Pts',(7.37638713024987,15.2,8.07144413099999));
#210465=CARTESIAN_POINT('Ctrl Pts',(7.38070779295821,15.2,8.07378669599998));
#210466=CARTESIAN_POINT('Ctrl Pts',(7.38416432331326,15.2,8.07566074810212));
#210467=CARTESIAN_POINT('Ctrl Pts',(7.38763676491183,15.2,8.07753605782662));
#210468=CARTESIAN_POINT('Ctrl Pts',(7.39112506777023,15.2,8.07941250404011));
#210469=CARTESIAN_POINT('Ctrl Pts',(7.39461337015335,15.2,8.08128894999794));
#210470=CARTESIAN_POINT('Ctrl Pts',(7.39811753065544,15.2,8.08316653394931));
#210471=CARTESIAN_POINT('Ctrl Pts',(7.40163749977249,15.2,8.0850451332487));
#210472=CARTESIAN_POINT('Ctrl Pts',(7.40515746936914,15.2,8.08692373280405));
#210473=CARTESIAN_POINT('Ctrl Pts',(7.40869324495761,15.2,8.0888033480632));
#210474=CARTESIAN_POINT('Ctrl Pts',(7.41224477659724,15.2,8.09068386033245));
#210475=CARTESIAN_POINT('Ctrl Pts',(7.41845995624073,15.2,8.09397475641931));
#210476=CARTESIAN_POINT('Ctrl Pts',(7.42472338657279,15.2,8.0972683997419));
#210477=CARTESIAN_POINT('Ctrl Pts',(7.43103478713523,15.2,8.10056415946707));
#210478=CARTESIAN_POINT('Ctrl Pts',(7.43464130216352,15.2,8.10244745095854));
#210479=CARTESIAN_POINT('Ctrl Pts',(7.43826348147363,15.2,8.10433143449833));
#210480=CARTESIAN_POINT('Ctrl Pts',(7.44190127374403,15.2,8.10621599277627));
#210481=CARTESIAN_POINT('Ctrl Pts',(7.44553906551878,15.2,8.10810055079744));
#210482=CARTESIAN_POINT('Ctrl Pts',(7.44919246907098,15.2,8.10998568487366));
#210483=CARTESIAN_POINT('Ctrl Pts',(7.45286143415835,15.2,8.11187127894169));
#210484=CARTESIAN_POINT('Ctrl Pts',(7.45653039974561,15.2,8.11375687326663));
#210485=CARTESIAN_POINT('Ctrl Pts',(7.4602149251899,15.2,8.1156429294083));
#210486=CARTESIAN_POINT('Ctrl Pts',(7.46391495955821,15.2,8.11752933173332));
#210487=CARTESIAN_POINT('Ctrl Pts',(7.46761499392653,15.2,8.11941573405834));
#210488=CARTESIAN_POINT('Ctrl Pts',(7.47133053725778,15.2,8.1213024847612));
#210489=CARTESIAN_POINT('Ctrl Pts',(7.47506153885158,15.2,8.12318947030851));
#210490=CARTESIAN_POINT('Ctrl Pts',(7.47879253993703,15.2,8.12507645559871));
#210491=CARTESIAN_POINT('Ctrl Pts',(7.48253899765449,15.2,8.12696367438608));
#210492=CARTESIAN_POINT('Ctrl Pts',(7.48630086203066,15.2,8.12885101774037));
#210493=CARTESIAN_POINT('Ctrl Pts',(7.49006272691937,15.2,8.1307383613518));
#210494=CARTESIAN_POINT('Ctrl Pts',(7.49383999707006,15.2,8.13262582863072));
#210495=CARTESIAN_POINT('Ctrl Pts',(7.49763262211165,15.2,8.13451330956692));
#210496=CARTESIAN_POINT('Ctrl Pts',(7.50142524663651,15.2,8.13640079024596));
#210497=CARTESIAN_POINT('Ctrl Pts',(7.50523322634269,15.2,8.13828828401109));
#210498=CARTESIAN_POINT('Ctrl Pts',(7.50905650886248,15.2,8.14017568207903));
#210499=CARTESIAN_POINT('Ctrl Pts',(7.51287979190317,15.2,8.14206308040412));
#210500=CARTESIAN_POINT('Ctrl Pts',(7.51671837775807,15.2,8.14395038339893));
#210501=CARTESIAN_POINT('Ctrl Pts',(7.52057221755085,15.2,8.14583748304048));
#210502=CARTESIAN_POINT('Ctrl Pts',(7.52442605681854,15.2,8.14772458242492));
#210503=CARTESIAN_POINT('Ctrl Pts',(7.52829514618711,15.2,8.14961147781384));
#210504=CARTESIAN_POINT('Ctrl Pts',(7.53217943792415,15.2,8.15149806260409));
#210505=CARTESIAN_POINT('Ctrl Pts',(7.53703480299238,15.2,8.15385629378468));
#210506=CARTESIAN_POINT('Ctrl Pts',(7.54191391844172,15.2,8.15621403873468));
#210507=CARTESIAN_POINT('Ctrl Pts',(7.54681668691272,15.2,8.15857109234583));
#210508=CARTESIAN_POINT('Ctrl Pts',(7.55270000886414,15.2,8.16139955657645));
#210509=CARTESIAN_POINT('Ctrl Pts',(7.55861739121975,15.2,8.1642270242862));
#210510=CARTESIAN_POINT('Ctrl Pts',(7.56456865833454,15.2,8.16705314343361));
#210511=CARTESIAN_POINT('Ctrl Pts',(7.56952804777705,15.2,8.16940824280868));
#210512=CARTESIAN_POINT('Ctrl Pts',(7.57451097031365,15.2,8.17176240398658));
#210513=CARTESIAN_POINT('Ctrl Pts',(7.57951732635339,15.2,8.17411542766721));
#210514=CARTESIAN_POINT('Ctrl Pts',(7.58352241140346,15.2,8.17599784671432));
#210515=CARTESIAN_POINT('Ctrl Pts',(7.58754249534214,15.2,8.17787953823468));
#210516=CARTESIAN_POINT('Ctrl Pts',(7.5915775244693,15.2,8.1797603992346));
#210517=CARTESIAN_POINT('Ctrl Pts',(7.59460379603979,15.2,8.18117104485641));
#210518=CARTESIAN_POINT('Ctrl Pts',(7.59763847602724,15.2,8.18258122312686));
#210519=CARTESIAN_POINT('Ctrl Pts',(7.60068154151379,15.2,8.18399089179038));
#210520=CARTESIAN_POINT('Ctrl Pts',(7.60372460700035,15.2,8.1854005604539));
#210521=CARTESIAN_POINT('Ctrl Pts',(7.60677605856173,15.2,8.18680971964756));
#210522=CARTESIAN_POINT('Ctrl Pts',(7.60983587544984,15.2,8.18821832684644));
#210523=CARTESIAN_POINT('Ctrl Pts',(7.61289569233794,15.2,8.18962693404532));
#210524=CARTESIAN_POINT('Ctrl Pts',(7.61596387265879,15.2,8.19103498917755));
#210525=CARTESIAN_POINT('Ctrl Pts',(7.61904039762921,15.2,8.19244244991816));
#210526=CARTESIAN_POINT('Ctrl Pts',(7.62211692315853,15.2,8.19384991091447));
#210527=CARTESIAN_POINT('Ctrl Pts',(7.62520179255686,15.2,8.19525677830226));
#210528=CARTESIAN_POINT('Ctrl Pts',(7.62829498367421,15.2,8.19666300975655));
#210529=CARTESIAN_POINT('Ctrl Pts',(7.63345030089196,15.2,8.19900672825094));
#210530=CARTESIAN_POINT('Ctrl Pts',(7.63862873644949,15.2,8.20134867962105));
#210531=CARTESIAN_POINT('Ctrl Pts',(7.64383018956121,15.2,8.20368867464392));
#210532=CARTESIAN_POINT('Ctrl Pts',(7.64799135273094,15.2,8.20556067096829));
#210533=CARTESIAN_POINT('Ctrl Pts',(7.65216724861038,15.2,8.20743141318144));
#210534=CARTESIAN_POINT('Ctrl Pts',(7.65635782628322,15.2,8.20930080628332));
#210535=CARTESIAN_POINT('Ctrl Pts',(7.65950075925237,15.2,8.21070285098238));
#210536=CARTESIAN_POINT('Ctrl Pts',(7.66265195108782,15.2,8.21210413679813));
#210537=CARTESIAN_POINT('Ctrl Pts',(7.66581137963899,15.2,8.21350462158066));
#210538=CARTESIAN_POINT('Ctrl Pts',(7.67002395142318,15.2,8.21537193479364));
#210539=CARTESIAN_POINT('Ctrl Pts',(7.67425116663779,15.2,8.21723782594256));
#210540=CARTESIAN_POINT('Ctrl Pts',(7.67849297708215,15.2,8.21910219980385));
#210541=CARTESIAN_POINT('Ctrl Pts',(7.68273478694857,15.2,8.22096657341112));
#210542=CARTESIAN_POINT('Ctrl Pts',(7.68699118905654,15.2,8.2228294300832));
#210543=CARTESIAN_POINT('Ctrl Pts',(7.69126213615087,15.2,8.22469067359782));
#210544=CARTESIAN_POINT('Ctrl Pts',(7.6944653466171,15.2,8.22608660629717));
#210545=CARTESIAN_POINT('Ctrl Pts',(7.69767673809946,15.2,8.22748163149661));
#210546=CARTESIAN_POINT('Ctrl Pts',(7.7008962890647,15.2,8.22887571073775));
#210547=CARTESIAN_POINT('Ctrl Pts',(7.70411584061482,15.2,8.23026979023215));
#210548=CARTESIAN_POINT('Ctrl Pts',(7.7073435517006,15.2,8.23166292400129));
#210549=CARTESIAN_POINT('Ctrl Pts',(7.71057940175531,15.2,8.23305507103681));
#210550=CARTESIAN_POINT('Ctrl Pts',(7.71381525122218,15.2,8.23444721781943));
#210551=CARTESIAN_POINT('Ctrl Pts',(7.71705923895058,15.2,8.23583837846679));
#210552=CARTESIAN_POINT('Ctrl Pts',(7.72031134462084,15.2,8.23722851473561));
#210553=CARTESIAN_POINT('Ctrl Pts',(7.72573152093486,15.2,8.23954540860116));
#210554=CARTESIAN_POINT('Ctrl Pts',(7.73117424467958,15.2,8.24185945493586));
#210555=CARTESIAN_POINT('Ctrl Pts',(7.73663942072308,15.2,8.24417047535227));
#210556=CARTESIAN_POINT('Ctrl Pts',(7.73991852623003,15.2,8.24555708755174));
#210557=CARTESIAN_POINT('Ctrl Pts',(7.74320571439489,15.2,8.24694260940127));
#210558=CARTESIAN_POINT('Ctrl Pts',(7.74650096385921,15.2,8.24832700460087));
#210559=CARTESIAN_POINT('Ctrl Pts',(7.74979621332352,15.2,8.24971139980047));
#210560=CARTESIAN_POINT('Ctrl Pts',(7.75309952323687,15.2,8.25109466731688));
#210561=CARTESIAN_POINT('Ctrl Pts',(7.75641087424155,15.2,8.25247676851666));
#210562=CARTESIAN_POINT('Ctrl Pts',(7.75972222524624,15.2,8.25385886971644));
#210563=CARTESIAN_POINT('Ctrl Pts',(7.76304161755893,15.2,8.25523980386629));
#210564=CARTESIAN_POINT('Ctrl Pts',(7.76636902814567,15.2,8.25661953556625));
#210565=CARTESIAN_POINT('Ctrl Pts',(7.76969643873239,15.2,8.25799926726622));
#210566=CARTESIAN_POINT('Ctrl Pts',(7.77303186940848,15.2,8.25937779563126));
#210567=CARTESIAN_POINT('Ctrl Pts',(7.7763752985781,15.2,8.26075508152518));
#210568=CARTESIAN_POINT('Ctrl Pts',(7.77971872774771,15.2,8.26213236741908));
#210569=CARTESIAN_POINT('Ctrl Pts',(7.78307015524069,15.2,8.26350841260007));
#210570=CARTESIAN_POINT('Ctrl Pts',(7.78642955978421,15.2,8.26488317846696));
#210571=CARTESIAN_POINT('Ctrl Pts',(7.79202856756017,15.2,8.26717445499503));
#210572=CARTESIAN_POINT('Ctrl Pts',(7.79764973525801,15.2,8.26946218059539));
#210573=CARTESIAN_POINT('Ctrl Pts',(7.80329296622843,15.2,8.27174618198458));
#210574=CARTESIAN_POINT('Ctrl Pts',(7.80667890530277,15.2,8.27311658301726));
#210575=CARTESIAN_POINT('Ctrl Pts',(7.8100727864627,15.2,8.27448564326624));
#210576=CARTESIAN_POINT('Ctrl Pts',(7.81347458999982,15.2,8.27585332679815));
#210577=CARTESIAN_POINT('Ctrl Pts',(7.81801032701934,15.2,8.27767690442659));
#210578=CARTESIAN_POINT('Ctrl Pts',(7.82256014663809,15.2,8.27949803396138));
#210579=CARTESIAN_POINT('Ctrl Pts',(7.82712399973012,15.2,8.28131662826542));
#210580=CARTESIAN_POINT('Ctrl Pts',(7.83054688970459,15.2,8.2826805740554));
#210581=CARTESIAN_POINT('Ctrl Pts',(7.83397767315083,15.2,8.28404309425095));
#210582=CARTESIAN_POINT('Ctrl Pts',(7.83741632965021,15.2,8.28540415211828));
#210583=CARTESIAN_POINT('Ctrl Pts',(7.84200120539916,15.2,8.28721889610623));
#210584=CARTESIAN_POINT('Ctrl Pts',(7.84660007774703,15.2,8.28903104099945));
#210585=CARTESIAN_POINT('Ctrl Pts',(7.85121289811045,15.2,8.2908405040979));
#210586=CARTESIAN_POINT('Ctrl Pts',(7.85467251306877,15.2,8.29219760129846));
#210587=CARTESIAN_POINT('Ctrl Pts',(7.85813997353016,15.2,8.29355318896095));
#210588=CARTESIAN_POINT('Ctrl Pts',(7.86161525800305,15.2,8.29490723070956));
#210589=CARTESIAN_POINT('Ctrl Pts',(7.86509054247594,15.2,8.29626127245817));
#210590=CARTESIAN_POINT('Ctrl Pts',(7.86857365102441,15.2,8.29761376882504));
#210591=CARTESIAN_POINT('Ctrl Pts',(7.87206456249672,15.2,8.2989646830321));
#210592=CARTESIAN_POINT('Ctrl Pts',(7.87555547396903,15.2,8.30031559723915));
#210593=CARTESIAN_POINT('Ctrl Pts',(7.87905418756256,15.2,8.30166492785189));
#210594=CARTESIAN_POINT('Ctrl Pts',(7.88256068510115,15.2,8.3030126456364));
#210595=CARTESIAN_POINT('Ctrl Pts',(7.88606718263973,15.2,8.30436036342091));
#210596=CARTESIAN_POINT('Ctrl Pts',(7.88958146472778,15.2,8.30570646745553));
#210597=CARTESIAN_POINT('Ctrl Pts',(7.89310351022376,15.2,8.30705092374024));
#210598=CARTESIAN_POINT('Ctrl Pts',(7.89662555635957,15.2,8.3083953802692));
#210599=CARTESIAN_POINT('Ctrl Pts',(7.90015536668925,15.2,8.30973818933102));
#210600=CARTESIAN_POINT('Ctrl Pts',(7.90369291574608,15.2,8.3110793087757));
#210601=CARTESIAN_POINT('Ctrl Pts',(7.90723046416027,15.2,8.31242042797673));
#210602=CARTESIAN_POINT('Ctrl Pts',(7.91077575090475,15.2,8.31375985704076));
#210603=CARTESIAN_POINT('Ctrl Pts',(7.91432875270405,15.2,8.31509755705879));
#210604=CARTESIAN_POINT('Ctrl Pts',(7.91788175450336,15.2,8.31643525707682));
#210605=CARTESIAN_POINT('Ctrl Pts',(7.92144247234112,15.2,8.31777122784645));
#210606=CARTESIAN_POINT('Ctrl Pts',(7.92501089566236,15.2,8.31910545566979));
#210607=CARTESIAN_POINT('Ctrl Pts',(7.92857931898359,15.2,8.32043968349314));
#210608=CARTESIAN_POINT('Ctrl Pts',(7.93215544959198,15.2,8.32177216810586));
#210609=CARTESIAN_POINT('Ctrl Pts',(7.93573928199995,15.2,8.32310290899999));
#210610=CARTESIAN_POINT('Origin',(-5.66257110645729E-14,15.2,-1.77635683940025E-14));
#210611=CARTESIAN_POINT('',(6.57080831899994,15.2,8.02901631899999));
#210612=CARTESIAN_POINT('',(6.57080831899994,12.2,8.02901631899999));
#210613=CARTESIAN_POINT('',(6.57080831899994,15.2,8.02901631899999));
#210614=CARTESIAN_POINT('Origin',(-5.66257110645729E-14,12.2,-1.77635683940025E-14));
#210615=CARTESIAN_POINT('Origin',(-5.66257110645729E-14,15.2,-1.77635683940025E-14));
#210616=CARTESIAN_POINT('Origin',(-5.66257110645729E-14,15.2,-1.77635683940025E-14));
#210617=CARTESIAN_POINT('',(6.97920857099994,15.2,9.14005731499999));
#210618=CARTESIAN_POINT('',(6.67046385465267,15.2,9.36775917498041));
#210619=CARTESIAN_POINT('Origin',(-5.66257110645729E-14,15.2,-1.77635683940025E-14));
#210620=CARTESIAN_POINT('',(6.67046385465267,12.2,9.36775917498041));
#210621=CARTESIAN_POINT('',(6.67046385499994,15.2,9.36775917499999));
#210622=CARTESIAN_POINT('',(6.97920857099994,12.2,9.14005731499999));
#210623=CARTESIAN_POINT('Origin',(-5.66257110645729E-14,12.2,-1.77635683940025E-14));
#210624=CARTESIAN_POINT('',(6.97920857099994,15.2,9.14005731499999));
#210625=CARTESIAN_POINT('Ctrl Pts',(6.67046385399994,15.2,9.36775917499999));
#210626=CARTESIAN_POINT('Ctrl Pts',(6.67046385399994,11.6,9.36775917499999));
#210627=CARTESIAN_POINT('Ctrl Pts',(6.66979225999994,15.2,9.36739372899999));
#210628=CARTESIAN_POINT('Ctrl Pts',(6.66979225999994,11.6,9.36739372899999));
#210629=CARTESIAN_POINT('Ctrl Pts',(6.66844959599994,15.2,9.36666279599999));
#210630=CARTESIAN_POINT('Ctrl Pts',(6.66844959599994,11.6,9.36666279599999));
#210631=CARTESIAN_POINT('Ctrl Pts',(6.66643717599994,15.2,9.36556626999998));
#210632=CARTESIAN_POINT('Ctrl Pts',(6.66643717599994,11.6,9.36556626999998));
#210633=CARTESIAN_POINT('Ctrl Pts',(6.66375709799994,15.2,9.36410398399998));
#210634=CARTESIAN_POINT('Ctrl Pts',(6.66375709799994,11.6,9.36410398399998));
#210635=CARTESIAN_POINT('Ctrl Pts',(6.66041225099994,15.2,9.36227570699998));
#210636=CARTESIAN_POINT('Ctrl Pts',(6.66041225099994,11.6,9.36227570699998));
#210637=CARTESIAN_POINT('Ctrl Pts',(6.65707265499995,15.2,9.36044700999999));
#210638=CARTESIAN_POINT('Ctrl Pts',(6.65707265499995,11.6,9.36044700999999));
#210639=CARTESIAN_POINT('Ctrl Pts',(6.65373830999994,15.2,9.35861789599999));
#210640=CARTESIAN_POINT('Ctrl Pts',(6.65373830999994,11.6,9.35861789599999));
#210641=CARTESIAN_POINT('Ctrl Pts',(6.65040921899994,15.2,9.35678837099999));
#210642=CARTESIAN_POINT('Ctrl Pts',(6.65040921899994,11.6,9.35678837099999));
#210643=CARTESIAN_POINT('Ctrl Pts',(6.64708538299994,15.2,9.35495843699999));
#210644=CARTESIAN_POINT('Ctrl Pts',(6.64708538299994,11.6,9.35495843699999));
#210645=CARTESIAN_POINT('Ctrl Pts',(6.64376680599994,15.2,9.35312810399999));
#210646=CARTESIAN_POINT('Ctrl Pts',(6.64376680599994,11.6,9.35312810399999));
#210647=CARTESIAN_POINT('Ctrl Pts',(6.64045349299994,15.2,9.35129737899998));
#210648=CARTESIAN_POINT('Ctrl Pts',(6.64045349299994,11.6,9.35129737899998));
#210649=CARTESIAN_POINT('Ctrl Pts',(6.63714544599994,15.2,9.34946627399999));
#210650=CARTESIAN_POINT('Ctrl Pts',(6.63714544599994,11.6,9.34946627399999));
#210651=CARTESIAN_POINT('Ctrl Pts',(6.63384266999994,15.2,9.34763479799999));
#210652=CARTESIAN_POINT('Ctrl Pts',(6.63384266999994,11.6,9.34763479799999));
#210653=CARTESIAN_POINT('Ctrl Pts',(6.63054516999994,15.2,9.34580296099998));
#210654=CARTESIAN_POINT('Ctrl Pts',(6.63054516999994,11.6,9.34580296099998));
#210655=CARTESIAN_POINT('Ctrl Pts',(6.62725294799994,15.2,9.34397077399998));
#210656=CARTESIAN_POINT('Ctrl Pts',(6.62725294799994,11.6,9.34397077399998));
#210657=CARTESIAN_POINT('Ctrl Pts',(6.62396601099994,15.2,9.34213824399999));
#210658=CARTESIAN_POINT('Ctrl Pts',(6.62396601099994,11.6,9.34213824399999));
#210659=CARTESIAN_POINT('Ctrl Pts',(6.62068435999994,15.2,9.34030537999998));
#210660=CARTESIAN_POINT('Ctrl Pts',(6.62068435999994,11.6,9.34030537999998));
#210661=CARTESIAN_POINT('Ctrl Pts',(6.61740799799994,15.2,9.33847218999999));
#210662=CARTESIAN_POINT('Ctrl Pts',(6.61740799799994,11.6,9.33847218999999));
#210663=CARTESIAN_POINT('Ctrl Pts',(6.61413692799995,15.2,9.33663867999999));
#210664=CARTESIAN_POINT('Ctrl Pts',(6.61413692799995,11.6,9.33663867999999));
#210665=CARTESIAN_POINT('Ctrl Pts',(6.61087115499994,15.2,9.33480485999999));
#210666=CARTESIAN_POINT('Ctrl Pts',(6.61087115499994,11.6,9.33480485999999));
#210667=CARTESIAN_POINT('Ctrl Pts',(6.60761068099994,15.2,9.33297073499999));
#210668=CARTESIAN_POINT('Ctrl Pts',(6.60761068099994,11.6,9.33297073499999));
#210669=CARTESIAN_POINT('Ctrl Pts',(6.60435550799994,15.2,9.33113631499998));
#210670=CARTESIAN_POINT('Ctrl Pts',(6.60435550799994,11.6,9.33113631499998));
#210671=CARTESIAN_POINT('Ctrl Pts',(6.60110564199995,15.2,9.32930160899998));
#210672=CARTESIAN_POINT('Ctrl Pts',(6.60110564199995,11.6,9.32930160899998));
#210673=CARTESIAN_POINT('Ctrl Pts',(6.59786108499994,15.2,9.32746662499999));
#210674=CARTESIAN_POINT('Ctrl Pts',(6.59786108499994,11.6,9.32746662499999));
#210675=CARTESIAN_POINT('Ctrl Pts',(6.59462184299994,15.2,9.32563137199999));
#210676=CARTESIAN_POINT('Ctrl Pts',(6.59462184299994,11.6,9.32563137199999));
#210677=CARTESIAN_POINT('Ctrl Pts',(6.59138791599994,15.2,9.32379585899999));
#210678=CARTESIAN_POINT('Ctrl Pts',(6.59138791599994,11.6,9.32379585899999));
#210679=CARTESIAN_POINT('Ctrl Pts',(6.58815930899994,15.2,9.32196009399998));
#210680=CARTESIAN_POINT('Ctrl Pts',(6.58815930899994,11.6,9.32196009399998));
#210681=CARTESIAN_POINT('Ctrl Pts',(6.58493602699994,15.2,9.32012408699999));
#210682=CARTESIAN_POINT('Ctrl Pts',(6.58493602699994,11.6,9.32012408699999));
#210683=CARTESIAN_POINT('Ctrl Pts',(6.58171807199994,15.2,9.31828784399999));
#210684=CARTESIAN_POINT('Ctrl Pts',(6.58171807199994,11.6,9.31828784399999));
#210685=CARTESIAN_POINT('Ctrl Pts',(6.57850544799994,15.2,9.31645137699999));
#210686=CARTESIAN_POINT('Ctrl Pts',(6.57850544799994,11.6,9.31645137699999));
#210687=CARTESIAN_POINT('Ctrl Pts',(6.57529815699994,15.2,9.31461469099998));
#210688=CARTESIAN_POINT('Ctrl Pts',(6.57529815699994,11.6,9.31461469099998));
#210689=CARTESIAN_POINT('Ctrl Pts',(6.57209620299994,15.2,9.31277779599998));
#210690=CARTESIAN_POINT('Ctrl Pts',(6.57209620299994,11.6,9.31277779599998));
#210691=CARTESIAN_POINT('Ctrl Pts',(6.56889959099995,15.2,9.31094069999999));
#210692=CARTESIAN_POINT('Ctrl Pts',(6.56889959099995,11.6,9.31094069999999));
#210693=CARTESIAN_POINT('Ctrl Pts',(6.56570832199994,15.2,9.30910341199999));
#210694=CARTESIAN_POINT('Ctrl Pts',(6.56570832199994,11.6,9.30910341199999));
#210695=CARTESIAN_POINT('Ctrl Pts',(6.56252240099994,15.2,9.30726594099998));
#210696=CARTESIAN_POINT('Ctrl Pts',(6.56252240099994,11.6,9.30726594099998));
#210697=CARTESIAN_POINT('Ctrl Pts',(6.55934183199994,15.2,9.30542829599998));
#210698=CARTESIAN_POINT('Ctrl Pts',(6.55934183199994,11.6,9.30542829599998));
#210699=CARTESIAN_POINT('Ctrl Pts',(6.55616661699994,15.2,9.30359048399998));
#210700=CARTESIAN_POINT('Ctrl Pts',(6.55616661699994,11.6,9.30359048399998));
#210701=CARTESIAN_POINT('Ctrl Pts',(6.55299675999995,15.2,9.30175251599999));
#210702=CARTESIAN_POINT('Ctrl Pts',(6.55299675999995,11.6,9.30175251599999));
#210703=CARTESIAN_POINT('Ctrl Pts',(6.54983226499994,15.2,9.29991439899998));
#210704=CARTESIAN_POINT('Ctrl Pts',(6.54983226499994,11.6,9.29991439899998));
#210705=CARTESIAN_POINT('Ctrl Pts',(6.54667313399995,15.2,9.29807614199999));
#210706=CARTESIAN_POINT('Ctrl Pts',(6.54667313399995,11.6,9.29807614199999));
#210707=CARTESIAN_POINT('Ctrl Pts',(6.54351937199994,15.2,9.29623775399998));
#210708=CARTESIAN_POINT('Ctrl Pts',(6.54351937199994,11.6,9.29623775399998));
#210709=CARTESIAN_POINT('Ctrl Pts',(6.54037098099994,15.2,9.29439924499999));
#210710=CARTESIAN_POINT('Ctrl Pts',(6.54037098099994,11.6,9.29439924499999));
#210711=CARTESIAN_POINT('Ctrl Pts',(6.53722796599994,15.2,9.29256062199999));
#210712=CARTESIAN_POINT('Ctrl Pts',(6.53722796599994,11.6,9.29256062199999));
#210713=CARTESIAN_POINT('Ctrl Pts',(6.53409032999994,15.2,9.29072189399999));
#210714=CARTESIAN_POINT('Ctrl Pts',(6.53409032999994,11.6,9.29072189399999));
#210715=CARTESIAN_POINT('Ctrl Pts',(6.53095807499994,15.2,9.28888306999998));
#210716=CARTESIAN_POINT('Ctrl Pts',(6.53095807499994,11.6,9.28888306999998));
#210717=CARTESIAN_POINT('Ctrl Pts',(6.52783120599994,15.2,9.28704415999999));
#210718=CARTESIAN_POINT('Ctrl Pts',(6.52783120599994,11.6,9.28704415999999));
#210719=CARTESIAN_POINT('Ctrl Pts',(6.52470972599994,15.2,9.28520517099999));
#210720=CARTESIAN_POINT('Ctrl Pts',(6.52470972599994,11.6,9.28520517099999));
#210721=CARTESIAN_POINT('Ctrl Pts',(6.52159363899995,15.2,9.28336611399999));
#210722=CARTESIAN_POINT('Ctrl Pts',(6.52159363899995,11.6,9.28336611399999));
#210723=CARTESIAN_POINT('Ctrl Pts',(6.51848294799994,15.2,9.28152699599998));
#210724=CARTESIAN_POINT('Ctrl Pts',(6.51848294799994,11.6,9.28152699599998));
#210725=CARTESIAN_POINT('Ctrl Pts',(6.51537765399994,15.2,9.27968782599999));
#210726=CARTESIAN_POINT('Ctrl Pts',(6.51537765399994,11.6,9.27968782599999));
#210727=CARTESIAN_POINT('Ctrl Pts',(6.51227776499994,15.2,9.27784861499998));
#210728=CARTESIAN_POINT('Ctrl Pts',(6.51227776499994,11.6,9.27784861499998));
#210729=CARTESIAN_POINT('Ctrl Pts',(6.50918327999994,15.2,9.27600936999998));
#210730=CARTESIAN_POINT('Ctrl Pts',(6.50918327999994,11.6,9.27600936999998));
#210731=CARTESIAN_POINT('Ctrl Pts',(6.50609420699994,15.2,9.27417009999999));
#210732=CARTESIAN_POINT('Ctrl Pts',(6.50609420699994,11.6,9.27417009999999));
#210733=CARTESIAN_POINT('Ctrl Pts',(6.50301054499994,15.2,9.27233081499999));
#210734=CARTESIAN_POINT('Ctrl Pts',(6.50301054499994,11.6,9.27233081499999));
#210735=CARTESIAN_POINT('Ctrl Pts',(6.49993229999994,15.2,9.27049152299999));
#210736=CARTESIAN_POINT('Ctrl Pts',(6.49993229999994,11.6,9.27049152299999));
#210737=CARTESIAN_POINT('Ctrl Pts',(6.49685947499994,15.2,9.26865223299998));
#210738=CARTESIAN_POINT('Ctrl Pts',(6.49685947499994,11.6,9.26865223299998));
#210739=CARTESIAN_POINT('Ctrl Pts',(6.49379207299994,15.2,9.26681295599998));
#210740=CARTESIAN_POINT('Ctrl Pts',(6.49379207299994,11.6,9.26681295599998));
#210741=CARTESIAN_POINT('Ctrl Pts',(6.49073009699994,15.2,9.26497369899998));
#210742=CARTESIAN_POINT('Ctrl Pts',(6.49073009699994,11.6,9.26497369899998));
#210743=CARTESIAN_POINT('Ctrl Pts',(6.48767355099994,15.2,9.26313447199998));
#210744=CARTESIAN_POINT('Ctrl Pts',(6.48767355099994,11.6,9.26313447199998));
#210745=CARTESIAN_POINT('Ctrl Pts',(6.48462243899994,15.2,9.26129528299998));
#210746=CARTESIAN_POINT('Ctrl Pts',(6.48462243899994,11.6,9.26129528299998));
#210747=CARTESIAN_POINT('Ctrl Pts',(6.48157676399994,15.2,9.25945614199998));
#210748=CARTESIAN_POINT('Ctrl Pts',(6.48157676399994,11.6,9.25945614199998));
#210749=CARTESIAN_POINT('Ctrl Pts',(6.47853652899994,15.2,9.25761705899999));
#210750=CARTESIAN_POINT('Ctrl Pts',(6.47853652899994,11.6,9.25761705899999));
#210751=CARTESIAN_POINT('Ctrl Pts',(6.47550173799995,15.2,9.25577804099999));
#210752=CARTESIAN_POINT('Ctrl Pts',(6.47550173799995,11.6,9.25577804099999));
#210753=CARTESIAN_POINT('Ctrl Pts',(6.47247239299994,15.2,9.25393909899999));
#210754=CARTESIAN_POINT('Ctrl Pts',(6.47247239299994,11.6,9.25393909899999));
#210755=CARTESIAN_POINT('Ctrl Pts',(6.46944849899994,15.2,9.25210024199998));
#210756=CARTESIAN_POINT('Ctrl Pts',(6.46944849899994,11.6,9.25210024199998));
#210757=CARTESIAN_POINT('Ctrl Pts',(6.46643005899994,15.2,9.25026147899998));
#210758=CARTESIAN_POINT('Ctrl Pts',(6.46643005899994,11.6,9.25026147899998));
#210759=CARTESIAN_POINT('Ctrl Pts',(6.46341707499994,15.2,9.24842281899998));
#210760=CARTESIAN_POINT('Ctrl Pts',(6.46341707499994,11.6,9.24842281899998));
#210761=CARTESIAN_POINT('Ctrl Pts',(6.46040955299994,15.2,9.24658427099999));
#210762=CARTESIAN_POINT('Ctrl Pts',(6.46040955299994,11.6,9.24658427099999));
#210763=CARTESIAN_POINT('Ctrl Pts',(6.45740749499994,15.2,9.24474584499999));
#210764=CARTESIAN_POINT('Ctrl Pts',(6.45740749499994,11.6,9.24474584499999));
#210765=CARTESIAN_POINT('Ctrl Pts',(6.45441090399994,15.2,9.24290754999999));
#210766=CARTESIAN_POINT('Ctrl Pts',(6.45441090399994,11.6,9.24290754999999));
#210767=CARTESIAN_POINT('Ctrl Pts',(6.45141978499994,15.2,9.24106939399999));
#210768=CARTESIAN_POINT('Ctrl Pts',(6.45141978499994,11.6,9.24106939399999));
#210769=CARTESIAN_POINT('Ctrl Pts',(6.44843413899994,15.2,9.23923138899998));
#210770=CARTESIAN_POINT('Ctrl Pts',(6.44843413899994,11.6,9.23923138899998));
#210771=CARTESIAN_POINT('Ctrl Pts',(6.44545397099994,15.2,9.23739354299999));
#210772=CARTESIAN_POINT('Ctrl Pts',(6.44545397099994,11.6,9.23739354299999));
#210773=CARTESIAN_POINT('Ctrl Pts',(6.44247928399994,15.2,9.23555586399999));
#210774=CARTESIAN_POINT('Ctrl Pts',(6.44247928399994,11.6,9.23555586399999));
#210775=CARTESIAN_POINT('Ctrl Pts',(6.43951008099994,15.2,9.23371836299999));
#210776=CARTESIAN_POINT('Ctrl Pts',(6.43951008099994,11.6,9.23371836299999));
#210777=CARTESIAN_POINT('Ctrl Pts',(6.43654636599994,15.2,9.23188105099998));
#210778=CARTESIAN_POINT('Ctrl Pts',(6.43654636599994,11.6,9.23188105099998));
#210779=CARTESIAN_POINT('Ctrl Pts',(6.43358814399994,15.2,9.23004393399999));
#210780=CARTESIAN_POINT('Ctrl Pts',(6.43358814399994,11.6,9.23004393399999));
#210781=CARTESIAN_POINT('Ctrl Pts',(6.43063541499994,15.2,9.22820702299998));
#210782=CARTESIAN_POINT('Ctrl Pts',(6.43063541499994,11.6,9.22820702299998));
#210783=CARTESIAN_POINT('Ctrl Pts',(6.42768818399994,15.2,9.22637032699999));
#210784=CARTESIAN_POINT('Ctrl Pts',(6.42768818399994,11.6,9.22637032699999));
#210785=CARTESIAN_POINT('Ctrl Pts',(6.42474645399994,15.2,9.22453385799999));
#210786=CARTESIAN_POINT('Ctrl Pts',(6.42474645399994,11.6,9.22453385799999));
#210787=CARTESIAN_POINT('Ctrl Pts',(6.42181022999995,15.2,9.22269762299998));
#210788=CARTESIAN_POINT('Ctrl Pts',(6.42181022999995,11.6,9.22269762299998));
#210789=CARTESIAN_POINT('Ctrl Pts',(6.41887951299994,15.2,9.22086163099999));
#210790=CARTESIAN_POINT('Ctrl Pts',(6.41887951299994,11.6,9.22086163099999));
#210791=CARTESIAN_POINT('Ctrl Pts',(6.41595430799994,15.2,9.21902589299999));
#210792=CARTESIAN_POINT('Ctrl Pts',(6.41595430799994,11.6,9.21902589299999));
#210793=CARTESIAN_POINT('Ctrl Pts',(6.41303461899994,15.2,9.21719041899999));
#210794=CARTESIAN_POINT('Ctrl Pts',(6.41303461899994,11.6,9.21719041899999));
#210795=CARTESIAN_POINT('Ctrl Pts',(6.41012044699994,15.2,9.21535521599999));
#210796=CARTESIAN_POINT('Ctrl Pts',(6.41012044699994,11.6,9.21535521599999));
#210797=CARTESIAN_POINT('Ctrl Pts',(6.40721179599994,15.2,9.21352029699998));
#210798=CARTESIAN_POINT('Ctrl Pts',(6.40721179599994,11.6,9.21352029699998));
#210799=CARTESIAN_POINT('Ctrl Pts',(6.40430867099994,15.2,9.21168566999999));
#210800=CARTESIAN_POINT('Ctrl Pts',(6.40430867099994,11.6,9.21168566999999));
#210801=CARTESIAN_POINT('Ctrl Pts',(6.40141107399994,15.2,9.20985134399999));
#210802=CARTESIAN_POINT('Ctrl Pts',(6.40141107399994,11.6,9.20985134399999));
#210803=CARTESIAN_POINT('Ctrl Pts',(6.39851900999994,15.2,9.20801732999998));
#210804=CARTESIAN_POINT('Ctrl Pts',(6.39851900999994,11.6,9.20801732999998));
#210805=CARTESIAN_POINT('Ctrl Pts',(6.39563247999994,15.2,9.20618363799999));
#210806=CARTESIAN_POINT('Ctrl Pts',(6.39563247999994,11.6,9.20618363799999));
#210807=CARTESIAN_POINT('Ctrl Pts',(6.39275148899995,15.2,9.20435027499998));
#210808=CARTESIAN_POINT('Ctrl Pts',(6.39275148899995,11.6,9.20435027499998));
#210809=CARTESIAN_POINT('Ctrl Pts',(6.38987603999994,15.2,9.20251725399999));
#210810=CARTESIAN_POINT('Ctrl Pts',(6.38987603999994,11.6,9.20251725399999));
#210811=CARTESIAN_POINT('Ctrl Pts',(6.38700613599994,15.2,9.20068458399999));
#210812=CARTESIAN_POINT('Ctrl Pts',(6.38700613599994,11.6,9.20068458399999));
#210813=CARTESIAN_POINT('Ctrl Pts',(6.38414177999994,15.2,9.19885227399998));
#210814=CARTESIAN_POINT('Ctrl Pts',(6.38414177999994,11.6,9.19885227399998));
#210815=CARTESIAN_POINT('Ctrl Pts',(6.38128297699994,15.2,9.19702033299998));
#210816=CARTESIAN_POINT('Ctrl Pts',(6.38128297699994,11.6,9.19702033299998));
#210817=CARTESIAN_POINT('Ctrl Pts',(6.37842972899994,15.2,9.19518877199998));
#210818=CARTESIAN_POINT('Ctrl Pts',(6.37842972899994,11.6,9.19518877199998));
#210819=CARTESIAN_POINT('Ctrl Pts',(6.37558203999994,15.2,9.19335760099998));
#210820=CARTESIAN_POINT('Ctrl Pts',(6.37558203999994,11.6,9.19335760099998));
#210821=CARTESIAN_POINT('Ctrl Pts',(6.37273991299994,15.2,9.19152682999999));
#210822=CARTESIAN_POINT('Ctrl Pts',(6.37273991299994,11.6,9.19152682999999));
#210823=CARTESIAN_POINT('Ctrl Pts',(6.36990335099994,15.2,9.18969646699999));
#210824=CARTESIAN_POINT('Ctrl Pts',(6.36990335099994,11.6,9.18969646699999));
#210825=CARTESIAN_POINT('Ctrl Pts',(6.36707235799994,15.2,9.18786652599999));
#210826=CARTESIAN_POINT('Ctrl Pts',(6.36707235799994,11.6,9.18786652599999));
#210827=CARTESIAN_POINT('Ctrl Pts',(6.36424693799994,15.2,9.18603701199999));
#210828=CARTESIAN_POINT('Ctrl Pts',(6.36424693799994,11.6,9.18603701199999));
#210829=CARTESIAN_POINT('Ctrl Pts',(6.36142709299994,15.2,9.18420793799999));
#210830=CARTESIAN_POINT('Ctrl Pts',(6.36142709299994,11.6,9.18420793799999));
#210831=CARTESIAN_POINT('Ctrl Pts',(6.35861282699994,15.2,9.18237931399998));
#210832=CARTESIAN_POINT('Ctrl Pts',(6.35861282699994,11.6,9.18237931399998));
#210833=CARTESIAN_POINT('Ctrl Pts',(6.35580414299994,15.2,9.18055114999999));
#210834=CARTESIAN_POINT('Ctrl Pts',(6.35580414299994,11.6,9.18055114999999));
#210835=CARTESIAN_POINT('Ctrl Pts',(6.35300104399994,15.2,9.17872345399999));
#210836=CARTESIAN_POINT('Ctrl Pts',(6.35300104399994,11.6,9.17872345399999));
#210837=CARTESIAN_POINT('Ctrl Pts',(6.35020353499994,15.2,9.17689623799999));
#210838=CARTESIAN_POINT('Ctrl Pts',(6.35020353499994,11.6,9.17689623799999));
#210839=CARTESIAN_POINT('Ctrl Pts',(6.34741161699995,15.2,9.17506951099998));
#210840=CARTESIAN_POINT('Ctrl Pts',(6.34741161699995,11.6,9.17506951099998));
#210841=CARTESIAN_POINT('Ctrl Pts',(6.34462529599994,15.2,9.17324328399998));
#210842=CARTESIAN_POINT('Ctrl Pts',(6.34462529599994,11.6,9.17324328399998));
#210843=CARTESIAN_POINT('Ctrl Pts',(6.34184457399994,15.2,9.17141756699999));
#210844=CARTESIAN_POINT('Ctrl Pts',(6.34184457399994,11.6,9.17141756699999));
#210845=CARTESIAN_POINT('Ctrl Pts',(6.33906945299994,15.2,9.16959236999999));
#210846=CARTESIAN_POINT('Ctrl Pts',(6.33906945299994,11.6,9.16959236999999));
#210847=CARTESIAN_POINT('Ctrl Pts',(6.33629993899994,15.2,9.16776770199998));
#210848=CARTESIAN_POINT('Ctrl Pts',(6.33629993899994,11.6,9.16776770199998));
#210849=CARTESIAN_POINT('Ctrl Pts',(6.33353603299994,15.2,9.16594357499999));
#210850=CARTESIAN_POINT('Ctrl Pts',(6.33353603299994,11.6,9.16594357499999));
#210851=CARTESIAN_POINT('Ctrl Pts',(6.33077773999994,15.2,9.16411999899999));
#210852=CARTESIAN_POINT('Ctrl Pts',(6.33077773999994,11.6,9.16411999899999));
#210853=CARTESIAN_POINT('Ctrl Pts',(6.32802506299995,15.2,9.16229698299999));
#210854=CARTESIAN_POINT('Ctrl Pts',(6.32802506299995,11.6,9.16229698299999));
#210855=CARTESIAN_POINT('Ctrl Pts',(6.32527800399994,15.2,9.16047453899999));
#210856=CARTESIAN_POINT('Ctrl Pts',(6.32527800399994,11.6,9.16047453899999));
#210857=CARTESIAN_POINT('Ctrl Pts',(6.32253656799994,15.2,9.15865267499999));
#210858=CARTESIAN_POINT('Ctrl Pts',(6.32253656799994,11.6,9.15865267499999));
#210859=CARTESIAN_POINT('Ctrl Pts',(6.31980075799994,15.2,9.15683140299999));
#210860=CARTESIAN_POINT('Ctrl Pts',(6.31980075799994,11.6,9.15683140299999));
#210861=CARTESIAN_POINT('Ctrl Pts',(6.31707057599994,15.2,9.15501073299998));
#210862=CARTESIAN_POINT('Ctrl Pts',(6.31707057599994,11.6,9.15501073299998));
#210863=CARTESIAN_POINT('Ctrl Pts',(6.31434602699994,15.2,9.15319067599999));
#210864=CARTESIAN_POINT('Ctrl Pts',(6.31434602699994,11.6,9.15319067599999));
#210865=CARTESIAN_POINT('Ctrl Pts',(6.31162711399995,15.2,9.15137123999998));
#210866=CARTESIAN_POINT('Ctrl Pts',(6.31162711399995,11.6,9.15137123999998));
#210867=CARTESIAN_POINT('Ctrl Pts',(6.30891383899994,15.2,9.14955243799999));
#210868=CARTESIAN_POINT('Ctrl Pts',(6.30891383899994,11.6,9.14955243799999));
#210869=CARTESIAN_POINT('Ctrl Pts',(6.30620620699994,15.2,9.14773428099998));
#210870=CARTESIAN_POINT('Ctrl Pts',(6.30620620699994,11.6,9.14773428099998));
#210871=CARTESIAN_POINT('Ctrl Pts',(6.30350422099994,15.2,9.14591677599999));
#210872=CARTESIAN_POINT('Ctrl Pts',(6.30350422099994,11.6,9.14591677599999));
#210873=CARTESIAN_POINT('Ctrl Pts',(6.30080788399994,15.2,9.14409993499999));
#210874=CARTESIAN_POINT('Ctrl Pts',(6.30080788399994,11.6,9.14409993499999));
#210875=CARTESIAN_POINT('Ctrl Pts',(6.29811719899994,15.2,9.14228377099998));
#210876=CARTESIAN_POINT('Ctrl Pts',(6.29811719899994,11.6,9.14228377099998));
#210877=CARTESIAN_POINT('Ctrl Pts',(6.29543216899994,15.2,9.14046829099998));
#210878=CARTESIAN_POINT('Ctrl Pts',(6.29543216899994,11.6,9.14046829099998));
#210879=CARTESIAN_POINT('Ctrl Pts',(6.29275279799994,15.2,9.13865350699999));
#210880=CARTESIAN_POINT('Ctrl Pts',(6.29275279799994,11.6,9.13865350699999));
#210881=CARTESIAN_POINT('Ctrl Pts',(6.29007908999994,15.2,9.13683942999998));
#210882=CARTESIAN_POINT('Ctrl Pts',(6.29007908999994,11.6,9.13683942999998));
#210883=CARTESIAN_POINT('Ctrl Pts',(6.28741104799994,15.2,9.13502606899998));
#210884=CARTESIAN_POINT('Ctrl Pts',(6.28741104799994,11.6,9.13502606899998));
#210885=CARTESIAN_POINT('Ctrl Pts',(6.28474867399994,15.2,9.13321343699998));
#210886=CARTESIAN_POINT('Ctrl Pts',(6.28474867399994,11.6,9.13321343699998));
#210887=CARTESIAN_POINT('Ctrl Pts',(6.28209197199994,15.2,9.13140154299998));
#210888=CARTESIAN_POINT('Ctrl Pts',(6.28209197199994,11.6,9.13140154299998));
#210889=CARTESIAN_POINT('Ctrl Pts',(6.27944094699994,15.2,9.12959039799999));
#210890=CARTESIAN_POINT('Ctrl Pts',(6.27944094699994,11.6,9.12959039799999));
#210891=CARTESIAN_POINT('Ctrl Pts',(6.27679559899994,15.2,9.12778001299999));
#210892=CARTESIAN_POINT('Ctrl Pts',(6.27679559899994,11.6,9.12778001299999));
#210893=CARTESIAN_POINT('Ctrl Pts',(6.27415593399994,15.2,9.12597039899998));
#210894=CARTESIAN_POINT('Ctrl Pts',(6.27415593399994,11.6,9.12597039899998));
#210895=CARTESIAN_POINT('Ctrl Pts',(6.27152195499994,15.2,9.12416156499999));
#210896=CARTESIAN_POINT('Ctrl Pts',(6.27152195499994,11.6,9.12416156499999));
#210897=CARTESIAN_POINT('Ctrl Pts',(6.26889366399994,15.2,9.12235352399998));
#210898=CARTESIAN_POINT('Ctrl Pts',(6.26889366399994,11.6,9.12235352399998));
#210899=CARTESIAN_POINT('Ctrl Pts',(6.26627106499994,15.2,9.12054628599999));
#210900=CARTESIAN_POINT('Ctrl Pts',(6.26627106499994,11.6,9.12054628599999));
#210901=CARTESIAN_POINT('Ctrl Pts',(6.26365416199994,15.2,9.11873985999998));
#210902=CARTESIAN_POINT('Ctrl Pts',(6.26365416199994,11.6,9.11873985999998));
#210903=CARTESIAN_POINT('Ctrl Pts',(6.26104295599994,15.2,9.11693425999999));
#210904=CARTESIAN_POINT('Ctrl Pts',(6.26104295599994,11.6,9.11693425999999));
#210905=CARTESIAN_POINT('Ctrl Pts',(6.25843745399994,15.2,9.11512949599998));
#210906=CARTESIAN_POINT('Ctrl Pts',(6.25843745399994,11.6,9.11512949599998));
#210907=CARTESIAN_POINT('Ctrl Pts',(6.25583765699994,15.2,9.11332557699998));
#210908=CARTESIAN_POINT('Ctrl Pts',(6.25583765699994,11.6,9.11332557699998));
#210909=CARTESIAN_POINT('Ctrl Pts',(6.25324356799994,15.2,9.11152251499999));
#210910=CARTESIAN_POINT('Ctrl Pts',(6.25324356799994,11.6,9.11152251499999));
#210911=CARTESIAN_POINT('Ctrl Pts',(6.25065519099994,15.2,9.10972032199999));
#210912=CARTESIAN_POINT('Ctrl Pts',(6.25065519099994,11.6,9.10972032199999));
#210913=CARTESIAN_POINT('Ctrl Pts',(6.24807252799994,15.2,9.10791900599998));
#210914=CARTESIAN_POINT('Ctrl Pts',(6.24807252799994,11.6,9.10791900599998));
#210915=CARTESIAN_POINT('Ctrl Pts',(6.24549558499995,15.2,9.10611858299998));
#210916=CARTESIAN_POINT('Ctrl Pts',(6.24549558499995,11.6,9.10611858299998));
#210917=CARTESIAN_POINT('Ctrl Pts',(6.24292436299994,15.2,9.10431905899999));
#210918=CARTESIAN_POINT('Ctrl Pts',(6.24292436299994,11.6,9.10431905899999));
#210919=CARTESIAN_POINT('Ctrl Pts',(6.24035886599994,15.2,9.10252044899998));
#210920=CARTESIAN_POINT('Ctrl Pts',(6.24035886599994,11.6,9.10252044899998));
#210921=CARTESIAN_POINT('Ctrl Pts',(6.23779909799994,15.2,9.10072276099999));
#210922=CARTESIAN_POINT('Ctrl Pts',(6.23779909799994,11.6,9.10072276099999));
#210923=CARTESIAN_POINT('Ctrl Pts',(6.23524505999994,15.2,9.09892600699998));
#210924=CARTESIAN_POINT('Ctrl Pts',(6.23524505999994,11.6,9.09892600699998));
#210925=CARTESIAN_POINT('Ctrl Pts',(6.23269675799994,15.2,9.09713019899998));
#210926=CARTESIAN_POINT('Ctrl Pts',(6.23269675799994,11.6,9.09713019899998));
#210927=CARTESIAN_POINT('Ctrl Pts',(6.23015419399994,15.2,9.09533534799999));
#210928=CARTESIAN_POINT('Ctrl Pts',(6.23015419399994,11.6,9.09533534799999));
#210929=CARTESIAN_POINT('Ctrl Pts',(6.22761737199995,15.2,9.09354146399998));
#210930=CARTESIAN_POINT('Ctrl Pts',(6.22761737199995,11.6,9.09354146399998));
#210931=CARTESIAN_POINT('Ctrl Pts',(6.22508629399994,15.2,9.09174855899998));
#210932=CARTESIAN_POINT('Ctrl Pts',(6.22508629399994,11.6,9.09174855899998));
#210933=CARTESIAN_POINT('Ctrl Pts',(6.22256096399994,15.2,9.08995664499999));
#210934=CARTESIAN_POINT('Ctrl Pts',(6.22256096399994,11.6,9.08995664499999));
#210935=CARTESIAN_POINT('Ctrl Pts',(6.22004138599995,15.2,9.08816573299998));
#210936=CARTESIAN_POINT('Ctrl Pts',(6.22004138599995,11.6,9.08816573299998));
#210937=CARTESIAN_POINT('Ctrl Pts',(6.21752756199994,15.2,9.08637583199998));
#210938=CARTESIAN_POINT('Ctrl Pts',(6.21752756199994,11.6,9.08637583199998));
#210939=CARTESIAN_POINT('Ctrl Pts',(6.21501949499994,15.2,9.08458695699998));
#210940=CARTESIAN_POINT('Ctrl Pts',(6.21501949499994,11.6,9.08458695699998));
#210941=CARTESIAN_POINT('Ctrl Pts',(6.21251718999994,15.2,9.08279911699999));
#210942=CARTESIAN_POINT('Ctrl Pts',(6.21251718999994,11.6,9.08279911699999));
#210943=CARTESIAN_POINT('Ctrl Pts',(6.21002064899994,15.2,9.08101232299998));
#210944=CARTESIAN_POINT('Ctrl Pts',(6.21002064899994,11.6,9.08101232299998));
#210945=CARTESIAN_POINT('Ctrl Pts',(6.20752987599994,15.2,9.07922658799999));
#210946=CARTESIAN_POINT('Ctrl Pts',(6.20752987599994,11.6,9.07922658799999));
#210947=CARTESIAN_POINT('Ctrl Pts',(6.20504487399994,15.2,9.07744192299998));
#210948=CARTESIAN_POINT('Ctrl Pts',(6.20504487399994,11.6,9.07744192299998));
#210949=CARTESIAN_POINT('Ctrl Pts',(6.20256564499994,15.2,9.07565833799998));
#210950=CARTESIAN_POINT('Ctrl Pts',(6.20256564499994,11.6,9.07565833799998));
#210951=CARTESIAN_POINT('Ctrl Pts',(6.20009219499994,15.2,9.07387584599999));
#210952=CARTESIAN_POINT('Ctrl Pts',(6.20009219499994,11.6,9.07387584599999));
#210953=CARTESIAN_POINT('Ctrl Pts',(6.19762452399995,15.2,9.07209445799998));
#210954=CARTESIAN_POINT('Ctrl Pts',(6.19762452399995,11.6,9.07209445799998));
#210955=CARTESIAN_POINT('Ctrl Pts',(6.19516263699994,15.2,9.07031418699999));
#210956=CARTESIAN_POINT('Ctrl Pts',(6.19516263699994,11.6,9.07031418699999));
#210957=CARTESIAN_POINT('Ctrl Pts',(6.19270653899994,15.2,9.06853504199999));
#210958=CARTESIAN_POINT('Ctrl Pts',(6.19270653899994,11.6,9.06853504199999));
#210959=CARTESIAN_POINT('Ctrl Pts',(6.19025622999994,15.2,9.06675703599999));
#210960=CARTESIAN_POINT('Ctrl Pts',(6.19025622999994,11.6,9.06675703599999));
#210961=CARTESIAN_POINT('Ctrl Pts',(6.18781171499994,15.2,9.06498017999999));
#210962=CARTESIAN_POINT('Ctrl Pts',(6.18781171499994,11.6,9.06498017999999));
#210963=CARTESIAN_POINT('Ctrl Pts',(6.18537299699994,15.2,9.06320448699999));
#210964=CARTESIAN_POINT('Ctrl Pts',(6.18537299699994,11.6,9.06320448699999));
#210965=CARTESIAN_POINT('Ctrl Pts',(6.18294007899994,15.2,9.06142996799998));
#210966=CARTESIAN_POINT('Ctrl Pts',(6.18294007899994,11.6,9.06142996799998));
#210967=CARTESIAN_POINT('Ctrl Pts',(6.18051296399994,15.2,9.05965663499998));
#210968=CARTESIAN_POINT('Ctrl Pts',(6.18051296399994,11.6,9.05965663499998));
#210969=CARTESIAN_POINT('Ctrl Pts',(6.17809165599994,15.2,9.05788449699998));
#210970=CARTESIAN_POINT('Ctrl Pts',(6.17809165599994,11.6,9.05788449699998));
#210971=CARTESIAN_POINT('Ctrl Pts',(6.17567615899994,15.2,9.05611356999999));
#210972=CARTESIAN_POINT('Ctrl Pts',(6.17567615899994,11.6,9.05611356999999));
#210973=CARTESIAN_POINT('Ctrl Pts',(6.17326647299994,15.2,9.05434386299999));
#210974=CARTESIAN_POINT('Ctrl Pts',(6.17326647299994,11.6,9.05434386299999));
#210975=CARTESIAN_POINT('Ctrl Pts',(6.17086260499994,15.2,9.05257538899999));
#210976=CARTESIAN_POINT('Ctrl Pts',(6.17086260499994,11.6,9.05257538899999));
#210977=CARTESIAN_POINT('Ctrl Pts',(6.16846455699994,15.2,9.05080815899998));
#210978=CARTESIAN_POINT('Ctrl Pts',(6.16846455699994,11.6,9.05080815899998));
#210979=CARTESIAN_POINT('Ctrl Pts',(6.16607233099994,15.2,9.04904218599999));
#210980=CARTESIAN_POINT('Ctrl Pts',(6.16607233099994,11.6,9.04904218599999));
#210981=CARTESIAN_POINT('Ctrl Pts',(6.16368593199994,15.2,9.04727748099998));
#210982=CARTESIAN_POINT('Ctrl Pts',(6.16368593199994,11.6,9.04727748099998));
#210983=CARTESIAN_POINT('Ctrl Pts',(6.16130536099995,15.2,9.04551405599998));
#210984=CARTESIAN_POINT('Ctrl Pts',(6.16130536099995,11.6,9.04551405599998));
#210985=CARTESIAN_POINT('Ctrl Pts',(6.15893062299994,15.2,9.04375192399998));
#210986=CARTESIAN_POINT('Ctrl Pts',(6.15893062299994,11.6,9.04375192399998));
#210987=CARTESIAN_POINT('Ctrl Pts',(6.15656172199994,15.2,9.04199109599999));
#210988=CARTESIAN_POINT('Ctrl Pts',(6.15656172199994,11.6,9.04199109599999));
#210989=CARTESIAN_POINT('Ctrl Pts',(6.15419865899994,15.2,9.04023158399998));
#210990=CARTESIAN_POINT('Ctrl Pts',(6.15419865899994,11.6,9.04023158399998));
#210991=CARTESIAN_POINT('Ctrl Pts',(6.15184143899994,15.2,9.03847339999999));
#210992=CARTESIAN_POINT('Ctrl Pts',(6.15184143899994,11.6,9.03847339999999));
#210993=CARTESIAN_POINT('Ctrl Pts',(6.14949006299994,15.2,9.03671655699998));
#210994=CARTESIAN_POINT('Ctrl Pts',(6.14949006299994,11.6,9.03671655699998));
#210995=CARTESIAN_POINT('Ctrl Pts',(6.14714453699994,15.2,9.03496106599999));
#210996=CARTESIAN_POINT('Ctrl Pts',(6.14714453699994,11.6,9.03496106599999));
#210997=CARTESIAN_POINT('Ctrl Pts',(6.14480486199994,15.2,9.03320694099998));
#210998=CARTESIAN_POINT('Ctrl Pts',(6.14480486199994,11.6,9.03320694099998));
#210999=CARTESIAN_POINT('Ctrl Pts',(6.14247104399994,15.2,9.03145419099998));
#211000=CARTESIAN_POINT('Ctrl Pts',(6.14247104399994,11.6,9.03145419099998));
#211001=CARTESIAN_POINT('Ctrl Pts',(6.14014308399994,15.2,9.02970283199998));
#211002=CARTESIAN_POINT('Ctrl Pts',(6.14014308399994,11.6,9.02970283199998));
#211003=CARTESIAN_POINT('Ctrl Pts',(6.13782098399994,15.2,9.02795287399999));
#211004=CARTESIAN_POINT('Ctrl Pts',(6.13782098399994,11.6,9.02795287399999));
#211005=CARTESIAN_POINT('Ctrl Pts',(6.13550474899994,15.2,9.02620432899998));
#211006=CARTESIAN_POINT('Ctrl Pts',(6.13550474899994,11.6,9.02620432899998));
#211007=CARTESIAN_POINT('Ctrl Pts',(6.13319438299994,15.2,9.02445720999999));
#211008=CARTESIAN_POINT('Ctrl Pts',(6.13319438299994,11.6,9.02445720999999));
#211009=CARTESIAN_POINT('Ctrl Pts',(6.13088988899994,15.2,9.02271152899999));
#211010=CARTESIAN_POINT('Ctrl Pts',(6.13088988899994,11.6,9.02271152899999));
#211011=CARTESIAN_POINT('Ctrl Pts',(6.12859126799994,15.2,9.02096729899998));
#211012=CARTESIAN_POINT('Ctrl Pts',(6.12859126799994,11.6,9.02096729899998));
#211013=CARTESIAN_POINT('Ctrl Pts',(6.12629852499994,15.2,9.01922453199998));
#211014=CARTESIAN_POINT('Ctrl Pts',(6.12629852499994,11.6,9.01922453199998));
#211015=CARTESIAN_POINT('Ctrl Pts',(6.12401166399994,15.2,9.01748324099999));
#211016=CARTESIAN_POINT('Ctrl Pts',(6.12401166399994,11.6,9.01748324099999));
#211017=CARTESIAN_POINT('Ctrl Pts',(6.12173068599994,15.2,9.01574343799999));
#211018=CARTESIAN_POINT('Ctrl Pts',(6.12173068599994,11.6,9.01574343799999));
#211019=CARTESIAN_POINT('Ctrl Pts',(6.11945559599994,15.2,9.01400513499999));
#211020=CARTESIAN_POINT('Ctrl Pts',(6.11945559599994,11.6,9.01400513499999));
#211021=CARTESIAN_POINT('Ctrl Pts',(6.11718639499994,15.2,9.01226834599999));
#211022=CARTESIAN_POINT('Ctrl Pts',(6.11718639499994,11.6,9.01226834599999));
#211023=CARTESIAN_POINT('Ctrl Pts',(6.11492308999994,15.2,9.01053308099998));
#211024=CARTESIAN_POINT('Ctrl Pts',(6.11492308999994,11.6,9.01053308099998));
#211025=CARTESIAN_POINT('Ctrl Pts',(6.11266567999994,15.2,9.00879935599999));
#211026=CARTESIAN_POINT('Ctrl Pts',(6.11266567999994,11.6,9.00879935599999));
#211027=CARTESIAN_POINT('Ctrl Pts',(6.11041416999995,15.2,9.00706718099999));
#211028=CARTESIAN_POINT('Ctrl Pts',(6.11041416999995,11.6,9.00706718099999));
#211029=CARTESIAN_POINT('Ctrl Pts',(6.10816856499994,15.2,9.00533656899999));
#211030=CARTESIAN_POINT('Ctrl Pts',(6.10816856499994,11.6,9.00533656899999));
#211031=CARTESIAN_POINT('Ctrl Pts',(6.10592886499994,15.2,9.00360753399998));
#211032=CARTESIAN_POINT('Ctrl Pts',(6.10592886499994,11.6,9.00360753399998));
#211033=CARTESIAN_POINT('Ctrl Pts',(6.10369507599994,15.2,9.00188008699999));
#211034=CARTESIAN_POINT('Ctrl Pts',(6.10369507599994,11.6,9.00188008699999));
#211035=CARTESIAN_POINT('Ctrl Pts',(6.10146719899994,15.2,9.00015424299998));
#211036=CARTESIAN_POINT('Ctrl Pts',(6.10146719899994,11.6,9.00015424299998));
#211037=CARTESIAN_POINT('Ctrl Pts',(6.09924523799994,15.2,8.99843001299999));
#211038=CARTESIAN_POINT('Ctrl Pts',(6.09924523799994,11.6,8.99843001299999));
#211039=CARTESIAN_POINT('Ctrl Pts',(6.09702919599994,15.2,8.99670740999999));
#211040=CARTESIAN_POINT('Ctrl Pts',(6.09702919599994,11.6,8.99670740999999));
#211041=CARTESIAN_POINT('Ctrl Pts',(6.09481907699994,15.2,8.99498644799999));
#211042=CARTESIAN_POINT('Ctrl Pts',(6.09481907699994,11.6,8.99498644799999));
#211043=CARTESIAN_POINT('Ctrl Pts',(6.09261488399994,15.2,8.99326713799999));
#211044=CARTESIAN_POINT('Ctrl Pts',(6.09261488399994,11.6,8.99326713799999));
#211045=CARTESIAN_POINT('Ctrl Pts',(6.09041661899994,15.2,8.99154949399998));
#211046=CARTESIAN_POINT('Ctrl Pts',(6.09041661899994,11.6,8.99154949399998));
#211047=CARTESIAN_POINT('Ctrl Pts',(6.08822428599994,15.2,8.98983352999998));
#211048=CARTESIAN_POINT('Ctrl Pts',(6.08822428599994,11.6,8.98983352999998));
#211049=CARTESIAN_POINT('Ctrl Pts',(6.08603788899994,15.2,8.98811925799999));
#211050=CARTESIAN_POINT('Ctrl Pts',(6.08603788899994,11.6,8.98811925799999));
#211051=CARTESIAN_POINT('Ctrl Pts',(6.08385742999994,15.2,8.98640669099999));
#211052=CARTESIAN_POINT('Ctrl Pts',(6.08385742999994,11.6,8.98640669099999));
#211053=CARTESIAN_POINT('Ctrl Pts',(6.08168291099994,15.2,8.98469584199999));
#211054=CARTESIAN_POINT('Ctrl Pts',(6.08168291099994,11.6,8.98469584199999));
#211055=CARTESIAN_POINT('Ctrl Pts',(6.07951433799995,15.2,8.98298672299998));
#211056=CARTESIAN_POINT('Ctrl Pts',(6.07951433799995,11.6,8.98298672299998));
#211057=CARTESIAN_POINT('Ctrl Pts',(6.07735171299994,15.2,8.98127934999999));
#211058=CARTESIAN_POINT('Ctrl Pts',(6.07735171299994,11.6,8.98127934999999));
#211059=CARTESIAN_POINT('Ctrl Pts',(6.07519503899994,15.2,8.97957373399999));
#211060=CARTESIAN_POINT('Ctrl Pts',(6.07519503899994,11.6,8.97957373399999));
#211061=CARTESIAN_POINT('Ctrl Pts',(6.07304431899995,15.2,8.97786988899998));
#211062=CARTESIAN_POINT('Ctrl Pts',(6.07304431899995,11.6,8.97786988899998));
#211063=CARTESIAN_POINT('Ctrl Pts',(6.07089955599994,15.2,8.97616782699998));
#211064=CARTESIAN_POINT('Ctrl Pts',(6.07089955599994,11.6,8.97616782699998));
#211065=CARTESIAN_POINT('Ctrl Pts',(6.06876075399994,15.2,8.97446756299999));
#211066=CARTESIAN_POINT('Ctrl Pts',(6.06876075399994,11.6,8.97446756299999));
#211067=CARTESIAN_POINT('Ctrl Pts',(6.06662791499994,15.2,8.97276910999998));
#211068=CARTESIAN_POINT('Ctrl Pts',(6.06662791499994,11.6,8.97276910999998));
#211069=CARTESIAN_POINT('Ctrl Pts',(6.06450104399994,15.2,8.97107248099999));
#211070=CARTESIAN_POINT('Ctrl Pts',(6.06450104399994,11.6,8.97107248099999));
#211071=CARTESIAN_POINT('Ctrl Pts',(6.06238014199994,15.2,8.96937768799998));
#211072=CARTESIAN_POINT('Ctrl Pts',(6.06238014199994,11.6,8.96937768799998));
#211073=CARTESIAN_POINT('Ctrl Pts',(6.06026521299994,15.2,8.96768474699999));
#211074=CARTESIAN_POINT('Ctrl Pts',(6.06026521299994,11.6,8.96768474699999));
#211075=CARTESIAN_POINT('Ctrl Pts',(6.05815626099994,15.2,8.96599366899999));
#211076=CARTESIAN_POINT('Ctrl Pts',(6.05815626099994,11.6,8.96599366899999));
#211077=CARTESIAN_POINT('Ctrl Pts',(6.05605328699995,15.2,8.96430446999998));
#211078=CARTESIAN_POINT('Ctrl Pts',(6.05605328699995,11.6,8.96430446999998));
#211079=CARTESIAN_POINT('Ctrl Pts',(6.05395629799994,15.2,8.96261716199999));
#211080=CARTESIAN_POINT('Ctrl Pts',(6.05395629799994,11.6,8.96261716199999));
#211081=CARTESIAN_POINT('Ctrl Pts',(6.05186529299995,15.2,8.96093175899999));
#211082=CARTESIAN_POINT('Ctrl Pts',(6.05186529299995,11.6,8.96093175899999));
#211083=CARTESIAN_POINT('Ctrl Pts',(6.04978027699994,15.2,8.95924827399998));
#211084=CARTESIAN_POINT('Ctrl Pts',(6.04978027699994,11.6,8.95924827399998));
#211085=CARTESIAN_POINT('Ctrl Pts',(6.04770125299994,15.2,8.95756672099999));
#211086=CARTESIAN_POINT('Ctrl Pts',(6.04770125299994,11.6,8.95756672099999));
#211087=CARTESIAN_POINT('Ctrl Pts',(6.04562822499994,15.2,8.95588711399999));
#211088=CARTESIAN_POINT('Ctrl Pts',(6.04562822499994,11.6,8.95588711399999));
#211089=CARTESIAN_POINT('Ctrl Pts',(6.04356119499994,15.2,8.95420946599998));
#211090=CARTESIAN_POINT('Ctrl Pts',(6.04356119499994,11.6,8.95420946599998));
#211091=CARTESIAN_POINT('Ctrl Pts',(6.04150016599994,15.2,8.95253379199998));
#211092=CARTESIAN_POINT('Ctrl Pts',(6.04150016599994,11.6,8.95253379199998));
#211093=CARTESIAN_POINT('Ctrl Pts',(6.03944514199994,15.2,8.95086010499998));
#211094=CARTESIAN_POINT('Ctrl Pts',(6.03944514199994,11.6,8.95086010499998));
#211095=CARTESIAN_POINT('Ctrl Pts',(6.03739612599994,15.2,8.94918841899998));
#211096=CARTESIAN_POINT('Ctrl Pts',(6.03739612599994,11.6,8.94918841899998));
#211097=CARTESIAN_POINT('Ctrl Pts',(6.03535311999994,15.2,8.94751874799999));
#211098=CARTESIAN_POINT('Ctrl Pts',(6.03535311999994,11.6,8.94751874799999));
#211099=CARTESIAN_POINT('Ctrl Pts',(6.03331612799994,15.2,8.94585110499998));
#211100=CARTESIAN_POINT('Ctrl Pts',(6.03331612799994,11.6,8.94585110499998));
#211101=CARTESIAN_POINT('Ctrl Pts',(6.03128515299994,15.2,8.94418550499999));
#211102=CARTESIAN_POINT('Ctrl Pts',(6.03128515299994,11.6,8.94418550499999));
#211103=CARTESIAN_POINT('Ctrl Pts',(6.02926019899994,15.2,8.94252196099998));
#211104=CARTESIAN_POINT('Ctrl Pts',(6.02926019899994,11.6,8.94252196099998));
#211105=CARTESIAN_POINT('Ctrl Pts',(6.02724126899994,15.2,8.94086048899998));
#211106=CARTESIAN_POINT('Ctrl Pts',(6.02724126899994,11.6,8.94086048899998));
#211107=CARTESIAN_POINT('Ctrl Pts',(6.02522836399994,15.2,8.93920110099998));
#211108=CARTESIAN_POINT('Ctrl Pts',(6.02522836399994,11.6,8.93920110099998));
#211109=CARTESIAN_POINT('Ctrl Pts',(6.02322148899994,15.2,8.93754381099999));
#211110=CARTESIAN_POINT('Ctrl Pts',(6.02322148899994,11.6,8.93754381099999));
#211111=CARTESIAN_POINT('Ctrl Pts',(6.02122064699994,15.2,8.93588863499998));
#211112=CARTESIAN_POINT('Ctrl Pts',(6.02122064699994,11.6,8.93588863499998));
#211113=CARTESIAN_POINT('Ctrl Pts',(6.01922584099994,15.2,8.93423558599999));
#211114=CARTESIAN_POINT('Ctrl Pts',(6.01922584099994,11.6,8.93423558599999));
#211115=CARTESIAN_POINT('Ctrl Pts',(6.01723707399994,15.2,8.93258467799999));
#211116=CARTESIAN_POINT('Ctrl Pts',(6.01723707399994,11.6,8.93258467799999));
#211117=CARTESIAN_POINT('Ctrl Pts',(6.01525434799994,15.2,8.93093592599998));
#211118=CARTESIAN_POINT('Ctrl Pts',(6.01525434799994,11.6,8.93093592599998));
#211119=CARTESIAN_POINT('Ctrl Pts',(6.01327766799994,15.2,8.92928934399999));
#211120=CARTESIAN_POINT('Ctrl Pts',(6.01327766799994,11.6,8.92928934399999));
#211121=CARTESIAN_POINT('Ctrl Pts',(6.01130703699994,15.2,8.92764494699998));
#211122=CARTESIAN_POINT('Ctrl Pts',(6.01130703699994,11.6,8.92764494699998));
#211123=CARTESIAN_POINT('Ctrl Pts',(6.00934245599994,15.2,8.92600274699999));
#211124=CARTESIAN_POINT('Ctrl Pts',(6.00934245599994,11.6,8.92600274699999));
#211125=CARTESIAN_POINT('Ctrl Pts',(6.00738392999994,15.2,8.92436276099998));
#211126=CARTESIAN_POINT('Ctrl Pts',(6.00738392999994,11.6,8.92436276099998));
#211127=CARTESIAN_POINT('Ctrl Pts',(6.00543146199994,15.2,8.92272500299999));
#211128=CARTESIAN_POINT('Ctrl Pts',(6.00543146199994,11.6,8.92272500299999));
#211129=CARTESIAN_POINT('Ctrl Pts',(6.00348505499994,15.2,8.92108948699999));
#211130=CARTESIAN_POINT('Ctrl Pts',(6.00348505499994,11.6,8.92108948699999));
#211131=CARTESIAN_POINT('Ctrl Pts',(6.00154470999994,15.2,8.91945622799999));
#211132=CARTESIAN_POINT('Ctrl Pts',(6.00154470999994,11.6,8.91945622799999));
#211133=CARTESIAN_POINT('Ctrl Pts',(5.99961043399994,15.2,8.91782523899998));
#211134=CARTESIAN_POINT('Ctrl Pts',(5.99961043399994,11.6,8.91782523899998));
#211135=CARTESIAN_POINT('Ctrl Pts',(5.99768222699995,15.2,8.91619653699999));
#211136=CARTESIAN_POINT('Ctrl Pts',(5.99768222699995,11.6,8.91619653699999));
#211137=CARTESIAN_POINT('Ctrl Pts',(5.99576009299994,15.2,8.91457013599998));
#211138=CARTESIAN_POINT('Ctrl Pts',(5.99576009299994,11.6,8.91457013599998));
#211139=CARTESIAN_POINT('Ctrl Pts',(5.99384403599994,15.2,8.91294604999998));
#211140=CARTESIAN_POINT('Ctrl Pts',(5.99384403599994,11.6,8.91294604999998));
#211141=CARTESIAN_POINT('Ctrl Pts',(5.99193405699994,15.2,8.91132429299999));
#211142=CARTESIAN_POINT('Ctrl Pts',(5.99193405699994,11.6,8.91132429299999));
#211143=CARTESIAN_POINT('Ctrl Pts',(5.99003016199994,15.2,8.90970488199999));
#211144=CARTESIAN_POINT('Ctrl Pts',(5.99003016199994,11.6,8.90970488199999));
#211145=CARTESIAN_POINT('Ctrl Pts',(5.98813235099994,15.2,8.90808782999999));
#211146=CARTESIAN_POINT('Ctrl Pts',(5.98813235099994,11.6,8.90808782999999));
#211147=CARTESIAN_POINT('Ctrl Pts',(5.98624062899995,15.2,8.90647315299999));
#211148=CARTESIAN_POINT('Ctrl Pts',(5.98624062899995,11.6,8.90647315299999));
#211149=CARTESIAN_POINT('Ctrl Pts',(5.98435499899994,15.2,8.90486086599999));
#211150=CARTESIAN_POINT('Ctrl Pts',(5.98435499899994,11.6,8.90486086599999));
#211151=CARTESIAN_POINT('Ctrl Pts',(5.98247546299995,15.2,8.90325098299999));
#211152=CARTESIAN_POINT('Ctrl Pts',(5.98247546299995,11.6,8.90325098299999));
#211153=CARTESIAN_POINT('Ctrl Pts',(5.98060202599994,15.2,8.90164351999999));
#211154=CARTESIAN_POINT('Ctrl Pts',(5.98060202599994,11.6,8.90164351999999));
#211155=CARTESIAN_POINT('Ctrl Pts',(5.97873468799994,15.2,8.90003849199999));
#211156=CARTESIAN_POINT('Ctrl Pts',(5.97873468799994,11.6,8.90003849199999));
#211157=CARTESIAN_POINT('Ctrl Pts',(5.97687345599994,15.2,8.89843591199998));
#211158=CARTESIAN_POINT('Ctrl Pts',(5.97687345599994,11.6,8.89843591199998));
#211159=CARTESIAN_POINT('Ctrl Pts',(5.97501832899995,15.2,8.89683579899998));
#211160=CARTESIAN_POINT('Ctrl Pts',(5.97501832899995,11.6,8.89683579899998));
#211161=CARTESIAN_POINT('Ctrl Pts',(5.97316931399994,15.2,8.89523816499998));
#211162=CARTESIAN_POINT('Ctrl Pts',(5.97316931399994,11.6,8.89523816499998));
#211163=CARTESIAN_POINT('Ctrl Pts',(5.97132640999994,15.2,8.89364302699999));
#211164=CARTESIAN_POINT('Ctrl Pts',(5.97132640999994,11.6,8.89364302699999));
#211165=CARTESIAN_POINT('Ctrl Pts',(5.96948962499994,15.2,8.89205039899998));
#211166=CARTESIAN_POINT('Ctrl Pts',(5.96948962499994,11.6,8.89205039899998));
#211167=CARTESIAN_POINT('Ctrl Pts',(5.96765895599994,15.2,8.89046029799999));
#211168=CARTESIAN_POINT('Ctrl Pts',(5.96765895599994,11.6,8.89046029799999));
#211169=CARTESIAN_POINT('Ctrl Pts',(5.96583441199994,15.2,8.88887273699999));
#211170=CARTESIAN_POINT('Ctrl Pts',(5.96583441199994,11.6,8.88887273699999));
#211171=CARTESIAN_POINT('Ctrl Pts',(5.96401599199995,15.2,8.88728773299999));
#211172=CARTESIAN_POINT('Ctrl Pts',(5.96401599199995,11.6,8.88728773299999));
#211173=CARTESIAN_POINT('Ctrl Pts',(5.96220370099994,15.2,8.88570530199999));
#211174=CARTESIAN_POINT('Ctrl Pts',(5.96220370099994,11.6,8.88570530199999));
#211175=CARTESIAN_POINT('Ctrl Pts',(5.96039754099994,15.2,8.88412545899998));
#211176=CARTESIAN_POINT('Ctrl Pts',(5.96039754099994,11.6,8.88412545899998));
#211177=CARTESIAN_POINT('Ctrl Pts',(5.95859751599994,15.2,8.88254821899999));
#211178=CARTESIAN_POINT('Ctrl Pts',(5.95859751599994,11.6,8.88254821899999));
#211179=CARTESIAN_POINT('Ctrl Pts',(5.95680362799994,15.2,8.88097359799998));
#211180=CARTESIAN_POINT('Ctrl Pts',(5.95680362799994,11.6,8.88097359799998));
#211181=CARTESIAN_POINT('Ctrl Pts',(5.95501588199995,15.2,8.87940161199998));
#211182=CARTESIAN_POINT('Ctrl Pts',(5.95501588199995,11.6,8.87940161199998));
#211183=CARTESIAN_POINT('Ctrl Pts',(5.95323427899994,15.2,8.87783227599999));
#211184=CARTESIAN_POINT('Ctrl Pts',(5.95323427899994,11.6,8.87783227599999));
#211185=CARTESIAN_POINT('Ctrl Pts',(5.95145882199994,15.2,8.87626560599998));
#211186=CARTESIAN_POINT('Ctrl Pts',(5.95145882199994,11.6,8.87626560599998));
#211187=CARTESIAN_POINT('Ctrl Pts',(5.94968951499995,15.2,8.87470161799998));
#211188=CARTESIAN_POINT('Ctrl Pts',(5.94968951499995,11.6,8.87470161799998));
#211189=CARTESIAN_POINT('Ctrl Pts',(5.94792636199994,15.2,8.87314032899998));
#211190=CARTESIAN_POINT('Ctrl Pts',(5.94792636199994,11.6,8.87314032899998));
#211191=CARTESIAN_POINT('Ctrl Pts',(5.94616936399994,15.2,8.87158175299999));
#211192=CARTESIAN_POINT('Ctrl Pts',(5.94616936399994,11.6,8.87158175299999));
#211193=CARTESIAN_POINT('Ctrl Pts',(5.94441852499994,15.2,8.87002590499998));
#211194=CARTESIAN_POINT('Ctrl Pts',(5.94441852499994,11.6,8.87002590499998));
#211195=CARTESIAN_POINT('Ctrl Pts',(5.94267384799994,15.2,8.86847280399999));
#211196=CARTESIAN_POINT('Ctrl Pts',(5.94267384799994,11.6,8.86847280399999));
#211197=CARTESIAN_POINT('Ctrl Pts',(5.94093533599994,15.2,8.86692246499998));
#211198=CARTESIAN_POINT('Ctrl Pts',(5.94093533599994,11.6,8.86692246499998));
#211199=CARTESIAN_POINT('Ctrl Pts',(5.93920299199994,15.2,8.86537490399999));
#211200=CARTESIAN_POINT('Ctrl Pts',(5.93920299199994,11.6,8.86537490399999));
#211201=CARTESIAN_POINT('Ctrl Pts',(5.93747681899995,15.2,8.86383013699999));
#211202=CARTESIAN_POINT('Ctrl Pts',(5.93747681899995,11.6,8.86383013699999));
#211203=CARTESIAN_POINT('Ctrl Pts',(5.93575681999994,15.2,8.86228817899998));
#211204=CARTESIAN_POINT('Ctrl Pts',(5.93575681999994,11.6,8.86228817899998));
#211205=CARTESIAN_POINT('Ctrl Pts',(5.93404299799994,15.2,8.86074904799998));
#211206=CARTESIAN_POINT('Ctrl Pts',(5.93404299799994,11.6,8.86074904799998));
#211207=CARTESIAN_POINT('Ctrl Pts',(5.93233535699994,15.2,8.85921275999999));
#211208=CARTESIAN_POINT('Ctrl Pts',(5.93233535699994,11.6,8.85921275999999));
#211209=CARTESIAN_POINT('Ctrl Pts',(5.93063389799994,15.2,8.85767933099999));
#211210=CARTESIAN_POINT('Ctrl Pts',(5.93063389799994,11.6,8.85767933099999));
#211211=CARTESIAN_POINT('Ctrl Pts',(5.92893862599994,15.2,8.85614877699999));
#211212=CARTESIAN_POINT('Ctrl Pts',(5.92893862599994,11.6,8.85614877699999));
#211213=CARTESIAN_POINT('Ctrl Pts',(5.92724954299994,15.2,8.85462111499999));
#211214=CARTESIAN_POINT('Ctrl Pts',(5.92724954299994,11.6,8.85462111499999));
#211215=CARTESIAN_POINT('Ctrl Pts',(5.92556665199995,15.2,8.85309636099999));
#211216=CARTESIAN_POINT('Ctrl Pts',(5.92556665199995,11.6,8.85309636099999));
#211217=CARTESIAN_POINT('Ctrl Pts',(5.92388995599994,15.2,8.85157453299998));
#211218=CARTESIAN_POINT('Ctrl Pts',(5.92388995599994,11.6,8.85157453299998));
#211219=CARTESIAN_POINT('Ctrl Pts',(5.92221945899994,15.2,8.85005564699998));
#211220=CARTESIAN_POINT('Ctrl Pts',(5.92221945899994,11.6,8.85005564699998));
#211221=CARTESIAN_POINT('Ctrl Pts',(5.92055516299995,15.2,8.84853971799998));
#211222=CARTESIAN_POINT('Ctrl Pts',(5.92055516299995,11.6,8.84853971799998));
#211223=CARTESIAN_POINT('Ctrl Pts',(5.91889706999994,15.2,8.84702676499998));
#211224=CARTESIAN_POINT('Ctrl Pts',(5.91889706999994,11.6,8.84702676499998));
#211225=CARTESIAN_POINT('Ctrl Pts',(5.91724518499994,15.2,8.84551680299998));
#211226=CARTESIAN_POINT('Ctrl Pts',(5.91724518499994,11.6,8.84551680299998));
#211227=CARTESIAN_POINT('Ctrl Pts',(5.91559951099994,15.2,8.84400984899998));
#211228=CARTESIAN_POINT('Ctrl Pts',(5.91559951099994,11.6,8.84400984899998));
#211229=CARTESIAN_POINT('Ctrl Pts',(5.91396004999994,15.2,8.84250592099999));
#211230=CARTESIAN_POINT('Ctrl Pts',(5.91396004999994,11.6,8.84250592099999));
#211231=CARTESIAN_POINT('Ctrl Pts',(5.91232680399995,15.2,8.84100503599999));
#211232=CARTESIAN_POINT('Ctrl Pts',(5.91232680399995,11.6,8.84100503599999));
#211233=CARTESIAN_POINT('Ctrl Pts',(5.91069977899994,15.2,8.83950720899998));
#211234=CARTESIAN_POINT('Ctrl Pts',(5.91069977899994,11.6,8.83950720899998));
#211235=CARTESIAN_POINT('Ctrl Pts',(5.90907897499994,15.2,8.83801245899999));
#211236=CARTESIAN_POINT('Ctrl Pts',(5.90907897499994,11.6,8.83801245899999));
#211237=CARTESIAN_POINT('Ctrl Pts',(5.90746439699994,15.2,8.83652080299999));
#211238=CARTESIAN_POINT('Ctrl Pts',(5.90746439699994,11.6,8.83652080299999));
#211239=CARTESIAN_POINT('Ctrl Pts',(5.90585604599994,15.2,8.83503225699998));
#211240=CARTESIAN_POINT('Ctrl Pts',(5.90585604599994,11.6,8.83503225699998));
#211241=CARTESIAN_POINT('Ctrl Pts',(5.90425392799995,15.2,8.83354683899999));
#211242=CARTESIAN_POINT('Ctrl Pts',(5.90425392799995,11.6,8.83354683899999));
#211243=CARTESIAN_POINT('Ctrl Pts',(5.90265804299994,15.2,8.83206456499998));
#211244=CARTESIAN_POINT('Ctrl Pts',(5.90265804299994,11.6,8.83206456499998));
#211245=CARTESIAN_POINT('Ctrl Pts',(5.90106839599994,15.2,8.83058545499999));
#211246=CARTESIAN_POINT('Ctrl Pts',(5.90106839599994,11.6,8.83058545499999));
#211247=CARTESIAN_POINT('Ctrl Pts',(5.89948498799994,15.2,8.82910952399998));
#211248=CARTESIAN_POINT('Ctrl Pts',(5.89948498799994,11.6,8.82910952399998));
#211249=CARTESIAN_POINT('Ctrl Pts',(5.89790782399994,15.2,8.82763678999999));
#211250=CARTESIAN_POINT('Ctrl Pts',(5.89790782399994,11.6,8.82763678999999));
#211251=CARTESIAN_POINT('Ctrl Pts',(5.89633690599994,15.2,8.82616727099998));
#211252=CARTESIAN_POINT('Ctrl Pts',(5.89633690599994,11.6,8.82616727099998));
#211253=CARTESIAN_POINT('Ctrl Pts',(5.89477223699994,15.2,8.82470098399999));
#211254=CARTESIAN_POINT('Ctrl Pts',(5.89477223699994,11.6,8.82470098399999));
#211255=CARTESIAN_POINT('Ctrl Pts',(5.89321381999994,15.2,8.82323794699998));
#211256=CARTESIAN_POINT('Ctrl Pts',(5.89321381999994,11.6,8.82323794699998));
#211257=CARTESIAN_POINT('Ctrl Pts',(5.89166165899995,15.2,8.82177817599998));
#211258=CARTESIAN_POINT('Ctrl Pts',(5.89166165899995,11.6,8.82177817599998));
#211259=CARTESIAN_POINT('Ctrl Pts',(5.89011575399994,15.2,8.82032169099999));
#211260=CARTESIAN_POINT('Ctrl Pts',(5.89011575399994,11.6,8.82032169099999));
#211261=CARTESIAN_POINT('Ctrl Pts',(5.88857611199994,15.2,8.81886850999998));
#211262=CARTESIAN_POINT('Ctrl Pts',(5.88857611199994,11.6,8.81886850999998));
#211263=CARTESIAN_POINT('Ctrl Pts',(5.88704273199995,15.2,8.81741864899999));
#211264=CARTESIAN_POINT('Ctrl Pts',(5.88704273199995,11.6,8.81741864899999));
#211265=CARTESIAN_POINT('Ctrl Pts',(5.88551561999994,15.2,8.81597212599999));
#211266=CARTESIAN_POINT('Ctrl Pts',(5.88551561999994,11.6,8.81597212599999));
#211267=CARTESIAN_POINT('Ctrl Pts',(5.88399477899994,15.2,8.81452895999999));
#211268=CARTESIAN_POINT('Ctrl Pts',(5.88399477899994,11.6,8.81452895999999));
#211269=CARTESIAN_POINT('Ctrl Pts',(5.88248020899995,15.2,8.81308916799998));
#211270=CARTESIAN_POINT('Ctrl Pts',(5.88248020899995,11.6,8.81308916799998));
#211271=CARTESIAN_POINT('Ctrl Pts',(5.88097191599994,15.2,8.81165276999998));
#211272=CARTESIAN_POINT('Ctrl Pts',(5.88097191599994,11.6,8.81165276999998));
#211273=CARTESIAN_POINT('Ctrl Pts',(5.87946990099995,15.2,8.81021978199998));
#211274=CARTESIAN_POINT('Ctrl Pts',(5.87946990099995,11.6,8.81021978199998));
#211275=CARTESIAN_POINT('Ctrl Pts',(5.87797416699994,15.2,8.80879022299998));
#211276=CARTESIAN_POINT('Ctrl Pts',(5.87797416699994,11.6,8.80879022299998));
#211277=CARTESIAN_POINT('Ctrl Pts',(5.87648471999994,15.2,8.80736411099999));
#211278=CARTESIAN_POINT('Ctrl Pts',(5.87648471999994,11.6,8.80736411099999));
#211279=CARTESIAN_POINT('Ctrl Pts',(5.87500155899994,15.2,8.80594146499998));
#211280=CARTESIAN_POINT('Ctrl Pts',(5.87500155899994,11.6,8.80594146499998));
#211281=CARTESIAN_POINT('Ctrl Pts',(5.87352468899994,15.2,8.80452230299999));
#211282=CARTESIAN_POINT('Ctrl Pts',(5.87352468899994,11.6,8.80452230299999));
#211283=CARTESIAN_POINT('Ctrl Pts',(5.87205411099994,15.2,8.80310664299999));
#211284=CARTESIAN_POINT('Ctrl Pts',(5.87205411099994,11.6,8.80310664299999));
#211285=CARTESIAN_POINT('Ctrl Pts',(5.87058983199994,15.2,8.80169450299999));
#211286=CARTESIAN_POINT('Ctrl Pts',(5.87058983199994,11.6,8.80169450299999));
#211287=CARTESIAN_POINT('Ctrl Pts',(5.86913184999994,15.2,8.80028590299998));
#211288=CARTESIAN_POINT('Ctrl Pts',(5.86913184999994,11.6,8.80028590299998));
#211289=CARTESIAN_POINT('Ctrl Pts',(5.86768017199994,15.2,8.79888086199998));
#211290=CARTESIAN_POINT('Ctrl Pts',(5.86768017199994,11.6,8.79888086199998));
#211291=CARTESIAN_POINT('Ctrl Pts',(5.86623479799995,15.2,8.79747939699998));
#211292=CARTESIAN_POINT('Ctrl Pts',(5.86623479799995,11.6,8.79747939699998));
#211293=CARTESIAN_POINT('Ctrl Pts',(5.86479573299994,15.2,8.79608152699999));
#211294=CARTESIAN_POINT('Ctrl Pts',(5.86479573299994,11.6,8.79608152699999));
#211295=CARTESIAN_POINT('Ctrl Pts',(5.86336297799994,15.2,8.79468727199999));
#211296=CARTESIAN_POINT('Ctrl Pts',(5.86336297799994,11.6,8.79468727199999));
#211297=CARTESIAN_POINT('Ctrl Pts',(5.86193653799994,15.2,8.79329664999998));
#211298=CARTESIAN_POINT('Ctrl Pts',(5.86193653799994,11.6,8.79329664999998));
#211299=CARTESIAN_POINT('Ctrl Pts',(5.86051641599994,15.2,8.79190967999998));
#211300=CARTESIAN_POINT('Ctrl Pts',(5.86051641599994,11.6,8.79190967999998));
#211301=CARTESIAN_POINT('Ctrl Pts',(5.85910261199994,15.2,8.79052638199998));
#211302=CARTESIAN_POINT('Ctrl Pts',(5.85910261199994,11.6,8.79052638199998));
#211303=CARTESIAN_POINT('Ctrl Pts',(5.85769513199994,15.2,8.78914677199998));
#211304=CARTESIAN_POINT('Ctrl Pts',(5.85769513199994,11.6,8.78914677199998));
#211305=CARTESIAN_POINT('Ctrl Pts',(5.85629397699994,15.2,8.78777087299999));
#211306=CARTESIAN_POINT('Ctrl Pts',(5.85629397699994,11.6,8.78777087299999));
#211307=CARTESIAN_POINT('Ctrl Pts',(5.85489915099994,15.2,8.78639870299999));
#211308=CARTESIAN_POINT('Ctrl Pts',(5.85489915099994,11.6,8.78639870299999));
#211309=CARTESIAN_POINT('Ctrl Pts',(5.85351065599995,15.2,8.78503028099999));
#211310=CARTESIAN_POINT('Ctrl Pts',(5.85351065599995,11.6,8.78503028099999));
#211311=CARTESIAN_POINT('Ctrl Pts',(5.85212849599994,15.2,8.78366562499998));
#211312=CARTESIAN_POINT('Ctrl Pts',(5.85212849599994,11.6,8.78366562499998));
#211313=CARTESIAN_POINT('Ctrl Pts',(5.85075267399994,15.2,8.78230475599998));
#211314=CARTESIAN_POINT('Ctrl Pts',(5.85075267399994,11.6,8.78230475599998));
#211315=CARTESIAN_POINT('Ctrl Pts',(5.84938319199994,15.2,8.78094769299998));
#211316=CARTESIAN_POINT('Ctrl Pts',(5.84938319199994,11.6,8.78094769299998));
#211317=CARTESIAN_POINT('Ctrl Pts',(5.84802005299994,15.2,8.77959445599998));
#211318=CARTESIAN_POINT('Ctrl Pts',(5.84802005299994,11.6,8.77959445599998));
#211319=CARTESIAN_POINT('Ctrl Pts',(5.84666325999994,15.2,8.77824506499999));
#211320=CARTESIAN_POINT('Ctrl Pts',(5.84666325999994,11.6,8.77824506499999));
#211321=CARTESIAN_POINT('Ctrl Pts',(5.84531281599994,15.2,8.77689953899999));
#211322=CARTESIAN_POINT('Ctrl Pts',(5.84531281599994,11.6,8.77689953899999));
#211323=CARTESIAN_POINT('Ctrl Pts',(5.84396872499994,15.2,8.77555789599998));
#211324=CARTESIAN_POINT('Ctrl Pts',(5.84396872499994,11.6,8.77555789599998));
#211325=CARTESIAN_POINT('Ctrl Pts',(5.84263098699994,15.2,8.77422015899998));
#211326=CARTESIAN_POINT('Ctrl Pts',(5.84263098699994,11.6,8.77422015899998));
#211327=CARTESIAN_POINT('Ctrl Pts',(5.84129960799994,15.2,8.77288634599999));
#211328=CARTESIAN_POINT('Ctrl Pts',(5.84129960799994,11.6,8.77288634599999));
#211329=CARTESIAN_POINT('Ctrl Pts',(5.83997458899995,15.2,8.77155647799999));
#211330=CARTESIAN_POINT('Ctrl Pts',(5.83997458899995,11.6,8.77155647799999));
#211331=CARTESIAN_POINT('Ctrl Pts',(5.83865593499994,15.2,8.77023057399999));
#211332=CARTESIAN_POINT('Ctrl Pts',(5.83865593499994,11.6,8.77023057399999));
#211333=CARTESIAN_POINT('Ctrl Pts',(5.83734364599994,15.2,8.76890865499998));
#211334=CARTESIAN_POINT('Ctrl Pts',(5.83734364599994,11.6,8.76890865499998));
#211335=CARTESIAN_POINT('Ctrl Pts',(5.83603772599995,15.2,8.76759074099999));
#211336=CARTESIAN_POINT('Ctrl Pts',(5.83603772599995,11.6,8.76759074099999));
#211337=CARTESIAN_POINT('Ctrl Pts',(5.83473817899995,15.2,8.76627685199999));
#211338=CARTESIAN_POINT('Ctrl Pts',(5.83473817899995,11.6,8.76627685199999));
#211339=CARTESIAN_POINT('Ctrl Pts',(5.83344500599994,15.2,8.76496700899999));
#211340=CARTESIAN_POINT('Ctrl Pts',(5.83344500599994,11.6,8.76496700899999));
#211341=CARTESIAN_POINT('Ctrl Pts',(5.83215821299994,15.2,8.76366122999999));
#211342=CARTESIAN_POINT('Ctrl Pts',(5.83215821299994,11.6,8.76366122999999));
#211343=CARTESIAN_POINT('Ctrl Pts',(5.83087779899994,15.2,8.76235953999998));
#211344=CARTESIAN_POINT('Ctrl Pts',(5.83087779899994,11.6,8.76235953999998));
#211345=CARTESIAN_POINT('Ctrl Pts',(5.82960376999995,15.2,8.76106195499998));
#211346=CARTESIAN_POINT('Ctrl Pts',(5.82960376999995,11.6,8.76106195499998));
#211347=CARTESIAN_POINT('Ctrl Pts',(5.82833612699994,15.2,8.75976849799999));
#211348=CARTESIAN_POINT('Ctrl Pts',(5.82833612699994,11.6,8.75976849799999));
#211349=CARTESIAN_POINT('Ctrl Pts',(5.82707487299994,15.2,8.75847918999998));
#211350=CARTESIAN_POINT('Ctrl Pts',(5.82707487299994,11.6,8.75847918999998));
#211351=CARTESIAN_POINT('Ctrl Pts',(5.82582001199994,15.2,8.75719405099998));
#211352=CARTESIAN_POINT('Ctrl Pts',(5.82582001199994,11.6,8.75719405099998));
#211353=CARTESIAN_POINT('Ctrl Pts',(5.82457154599994,15.2,8.75591310099999));
#211354=CARTESIAN_POINT('Ctrl Pts',(5.82457154599994,11.6,8.75591310099999));
#211355=CARTESIAN_POINT('Ctrl Pts',(5.82332947799994,15.2,8.75463636299998));
#211356=CARTESIAN_POINT('Ctrl Pts',(5.82332947799994,11.6,8.75463636299998));
#211357=CARTESIAN_POINT('Ctrl Pts',(5.82209381199994,15.2,8.75336385699999));
#211358=CARTESIAN_POINT('Ctrl Pts',(5.82209381199994,11.6,8.75336385699999));
#211359=CARTESIAN_POINT('Ctrl Pts',(5.82086454899994,15.2,8.75209560299999));
#211360=CARTESIAN_POINT('Ctrl Pts',(5.82086454899994,11.6,8.75209560299999));
#211361=CARTESIAN_POINT('Ctrl Pts',(5.81964169299994,15.2,8.75083162499998));
#211362=CARTESIAN_POINT('Ctrl Pts',(5.81964169299994,11.6,8.75083162499998));
#211363=CARTESIAN_POINT('Ctrl Pts',(5.81842524599995,15.2,8.74957194099999));
#211364=CARTESIAN_POINT('Ctrl Pts',(5.81842524599995,11.6,8.74957194099999));
#211365=CARTESIAN_POINT('Ctrl Pts',(5.81721521199994,15.2,8.74831657499998));
#211366=CARTESIAN_POINT('Ctrl Pts',(5.81721521199994,11.6,8.74831657499998));
#211367=CARTESIAN_POINT('Ctrl Pts',(5.81601159299994,15.2,8.74706554699999));
#211368=CARTESIAN_POINT('Ctrl Pts',(5.81601159299994,11.6,8.74706554699999));
#211369=CARTESIAN_POINT('Ctrl Pts',(5.81481439199995,15.2,8.74581887799999));
#211370=CARTESIAN_POINT('Ctrl Pts',(5.81481439199995,11.6,8.74581887799999));
#211371=CARTESIAN_POINT('Ctrl Pts',(5.81362361299995,15.2,8.74457659099999));
#211372=CARTESIAN_POINT('Ctrl Pts',(5.81362361299995,11.6,8.74457659099999));
#211373=CARTESIAN_POINT('Ctrl Pts',(5.81243925699994,15.2,8.74333870699999));
#211374=CARTESIAN_POINT('Ctrl Pts',(5.81243925699994,11.6,8.74333870699999));
#211375=CARTESIAN_POINT('Ctrl Pts',(5.81126132699994,15.2,8.74210524899999));
#211376=CARTESIAN_POINT('Ctrl Pts',(5.81126132699994,11.6,8.74210524899999));
#211377=CARTESIAN_POINT('Ctrl Pts',(5.81008982699994,15.2,8.74087623599999));
#211378=CARTESIAN_POINT('Ctrl Pts',(5.81008982699994,11.6,8.74087623599999));
#211379=CARTESIAN_POINT('Ctrl Pts',(5.80892475999994,15.2,8.73965169199998));
#211380=CARTESIAN_POINT('Ctrl Pts',(5.80892475999994,11.6,8.73965169199998));
#211381=CARTESIAN_POINT('Ctrl Pts',(5.80776612699994,15.2,8.73843163899998));
#211382=CARTESIAN_POINT('Ctrl Pts',(5.80776612699994,11.6,8.73843163899998));
#211383=CARTESIAN_POINT('Ctrl Pts',(5.80661393399994,15.2,8.73721609899999));
#211384=CARTESIAN_POINT('Ctrl Pts',(5.80661393399994,11.6,8.73721609899999));
#211385=CARTESIAN_POINT('Ctrl Pts',(5.80546818099994,15.2,8.73600509399999));
#211386=CARTESIAN_POINT('Ctrl Pts',(5.80546818099994,11.6,8.73600509399999));
#211387=CARTESIAN_POINT('Ctrl Pts',(5.80432887199994,15.2,8.73479864499998));
#211388=CARTESIAN_POINT('Ctrl Pts',(5.80432887199994,11.6,8.73479864499998));
#211389=CARTESIAN_POINT('Ctrl Pts',(5.80319600899994,15.2,8.73359677599998));
#211390=CARTESIAN_POINT('Ctrl Pts',(5.80319600899994,11.6,8.73359677599998));
#211391=CARTESIAN_POINT('Ctrl Pts',(5.80206959599994,15.2,8.73239950899999));
#211392=CARTESIAN_POINT('Ctrl Pts',(5.80206959599994,11.6,8.73239950899999));
#211393=CARTESIAN_POINT('Ctrl Pts',(5.80094963499994,15.2,8.73120686599999));
#211394=CARTESIAN_POINT('Ctrl Pts',(5.80094963499994,11.6,8.73120686599999));
#211395=CARTESIAN_POINT('Ctrl Pts',(5.79983612799994,15.2,8.73001887099999));
#211396=CARTESIAN_POINT('Ctrl Pts',(5.79983612799994,11.6,8.73001887099999));
#211397=CARTESIAN_POINT('Ctrl Pts',(5.79872907999994,15.2,8.72883554599999));
#211398=CARTESIAN_POINT('Ctrl Pts',(5.79872907999994,11.6,8.72883554599999));
#211399=CARTESIAN_POINT('Ctrl Pts',(5.79762849299994,15.2,8.72765691299998));
#211400=CARTESIAN_POINT('Ctrl Pts',(5.79762849299994,11.6,8.72765691299998));
#211401=CARTESIAN_POINT('Ctrl Pts',(5.79653436899994,15.2,8.72648299499998));
#211402=CARTESIAN_POINT('Ctrl Pts',(5.79653436899994,11.6,8.72648299499998));
#211403=CARTESIAN_POINT('Ctrl Pts',(5.79544671099995,15.2,8.72531381599998));
#211404=CARTESIAN_POINT('Ctrl Pts',(5.79544671099995,11.6,8.72531381599998));
#211405=CARTESIAN_POINT('Ctrl Pts',(5.79436552299994,15.2,8.72414939899999));
#211406=CARTESIAN_POINT('Ctrl Pts',(5.79436552299994,11.6,8.72414939899999));
#211407=CARTESIAN_POINT('Ctrl Pts',(5.79329080699994,15.2,8.72298976599998));
#211408=CARTESIAN_POINT('Ctrl Pts',(5.79329080699994,11.6,8.72298976599998));
#211409=CARTESIAN_POINT('Ctrl Pts',(5.79222256599994,15.2,8.72183494199999));
#211410=CARTESIAN_POINT('Ctrl Pts',(5.79222256599994,11.6,8.72183494199999));
#211411=CARTESIAN_POINT('Ctrl Pts',(5.79116080199994,15.2,8.72068494799999));
#211412=CARTESIAN_POINT('Ctrl Pts',(5.79116080199994,11.6,8.72068494799999));
#211413=CARTESIAN_POINT('Ctrl Pts',(5.79010551899994,15.2,8.71953980899999));
#211414=CARTESIAN_POINT('Ctrl Pts',(5.79010551899994,11.6,8.71953980899999));
#211415=CARTESIAN_POINT('Ctrl Pts',(5.78905671899995,15.2,8.71839954799999));
#211416=CARTESIAN_POINT('Ctrl Pts',(5.78905671899995,11.6,8.71839954799999));
#211417=CARTESIAN_POINT('Ctrl Pts',(5.78801440499994,15.2,8.71726418999998));
#211418=CARTESIAN_POINT('Ctrl Pts',(5.78801440499994,11.6,8.71726418999998));
#211419=CARTESIAN_POINT('Ctrl Pts',(5.78697857999994,15.2,8.71613375699998));
#211420=CARTESIAN_POINT('Ctrl Pts',(5.78697857999994,11.6,8.71613375699998));
#211421=CARTESIAN_POINT('Ctrl Pts',(5.78594924699994,15.2,8.71500827299998));
#211422=CARTESIAN_POINT('Ctrl Pts',(5.78594924699994,11.6,8.71500827299998));
#211423=CARTESIAN_POINT('Ctrl Pts',(5.78492640799994,15.2,8.71388776199998));
#211424=CARTESIAN_POINT('Ctrl Pts',(5.78492640799994,11.6,8.71388776199998));
#211425=CARTESIAN_POINT('Ctrl Pts',(5.78391006599994,15.2,8.71277224899998));
#211426=CARTESIAN_POINT('Ctrl Pts',(5.78391006599994,11.6,8.71277224899998));
#211427=CARTESIAN_POINT('Ctrl Pts',(5.78290022499995,15.2,8.71166175799999));
#211428=CARTESIAN_POINT('Ctrl Pts',(5.78290022499995,11.6,8.71166175799999));
#211429=CARTESIAN_POINT('Ctrl Pts',(5.78189688599994,15.2,8.71055631299999));
#211430=CARTESIAN_POINT('Ctrl Pts',(5.78189688599994,11.6,8.71055631299999));
#211431=CARTESIAN_POINT('Ctrl Pts',(5.78090005399994,15.2,8.70945593699999));
#211432=CARTESIAN_POINT('Ctrl Pts',(5.78090005399994,11.6,8.70945593699999));
#211433=CARTESIAN_POINT('Ctrl Pts',(5.77990972899994,15.2,8.70836065599999));
#211434=CARTESIAN_POINT('Ctrl Pts',(5.77990972899994,11.6,8.70836065599999));
#211435=CARTESIAN_POINT('Ctrl Pts',(5.77892591699994,15.2,8.70727049299998));
#211436=CARTESIAN_POINT('Ctrl Pts',(5.77892591699994,11.6,8.70727049299998));
#211437=CARTESIAN_POINT('Ctrl Pts',(5.77794861699994,15.2,8.70618547499999));
#211438=CARTESIAN_POINT('Ctrl Pts',(5.77794861699994,11.6,8.70618547499999));
#211439=CARTESIAN_POINT('Ctrl Pts',(5.77697783599994,15.2,8.70510562499998));
#211440=CARTESIAN_POINT('Ctrl Pts',(5.77697783599994,11.6,8.70510562499998));
#211441=CARTESIAN_POINT('Ctrl Pts',(5.77601357299995,15.2,8.70403096699999));
#211442=CARTESIAN_POINT('Ctrl Pts',(5.77601357299995,11.6,8.70403096699999));
#211443=CARTESIAN_POINT('Ctrl Pts',(5.77505583299994,15.2,8.70296152799998));
#211444=CARTESIAN_POINT('Ctrl Pts',(5.77505583299994,11.6,8.70296152799998));
#211445=CARTESIAN_POINT('Ctrl Pts',(5.77410461799994,15.2,8.70189733199998));
#211446=CARTESIAN_POINT('Ctrl Pts',(5.77410461799994,11.6,8.70189733199998));
#211447=CARTESIAN_POINT('Ctrl Pts',(5.77315993099995,15.2,8.70083840499999));
#211448=CARTESIAN_POINT('Ctrl Pts',(5.77315993099995,11.6,8.70083840499999));
#211449=CARTESIAN_POINT('Ctrl Pts',(5.77222177499994,15.2,8.69978477099998));
#211450=CARTESIAN_POINT('Ctrl Pts',(5.77222177499994,11.6,8.69978477099998));
#211451=CARTESIAN_POINT('Ctrl Pts',(5.77129015299994,15.2,8.69873645499998));
#211452=CARTESIAN_POINT('Ctrl Pts',(5.77129015299994,11.6,8.69873645499998));
#211453=CARTESIAN_POINT('Ctrl Pts',(5.77036506699995,15.2,8.69769348399998));
#211454=CARTESIAN_POINT('Ctrl Pts',(5.77036506699995,11.6,8.69769348399998));
#211455=CARTESIAN_POINT('Ctrl Pts',(5.76944651999994,15.2,8.69665588399998));
#211456=CARTESIAN_POINT('Ctrl Pts',(5.76944651999994,11.6,8.69665588399998));
#211457=CARTESIAN_POINT('Ctrl Pts',(5.76853451499994,15.2,8.69562367799999));
#211458=CARTESIAN_POINT('Ctrl Pts',(5.76853451499994,11.6,8.69562367799999));
#211459=CARTESIAN_POINT('Ctrl Pts',(5.76762905499995,15.2,8.69459689299998));
#211460=CARTESIAN_POINT('Ctrl Pts',(5.76762905499995,11.6,8.69459689299998));
#211461=CARTESIAN_POINT('Ctrl Pts',(5.76673014099994,15.2,8.69357555699998));
#211462=CARTESIAN_POINT('Ctrl Pts',(5.76673014099994,11.6,8.69357555699998));
#211463=CARTESIAN_POINT('Ctrl Pts',(5.76583777899994,15.2,8.69255969399998));
#211464=CARTESIAN_POINT('Ctrl Pts',(5.76583777899994,11.6,8.69255969399998));
#211465=CARTESIAN_POINT('Ctrl Pts',(5.76495196899995,15.2,8.69154932999999));
#211466=CARTESIAN_POINT('Ctrl Pts',(5.76495196899995,11.6,8.69154932999999));
#211467=CARTESIAN_POINT('Ctrl Pts',(5.76407271499994,15.2,8.69054449199999));
#211468=CARTESIAN_POINT('Ctrl Pts',(5.76407271499994,11.6,8.69054449199999));
#211469=CARTESIAN_POINT('Ctrl Pts',(5.76320001899995,15.2,8.68954520599999));
#211470=CARTESIAN_POINT('Ctrl Pts',(5.76320001899995,11.6,8.68954520599999));
#211471=CARTESIAN_POINT('Ctrl Pts',(5.76233388499994,15.2,8.68855149899998));
#211472=CARTESIAN_POINT('Ctrl Pts',(5.76233388499994,11.6,8.68855149899998));
#211473=CARTESIAN_POINT('Ctrl Pts',(5.76147431499995,15.2,8.68756339699999));
#211474=CARTESIAN_POINT('Ctrl Pts',(5.76147431499995,11.6,8.68756339699999));
#211475=CARTESIAN_POINT('Ctrl Pts',(5.76062131199994,15.2,8.68658092599999));
#211476=CARTESIAN_POINT('Ctrl Pts',(5.76062131199994,11.6,8.68658092599999));
#211477=CARTESIAN_POINT('Ctrl Pts',(5.75977487799994,15.2,8.68560411499999));
#211478=CARTESIAN_POINT('Ctrl Pts',(5.75977487799994,11.6,8.68560411499999));
#211479=CARTESIAN_POINT('Ctrl Pts',(5.75893501599994,15.2,8.68463298899999));
#211480=CARTESIAN_POINT('Ctrl Pts',(5.75893501599994,11.6,8.68463298899999));
#211481=CARTESIAN_POINT('Ctrl Pts',(5.75810172999994,15.2,8.68366757599999));
#211482=CARTESIAN_POINT('Ctrl Pts',(5.75810172999994,11.6,8.68366757599999));
#211483=CARTESIAN_POINT('Ctrl Pts',(5.75727501999994,15.2,8.68270790299999));
#211484=CARTESIAN_POINT('Ctrl Pts',(5.75727501999994,11.6,8.68270790299999));
#211485=CARTESIAN_POINT('Ctrl Pts',(5.75645489199994,15.2,8.68175399699999));
#211486=CARTESIAN_POINT('Ctrl Pts',(5.75645489199994,11.6,8.68175399699999));
#211487=CARTESIAN_POINT('Ctrl Pts',(5.75564134699994,15.2,8.68080588599998));
#211488=CARTESIAN_POINT('Ctrl Pts',(5.75564134699994,11.6,8.68080588599998));
#211489=CARTESIAN_POINT('Ctrl Pts',(5.75483438799995,15.2,8.67986359699999));
#211490=CARTESIAN_POINT('Ctrl Pts',(5.75483438799995,11.6,8.67986359699999));
#211491=CARTESIAN_POINT('Ctrl Pts',(5.75403401799995,15.2,8.67892715799999));
#211492=CARTESIAN_POINT('Ctrl Pts',(5.75403401799995,11.6,8.67892715799999));
#211493=CARTESIAN_POINT('Ctrl Pts',(5.75324023999994,15.2,8.67799659699998));
#211494=CARTESIAN_POINT('Ctrl Pts',(5.75324023999994,11.6,8.67799659699998));
#211495=CARTESIAN_POINT('Ctrl Pts',(5.75245305499994,15.2,8.67707194299999));
#211496=CARTESIAN_POINT('Ctrl Pts',(5.75245305499994,11.6,8.67707194299999));
#211497=CARTESIAN_POINT('Ctrl Pts',(5.75167246799994,15.2,8.67615322099999));
#211498=CARTESIAN_POINT('Ctrl Pts',(5.75167246799994,11.6,8.67615322099999));
#211499=CARTESIAN_POINT('Ctrl Pts',(5.75089847999994,15.2,8.67524046099999));
#211500=CARTESIAN_POINT('Ctrl Pts',(5.75089847999994,11.6,8.67524046099999));
#211501=CARTESIAN_POINT('Ctrl Pts',(5.75013109599994,15.2,8.67433369199999));
#211502=CARTESIAN_POINT('Ctrl Pts',(5.75013109599994,11.6,8.67433369199999));
#211503=CARTESIAN_POINT('Ctrl Pts',(5.74937031599994,15.2,8.67343294199999));
#211504=CARTESIAN_POINT('Ctrl Pts',(5.74937031599994,11.6,8.67343294199999));
#211505=CARTESIAN_POINT('Ctrl Pts',(5.74861614399994,15.2,8.67253823899999));
#211506=CARTESIAN_POINT('Ctrl Pts',(5.74861614399994,11.6,8.67253823899999));
#211507=CARTESIAN_POINT('Ctrl Pts',(5.74786858399994,15.2,8.67164961299999));
#211508=CARTESIAN_POINT('Ctrl Pts',(5.74786858399994,11.6,8.67164961299999));
#211509=CARTESIAN_POINT('Ctrl Pts',(5.74712763499994,15.2,8.67076709099998));
#211510=CARTESIAN_POINT('Ctrl Pts',(5.74712763499994,11.6,8.67076709099998));
#211511=CARTESIAN_POINT('Ctrl Pts',(5.74639330499994,15.2,8.66989070399999));
#211512=CARTESIAN_POINT('Ctrl Pts',(5.74639330499994,11.6,8.66989070399999));
#211513=CARTESIAN_POINT('Ctrl Pts',(5.74566559199994,15.2,8.66902047899998));
#211514=CARTESIAN_POINT('Ctrl Pts',(5.74566559199994,11.6,8.66902047899998));
#211515=CARTESIAN_POINT('Ctrl Pts',(5.74494450099994,15.2,8.66815644699999));
#211516=CARTESIAN_POINT('Ctrl Pts',(5.74494450099994,11.6,8.66815644699999));
#211517=CARTESIAN_POINT('Ctrl Pts',(5.74423003499994,15.2,8.66729863599998));
#211518=CARTESIAN_POINT('Ctrl Pts',(5.74423003499994,11.6,8.66729863599998));
#211519=CARTESIAN_POINT('Ctrl Pts',(5.74352219599994,15.2,8.66644707799999));
#211520=CARTESIAN_POINT('Ctrl Pts',(5.74352219599994,11.6,8.66644707799999));
#211521=CARTESIAN_POINT('Ctrl Pts',(5.74282098799995,15.2,8.66560179999999));
#211522=CARTESIAN_POINT('Ctrl Pts',(5.74282098799995,11.6,8.66560179999999));
#211523=CARTESIAN_POINT('Ctrl Pts',(5.74212640999994,15.2,8.66476283199999));
#211524=CARTESIAN_POINT('Ctrl Pts',(5.74212640999994,11.6,8.66476283199999));
#211525=CARTESIAN_POINT('Ctrl Pts',(5.74143846899994,15.2,8.66393020599999));
#211526=CARTESIAN_POINT('Ctrl Pts',(5.74143846899994,11.6,8.66393020599999));
#211527=CARTESIAN_POINT('Ctrl Pts',(5.74075716599994,15.2,8.66310394999999));
#211528=CARTESIAN_POINT('Ctrl Pts',(5.74075716599994,11.6,8.66310394999999));
#211529=CARTESIAN_POINT('Ctrl Pts',(5.74008250299994,15.2,8.66228409699998));
#211530=CARTESIAN_POINT('Ctrl Pts',(5.74008250299994,11.6,8.66228409699998));
#211531=CARTESIAN_POINT('Ctrl Pts',(5.73941448499995,15.2,8.66147067399999));
#211532=CARTESIAN_POINT('Ctrl Pts',(5.73941448499995,11.6,8.66147067399999));
#211533=CARTESIAN_POINT('Ctrl Pts',(5.73875311199994,15.2,8.66066371299999));
#211534=CARTESIAN_POINT('Ctrl Pts',(5.73875311199994,11.6,8.66066371299999));
#211535=CARTESIAN_POINT('Ctrl Pts',(5.73809838799994,15.2,8.65986324599999));
#211536=CARTESIAN_POINT('Ctrl Pts',(5.73809838799994,11.6,8.65986324599999));
#211537=CARTESIAN_POINT('Ctrl Pts',(5.73745031599994,15.2,8.65906930299998));
#211538=CARTESIAN_POINT('Ctrl Pts',(5.73745031599994,11.6,8.65906930299998));
#211539=CARTESIAN_POINT('Ctrl Pts',(5.73680889799995,15.2,8.65828191399999));
#211540=CARTESIAN_POINT('Ctrl Pts',(5.73680889799995,11.6,8.65828191399999));
#211541=CARTESIAN_POINT('Ctrl Pts',(5.73617413699995,15.2,8.65750111099998));
#211542=CARTESIAN_POINT('Ctrl Pts',(5.73617413699995,11.6,8.65750111099998));
#211543=CARTESIAN_POINT('Ctrl Pts',(5.73554603599994,15.2,8.65672692399999));
#211544=CARTESIAN_POINT('Ctrl Pts',(5.73554603599994,11.6,8.65672692399999));
#211545=CARTESIAN_POINT('Ctrl Pts',(5.73492459799994,15.2,8.65595938799999));
#211546=CARTESIAN_POINT('Ctrl Pts',(5.73492459799994,11.6,8.65595938799999));
#211547=CARTESIAN_POINT('Ctrl Pts',(5.73430982499994,15.2,8.65519853099999));
#211548=CARTESIAN_POINT('Ctrl Pts',(5.73430982499994,11.6,8.65519853099999));
#211549=CARTESIAN_POINT('Ctrl Pts',(5.73370172099994,15.2,8.65444438599998));
#211550=CARTESIAN_POINT('Ctrl Pts',(5.73370172099994,11.6,8.65444438599998));
#211551=CARTESIAN_POINT('Ctrl Pts',(5.73310028599994,15.2,8.65369698599999));
#211552=CARTESIAN_POINT('Ctrl Pts',(5.73310028599994,11.6,8.65369698599999));
#211553=CARTESIAN_POINT('Ctrl Pts',(5.73250552599994,15.2,8.65295636199999));
#211554=CARTESIAN_POINT('Ctrl Pts',(5.73250552599994,11.6,8.65295636199999));
#211555=CARTESIAN_POINT('Ctrl Pts',(5.73191744099995,15.2,8.65222254499999));
#211556=CARTESIAN_POINT('Ctrl Pts',(5.73191744099995,11.6,8.65222254499999));
#211557=CARTESIAN_POINT('Ctrl Pts',(5.73133603499994,15.2,8.65149556999998));
#211558=CARTESIAN_POINT('Ctrl Pts',(5.73133603499994,11.6,8.65149556999998));
#211559=CARTESIAN_POINT('Ctrl Pts',(5.73076461999994,15.2,8.65077961499999));
#211560=CARTESIAN_POINT('Ctrl Pts',(5.73076461999994,11.6,8.65077961499999));
#211561=CARTESIAN_POINT('Ctrl Pts',(5.73031342099994,15.2,8.65021312599998));
#211562=CARTESIAN_POINT('Ctrl Pts',(5.73031342099994,11.6,8.65021312599998));
#211563=CARTESIAN_POINT('Ctrl Pts',(5.72997879099994,15.2,8.64979234999998));
#211564=CARTESIAN_POINT('Ctrl Pts',(5.72997879099994,11.6,8.64979234999998));
#211565=CARTESIAN_POINT('Ctrl Pts',(5.72975808699995,15.2,8.64951454399998));
#211566=CARTESIAN_POINT('Ctrl Pts',(5.72975808699995,11.6,8.64951454399998));
#211567=CARTESIAN_POINT('Ctrl Pts',(5.72964966099994,15.2,8.64937799999998));
#211568=CARTESIAN_POINT('Ctrl Pts',(5.72964966099994,11.6,8.64937799999998));
#211569=CARTESIAN_POINT('',(5.72964966093445,12.2,8.64937799923444));
#211570=CARTESIAN_POINT('',(5.72964966093445,15.2,8.64937799923444));
#211571=CARTESIAN_POINT('',(5.72964966099994,12.2,8.64937799899998));
#211572=CARTESIAN_POINT('Ctrl Pts',(6.67046385399994,12.2,9.36775917499999));
#211573=CARTESIAN_POINT('Ctrl Pts',(6.6671058818474,12.2,9.36593194382869));
#211574=CARTESIAN_POINT('Ctrl Pts',(6.66375578545945,12.2,9.36410408905281));
#211575=CARTESIAN_POINT('Ctrl Pts',(6.66041356410863,12.2,9.36227560222762));
#211576=CARTESIAN_POINT('Ctrl Pts',(6.65707134275782,12.2,9.36044711540242));
#211577=CARTESIAN_POINT('Ctrl Pts',(6.65373699675645,12.2,9.35861799819552));
#211578=CARTESIAN_POINT('Ctrl Pts',(6.65041053341856,12.2,9.35678826917066));
#211579=CARTESIAN_POINT('Ctrl Pts',(6.64597524856516,12.2,9.35434863024926));
#211580=CARTESIAN_POINT('Ctrl Pts',(6.64155397840679,12.2,9.35190790080295));
#211581=CARTESIAN_POINT('Ctrl Pts',(6.63714676338973,12.2,9.34946618105871));
#211582=CARTESIAN_POINT('Ctrl Pts',(6.63384135242718,12.2,9.34763489141686));
#211583=CARTESIAN_POINT('Ctrl Pts',(6.63054384824704,12.2,9.34580304603342));
#211584=CARTESIAN_POINT('Ctrl Pts',(6.62725426919988,12.2,9.34397068826666));
#211585=CARTESIAN_POINT('Ctrl Pts',(6.62396469015272,12.2,9.34213833049989));
#211586=CARTESIAN_POINT('Ctrl Pts',(6.62068303692194,12.2,9.34030545949983));
#211587=CARTESIAN_POINT('Ctrl Pts',(6.61740932137352,12.2,9.33847211023315));
#211588=CARTESIAN_POINT('Ctrl Pts',(6.61413560582511,12.2,9.33663876096647));
#211589=CARTESIAN_POINT('Ctrl Pts',(6.61086983012559,12.2,9.33480493332982));
#211590=CARTESIAN_POINT('Ctrl Pts',(6.60761200691361,12.2,9.33297066159654));
#211591=CARTESIAN_POINT('Ctrl Pts',(6.60435418370163,12.2,9.33113638986326));
#211592=CARTESIAN_POINT('Ctrl Pts',(6.60110431353991,12.2,9.32930167583331));
#211593=CARTESIAN_POINT('Ctrl Pts',(6.59786241440663,12.2,9.32746655815004));
#211594=CARTESIAN_POINT('Ctrl Pts',(6.59462051468439,12.2,9.3256314401334));
#211595=CARTESIAN_POINT('Ctrl Pts',(6.59138658419773,12.2,9.32379591866663));
#211596=CARTESIAN_POINT('Ctrl Pts',(6.58816063952165,12.2,9.32196003306644));
#211597=CARTESIAN_POINT('Ctrl Pts',(6.58493469543161,12.2,9.32012414779976));
#211598=CARTESIAN_POINT('Ctrl Pts',(6.58171673804949,12.2,9.31828789789976));
#211599=CARTESIAN_POINT('Ctrl Pts',(6.5785067809168,12.2,9.31645132209146));
#211600=CARTESIAN_POINT('Ctrl Pts',(6.57422683826761,12.2,9.31400255445826));
#211601=CARTESIAN_POINT('Ctrl Pts',(6.56996111897463,12.2,9.31155320486088));
#211602=CARTESIAN_POINT('Ctrl Pts',(6.56570965960855,12.2,9.30910336660547));
#211603=CARTESIAN_POINT('Ctrl Pts',(6.56039533496649,12.2,9.30604106853587));
#211604=CARTESIAN_POINT('Ctrl Pts',(6.55510329421805,12.2,9.30297800795032));
#211605=CARTESIAN_POINT('Ctrl Pts',(6.54983360636966,12.2,9.29991436420034));
#211606=CARTESIAN_POINT('Ctrl Pts',(6.54667179377551,12.2,9.29807617801715));
#211607=CARTESIAN_POINT('Ctrl Pts',(6.54351802822246,12.2,9.29623778218396));
#211608=CARTESIAN_POINT('Ctrl Pts',(6.54037232566899,12.2,9.29439921691746));
#211609=CARTESIAN_POINT('Ctrl Pts',(6.53722662254404,12.2,9.29256065131694));
#211610=CARTESIAN_POINT('Ctrl Pts',(6.53408898292138,12.2,9.29072191463304));
#211611=CARTESIAN_POINT('Ctrl Pts',(6.53095942080099,12.2,9.28888304807412));
#211612=CARTESIAN_POINT('Ctrl Pts',(6.52782985924913,12.2,9.28704418184924));
#211613=CARTESIAN_POINT('Ctrl Pts',(6.52470837625576,12.2,9.28520518526925));
#211614=CARTESIAN_POINT('Ctrl Pts',(6.52159498738094,12.2,9.28336609841083));
#211615=CARTESIAN_POINT('Ctrl Pts',(6.51848159850612,12.2,9.28152701155243));
#211616=CARTESIAN_POINT('Ctrl Pts',(6.51537630233253,12.2,9.27968783358269));
#211617=CARTESIAN_POINT('Ctrl Pts',(6.51227911573743,12.2,9.27784860631618));
#211618=CARTESIAN_POINT('Ctrl Pts',(6.50918192914233,12.2,9.27600937904966));
#211619=CARTESIAN_POINT('Ctrl Pts',(6.50609285223794,12.2,9.27417010098316));
#211620=CARTESIAN_POINT('Ctrl Pts',(6.50301189922488,12.2,9.27233081325832));
#211621=CARTESIAN_POINT('Ctrl Pts',(6.49993094621182,12.2,9.27049152553348));
#211622=CARTESIAN_POINT('Ctrl Pts',(6.4968581184401,12.2,9.2686522274503));
#211623=CARTESIAN_POINT('Ctrl Pts',(6.49379342984241,12.2,9.26681296122546));
#211624=CARTESIAN_POINT('Ctrl Pts',(6.49072874124472,12.2,9.26497369500062));
#211625=CARTESIAN_POINT('Ctrl Pts',(6.4876721920548,12.2,9.26313445950077));
#211626=CARTESIAN_POINT('Ctrl Pts',(6.48462379891444,12.2,9.26129529540092));
#211627=CARTESIAN_POINT('Ctrl Pts',(6.48157540522029,12.2,9.25945613096695));
#211628=CARTESIAN_POINT('Ctrl Pts',(6.47853516701179,12.2,9.25761703901634));
#211629=CARTESIAN_POINT('Ctrl Pts',(6.4755030988639,12.2,9.25577805958242));
#211630=CARTESIAN_POINT('Ctrl Pts',(6.47247103126683,12.2,9.25393908048258));
#211631=CARTESIAN_POINT('Ctrl Pts',(6.46944713415664,12.2,9.25210021516928));
#211632=CARTESIAN_POINT('Ctrl Pts',(6.46643142244985,12.2,9.25026150439425));
#211633=CARTESIAN_POINT('Ctrl Pts',(6.46341571074305,12.2,9.24842279361922));
#211634=CARTESIAN_POINT('Ctrl Pts',(6.46040818549674,12.2,9.24658423726613));
#211635=CARTESIAN_POINT('Ctrl Pts',(6.45740886143977,12.2,9.24474587754128));
#211636=CARTESIAN_POINT('Ctrl Pts',(6.4544095373828,12.2,9.24290751781643));
#211637=CARTESIAN_POINT('Ctrl Pts',(6.45141841504151,12.2,9.24106935351654));
#211638=CARTESIAN_POINT('Ctrl Pts',(6.44843550848322,12.2,9.23923142874998));
#211639=CARTESIAN_POINT('Ctrl Pts',(6.44545260192492,12.2,9.23739350398342));
#211640=CARTESIAN_POINT('Ctrl Pts',(6.44247791184965,12.2,9.23555581613354));
#211641=CARTESIAN_POINT('Ctrl Pts',(6.4395114533317,12.2,9.2337184104086));
#211642=CARTESIAN_POINT('Ctrl Pts',(6.43654499481376,12.2,9.23188100468366));
#211643=CARTESIAN_POINT('Ctrl Pts',(6.43358676976188,12.2,9.23004387978044));
#211644=CARTESIAN_POINT('Ctrl Pts',(6.43063679005406,12.2,9.22820707713037));
#211645=CARTESIAN_POINT('Ctrl Pts',(6.42768681034623,12.2,9.22637027448029));
#211646=CARTESIAN_POINT('Ctrl Pts',(6.42474507756727,12.2,9.22453379676693));
#211647=CARTESIAN_POINT('Ctrl Pts',(6.42181160742272,12.2,9.22269768416692));
#211648=CARTESIAN_POINT('Ctrl Pts',(6.41887813674525,12.2,9.22086157123335));
#211649=CARTESIAN_POINT('Ctrl Pts',(6.41595292835348,12.2,9.21902582433324));
#211650=CARTESIAN_POINT('Ctrl Pts',(6.413035997639,12.2,9.21719048639988));
#211651=CARTESIAN_POINT('Ctrl Pts',(6.40914675756954,12.2,9.21474336971111));
#211652=CARTESIAN_POINT('Ctrl Pts',(6.40527223088432,12.2,9.21229698082504));
#211653=CARTESIAN_POINT('Ctrl Pts',(6.40141245753223,12.2,9.20985142219158));
#211654=CARTESIAN_POINT('Ctrl Pts',(6.39851762738668,12.2,9.20801725313317));
#211655=CARTESIAN_POINT('Ctrl Pts',(6.395631094847,12.2,9.20618355192969));
#211656=CARTESIAN_POINT('Ctrl Pts',(6.39275287505683,12.2,9.20435036082133));
#211657=CARTESIAN_POINT('Ctrl Pts',(6.38987465526665,12.2,9.20251716971296));
#211658=CARTESIAN_POINT('Ctrl Pts',(6.38700474795421,12.2,9.20068449126623));
#211659=CARTESIAN_POINT('Ctrl Pts',(6.38414316884872,12.2,9.19885236666605));
#211660=CARTESIAN_POINT('Ctrl Pts',(6.38128158922337,12.2,9.19702024173304));
#211661=CARTESIAN_POINT('Ctrl Pts',(6.37842833804203,12.2,9.19518867110018));
#211662=CARTESIAN_POINT('Ctrl Pts',(6.37558342987971,12.2,9.19335770058416));
#211663=CARTESIAN_POINT('Ctrl Pts',(6.3727385222342,12.2,9.19152673040077));
#211664=CARTESIAN_POINT('Ctrl Pts',(6.3699019570716,12.2,9.18969635930069));
#211665=CARTESIAN_POINT('Ctrl Pts',(6.36707375092509,12.2,9.18786663261722));
#211666=CARTESIAN_POINT('Ctrl Pts',(6.36424554477857,12.2,9.18603690593375));
#211667=CARTESIAN_POINT('Ctrl Pts',(6.3614256971579,12.2,9.18420782217351));
#211668=CARTESIAN_POINT('Ctrl Pts',(6.35861422249733,12.2,9.18237942898165));
#211669=CARTESIAN_POINT('Ctrl Pts',(6.35580274783677,12.2,9.18055103578979));
#211670=CARTESIAN_POINT('Ctrl Pts',(6.35299964591362,12.2,9.1787233308769));
#211671=CARTESIAN_POINT('Ctrl Pts',(6.35020493279409,12.2,9.17689636026831));
#211672=CARTESIAN_POINT('Ctrl Pts',(6.34647864829625,12.2,9.17446039923558));
#211673=CARTESIAN_POINT('Ctrl Pts',(6.34276727724823,12.2,9.17202574417628));
#211674=CARTESIAN_POINT('Ctrl Pts',(6.33907085410387,12.2,9.16959250187715));
#211675=CARTESIAN_POINT('Ctrl Pts',(6.33537443146315,12.2,9.16715925990955));
#211676=CARTESIAN_POINT('Ctrl Pts',(6.33169295780377,12.2,9.16472743152231));
#211677=CARTESIAN_POINT('Ctrl Pts',(6.32802646782476,12.2,9.16229712616534));
#211678=CARTESIAN_POINT('Ctrl Pts',(6.32435997734619,12.2,9.15986682047724));
#211679=CARTESIAN_POINT('Ctrl Pts',(6.32070847097307,12.2,9.15743803640397));
#211680=CARTESIAN_POINT('Ctrl Pts',(6.31707198370562,12.2,9.15501088587279));
#211681=CARTESIAN_POINT('Ctrl Pts',(6.31252637486905,12.2,9.15197694787417));
#211682=CARTESIAN_POINT('Ctrl Pts',(6.30800423474288,12.2,9.1489455615425));
#211683=CARTESIAN_POINT('Ctrl Pts',(6.30350563266148,12.2,9.14591694161217));
#211684=CARTESIAN_POINT('Ctrl Pts',(6.29990675129056,12.2,9.14349404586599));
#211685=CARTESIAN_POINT('Ctrl Pts',(6.29632293268712,12.2,9.14107292328902));
#211686=CARTESIAN_POINT('Ctrl Pts',(6.29275421403344,12.2,9.1386536839311));
#211687=CARTESIAN_POINT('Ctrl Pts',(6.28918549489351,12.2,9.13623444424358));
#211688=CARTESIAN_POINT('Ctrl Pts',(6.28563187545207,12.2,9.13381708826275));
#211689=CARTESIAN_POINT('Ctrl Pts',(6.28209339069486,12.2,9.13140172989951));
#211690=CARTESIAN_POINT('Ctrl Pts',(6.27855490641977,12.2,9.12898637186537));
#211691=CARTESIAN_POINT('Ctrl Pts',(6.27503155668436,12.2,9.12657301194737));
#211692=CARTESIAN_POINT('Ctrl Pts',(6.27152337730349,12.2,9.12416176342212));
#211693=CARTESIAN_POINT('Ctrl Pts',(6.26801519744462,12.2,9.12175051456834));
#211694=CARTESIAN_POINT('Ctrl Pts',(6.26452218674315,12.2,9.11934137720371));
#211695=CARTESIAN_POINT('Ctrl Pts',(6.26104438166573,12.2,9.11693446879491));
#211696=CARTESIAN_POINT('Ctrl Pts',(6.25756657706216,12.2,9.11452756071404));
#211697=CARTESIAN_POINT('Ctrl Pts',(6.2541039794808,12.2,9.11212287958908));
#211698=CARTESIAN_POINT('Ctrl Pts',(6.25065662003354,12.2,9.10972054166525));
#211699=CARTESIAN_POINT('Ctrl Pts',(6.24634742037217,12.2,9.10671761901499));
#211700=CARTESIAN_POINT('Ctrl Pts',(6.24206203533554,12.2,9.10371836136277));
#211701=CARTESIAN_POINT('Ctrl Pts',(6.23780053082039,12.2,9.10072299469589));
#211702=CARTESIAN_POINT('Ctrl Pts',(6.23439132702247,12.2,9.09832670123178));
#211703=CARTESIAN_POINT('Ctrl Pts',(6.23099740759029,12.2,9.095932900018));
#211704=CARTESIAN_POINT('Ctrl Pts',(6.22761880774049,12.2,9.09354170855452));
#211705=CARTESIAN_POINT('Ctrl Pts',(6.22424020835103,12.2,9.09115051741683));
#211706=CARTESIAN_POINT('Ctrl Pts',(6.22087692853601,12.2,9.08876193805375));
#211707=CARTESIAN_POINT('Ctrl Pts',(6.21752900175238,12.2,9.08637608879615));
#211708=CARTESIAN_POINT('Ctrl Pts',(6.21418107451258,12.2,9.08399023921346));
#211709=CARTESIAN_POINT('Ctrl Pts',(6.21084850170585,12.2,9.08160712092661));
#211710=CARTESIAN_POINT('Ctrl Pts',(6.20753131847051,12.2,9.07922685529708));
#211711=CARTESIAN_POINT('Ctrl Pts',(6.20421413568714,12.2,9.07684658999184));
#211712=CARTESIAN_POINT('Ctrl Pts',(6.20091234171459,12.2,9.07446917552217));
#211713=CARTESIAN_POINT('Ctrl Pts',(6.19762597053721,12.2,9.07209473760486));
#211714=CARTESIAN_POINT('Ctrl Pts',(6.19433959891206,12.2,9.06972029936403));
#211715=CARTESIAN_POINT('Ctrl Pts',(6.19106865276064,12.2,9.06734883552906));
#211716=CARTESIAN_POINT('Ctrl Pts',(6.18781316424988,12.2,9.06498047073331));
#211717=CARTESIAN_POINT('Ctrl Pts',(6.18455767573913,12.2,9.06261210593757));
#211718=CARTESIAN_POINT('Ctrl Pts',(6.18131764480794,12.2,9.06024684137829));
#211719=CARTESIAN_POINT('Ctrl Pts',(6.17809310818935,12.2,9.05788479930545));
#211720=CARTESIAN_POINT('Ctrl Pts',(6.1748685720101,12.2,9.05552275755444));
#211721=CARTESIAN_POINT('Ctrl Pts',(6.17165952789167,12.2,9.05316394038639));
#211722=CARTESIAN_POINT('Ctrl Pts',(6.16846601252706,12.2,9.05080847323491));
#211723=CARTESIAN_POINT('Ctrl Pts',(6.16447411799498,12.2,9.04786413905486));
#211724=CARTESIAN_POINT('Ctrl Pts',(6.16050648444987,12.2,9.04492503999997));
#211725=CARTESIAN_POINT('Ctrl Pts',(6.15656318153321,12.2,9.04199142499997));
#211726=CARTESIAN_POINT('Ctrl Pts',(6.15340853902796,12.2,9.03964453287206));
#211727=CARTESIAN_POINT('Ctrl Pts',(6.15026946639395,12.2,9.03730114992513));
#211728=CARTESIAN_POINT('Ctrl Pts',(6.14714599928086,12.2,9.03496140707575));
#211729=CARTESIAN_POINT('Ctrl Pts',(6.14402253259335,12.2,9.03262166454518));
#211730=CARTESIAN_POINT('Ctrl Pts',(6.1409146728383,12.2,9.03028556102427));
#211731=CARTESIAN_POINT('Ctrl Pts',(6.13782245024366,12.2,9.0279532272599));
#211732=CARTESIAN_POINT('Ctrl Pts',(6.13473022722772,12.2,9.02562089317774));
#211733=CARTESIAN_POINT('Ctrl Pts',(6.13165364598967,12.2,9.02329232778231));
#211734=CARTESIAN_POINT('Ctrl Pts',(6.1285927369911,12.2,9.02096766437823));
#211735=CARTESIAN_POINT('Ctrl Pts',(6.12553182840959,12.2,9.01864300129088));
#211736=CARTESIAN_POINT('Ctrl Pts',(6.12248659518995,12.2,9.0163222401336));
#211737=CARTESIAN_POINT('Ctrl Pts',(6.11945706854769,12.2,9.01400551365607));
#211738=CARTESIAN_POINT('Ctrl Pts',(6.11642754149265,12.2,9.01168878686287));
#211739=CARTESIAN_POINT('Ctrl Pts',(6.11341372247396,12.2,9.0093760948308));
#211740=CARTESIAN_POINT('Ctrl Pts',(6.11041564577326,12.2,9.00706757142334));
#211741=CARTESIAN_POINT('Ctrl Pts',(6.10741756948106,12.2,9.00475904833043));
#211742=CARTESIAN_POINT('Ctrl Pts',(6.10443523627051,12.2,9.00245469451696));
#211743=CARTESIAN_POINT('Ctrl Pts',(6.10146867823422,12.2,9.00015464670471));
#211744=CARTESIAN_POINT('Ctrl Pts',(6.09850211979372,12.2,8.99785459857906));
#211745=CARTESIAN_POINT('Ctrl Pts',(6.09555133760237,12.2,8.99555885554841));
#211746=CARTESIAN_POINT('Ctrl Pts',(6.09261636577676,12.2,8.9932675543127));
#211747=CARTESIAN_POINT('Ctrl Pts',(6.08968139435104,12.2,8.99097625338917));
#211748=CARTESIAN_POINT('Ctrl Pts',(6.08676223358588,12.2,8.98868939669511));
#211749=CARTESIAN_POINT('Ctrl Pts',(6.08385891545459,12.2,8.98640712082283));
#211750=CARTESIAN_POINT('Ctrl Pts',(6.08095559692772,12.2,8.9841248446396));
#211751=CARTESIAN_POINT('Ctrl Pts',(6.07806812308744,12.2,8.98184714922667));
#211752=CARTESIAN_POINT('Ctrl Pts',(6.07519652726528,12.2,8.97957417654753));
#211753=CARTESIAN_POINT('Ctrl Pts',(6.07232493183439,12.2,8.97730120417809));
#211754=CARTESIAN_POINT('Ctrl Pts',(6.06946921353368,12.2,8.97503295278828));
#211755=CARTESIAN_POINT('Ctrl Pts',(6.06662940743087,12.2,8.9727695663617));
#211756=CARTESIAN_POINT('Ctrl Pts',(6.06378960094111,12.2,8.97050617962672));
#211757=CARTESIAN_POINT('Ctrl Pts',(6.06096570593593,12.2,8.96824765529258));
#211758=CARTESIAN_POINT('Ctrl Pts',(6.05815775554798,12.2,8.9659941387151));
#211759=CARTESIAN_POINT('Ctrl Pts',(6.0553498055426,12.2,8.96374062244466));
#211760=CARTESIAN_POINT('Ctrl Pts',(6.05255780151458,12.2,8.961492114295));
#211761=CARTESIAN_POINT('Ctrl Pts',(6.04978177546211,12.2,8.95924875736676));
#211762=CARTESIAN_POINT('Ctrl Pts',(6.0470057490314,12.2,8.95700540013286));
#211763=CARTESIAN_POINT('Ctrl Pts',(6.04424570233554,12.2,8.95476719471332));
#211764=CARTESIAN_POINT('Ctrl Pts',(6.04150166724154,12.2,8.95253428875829));
#211765=CARTESIAN_POINT('Ctrl Pts',(6.03875763214755,12.2,8.95030138280327));
#211766=CARTESIAN_POINT('Ctrl Pts',(6.03602960957208,12.2,8.94807377593496));
#211767=CARTESIAN_POINT('Ctrl Pts',(6.03331763181482,12.2,8.94585161536998));
#211768=CARTESIAN_POINT('Ctrl Pts',(6.03060565442707,12.2,8.94362945510777));
#211769=CARTESIAN_POINT('Ctrl Pts',(6.02790972416707,12.2,8.94141274234743));
#211770=CARTESIAN_POINT('Ctrl Pts',(6.02522987148504,12.2,8.93920162551813));
#211771=CARTESIAN_POINT('Ctrl Pts',(6.02255001843789,12.2,8.93699050838758));
#211772=CARTESIAN_POINT('Ctrl Pts',(6.01988624559575,12.2,8.93478498847348));
#211773=CARTESIAN_POINT('Ctrl Pts',(6.017238583842,12.2,8.93258521663197));
#211774=CARTESIAN_POINT('Ctrl Pts',(6.014590922449,12.2,8.93038544509017));
#211775=CARTESIAN_POINT('Ctrl Pts',(6.01195937395665,12.2,8.92819142275318));
#211776=CARTESIAN_POINT('Ctrl Pts',(6.00934396994718,12.2,8.9260033006539));
#211777=CARTESIAN_POINT('Ctrl Pts',(6.00672856558136,12.2,8.92381517825648));
#211778=CARTESIAN_POINT('Ctrl Pts',(6.00412930736298,12.2,8.92163295911099));
#211779=CARTESIAN_POINT('Ctrl Pts',(6.00154622681681,12.2,8.91945679521755));
#211780=CARTESIAN_POINT('Ctrl Pts',(5.99896314662258,12.2,8.9172806316206));
#211781=CARTESIAN_POINT('Ctrl Pts',(5.99639624582055,12.2,8.91511052588654));
#211782=CARTESIAN_POINT('Ctrl Pts',(5.99384555575022,12.2,8.91294663245192));
#211783=CARTESIAN_POINT('Ctrl Pts',(5.99065719290165,12.2,8.91024176543752));
#211784=CARTESIAN_POINT('Ctrl Pts',(5.98749416057878,12.2,8.90754660677615));
#211785=CARTESIAN_POINT('Ctrl Pts',(5.98435652273024,12.2,8.9048614671923));
#211786=CARTESIAN_POINT('Ctrl Pts',(5.9812188848817,12.2,8.90217632760845));
#211787=CARTESIAN_POINT('Ctrl Pts',(5.97810664153232,12.2,8.89950120595799));
#211788=CARTESIAN_POINT('Ctrl Pts',(5.9750198569349,12.2,8.89683641879307));
#211789=CARTESIAN_POINT('Ctrl Pts',(5.97193307233748,12.2,8.89417163162817));
#211790=CARTESIAN_POINT('Ctrl Pts',(5.96887174610543,12.2,8.89151717811661));
#211791=CARTESIAN_POINT('Ctrl Pts',(5.96583594304987,12.2,8.88887337624163));
#211792=CARTESIAN_POINT('Ctrl Pts',(5.96280013999433,12.2,8.88622957436663));
#211793=CARTESIAN_POINT('Ctrl Pts',(5.95978985804985,12.2,8.88359642708883));
#211794=CARTESIAN_POINT('Ctrl Pts',(5.95680516346653,12.2,8.88097425674161));
#211795=CARTESIAN_POINT('Ctrl Pts',(5.95382046888323,12.2,8.87835208639441));
#211796=CARTESIAN_POINT('Ctrl Pts',(5.95086135960598,12.2,8.87574089275476));
#211797=CARTESIAN_POINT('Ctrl Pts',(5.94792790077328,12.2,8.87314100725687));
#211798=CARTESIAN_POINT('Ctrl Pts',(5.94499444194058,12.2,8.87054112175899));
#211799=CARTESIAN_POINT('Ctrl Pts',(5.94208663164353,12.2,8.86795254016976));
#211800=CARTESIAN_POINT('Ctrl Pts',(5.93920453456154,12.2,8.86537560232316));
#211801=CARTESIAN_POINT('Ctrl Pts',(5.93632243747956,12.2,8.86279866447657));
#211802=CARTESIAN_POINT('Ctrl Pts',(5.93346605321914,12.2,8.86023336646575));
#211803=CARTESIAN_POINT('Ctrl Pts',(5.93063544453991,12.2,8.85768004959138));
#211804=CARTESIAN_POINT('Ctrl Pts',(5.92780483586069,12.2,8.85512673271699));
#211805=CARTESIAN_POINT('Ctrl Pts',(5.92500000295331,12.2,8.85258539625413));
#211806=CARTESIAN_POINT('Ctrl Pts',(5.92222100892737,12.2,8.85005638598975));
#211807=CARTESIAN_POINT('Ctrl Pts',(5.91944201490143,12.2,8.84752737572535));
#211808=CARTESIAN_POINT('Ctrl Pts',(5.91668885870217,12.2,8.84501069001584));
#211809=CARTESIAN_POINT('Ctrl Pts',(5.9139616034265,12.2,8.84250668140577));
#211810=CARTESIAN_POINT('Ctrl Pts',(5.91123434815083,12.2,8.84000267279569));
#211811=CARTESIAN_POINT('Ctrl Pts',(5.90853299426447,12.2,8.83751133963026));
#211812=CARTESIAN_POINT('Ctrl Pts',(5.90585760384995,12.2,8.83503303865913));
#211813=CARTESIAN_POINT('Ctrl Pts',(5.90318221372705,12.2,8.83255473795813));
#211814=CARTESIAN_POINT('Ctrl Pts',(5.90053278688699,12.2,8.83008946886562));
#211815=CARTESIAN_POINT('Ctrl Pts',(5.89790938585136,12.2,8.82763759406233));
#211816=CARTESIAN_POINT('Ctrl Pts',(5.89528598452978,12.2,8.82518571899178));
#211817=CARTESIAN_POINT('Ctrl Pts',(5.8926886087717,12.2,8.82274723660714));
#211818=CARTESIAN_POINT('Ctrl Pts',(5.89011732001954,12.2,8.82032251730044));
#211819=CARTESIAN_POINT('Ctrl Pts',(5.88754603126739,12.2,8.81789779799374));
#211820=CARTESIAN_POINT('Ctrl Pts',(5.88500083064228,12.2,8.81548683936562));
#211821=CARTESIAN_POINT('Ctrl Pts',(5.88248177850073,12.2,8.8130900167449));
#211822=CARTESIAN_POINT('Ctrl Pts',(5.87996272635918,12.2,8.81069319412419));
#211823=CARTESIAN_POINT('Ctrl Pts',(5.87746982396273,12.2,8.80831050698901));
#211824=CARTESIAN_POINT('Ctrl Pts',(5.87500313187802,12.2,8.80594233615491));
#211825=CARTESIAN_POINT('Ctrl Pts',(5.87253643979331,12.2,8.80357416532081));
#211826=CARTESIAN_POINT('Ctrl Pts',(5.87009595785373,12.2,8.80122050867043));
#211827=CARTESIAN_POINT('Ctrl Pts',(5.86768174819959,12.2,8.79888175616966));
#211828=CARTESIAN_POINT('Ctrl Pts',(5.86478469671989,12.2,8.79607525327071));
#211829=CARTESIAN_POINT('Ctrl Pts',(5.86192547658248,12.2,8.79329020901056));
#211830=CARTESIAN_POINT('Ctrl Pts',(5.85910419326574,12.2,8.79052730435944));
#211831=CARTESIAN_POINT('Ctrl Pts',(5.85628290969271,12.2,8.78776439945734));
#211832=CARTESIAN_POINT('Ctrl Pts',(5.85349956259004,12.2,8.78502363625738));
#211833=CARTESIAN_POINT('Ctrl Pts',(5.85075425885876,12.2,8.78230570736025));
#211834=CARTESIAN_POINT('Ctrl Pts',(5.84755140487964,12.2,8.77913479068393));
#211835=CARTESIAN_POINT('Ctrl Pts',(5.84440032854945,12.2,8.77599495627641));
#211836=CARTESIAN_POINT('Ctrl Pts',(5.84130119832276,12.2,8.77288733252362));
#211837=CARTESIAN_POINT('Ctrl Pts',(5.83864480067538,12.2,8.77022365471015));
#211838=CARTESIAN_POINT('Ctrl Pts',(5.83602656652335,12.2,8.76758364347395));
#211839=CARTESIAN_POINT('Ctrl Pts',(5.83344660080109,12.2,8.76496802491582));
#211840=CARTESIAN_POINT('Ctrl Pts',(5.83086663531318,12.2,8.76235240659527));
#211841=CARTESIAN_POINT('Ctrl Pts',(5.82832493726317,12.2,8.75976118361123));
#211842=CARTESIAN_POINT('Ctrl Pts',(5.82582161075935,12.2,8.7571950982761));
#211843=CARTESIAN_POINT('Ctrl Pts',(5.82331828425552,12.2,8.75462901294098));
#211844=CARTESIAN_POINT('Ctrl Pts',(5.82085332991217,12.2,8.75208806698448));
#211845=CARTESIAN_POINT('Ctrl Pts',(5.8184268494977,12.2,8.74957302074075));
#211846=CARTESIAN_POINT('Ctrl Pts',(5.81600036886283,12.2,8.74705797426858));
#211847=CARTESIAN_POINT('Ctrl Pts',(5.81361236392419,12.2,8.74456882772578));
#211848=CARTESIAN_POINT('Ctrl Pts',(5.81126293426436,12.2,8.74210636005346));
#211849=CARTESIAN_POINT('Ctrl Pts',(5.80891350481795,12.2,8.73964389260483));
#211850=CARTESIAN_POINT('Ctrl Pts',(5.80660265493396,12.2,8.73720810406243));
#211851=CARTESIAN_POINT('Ctrl Pts',(5.80433048351653,12.2,8.73479978998325));
#211852=CARTESIAN_POINT('Ctrl Pts',(5.80205831209908,12.2,8.73239147590408));
#211853=CARTESIAN_POINT('Ctrl Pts',(5.79982481950369,12.2,8.73001063901449));
#211854=CARTESIAN_POINT('Ctrl Pts',(5.79763010899744,12.2,8.7276580920147));
#211855=CARTESIAN_POINT('Ctrl Pts',(5.79543539829184,12.2,8.72530554480121));
#211856=CARTESIAN_POINT('Ctrl Pts',(5.79327946874741,12.2,8.72298129074938));
#211857=CARTESIAN_POINT('Ctrl Pts',(5.7911624220285,12.2,8.72068616151131));
#211858=CARTESIAN_POINT('Ctrl Pts',(5.7890453755019,12.2,8.71839103248172));
#211859=CARTESIAN_POINT('Ctrl Pts',(5.78696721260079,12.2,8.71612503132703));
#211860=CARTESIAN_POINT('Ctrl Pts',(5.78492803225821,12.2,8.7138890114916));
#211861=CARTESIAN_POINT('Ctrl Pts',(5.78288885191562,12.2,8.71165299165615));
#211862=CARTESIAN_POINT('Ctrl Pts',(5.78088865678534,12.2,8.70944695629186));
#211863=CARTESIAN_POINT('Ctrl Pts',(5.77892754525635,12.2,8.7072717794271));
#211864=CARTESIAN_POINT('Ctrl Pts',(5.77696643354925,12.2,8.70509660236476));
#211865=CARTESIAN_POINT('Ctrl Pts',(5.77504440614461,12.2,8.70295228505764));
#211866=CARTESIAN_POINT('Ctrl Pts',(5.77316156354465,12.2,8.700839728028));
#211867=CARTESIAN_POINT('Ctrl Pts',(5.77127872111573,12.2,8.69872717119023));
#211868=CARTESIAN_POINT('Ctrl Pts',(5.76943506489992,12.2,8.69664637181713));
#211869=CARTESIAN_POINT('Ctrl Pts',(5.76763069154072,12.2,8.69459825521566));
#211870=CARTESIAN_POINT('Ctrl Pts',(5.76582631818152,12.2,8.69255013861418));
#211871=CARTESIAN_POINT('Ctrl Pts',(5.76406122962478,12.2,8.69053470495421));
#211872=CARTESIAN_POINT('Ctrl Pts',(5.76233552610243,12.2,8.68855290035808));
#211873=CARTESIAN_POINT('Ctrl Pts',(5.76060982242332,12.2,8.68657109558192));
#211874=CARTESIAN_POINT('Ctrl Pts',(5.75892350278245,12.2,8.6846229190683));
#211875=CARTESIAN_POINT('Ctrl Pts',(5.75727666527871,12.2,8.68270934454968));
#211876=CARTESIAN_POINT('Ctrl Pts',(5.75562982792455,12.2,8.68079577020487));
#211877=CARTESIAN_POINT('Ctrl Pts',(5.75402247582258,12.2,8.67891679728942));
#211878=CARTESIAN_POINT('Ctrl Pts',(5.75245470438126,12.2,8.67707342594128));
#211879=CARTESIAN_POINT('Ctrl Pts',(5.75088693293994,12.2,8.67523005459314));
#211880=CARTESIAN_POINT('Ctrl Pts',(5.74935874527049,12.2,8.67342228223386));
#211881=CARTESIAN_POINT('Ctrl Pts',(5.74787023690616,12.2,8.67165113912993));
#211882=CARTESIAN_POINT('Ctrl Pts',(5.74638172854184,12.2,8.66987999602601));
#211883=CARTESIAN_POINT('Ctrl Pts',(5.74493290056333,12.2,8.66814547940082));
#211884=CARTESIAN_POINT('Ctrl Pts',(5.7435238538618,12.2,8.66644864820988));
#211885=CARTESIAN_POINT('Ctrl Pts',(5.74211480703228,12.2,8.66475181686481));
#211886=CARTESIAN_POINT('Ctrl Pts',(5.74074553694831,12.2,8.66309266816506));
#211887=CARTESIAN_POINT('Ctrl Pts',(5.73941614621092,12.2,8.66147228941177));
#211888=CARTESIAN_POINT('Ctrl Pts',(5.73808675559428,12.2,8.65985191080565));
#211889=CARTESIAN_POINT('Ctrl Pts',(5.7367972402858,12.2,8.65827030439334));
#211890=CARTESIAN_POINT('Ctrl Pts',(5.73554770174212,12.2,8.65672858669229));
#211891=CARTESIAN_POINT('Ctrl Pts',(5.7334711343,12.2,8.65416645621689));
#211892=CARTESIAN_POINT('Ctrl Pts',(5.73150497962641,12.2,8.65171445644522));
#211893=CARTESIAN_POINT('Ctrl Pts',(5.72964966099994,12.2,8.64937799999998));
#211894=CARTESIAN_POINT('Ctrl Pts',(5.72964966099994,15.2,8.64937799999998));
#211895=CARTESIAN_POINT('Ctrl Pts',(5.73076070896187,15.2,8.65077717485576));
#211896=CARTESIAN_POINT('Ctrl Pts',(5.731911500976,15.2,8.65221780246531));
#211897=CARTESIAN_POINT('Ctrl Pts',(5.7331019545695,15.2,8.65369867983773));
#211898=CARTESIAN_POINT('Ctrl Pts',(5.73429814913197,15.2,8.65518669874938));
#211899=CARTESIAN_POINT('Ctrl Pts',(5.73553438373783,15.2,8.65671537363565));
#211900=CARTESIAN_POINT('Ctrl Pts',(5.73681056237342,15.2,8.65828356063504));
#211901=CARTESIAN_POINT('Ctrl Pts',(5.73808674089308,15.2,8.65985174749198));
#211902=CARTESIAN_POINT('Ctrl Pts',(5.73940286065744,15.2,8.66145944675969));
#211903=CARTESIAN_POINT('Ctrl Pts',(5.74075882602487,15.2,8.66310555069991));
#211904=CARTESIAN_POINT('Ctrl Pts',(5.74211479139229,15.2,8.66475165464014));
#211905=CARTESIAN_POINT('Ctrl Pts',(5.74351060050216,15.2,8.66643616409547));
#211906=CARTESIAN_POINT('Ctrl Pts',(5.74494615710277,15.2,8.66815800211678));
#211907=CARTESIAN_POINT('Ctrl Pts',(5.74638171383377,15.2,8.6698798402945));
#211908=CARTESIAN_POINT('Ctrl Pts',(5.74785701674642,15.2,8.67163900569532));
#211909=CARTESIAN_POINT('Ctrl Pts',(5.74937196816501,15.2,8.6734344539623));
#211910=CARTESIAN_POINT('Ctrl Pts',(5.75088691944599,15.2,8.67522990206619));
#211911=CARTESIAN_POINT('Ctrl Pts',(5.75244151836787,15.2,8.6770616323184));
#211912=CARTESIAN_POINT('Ctrl Pts',(5.75403566598394,15.2,8.67892862750911));
#211913=CARTESIAN_POINT('Ctrl Pts',(5.7556298136,15.2,8.68079562269983));
#211914=CARTESIAN_POINT('Ctrl Pts',(5.75726351227137,15.2,8.68269788279138));
#211915=CARTESIAN_POINT('Ctrl Pts',(5.75893665987552,15.2,8.6846344171362));
#211916=CARTESIAN_POINT('Ctrl Pts',(5.76060980763166,15.2,8.68657095165691));
#211917=CARTESIAN_POINT('Ctrl Pts',(5.76232240510937,15.2,8.68854176053192));
#211918=CARTESIAN_POINT('Ctrl Pts',(5.76407435470751,15.2,8.69054588022672));
#211919=CARTESIAN_POINT('Ctrl Pts',(5.76582630414653,15.2,8.69254999973948));
#211920=CARTESIAN_POINT('Ctrl Pts',(5.76761760416457,15.2,8.69458743088663));
#211921=CARTESIAN_POINT('Ctrl Pts',(5.76944815559981,15.2,8.6966572326462));
#211922=CARTESIAN_POINT('Ctrl Pts',(5.77127870703505,15.2,8.69872703440579));
#211923=CARTESIAN_POINT('Ctrl Pts',(5.77314850964208,15.2,8.70082920789601));
#211924=CARTESIAN_POINT('Ctrl Pts',(5.77505746415434,15.2,8.70296283865045));
#211925=CARTESIAN_POINT('Ctrl Pts',(5.77696641866661,15.2,8.70509646940489));
#211926=CARTESIAN_POINT('Ctrl Pts',(5.77891452415813,15.2,8.70726155765079));
#211927=CARTESIAN_POINT('Ctrl Pts',(5.78090168058329,15.2,8.70945721048562));
#211928=CARTESIAN_POINT('Ctrl Pts',(5.78288883718896,15.2,8.7116528635199));
#211929=CARTESIAN_POINT('Ctrl Pts',(5.78491504540668,15.2,8.71387908124878));
#211930=CARTESIAN_POINT('Ctrl Pts',(5.78698020310426,15.2,8.716134994373));
#211931=CARTESIAN_POINT('Ctrl Pts',(5.78938955347004,15.2,8.71876689271056));
#211932=CARTESIAN_POINT('Ctrl Pts',(5.79185192008576,15.2,8.72143920784557));
#211933=CARTESIAN_POINT('Ctrl Pts',(5.79436714077323,15.2,8.72415059477162));
#211934=CARTESIAN_POINT('Ctrl Pts',(5.79652304447141,15.2,8.72647464097966));
#211935=CARTESIAN_POINT('Ctrl Pts',(5.79871778110668,15.2,8.7288273938155));
#211936=CARTESIAN_POINT('Ctrl Pts',(5.80095124864676,15.2,8.73120802811313));
#211937=CARTESIAN_POINT('Ctrl Pts',(5.80318471598397,15.2,8.73358866219452));
#211938=CARTESIAN_POINT('Ctrl Pts',(5.80545691140975,15.2,8.73599717787366));
#211939=CARTESIAN_POINT('Ctrl Pts',(5.8077677368241,15.2,8.73843276711731));
#211940=CARTESIAN_POINT('Ctrl Pts',(5.81123397515551,15.2,8.74208615120402));
#211941=CARTESIAN_POINT('Ctrl Pts',(5.81478712865559,15.2,8.74580045114671));
#211942=CARTESIAN_POINT('Ctrl Pts',(5.8184268494977,15.2,8.74957302074075));
#211943=CARTESIAN_POINT('Ctrl Pts',(5.82085332991218,15.2,8.75208806698448));
#211944=CARTESIAN_POINT('Ctrl Pts',(5.82331828425553,15.2,8.75462901294099));
#211945=CARTESIAN_POINT('Ctrl Pts',(5.82582161075935,15.2,8.75719509827611));
#211946=CARTESIAN_POINT('Ctrl Pts',(5.82832493726318,15.2,8.75976118361123));
#211947=CARTESIAN_POINT('Ctrl Pts',(5.83086663531317,15.2,8.76235240659527));
#211948=CARTESIAN_POINT('Ctrl Pts',(5.8334466008011,15.2,8.76496802491582));
#211949=CARTESIAN_POINT('Ctrl Pts',(5.83602656652336,15.2,8.76758364347396));
#211950=CARTESIAN_POINT('Ctrl Pts',(5.83864480067538,15.2,8.77022365471015));
#211951=CARTESIAN_POINT('Ctrl Pts',(5.84130119832277,15.2,8.77288733252363));
#211952=CARTESIAN_POINT('Ctrl Pts',(5.84395759572888,15.2,8.77555101009516));
#211953=CARTESIAN_POINT('Ctrl Pts',(5.84665215749663,15.2,8.77823835307859));
#211954=CARTESIAN_POINT('Ctrl Pts',(5.84938477789897,15.2,8.78094864964775));
#211955=CARTESIAN_POINT('Ctrl Pts',(5.85211739830131,15.2,8.78365894621693));
#211956=CARTESIAN_POINT('Ctrl Pts',(5.8548880786423,15.2,8.78639219407594));
#211957=CARTESIAN_POINT('Ctrl Pts',(5.85769671312197,15.2,8.7891476995582));
#211958=CARTESIAN_POINT('Ctrl Pts',(5.86050534760164,15.2,8.79190320504047));
#211959=CARTESIAN_POINT('Ctrl Pts',(5.86335193650951,15.2,8.79468096380633));
#211960=CARTESIAN_POINT('Ctrl Pts',(5.86623637490215,15.2,8.79748029545316));
#211961=CARTESIAN_POINT('Ctrl Pts',(5.86864007365003,15.2,8.79981307191029));
#211962=CARTESIAN_POINT('Ctrl Pts',(5.87107005561963,15.2,8.80216082902547));
#211963=CARTESIAN_POINT('Ctrl Pts',(5.87352626172862,15.2,8.80452317819096));
#211964=CARTESIAN_POINT('Ctrl Pts',(5.87598246783761,15.2,8.80688552735646));
#211965=CARTESIAN_POINT('Ctrl Pts',(5.87846489537969,15.2,8.8092624695595));
#211966=CARTESIAN_POINT('Ctrl Pts',(5.88097348522543,15.2,8.81165362224742));
#211967=CARTESIAN_POINT('Ctrl Pts',(5.88348207507117,15.2,8.81404477493533));
#211968=CARTESIAN_POINT('Ctrl Pts',(5.88601682607281,15.2,8.81645014055365));
#211969=CARTESIAN_POINT('Ctrl Pts',(5.88857767739089,15.2,8.81886933985848));
#211970=CARTESIAN_POINT('Ctrl Pts',(5.89113852870896,15.2,8.82128853916331));
#211971=CARTESIAN_POINT('Ctrl Pts',(5.89372547933051,15.2,8.82372157627962));
#211972=CARTESIAN_POINT('Ctrl Pts',(5.89633846807914,15.2,8.82616807884836));
#211973=CARTESIAN_POINT('Ctrl Pts',(5.89895145682779,15.2,8.82861458141711));
#211974=CARTESIAN_POINT('Ctrl Pts',(5.90159048412528,15.2,8.83107455085408));
#211975=CARTESIAN_POINT('Ctrl Pts',(5.9042554862901,15.2,8.83354762503194));
#211976=CARTESIAN_POINT('Ctrl Pts',(5.90745348877168,15.2,8.83651531393756));
#211977=CARTESIAN_POINT('Ctrl Pts',(5.9106888972146,15.2,8.83950187118285));
#211978=CARTESIAN_POINT('Ctrl Pts',(5.9139616034265,15.2,8.84250668140577));
#211979=CARTESIAN_POINT('Ctrl Pts',(5.91668885870217,15.2,8.84501069001585));
#211980=CARTESIAN_POINT('Ctrl Pts',(5.91944201490142,15.2,8.84752737572535));
#211981=CARTESIAN_POINT('Ctrl Pts',(5.92222100892737,15.2,8.85005638598975));
#211982=CARTESIAN_POINT('Ctrl Pts',(5.92500000295333,15.2,8.85258539625415));
#211983=CARTESIAN_POINT('Ctrl Pts',(5.9278048358607,15.2,8.85512673271699));
#211984=CARTESIAN_POINT('Ctrl Pts',(5.93063544453991,15.2,8.85768004959138));
#211985=CARTESIAN_POINT('Ctrl Pts',(5.93346605321913,15.2,8.86023336646575));
#211986=CARTESIAN_POINT('Ctrl Pts',(5.93632243747956,15.2,8.86279866447656));
#211987=CARTESIAN_POINT('Ctrl Pts',(5.93920453456154,15.2,8.86537560232316));
#211988=CARTESIAN_POINT('Ctrl Pts',(5.94266305093427,15.2,8.86846792762673));
#211989=CARTESIAN_POINT('Ctrl Pts',(5.94615859363737,15.2,8.87157701808228));
#211990=CARTESIAN_POINT('Ctrl Pts',(5.94969105308986,15.2,8.87470229238431));
#211991=CARTESIAN_POINT('Ctrl Pts',(5.95322351286323,15.2,8.87782756697023));
#211992=CARTESIAN_POINT('Ctrl Pts',(5.95679289023178,15.2,8.88096902934102));
#211993=CARTESIAN_POINT('Ctrl Pts',(5.96039907492991,15.2,8.88412610993042));
#211994=CARTESIAN_POINT('Ctrl Pts',(5.96340422868123,15.2,8.88675701027819));
#211995=CARTESIAN_POINT('Ctrl Pts',(5.96643494304858,15.2,8.88939875880627));
#211996=CARTESIAN_POINT('Ctrl Pts',(5.96949115429991,15.2,8.89205103089015));
#211997=CARTESIAN_POINT('Ctrl Pts',(5.97254736555123,15.2,8.89470330297401));
#211998=CARTESIAN_POINT('Ctrl Pts',(5.97562907338701,15.2,8.8973660997816));
#211999=CARTESIAN_POINT('Ctrl Pts',(5.978736214794,15.2,8.90003910436029));
#212000=CARTESIAN_POINT('Ctrl Pts',(5.98184335620099,15.2,8.90271210893899));
#212001=CARTESIAN_POINT('Ctrl Pts',(5.98497593003309,15.2,8.90539531874586));
#212002=CARTESIAN_POINT('Ctrl Pts',(5.98813387364629,15.2,8.9080884240939));
#212003=CARTESIAN_POINT('Ctrl Pts',(5.99066022833032,15.2,8.91024290819619));
#212004=CARTESIAN_POINT('Ctrl Pts',(5.99320281850387,15.2,8.91240372497264));
#212005=CARTESIAN_POINT('Ctrl Pts',(5.99576161201585,15.2,8.91457071457287));
#212006=CARTESIAN_POINT('Ctrl Pts',(5.99832040587646,15.2,8.91673770446834));
#212007=CARTESIAN_POINT('Ctrl Pts',(6.00089540309832,15.2,8.9189108695436));
#212008=CARTESIAN_POINT('Ctrl Pts',(6.00348657092596,15.2,8.92109005154954));
#212009=CARTESIAN_POINT('Ctrl Pts',(6.00607773840056,15.2,8.92326923325856));
#212010=CARTESIAN_POINT('Ctrl Pts',(6.00868507520109,15.2,8.92545443323651));
#212011=CARTESIAN_POINT('Ctrl Pts',(6.0113085493189,15.2,8.92764549611256));
#212012=CARTESIAN_POINT('Ctrl Pts',(6.01393202379415,15.2,8.92983655928714));
#212013=CARTESIAN_POINT('Ctrl Pts',(6.01657163575746,15.2,8.93203348492911));
#212014=CARTESIAN_POINT('Ctrl Pts',(6.01922735095881,15.2,8.93423612143842));
#212015=CARTESIAN_POINT('Ctrl Pts',(6.02188306579832,15.2,8.93643875764762));
#212016=CARTESIAN_POINT('Ctrl Pts',(6.02455488531346,15.2,8.93864710454405));
#212017=CARTESIAN_POINT('Ctrl Pts',(6.02724277489327,15.2,8.94086100969541));
#212018=CARTESIAN_POINT('Ctrl Pts',(6.03060263714272,15.2,8.94362839136083));
#212019=CARTESIAN_POINT('Ctrl Pts',(6.03398761037835,15.2,8.94640446026837));
#212020=CARTESIAN_POINT('Ctrl Pts',(6.03739762829368,15.2,8.94918892255957));
#212021=CARTESIAN_POINT('Ctrl Pts',(6.04012564277461,15.2,8.95141649251393));
#212022=CARTESIAN_POINT('Ctrl Pts',(6.04286968619365,15.2,8.95364943538289));
#212023=CARTESIAN_POINT('Ctrl Pts',(6.045629724734,15.2,8.95588760394965));
#212024=CARTESIAN_POINT('Ctrl Pts',(6.04976978216848,15.2,8.95924485649484));
#212025=CARTESIAN_POINT('Ctrl Pts',(6.05394583034862,15.2,8.96261386415592));
#212026=CARTESIAN_POINT('Ctrl Pts',(6.05815775554797,15.2,8.9659941387151));
#212027=CARTESIAN_POINT('Ctrl Pts',(6.06096570593592,15.2,8.96824765529257));
#212028=CARTESIAN_POINT('Ctrl Pts',(6.06378960094112,15.2,8.97050617962673));
#212029=CARTESIAN_POINT('Ctrl Pts',(6.06662940743087,15.2,8.9727695663617));
#212030=CARTESIAN_POINT('Ctrl Pts',(6.07017916534957,15.2,8.97559879962621));
#212031=CARTESIAN_POINT('Ctrl Pts',(6.07375378580201,15.2,8.9784356338825));
#212032=CARTESIAN_POINT('Ctrl Pts',(6.0773532012207,15.2,8.98127978964699));
#212033=CARTESIAN_POINT('Ctrl Pts',(6.08023273332025,15.2,8.98355511407257));
#212034=CARTESIAN_POINT('Ctrl Pts',(6.08312813661161,15.2,8.98583512653592));
#212035=CARTESIAN_POINT('Ctrl Pts',(6.0860393734979,15.2,8.98811968424841));
#212036=CARTESIAN_POINT('Ctrl Pts',(6.08895061078086,15.2,8.99040424227218));
#212037=CARTESIAN_POINT('Ctrl Pts',(6.09187768442181,15.2,8.99269334799673));
#212038=CARTESIAN_POINT('Ctrl Pts',(6.09482055897272,15.2,8.99498686139996));
#212039=CARTESIAN_POINT('Ctrl Pts',(6.09849915196087,15.2,8.99785375299776));
#212040=CARTESIAN_POINT('Ctrl Pts',(6.10220243617994,15.2,9.00072753154841));
#212041=CARTESIAN_POINT('Ctrl Pts',(6.10593034319584,15.2,9.00360793141007));
#212042=CARTESIAN_POINT('Ctrl Pts',(6.1096582498054,15.2,9.00648833095775));
#212043=CARTESIAN_POINT('Ctrl Pts',(6.11341078093621,15.2,9.00937535045964));
#212044=CARTESIAN_POINT('Ctrl Pts',(6.11718786843918,15.2,9.01226872667151));
#212045=CARTESIAN_POINT('Ctrl Pts',(6.12020953893558,15.2,9.01458342801947));
#212046=CARTESIAN_POINT('Ctrl Pts',(6.12324692625293,15.2,9.01690219692061));
#212047=CARTESIAN_POINT('Ctrl Pts',(6.12629999547488,15.2,9.01922490099164));
#212048=CARTESIAN_POINT('Ctrl Pts',(6.13011633179433,15.2,9.0221282809222));
#212049=CARTESIAN_POINT('Ctrl Pts',(6.13395717168436,15.2,9.02503780981607));
#212050=CARTESIAN_POINT('Ctrl Pts',(6.13782245024366,15.2,9.02795322725989));
#212051=CARTESIAN_POINT('Ctrl Pts',(6.14323384031094,15.2,9.03203481174479));
#212052=CARTESIAN_POINT('Ctrl Pts',(6.14869312389253,15.2,9.03612794009108));
#212053=CARTESIAN_POINT('Ctrl Pts',(6.15420012023107,15.2,9.04023191639174));
#212054=CARTESIAN_POINT('Ctrl Pts',(6.15734697497541,15.2,9.04257704547816));
#212055=CARTESIAN_POINT('Ctrl Pts',(6.16050940936771,15.2,9.04492571573077));
#212056=CARTESIAN_POINT('Ctrl Pts',(6.16368738877356,15.2,9.04727780081605));
#212057=CARTESIAN_POINT('Ctrl Pts',(6.16765986335562,15.2,9.050217907413));
#212058=CARTESIAN_POINT('Ctrl Pts',(6.17165662644063,15.2,9.05316334821277));
#212059=CARTESIAN_POINT('Ctrl Pts',(6.17567761180603,15.2,9.0561138750317));
#212060=CARTESIAN_POINT('Ctrl Pts',(6.17889440027367,15.2,9.05847429661549));
#212061=CARTESIAN_POINT('Ctrl Pts',(6.18212669035232,15.2,9.06083797404374));
#212062=CARTESIAN_POINT('Ctrl Pts',(6.1853744475309,15.2,9.06320478089528));
#212063=CARTESIAN_POINT('Ctrl Pts',(6.19024608285629,15.2,9.06675499085012));
#212064=CARTESIAN_POINT('Ctrl Pts',(6.19515251938776,15.2,9.07031224414614));
#212065=CARTESIAN_POINT('Ctrl Pts',(6.20009363979154,15.2,9.07387612201664));
#212066=CARTESIAN_POINT('Ctrl Pts',(6.20421124027763,15.2,9.07684602034995));
#212067=CARTESIAN_POINT('Ctrl Pts',(6.20835292641652,15.2,9.07982051850473));
#212068=CARTESIAN_POINT('Ctrl Pts',(6.21251863101882,15.2,9.08279937851827));
#212069=CARTESIAN_POINT('Ctrl Pts',(6.21585119442823,15.2,9.08518246633427));
#212070=CARTESIAN_POINT('Ctrl Pts',(6.21919913004318,15.2,9.08756834573277));
#212071=CARTESIAN_POINT('Ctrl Pts',(6.22256240143333,15.2,9.08995689509278));
#212072=CARTESIAN_POINT('Ctrl Pts',(6.22592567328172,15.2,9.09234544477823));
#212073=CARTESIAN_POINT('Ctrl Pts',(6.22930428199803,15.2,9.09473666661102));
#212074=CARTESIAN_POINT('Ctrl Pts',(6.23269819251648,15.2,9.0971304382416));
#212075=CARTESIAN_POINT('Ctrl Pts',(6.23694058043335,15.2,9.10012265261674));
#212076=CARTESIAN_POINT('Ctrl Pts',(6.2412068781049,15.2,9.10311885343798));
#212077=CARTESIAN_POINT('Ctrl Pts',(6.24549701527722,15.2,9.10611880782661));
#212078=CARTESIAN_POINT('Ctrl Pts',(6.24892912473451,15.2,9.10851877114132));
#212079=CARTESIAN_POINT('Ctrl Pts',(6.25237649344894,15.2,9.11092113838697));
#212080=CARTESIAN_POINT('Ctrl Pts',(6.25583908344209,15.2,9.11332579085681));
#212081=CARTESIAN_POINT('Ctrl Pts',(6.25930167390702,15.2,9.1157304436543));
#212082=CARTESIAN_POINT('Ctrl Pts',(6.26277948772895,15.2,9.11813738085479));
#212083=CARTESIAN_POINT('Ctrl Pts',(6.26627248897488,15.2,9.12054648904165));
#212084=CARTESIAN_POINT('Ctrl Pts',(6.27063874029432,15.2,9.1235578741111));
#212085=CARTESIAN_POINT('Ctrl Pts',(6.27502872253217,15.2,9.12657264784901));
#212086=CARTESIAN_POINT('Ctrl Pts',(6.27944236630229,15.2,9.12959058800162));
#212087=CARTESIAN_POINT('Ctrl Pts',(6.28297328102973,15.2,9.13200493992634));
#212088=CARTESIAN_POINT('Ctrl Pts',(6.2865193398131,15.2,9.13442131805804));
#212089=CARTESIAN_POINT('Ctrl Pts',(6.2900805059093,15.2,9.13683960863792));
#212090=CARTESIAN_POINT('Ctrl Pts',(6.29364167249071,15.2,9.13925789954729));
#212091=CARTESIAN_POINT('Ctrl Pts',(6.29721794913749,15.2,9.14167810184575));
#212092=CARTESIAN_POINT('Ctrl Pts',(6.30080929699988,15.2,9.14410010419998));
#212093=CARTESIAN_POINT('Ctrl Pts',(6.30529848158322,15.2,9.14712760697777));
#212094=CARTESIAN_POINT('Ctrl Pts',(6.30981121798725,15.2,9.15015792190452));
#212095=CARTESIAN_POINT('Ctrl Pts',(6.31434743599403,15.2,9.1531908312933));
#212096=CARTESIAN_POINT('Ctrl Pts',(6.31797641010277,15.2,9.15561715860597));
#212097=CARTESIAN_POINT('Ctrl Pts',(6.32162041321341,15.2,9.1580451462793));
#212098=CARTESIAN_POINT('Ctrl Pts',(6.32527940913498,15.2,9.16047468363608));
#212099=CARTESIAN_POINT('Ctrl Pts',(6.32893840555508,15.2,9.16290422132388));
#212100=CARTESIAN_POINT('Ctrl Pts',(6.33261239449883,15.2,9.16533530832297));
#212101=CARTESIAN_POINT('Ctrl Pts',(6.33630134103322,15.2,9.16776783723332));
#212102=CARTESIAN_POINT('Ctrl Pts',(6.3399902875676,15.2,9.17020036614366));
#212103=CARTESIAN_POINT('Ctrl Pts',(6.34369419106484,15.2,9.17263433475696));
#212104=CARTESIAN_POINT('Ctrl Pts',(6.34741301682459,15.2,9.17506963638982));
#212105=CARTESIAN_POINT('Ctrl Pts',(6.35113184207766,15.2,9.17750493769088));
#212106=CARTESIAN_POINT('Ctrl Pts',(6.35486558978681,15.2,9.17994157150321));
#212107=CARTESIAN_POINT('Ctrl Pts',(6.35861422249733,15.2,9.18237942898165));
#212108=CARTESIAN_POINT('Ctrl Pts',(6.36142569715791,15.2,9.18420782217352));
#212109=CARTESIAN_POINT('Ctrl Pts',(6.36424554477858,15.2,9.18603690593376));
#212110=CARTESIAN_POINT('Ctrl Pts',(6.36707375092508,15.2,9.18786663261722));
#212111=CARTESIAN_POINT('Ctrl Pts',(6.36990195707159,15.2,9.18969635930068));
#212112=CARTESIAN_POINT('Ctrl Pts',(6.3727385222342,15.2,9.19152673040077));
#212113=CARTESIAN_POINT('Ctrl Pts',(6.3755834298797,15.2,9.19335770058416));
#212114=CARTESIAN_POINT('Ctrl Pts',(6.37937664041824,15.2,9.19579899438376));
#212115=CARTESIAN_POINT('Ctrl Pts',(6.38318468323784,15.2,9.19824135485738));
#212116=CARTESIAN_POINT('Ctrl Pts',(6.38700752301916,15.2,9.20068467400165));
#212117=CARTESIAN_POINT('Ctrl Pts',(6.38987465259472,15.2,9.2025171631934));
#212118=CARTESIAN_POINT('Ctrl Pts',(6.39275010465566,15.2,9.20435019368994));
#212119=CARTESIAN_POINT('Ctrl Pts',(6.3956338647306,15.2,9.20618372029832));
#212120=CARTESIAN_POINT('Ctrl Pts',(6.39851762480555,15.2,9.20801724690669));
#212121=CARTESIAN_POINT('Ctrl Pts',(6.40140969210666,15.2,9.20985126946672));
#212122=CARTESIAN_POINT('Ctrl Pts',(6.40431005270888,15.2,9.2116857450667));
#212123=CARTESIAN_POINT('Ctrl Pts',(6.40914398722156,15.2,9.21474320451106));
#212124=CARTESIAN_POINT('Ctrl Pts',(6.41400095629875,15.2,9.21780192074995));
#212125=CARTESIAN_POINT('Ctrl Pts',(6.41888089067255,15.2,9.22086169429155));
#212126=CARTESIAN_POINT('Ctrl Pts',(6.42180885119044,15.2,9.22269755834981));
#212127=CARTESIAN_POINT('Ctrl Pts',(6.42474507849111,15.2,9.22453380161966));
#212128=CARTESIAN_POINT('Ctrl Pts',(6.42768955869695,15.2,9.22637038335299));
#212129=CARTESIAN_POINT('Ctrl Pts',(6.43063403890278,15.2,9.22820696508631));
#212130=CARTESIAN_POINT('Ctrl Pts',(6.43358677037976,15.2,9.23004388566625));
#212131=CARTESIAN_POINT('Ctrl Pts',(6.43654773856273,15.2,9.23188109939114));
#212132=CARTESIAN_POINT('Ctrl Pts',(6.44148268571366,15.2,9.23494312237719));
#212133=CARTESIAN_POINT('Ctrl Pts',(6.44644051555031,15.2,9.2380059652049));
#212134=CARTESIAN_POINT('Ctrl Pts',(6.45142115263176,15.2,9.24106943131595));
#212135=CARTESIAN_POINT('Ctrl Pts',(6.45440953531495,15.2,9.24290751124971));
#212136=CARTESIAN_POINT('Ctrl Pts',(6.45740612943379,15.2,9.24474581541689));
#212137=CARTESIAN_POINT('Ctrl Pts',(6.46041091966327,15.2,9.24658430189244));
#212138=CARTESIAN_POINT('Ctrl Pts',(6.46441730572614,15.2,9.24903561663653));
#212139=CARTESIAN_POINT('Ctrl Pts',(6.46843826381987,15.2,9.25148725543762));
#212140=CARTESIAN_POINT('Ctrl Pts',(6.47247375573047,15.2,9.25393912024831));
#212141=CARTESIAN_POINT('Ctrl Pts',(6.47550037480087,15.2,9.25577801893985));
#212142=CARTESIAN_POINT('Ctrl Pts',(6.47853516907962,15.2,9.25761704504969));
#212143=CARTESIAN_POINT('Ctrl Pts',(6.48157812367667,15.2,9.25945615627452));
#212144=CARTESIAN_POINT('Ctrl Pts',(6.48462107827373,15.2,9.26129526749935));
#212145=CARTESIAN_POINT('Ctrl Pts',(6.48767219327857,15.2,9.26313446489919));
#212146=CARTESIAN_POINT('Ctrl Pts',(6.49073145383298,15.2,9.26497370608236));
#212147=CARTESIAN_POINT('Ctrl Pts',(6.49379071494315,15.2,9.26681294759966));
#212148=CARTESIAN_POINT('Ctrl Pts',(6.49685812047229,15.2,9.26865223348365));
#212149=CARTESIAN_POINT('Ctrl Pts',(6.49993365567036,15.2,9.27049152391762));
#212150=CARTESIAN_POINT('Ctrl Pts',(6.50300919030972,15.2,9.27233081401745));
#212151=CARTESIAN_POINT('Ctrl Pts',(6.50609285466531,15.2,9.27417010731729));
#212152=CARTESIAN_POINT('Ctrl Pts',(6.50918463326203,15.2,9.2760093639588));
#212153=CARTESIAN_POINT('Ctrl Pts',(6.51433759777712,15.2,9.27907479180602));
#212154=CARTESIAN_POINT('Ctrl Pts',(6.51951310256993,15.2,9.28214011708603));
#212155=CARTESIAN_POINT('Ctrl Pts',(6.52471107484504,15.2,9.28520515432246));
#212156=CARTESIAN_POINT('Ctrl Pts',(6.5278298580968,15.2,9.2870441765975));
#212157=CARTESIAN_POINT('Ctrl Pts',(6.5309567305216,15.2,9.28888309506723));
#212158=CARTESIAN_POINT('Ctrl Pts',(6.53409167561673,15.2,9.29072187020875));
#212159=CARTESIAN_POINT('Ctrl Pts',(6.53827160222041,15.2,9.29317357028608));
#212160=CARTESIAN_POINT('Ctrl Pts',(6.54246588093787,15.2,9.2956250134468));
#212161=CARTESIAN_POINT('Ctrl Pts',(6.54667447553679,15.2,9.29807610885757));
#212162=CARTESIAN_POINT('Ctrl Pts',(6.55088307070914,15.2,9.30052720460229));
#212163=CARTESIAN_POINT('Ctrl Pts',(6.55510598126924,15.2,9.30297795047366));
#212164=CARTESIAN_POINT('Ctrl Pts',(6.55934317051944,15.2,9.30542825428499));
#212165=CARTESIAN_POINT('Ctrl Pts',(6.56358035919234,15.2,9.30787855776247));
#212166=CARTESIAN_POINT('Ctrl Pts',(6.56783182778595,15.2,9.31032841916913));
#212167=CARTESIAN_POINT('Ctrl Pts',(6.57209753776912,15.2,9.31277774535785));
#212168=CARTESIAN_POINT('Ctrl Pts',(6.57636324833349,15.2,9.31522707188029));
#212169=CARTESIAN_POINT('Ctrl Pts',(6.58064320086586,15.2,9.31767586224991));
#212170=CARTESIAN_POINT('Ctrl Pts',(6.58493735876655,15.2,9.32012402804999));
#212171=CARTESIAN_POINT('Ctrl Pts',(6.58815797689953,15.2,9.32196015223327));
#212172=CARTESIAN_POINT('Ctrl Pts',(6.59138658726553,15.2,9.32379592456658));
#212173=CARTESIAN_POINT('Ctrl Pts',(6.5946231714389,15.2,9.32563130679159));
#212174=CARTESIAN_POINT('Ctrl Pts',(6.59785975561227,15.2,9.3274666890166));
#212175=CARTESIAN_POINT('Ctrl Pts',(6.60110431487729,15.2,9.32930168082));
#212176=CARTESIAN_POINT('Ctrl Pts',(6.60435683408735,15.2,9.33113624313671));
#212177=CARTESIAN_POINT('Ctrl Pts',(6.60760935329742,15.2,9.33297080545342));
#212178=CARTESIAN_POINT('Ctrl Pts',(6.61086983042388,15.2,9.33480493775014));
#212179=CARTESIAN_POINT('Ctrl Pts',(6.61413825151238,15.2,9.33663860205858));
#212180=CARTESIAN_POINT('Ctrl Pts',(6.61740667319464,15.2,9.33847226670014));
#212181=CARTESIAN_POINT('Ctrl Pts',(6.62068303892081,15.2,9.34030546433323));
#212182=CARTESIAN_POINT('Ctrl Pts',(6.62396733323254,15.2,9.34213816089119));
#212183=CARTESIAN_POINT('Ctrl Pts',(6.62725162694763,15.2,9.3439708571162));
#212184=CARTESIAN_POINT('Ctrl Pts',(6.6305438517456,15.2,9.34580305239956));
#212185=CARTESIAN_POINT('Ctrl Pts',(6.63384398933474,15.2,9.34763470795797));
#212186=CARTESIAN_POINT('Ctrl Pts',(6.63934421884978,15.2,9.35068746733289));
#212187=CARTESIAN_POINT('Ctrl Pts',(6.64486642765394,15.2,9.3537387206851));
#212188=CARTESIAN_POINT('Ctrl Pts',(6.65041053341855,15.2,9.35678826917066));
#212189=CARTESIAN_POINT('Ctrl Pts',(6.65373699675646,15.2,9.35861799819552));
#212190=CARTESIAN_POINT('Ctrl Pts',(6.65707134275782,15.2,9.36044711540242));
#212191=CARTESIAN_POINT('Ctrl Pts',(6.66041356410864,15.2,9.36227560222762));
#212192=CARTESIAN_POINT('Ctrl Pts',(6.66375578545946,15.2,9.36410408905281));
#212193=CARTESIAN_POINT('Ctrl Pts',(6.6671058818474,15.2,9.36593194382869));
#212194=CARTESIAN_POINT('Ctrl Pts',(6.67046385399994,15.2,9.36775917499999));
#212195=CARTESIAN_POINT('Ctrl Pts',(6.57080831899994,15.2,8.02901631899999));
#212196=CARTESIAN_POINT('Ctrl Pts',(6.57080831899994,11.6,8.02901631899999));
#212197=CARTESIAN_POINT('Ctrl Pts',(6.57090674099994,15.2,8.02916024099999));
#212198=CARTESIAN_POINT('Ctrl Pts',(6.57090674099994,11.6,8.02916024099999));
#212199=CARTESIAN_POINT('Ctrl Pts',(6.57110695099994,15.2,8.02945316199999));
#212200=CARTESIAN_POINT('Ctrl Pts',(6.57110695099994,11.6,8.02945316199999));
#212201=CARTESIAN_POINT('Ctrl Pts',(6.57141009899994,15.2,8.02989715799999));
#212202=CARTESIAN_POINT('Ctrl Pts',(6.57141009899994,11.6,8.02989715799999));
#212203=CARTESIAN_POINT('Ctrl Pts',(6.57181801899994,15.2,8.03049556499998));
#212204=CARTESIAN_POINT('Ctrl Pts',(6.57181801899994,11.6,8.03049556499998));
#212205=CARTESIAN_POINT('Ctrl Pts',(6.57233322399994,15.2,8.03125297399998));
#212206=CARTESIAN_POINT('Ctrl Pts',(6.57233322399994,11.6,8.03125297399998));
#212207=CARTESIAN_POINT('Ctrl Pts',(6.57285600599994,15.2,8.03202318499999));
#212208=CARTESIAN_POINT('Ctrl Pts',(6.57285600599994,11.6,8.03202318499999));
#212209=CARTESIAN_POINT('Ctrl Pts',(6.57338334999994,15.2,8.03280179799999));
#212210=CARTESIAN_POINT('Ctrl Pts',(6.57338334999994,11.6,8.03280179799999));
#212211=CARTESIAN_POINT('Ctrl Pts',(6.57391522699994,15.2,8.03358879999998));
#212212=CARTESIAN_POINT('Ctrl Pts',(6.57391522699994,11.6,8.03358879999998));
#212213=CARTESIAN_POINT('Ctrl Pts',(6.57445160499995,15.2,8.03438417899999));
#212214=CARTESIAN_POINT('Ctrl Pts',(6.57445160499995,11.6,8.03438417899999));
#212215=CARTESIAN_POINT('Ctrl Pts',(6.57499245699994,15.2,8.03518792399998));
#212216=CARTESIAN_POINT('Ctrl Pts',(6.57499245699994,11.6,8.03518792399998));
#212217=CARTESIAN_POINT('Ctrl Pts',(6.57553775199994,15.2,8.03600002099999));
#212218=CARTESIAN_POINT('Ctrl Pts',(6.57553775199994,11.6,8.03600002099999));
#212219=CARTESIAN_POINT('Ctrl Pts',(6.57608745899994,15.2,8.03682046099999));
#212220=CARTESIAN_POINT('Ctrl Pts',(6.57608745899994,11.6,8.03682046099999));
#212221=CARTESIAN_POINT('Ctrl Pts',(6.57664155099994,15.2,8.03764922899998));
#212222=CARTESIAN_POINT('Ctrl Pts',(6.57664155099994,11.6,8.03764922899998));
#212223=CARTESIAN_POINT('Ctrl Pts',(6.57719999699995,15.2,8.03848631499999));
#212224=CARTESIAN_POINT('Ctrl Pts',(6.57719999699995,11.6,8.03848631499999));
#212225=CARTESIAN_POINT('Ctrl Pts',(6.57776276799994,15.2,8.03933170599999));
#212226=CARTESIAN_POINT('Ctrl Pts',(6.57776276799994,11.6,8.03933170599999));
#212227=CARTESIAN_POINT('Ctrl Pts',(6.57832983599994,15.2,8.04018538999999));
#212228=CARTESIAN_POINT('Ctrl Pts',(6.57832983599994,11.6,8.04018538999999));
#212229=CARTESIAN_POINT('Ctrl Pts',(6.57890117199995,15.2,8.04104735799999));
#212230=CARTESIAN_POINT('Ctrl Pts',(6.57890117199995,11.6,8.04104735799999));
#212231=CARTESIAN_POINT('Ctrl Pts',(6.57947674699995,15.2,8.04191759399998));
#212232=CARTESIAN_POINT('Ctrl Pts',(6.57947674699995,11.6,8.04191759399998));
#212233=CARTESIAN_POINT('Ctrl Pts',(6.58005653199995,15.2,8.04279608999998));
#212234=CARTESIAN_POINT('Ctrl Pts',(6.58005653199995,11.6,8.04279608999998));
#212235=CARTESIAN_POINT('Ctrl Pts',(6.58064049899994,15.2,8.04368283299999));
#212236=CARTESIAN_POINT('Ctrl Pts',(6.58064049899994,11.6,8.04368283299999));
#212237=CARTESIAN_POINT('Ctrl Pts',(6.58122861999995,15.2,8.04457781099998));
#212238=CARTESIAN_POINT('Ctrl Pts',(6.58122861999995,11.6,8.04457781099998));
#212239=CARTESIAN_POINT('Ctrl Pts',(6.58182086699994,15.2,8.04548101299999));
#212240=CARTESIAN_POINT('Ctrl Pts',(6.58182086699994,11.6,8.04548101299999));
#212241=CARTESIAN_POINT('Ctrl Pts',(6.58241721199994,15.2,8.04639242699999));
#212242=CARTESIAN_POINT('Ctrl Pts',(6.58241721199994,11.6,8.04639242699999));
#212243=CARTESIAN_POINT('Ctrl Pts',(6.58301762599995,15.2,8.04731204199998));
#212244=CARTESIAN_POINT('Ctrl Pts',(6.58301762599995,11.6,8.04731204199998));
#212245=CARTESIAN_POINT('Ctrl Pts',(6.58362208299994,15.2,8.04823984599999));
#212246=CARTESIAN_POINT('Ctrl Pts',(6.58362208299994,11.6,8.04823984599999));
#212247=CARTESIAN_POINT('Ctrl Pts',(6.58423055399994,15.2,8.04917582899999));
#212248=CARTESIAN_POINT('Ctrl Pts',(6.58423055399994,11.6,8.04917582899999));
#212249=CARTESIAN_POINT('Ctrl Pts',(6.58484301299994,15.2,8.05011997899998));
#212250=CARTESIAN_POINT('Ctrl Pts',(6.58484301299994,11.6,8.05011997899998));
#212251=CARTESIAN_POINT('Ctrl Pts',(6.58545943099995,15.2,8.05107228299999));
#212252=CARTESIAN_POINT('Ctrl Pts',(6.58545943099995,11.6,8.05107228299999));
#212253=CARTESIAN_POINT('Ctrl Pts',(6.58607978199995,15.2,8.05203273199999));
#212254=CARTESIAN_POINT('Ctrl Pts',(6.58607978199995,11.6,8.05203273199999));
#212255=CARTESIAN_POINT('Ctrl Pts',(6.58670403999994,15.2,8.05300131399999));
#212256=CARTESIAN_POINT('Ctrl Pts',(6.58670403999994,11.6,8.05300131399999));
#212257=CARTESIAN_POINT('Ctrl Pts',(6.58733217599995,15.2,8.05397801699998));
#212258=CARTESIAN_POINT('Ctrl Pts',(6.58733217599995,11.6,8.05397801699998));
#212259=CARTESIAN_POINT('Ctrl Pts',(6.58796416399994,15.2,8.05496283099998));
#212260=CARTESIAN_POINT('Ctrl Pts',(6.58796416399994,11.6,8.05496283099998));
#212261=CARTESIAN_POINT('Ctrl Pts',(6.58859997799994,15.2,8.05595574499998));
#212262=CARTESIAN_POINT('Ctrl Pts',(6.58859997799994,11.6,8.05595574499998));
#212263=CARTESIAN_POINT('Ctrl Pts',(6.58923958999994,15.2,8.05695674699999));
#212264=CARTESIAN_POINT('Ctrl Pts',(6.58923958999994,11.6,8.05695674699999));
#212265=CARTESIAN_POINT('Ctrl Pts',(6.58988297499994,15.2,8.05796582699998));
#212266=CARTESIAN_POINT('Ctrl Pts',(6.58988297499994,11.6,8.05796582699998));
#212267=CARTESIAN_POINT('Ctrl Pts',(6.59053010699994,15.2,8.05898297299999));
#212268=CARTESIAN_POINT('Ctrl Pts',(6.59053010699994,11.6,8.05898297299999));
#212269=CARTESIAN_POINT('Ctrl Pts',(6.59118095799994,15.2,8.06000817499999));
#212270=CARTESIAN_POINT('Ctrl Pts',(6.59118095799994,11.6,8.06000817499999));
#212271=CARTESIAN_POINT('Ctrl Pts',(6.59183550399994,15.2,8.06104142099999));
#212272=CARTESIAN_POINT('Ctrl Pts',(6.59183550399994,11.6,8.06104142099999));
#212273=CARTESIAN_POINT('Ctrl Pts',(6.59249371899994,15.2,8.06208270099999));
#212274=CARTESIAN_POINT('Ctrl Pts',(6.59249371899994,11.6,8.06208270099999));
#212275=CARTESIAN_POINT('Ctrl Pts',(6.59315557499994,15.2,8.06313200399998));
#212276=CARTESIAN_POINT('Ctrl Pts',(6.59315557499994,11.6,8.06313200399998));
#212277=CARTESIAN_POINT('Ctrl Pts',(6.59382104899994,15.2,8.06418931799998));
#212278=CARTESIAN_POINT('Ctrl Pts',(6.59382104899994,11.6,8.06418931799998));
#212279=CARTESIAN_POINT('Ctrl Pts',(6.59449011399994,15.2,8.06525463399998));
#212280=CARTESIAN_POINT('Ctrl Pts',(6.59449011399994,11.6,8.06525463399998));
#212281=CARTESIAN_POINT('Ctrl Pts',(6.59516274499994,15.2,8.06632794099999));
#212282=CARTESIAN_POINT('Ctrl Pts',(6.59516274499994,11.6,8.06632794099999));
#212283=CARTESIAN_POINT('Ctrl Pts',(6.59583891699994,15.2,8.06740922799998));
#212284=CARTESIAN_POINT('Ctrl Pts',(6.59583891699994,11.6,8.06740922799998));
#212285=CARTESIAN_POINT('Ctrl Pts',(6.59651860399994,15.2,8.06849848399998));
#212286=CARTESIAN_POINT('Ctrl Pts',(6.59651860399994,11.6,8.06849848399998));
#212287=CARTESIAN_POINT('Ctrl Pts',(6.59720178199994,15.2,8.06959569799999));
#212288=CARTESIAN_POINT('Ctrl Pts',(6.59720178199994,11.6,8.06959569799999));
#212289=CARTESIAN_POINT('Ctrl Pts',(6.59788842499994,15.2,8.07070086099999));
#212290=CARTESIAN_POINT('Ctrl Pts',(6.59788842499994,11.6,8.07070086099999));
#212291=CARTESIAN_POINT('Ctrl Pts',(6.59857850999994,15.2,8.07181396099999));
#212292=CARTESIAN_POINT('Ctrl Pts',(6.59857850999994,11.6,8.07181396099999));
#212293=CARTESIAN_POINT('Ctrl Pts',(6.59927200899994,15.2,8.07293498699998));
#212294=CARTESIAN_POINT('Ctrl Pts',(6.59927200899994,11.6,8.07293498699998));
#212295=CARTESIAN_POINT('Ctrl Pts',(6.59996890099994,15.2,8.07406392999999));
#212296=CARTESIAN_POINT('Ctrl Pts',(6.59996890099994,11.6,8.07406392999999));
#212297=CARTESIAN_POINT('Ctrl Pts',(6.60066915899994,15.2,8.07520077899999));
#212298=CARTESIAN_POINT('Ctrl Pts',(6.60066915899994,11.6,8.07520077899999));
#212299=CARTESIAN_POINT('Ctrl Pts',(6.60137275999994,15.2,8.07634552299999));
#212300=CARTESIAN_POINT('Ctrl Pts',(6.60137275999994,11.6,8.07634552299999));
#212301=CARTESIAN_POINT('Ctrl Pts',(6.60207967899994,15.2,8.07749815299999));
#212302=CARTESIAN_POINT('Ctrl Pts',(6.60207967899994,11.6,8.07749815299999));
#212303=CARTESIAN_POINT('Ctrl Pts',(6.60278989199995,15.2,8.07865865699998));
#212304=CARTESIAN_POINT('Ctrl Pts',(6.60278989199995,11.6,8.07865865699998));
#212305=CARTESIAN_POINT('Ctrl Pts',(6.60350337599994,15.2,8.07982702499999));
#212306=CARTESIAN_POINT('Ctrl Pts',(6.60350337599994,11.6,8.07982702499999));
#212307=CARTESIAN_POINT('Ctrl Pts',(6.60422010499994,15.2,8.08100324799998));
#212308=CARTESIAN_POINT('Ctrl Pts',(6.60422010499994,11.6,8.08100324799998));
#212309=CARTESIAN_POINT('Ctrl Pts',(6.60494005699994,15.2,8.08218731499998));
#212310=CARTESIAN_POINT('Ctrl Pts',(6.60494005699994,11.6,8.08218731499998));
#212311=CARTESIAN_POINT('Ctrl Pts',(6.60566320699994,15.2,8.08337921499999));
#212312=CARTESIAN_POINT('Ctrl Pts',(6.60566320699994,11.6,8.08337921499999));
#212313=CARTESIAN_POINT('Ctrl Pts',(6.60638953399994,15.2,8.08457893799999));
#212314=CARTESIAN_POINT('Ctrl Pts',(6.60638953399994,11.6,8.08457893799999));
#212315=CARTESIAN_POINT('Ctrl Pts',(6.60711900899994,15.2,8.08578647499999));
#212316=CARTESIAN_POINT('Ctrl Pts',(6.60711900899994,11.6,8.08578647499999));
#212317=CARTESIAN_POINT('Ctrl Pts',(6.60785161499994,15.2,8.08700181499999));
#212318=CARTESIAN_POINT('Ctrl Pts',(6.60785161499994,11.6,8.08700181499999));
#212319=CARTESIAN_POINT('Ctrl Pts',(6.60858732499994,15.2,8.08822494799998));
#212320=CARTESIAN_POINT('Ctrl Pts',(6.60858732499994,11.6,8.08822494799998));
#212321=CARTESIAN_POINT('Ctrl Pts',(6.60932611599995,15.2,8.08945586299998));
#212322=CARTESIAN_POINT('Ctrl Pts',(6.60932611599995,11.6,8.08945586299998));
#212323=CARTESIAN_POINT('Ctrl Pts',(6.61006796499994,15.2,8.09069455199998));
#212324=CARTESIAN_POINT('Ctrl Pts',(6.61006796499994,11.6,8.09069455199998));
#212325=CARTESIAN_POINT('Ctrl Pts',(6.61081285099994,15.2,8.09194100299998));
#212326=CARTESIAN_POINT('Ctrl Pts',(6.61081285099994,11.6,8.09194100299998));
#212327=CARTESIAN_POINT('Ctrl Pts',(6.61156074799995,15.2,8.09319520799999));
#212328=CARTESIAN_POINT('Ctrl Pts',(6.61156074799995,11.6,8.09319520799999));
#212329=CARTESIAN_POINT('Ctrl Pts',(6.61231163599994,15.2,8.09445715399999));
#212330=CARTESIAN_POINT('Ctrl Pts',(6.61231163599994,11.6,8.09445715399999));
#212331=CARTESIAN_POINT('Ctrl Pts',(6.61306548999994,15.2,8.09572683299999));
#212332=CARTESIAN_POINT('Ctrl Pts',(6.61306548999994,11.6,8.09572683299999));
#212333=CARTESIAN_POINT('Ctrl Pts',(6.61382228899994,15.2,8.09700423699999));
#212334=CARTESIAN_POINT('Ctrl Pts',(6.61382228899994,11.6,8.09700423699999));
#212335=CARTESIAN_POINT('Ctrl Pts',(6.61458201099994,15.2,8.09828935199998));
#212336=CARTESIAN_POINT('Ctrl Pts',(6.61458201099994,11.6,8.09828935199998));
#212337=CARTESIAN_POINT('Ctrl Pts',(6.61534463099994,15.2,8.09958217099998));
#212338=CARTESIAN_POINT('Ctrl Pts',(6.61534463099994,11.6,8.09958217099998));
#212339=CARTESIAN_POINT('Ctrl Pts',(6.61611012899994,15.2,8.10088268299998));
#212340=CARTESIAN_POINT('Ctrl Pts',(6.61611012899994,11.6,8.10088268299998));
#212341=CARTESIAN_POINT('Ctrl Pts',(6.61687848099994,15.2,8.10219087899998));
#212342=CARTESIAN_POINT('Ctrl Pts',(6.61687848099994,11.6,8.10219087899998));
#212343=CARTESIAN_POINT('Ctrl Pts',(6.61764966699994,15.2,8.10350674899999));
#212344=CARTESIAN_POINT('Ctrl Pts',(6.61764966699994,11.6,8.10350674899999));
#212345=CARTESIAN_POINT('Ctrl Pts',(6.61842366399994,15.2,8.10483028299998));
#212346=CARTESIAN_POINT('Ctrl Pts',(6.61842366399994,11.6,8.10483028299998));
#212347=CARTESIAN_POINT('Ctrl Pts',(6.61920044999994,15.2,8.10616147099999));
#212348=CARTESIAN_POINT('Ctrl Pts',(6.61920044999994,11.6,8.10616147099999));
#212349=CARTESIAN_POINT('Ctrl Pts',(6.61998000099994,15.2,8.10750030399999));
#212350=CARTESIAN_POINT('Ctrl Pts',(6.61998000099994,11.6,8.10750030399999));
#212351=CARTESIAN_POINT('Ctrl Pts',(6.62076229999994,15.2,8.10884677099999));
#212352=CARTESIAN_POINT('Ctrl Pts',(6.62076229999994,11.6,8.10884677099999));
#212353=CARTESIAN_POINT('Ctrl Pts',(6.62154732099994,15.2,8.11020086499998));
#212354=CARTESIAN_POINT('Ctrl Pts',(6.62154732099994,11.6,8.11020086499998));
#212355=CARTESIAN_POINT('Ctrl Pts',(6.62233504499994,15.2,8.11156257399999));
#212356=CARTESIAN_POINT('Ctrl Pts',(6.62233504499994,11.6,8.11156257399999));
#212357=CARTESIAN_POINT('Ctrl Pts',(6.62312544999994,15.2,8.11293188899998));
#212358=CARTESIAN_POINT('Ctrl Pts',(6.62312544999994,11.6,8.11293188899998));
#212359=CARTESIAN_POINT('Ctrl Pts',(6.62391851399994,15.2,8.11430880099999));
#212360=CARTESIAN_POINT('Ctrl Pts',(6.62391851399994,11.6,8.11430880099999));
#212361=CARTESIAN_POINT('Ctrl Pts',(6.62471421499994,15.2,8.11569329899999));
#212362=CARTESIAN_POINT('Ctrl Pts',(6.62471421499994,11.6,8.11569329899999));
#212363=CARTESIAN_POINT('Ctrl Pts',(6.62551253299994,15.2,8.11708537599999));
#212364=CARTESIAN_POINT('Ctrl Pts',(6.62551253299994,11.6,8.11708537599999));
#212365=CARTESIAN_POINT('Ctrl Pts',(6.62631344799994,15.2,8.11848501999999));
#212366=CARTESIAN_POINT('Ctrl Pts',(6.62631344799994,11.6,8.11848501999999));
#212367=CARTESIAN_POINT('Ctrl Pts',(6.62711693599995,15.2,8.11989222299999));
#212368=CARTESIAN_POINT('Ctrl Pts',(6.62711693599995,11.6,8.11989222299999));
#212369=CARTESIAN_POINT('Ctrl Pts',(6.62792297799994,15.2,8.12130697599999));
#212370=CARTESIAN_POINT('Ctrl Pts',(6.62792297799994,11.6,8.12130697599999));
#212371=CARTESIAN_POINT('Ctrl Pts',(6.62873155399994,15.2,8.12272926799999));
#212372=CARTESIAN_POINT('Ctrl Pts',(6.62873155399994,11.6,8.12272926799999));
#212373=CARTESIAN_POINT('Ctrl Pts',(6.62954264199994,15.2,8.12415908999998));
#212374=CARTESIAN_POINT('Ctrl Pts',(6.62954264199994,11.6,8.12415908999998));
#212375=CARTESIAN_POINT('Ctrl Pts',(6.63035622099994,15.2,8.12559643399998));
#212376=CARTESIAN_POINT('Ctrl Pts',(6.63035622099994,11.6,8.12559643399998));
#212377=CARTESIAN_POINT('Ctrl Pts',(6.63117226999994,15.2,8.12704128899998));
#212378=CARTESIAN_POINT('Ctrl Pts',(6.63117226999994,11.6,8.12704128899998));
#212379=CARTESIAN_POINT('Ctrl Pts',(6.63199076999994,15.2,8.12849364699998));
#212380=CARTESIAN_POINT('Ctrl Pts',(6.63199076999994,11.6,8.12849364699998));
#212381=CARTESIAN_POINT('Ctrl Pts',(6.63281169999994,15.2,8.12995349699998));
#212382=CARTESIAN_POINT('Ctrl Pts',(6.63281169999994,11.6,8.12995349699998));
#212383=CARTESIAN_POINT('Ctrl Pts',(6.63363503799994,15.2,8.13142083199999));
#212384=CARTESIAN_POINT('Ctrl Pts',(6.63363503799994,11.6,8.13142083199999));
#212385=CARTESIAN_POINT('Ctrl Pts',(6.63446076799994,15.2,8.13289564099998));
#212386=CARTESIAN_POINT('Ctrl Pts',(6.63446076799994,11.6,8.13289564099998));
#212387=CARTESIAN_POINT('Ctrl Pts',(6.63528886399994,15.2,8.13437791499998));
#212388=CARTESIAN_POINT('Ctrl Pts',(6.63528886399994,11.6,8.13437791499998));
#212389=CARTESIAN_POINT('Ctrl Pts',(6.63611931099994,15.2,8.13586764599999));
#212390=CARTESIAN_POINT('Ctrl Pts',(6.63611931099994,11.6,8.13586764599999));
#212391=CARTESIAN_POINT('Ctrl Pts',(6.63695208599994,15.2,8.13736482299999));
#212392=CARTESIAN_POINT('Ctrl Pts',(6.63695208599994,11.6,8.13736482299999));
#212393=CARTESIAN_POINT('Ctrl Pts',(6.63778716999994,15.2,8.13886943899998));
#212394=CARTESIAN_POINT('Ctrl Pts',(6.63778716999994,11.6,8.13886943899998));
#212395=CARTESIAN_POINT('Ctrl Pts',(6.63862454399994,15.2,8.14038148399998));
#212396=CARTESIAN_POINT('Ctrl Pts',(6.63862454399994,11.6,8.14038148399998));
#212397=CARTESIAN_POINT('Ctrl Pts',(6.63946418699994,15.2,8.14190094699999));
#212398=CARTESIAN_POINT('Ctrl Pts',(6.63946418699994,11.6,8.14190094699999));
#212399=CARTESIAN_POINT('Ctrl Pts',(6.64030607799994,15.2,8.14342782199999));
#212400=CARTESIAN_POINT('Ctrl Pts',(6.64030607799994,11.6,8.14342782199999));
#212401=CARTESIAN_POINT('Ctrl Pts',(6.64115019999994,15.2,8.14496209799999));
#212402=CARTESIAN_POINT('Ctrl Pts',(6.64115019999994,11.6,8.14496209799999));
#212403=CARTESIAN_POINT('Ctrl Pts',(6.64199653299994,15.2,8.14650376599998));
#212404=CARTESIAN_POINT('Ctrl Pts',(6.64199653299994,11.6,8.14650376599998));
#212405=CARTESIAN_POINT('Ctrl Pts',(6.64284505599994,15.2,8.14805281799998));
#212406=CARTESIAN_POINT('Ctrl Pts',(6.64284505599994,11.6,8.14805281799998));
#212407=CARTESIAN_POINT('Ctrl Pts',(6.64369575099995,15.2,8.14960924399998));
#212408=CARTESIAN_POINT('Ctrl Pts',(6.64369575099995,11.6,8.14960924399998));
#212409=CARTESIAN_POINT('Ctrl Pts',(6.64454859899994,15.2,8.15117303499999));
#212410=CARTESIAN_POINT('Ctrl Pts',(6.64454859899994,11.6,8.15117303499999));
#212411=CARTESIAN_POINT('Ctrl Pts',(6.64540357999994,15.2,8.15274418299998));
#212412=CARTESIAN_POINT('Ctrl Pts',(6.64540357999994,11.6,8.15274418299998));
#212413=CARTESIAN_POINT('Ctrl Pts',(6.64626067299994,15.2,8.15432267999999));
#212414=CARTESIAN_POINT('Ctrl Pts',(6.64626067299994,11.6,8.15432267999999));
#212415=CARTESIAN_POINT('Ctrl Pts',(6.64711986199994,15.2,8.15590851399998));
#212416=CARTESIAN_POINT('Ctrl Pts',(6.64711986199994,11.6,8.15590851399998));
#212417=CARTESIAN_POINT('Ctrl Pts',(6.64798112699994,15.2,8.15750167699999));
#212418=CARTESIAN_POINT('Ctrl Pts',(6.64798112699994,11.6,8.15750167699999));
#212419=CARTESIAN_POINT('Ctrl Pts',(6.64884444799994,15.2,8.15910216299999));
#212420=CARTESIAN_POINT('Ctrl Pts',(6.64884444799994,11.6,8.15910216299999));
#212421=CARTESIAN_POINT('Ctrl Pts',(6.64970980799994,15.2,8.16070995999999));
#212422=CARTESIAN_POINT('Ctrl Pts',(6.64970980799994,11.6,8.16070995999999));
#212423=CARTESIAN_POINT('Ctrl Pts',(6.65057718599994,15.2,8.16232506099999));
#212424=CARTESIAN_POINT('Ctrl Pts',(6.65057718599994,11.6,8.16232506099999));
#212425=CARTESIAN_POINT('Ctrl Pts',(6.65144656499994,15.2,8.16394745499998));
#212426=CARTESIAN_POINT('Ctrl Pts',(6.65144656499994,11.6,8.16394745499998));
#212427=CARTESIAN_POINT('Ctrl Pts',(6.65231792499994,15.2,8.16557713599998));
#212428=CARTESIAN_POINT('Ctrl Pts',(6.65231792499994,11.6,8.16557713599998));
#212429=CARTESIAN_POINT('Ctrl Pts',(6.65319124899994,15.2,8.16721409299999));
#212430=CARTESIAN_POINT('Ctrl Pts',(6.65319124899994,11.6,8.16721409299999));
#212431=CARTESIAN_POINT('Ctrl Pts',(6.65406651699994,15.2,8.16885831899998));
#212432=CARTESIAN_POINT('Ctrl Pts',(6.65406651699994,11.6,8.16885831899998));
#212433=CARTESIAN_POINT('Ctrl Pts',(6.65494371099994,15.2,8.17050980299998));
#212434=CARTESIAN_POINT('Ctrl Pts',(6.65494371099994,11.6,8.17050980299998));
#212435=CARTESIAN_POINT('Ctrl Pts',(6.65582281299994,15.2,8.17216853899998));
#212436=CARTESIAN_POINT('Ctrl Pts',(6.65582281299994,11.6,8.17216853899998));
#212437=CARTESIAN_POINT('Ctrl Pts',(6.65670380499994,15.2,8.17383451699998));
#212438=CARTESIAN_POINT('Ctrl Pts',(6.65670380499994,11.6,8.17383451699998));
#212439=CARTESIAN_POINT('Ctrl Pts',(6.65758666799994,15.2,8.17550772799999));
#212440=CARTESIAN_POINT('Ctrl Pts',(6.65758666799994,11.6,8.17550772799999));
#212441=CARTESIAN_POINT('Ctrl Pts',(6.65847138399994,15.2,8.17718816299998));
#212442=CARTESIAN_POINT('Ctrl Pts',(6.65847138399994,11.6,8.17718816299998));
#212443=CARTESIAN_POINT('Ctrl Pts',(6.65935793499994,15.2,8.17887581499999));
#212444=CARTESIAN_POINT('Ctrl Pts',(6.65935793499994,11.6,8.17887581499999));
#212445=CARTESIAN_POINT('Ctrl Pts',(6.66024630299995,15.2,8.18057067299998));
#212446=CARTESIAN_POINT('Ctrl Pts',(6.66024630299995,11.6,8.18057067299998));
#212447=CARTESIAN_POINT('Ctrl Pts',(6.66113646899994,15.2,8.18227273199999));
#212448=CARTESIAN_POINT('Ctrl Pts',(6.66113646899994,11.6,8.18227273199999));
#212449=CARTESIAN_POINT('Ctrl Pts',(6.66202841699994,15.2,8.18398197899998));
#212450=CARTESIAN_POINT('Ctrl Pts',(6.66202841699994,11.6,8.18398197899998));
#212451=CARTESIAN_POINT('Ctrl Pts',(6.66292212899994,15.2,8.18569840899999));
#212452=CARTESIAN_POINT('Ctrl Pts',(6.66292212899994,11.6,8.18569840899999));
#212453=CARTESIAN_POINT('Ctrl Pts',(6.66381758599995,15.2,8.18742201199999));
#212454=CARTESIAN_POINT('Ctrl Pts',(6.66381758599995,11.6,8.18742201199999));
#212455=CARTESIAN_POINT('Ctrl Pts',(6.66471477099994,15.2,8.18915277999999));
#212456=CARTESIAN_POINT('Ctrl Pts',(6.66471477099994,11.6,8.18915277999999));
#212457=CARTESIAN_POINT('Ctrl Pts',(6.66561366699994,15.2,8.19089070399999));
#212458=CARTESIAN_POINT('Ctrl Pts',(6.66561366699994,11.6,8.19089070399999));
#212459=CARTESIAN_POINT('Ctrl Pts',(6.66651425399994,15.2,8.19263577599998));
#212460=CARTESIAN_POINT('Ctrl Pts',(6.66651425399994,11.6,8.19263577599998));
#212461=CARTESIAN_POINT('Ctrl Pts',(6.66741651699994,15.2,8.19438798599998));
#212462=CARTESIAN_POINT('Ctrl Pts',(6.66741651699994,11.6,8.19438798599998));
#212463=CARTESIAN_POINT('Ctrl Pts',(6.66832043699995,15.2,8.19614732799998));
#212464=CARTESIAN_POINT('Ctrl Pts',(6.66832043699995,11.6,8.19614732799998));
#212465=CARTESIAN_POINT('Ctrl Pts',(6.66922599799994,15.2,8.19791379099998));
#212466=CARTESIAN_POINT('Ctrl Pts',(6.66922599799994,11.6,8.19791379099998));
#212467=CARTESIAN_POINT('Ctrl Pts',(6.67013318299994,15.2,8.19968736899998));
#212468=CARTESIAN_POINT('Ctrl Pts',(6.67013318299994,11.6,8.19968736899998));
#212469=CARTESIAN_POINT('Ctrl Pts',(6.67104197299994,15.2,8.20146805199998));
#212470=CARTESIAN_POINT('Ctrl Pts',(6.67104197299994,11.6,8.20146805199998));
#212471=CARTESIAN_POINT('Ctrl Pts',(6.67195235199994,15.2,8.20325583299999));
#212472=CARTESIAN_POINT('Ctrl Pts',(6.67195235199994,11.6,8.20325583299999));
#212473=CARTESIAN_POINT('Ctrl Pts',(6.67286430199994,15.2,8.20505070199999));
#212474=CARTESIAN_POINT('Ctrl Pts',(6.67286430199994,11.6,8.20505070199999));
#212475=CARTESIAN_POINT('Ctrl Pts',(6.67377780699994,15.2,8.20685265099998));
#212476=CARTESIAN_POINT('Ctrl Pts',(6.67377780699994,11.6,8.20685265099998));
#212477=CARTESIAN_POINT('Ctrl Pts',(6.67469284899994,15.2,8.20866167399998));
#212478=CARTESIAN_POINT('Ctrl Pts',(6.67469284899994,11.6,8.20866167399998));
#212479=CARTESIAN_POINT('Ctrl Pts',(6.67560941099994,15.2,8.21047775899999));
#212480=CARTESIAN_POINT('Ctrl Pts',(6.67560941099994,11.6,8.21047775899999));
#212481=CARTESIAN_POINT('Ctrl Pts',(6.67652747899995,15.2,8.21230089999998));
#212482=CARTESIAN_POINT('Ctrl Pts',(6.67652747899995,11.6,8.21230089999998));
#212483=CARTESIAN_POINT('Ctrl Pts',(6.67744703199994,15.2,8.21413108799998));
#212484=CARTESIAN_POINT('Ctrl Pts',(6.67744703199994,11.6,8.21413108799998));
#212485=CARTESIAN_POINT('Ctrl Pts',(6.67836805499994,15.2,8.21596831599999));
#212486=CARTESIAN_POINT('Ctrl Pts',(6.67836805499994,11.6,8.21596831599999));
#212487=CARTESIAN_POINT('Ctrl Pts',(6.67929053299994,15.2,8.21781257299998));
#212488=CARTESIAN_POINT('Ctrl Pts',(6.67929053299994,11.6,8.21781257299998));
#212489=CARTESIAN_POINT('Ctrl Pts',(6.68021444599994,15.2,8.21966385399998));
#212490=CARTESIAN_POINT('Ctrl Pts',(6.68021444599994,11.6,8.21966385399998));
#212491=CARTESIAN_POINT('Ctrl Pts',(6.68113978099995,15.2,8.22152214899998));
#212492=CARTESIAN_POINT('Ctrl Pts',(6.68113978099995,11.6,8.22152214899998));
#212493=CARTESIAN_POINT('Ctrl Pts',(6.68206651899995,15.2,8.22338744899999));
#212494=CARTESIAN_POINT('Ctrl Pts',(6.68206651899995,11.6,8.22338744899999));
#212495=CARTESIAN_POINT('Ctrl Pts',(6.68299464399994,15.2,8.22525974799999));
#212496=CARTESIAN_POINT('Ctrl Pts',(6.68299464399994,11.6,8.22525974799999));
#212497=CARTESIAN_POINT('Ctrl Pts',(6.68392413999994,15.2,8.22713903699999));
#212498=CARTESIAN_POINT('Ctrl Pts',(6.68392413999994,11.6,8.22713903699999));
#212499=CARTESIAN_POINT('Ctrl Pts',(6.68485499199994,15.2,8.22902530699999));
#212500=CARTESIAN_POINT('Ctrl Pts',(6.68485499199994,11.6,8.22902530699999));
#212501=CARTESIAN_POINT('Ctrl Pts',(6.68578717999995,15.2,8.23091854999999));
#212502=CARTESIAN_POINT('Ctrl Pts',(6.68578717999995,11.6,8.23091854999999));
#212503=CARTESIAN_POINT('Ctrl Pts',(6.68672069299994,15.2,8.23281875899998));
#212504=CARTESIAN_POINT('Ctrl Pts',(6.68672069299994,11.6,8.23281875899998));
#212505=CARTESIAN_POINT('Ctrl Pts',(6.68765550999994,15.2,8.23472592499999));
#212506=CARTESIAN_POINT('Ctrl Pts',(6.68765550999994,11.6,8.23472592499999));
#212507=CARTESIAN_POINT('Ctrl Pts',(6.68859161699995,15.2,8.23664004199999));
#212508=CARTESIAN_POINT('Ctrl Pts',(6.68859161699995,11.6,8.23664004199999));
#212509=CARTESIAN_POINT('Ctrl Pts',(6.68952899899995,15.2,8.23856109799999));
#212510=CARTESIAN_POINT('Ctrl Pts',(6.68952899899995,11.6,8.23856109799999));
#212511=CARTESIAN_POINT('Ctrl Pts',(6.69046763699994,15.2,8.24048908699999));
#212512=CARTESIAN_POINT('Ctrl Pts',(6.69046763699994,11.6,8.24048908699999));
#212513=CARTESIAN_POINT('Ctrl Pts',(6.69140751799994,15.2,8.24242400199999));
#212514=CARTESIAN_POINT('Ctrl Pts',(6.69140751799994,11.6,8.24242400199999));
#212515=CARTESIAN_POINT('Ctrl Pts',(6.69234862499994,15.2,8.24436583299999));
#212516=CARTESIAN_POINT('Ctrl Pts',(6.69234862499994,11.6,8.24436583299999));
#212517=CARTESIAN_POINT('Ctrl Pts',(6.69329094199994,15.2,8.24631457399999));
#212518=CARTESIAN_POINT('Ctrl Pts',(6.69329094199994,11.6,8.24631457399999));
#212519=CARTESIAN_POINT('Ctrl Pts',(6.69423445299994,15.2,8.24827021499999));
#212520=CARTESIAN_POINT('Ctrl Pts',(6.69423445299994,11.6,8.24827021499999));
#212521=CARTESIAN_POINT('Ctrl Pts',(6.69517914399994,15.2,8.25023274999998));
#212522=CARTESIAN_POINT('Ctrl Pts',(6.69517914399994,11.6,8.25023274999998));
#212523=CARTESIAN_POINT('Ctrl Pts',(6.69612499799995,15.2,8.25220216899999));
#212524=CARTESIAN_POINT('Ctrl Pts',(6.69612499799995,11.6,8.25220216899999));
#212525=CARTESIAN_POINT('Ctrl Pts',(6.69707199899994,15.2,8.25417846599999));
#212526=CARTESIAN_POINT('Ctrl Pts',(6.69707199899994,11.6,8.25417846599999));
#212527=CARTESIAN_POINT('Ctrl Pts',(6.69802013099994,15.2,8.25616163199999));
#212528=CARTESIAN_POINT('Ctrl Pts',(6.69802013099994,11.6,8.25616163199999));
#212529=CARTESIAN_POINT('Ctrl Pts',(6.69896938099994,15.2,8.25815165899999));
#212530=CARTESIAN_POINT('Ctrl Pts',(6.69896938099994,11.6,8.25815165899999));
#212531=CARTESIAN_POINT('Ctrl Pts',(6.69991973099994,15.2,8.26014853899999));
#212532=CARTESIAN_POINT('Ctrl Pts',(6.69991973099994,11.6,8.26014853899999));
#212533=CARTESIAN_POINT('Ctrl Pts',(6.70087116699994,15.2,8.26215226499999));
#212534=CARTESIAN_POINT('Ctrl Pts',(6.70087116699994,11.6,8.26215226499999));
#212535=CARTESIAN_POINT('Ctrl Pts',(6.70182367299994,15.2,8.26416282799999));
#212536=CARTESIAN_POINT('Ctrl Pts',(6.70182367299994,11.6,8.26416282799999));
#212537=CARTESIAN_POINT('Ctrl Pts',(6.70277723299994,15.2,8.26618022199998));
#212538=CARTESIAN_POINT('Ctrl Pts',(6.70277723299994,11.6,8.26618022199998));
#212539=CARTESIAN_POINT('Ctrl Pts',(6.70373183299994,15.2,8.26820443599999));
#212540=CARTESIAN_POINT('Ctrl Pts',(6.70373183299994,11.6,8.26820443599999));
#212541=CARTESIAN_POINT('Ctrl Pts',(6.70468745899995,15.2,8.27023546499999));
#212542=CARTESIAN_POINT('Ctrl Pts',(6.70468745899995,11.6,8.27023546499999));
#212543=CARTESIAN_POINT('Ctrl Pts',(6.70564409299995,15.2,8.27227329999998));
#212544=CARTESIAN_POINT('Ctrl Pts',(6.70564409299995,11.6,8.27227329999998));
#212545=CARTESIAN_POINT('Ctrl Pts',(6.70660172299994,15.2,8.27431793299999));
#212546=CARTESIAN_POINT('Ctrl Pts',(6.70660172299994,11.6,8.27431793299999));
#212547=CARTESIAN_POINT('Ctrl Pts',(6.70756033099994,15.2,8.27636935799998));
#212548=CARTESIAN_POINT('Ctrl Pts',(6.70756033099994,11.6,8.27636935799998));
#212549=CARTESIAN_POINT('Ctrl Pts',(6.70851990399994,15.2,8.27842756399999));
#212550=CARTESIAN_POINT('Ctrl Pts',(6.70851990399994,11.6,8.27842756399999));
#212551=CARTESIAN_POINT('Ctrl Pts',(6.70948042599994,15.2,8.28049254499999));
#212552=CARTESIAN_POINT('Ctrl Pts',(6.70948042599994,11.6,8.28049254499999));
#212553=CARTESIAN_POINT('Ctrl Pts',(6.71044188299994,15.2,8.28256429499999));
#212554=CARTESIAN_POINT('Ctrl Pts',(6.71044188299994,11.6,8.28256429499999));
#212555=CARTESIAN_POINT('Ctrl Pts',(6.71140425899994,15.2,8.28464280299999));
#212556=CARTESIAN_POINT('Ctrl Pts',(6.71140425899994,11.6,8.28464280299999));
#212557=CARTESIAN_POINT('Ctrl Pts',(6.71236754099994,15.2,8.28672806399998));
#212558=CARTESIAN_POINT('Ctrl Pts',(6.71236754099994,11.6,8.28672806399998));
#212559=CARTESIAN_POINT('Ctrl Pts',(6.71333171199994,15.2,8.28882006799999));
#212560=CARTESIAN_POINT('Ctrl Pts',(6.71333171199994,11.6,8.28882006799999));
#212561=CARTESIAN_POINT('Ctrl Pts',(6.71429675799994,15.2,8.29091880899998));
#212562=CARTESIAN_POINT('Ctrl Pts',(6.71429675799994,11.6,8.29091880899998));
#212563=CARTESIAN_POINT('Ctrl Pts',(6.71526266699995,15.2,8.29302427799998));
#212564=CARTESIAN_POINT('Ctrl Pts',(6.71526266699995,11.6,8.29302427799998));
#212565=CARTESIAN_POINT('Ctrl Pts',(6.71622941999994,15.2,8.29513646899999));
#212566=CARTESIAN_POINT('Ctrl Pts',(6.71622941999994,11.6,8.29513646899999));
#212567=CARTESIAN_POINT('Ctrl Pts',(6.71719700699994,15.2,8.29725537299998));
#212568=CARTESIAN_POINT('Ctrl Pts',(6.71719700699994,11.6,8.29725537299998));
#212569=CARTESIAN_POINT('Ctrl Pts',(6.71816540999994,15.2,8.29938098199998));
#212570=CARTESIAN_POINT('Ctrl Pts',(6.71816540999994,11.6,8.29938098199998));
#212571=CARTESIAN_POINT('Ctrl Pts',(6.71913461599994,15.2,8.30151328999998));
#212572=CARTESIAN_POINT('Ctrl Pts',(6.71913461599994,11.6,8.30151328999998));
#212573=CARTESIAN_POINT('Ctrl Pts',(6.72010461099994,15.2,8.30365228699998));
#212574=CARTESIAN_POINT('Ctrl Pts',(6.72010461099994,11.6,8.30365228699998));
#212575=CARTESIAN_POINT('Ctrl Pts',(6.72107537999994,15.2,8.30579796799999));
#212576=CARTESIAN_POINT('Ctrl Pts',(6.72107537999994,11.6,8.30579796799999));
#212577=CARTESIAN_POINT('Ctrl Pts',(6.72204690799994,15.2,8.30795032399998));
#212578=CARTESIAN_POINT('Ctrl Pts',(6.72204690799994,11.6,8.30795032399998));
#212579=CARTESIAN_POINT('Ctrl Pts',(6.72301918199994,15.2,8.31010934699999));
#212580=CARTESIAN_POINT('Ctrl Pts',(6.72301918199994,11.6,8.31010934699999));
#212581=CARTESIAN_POINT('Ctrl Pts',(6.72399218799994,15.2,8.31227503099999));
#212582=CARTESIAN_POINT('Ctrl Pts',(6.72399218799994,11.6,8.31227503099999));
#212583=CARTESIAN_POINT('Ctrl Pts',(6.72496590999994,15.2,8.31444736699999));
#212584=CARTESIAN_POINT('Ctrl Pts',(6.72496590999994,11.6,8.31444736699999));
#212585=CARTESIAN_POINT('Ctrl Pts',(6.72594033699994,15.2,8.31662634799999));
#212586=CARTESIAN_POINT('Ctrl Pts',(6.72594033699994,11.6,8.31662634799999));
#212587=CARTESIAN_POINT('Ctrl Pts',(6.72691545099994,15.2,8.31881196599999));
#212588=CARTESIAN_POINT('Ctrl Pts',(6.72691545099994,11.6,8.31881196599999));
#212589=CARTESIAN_POINT('Ctrl Pts',(6.72789124099994,15.2,8.32100421499998));
#212590=CARTESIAN_POINT('Ctrl Pts',(6.72789124099994,11.6,8.32100421499998));
#212591=CARTESIAN_POINT('Ctrl Pts',(6.72886769299994,15.2,8.32320308499998));
#212592=CARTESIAN_POINT('Ctrl Pts',(6.72886769299994,11.6,8.32320308499998));
#212593=CARTESIAN_POINT('Ctrl Pts',(6.72984478999994,15.2,8.32540856999999));
#212594=CARTESIAN_POINT('Ctrl Pts',(6.72984478999994,11.6,8.32540856999999));
#212595=CARTESIAN_POINT('Ctrl Pts',(6.73082252199994,15.2,8.32762066199999));
#212596=CARTESIAN_POINT('Ctrl Pts',(6.73082252199994,11.6,8.32762066199999));
#212597=CARTESIAN_POINT('Ctrl Pts',(6.73180087299994,15.2,8.32983935599999));
#212598=CARTESIAN_POINT('Ctrl Pts',(6.73180087299994,11.6,8.32983935599999));
#212599=CARTESIAN_POINT('Ctrl Pts',(6.73277982899994,15.2,8.33206463999998));
#212600=CARTESIAN_POINT('Ctrl Pts',(6.73277982899994,11.6,8.33206463999998));
#212601=CARTESIAN_POINT('Ctrl Pts',(6.73375937699995,15.2,8.33429650999998));
#212602=CARTESIAN_POINT('Ctrl Pts',(6.73375937699995,11.6,8.33429650999998));
#212603=CARTESIAN_POINT('Ctrl Pts',(6.73473950299995,15.2,8.33653495699998));
#212604=CARTESIAN_POINT('Ctrl Pts',(6.73473950299995,11.6,8.33653495699998));
#212605=CARTESIAN_POINT('Ctrl Pts',(6.73572019399994,15.2,8.33877997399998));
#212606=CARTESIAN_POINT('Ctrl Pts',(6.73572019399994,11.6,8.33877997399998));
#212607=CARTESIAN_POINT('Ctrl Pts',(6.73670143599994,15.2,8.34103155399998));
#212608=CARTESIAN_POINT('Ctrl Pts',(6.73670143599994,11.6,8.34103155399998));
#212609=CARTESIAN_POINT('Ctrl Pts',(6.73768321599994,15.2,8.34328968899998));
#212610=CARTESIAN_POINT('Ctrl Pts',(6.73768321599994,11.6,8.34328968899998));
#212611=CARTESIAN_POINT('Ctrl Pts',(6.73866551799994,15.2,8.34555437199998));
#212612=CARTESIAN_POINT('Ctrl Pts',(6.73866551799994,11.6,8.34555437199998));
#212613=CARTESIAN_POINT('Ctrl Pts',(6.73964833099994,15.2,8.34782559399999));
#212614=CARTESIAN_POINT('Ctrl Pts',(6.73964833099994,11.6,8.34782559399999));
#212615=CARTESIAN_POINT('Ctrl Pts',(6.74063164199994,15.2,8.35010335099999));
#212616=CARTESIAN_POINT('Ctrl Pts',(6.74063164199994,11.6,8.35010335099999));
#212617=CARTESIAN_POINT('Ctrl Pts',(6.74161543499994,15.2,8.35238763299999));
#212618=CARTESIAN_POINT('Ctrl Pts',(6.74161543499994,11.6,8.35238763299999));
#212619=CARTESIAN_POINT('Ctrl Pts',(6.74259969899994,15.2,8.35467843299998));
#212620=CARTESIAN_POINT('Ctrl Pts',(6.74259969899994,11.6,8.35467843299998));
#212621=CARTESIAN_POINT('Ctrl Pts',(6.74358441899994,15.2,8.35697574399998));
#212622=CARTESIAN_POINT('Ctrl Pts',(6.74358441899994,11.6,8.35697574399998));
#212623=CARTESIAN_POINT('Ctrl Pts',(6.74456958199994,15.2,8.35927955899999));
#212624=CARTESIAN_POINT('Ctrl Pts',(6.74456958199994,11.6,8.35927955899999));
#212625=CARTESIAN_POINT('Ctrl Pts',(6.74555517699994,15.2,8.36158986999998));
#212626=CARTESIAN_POINT('Ctrl Pts',(6.74555517699994,11.6,8.36158986999998));
#212627=CARTESIAN_POINT('Ctrl Pts',(6.74654118699994,15.2,8.36390667099998));
#212628=CARTESIAN_POINT('Ctrl Pts',(6.74654118699994,11.6,8.36390667099998));
#212629=CARTESIAN_POINT('Ctrl Pts',(6.74752760399994,15.2,8.36622995199999));
#212630=CARTESIAN_POINT('Ctrl Pts',(6.74752760399994,11.6,8.36622995199999));
#212631=CARTESIAN_POINT('Ctrl Pts',(6.74851440899995,15.2,8.36855970899999));
#212632=CARTESIAN_POINT('Ctrl Pts',(6.74851440899995,11.6,8.36855970899999));
#212633=CARTESIAN_POINT('Ctrl Pts',(6.74950159299994,15.2,8.37089593199998));
#212634=CARTESIAN_POINT('Ctrl Pts',(6.74950159299994,11.6,8.37089593199998));
#212635=CARTESIAN_POINT('Ctrl Pts',(6.75048914099994,15.2,8.37323861399998));
#212636=CARTESIAN_POINT('Ctrl Pts',(6.75048914099994,11.6,8.37323861399998));
#212637=CARTESIAN_POINT('Ctrl Pts',(6.75147703999994,15.2,8.37558774999999));
#212638=CARTESIAN_POINT('Ctrl Pts',(6.75147703999994,11.6,8.37558774999999));
#212639=CARTESIAN_POINT('Ctrl Pts',(6.75246527899994,15.2,8.37794333099998));
#212640=CARTESIAN_POINT('Ctrl Pts',(6.75246527899994,11.6,8.37794333099998));
#212641=CARTESIAN_POINT('Ctrl Pts',(6.75345384399994,15.2,8.38030534999999));
#212642=CARTESIAN_POINT('Ctrl Pts',(6.75345384399994,11.6,8.38030534999999));
#212643=CARTESIAN_POINT('Ctrl Pts',(6.75444272099995,15.2,8.38267379999999));
#212644=CARTESIAN_POINT('Ctrl Pts',(6.75444272099995,11.6,8.38267379999999));
#212645=CARTESIAN_POINT('Ctrl Pts',(6.75543189899994,15.2,8.38504867299999));
#212646=CARTESIAN_POINT('Ctrl Pts',(6.75543189899994,11.6,8.38504867299999));
#212647=CARTESIAN_POINT('Ctrl Pts',(6.75642136399994,15.2,8.38742996299998));
#212648=CARTESIAN_POINT('Ctrl Pts',(6.75642136399994,11.6,8.38742996299998));
#212649=CARTESIAN_POINT('Ctrl Pts',(6.75741110399994,15.2,8.38981766199998));
#212650=CARTESIAN_POINT('Ctrl Pts',(6.75741110399994,11.6,8.38981766199998));
#212651=CARTESIAN_POINT('Ctrl Pts',(6.75840110499994,15.2,8.39221176299999));
#212652=CARTESIAN_POINT('Ctrl Pts',(6.75840110499994,11.6,8.39221176299999));
#212653=CARTESIAN_POINT('Ctrl Pts',(6.75939135499994,15.2,8.39461225999998));
#212654=CARTESIAN_POINT('Ctrl Pts',(6.75939135499994,11.6,8.39461225999998));
#212655=CARTESIAN_POINT('Ctrl Pts',(6.76038184399994,15.2,8.39701914299999));
#212656=CARTESIAN_POINT('Ctrl Pts',(6.76038184399994,11.6,8.39701914299999));
#212657=CARTESIAN_POINT('Ctrl Pts',(6.76137255499994,15.2,8.39943240699998));
#212658=CARTESIAN_POINT('Ctrl Pts',(6.76137255499994,11.6,8.39943240699998));
#212659=CARTESIAN_POINT('Ctrl Pts',(6.76236347699994,15.2,8.40185204399998));
#212660=CARTESIAN_POINT('Ctrl Pts',(6.76236347699994,11.6,8.40185204399998));
#212661=CARTESIAN_POINT('Ctrl Pts',(6.76335459899994,15.2,8.40427804899999));
#212662=CARTESIAN_POINT('Ctrl Pts',(6.76335459899994,11.6,8.40427804899999));
#212663=CARTESIAN_POINT('Ctrl Pts',(6.76434590699994,15.2,8.40671041199998));
#212664=CARTESIAN_POINT('Ctrl Pts',(6.76434590699994,11.6,8.40671041199998));
#212665=CARTESIAN_POINT('Ctrl Pts',(6.76533738899994,15.2,8.40914912599998));
#212666=CARTESIAN_POINT('Ctrl Pts',(6.76533738899994,11.6,8.40914912599998));
#212667=CARTESIAN_POINT('Ctrl Pts',(6.76632903299994,15.2,8.41159418599998));
#212668=CARTESIAN_POINT('Ctrl Pts',(6.76632903299994,11.6,8.41159418599998));
#212669=CARTESIAN_POINT('Ctrl Pts',(6.76732082599995,15.2,8.41404558399999));
#212670=CARTESIAN_POINT('Ctrl Pts',(6.76732082599995,11.6,8.41404558399999));
#212671=CARTESIAN_POINT('Ctrl Pts',(6.76831275599994,15.2,8.41650331199999));
#212672=CARTESIAN_POINT('Ctrl Pts',(6.76831275599994,11.6,8.41650331199999));
#212673=CARTESIAN_POINT('Ctrl Pts',(6.76930481099994,15.2,8.41896736399999));
#212674=CARTESIAN_POINT('Ctrl Pts',(6.76930481099994,11.6,8.41896736399999));
#212675=CARTESIAN_POINT('Ctrl Pts',(6.77029697699994,15.2,8.42143773199999));
#212676=CARTESIAN_POINT('Ctrl Pts',(6.77029697699994,11.6,8.42143773199999));
#212677=CARTESIAN_POINT('Ctrl Pts',(6.77128924399995,15.2,8.42391440999998));
#212678=CARTESIAN_POINT('Ctrl Pts',(6.77128924399995,11.6,8.42391440999998));
#212679=CARTESIAN_POINT('Ctrl Pts',(6.77228159899994,15.2,8.42639739099998));
#212680=CARTESIAN_POINT('Ctrl Pts',(6.77228159899994,11.6,8.42639739099998));
#212681=CARTESIAN_POINT('Ctrl Pts',(6.77327402999994,15.2,8.42888666499999));
#212682=CARTESIAN_POINT('Ctrl Pts',(6.77327402999994,11.6,8.42888666499999));
#212683=CARTESIAN_POINT('Ctrl Pts',(6.77426652499994,15.2,8.43138222999999));
#212684=CARTESIAN_POINT('Ctrl Pts',(6.77426652499994,11.6,8.43138222999999));
#212685=CARTESIAN_POINT('Ctrl Pts',(6.77525906999994,15.2,8.43388407499998));
#212686=CARTESIAN_POINT('Ctrl Pts',(6.77525906999994,11.6,8.43388407499998));
#212687=CARTESIAN_POINT('Ctrl Pts',(6.77625165599994,15.2,8.43639219399999));
#212688=CARTESIAN_POINT('Ctrl Pts',(6.77625165599994,11.6,8.43639219399999));
#212689=CARTESIAN_POINT('Ctrl Pts',(6.77724426899994,15.2,8.43890658099999));
#212690=CARTESIAN_POINT('Ctrl Pts',(6.77724426899994,11.6,8.43890658099999));
#212691=CARTESIAN_POINT('Ctrl Pts',(6.77823689699995,15.2,8.44142722899999));
#212692=CARTESIAN_POINT('Ctrl Pts',(6.77823689699995,11.6,8.44142722899999));
#212693=CARTESIAN_POINT('Ctrl Pts',(6.77922952999994,15.2,8.44395412899999));
#212694=CARTESIAN_POINT('Ctrl Pts',(6.77922952999994,11.6,8.44395412899999));
#212695=CARTESIAN_POINT('Ctrl Pts',(6.78022215399994,15.2,8.44648727499998));
#212696=CARTESIAN_POINT('Ctrl Pts',(6.78022215399994,11.6,8.44648727499998));
#212697=CARTESIAN_POINT('Ctrl Pts',(6.78121475799994,15.2,8.44902666199999));
#212698=CARTESIAN_POINT('Ctrl Pts',(6.78121475799994,11.6,8.44902666199999));
#212699=CARTESIAN_POINT('Ctrl Pts',(6.78220733099994,15.2,8.45157227999999));
#212700=CARTESIAN_POINT('Ctrl Pts',(6.78220733099994,11.6,8.45157227999999));
#212701=CARTESIAN_POINT('Ctrl Pts',(6.78319985999994,15.2,8.45412412399998));
#212702=CARTESIAN_POINT('Ctrl Pts',(6.78319985999994,11.6,8.45412412399998));
#212703=CARTESIAN_POINT('Ctrl Pts',(6.78419233199994,15.2,8.45668218599998));
#212704=CARTESIAN_POINT('Ctrl Pts',(6.78419233199994,11.6,8.45668218599998));
#212705=CARTESIAN_POINT('Ctrl Pts',(6.78518473799994,15.2,8.45924645999999));
#212706=CARTESIAN_POINT('Ctrl Pts',(6.78518473799994,11.6,8.45924645999999));
#212707=CARTESIAN_POINT('Ctrl Pts',(6.78617706499994,15.2,8.46181693899998));
#212708=CARTESIAN_POINT('Ctrl Pts',(6.78617706499994,11.6,8.46181693899998));
#212709=CARTESIAN_POINT('Ctrl Pts',(6.78716930199994,15.2,8.46439361399998));
#212710=CARTESIAN_POINT('Ctrl Pts',(6.78716930199994,11.6,8.46439361399998));
#212711=CARTESIAN_POINT('Ctrl Pts',(6.78816143599994,15.2,8.46697648099998));
#212712=CARTESIAN_POINT('Ctrl Pts',(6.78816143599994,11.6,8.46697648099998));
#212713=CARTESIAN_POINT('Ctrl Pts',(6.78915345799994,15.2,8.46956553199998));
#212714=CARTESIAN_POINT('Ctrl Pts',(6.78915345799994,11.6,8.46956553199998));
#212715=CARTESIAN_POINT('Ctrl Pts',(6.79014535299994,15.2,8.47216075999999));
#212716=CARTESIAN_POINT('Ctrl Pts',(6.79014535299994,11.6,8.47216075999999));
#212717=CARTESIAN_POINT('Ctrl Pts',(6.79113711199994,15.2,8.47476215799999));
#212718=CARTESIAN_POINT('Ctrl Pts',(6.79113711199994,11.6,8.47476215799999));
#212719=CARTESIAN_POINT('Ctrl Pts',(6.79212872199995,15.2,8.47736971999998));
#212720=CARTESIAN_POINT('Ctrl Pts',(6.79212872199995,11.6,8.47736971999998));
#212721=CARTESIAN_POINT('Ctrl Pts',(6.79312017299995,15.2,8.47998343599999));
#212722=CARTESIAN_POINT('Ctrl Pts',(6.79312017299995,11.6,8.47998343599999));
#212723=CARTESIAN_POINT('Ctrl Pts',(6.79411145299994,15.2,8.48260330499999));
#212724=CARTESIAN_POINT('Ctrl Pts',(6.79411145299994,11.6,8.48260330499999));
#212725=CARTESIAN_POINT('Ctrl Pts',(6.79510254999995,15.2,8.48522931399999));
#212726=CARTESIAN_POINT('Ctrl Pts',(6.79510254999995,11.6,8.48522931399999));
#212727=CARTESIAN_POINT('Ctrl Pts',(6.79609345299995,15.2,8.48786145899999));
#212728=CARTESIAN_POINT('Ctrl Pts',(6.79609345299995,11.6,8.48786145899999));
#212729=CARTESIAN_POINT('Ctrl Pts',(6.79708415199994,15.2,8.49049973299999));
#212730=CARTESIAN_POINT('Ctrl Pts',(6.79708415199994,11.6,8.49049973299999));
#212731=CARTESIAN_POINT('Ctrl Pts',(6.79807463299994,15.2,8.49314413099999));
#212732=CARTESIAN_POINT('Ctrl Pts',(6.79807463299994,11.6,8.49314413099999));
#212733=CARTESIAN_POINT('Ctrl Pts',(6.79906488699995,15.2,8.49579464199999));
#212734=CARTESIAN_POINT('Ctrl Pts',(6.79906488699995,11.6,8.49579464199999));
#212735=CARTESIAN_POINT('Ctrl Pts',(6.80005490199994,15.2,8.49845126299999));
#212736=CARTESIAN_POINT('Ctrl Pts',(6.80005490199994,11.6,8.49845126299999));
#212737=CARTESIAN_POINT('Ctrl Pts',(6.80104466699994,15.2,8.50111398499998));
#212738=CARTESIAN_POINT('Ctrl Pts',(6.80104466699994,11.6,8.50111398499998));
#212739=CARTESIAN_POINT('Ctrl Pts',(6.80203416999994,15.2,8.50378280199998));
#212740=CARTESIAN_POINT('Ctrl Pts',(6.80203416999994,11.6,8.50378280199998));
#212741=CARTESIAN_POINT('Ctrl Pts',(6.80302340199994,15.2,8.50645770699998));
#212742=CARTESIAN_POINT('Ctrl Pts',(6.80302340199994,11.6,8.50645770699998));
#212743=CARTESIAN_POINT('Ctrl Pts',(6.80401234899994,15.2,8.50913869399999));
#212744=CARTESIAN_POINT('Ctrl Pts',(6.80401234899994,11.6,8.50913869399999));
#212745=CARTESIAN_POINT('Ctrl Pts',(6.80500100199994,15.2,8.51182575499998));
#212746=CARTESIAN_POINT('Ctrl Pts',(6.80500100199994,11.6,8.51182575499998));
#212747=CARTESIAN_POINT('Ctrl Pts',(6.80598934999994,15.2,8.51451888299999));
#212748=CARTESIAN_POINT('Ctrl Pts',(6.80598934999994,11.6,8.51451888299999));
#212749=CARTESIAN_POINT('Ctrl Pts',(6.80697738099994,15.2,8.51721807399999));
#212750=CARTESIAN_POINT('Ctrl Pts',(6.80697738099994,11.6,8.51721807399999));
#212751=CARTESIAN_POINT('Ctrl Pts',(6.80796508399995,15.2,8.51992331899999));
#212752=CARTESIAN_POINT('Ctrl Pts',(6.80796508399995,11.6,8.51992331899999));
#212753=CARTESIAN_POINT('Ctrl Pts',(6.80895244899994,15.2,8.52263460999998));
#212754=CARTESIAN_POINT('Ctrl Pts',(6.80895244899994,11.6,8.52263460999998));
#212755=CARTESIAN_POINT('Ctrl Pts',(6.80993946499994,15.2,8.52535194399999));
#212756=CARTESIAN_POINT('Ctrl Pts',(6.80993946499994,11.6,8.52535194399999));
#212757=CARTESIAN_POINT('Ctrl Pts',(6.81092611999994,15.2,8.52807530999998));
#212758=CARTESIAN_POINT('Ctrl Pts',(6.81092611999994,11.6,8.52807530999998));
#212759=CARTESIAN_POINT('Ctrl Pts',(6.81191240399994,15.2,8.53080470399998));
#212760=CARTESIAN_POINT('Ctrl Pts',(6.81191240399994,11.6,8.53080470399998));
#212761=CARTESIAN_POINT('Ctrl Pts',(6.81289830599995,15.2,8.53354011999999));
#212762=CARTESIAN_POINT('Ctrl Pts',(6.81289830599995,11.6,8.53354011999999));
#212763=CARTESIAN_POINT('Ctrl Pts',(6.81388381499994,15.2,8.53628154899998));
#212764=CARTESIAN_POINT('Ctrl Pts',(6.81388381499994,11.6,8.53628154899998));
#212765=CARTESIAN_POINT('Ctrl Pts',(6.81486892199994,15.2,8.53902898499998));
#212766=CARTESIAN_POINT('Ctrl Pts',(6.81486892199994,11.6,8.53902898499998));
#212767=CARTESIAN_POINT('Ctrl Pts',(6.81585361299994,15.2,8.54178242199998));
#212768=CARTESIAN_POINT('Ctrl Pts',(6.81585361299994,11.6,8.54178242199998));
#212769=CARTESIAN_POINT('Ctrl Pts',(6.81683788099994,15.2,8.54454185299998));
#212770=CARTESIAN_POINT('Ctrl Pts',(6.81683788099994,11.6,8.54454185299998));
#212771=CARTESIAN_POINT('Ctrl Pts',(6.81782171199995,15.2,8.54730727199998));
#212772=CARTESIAN_POINT('Ctrl Pts',(6.81782171199995,11.6,8.54730727199998));
#212773=CARTESIAN_POINT('Ctrl Pts',(6.81880509699995,15.2,8.55007867099999));
#212774=CARTESIAN_POINT('Ctrl Pts',(6.81880509699995,11.6,8.55007867099999));
#212775=CARTESIAN_POINT('Ctrl Pts',(6.81978802599994,15.2,8.55285604299999));
#212776=CARTESIAN_POINT('Ctrl Pts',(6.81978802599994,11.6,8.55285604299999));
#212777=CARTESIAN_POINT('Ctrl Pts',(6.82077048599994,15.2,8.55563938299999));
#212778=CARTESIAN_POINT('Ctrl Pts',(6.82077048599994,11.6,8.55563938299999));
#212779=CARTESIAN_POINT('Ctrl Pts',(6.82175246999994,15.2,8.55842868399998));
#212780=CARTESIAN_POINT('Ctrl Pts',(6.82175246999994,11.6,8.55842868399998));
#212781=CARTESIAN_POINT('Ctrl Pts',(6.82273396499994,15.2,8.56122393999998));
#212782=CARTESIAN_POINT('Ctrl Pts',(6.82273396499994,11.6,8.56122393999998));
#212783=CARTESIAN_POINT('Ctrl Pts',(6.82371496099995,15.2,8.56402514099998));
#212784=CARTESIAN_POINT('Ctrl Pts',(6.82371496099995,11.6,8.56402514099998));
#212785=CARTESIAN_POINT('Ctrl Pts',(6.82469544599994,15.2,8.56683228399999));
#212786=CARTESIAN_POINT('Ctrl Pts',(6.82469544599994,11.6,8.56683228399999));
#212787=CARTESIAN_POINT('Ctrl Pts',(6.82567541399994,15.2,8.56964536099999));
#212788=CARTESIAN_POINT('Ctrl Pts',(6.82567541399994,11.6,8.56964536099999));
#212789=CARTESIAN_POINT('Ctrl Pts',(6.82665484999994,15.2,8.57246436599999));
#212790=CARTESIAN_POINT('Ctrl Pts',(6.82665484999994,11.6,8.57246436599999));
#212791=CARTESIAN_POINT('Ctrl Pts',(6.82763374599994,15.2,8.57528929199999));
#212792=CARTESIAN_POINT('Ctrl Pts',(6.82763374599994,11.6,8.57528929199999));
#212793=CARTESIAN_POINT('Ctrl Pts',(6.82861209099995,15.2,8.57812013199998));
#212794=CARTESIAN_POINT('Ctrl Pts',(6.82861209099995,11.6,8.57812013199998));
#212795=CARTESIAN_POINT('Ctrl Pts',(6.82958987399994,15.2,8.58095687999998));
#212796=CARTESIAN_POINT('Ctrl Pts',(6.82958987399994,11.6,8.58095687999998));
#212797=CARTESIAN_POINT('Ctrl Pts',(6.83056708699994,15.2,8.58379952899998));
#212798=CARTESIAN_POINT('Ctrl Pts',(6.83056708699994,11.6,8.58379952899998));
#212799=CARTESIAN_POINT('Ctrl Pts',(6.83154371799994,15.2,8.58664807299999));
#212800=CARTESIAN_POINT('Ctrl Pts',(6.83154371799994,11.6,8.58664807299999));
#212801=CARTESIAN_POINT('Ctrl Pts',(6.83251975599994,15.2,8.58950250499999));
#212802=CARTESIAN_POINT('Ctrl Pts',(6.83251975599994,11.6,8.58950250499999));
#212803=CARTESIAN_POINT('Ctrl Pts',(6.83349519199994,15.2,8.59236281799999));
#212804=CARTESIAN_POINT('Ctrl Pts',(6.83349519199994,11.6,8.59236281799999));
#212805=CARTESIAN_POINT('Ctrl Pts',(6.83447001599994,15.2,8.59522900599998));
#212806=CARTESIAN_POINT('Ctrl Pts',(6.83447001599994,11.6,8.59522900599998));
#212807=CARTESIAN_POINT('Ctrl Pts',(6.83544421899994,15.2,8.59810106299999));
#212808=CARTESIAN_POINT('Ctrl Pts',(6.83544421899994,11.6,8.59810106299999));
#212809=CARTESIAN_POINT('Ctrl Pts',(6.83641778699994,15.2,8.60097898199999));
#212810=CARTESIAN_POINT('Ctrl Pts',(6.83641778699994,11.6,8.60097898199999));
#212811=CARTESIAN_POINT('Ctrl Pts',(6.83739071399994,15.2,8.60386275599998));
#212812=CARTESIAN_POINT('Ctrl Pts',(6.83739071399994,11.6,8.60386275599998));
#212813=CARTESIAN_POINT('Ctrl Pts',(6.83836298699994,15.2,8.60675237899999));
#212814=CARTESIAN_POINT('Ctrl Pts',(6.83836298699994,11.6,8.60675237899999));
#212815=CARTESIAN_POINT('Ctrl Pts',(6.83933459699994,15.2,8.60964784399999));
#212816=CARTESIAN_POINT('Ctrl Pts',(6.83933459699994,11.6,8.60964784399999));
#212817=CARTESIAN_POINT('Ctrl Pts',(6.84030553599994,15.2,8.61254914499998));
#212818=CARTESIAN_POINT('Ctrl Pts',(6.84030553599994,11.6,8.61254914499998));
#212819=CARTESIAN_POINT('Ctrl Pts',(6.84127578999994,15.2,8.61545627499999));
#212820=CARTESIAN_POINT('Ctrl Pts',(6.84127578999994,11.6,8.61545627499999));
#212821=CARTESIAN_POINT('Ctrl Pts',(6.84224535299994,15.2,8.61836922799998));
#212822=CARTESIAN_POINT('Ctrl Pts',(6.84224535299994,11.6,8.61836922799998));
#212823=CARTESIAN_POINT('Ctrl Pts',(6.84321421299994,15.2,8.62128799799999));
#212824=CARTESIAN_POINT('Ctrl Pts',(6.84321421299994,11.6,8.62128799799999));
#212825=CARTESIAN_POINT('Ctrl Pts',(6.84418235899994,15.2,8.62421257699998));
#212826=CARTESIAN_POINT('Ctrl Pts',(6.84418235899994,11.6,8.62421257699998));
#212827=CARTESIAN_POINT('Ctrl Pts',(6.84514978399994,15.2,8.62714295999999));
#212828=CARTESIAN_POINT('Ctrl Pts',(6.84514978399994,11.6,8.62714295999999));
#212829=CARTESIAN_POINT('Ctrl Pts',(6.84611647599994,15.2,8.63007913899999));
#212830=CARTESIAN_POINT('Ctrl Pts',(6.84611647599994,11.6,8.63007913899999));
#212831=CARTESIAN_POINT('Ctrl Pts',(6.84708242699994,15.2,8.63302110999999));
#212832=CARTESIAN_POINT('Ctrl Pts',(6.84708242699994,11.6,8.63302110999999));
#212833=CARTESIAN_POINT('Ctrl Pts',(6.84804762499994,15.2,8.63596886399998));
#212834=CARTESIAN_POINT('Ctrl Pts',(6.84804762499994,11.6,8.63596886399998));
#212835=CARTESIAN_POINT('Ctrl Pts',(6.84901206199994,15.2,8.63892239499998));
#212836=CARTESIAN_POINT('Ctrl Pts',(6.84901206199994,11.6,8.63892239499998));
#212837=CARTESIAN_POINT('Ctrl Pts',(6.84997572699994,15.2,8.64188169799998));
#212838=CARTESIAN_POINT('Ctrl Pts',(6.84997572699994,11.6,8.64188169799998));
#212839=CARTESIAN_POINT('Ctrl Pts',(6.85093861099995,15.2,8.64484676499998));
#212840=CARTESIAN_POINT('Ctrl Pts',(6.85093861099995,11.6,8.64484676499998));
#212841=CARTESIAN_POINT('Ctrl Pts',(6.85190070399995,15.2,8.64781759099999));
#212842=CARTESIAN_POINT('Ctrl Pts',(6.85190070399995,11.6,8.64781759099999));
#212843=CARTESIAN_POINT('Ctrl Pts',(6.85286199699994,15.2,8.65079416799999));
#212844=CARTESIAN_POINT('Ctrl Pts',(6.85286199699994,11.6,8.65079416799999));
#212845=CARTESIAN_POINT('Ctrl Pts',(6.85382247899994,15.2,8.65377649199999));
#212846=CARTESIAN_POINT('Ctrl Pts',(6.85382247899994,11.6,8.65377649199999));
#212847=CARTESIAN_POINT('Ctrl Pts',(6.85478214199994,15.2,8.65676455299998));
#212848=CARTESIAN_POINT('Ctrl Pts',(6.85478214199994,11.6,8.65676455299998));
#212849=CARTESIAN_POINT('Ctrl Pts',(6.85574097599994,15.2,8.65975834699999));
#212850=CARTESIAN_POINT('Ctrl Pts',(6.85574097599994,11.6,8.65975834699999));
#212851=CARTESIAN_POINT('Ctrl Pts',(6.85669896999994,15.2,8.66275786799999));
#212852=CARTESIAN_POINT('Ctrl Pts',(6.85669896999994,11.6,8.66275786799999));
#212853=CARTESIAN_POINT('Ctrl Pts',(6.85765611699994,15.2,8.66576310799999));
#212854=CARTESIAN_POINT('Ctrl Pts',(6.85765611699994,11.6,8.66576310799999));
#212855=CARTESIAN_POINT('Ctrl Pts',(6.85861240499994,15.2,8.66877406199999));
#212856=CARTESIAN_POINT('Ctrl Pts',(6.85861240499994,11.6,8.66877406199999));
#212857=CARTESIAN_POINT('Ctrl Pts',(6.85956782499994,15.2,8.67179072199999));
#212858=CARTESIAN_POINT('Ctrl Pts',(6.85956782499994,11.6,8.67179072199999));
#212859=CARTESIAN_POINT('Ctrl Pts',(6.86052236999994,15.2,8.67481308299999));
#212860=CARTESIAN_POINT('Ctrl Pts',(6.86052236999994,11.6,8.67481308299999));
#212861=CARTESIAN_POINT('Ctrl Pts',(6.86147602799994,15.2,8.67784113899998));
#212862=CARTESIAN_POINT('Ctrl Pts',(6.86147602799994,11.6,8.67784113899998));
#212863=CARTESIAN_POINT('Ctrl Pts',(6.86242878899994,15.2,8.68087488199999));
#212864=CARTESIAN_POINT('Ctrl Pts',(6.86242878899994,11.6,8.68087488199999));
#212865=CARTESIAN_POINT('Ctrl Pts',(6.86338064599994,15.2,8.68391430699998));
#212866=CARTESIAN_POINT('Ctrl Pts',(6.86338064599994,11.6,8.68391430699998));
#212867=CARTESIAN_POINT('Ctrl Pts',(6.86433158899994,15.2,8.68695940699999));
#212868=CARTESIAN_POINT('Ctrl Pts',(6.86433158899994,11.6,8.68695940699999));
#212869=CARTESIAN_POINT('Ctrl Pts',(6.86528160599994,15.2,8.69001017499999));
#212870=CARTESIAN_POINT('Ctrl Pts',(6.86528160599994,11.6,8.69001017499999));
#212871=CARTESIAN_POINT('Ctrl Pts',(6.86623069199994,15.2,8.69306660699999));
#212872=CARTESIAN_POINT('Ctrl Pts',(6.86623069199994,11.6,8.69306660699999));
#212873=CARTESIAN_POINT('Ctrl Pts',(6.86717883499994,15.2,8.69612869499999));
#212874=CARTESIAN_POINT('Ctrl Pts',(6.86717883499994,11.6,8.69612869499999));
#212875=CARTESIAN_POINT('Ctrl Pts',(6.86812602599994,15.2,8.69919643199999));
#212876=CARTESIAN_POINT('Ctrl Pts',(6.86812602599994,11.6,8.69919643199999));
#212877=CARTESIAN_POINT('Ctrl Pts',(6.86907225599994,15.2,8.70226981399998));
#212878=CARTESIAN_POINT('Ctrl Pts',(6.86907225599994,11.6,8.70226981399998));
#212879=CARTESIAN_POINT('Ctrl Pts',(6.87001751699994,15.2,8.70534883199999));
#212880=CARTESIAN_POINT('Ctrl Pts',(6.87001751699994,11.6,8.70534883199999));
#212881=CARTESIAN_POINT('Ctrl Pts',(6.87096179699994,15.2,8.70843347999998));
#212882=CARTESIAN_POINT('Ctrl Pts',(6.87096179699994,11.6,8.70843347999998));
#212883=CARTESIAN_POINT('Ctrl Pts',(6.87190508999994,15.2,8.71152375499998));
#212884=CARTESIAN_POINT('Ctrl Pts',(6.87190508999994,11.6,8.71152375499998));
#212885=CARTESIAN_POINT('Ctrl Pts',(6.87284738499994,15.2,8.71461964699999));
#212886=CARTESIAN_POINT('Ctrl Pts',(6.87284738499994,11.6,8.71461964699999));
#212887=CARTESIAN_POINT('Ctrl Pts',(6.87378867299994,15.2,8.71772115099999));
#212888=CARTESIAN_POINT('Ctrl Pts',(6.87378867299994,11.6,8.71772115099999));
#212889=CARTESIAN_POINT('Ctrl Pts',(6.87472894499995,15.2,8.72082825999998));
#212890=CARTESIAN_POINT('Ctrl Pts',(6.87472894499995,11.6,8.72082825999998));
#212891=CARTESIAN_POINT('Ctrl Pts',(6.87566819199994,15.2,8.72394096899999));
#212892=CARTESIAN_POINT('Ctrl Pts',(6.87566819199994,11.6,8.72394096899999));
#212893=CARTESIAN_POINT('Ctrl Pts',(6.87660640499994,15.2,8.72705927199998));
#212894=CARTESIAN_POINT('Ctrl Pts',(6.87660640499994,11.6,8.72705927199998));
#212895=CARTESIAN_POINT('Ctrl Pts',(6.87754357599994,15.2,8.73018315999998));
#212896=CARTESIAN_POINT('Ctrl Pts',(6.87754357599994,11.6,8.73018315999998));
#212897=CARTESIAN_POINT('Ctrl Pts',(6.87847969399995,15.2,8.73331262999999));
#212898=CARTESIAN_POINT('Ctrl Pts',(6.87847969399995,11.6,8.73331262999999));
#212899=CARTESIAN_POINT('Ctrl Pts',(6.87941475099994,15.2,8.73644767499999));
#212900=CARTESIAN_POINT('Ctrl Pts',(6.87941475099994,11.6,8.73644767499999));
#212901=CARTESIAN_POINT('Ctrl Pts',(6.88034873899994,15.2,8.73958828699998));
#212902=CARTESIAN_POINT('Ctrl Pts',(6.88034873899994,11.6,8.73958828699998));
#212903=CARTESIAN_POINT('Ctrl Pts',(6.88128164699994,15.2,8.74273446099998));
#212904=CARTESIAN_POINT('Ctrl Pts',(6.88128164699994,11.6,8.74273446099998));
#212905=CARTESIAN_POINT('Ctrl Pts',(6.88221346799994,15.2,8.74588618999999));
#212906=CARTESIAN_POINT('Ctrl Pts',(6.88221346799994,11.6,8.74588618999999));
#212907=CARTESIAN_POINT('Ctrl Pts',(6.88314419099994,15.2,8.74904346999998));
#212908=CARTESIAN_POINT('Ctrl Pts',(6.88314419099994,11.6,8.74904346999998));
#212909=CARTESIAN_POINT('Ctrl Pts',(6.88407380999994,15.2,8.75220629299999));
#212910=CARTESIAN_POINT('Ctrl Pts',(6.88407380999994,11.6,8.75220629299999));
#212911=CARTESIAN_POINT('Ctrl Pts',(6.88500231399994,15.2,8.75537465099999));
#212912=CARTESIAN_POINT('Ctrl Pts',(6.88500231399994,11.6,8.75537465099999));
#212913=CARTESIAN_POINT('Ctrl Pts',(6.88592969499994,15.2,8.75854854099998));
#212914=CARTESIAN_POINT('Ctrl Pts',(6.88592969499994,11.6,8.75854854099998));
#212915=CARTESIAN_POINT('Ctrl Pts',(6.88685594399994,15.2,8.76172795599999));
#212916=CARTESIAN_POINT('Ctrl Pts',(6.88685594399994,11.6,8.76172795599999));
#212917=CARTESIAN_POINT('Ctrl Pts',(6.88778105099995,15.2,8.76491288799999));
#212918=CARTESIAN_POINT('Ctrl Pts',(6.88778105099995,11.6,8.76491288799999));
#212919=CARTESIAN_POINT('Ctrl Pts',(6.88870501099994,15.2,8.76810333299998));
#212920=CARTESIAN_POINT('Ctrl Pts',(6.88870501099994,11.6,8.76810333299998));
#212921=CARTESIAN_POINT('Ctrl Pts',(6.88962781099994,15.2,8.77129928399999));
#212922=CARTESIAN_POINT('Ctrl Pts',(6.88962781099994,11.6,8.77129928399999));
#212923=CARTESIAN_POINT('Ctrl Pts',(6.89054944499994,15.2,8.77450073399999));
#212924=CARTESIAN_POINT('Ctrl Pts',(6.89054944499994,11.6,8.77450073399999));
#212925=CARTESIAN_POINT('Ctrl Pts',(6.89146990199994,15.2,8.77770767799999));
#212926=CARTESIAN_POINT('Ctrl Pts',(6.89146990199994,11.6,8.77770767799999));
#212927=CARTESIAN_POINT('Ctrl Pts',(6.89238917499994,15.2,8.78092010899999));
#212928=CARTESIAN_POINT('Ctrl Pts',(6.89238917499994,11.6,8.78092010899999));
#212929=CARTESIAN_POINT('Ctrl Pts',(6.89330725499994,15.2,8.78413802199999));
#212930=CARTESIAN_POINT('Ctrl Pts',(6.89330725499994,11.6,8.78413802199999));
#212931=CARTESIAN_POINT('Ctrl Pts',(6.89422413499994,15.2,8.78736140899999));
#212932=CARTESIAN_POINT('Ctrl Pts',(6.89422413499994,11.6,8.78736140899999));
#212933=CARTESIAN_POINT('Ctrl Pts',(6.89513980299994,15.2,8.79059026499998));
#212934=CARTESIAN_POINT('Ctrl Pts',(6.89513980299994,11.6,8.79059026499998));
#212935=CARTESIAN_POINT('Ctrl Pts',(6.89605425299994,15.2,8.79382458399999));
#212936=CARTESIAN_POINT('Ctrl Pts',(6.89605425299994,11.6,8.79382458399999));
#212937=CARTESIAN_POINT('Ctrl Pts',(6.89696747599994,15.2,8.79706435899998));
#212938=CARTESIAN_POINT('Ctrl Pts',(6.89696747599994,11.6,8.79706435899998));
#212939=CARTESIAN_POINT('Ctrl Pts',(6.89787946299995,15.2,8.80030958399999));
#212940=CARTESIAN_POINT('Ctrl Pts',(6.89787946299995,11.6,8.80030958399999));
#212941=CARTESIAN_POINT('Ctrl Pts',(6.89879020599995,15.2,8.80356025499999));
#212942=CARTESIAN_POINT('Ctrl Pts',(6.89879020599995,11.6,8.80356025499999));
#212943=CARTESIAN_POINT('Ctrl Pts',(6.89969969499994,15.2,8.80681636199999));
#212944=CARTESIAN_POINT('Ctrl Pts',(6.89969969499994,11.6,8.80681636199999));
#212945=CARTESIAN_POINT('Ctrl Pts',(6.90060792399994,15.2,8.81007790299999));
#212946=CARTESIAN_POINT('Ctrl Pts',(6.90060792399994,11.6,8.81007790299999));
#212947=CARTESIAN_POINT('Ctrl Pts',(6.90151488199994,15.2,8.81334486799998));
#212948=CARTESIAN_POINT('Ctrl Pts',(6.90151488199994,11.6,8.81334486799998));
#212949=CARTESIAN_POINT('Ctrl Pts',(6.90242056299994,15.2,8.81661725299999));
#212950=CARTESIAN_POINT('Ctrl Pts',(6.90242056299994,11.6,8.81661725299999));
#212951=CARTESIAN_POINT('Ctrl Pts',(6.90332495699994,15.2,8.81989505199999));
#212952=CARTESIAN_POINT('Ctrl Pts',(6.90332495699994,11.6,8.81989505199999));
#212953=CARTESIAN_POINT('Ctrl Pts',(6.90422805599994,15.2,8.82317825799999));
#212954=CARTESIAN_POINT('Ctrl Pts',(6.90422805599994,11.6,8.82317825799999));
#212955=CARTESIAN_POINT('Ctrl Pts',(6.90512985199994,15.2,8.82646686599998));
#212956=CARTESIAN_POINT('Ctrl Pts',(6.90512985199994,11.6,8.82646686599998));
#212957=CARTESIAN_POINT('Ctrl Pts',(6.90603033499994,15.2,8.82976086899999));
#212958=CARTESIAN_POINT('Ctrl Pts',(6.90603033499994,11.6,8.82976086899999));
#212959=CARTESIAN_POINT('Ctrl Pts',(6.90692949899994,15.2,8.83306025999998));
#212960=CARTESIAN_POINT('Ctrl Pts',(6.90692949899994,11.6,8.83306025999998));
#212961=CARTESIAN_POINT('Ctrl Pts',(6.90782733599994,15.2,8.83636503599998));
#212962=CARTESIAN_POINT('Ctrl Pts',(6.90782733599994,11.6,8.83636503599998));
#212963=CARTESIAN_POINT('Ctrl Pts',(6.90872383499994,15.2,8.83967518699999));
#212964=CARTESIAN_POINT('Ctrl Pts',(6.90872383499994,11.6,8.83967518699999));
#212965=CARTESIAN_POINT('Ctrl Pts',(6.90961898899995,15.2,8.84299070899999));
#212966=CARTESIAN_POINT('Ctrl Pts',(6.90961898899995,11.6,8.84299070899999));
#212967=CARTESIAN_POINT('Ctrl Pts',(6.91051278999994,15.2,8.84631159699998));
#212968=CARTESIAN_POINT('Ctrl Pts',(6.91051278999994,11.6,8.84631159699998));
#212969=CARTESIAN_POINT('Ctrl Pts',(6.91140523099994,15.2,8.84963784299998));
#212970=CARTESIAN_POINT('Ctrl Pts',(6.91140523099994,11.6,8.84963784299998));
#212971=CARTESIAN_POINT('Ctrl Pts',(6.91229630099994,15.2,8.85296944199998));
#212972=CARTESIAN_POINT('Ctrl Pts',(6.91229630099994,11.6,8.85296944199998));
#212973=CARTESIAN_POINT('Ctrl Pts',(6.91318599399994,15.2,8.85630638799999));
#212974=CARTESIAN_POINT('Ctrl Pts',(6.91318599399994,11.6,8.85630638799999));
#212975=CARTESIAN_POINT('Ctrl Pts',(6.91407430099994,15.2,8.85964867299998));
#212976=CARTESIAN_POINT('Ctrl Pts',(6.91407430099994,11.6,8.85964867299998));
#212977=CARTESIAN_POINT('Ctrl Pts',(6.91496121499994,15.2,8.86299629399998));
#212978=CARTESIAN_POINT('Ctrl Pts',(6.91496121499994,11.6,8.86299629399998));
#212979=CARTESIAN_POINT('Ctrl Pts',(6.91584672499994,15.2,8.86634924299998));
#212980=CARTESIAN_POINT('Ctrl Pts',(6.91584672499994,11.6,8.86634924299998));
#212981=CARTESIAN_POINT('Ctrl Pts',(6.91673082599995,15.2,8.86970751299998));
#212982=CARTESIAN_POINT('Ctrl Pts',(6.91673082599995,11.6,8.86970751299998));
#212983=CARTESIAN_POINT('Ctrl Pts',(6.91761350799994,15.2,8.87307110099999));
#212984=CARTESIAN_POINT('Ctrl Pts',(6.91761350799994,11.6,8.87307110099999));
#212985=CARTESIAN_POINT('Ctrl Pts',(6.91849476599994,15.2,8.87643999799998));
#212986=CARTESIAN_POINT('Ctrl Pts',(6.91849476599994,11.6,8.87643999799998));
#212987=CARTESIAN_POINT('Ctrl Pts',(6.91937458799995,15.2,8.87981419999999));
#212988=CARTESIAN_POINT('Ctrl Pts',(6.91937458799995,11.6,8.87981419999999));
#212989=CARTESIAN_POINT('Ctrl Pts',(6.92025296699994,15.2,8.88319369999999));
#212990=CARTESIAN_POINT('Ctrl Pts',(6.92025296699994,11.6,8.88319369999999));
#212991=CARTESIAN_POINT('Ctrl Pts',(6.92112989699995,15.2,8.88657849199999));
#212992=CARTESIAN_POINT('Ctrl Pts',(6.92112989699995,11.6,8.88657849199999));
#212993=CARTESIAN_POINT('Ctrl Pts',(6.92200536799994,15.2,8.88996856999999));
#212994=CARTESIAN_POINT('Ctrl Pts',(6.92200536799994,11.6,8.88996856999999));
#212995=CARTESIAN_POINT('Ctrl Pts',(6.92287937299994,15.2,8.89336392899999));
#212996=CARTESIAN_POINT('Ctrl Pts',(6.92287937299994,11.6,8.89336392899999));
#212997=CARTESIAN_POINT('Ctrl Pts',(6.92375190399994,15.2,8.89676456099998));
#212998=CARTESIAN_POINT('Ctrl Pts',(6.92375190399994,11.6,8.89676456099998));
#212999=CARTESIAN_POINT('Ctrl Pts',(6.92462295199994,15.2,8.90017046199999));
#213000=CARTESIAN_POINT('Ctrl Pts',(6.92462295199994,11.6,8.90017046199999));
#213001=CARTESIAN_POINT('Ctrl Pts',(6.92549251099994,15.2,8.90358162499999));
#213002=CARTESIAN_POINT('Ctrl Pts',(6.92549251099994,11.6,8.90358162499999));
#213003=CARTESIAN_POINT('Ctrl Pts',(6.92636057199994,15.2,8.90699804499998));
#213004=CARTESIAN_POINT('Ctrl Pts',(6.92636057199994,11.6,8.90699804499998));
#213005=CARTESIAN_POINT('Ctrl Pts',(6.92722712699994,15.2,8.91041971399999));
#213006=CARTESIAN_POINT('Ctrl Pts',(6.92722712699994,11.6,8.91041971399999));
#213007=CARTESIAN_POINT('Ctrl Pts',(6.92809216799994,15.2,8.91384662599998));
#213008=CARTESIAN_POINT('Ctrl Pts',(6.92809216799994,11.6,8.91384662599998));
#213009=CARTESIAN_POINT('Ctrl Pts',(6.92895568699995,15.2,8.91727877899999));
#213010=CARTESIAN_POINT('Ctrl Pts',(6.92895568699995,11.6,8.91727877899999));
#213011=CARTESIAN_POINT('Ctrl Pts',(6.92981767799994,15.2,8.92071616199999));
#213012=CARTESIAN_POINT('Ctrl Pts',(6.92981767799994,11.6,8.92071616199999));
#213013=CARTESIAN_POINT('Ctrl Pts',(6.93067813199994,15.2,8.92415877199999));
#213014=CARTESIAN_POINT('Ctrl Pts',(6.93067813199994,11.6,8.92415877199999));
#213015=CARTESIAN_POINT('Ctrl Pts',(6.93153704099994,15.2,8.92760660299999));
#213016=CARTESIAN_POINT('Ctrl Pts',(6.93153704099994,11.6,8.92760660299999));
#213017=CARTESIAN_POINT('Ctrl Pts',(6.93239439699994,15.2,8.93105964699998));
#213018=CARTESIAN_POINT('Ctrl Pts',(6.93239439699994,11.6,8.93105964699998));
#213019=CARTESIAN_POINT('Ctrl Pts',(6.93325019299994,15.2,8.93451789999999));
#213020=CARTESIAN_POINT('Ctrl Pts',(6.93325019299994,11.6,8.93451789999999));
#213021=CARTESIAN_POINT('Ctrl Pts',(6.93410442099994,15.2,8.93798135499999));
#213022=CARTESIAN_POINT('Ctrl Pts',(6.93410442099994,11.6,8.93798135499999));
#213023=CARTESIAN_POINT('Ctrl Pts',(6.93495707299994,15.2,8.94145000699999));
#213024=CARTESIAN_POINT('Ctrl Pts',(6.93495707299994,11.6,8.94145000699999));
#213025=CARTESIAN_POINT('Ctrl Pts',(6.93580814299994,15.2,8.94492384899999));
#213026=CARTESIAN_POINT('Ctrl Pts',(6.93580814299994,11.6,8.94492384899999));
#213027=CARTESIAN_POINT('Ctrl Pts',(6.93665761999994,15.2,8.94840287599998));
#213028=CARTESIAN_POINT('Ctrl Pts',(6.93665761999994,11.6,8.94840287599998));
#213029=CARTESIAN_POINT('Ctrl Pts',(6.93750550099994,15.2,8.95188708099998));
#213030=CARTESIAN_POINT('Ctrl Pts',(6.93750550099994,11.6,8.95188708099998));
#213031=CARTESIAN_POINT('Ctrl Pts',(6.93835177299994,15.2,8.95537645999998));
#213032=CARTESIAN_POINT('Ctrl Pts',(6.93835177299994,11.6,8.95537645999998));
#213033=CARTESIAN_POINT('Ctrl Pts',(6.93919643299994,15.2,8.95887100399998));
#213034=CARTESIAN_POINT('Ctrl Pts',(6.93919643299994,11.6,8.95887100399998));
#213035=CARTESIAN_POINT('Ctrl Pts',(6.94003947099994,15.2,8.96237070999998));
#213036=CARTESIAN_POINT('Ctrl Pts',(6.94003947099994,11.6,8.96237070999998));
#213037=CARTESIAN_POINT('Ctrl Pts',(6.94088087899994,15.2,8.96587557099998));
#213038=CARTESIAN_POINT('Ctrl Pts',(6.94088087899994,11.6,8.96587557099998));
#213039=CARTESIAN_POINT('Ctrl Pts',(6.94172065299994,15.2,8.96938558099999));
#213040=CARTESIAN_POINT('Ctrl Pts',(6.94172065299994,11.6,8.96938558099999));
#213041=CARTESIAN_POINT('Ctrl Pts',(6.94255878099994,15.2,8.97290073299999));
#213042=CARTESIAN_POINT('Ctrl Pts',(6.94255878099994,11.6,8.97290073299999));
#213043=CARTESIAN_POINT('Ctrl Pts',(6.94339525799994,15.2,8.97642102299999));
#213044=CARTESIAN_POINT('Ctrl Pts',(6.94339525799994,11.6,8.97642102299999));
#213045=CARTESIAN_POINT('Ctrl Pts',(6.94423007699994,15.2,8.97994644399999));
#213046=CARTESIAN_POINT('Ctrl Pts',(6.94423007699994,11.6,8.97994644399999));
#213047=CARTESIAN_POINT('Ctrl Pts',(6.94506322799994,15.2,8.98347699099999));
#213048=CARTESIAN_POINT('Ctrl Pts',(6.94506322799994,11.6,8.98347699099999));
#213049=CARTESIAN_POINT('Ctrl Pts',(6.94589470499994,15.2,8.98701265699999));
#213050=CARTESIAN_POINT('Ctrl Pts',(6.94589470499994,11.6,8.98701265699999));
#213051=CARTESIAN_POINT('Ctrl Pts',(6.94672450099994,15.2,8.99055343599999));
#213052=CARTESIAN_POINT('Ctrl Pts',(6.94672450099994,11.6,8.99055343599999));
#213053=CARTESIAN_POINT('Ctrl Pts',(6.94755260899995,15.2,8.99409932399998));
#213054=CARTESIAN_POINT('Ctrl Pts',(6.94755260899995,11.6,8.99409932399998));
#213055=CARTESIAN_POINT('Ctrl Pts',(6.94837901999994,15.2,8.99765031299999));
#213056=CARTESIAN_POINT('Ctrl Pts',(6.94837901999994,11.6,8.99765031299999));
#213057=CARTESIAN_POINT('Ctrl Pts',(6.94920372699994,15.2,9.00120639899999));
#213058=CARTESIAN_POINT('Ctrl Pts',(6.94920372699994,11.6,9.00120639899999));
#213059=CARTESIAN_POINT('Ctrl Pts',(6.95002672299994,15.2,9.00476757299998));
#213060=CARTESIAN_POINT('Ctrl Pts',(6.95002672299994,11.6,9.00476757299998));
#213061=CARTESIAN_POINT('Ctrl Pts',(6.95084800199994,15.2,9.00833383299998));
#213062=CARTESIAN_POINT('Ctrl Pts',(6.95084800199994,11.6,9.00833383299998));
#213063=CARTESIAN_POINT('Ctrl Pts',(6.95166755399995,15.2,9.01190517099998));
#213064=CARTESIAN_POINT('Ctrl Pts',(6.95166755399995,11.6,9.01190517099998));
#213065=CARTESIAN_POINT('Ctrl Pts',(6.95248537399995,15.2,9.01548158099999));
#213066=CARTESIAN_POINT('Ctrl Pts',(6.95248537399995,11.6,9.01548158099999));
#213067=CARTESIAN_POINT('Ctrl Pts',(6.95330145399994,15.2,9.01906305799999));
#213068=CARTESIAN_POINT('Ctrl Pts',(6.95330145399994,11.6,9.01906305799999));
#213069=CARTESIAN_POINT('Ctrl Pts',(6.95411578499994,15.2,9.02264959699998));
#213070=CARTESIAN_POINT('Ctrl Pts',(6.95411578499994,11.6,9.02264959699998));
#213071=CARTESIAN_POINT('Ctrl Pts',(6.95492836299994,15.2,9.02624118899999));
#213072=CARTESIAN_POINT('Ctrl Pts',(6.95492836299994,11.6,9.02624118899999));
#213073=CARTESIAN_POINT('Ctrl Pts',(6.95573917799994,15.2,9.02983783099998));
#213074=CARTESIAN_POINT('Ctrl Pts',(6.95573917799994,11.6,9.02983783099998));
#213075=CARTESIAN_POINT('Ctrl Pts',(6.95654822399994,15.2,9.03343951599999));
#213076=CARTESIAN_POINT('Ctrl Pts',(6.95654822399994,11.6,9.03343951599999));
#213077=CARTESIAN_POINT('Ctrl Pts',(6.95735549299994,15.2,9.03704623899999));
#213078=CARTESIAN_POINT('Ctrl Pts',(6.95735549299994,11.6,9.03704623899999));
#213079=CARTESIAN_POINT('Ctrl Pts',(6.95816097799994,15.2,9.04065799199999));
#213080=CARTESIAN_POINT('Ctrl Pts',(6.95816097799994,11.6,9.04065799199999));
#213081=CARTESIAN_POINT('Ctrl Pts',(6.95896467299994,15.2,9.04427477199999));
#213082=CARTESIAN_POINT('Ctrl Pts',(6.95896467299994,11.6,9.04427477199999));
#213083=CARTESIAN_POINT('Ctrl Pts',(6.95976656999994,15.2,9.04789657199998));
#213084=CARTESIAN_POINT('Ctrl Pts',(6.95976656999994,11.6,9.04789657199998));
#213085=CARTESIAN_POINT('Ctrl Pts',(6.96056666199994,15.2,9.05152338599999));
#213086=CARTESIAN_POINT('Ctrl Pts',(6.96056666199994,11.6,9.05152338599999));
#213087=CARTESIAN_POINT('Ctrl Pts',(6.96136494299994,15.2,9.05515520899998));
#213088=CARTESIAN_POINT('Ctrl Pts',(6.96136494299994,11.6,9.05515520899998));
#213089=CARTESIAN_POINT('Ctrl Pts',(6.96216140399994,15.2,9.05879203399999));
#213090=CARTESIAN_POINT('Ctrl Pts',(6.96216140399994,11.6,9.05879203399999));
#213091=CARTESIAN_POINT('Ctrl Pts',(6.96295603899994,15.2,9.06243385699998));
#213092=CARTESIAN_POINT('Ctrl Pts',(6.96295603899994,11.6,9.06243385699998));
#213093=CARTESIAN_POINT('Ctrl Pts',(6.96374883999994,15.2,9.06608066999999));
#213094=CARTESIAN_POINT('Ctrl Pts',(6.96374883999994,11.6,9.06608066999999));
#213095=CARTESIAN_POINT('Ctrl Pts',(6.96453979999994,15.2,9.06973246599998));
#213096=CARTESIAN_POINT('Ctrl Pts',(6.96453979999994,11.6,9.06973246599998));
#213097=CARTESIAN_POINT('Ctrl Pts',(6.96532891099994,15.2,9.07338924299999));
#213098=CARTESIAN_POINT('Ctrl Pts',(6.96532891099994,11.6,9.07338924299999));
#213099=CARTESIAN_POINT('Ctrl Pts',(6.96611616599994,15.2,9.07705099099999));
#213100=CARTESIAN_POINT('Ctrl Pts',(6.96611616599994,11.6,9.07705099099999));
#213101=CARTESIAN_POINT('Ctrl Pts',(6.96690156099994,15.2,9.08071770699999));
#213102=CARTESIAN_POINT('Ctrl Pts',(6.96690156099994,11.6,9.08071770699999));
#213103=CARTESIAN_POINT('Ctrl Pts',(6.96768508599994,15.2,9.08438938599998));
#213104=CARTESIAN_POINT('Ctrl Pts',(6.96768508599994,11.6,9.08438938599998));
#213105=CARTESIAN_POINT('Ctrl Pts',(6.96846673699994,15.2,9.08806602099999));
#213106=CARTESIAN_POINT('Ctrl Pts',(6.96846673699994,11.6,9.08806602099999));
#213107=CARTESIAN_POINT('Ctrl Pts',(6.96924650799994,15.2,9.09174760899998));
#213108=CARTESIAN_POINT('Ctrl Pts',(6.96924650799994,11.6,9.09174760899998));
#213109=CARTESIAN_POINT('Ctrl Pts',(6.97002438999994,15.2,9.09543414099998));
#213110=CARTESIAN_POINT('Ctrl Pts',(6.97002438999994,11.6,9.09543414099998));
#213111=CARTESIAN_POINT('Ctrl Pts',(6.97080037899994,15.2,9.09912561499999));
#213112=CARTESIAN_POINT('Ctrl Pts',(6.97080037899994,11.6,9.09912561499999));
#213113=CARTESIAN_POINT('Ctrl Pts',(6.97157446399994,15.2,9.10282202199999));
#213114=CARTESIAN_POINT('Ctrl Pts',(6.97157446399994,11.6,9.10282202199999));
#213115=CARTESIAN_POINT('Ctrl Pts',(6.97234663699994,15.2,9.10652335599998));
#213116=CARTESIAN_POINT('Ctrl Pts',(6.97234663699994,11.6,9.10652335599998));
#213117=CARTESIAN_POINT('Ctrl Pts',(6.97311689199994,15.2,9.11022960899999));
#213118=CARTESIAN_POINT('Ctrl Pts',(6.97311689199994,11.6,9.11022960899999));
#213119=CARTESIAN_POINT('Ctrl Pts',(6.97388521799994,15.2,9.11394077399999));
#213120=CARTESIAN_POINT('Ctrl Pts',(6.97388521799994,11.6,9.11394077399999));
#213121=CARTESIAN_POINT('Ctrl Pts',(6.97465160699994,15.2,9.11765684499999));
#213122=CARTESIAN_POINT('Ctrl Pts',(6.97465160699994,11.6,9.11765684499999));
#213123=CARTESIAN_POINT('Ctrl Pts',(6.97541605599994,15.2,9.12137781699998));
#213124=CARTESIAN_POINT('Ctrl Pts',(6.97541605599994,11.6,9.12137781699998));
#213125=CARTESIAN_POINT('Ctrl Pts',(6.97617855799994,15.2,9.12510368599998));
#213126=CARTESIAN_POINT('Ctrl Pts',(6.97617855799994,11.6,9.12510368599998));
#213127=CARTESIAN_POINT('Ctrl Pts',(6.97693911099995,15.2,9.12883444899999));
#213128=CARTESIAN_POINT('Ctrl Pts',(6.97693911099995,11.6,9.12883444899999));
#213129=CARTESIAN_POINT('Ctrl Pts',(6.97769771099994,15.2,9.13257010499999));
#213130=CARTESIAN_POINT('Ctrl Pts',(6.97769771099994,11.6,9.13257010499999));
#213131=CARTESIAN_POINT('Ctrl Pts',(6.97830303199994,15.2,9.13556254299999));
#213132=CARTESIAN_POINT('Ctrl Pts',(6.97830303199994,11.6,9.13556254299999));
#213133=CARTESIAN_POINT('Ctrl Pts',(6.97875614299994,15.2,9.13780907399998));
#213134=CARTESIAN_POINT('Ctrl Pts',(6.97875614299994,11.6,9.13780907399998));
#213135=CARTESIAN_POINT('Ctrl Pts',(6.97905782599994,15.2,9.13930773799999));
#213136=CARTESIAN_POINT('Ctrl Pts',(6.97905782599994,11.6,9.13930773799999));
#213137=CARTESIAN_POINT('Ctrl Pts',(6.97920857099994,15.2,9.14005731499999));
#213138=CARTESIAN_POINT('Ctrl Pts',(6.97920857099994,11.6,9.14005731499999));
#213139=CARTESIAN_POINT('Ctrl Pts',(6.57080831899994,15.2,8.02901631899999));
#213140=CARTESIAN_POINT('Ctrl Pts',(6.57181685709479,15.2,8.03049109922884));
#213141=CARTESIAN_POINT('Ctrl Pts',(6.57285322895298,15.2,8.03201610932772));
#213142=CARTESIAN_POINT('Ctrl Pts',(6.57391635217513,15.2,8.03359089408577));
#213143=CARTESIAN_POINT('Ctrl Pts',(6.57498460231485,15.2,8.03517327325192));
#213144=CARTESIAN_POINT('Ctrl Pts',(6.57607986599813,15.2,8.03680591632581));
#213145=CARTESIAN_POINT('Ctrl Pts',(6.57720107836676,15.2,8.03848839142112));
#213146=CARTESIAN_POINT('Ctrl Pts',(6.57850915931071,15.2,8.04045127880305));
#213147=CARTESIAN_POINT('Ctrl Pts',(6.57985256090342,15.2,8.0424819924996));
#213148=CARTESIAN_POINT('Ctrl Pts',(6.58122965137125,15.2,8.04457986679557));
#213149=CARTESIAN_POINT('Ctrl Pts',(6.58241001476725,15.2,8.04637804497357));
#213150=CARTESIAN_POINT('Ctrl Pts',(6.5836151303474,15.2,8.04822556534917));
#213151=CARTESIAN_POINT('Ctrl Pts',(6.58484400289384,15.2,8.05012201771681));
#213152=CARTESIAN_POINT('Ctrl Pts',(6.58607287532866,15.2,8.05201846991219));
#213153=CARTESIAN_POINT('Ctrl Pts',(6.5873255059879,15.2,8.05396385292234));
#213154=CARTESIAN_POINT('Ctrl Pts',(6.5886009275249,15.2,8.05595776701655));
#213155=CARTESIAN_POINT('Ctrl Pts',(6.58987634906188,15.2,8.05795168111077));
#213156=CARTESIAN_POINT('Ctrl Pts',(6.59117456239721,15.2,8.05999412543044));
#213157=CARTESIAN_POINT('Ctrl Pts',(6.59249462916393,15.2,8.06208470653945));
#213158=CARTESIAN_POINT('Ctrl Pts',(6.59381469605055,15.2,8.06417528783836));
#213159=CARTESIAN_POINT('Ctrl Pts',(6.59515661597275,15.2,8.06631400529914));
#213160=CARTESIAN_POINT('Ctrl Pts',(6.59651947688179,15.2,8.06850047375489));
#213161=CARTESIAN_POINT('Ctrl Pts',(6.59788233766702,15.2,8.07068694201203));
#213162=CARTESIAN_POINT('Ctrl Pts',(6.59926613977845,15.2,8.07292116150669));
#213163=CARTESIAN_POINT('Ctrl Pts',(6.60066999473389,15.2,8.07520275276762));
#213164=CARTESIAN_POINT('Ctrl Pts',(6.60207384968932,15.2,8.07748434402855));
#213165=CARTESIAN_POINT('Ctrl Pts',(6.60349775834128,15.2,8.07981330796732));
#213166=CARTESIAN_POINT('Ctrl Pts',(6.60494085645468,15.2,8.08218927312894));
#213167=CARTESIAN_POINT('Ctrl Pts',(6.60638395469915,15.2,8.08456523850639));
#213168=CARTESIAN_POINT('Ctrl Pts',(6.6078462442627,15.2,8.08698820426467));
#213169=CARTESIAN_POINT('Ctrl Pts',(6.60932688067797,15.2,8.08945780673577));
#213170=CARTESIAN_POINT('Ctrl Pts',(6.61080751695876,15.2,8.09192740898253));
#213171=CARTESIAN_POINT('Ctrl Pts',(6.61230650277865,15.2,8.09444364778919));
#213172=CARTESIAN_POINT('Ctrl Pts',(6.61382301980764,15.2,8.09700616494809));
#213173=CARTESIAN_POINT('Ctrl Pts',(6.61533953683664,15.2,8.09956868210699));
#213174=CARTESIAN_POINT('Ctrl Pts',(6.61687358203922,15.2,8.10217747604554));
#213175=CARTESIAN_POINT('Ctrl Pts',(6.6184243611488,15.2,8.10483219636375));
#213176=CARTESIAN_POINT('Ctrl Pts',(6.6199751402584,15.2,8.10748691668196));
#213177=CARTESIAN_POINT('Ctrl Pts',(6.62154264930262,15.2,8.11018756270347));
#213178=CARTESIAN_POINT('Ctrl Pts',(6.62312611457732,15.2,8.11293378793391));
#213179=CARTESIAN_POINT('Ctrl Pts',(6.62523740180204,15.2,8.1165954219071));
#213180=CARTESIAN_POINT('Ctrl Pts',(6.62737704680761,15.2,8.12033808468612));
#213181=CARTESIAN_POINT('Ctrl Pts',(6.62954326492701,15.2,8.12416097078744));
#213182=CARTESIAN_POINT('Ctrl Pts',(6.631167928369,15.2,8.127028135103));
#213183=CARTESIAN_POINT('Ctrl Pts',(6.63280753706155,15.2,8.12994042577014));
#213184=CARTESIAN_POINT('Ctrl Pts',(6.63446135959234,15.2,8.13289750725959));
#213185=CARTESIAN_POINT('Ctrl Pts',(6.63611518212314,15.2,8.13585458874903));
#213186=CARTESIAN_POINT('Ctrl Pts',(6.63778321817001,15.2,8.13885646332167));
#213187=CARTESIAN_POINT('Ctrl Pts',(6.63946474894167,15.2,8.1419027997924));
#213188=CARTESIAN_POINT('Ctrl Pts',(6.64114627986605,15.2,8.14494913653984));
#213189=CARTESIAN_POINT('Ctrl Pts',(6.64284130675046,15.2,8.14803993675109));
#213190=CARTESIAN_POINT('Ctrl Pts',(6.64454913242775,15.2,8.15117487459163));
#213191=CARTESIAN_POINT('Ctrl Pts',(6.64625695794992,15.2,8.15430981214742));
#213192=CARTESIAN_POINT('Ctrl Pts',(6.64797757785682,15.2,8.15748888975759));
#213193=CARTESIAN_POINT('Ctrl Pts',(6.64971031262775,15.2,8.16071178614242));
#213194=CARTESIAN_POINT('Ctrl Pts',(6.65144304739867,15.2,8.16393468252726));
#213195=CARTESIAN_POINT('Ctrl Pts',(6.65318789496859,15.2,8.16720139724187));
#213196=CARTESIAN_POINT('Ctrl Pts',(6.65494418790425,15.2,8.17051161578635));
#213197=CARTESIAN_POINT('Ctrl Pts',(6.65670048083992,15.2,8.17382183433081));
#213198=CARTESIAN_POINT('Ctrl Pts',(6.65846822131309,15.2,8.17717555743936));
#213199=CARTESIAN_POINT('Ctrl Pts',(6.66024675233107,15.2,8.18057247281299));
#213200=CARTESIAN_POINT('Ctrl Pts',(6.66202528351059,15.2,8.18396938849518));
#213201=CARTESIAN_POINT('Ctrl Pts',(6.66381460970786,15.2,8.18740949648156));
#213202=CARTESIAN_POINT('Ctrl Pts',(6.66561408988971,15.2,8.19089249117325));
#213203=CARTESIAN_POINT('Ctrl Pts',(6.66741356990811,15.2,8.19437548554857));
#213204=CARTESIAN_POINT('Ctrl Pts',(6.66922320412363,15.2,8.1979013640035));
#213205=CARTESIAN_POINT('Ctrl Pts',(6.67104237023243,15.2,8.20146982647329));
#213206=CARTESIAN_POINT('Ctrl Pts',(6.67255834204486,15.2,8.20444354530617));
#213207=CARTESIAN_POINT('Ctrl Pts',(6.67408093153883,15.2,8.20744683568326));
#213208=CARTESIAN_POINT('Ctrl Pts',(6.67560978744159,15.2,8.2104795229749));
#213209=CARTESIAN_POINT('Ctrl Pts',(6.67713864334436,15.2,8.21351221026653));
#213210=CARTESIAN_POINT('Ctrl Pts',(6.67867376366598,15.2,8.21657429548192));
#213211=CARTESIAN_POINT('Ctrl Pts',(6.68021480145077,15.2,8.21966560750993));
#213212=CARTESIAN_POINT('Ctrl Pts',(6.68175583923556,15.2,8.22275691953794));
#213213=CARTESIAN_POINT('Ctrl Pts',(6.68330279499564,15.2,8.22587745733786));
#213214=CARTESIAN_POINT('Ctrl Pts',(6.6848553261765,15.2,8.2290270504644));
#213215=CARTESIAN_POINT('Ctrl Pts',(6.68671836352583,15.2,8.23280656207892));
#213216=CARTESIAN_POINT('Ctrl Pts',(6.68858943118284,15.2,8.23662791582342));
#213217=CARTESIAN_POINT('Ctrl Pts',(6.69046794761425,15.2,8.24049081826456));
#213218=CARTESIAN_POINT('Ctrl Pts',(6.69203337803064,15.2,8.24370990374914));
#213219=CARTESIAN_POINT('Ctrl Pts',(6.69360398287526,15.2,8.24695784379444));
#213220=CARTESIAN_POINT('Ctrl Pts',(6.69517943475741,15.2,8.25023447103147));
#213221=CARTESIAN_POINT('Ctrl Pts',(6.69675488663955,15.2,8.25351109826849));
#213222=CARTESIAN_POINT('Ctrl Pts',(6.69833518289994,15.2,8.25681641326103));
#213223=CARTESIAN_POINT('Ctrl Pts',(6.69992000248326,15.2,8.26015025048324));
#213224=CARTESIAN_POINT('Ctrl Pts',(6.70150482206659,15.2,8.26348408770544));
#213225=CARTESIAN_POINT('Ctrl Pts',(6.70309416312688,15.2,8.26684644767516));
#213226=CARTESIAN_POINT('Ctrl Pts',(6.7046877110508,15.2,8.2702371665101));
#213227=CARTESIAN_POINT('Ctrl Pts',(6.70659996849003,15.2,8.27430602896418));
#213228=CARTESIAN_POINT('Ctrl Pts',(6.70851828215691,15.2,8.2784157278098));
#213229=CARTESIAN_POINT('Ctrl Pts',(6.71044211267011,15.2,8.28256598432389));
#213230=CARTESIAN_POINT('Ctrl Pts',(6.71204530482267,15.2,8.28602453154462));
#213231=CARTESIAN_POINT('Ctrl Pts',(6.71365232831704,15.2,8.28951124262168));
#213232=CARTESIAN_POINT('Ctrl Pts',(6.71526287796963,15.2,8.29302595824522));
#213233=CARTESIAN_POINT('Ctrl Pts',(6.71687342762222,15.2,8.29654067386875));
#213234=CARTESIAN_POINT('Ctrl Pts',(6.71848750324171,15.2,8.30008339392071));
#213235=CARTESIAN_POINT('Ctrl Pts',(6.72010480449905,15.2,8.30365395796463));
#213236=CARTESIAN_POINT('Ctrl Pts',(6.72172210575639,15.2,8.30722452200856));
#213237=CARTESIAN_POINT('Ctrl Pts',(6.72334263070549,15.2,8.31082293178325));
#213238=CARTESIAN_POINT('Ctrl Pts',(6.72496608619161,15.2,8.31444902824158));
#213239=CARTESIAN_POINT('Ctrl Pts',(6.72658954167772,15.2,8.31807512469992));
#213240=CARTESIAN_POINT('Ctrl Pts',(6.72821592633883,15.2,8.32172890851102));
#213241=CARTESIAN_POINT('Ctrl Pts',(6.72984494869994,15.2,8.32541022177491));
#213242=CARTESIAN_POINT('Ctrl Pts',(6.73147397106104,15.2,8.32909153503879));
#213243=CARTESIAN_POINT('Ctrl Pts',(6.7331056319434,15.2,8.33280038045713));
#213244=CARTESIAN_POINT('Ctrl Pts',(6.7347396442425,15.2,8.33653659950195));
#213245=CARTESIAN_POINT('Ctrl Pts',(6.73637365654159,15.2,8.34027281854678));
#213246=CARTESIAN_POINT('Ctrl Pts',(6.73801002092921,15.2,8.34403641308545));
#213247=CARTESIAN_POINT('Ctrl Pts',(6.73964845558211,15.2,8.347827227948));
#213248=CARTESIAN_POINT('Ctrl Pts',(6.741286890235,15.2,8.35161804281056));
#213249=CARTESIAN_POINT('Ctrl Pts',(6.74292739366837,15.2,8.355436079239));
#213250=CARTESIAN_POINT('Ctrl Pts',(6.74456969005736,15.2,8.35928118326822));
#213251=CARTESIAN_POINT('Ctrl Pts',(6.74588352706115,15.2,8.36235726624014));
#213252=CARTESIAN_POINT('Ctrl Pts',(6.7471985122176,15.2,8.36545067278518));
#213253=CARTESIAN_POINT('Ctrl Pts',(6.74851450350898,15.2,8.36856132507363));
#213254=CARTESIAN_POINT('Ctrl Pts',(6.74983049497967,15.2,8.3716719777859));
#213255=CARTESIAN_POINT('Ctrl Pts',(6.75114749275803,15.2,8.37479987469578));
#213256=CARTESIAN_POINT('Ctrl Pts',(6.75246536060769,15.2,8.37794494075719));
#213257=CARTESIAN_POINT('Ctrl Pts',(6.75378322827778,15.2,8.38109000639009));
#213258=CARTESIAN_POINT('Ctrl Pts',(6.75510196406992,15.2,8.38425223983344));
#213259=CARTESIAN_POINT('Ctrl Pts',(6.75642143251754,15.2,8.38743156473844));
#213260=CARTESIAN_POINT('Ctrl Pts',(6.75774090114493,15.2,8.39061089007662));
#213261=CARTESIAN_POINT('Ctrl Pts',(6.75906110102841,15.2,8.39380730742622));
#213262=CARTESIAN_POINT('Ctrl Pts',(6.76038189955084,15.2,8.39702073822711));
#213263=CARTESIAN_POINT('Ctrl Pts',(6.76170269789331,15.2,8.40023416859018));
#213264=CARTESIAN_POINT('Ctrl Pts',(6.76302409172527,15.2,8.40346461550287));
#213265=CARTESIAN_POINT('Ctrl Pts',(6.76434595028382,15.2,8.40671199923564));
#213266=CARTESIAN_POINT('Ctrl Pts',(6.76566780902246,15.2,8.40995938341087));
#213267=CARTESIAN_POINT('Ctrl Pts',(6.76699013193896,15.2,8.41322370691553));
#213268=CARTESIAN_POINT('Ctrl Pts',(6.76831278723328,15.2,8.41650489298325));
#213269=CARTESIAN_POINT('Ctrl Pts',(6.76963544252758,15.2,8.41978607905095));
#213270=CARTESIAN_POINT('Ctrl Pts',(6.77095842881082,15.2,8.4230841286762));
#213271=CARTESIAN_POINT('Ctrl Pts',(6.77228161821629,15.2,8.42639896485858));
#213272=CARTESIAN_POINT('Ctrl Pts',(6.77360480744148,15.2,8.42971380058932));
#213273=CARTESIAN_POINT('Ctrl Pts',(6.77492819831234,15.2,8.43304542463676));
#213274=CARTESIAN_POINT('Ctrl Pts',(6.77625166276571,15.2,8.43639376098931));
#213275=CARTESIAN_POINT('Ctrl Pts',(6.77823685953593,15.2,8.44141626574624));
#213276=CARTESIAN_POINT('Ctrl Pts',(6.78022222002234,15.2,8.44647637519039));
#213277=CARTESIAN_POINT('Ctrl Pts',(6.78220731978357,15.2,8.45157383591931));
#213278=CARTESIAN_POINT('Ctrl Pts',(6.7838615696447,15.2,8.45582172001441));
#213279=CARTESIAN_POINT('Ctrl Pts',(6.78551563503645,15.2,8.46009554375456));
#213280=CARTESIAN_POINT('Ctrl Pts',(6.78716927609131,15.2,8.46439516146755));
#213281=CARTESIAN_POINT('Ctrl Pts',(6.7884921890073,15.2,8.4678348558254));
#213282=CARTESIAN_POINT('Ctrl Pts',(6.78981483008878,15.2,8.4712910599492));
#213283=CARTESIAN_POINT('Ctrl Pts',(6.79113707488304,15.2,8.47476369925064));
#213284=CARTESIAN_POINT('Ctrl Pts',(6.79245931949714,15.2,8.47823633807893));
#213285=CARTESIAN_POINT('Ctrl Pts',(6.79378116923355,15.2,8.48172541230115));
#213286=CARTESIAN_POINT('Ctrl Pts',(6.79510250129224,15.2,8.48523084740179));
#213287=CARTESIAN_POINT('Ctrl Pts',(6.79675416650063,15.2,8.4896126416358));
#213288=CARTESIAN_POINT('Ctrl Pts',(6.79840502414815,15.2,8.4940200027491));
#213289=CARTESIAN_POINT('Ctrl Pts',(6.80005483930009,15.2,8.49845278776043));
#213290=CARTESIAN_POINT('Ctrl Pts',(6.80170465445202,15.2,8.50288557277178));
#213291=CARTESIAN_POINT('Ctrl Pts',(6.80335342639768,15.2,8.50734378141373));
#213292=CARTESIAN_POINT('Ctrl Pts',(6.80500092563386,15.2,8.51182727148185));
#213293=CARTESIAN_POINT('Ctrl Pts',(6.80664842487003,15.2,8.51631076154996));
#213294=CARTESIAN_POINT('Ctrl Pts',(6.80829465035342,15.2,8.52081953613825));
#213295=CARTESIAN_POINT('Ctrl Pts',(6.80993937465904,15.2,8.52535345176188));
#213296=CARTESIAN_POINT('Ctrl Pts',(6.81125515417524,15.2,8.52898058445846));
#213297=CARTESIAN_POINT('Ctrl Pts',(6.81256997178956,15.2,8.53262380823073));
#213298=CARTESIAN_POINT('Ctrl Pts',(6.81388371464891,15.2,8.53628305128099));
#213299=CARTESIAN_POINT('Ctrl Pts',(6.81519745732926,15.2,8.53994229383269));
#213300=CARTESIAN_POINT('Ctrl Pts',(6.81651012421375,15.2,8.54361755584278));
#213301=CARTESIAN_POINT('Ctrl Pts',(6.81782160038439,15.2,8.54730876670666));
#213302=CARTESIAN_POINT('Ctrl Pts',(6.81913307673373,15.2,8.55099997807347));
#213303=CARTESIAN_POINT('Ctrl Pts',(6.82044336308847,15.2,8.55470713570607));
#213304=CARTESIAN_POINT('Ctrl Pts',(6.82175234788195,15.2,8.5584301730211));
#213305=CARTESIAN_POINT('Ctrl Pts',(6.82338857878461,15.2,8.56308396941128));
#213306=CARTESIAN_POINT('Ctrl Pts',(6.82502277306912,15.2,8.56776257169818));
#213307=CARTESIAN_POINT('Ctrl Pts',(6.82665471516439,15.2,8.572465846796));
#213308=CARTESIAN_POINT('Ctrl Pts',(6.82796026873388,15.2,8.57622846656667));
#213309=CARTESIAN_POINT('Ctrl Pts',(6.82926438011927,15.2,8.58000687479833));
#213310=CARTESIAN_POINT('Ctrl Pts',(6.83056694140179,15.2,8.58380100243157));
#213311=CARTESIAN_POINT('Ctrl Pts',(6.83186950286176,15.2,8.58759513058177));
#213312=CARTESIAN_POINT('Ctrl Pts',(6.83317051068823,15.2,8.59140497740054));
#213313=CARTESIAN_POINT('Ctrl Pts',(6.83446986081449,15.2,8.59523047355448));
#213314=CARTESIAN_POINT('Ctrl Pts',(6.83576921076371,15.2,8.59905596918719));
#213315=CARTESIAN_POINT('Ctrl Pts',(6.8370669000966,15.2,8.60289711458346));
#213316=CARTESIAN_POINT('Ctrl Pts',(6.8383628210464,15.2,8.60675383887768));
#213317=CARTESIAN_POINT('Ctrl Pts',(6.83965874217276,15.2,8.61061056369739));
#213318=CARTESIAN_POINT('Ctrl Pts',(6.84095289646064,15.2,8.61448286745074));
#213319=CARTESIAN_POINT('Ctrl Pts',(6.84224517725917,15.2,8.61837068223592));
#213320=CARTESIAN_POINT('Ctrl Pts',(6.84353745788162,15.2,8.62225849649138));
#213321=CARTESIAN_POINT('Ctrl Pts',(6.84482786305553,15.2,8.62616182069504));
#213322=CARTESIAN_POINT('Ctrl Pts',(6.84611629050596,15.2,8.63008058631755));
#213323=CARTESIAN_POINT('Ctrl Pts',(6.84772682495066,15.2,8.63497904374613));
#213324=CARTESIAN_POINT('Ctrl Pts',(6.84933426686765,15.2,8.6399016274827));
#213325=CARTESIAN_POINT('Ctrl Pts',(6.85093841304846,15.2,8.64484820407792));
#213326=CARTESIAN_POINT('Ctrl Pts',(6.85254255922927,15.2,8.64979478067313));
#213327=CARTESIAN_POINT('Ctrl Pts',(6.85414341035111,15.2,8.65476534971123));
#213328=CARTESIAN_POINT('Ctrl Pts',(6.85574076584785,15.2,8.65975977815357));
#213329=CARTESIAN_POINT('Ctrl Pts',(6.85701865031487,15.2,8.6637553211252));
#213330=CARTESIAN_POINT('Ctrl Pts',(6.85829429729866,15.2,8.66776613396156));
#213331=CARTESIAN_POINT('Ctrl Pts',(6.85956760631236,15.2,8.67179214757087));
#213332=CARTESIAN_POINT('Ctrl Pts',(6.86115924249273,15.2,8.67682466430823));
#213333=CARTESIAN_POINT('Ctrl Pts',(6.86274722550929,15.2,8.68188093511996));
#213334=CARTESIAN_POINT('Ctrl Pts',(6.86433135766187,15.2,8.6869608243573));
#213335=CARTESIAN_POINT('Ctrl Pts',(6.86559866328032,15.2,8.69102473541494));
#213336=CARTESIAN_POINT('Ctrl Pts',(6.86686350589278,15.2,8.69510376413461));
#213337=CARTESIAN_POINT('Ctrl Pts',(6.86812578557511,15.2,8.69919784261427));
#213338=CARTESIAN_POINT('Ctrl Pts',(6.869703635307,15.2,8.70431544113219));
#213339=CARTESIAN_POINT('Ctrl Pts',(6.87127748189704,15.2,8.7094565538135));
#213340=CARTESIAN_POINT('Ctrl Pts',(6.87284713314727,15.2,8.71462104964565));
#213341=CARTESIAN_POINT('Ctrl Pts',(6.87410285421589,15.2,8.71875264653653));
#213342=CARTESIAN_POINT('Ctrl Pts',(6.87535588956473,15.2,8.7228992084125));
#213343=CARTESIAN_POINT('Ctrl Pts',(6.87660614457714,15.2,8.72706066864027));
#213344=CARTESIAN_POINT('Ctrl Pts',(6.87785639941919,15.2,8.73122212830105));
#213345=CARTESIAN_POINT('Ctrl Pts',(6.87910387255866,15.2,8.73539848700974));
#213346=CARTESIAN_POINT('Ctrl Pts',(6.88034846885267,15.2,8.73958967687517));
#213347=CARTESIAN_POINT('Ctrl Pts',(6.88159306531626,15.2,8.74378086731166));
#213348=CARTESIAN_POINT('Ctrl Pts',(6.88283478369778,15.2,8.74798689018359));
#213349=CARTESIAN_POINT('Ctrl Pts',(6.8840735313762,15.2,8.75220767713678));
#213350=CARTESIAN_POINT('Ctrl Pts',(6.88531227888583,15.2,8.7564284635149));
#213351=CARTESIAN_POINT('Ctrl Pts',(6.88654805374886,15.2,8.76066401515675));
#213352=CARTESIAN_POINT('Ctrl Pts',(6.88778076398174,15.2,8.76491426553001));
#213353=CARTESIAN_POINT('Ctrl Pts',(6.88901347438257,15.2,8.76916451648237));
#213354=CARTESIAN_POINT('Ctrl Pts',(6.89024312013394,15.2,8.77342946685009));
#213355=CARTESIAN_POINT('Ctrl Pts',(6.89146960598412,15.2,8.77770904976951));
#213356=CARTESIAN_POINT('Ctrl Pts',(6.89238947028821,15.2,8.78091873666753));
#213357=CARTESIAN_POINT('Ctrl Pts',(6.89330755882824,15.2,8.78413665529961));
#213358=CARTESIAN_POINT('Ctrl Pts',(6.89422383204912,15.2,8.78736277623867));
#213359=CARTESIAN_POINT('Ctrl Pts',(6.8957509541394,15.2,8.7927396446658));
#213360=CARTESIAN_POINT('Ctrl Pts',(6.89727303364441,15.2,8.79813929989994));
#213361=CARTESIAN_POINT('Ctrl Pts',(6.89878989253329,15.2,8.80356161406659));
#213362=CARTESIAN_POINT('Ctrl Pts',(6.89970000783355,15.2,8.80681500244837));
#213363=CARTESIAN_POINT('Ctrl Pts',(6.90060824381724,15.2,8.81007654816319));
#213364=CARTESIAN_POINT('Ctrl Pts',(6.9015145626178,15.2,8.81334622262701));
#213365=CARTESIAN_POINT('Ctrl Pts',(6.90242088141836,15.2,8.81661589709082));
#213366=CARTESIAN_POINT('Ctrl Pts',(6.90332528329616,15.2,8.81989370130379));
#213367=CARTESIAN_POINT('Ctrl Pts',(6.90422773005867,15.2,8.8231796078476));
#213368=CARTESIAN_POINT('Ctrl Pts',(6.90513017682119,15.2,8.82646551439141));
#213369=CARTESIAN_POINT('Ctrl Pts',(6.90603066735313,15.2,8.82975952263449));
#213370=CARTESIAN_POINT('Ctrl Pts',(6.90692916702908,15.2,8.83306160547174));
#213371=CARTESIAN_POINT('Ctrl Pts',(6.90782766686827,15.2,8.83636368890887));
#213372=CARTESIAN_POINT('Ctrl Pts',(6.90872417394857,15.2,8.83967384625665));
#213373=CARTESIAN_POINT('Ctrl Pts',(6.90961865095329,15.2,8.84299205119831));
#213374=CARTESIAN_POINT('Ctrl Pts',(6.91051312779551,15.2,8.84631025553717));
#213375=CARTESIAN_POINT('Ctrl Pts',(6.91140557597951,15.2,8.84963650730062));
#213376=CARTESIAN_POINT('Ctrl Pts',(6.91229595682197,15.2,8.85297077909683));
#213377=CARTESIAN_POINT('Ctrl Pts',(6.91318633766444,15.2,8.85630505089304));
#213378=CARTESIAN_POINT('Ctrl Pts',(6.91407465274561,15.2,8.85964734174278));
#213379=CARTESIAN_POINT('Ctrl Pts',(6.91496086405076,15.2,8.86299762601131));
#213380=CARTESIAN_POINT('Ctrl Pts',(6.91614247907064,15.2,8.86746467149981));
#213381=CARTESIAN_POINT('Ctrl Pts',(6.91732035466747,15.2,8.87194592513662));
#213382=CARTESIAN_POINT('Ctrl Pts',(6.91849440684967,15.2,8.87644132348994));
#213383=CARTESIAN_POINT('Ctrl Pts',(6.91937494618627,15.2,8.87981287302055));
#213384=CARTESIAN_POINT('Ctrl Pts',(6.92025333254726,15.2,8.88319237921167));
#213385=CARTESIAN_POINT('Ctrl Pts',(6.92112953246597,15.2,8.88657981424674));
#213386=CARTESIAN_POINT('Ctrl Pts',(6.9220057322255,15.2,8.88996724866642));
#213387=CARTESIAN_POINT('Ctrl Pts',(6.92287974452682,15.2,8.89336261267731));
#213388=CARTESIAN_POINT('Ctrl Pts',(6.92375153336995,15.2,8.89676587859603));
#213389=CARTESIAN_POINT('Ctrl Pts',(6.92520451482796,15.2,8.90243798866665));
#213390=CARTESIAN_POINT('Ctrl Pts',(6.92665132191786,15.2,8.90813204995426));
#213391=CARTESIAN_POINT('Ctrl Pts',(6.92809178768382,15.2,8.91384793683853));
#213392=CARTESIAN_POINT('Ctrl Pts',(6.92895606711199,15.2,8.9172774688445));
#213393=CARTESIAN_POINT('Ctrl Pts',(6.92981806504173,15.2,8.92071485781676));
#213394=CARTESIAN_POINT('Ctrl Pts',(6.93067774584363,15.2,8.92416007760892));
#213395=CARTESIAN_POINT('Ctrl Pts',(6.93153742664552,15.2,8.92760529740109));
#213396=CARTESIAN_POINT('Ctrl Pts',(6.93239478969769,15.2,8.93105834714234));
#213397=CARTESIAN_POINT('Ctrl Pts',(6.93324980099996,15.2,8.93451920051659));
#213398=CARTESIAN_POINT('Ctrl Pts',(6.93410481230223,15.2,8.93798005389085));
#213399=CARTESIAN_POINT('Ctrl Pts',(6.93495747183793,15.2,8.94144871098147));
#213400=CARTESIAN_POINT('Ctrl Pts',(6.93580774472391,15.2,8.94492514485446));
#213401=CARTESIAN_POINT('Ctrl Pts',(6.93665801760989,15.2,8.94840157872746));
#213402=CARTESIAN_POINT('Ctrl Pts',(6.93750590432937,15.2,8.95188578966663));
#213403=CARTESIAN_POINT('Ctrl Pts',(6.93835136975731,15.2,8.95537775053869));
#213404=CARTESIAN_POINT('Ctrl Pts',(6.93919683533885,15.2,8.95886971204513));
#213405=CARTESIAN_POINT('Ctrl Pts',(6.94003988016138,15.2,8.9623694235371));
#213406=CARTESIAN_POINT('Ctrl Pts',(6.94088047061654,15.2,8.96587685900623));
#213407=CARTESIAN_POINT('Ctrl Pts',(6.941721060919,15.2,8.96938429383817));
#213408=CARTESIAN_POINT('Ctrl Pts',(6.94255919633385,15.2,8.97289945139939));
#213409=CARTESIAN_POINT('Ctrl Pts',(6.94339484363661,15.2,8.97642230644826));
#213410=CARTESIAN_POINT('Ctrl Pts',(6.94423049093937,15.2,8.97994516149713));
#213411=CARTESIAN_POINT('Ctrl Pts',(6.94506364895419,15.2,8.98347571369694));
#213412=CARTESIAN_POINT('Ctrl Pts',(6.94589428484046,15.2,8.9870139356524));
#213413=CARTESIAN_POINT('Ctrl Pts',(6.94672492072673,15.2,8.99055215760786));
#213414=CARTESIAN_POINT('Ctrl Pts',(6.9475530356133,15.2,8.99409805037904));
#213415=CARTESIAN_POINT('Ctrl Pts',(6.94837859399996,15.2,8.99765158720827));
#213416=CARTESIAN_POINT('Ctrl Pts',(6.94920415238664,15.2,9.00120512403751));
#213417=CARTESIAN_POINT('Ctrl Pts',(6.95002715535674,15.2,9.00476630384141));
#213418=CARTESIAN_POINT('Ctrl Pts',(6.95084757020216,15.2,9.00833510212773));
#213419=CARTESIAN_POINT('Ctrl Pts',(6.95194145676207,15.2,9.01309350027503));
#213420=CARTESIAN_POINT('Ctrl Pts',(6.95303074152221,15.2,9.01786544049333));
#213421=CARTESIAN_POINT('Ctrl Pts',(6.95411534685732,15.2,9.02265086099441));
#213422=CARTESIAN_POINT('Ctrl Pts',(6.95492880078478,15.2,9.02623992604421));
#213423=CARTESIAN_POINT('Ctrl Pts',(6.95573962300094,15.2,9.0298365725399));
#213424=CARTESIAN_POINT('Ctrl Pts',(6.95654777984634,15.2,9.03344077586792));
#213425=CARTESIAN_POINT('Ctrl Pts',(6.95789470797095,15.2,9.03944778163286));
#213426=CARTESIAN_POINT('Ctrl Pts',(6.95923423285408,15.2,9.04547577529457));
#213427=CARTESIAN_POINT('Ctrl Pts',(6.96056620931203,15.2,9.05152463862899));
#213428=CARTESIAN_POINT('Ctrl Pts',(6.96136539515776,15.2,9.05515395649778));
#213429=CARTESIAN_POINT('Ctrl Pts',(6.96216186315926,15.2,9.05879078725241));
#213430=CARTESIAN_POINT('Ctrl Pts',(6.96295558050902,15.2,9.06243510451158));
#213431=CARTESIAN_POINT('Ctrl Pts',(6.96374929785877,15.2,9.06607942177076));
#213432=CARTESIAN_POINT('Ctrl Pts',(6.96454026450762,15.2,9.06973122396299));
#213433=CARTESIAN_POINT('Ctrl Pts',(6.96532844702425,15.2,9.07339048580495));
#213434=CARTESIAN_POINT('Ctrl Pts',(6.96637935714186,15.2,9.0782695020374));
#213435=CARTESIAN_POINT('Ctrl Pts',(6.96742531992227,15.2,9.08316177839994));
#213436=CARTESIAN_POINT('Ctrl Pts',(6.96846626714516,15.2,9.08806726000199));
#213437=CARTESIAN_POINT('Ctrl Pts',(6.96950721422621,15.2,9.09297274093567));
#213438=CARTESIAN_POINT('Ctrl Pts',(6.97054314812736,15.2,9.09789142717872));
#213439=CARTESIAN_POINT('Ctrl Pts',(6.97157398593231,15.2,9.10282325333021));
#213440=CARTESIAN_POINT('Ctrl Pts',(6.97234711432113,15.2,9.10652212311181));
#213441=CARTESIAN_POINT('Ctrl Pts',(6.97311737659069,15.2,9.11022838219846));
#213442=CARTESIAN_POINT('Ctrl Pts',(6.97388473364314,15.2,9.11394199978984));
#213443=CARTESIAN_POINT('Ctrl Pts',(6.97465209069559,15.2,9.11765561738122));
#213444=CARTESIAN_POINT('Ctrl Pts',(6.97541654334455,15.2,9.12137659300695));
#213445=CARTESIAN_POINT('Ctrl Pts',(6.97617807056728,15.2,9.12510490870382));
#213446=CARTESIAN_POINT('Ctrl Pts',(6.97719344028981,15.2,9.13007599675117));
#213447=CARTESIAN_POINT('Ctrl Pts',(6.97820360405943,15.2,9.13506013363826));
#213448=CARTESIAN_POINT('Ctrl Pts',(6.97920857099994,15.2,9.14005731499999));
#213449=CARTESIAN_POINT('Ctrl Pts',(6.57080831899994,12.2,8.02901631899999));
#213450=CARTESIAN_POINT('Ctrl Pts',(6.57181685709479,12.2,8.03049109922884));
#213451=CARTESIAN_POINT('Ctrl Pts',(6.57285322895298,12.2,8.03201610932772));
#213452=CARTESIAN_POINT('Ctrl Pts',(6.57391635217513,12.2,8.03359089408577));
#213453=CARTESIAN_POINT('Ctrl Pts',(6.57498460231485,12.2,8.03517327325192));
#213454=CARTESIAN_POINT('Ctrl Pts',(6.57607986599813,12.2,8.03680591632581));
#213455=CARTESIAN_POINT('Ctrl Pts',(6.57720107836676,12.2,8.03848839142112));
#213456=CARTESIAN_POINT('Ctrl Pts',(6.57850915931071,12.2,8.04045127880305));
#213457=CARTESIAN_POINT('Ctrl Pts',(6.57985256090342,12.2,8.0424819924996));
#213458=CARTESIAN_POINT('Ctrl Pts',(6.58122965137125,12.2,8.04457986679557));
#213459=CARTESIAN_POINT('Ctrl Pts',(6.58241001476725,12.2,8.04637804497357));
#213460=CARTESIAN_POINT('Ctrl Pts',(6.5836151303474,12.2,8.04822556534917));
#213461=CARTESIAN_POINT('Ctrl Pts',(6.58484400289384,12.2,8.05012201771681));
#213462=CARTESIAN_POINT('Ctrl Pts',(6.58607287532866,12.2,8.05201846991219));
#213463=CARTESIAN_POINT('Ctrl Pts',(6.5873255059879,12.2,8.05396385292234));
#213464=CARTESIAN_POINT('Ctrl Pts',(6.5886009275249,12.2,8.05595776701656));
#213465=CARTESIAN_POINT('Ctrl Pts',(6.58987634906188,12.2,8.05795168111077));
#213466=CARTESIAN_POINT('Ctrl Pts',(6.59117456239721,12.2,8.05999412543044));
#213467=CARTESIAN_POINT('Ctrl Pts',(6.59249462916393,12.2,8.06208470653945));
#213468=CARTESIAN_POINT('Ctrl Pts',(6.59381469605055,12.2,8.06417528783836));
#213469=CARTESIAN_POINT('Ctrl Pts',(6.59515661597275,12.2,8.06631400529914));
#213470=CARTESIAN_POINT('Ctrl Pts',(6.59651947688179,12.2,8.06850047375489));
#213471=CARTESIAN_POINT('Ctrl Pts',(6.59788233766702,12.2,8.07068694201203));
#213472=CARTESIAN_POINT('Ctrl Pts',(6.59926613977845,12.2,8.07292116150669));
#213473=CARTESIAN_POINT('Ctrl Pts',(6.60066999473389,12.2,8.07520275276762));
#213474=CARTESIAN_POINT('Ctrl Pts',(6.60207384968932,12.2,8.07748434402855));
#213475=CARTESIAN_POINT('Ctrl Pts',(6.60349775834128,12.2,8.07981330796732));
#213476=CARTESIAN_POINT('Ctrl Pts',(6.60494085645468,12.2,8.08218927312894));
#213477=CARTESIAN_POINT('Ctrl Pts',(6.60638395469915,12.2,8.08456523850638));
#213478=CARTESIAN_POINT('Ctrl Pts',(6.6078462442627,12.2,8.08698820426467));
#213479=CARTESIAN_POINT('Ctrl Pts',(6.60932688067797,12.2,8.08945780673577));
#213480=CARTESIAN_POINT('Ctrl Pts',(6.61080751695876,12.2,8.09192740898253));
#213481=CARTESIAN_POINT('Ctrl Pts',(6.61230650277865,12.2,8.09444364778919));
#213482=CARTESIAN_POINT('Ctrl Pts',(6.61382301980764,12.2,8.09700616494809));
#213483=CARTESIAN_POINT('Ctrl Pts',(6.61533953683664,12.2,8.09956868210699));
#213484=CARTESIAN_POINT('Ctrl Pts',(6.61687358203922,12.2,8.10217747604554));
#213485=CARTESIAN_POINT('Ctrl Pts',(6.6184243611488,12.2,8.10483219636375));
#213486=CARTESIAN_POINT('Ctrl Pts',(6.6199751402584,12.2,8.10748691668196));
#213487=CARTESIAN_POINT('Ctrl Pts',(6.62154264930262,12.2,8.11018756270347));
#213488=CARTESIAN_POINT('Ctrl Pts',(6.62312611457732,12.2,8.11293378793391));
#213489=CARTESIAN_POINT('Ctrl Pts',(6.62497349082704,12.2,8.11613771753573));
#213490=CARTESIAN_POINT('Ctrl Pts',(6.62684257807194,12.2,8.11940368562293));
#213491=CARTESIAN_POINT('Ctrl Pts',(6.62873218192006,12.2,8.12273115035301));
#213492=CARTESIAN_POINT('Ctrl Pts',(6.63035184242433,12.2,8.1255832630898));
#213493=CARTESIAN_POINT('Ctrl Pts',(6.63198657150547,12.2,8.12848055834052));
#213494=CARTESIAN_POINT('Ctrl Pts',(6.63363563609634,12.2,8.13142270083728));
#213495=CARTESIAN_POINT('Ctrl Pts',(6.63528470053742,12.2,8.1343648430668));
#213496=CARTESIAN_POINT('Ctrl Pts',(6.63694809790168,12.2,8.1373518322318));
#213497=CARTESIAN_POINT('Ctrl Pts',(6.63862511134138,12.2,8.14038333870698));
#213498=CARTESIAN_POINT('Ctrl Pts',(6.64030212478107,12.2,8.14341484518217));
#213499=CARTESIAN_POINT('Ctrl Pts',(6.64199274946127,12.2,8.14649086962036));
#213500=CARTESIAN_POINT('Ctrl Pts',(6.6436962891488,12.2,8.14961108508838));
#213501=CARTESIAN_POINT('Ctrl Pts',(6.64539982883633,12.2,8.15273130055639));
#213502=CARTESIAN_POINT('Ctrl Pts',(6.64711627975847,12.2,8.15589570914476));
#213503=CARTESIAN_POINT('Ctrl Pts',(6.64884495752816,12.2,8.15910399044188));
#213504=CARTESIAN_POINT('Ctrl Pts',(6.65057363545487,12.2,8.16231227203041));
#213505=CARTESIAN_POINT('Ctrl Pts',(6.65231453949944,12.2,8.1655644249565));
#213506=CARTESIAN_POINT('Ctrl Pts',(6.65406699859548,12.2,8.16886013372137));
#213507=CARTESIAN_POINT('Ctrl Pts',(6.65581945753233,12.2,8.17215584218689));
#213508=CARTESIAN_POINT('Ctrl Pts',(6.65758347338056,12.2,8.17549510798934));
#213509=CARTESIAN_POINT('Ctrl Pts',(6.65935838924079,12.2,8.17887761654838));
#213510=CARTESIAN_POINT('Ctrl Pts',(6.66113330510102,12.2,8.18226012510744));
#213511=CARTESIAN_POINT('Ctrl Pts',(6.66291912067844,12.2,8.18568587817577));
#213512=CARTESIAN_POINT('Ctrl Pts',(6.66471519852916,12.2,8.18915456863017));
#213513=CARTESIAN_POINT('Ctrl Pts',(6.66651127654302,12.2,8.19262325939965));
#213514=CARTESIAN_POINT('Ctrl Pts',(6.66831761217702,12.2,8.19613488566173));
#213515=CARTESIAN_POINT('Ctrl Pts',(6.67013358445062,12.2,8.19968914561884));
#213516=CARTESIAN_POINT('Ctrl Pts',(6.67164689459615,12.2,8.20265102875501));
#213517=CARTESIAN_POINT('Ctrl Pts',(6.67316689471018,12.2,8.20564251785934));
#213518=CARTESIAN_POINT('Ctrl Pts',(6.67469322922457,12.2,8.20866343994505));
#213519=CARTESIAN_POINT('Ctrl Pts',(6.67621956373898,12.2,8.21168436203077));
#213520=CARTESIAN_POINT('Ctrl Pts',(6.67775223513403,12.2,8.21473471540034));
#213521=CARTESIAN_POINT('Ctrl Pts',(6.67929089200952,12.2,8.21781432936106));
#213522=CARTESIAN_POINT('Ctrl Pts',(6.68082954871729,12.2,8.22089394298609));
#213523=CARTESIAN_POINT('Ctrl Pts',(6.68237419135549,12.2,8.22400281753944));
#213524=CARTESIAN_POINT('Ctrl Pts',(6.68392447875549,12.2,8.22714078184781));
#213525=CARTESIAN_POINT('Ctrl Pts',(6.68609488138585,12.2,8.23153393242677));
#213526=CARTESIAN_POINT('Ctrl Pts',(6.68827634499719,12.2,8.23598409851597));
#213527=CARTESIAN_POINT('Ctrl Pts',(6.69046794761425,12.2,8.24049081826456));
#213528=CARTESIAN_POINT('Ctrl Pts',(6.69203337803064,12.2,8.24370990374914));
#213529=CARTESIAN_POINT('Ctrl Pts',(6.69360398287526,12.2,8.24695784379444));
#213530=CARTESIAN_POINT('Ctrl Pts',(6.69517943475741,12.2,8.25023447103147));
#213531=CARTESIAN_POINT('Ctrl Pts',(6.69675488663955,12.2,8.25351109826849));
#213532=CARTESIAN_POINT('Ctrl Pts',(6.69833518289994,12.2,8.25681641326104));
#213533=CARTESIAN_POINT('Ctrl Pts',(6.69992000248327,12.2,8.26015025048325));
#213534=CARTESIAN_POINT('Ctrl Pts',(6.7015048220666,12.2,8.26348408770545));
#213535=CARTESIAN_POINT('Ctrl Pts',(6.70309416312688,12.2,8.26684644767516));
#213536=CARTESIAN_POINT('Ctrl Pts',(6.7046877110508,12.2,8.2702371665101));
#213537=CARTESIAN_POINT('Ctrl Pts',(6.70628125897473,12.2,8.27362788534503));
#213538=CARTESIAN_POINT('Ctrl Pts',(6.70787901275451,12.2,8.27704696277963));
#213539=CARTESIAN_POINT('Ctrl Pts',(6.70948065983804,12.2,8.28049423743388));
#213540=CARTESIAN_POINT('Ctrl Pts',(6.71108230692158,12.2,8.28394151208813));
#213541=CARTESIAN_POINT('Ctrl Pts',(6.71268784678278,12.2,8.28741698396107));
#213542=CARTESIAN_POINT('Ctrl Pts',(6.71429697379686,12.2,8.29092049125421));
#213543=CARTESIAN_POINT('Ctrl Pts',(6.7162279261436,12.2,8.29512469985322));
#213544=CARTESIAN_POINT('Ctrl Pts',(6.71816404306076,12.2,8.29936928126761));
#213545=CARTESIAN_POINT('Ctrl Pts',(6.72010480449906,12.2,8.30365395796463));
#213546=CARTESIAN_POINT('Ctrl Pts',(6.72172210575639,12.2,8.30722452200856));
#213547=CARTESIAN_POINT('Ctrl Pts',(6.72334263070548,12.2,8.31082293178325));
#213548=CARTESIAN_POINT('Ctrl Pts',(6.7249660861916,12.2,8.31444902824158));
#213549=CARTESIAN_POINT('Ctrl Pts',(6.72658954167771,12.2,8.31807512469991));
#213550=CARTESIAN_POINT('Ctrl Pts',(6.72821592633883,12.2,8.32172890851102));
#213551=CARTESIAN_POINT('Ctrl Pts',(6.72984494869994,12.2,8.32541022177491));
#213552=CARTESIAN_POINT('Ctrl Pts',(6.73147397106104,12.2,8.32909153503879));
#213553=CARTESIAN_POINT('Ctrl Pts',(6.7331056319434,12.2,8.33280038045713));
#213554=CARTESIAN_POINT('Ctrl Pts',(6.7347396442425,12.2,8.33653659950195));
#213555=CARTESIAN_POINT('Ctrl Pts',(6.73637365654159,12.2,8.34027281854678));
#213556=CARTESIAN_POINT('Ctrl Pts',(6.73801002092921,12.2,8.34403641308545));
#213557=CARTESIAN_POINT('Ctrl Pts',(6.73964845558211,12.2,8.347827227948));
#213558=CARTESIAN_POINT('Ctrl Pts',(6.741286890235,12.2,8.35161804281056));
#213559=CARTESIAN_POINT('Ctrl Pts',(6.74292739366837,12.2,8.355436079239));
#213560=CARTESIAN_POINT('Ctrl Pts',(6.74456969005736,12.2,8.35928118326822));
#213561=CARTESIAN_POINT('Ctrl Pts',(6.74588352706115,12.2,8.36235726624014));
#213562=CARTESIAN_POINT('Ctrl Pts',(6.7471985122176,12.2,8.36545067278518));
#213563=CARTESIAN_POINT('Ctrl Pts',(6.74851450350898,12.2,8.36856132507363));
#213564=CARTESIAN_POINT('Ctrl Pts',(6.74983049497967,12.2,8.3716719777859));
#213565=CARTESIAN_POINT('Ctrl Pts',(6.75114749275803,12.2,8.37479987469578));
#213566=CARTESIAN_POINT('Ctrl Pts',(6.75246536060769,12.2,8.37794494075719));
#213567=CARTESIAN_POINT('Ctrl Pts',(6.75378322827778,12.2,8.38109000639009));
#213568=CARTESIAN_POINT('Ctrl Pts',(6.75510196406992,12.2,8.38425223983344));
#213569=CARTESIAN_POINT('Ctrl Pts',(6.75642143251754,12.2,8.38743156473844));
#213570=CARTESIAN_POINT('Ctrl Pts',(6.75774090114493,12.2,8.39061089007662));
#213571=CARTESIAN_POINT('Ctrl Pts',(6.75906110102841,12.2,8.39380730742622));
#213572=CARTESIAN_POINT('Ctrl Pts',(6.76038189955084,12.2,8.39702073822711));
#213573=CARTESIAN_POINT('Ctrl Pts',(6.76170269789331,12.2,8.40023416859018));
#213574=CARTESIAN_POINT('Ctrl Pts',(6.76302409172527,12.2,8.40346461550287));
#213575=CARTESIAN_POINT('Ctrl Pts',(6.76434595028382,12.2,8.40671199923564));
#213576=CARTESIAN_POINT('Ctrl Pts',(6.76566780902246,12.2,8.40995938341088));
#213577=CARTESIAN_POINT('Ctrl Pts',(6.76699013193896,12.2,8.41322370691553));
#213578=CARTESIAN_POINT('Ctrl Pts',(6.76831278723328,12.2,8.41650489298325));
#213579=CARTESIAN_POINT('Ctrl Pts',(6.76963544252758,12.2,8.41978607905095));
#213580=CARTESIAN_POINT('Ctrl Pts',(6.77095842881082,12.2,8.4230841286762));
#213581=CARTESIAN_POINT('Ctrl Pts',(6.77228161821629,12.2,8.42639896485858));
#213582=CARTESIAN_POINT('Ctrl Pts',(6.77360480744148,12.2,8.42971380058932));
#213583=CARTESIAN_POINT('Ctrl Pts',(6.77492819831234,12.2,8.43304542463677));
#213584=CARTESIAN_POINT('Ctrl Pts',(6.77625166276571,12.2,8.43639376098931));
#213585=CARTESIAN_POINT('Ctrl Pts',(6.77757512739941,12.2,8.43974209779807));
#213586=CARTESIAN_POINT('Ctrl Pts',(6.77889866503309,12.2,8.44310714774182));
#213587=CARTESIAN_POINT('Ctrl Pts',(6.78022214921633,12.2,8.44648883576116));
#213588=CARTESIAN_POINT('Ctrl Pts',(6.78154563321924,12.2,8.44987052331975));
#213589=CARTESIAN_POINT('Ctrl Pts',(6.78286906468882,12.2,8.45326884904839));
#213590=CARTESIAN_POINT('Ctrl Pts',(6.78419231535843,12.2,8.45668373871257));
#213591=CARTESIAN_POINT('Ctrl Pts',(6.78551556620833,12.2,8.46009862884203));
#213592=CARTESIAN_POINT('Ctrl Pts',(6.78683863867041,12.2,8.46353008264707));
#213593=CARTESIAN_POINT('Ctrl Pts',(6.78816140814188,12.2,8.46697802750866));
#213594=CARTESIAN_POINT('Ctrl Pts',(6.78948417743313,12.2,8.47042597190047));
#213595=CARTESIAN_POINT('Ctrl Pts',(6.79080664278882,12.2,8.4738904071873));
#213596=CARTESIAN_POINT('Ctrl Pts',(6.7921286821252,12.2,8.47737125829051));
#213597=CARTESIAN_POINT('Ctrl Pts',(6.79345072164171,12.2,8.48085210986798));
#213598=CARTESIAN_POINT('Ctrl Pts',(6.79477233533599,12.2,8.48434937936146));
#213599=CARTESIAN_POINT('Ctrl Pts',(6.7960934020746,12.2,8.48786299155397));
#213600=CARTESIAN_POINT('Ctrl Pts',(6.79741446863322,12.2,8.49137660326776));
#213601=CARTESIAN_POINT('Ctrl Pts',(6.79873498728644,12.2,8.49490656004127));
#213602=CARTESIAN_POINT('Ctrl Pts',(6.80005483930009,12.2,8.49845278776043));
#213603=CARTESIAN_POINT('Ctrl Pts',(6.80170465445202,12.2,8.50288557277178));
#213604=CARTESIAN_POINT('Ctrl Pts',(6.80335342639768,12.2,8.50734378141373));
#213605=CARTESIAN_POINT('Ctrl Pts',(6.80500092563386,12.2,8.51182727148185));
#213606=CARTESIAN_POINT('Ctrl Pts',(6.80631892509463,12.2,8.51541406373182));
#213607=CARTESIAN_POINT('Ctrl Pts',(6.80763610905532,12.2,8.51901703822544));
#213608=CARTESIAN_POINT('Ctrl Pts',(6.80895236184921,12.2,8.52263612097927));
#213609=CARTESIAN_POINT('Ctrl Pts',(6.81026861446377,12.2,8.52625520324002));
#213610=CARTESIAN_POINT('Ctrl Pts',(6.81158393472871,12.2,8.52989039369603));
#213611=CARTESIAN_POINT('Ctrl Pts',(6.8128982075759,12.2,8.53354162274519));
#213612=CARTESIAN_POINT('Ctrl Pts',(6.81421248060215,12.2,8.53719285229184));
#213613=CARTESIAN_POINT('Ctrl Pts',(6.81552570710522,12.2,8.54086011752718));
#213614=CARTESIAN_POINT('Ctrl Pts',(6.81683777189887,12.2,8.54454335028452));
#213615=CARTESIAN_POINT('Ctrl Pts',(6.81814983651375,12.2,8.54822658254003));
#213616=CARTESIAN_POINT('Ctrl Pts',(6.81946073862053,12.2,8.55192577967837));
#213617=CARTESIAN_POINT('Ctrl Pts',(6.82077036673582,12.2,8.55564087265085));
#213618=CARTESIAN_POINT('Ctrl Pts',(6.82207999502956,12.2,8.5593559661295));
#213619=CARTESIAN_POINT('Ctrl Pts',(6.82338834909869,12.2,8.56308695474234));
#213620=CARTESIAN_POINT('Ctrl Pts',(6.82469531667584,12.2,8.56683376751915));
#213621=CARTESIAN_POINT('Ctrl Pts',(6.82600228407492,12.2,8.57058057978546));
#213622=CARTESIAN_POINT('Ctrl Pts',(6.82730786614041,12.2,8.57434321740655));
#213623=CARTESIAN_POINT('Ctrl Pts',(6.82861195031173,12.2,8.57812160837383));
#213624=CARTESIAN_POINT('Ctrl Pts',(6.82991603466074,12.2,8.58189999985591));
#213625=CARTESIAN_POINT('Ctrl Pts',(6.8312186238096,12.2,8.58569414577284));
#213626=CARTESIAN_POINT('Ctrl Pts',(6.83251960549162,12.2,8.58950397525826));
#213627=CARTESIAN_POINT('Ctrl Pts',(6.83382058717364,12.2,8.59331380474367));
#213628=CARTESIAN_POINT('Ctrl Pts',(6.83511996455545,12.2,8.59713931823089));
#213629=CARTESIAN_POINT('Ctrl Pts',(6.83641762690379,12.2,8.6009804463863));
#213630=CARTESIAN_POINT('Ctrl Pts',(6.83771528907532,12.2,8.60482157401836));
#213631=CARTESIAN_POINT('Ctrl Pts',(6.83901123726094,12.2,8.60867831564833));
#213632=CARTESIAN_POINT('Ctrl Pts',(6.8403053647108,12.2,8.61255060194184));
#213633=CARTESIAN_POINT('Ctrl Pts',(6.84159949233701,12.2,8.61642288876295));
#213634=CARTESIAN_POINT('Ctrl Pts',(6.84289179914979,12.2,8.62031072085456));
#213635=CARTESIAN_POINT('Ctrl Pts',(6.84418217889552,12.2,8.62421402854141));
#213636=CARTESIAN_POINT('Ctrl Pts',(6.84547255846543,12.2,8.62811733569644));
#213637=CARTESIAN_POINT('Ctrl Pts',(6.84676101244702,12.2,8.63203611887053));
#213638=CARTESIAN_POINT('Ctrl Pts',(6.84804743461977,12.2,8.63597030793678));
#213639=CARTESIAN_POINT('Ctrl Pts',(6.84933385696779,12.2,8.63990449753907));
#213640=CARTESIAN_POINT('Ctrl Pts',(6.85061824779612,12.2,8.64385409422376));
#213641=CARTESIAN_POINT('Ctrl Pts',(6.85190050408809,12.2,8.64781902910754));
#213642=CARTESIAN_POINT('Ctrl Pts',(6.85318276020535,12.2,8.6517839634511));
#213643=CARTESIAN_POINT('Ctrl Pts',(6.85446288155493,12.2,8.65576423572633));
#213644=CARTESIAN_POINT('Ctrl Pts',(6.85574076584785,12.2,8.65975977815357));
#213645=CARTESIAN_POINT('Ctrl Pts',(6.85701865031487,12.2,8.6637553211252));
#213646=CARTESIAN_POINT('Ctrl Pts',(6.85829429729866,12.2,8.66776613396156));
#213647=CARTESIAN_POINT('Ctrl Pts',(6.85956760631236,12.2,8.67179214757087));
#213648=CARTESIAN_POINT('Ctrl Pts',(6.86084091515256,12.2,8.67581816063164));
#213649=CARTESIAN_POINT('Ctrl Pts',(6.86211188526822,12.2,8.67985937619763));
#213650=CARTESIAN_POINT('Ctrl Pts',(6.86338041727588,12.2,8.68391572508671));
#213651=CARTESIAN_POINT('Ctrl Pts',(6.86464894945638,12.2,8.68797207452847));
#213652=CARTESIAN_POINT('Ctrl Pts',(6.86591504192623,12.2,8.69204355764752));
#213653=CARTESIAN_POINT('Ctrl Pts',(6.86717859700082,12.2,8.69613010727772));
#213654=CARTESIAN_POINT('Ctrl Pts',(6.86844215190325,12.2,8.70021665635113));
#213655=CARTESIAN_POINT('Ctrl Pts',(6.86970316904958,12.2,8.7043182717455));
#213656=CARTESIAN_POINT('Ctrl Pts',(6.87096155000254,12.2,8.70843488601853));
#213657=CARTESIAN_POINT('Ctrl Pts',(6.87221993112694,12.2,8.71255150085243));
#213658=CARTESIAN_POINT('Ctrl Pts',(6.873475677015,12.2,8.71668311504338));
#213659=CARTESIAN_POINT('Ctrl Pts',(6.87472868874996,12.2,8.72082965999159));
#213660=CARTESIAN_POINT('Ctrl Pts',(6.87598170048491,12.2,8.72497620493979));
#213661=CARTESIAN_POINT('Ctrl Pts',(6.87723197977511,12.2,8.72913768169534));
#213662=CARTESIAN_POINT('Ctrl Pts',(6.87847942895391,12.2,8.73331402442444));
#213663=CARTESIAN_POINT('Ctrl Pts',(6.87972687796275,12.2,8.73749036658451));
#213664=CARTESIAN_POINT('Ctrl Pts',(6.88097149858108,12.2,8.74168157270519));
#213665=CARTESIAN_POINT('Ctrl Pts',(6.88221319354078,12.2,8.74588757771374));
#213666=CARTESIAN_POINT('Ctrl Pts',(6.88345488866965,12.2,8.75009358329535));
#213667=CARTESIAN_POINT('Ctrl Pts',(6.88469365984886,12.2,8.75431438686847));
#213668=CARTESIAN_POINT('Ctrl Pts',(6.88592941219367,12.2,8.75854992293411));
#213669=CARTESIAN_POINT('Ctrl Pts',(6.88716516437011,12.2,8.76278545842266));
#213670=CARTESIAN_POINT('Ctrl Pts',(6.88839789773583,12.2,8.76703572543434));
#213671=CARTESIAN_POINT('Ctrl Pts',(6.88962751935774,12.2,8.77130065841808));
#213672=CARTESIAN_POINT('Ctrl Pts',(6.89054973561605,12.2,8.77449935830115));
#213673=CARTESIAN_POINT('Ctrl Pts',(6.89147020074281,12.2,8.77770630735176));
#213674=CARTESIAN_POINT('Ctrl Pts',(6.89238887658886,12.2,8.78092147885295));
#213675=CARTESIAN_POINT('Ctrl Pts',(6.89330755243492,12.2,8.78413665035414));
#213676=CARTESIAN_POINT('Ctrl Pts',(6.89422443993347,12.2,8.78736004319732));
#213677=CARTESIAN_POINT('Ctrl Pts',(6.89513949827547,12.2,8.79059163003711));
#213678=CARTESIAN_POINT('Ctrl Pts',(6.89605455678372,12.2,8.79382321746398));
#213679=CARTESIAN_POINT('Ctrl Pts',(6.89696778779977,12.2,8.79706299826816));
#213680=CARTESIAN_POINT('Ctrl Pts',(6.89787915218197,12.2,8.80031094615799));
#213681=CARTESIAN_POINT('Ctrl Pts',(6.89879051639861,12.2,8.80355889345778));
#213682=CARTESIAN_POINT('Ctrl Pts',(6.89970001363199,12.2,8.80681500710709));
#213683=CARTESIAN_POINT('Ctrl Pts',(6.90060760639052,12.2,8.81007925940587));
#213684=CARTESIAN_POINT('Ctrl Pts',(6.90151519914904,12.2,8.81334351170466));
#213685=CARTESIAN_POINT('Ctrl Pts',(6.90242088744619,12.2,8.81661590187384));
#213686=CARTESIAN_POINT('Ctrl Pts',(6.90332463325078,12.2,8.81989640376958));
#213687=CARTESIAN_POINT('Ctrl Pts',(6.90422837905537,12.2,8.82317690566531));
#213688=CARTESIAN_POINT('Ctrl Pts',(6.90513018234441,12.2,8.82646551955179));
#213689=CARTESIAN_POINT('Ctrl Pts',(6.90603000523247,12.2,8.82976221603026));
#213690=CARTESIAN_POINT('Ctrl Pts',(6.90692982812054,12.2,8.83305891250873));
#213691=CARTESIAN_POINT('Ctrl Pts',(6.90782767280132,12.2,8.83636369337671));
#213692=CARTESIAN_POINT('Ctrl Pts',(6.90872349864395,12.2,8.83967652938063));
#213693=CARTESIAN_POINT('Ctrl Pts',(6.90961932448657,12.2,8.84298936538455));
#213694=CARTESIAN_POINT('Ctrl Pts',(6.91051313333768,12.2,8.8463102585963));
#213695=CARTESIAN_POINT('Ctrl Pts',(6.91140488809722,12.2,8.8496391805159));
#213696=CARTESIAN_POINT('Ctrl Pts',(6.91229664301877,12.2,8.85296810304025));
#213697=CARTESIAN_POINT('Ctrl Pts',(6.91318634303141,12.2,8.85630505465857));
#213698=CARTESIAN_POINT('Ctrl Pts',(6.91407395291013,12.2,8.85965000768748));
#213699=CARTESIAN_POINT('Ctrl Pts',(6.9149615626276,12.2,8.86299496010873));
#213700=CARTESIAN_POINT('Ctrl Pts',(6.91584708057573,12.2,8.86634791455353));
#213701=CARTESIAN_POINT('Ctrl Pts',(6.91673047146252,12.2,8.86970884310027));
#213702=CARTESIAN_POINT('Ctrl Pts',(6.91761386234932,12.2,8.873069771647));
#213703=CARTESIAN_POINT('Ctrl Pts',(6.91849512742788,12.2,8.87643867454014));
#213704=CARTESIAN_POINT('Ctrl Pts',(6.91937422735408,12.2,8.87981552487648));
#213705=CARTESIAN_POINT('Ctrl Pts',(6.92025332728029,12.2,8.88319237521282));
#213706=CARTESIAN_POINT('Ctrl Pts',(6.92113026414842,12.2,8.88657717238988));
#213707=CARTESIAN_POINT('Ctrl Pts',(6.92200500149163,12.2,8.88996989022494));
#213708=CARTESIAN_POINT('Ctrl Pts',(6.92287973883485,12.2,8.89336260806001));
#213709=CARTESIAN_POINT('Ctrl Pts',(6.92375227678649,12.2,8.89676324576975));
#213710=CARTESIAN_POINT('Ctrl Pts',(6.92462257963006,12.2,8.9001717771452));
#213711=CARTESIAN_POINT('Ctrl Pts',(6.92549288247362,12.2,8.90358030852063));
#213712=CARTESIAN_POINT('Ctrl Pts',(6.92636095098704,12.2,8.90699673390843));
#213713=CARTESIAN_POINT('Ctrl Pts',(6.92722674833243,12.2,8.91042102412082));
#213714=CARTESIAN_POINT('Ctrl Pts',(6.92809254567781,12.2,8.91384531433321));
#213715=CARTESIAN_POINT('Ctrl Pts',(6.92895607180986,12.2,8.91727747197607));
#213716=CARTESIAN_POINT('Ctrl Pts',(6.92981729357054,12.2,8.92071746797501));
#213717=CARTESIAN_POINT('Ctrl Pts',(6.93067851548769,12.2,8.92415746459888));
#213718=CARTESIAN_POINT('Ctrl Pts',(6.93153743167919,12.2,8.92760530143334));
#213719=CARTESIAN_POINT('Ctrl Pts',(6.93239400717836,12.2,8.93106094997828));
#213720=CARTESIAN_POINT('Ctrl Pts',(6.93325058252192,12.2,8.93451659789544));
#213721=CARTESIAN_POINT('Ctrl Pts',(6.93410481729059,12.2,8.93798005852054));
#213722=CARTESIAN_POINT('Ctrl Pts',(6.93495667755111,12.2,8.9414513048951));
#213723=CARTESIAN_POINT('Ctrl Pts',(6.93580853781162,12.2,8.94492255126966));
#213724=CARTESIAN_POINT('Ctrl Pts',(6.93665802303074,12.2,8.94840158312663));
#213725=CARTESIAN_POINT('Ctrl Pts',(6.9375050988333,12.2,8.95188837445826));
#213726=CARTESIAN_POINT('Ctrl Pts',(6.93835217463585,12.2,8.9553751657899));
#213727=CARTESIAN_POINT('Ctrl Pts',(6.93919684097184,12.2,8.95886971554625));
#213728=CARTESIAN_POINT('Ctrl Pts',(6.94003906344145,12.2,8.96237199837663));
#213729=CARTESIAN_POINT('Ctrl Pts',(6.94088128591105,12.2,8.96587428120702));
#213730=CARTESIAN_POINT('Ctrl Pts',(6.94172106605958,12.2,8.96938429620575));
#213731=CARTESIAN_POINT('Ctrl Pts',(6.94255836807128,12.2,8.97290201679442));
#213732=CARTESIAN_POINT('Ctrl Pts',(6.94339567008296,12.2,8.9764197373831));
#213733=CARTESIAN_POINT('Ctrl Pts',(6.94423049588175,12.2,8.97994516415916));
#213734=CARTESIAN_POINT('Ctrl Pts',(6.94506280931018,12.2,8.98347826998806));
#213735=CARTESIAN_POINT('Ctrl Pts',(6.94617256064889,12.2,8.98818907818783));
#213736=CARTESIAN_POINT('Ctrl Pts',(6.94727784938442,12.2,8.99291353767225));
#213737=CARTESIAN_POINT('Ctrl Pts',(6.94837859399996,12.2,8.99765158720827));
#213738=CARTESIAN_POINT('Ctrl Pts',(6.94920415238664,12.2,9.00120512403751));
#213739=CARTESIAN_POINT('Ctrl Pts',(6.95002715535674,12.2,9.0047663038414));
#213740=CARTESIAN_POINT('Ctrl Pts',(6.95084757020216,12.2,9.00833510212772));
#213741=CARTESIAN_POINT('Ctrl Pts',(6.95166798504757,12.2,9.01190390041404));
#213742=CARTESIAN_POINT('Ctrl Pts',(6.95248581166414,12.2,9.01548031530866));
#213743=CARTESIAN_POINT('Ctrl Pts',(6.95330101663388,12.2,9.01906432277325));
#213744=CARTESIAN_POINT('Ctrl Pts',(6.95411622160362,12.2,9.02264833023785));
#213745=CARTESIAN_POINT('Ctrl Pts',(6.95492880566913,12.2,9.02623992811379));
#213746=CARTESIAN_POINT('Ctrl Pts',(6.95573873555673,12.2,9.02983909098199));
#213747=CARTESIAN_POINT('Ctrl Pts',(6.95654866559146,12.2,9.03343825450403));
#213748=CARTESIAN_POINT('Ctrl Pts',(6.95735594112546,12.2,9.03704498289489));
#213749=CARTESIAN_POINT('Ctrl Pts',(6.95816053065869,12.2,9.04065924950451));
#213750=CARTESIAN_POINT('Ctrl Pts',(6.95896512004576,12.2,9.04427351545755));
#213751=CARTESIAN_POINT('Ctrl Pts',(6.9597670234663,12.2,9.0478953207602));
#213752=CARTESIAN_POINT('Ctrl Pts',(6.96056620931203,12.2,9.05152463862899));
#213753=CARTESIAN_POINT('Ctrl Pts',(6.96136539515776,12.2,9.05515395649778));
#213754=CARTESIAN_POINT('Ctrl Pts',(6.96216186315926,12.2,9.05879078725241));
#213755=CARTESIAN_POINT('Ctrl Pts',(6.96295558050902,12.2,9.06243510451158));
#213756=CARTESIAN_POINT('Ctrl Pts',(6.96374929785877,12.2,9.06607942177076));
#213757=CARTESIAN_POINT('Ctrl Pts',(6.96454026450762,12.2,9.06973122396299));
#213758=CARTESIAN_POINT('Ctrl Pts',(6.96532844702425,12.2,9.07339048580495));
#213759=CARTESIAN_POINT('Ctrl Pts',(6.96637935714186,12.2,9.0782695020374));
#213760=CARTESIAN_POINT('Ctrl Pts',(6.96742531992227,12.2,9.08316177839994));
#213761=CARTESIAN_POINT('Ctrl Pts',(6.96846626714516,12.2,9.08806726000199));
#213762=CARTESIAN_POINT('Ctrl Pts',(6.96924697749141,12.2,9.09174637086934));
#213763=CARTESIAN_POINT('Ctrl Pts',(6.97002486692947,12.2,9.09543290893625));
#213764=CARTESIAN_POINT('Ctrl Pts',(6.97079990310939,12.2,9.0991268486777));
#213765=CARTESIAN_POINT('Ctrl Pts',(6.9718332846357,12.2,9.1040521014426));
#213766=CARTESIAN_POINT('Ctrl Pts',(6.972861590953,12.2,9.10899050989288));
#213767=CARTESIAN_POINT('Ctrl Pts',(6.97388473364314,12.2,9.11394199978984));
#213768=CARTESIAN_POINT('Ctrl Pts',(6.97465209069559,12.2,9.11765561738122));
#213769=CARTESIAN_POINT('Ctrl Pts',(6.97541654334455,12.2,9.12137659300695));
#213770=CARTESIAN_POINT('Ctrl Pts',(6.97617807056728,12.2,9.12510490870382));
#213771=CARTESIAN_POINT('Ctrl Pts',(6.97719344028981,12.2,9.13007599675117));
#213772=CARTESIAN_POINT('Ctrl Pts',(6.97820360405943,12.2,9.13506013363826));
#213773=CARTESIAN_POINT('Ctrl Pts',(6.97920857099994,12.2,9.14005731499999));
#213774=CARTESIAN_POINT('Origin',(-5.66257110645729E-14,15.2,-1.77635683940025E-14));
#213775=CARTESIAN_POINT('',(5.36127880565669,15.2,8.88241603231688));
#213776=CARTESIAN_POINT('',(5.36127880565669,12.2,8.88241603231688));
#213777=CARTESIAN_POINT('',(5.36127880599994,15.2,8.88241603199998));
#213778=CARTESIAN_POINT('Origin',(-5.66257110645729E-14,12.2,-1.77635683940025E-14));
#213779=CARTESIAN_POINT('Origin',(-5.66257110645729E-14,15.2,-1.77635683940025E-14));
#213780=CARTESIAN_POINT('Origin',(-5.66257110645729E-14,15.2,-1.77635683940025E-14));
#213781=CARTESIAN_POINT('',(5.60740451299995,15.2,10.04026965));
#213782=CARTESIAN_POINT('',(5.2693970185908,15.2,10.2217148785196));
#213783=CARTESIAN_POINT('Origin',(-5.66257110645729E-14,15.2,-1.77635683940025E-14));
#213784=CARTESIAN_POINT('',(5.2693970185908,12.2,10.2217148785196));
#213785=CARTESIAN_POINT('',(5.26939701899994,15.2,10.221714879));
#213786=CARTESIAN_POINT('',(5.60740451299995,12.2,10.04026965));
#213787=CARTESIAN_POINT('Origin',(-5.66257110645729E-14,12.2,-1.77635683940025E-14));
#213788=CARTESIAN_POINT('',(5.60740451299995,15.2,10.04026965));
#213789=CARTESIAN_POINT('Ctrl Pts',(5.36127880499994,15.2,8.88241603299999));
#213790=CARTESIAN_POINT('Ctrl Pts',(5.36127880499994,11.6,8.88241603299999));
#213791=CARTESIAN_POINT('Ctrl Pts',(5.36135574299994,15.2,8.88257249699999));
#213792=CARTESIAN_POINT('Ctrl Pts',(5.36135574299994,11.6,8.88257249699999));
#213793=CARTESIAN_POINT('Ctrl Pts',(5.36151222899994,15.2,8.88289092999998));
#213794=CARTESIAN_POINT('Ctrl Pts',(5.36151222899994,11.6,8.88289092999998));
#213795=CARTESIAN_POINT('Ctrl Pts',(5.36174910299994,15.2,8.88337354899999));
#213796=CARTESIAN_POINT('Ctrl Pts',(5.36174910299994,11.6,8.88337354899999));
#213797=CARTESIAN_POINT('Ctrl Pts',(5.36206770999994,15.2,8.88402391699999));
#213798=CARTESIAN_POINT('Ctrl Pts',(5.36206770999994,11.6,8.88402391699999));
#213799=CARTESIAN_POINT('Ctrl Pts',(5.36246987999994,15.2,8.88484693899999));
#213800=CARTESIAN_POINT('Ctrl Pts',(5.36246987999994,11.6,8.88484693899999));
#213801=CARTESIAN_POINT('Ctrl Pts',(5.36287772799994,15.2,8.88568370999998));
#213802=CARTESIAN_POINT('Ctrl Pts',(5.36287772799994,11.6,8.88568370999998));
#213803=CARTESIAN_POINT('Ctrl Pts',(5.36328889699995,15.2,8.88652944599999));
#213804=CARTESIAN_POINT('Ctrl Pts',(5.36328889699995,11.6,8.88652944599999));
#213805=CARTESIAN_POINT('Ctrl Pts',(5.36370335799995,15.2,8.88738413199999));
#213806=CARTESIAN_POINT('Ctrl Pts',(5.36370335799995,11.6,8.88738413199999));
#213807=CARTESIAN_POINT('Ctrl Pts',(5.36412108299994,15.2,8.88824774999998));
#213808=CARTESIAN_POINT('Ctrl Pts',(5.36412108299994,11.6,8.88824774999998));
#213809=CARTESIAN_POINT('Ctrl Pts',(5.36454204499995,15.2,8.88912028399999));
#213810=CARTESIAN_POINT('Ctrl Pts',(5.36454204499995,11.6,8.88912028399999));
#213811=CARTESIAN_POINT('Ctrl Pts',(5.36496621399994,15.2,8.89000171999999));
#213812=CARTESIAN_POINT('Ctrl Pts',(5.36496621399994,11.6,8.89000171999999));
#213813=CARTESIAN_POINT('Ctrl Pts',(5.36539356699994,15.2,8.89089203999998));
#213814=CARTESIAN_POINT('Ctrl Pts',(5.36539356699994,11.6,8.89089203999998));
#213815=CARTESIAN_POINT('Ctrl Pts',(5.36582407199995,15.2,8.89179122799998));
#213816=CARTESIAN_POINT('Ctrl Pts',(5.36582407199995,11.6,8.89179122799998));
#213817=CARTESIAN_POINT('Ctrl Pts',(5.36625770499994,15.2,8.89269926899999));
#213818=CARTESIAN_POINT('Ctrl Pts',(5.36625770499994,11.6,8.89269926899999));
#213819=CARTESIAN_POINT('Ctrl Pts',(5.36669443599994,15.2,8.89361614499999));
#213820=CARTESIAN_POINT('Ctrl Pts',(5.36669443599994,11.6,8.89361614499999));
#213821=CARTESIAN_POINT('Ctrl Pts',(5.36713423999994,15.2,8.89454184299998));
#213822=CARTESIAN_POINT('Ctrl Pts',(5.36713423999994,11.6,8.89454184299998));
#213823=CARTESIAN_POINT('Ctrl Pts',(5.36757708999994,15.2,8.89547634599998));
#213824=CARTESIAN_POINT('Ctrl Pts',(5.36757708999994,11.6,8.89547634599998));
#213825=CARTESIAN_POINT('Ctrl Pts',(5.36802295899994,15.2,8.89641963799999));
#213826=CARTESIAN_POINT('Ctrl Pts',(5.36802295899994,11.6,8.89641963799999));
#213827=CARTESIAN_POINT('Ctrl Pts',(5.36847181899994,15.2,8.89737170399999));
#213828=CARTESIAN_POINT('Ctrl Pts',(5.36847181899994,11.6,8.89737170399999));
#213829=CARTESIAN_POINT('Ctrl Pts',(5.36892364499994,15.2,8.89833252799999));
#213830=CARTESIAN_POINT('Ctrl Pts',(5.36892364499994,11.6,8.89833252799999));
#213831=CARTESIAN_POINT('Ctrl Pts',(5.36937841199994,15.2,8.89930209499998));
#213832=CARTESIAN_POINT('Ctrl Pts',(5.36937841199994,11.6,8.89930209499998));
#213833=CARTESIAN_POINT('Ctrl Pts',(5.36983609099994,15.2,8.90028038899998));
#213834=CARTESIAN_POINT('Ctrl Pts',(5.36983609099994,11.6,8.90028038899998));
#213835=CARTESIAN_POINT('Ctrl Pts',(5.37029665799994,15.2,8.90126739499999));
#213836=CARTESIAN_POINT('Ctrl Pts',(5.37029665799994,11.6,8.90126739499999));
#213837=CARTESIAN_POINT('Ctrl Pts',(5.37076008699994,15.2,8.90226309799999));
#213838=CARTESIAN_POINT('Ctrl Pts',(5.37076008699994,11.6,8.90226309799999));
#213839=CARTESIAN_POINT('Ctrl Pts',(5.37122634999994,15.2,8.90326748199998));
#213840=CARTESIAN_POINT('Ctrl Pts',(5.37122634999994,11.6,8.90326748199998));
#213841=CARTESIAN_POINT('Ctrl Pts',(5.37169542399995,15.2,8.90428053199999));
#213842=CARTESIAN_POINT('Ctrl Pts',(5.37169542399995,11.6,8.90428053199999));
#213843=CARTESIAN_POINT('Ctrl Pts',(5.37216728199994,15.2,8.90530223299999));
#213844=CARTESIAN_POINT('Ctrl Pts',(5.37216728199994,11.6,8.90530223299999));
#213845=CARTESIAN_POINT('Ctrl Pts',(5.37264189899994,15.2,8.90633256999998));
#213846=CARTESIAN_POINT('Ctrl Pts',(5.37264189899994,11.6,8.90633256999998));
#213847=CARTESIAN_POINT('Ctrl Pts',(5.37311924999995,15.2,8.90737152799998));
#213848=CARTESIAN_POINT('Ctrl Pts',(5.37311924999995,11.6,8.90737152799998));
#213849=CARTESIAN_POINT('Ctrl Pts',(5.37359930999994,15.2,8.90841909199998));
#213850=CARTESIAN_POINT('Ctrl Pts',(5.37359930999994,11.6,8.90841909199998));
#213851=CARTESIAN_POINT('Ctrl Pts',(5.37408205299994,15.2,8.90947524699998));
#213852=CARTESIAN_POINT('Ctrl Pts',(5.37408205299994,11.6,8.90947524699998));
#213853=CARTESIAN_POINT('Ctrl Pts',(5.37456745499994,15.2,8.91053997799998));
#213854=CARTESIAN_POINT('Ctrl Pts',(5.37456745499994,11.6,8.91053997799998));
#213855=CARTESIAN_POINT('Ctrl Pts',(5.37505548999994,15.2,8.91161327199999));
#213856=CARTESIAN_POINT('Ctrl Pts',(5.37505548999994,11.6,8.91161327199999));
#213857=CARTESIAN_POINT('Ctrl Pts',(5.37554613599994,15.2,8.91269511099999));
#213858=CARTESIAN_POINT('Ctrl Pts',(5.37554613599994,11.6,8.91269511099999));
#213859=CARTESIAN_POINT('Ctrl Pts',(5.37603936499995,15.2,8.91378548299999));
#213860=CARTESIAN_POINT('Ctrl Pts',(5.37603936499995,11.6,8.91378548299999));
#213861=CARTESIAN_POINT('Ctrl Pts',(5.37653515399994,15.2,8.91488437299999));
#213862=CARTESIAN_POINT('Ctrl Pts',(5.37653515399994,11.6,8.91488437299999));
#213863=CARTESIAN_POINT('Ctrl Pts',(5.37703347999994,15.2,8.91599176499999));
#213864=CARTESIAN_POINT('Ctrl Pts',(5.37703347999994,11.6,8.91599176499999));
#213865=CARTESIAN_POINT('Ctrl Pts',(5.37753431699994,15.2,8.91710764599999));
#213866=CARTESIAN_POINT('Ctrl Pts',(5.37753431699994,11.6,8.91710764599999));
#213867=CARTESIAN_POINT('Ctrl Pts',(5.37803764199994,15.2,8.91823200099999));
#213868=CARTESIAN_POINT('Ctrl Pts',(5.37803764199994,11.6,8.91823200099999));
#213869=CARTESIAN_POINT('Ctrl Pts',(5.37854343099994,15.2,8.91936481499998));
#213870=CARTESIAN_POINT('Ctrl Pts',(5.37854343099994,11.6,8.91936481499998));
#213871=CARTESIAN_POINT('Ctrl Pts',(5.37905165999994,15.2,8.92050607499998));
#213872=CARTESIAN_POINT('Ctrl Pts',(5.37905165999994,11.6,8.92050607499998));
#213873=CARTESIAN_POINT('Ctrl Pts',(5.37956230399994,15.2,8.92165576499998));
#213874=CARTESIAN_POINT('Ctrl Pts',(5.37956230399994,11.6,8.92165576499998));
#213875=CARTESIAN_POINT('Ctrl Pts',(5.38007534199994,15.2,8.92281387299998));
#213876=CARTESIAN_POINT('Ctrl Pts',(5.38007534199994,11.6,8.92281387299998));
#213877=CARTESIAN_POINT('Ctrl Pts',(5.38059074799994,15.2,8.92398038299999));
#213878=CARTESIAN_POINT('Ctrl Pts',(5.38059074799994,11.6,8.92398038299999));
#213879=CARTESIAN_POINT('Ctrl Pts',(5.38110849899994,15.2,8.92515528099998));
#213880=CARTESIAN_POINT('Ctrl Pts',(5.38110849899994,11.6,8.92515528099998));
#213881=CARTESIAN_POINT('Ctrl Pts',(5.38162857399994,15.2,8.92633855399998));
#213882=CARTESIAN_POINT('Ctrl Pts',(5.38162857399994,11.6,8.92633855399998));
#213883=CARTESIAN_POINT('Ctrl Pts',(5.38215094699994,15.2,8.92753018699998));
#213884=CARTESIAN_POINT('Ctrl Pts',(5.38215094699994,11.6,8.92753018699998));
#213885=CARTESIAN_POINT('Ctrl Pts',(5.38267559599994,15.2,8.92873016599999));
#213886=CARTESIAN_POINT('Ctrl Pts',(5.38267559599994,11.6,8.92873016599999));
#213887=CARTESIAN_POINT('Ctrl Pts',(5.38320249799994,15.2,8.92993847799998));
#213888=CARTESIAN_POINT('Ctrl Pts',(5.38320249799994,11.6,8.92993847799998));
#213889=CARTESIAN_POINT('Ctrl Pts',(5.38373163099994,15.2,8.93115510699998));
#213890=CARTESIAN_POINT('Ctrl Pts',(5.38373163099994,11.6,8.93115510699998));
#213891=CARTESIAN_POINT('Ctrl Pts',(5.38426297099994,15.2,8.93238004199999));
#213892=CARTESIAN_POINT('Ctrl Pts',(5.38426297099994,11.6,8.93238004199999));
#213893=CARTESIAN_POINT('Ctrl Pts',(5.38479649699994,15.2,8.93361326699999));
#213894=CARTESIAN_POINT('Ctrl Pts',(5.38479649699994,11.6,8.93361326699999));
#213895=CARTESIAN_POINT('Ctrl Pts',(5.38533218399994,15.2,8.93485476999999));
#213896=CARTESIAN_POINT('Ctrl Pts',(5.38533218399994,11.6,8.93485476999999));
#213897=CARTESIAN_POINT('Ctrl Pts',(5.38587001199994,15.2,8.93610453599998));
#213898=CARTESIAN_POINT('Ctrl Pts',(5.38587001199994,11.6,8.93610453599998));
#213899=CARTESIAN_POINT('Ctrl Pts',(5.38640995699994,15.2,8.93736255199999));
#213900=CARTESIAN_POINT('Ctrl Pts',(5.38640995699994,11.6,8.93736255199999));
#213901=CARTESIAN_POINT('Ctrl Pts',(5.38695199599994,15.2,8.93862880299999));
#213902=CARTESIAN_POINT('Ctrl Pts',(5.38695199599994,11.6,8.93862880299999));
#213903=CARTESIAN_POINT('Ctrl Pts',(5.38749611099994,15.2,8.93990327699999));
#213904=CARTESIAN_POINT('Ctrl Pts',(5.38749611099994,11.6,8.93990327699999));
#213905=CARTESIAN_POINT('Ctrl Pts',(5.38804227499995,15.2,8.94118596099998));
#213906=CARTESIAN_POINT('Ctrl Pts',(5.38804227499995,11.6,8.94118596099998));
#213907=CARTESIAN_POINT('Ctrl Pts',(5.38859046899994,15.2,8.94247683999998));
#213908=CARTESIAN_POINT('Ctrl Pts',(5.38859046899994,11.6,8.94247683999998));
#213909=CARTESIAN_POINT('Ctrl Pts',(5.38914067099994,15.2,8.94377590099998));
#213910=CARTESIAN_POINT('Ctrl Pts',(5.38914067099994,11.6,8.94377590099998));
#213911=CARTESIAN_POINT('Ctrl Pts',(5.38969285799995,15.2,8.94508313099998));
#213912=CARTESIAN_POINT('Ctrl Pts',(5.38969285799995,11.6,8.94508313099998));
#213913=CARTESIAN_POINT('Ctrl Pts',(5.39024700899994,15.2,8.94639851699999));
#213914=CARTESIAN_POINT('Ctrl Pts',(5.39024700899994,11.6,8.94639851699999));
#213915=CARTESIAN_POINT('Ctrl Pts',(5.39080310299994,15.2,8.94772204399998));
#213916=CARTESIAN_POINT('Ctrl Pts',(5.39080310299994,11.6,8.94772204399998));
#213917=CARTESIAN_POINT('Ctrl Pts',(5.39136111799994,15.2,8.94905370099998));
#213918=CARTESIAN_POINT('Ctrl Pts',(5.39136111799994,11.6,8.94905370099998));
#213919=CARTESIAN_POINT('Ctrl Pts',(5.39192103299994,15.2,8.95039347299999));
#213920=CARTESIAN_POINT('Ctrl Pts',(5.39192103299994,11.6,8.95039347299999));
#213921=CARTESIAN_POINT('Ctrl Pts',(5.39248282599995,15.2,8.95174134799999));
#213922=CARTESIAN_POINT('Ctrl Pts',(5.39248282599995,11.6,8.95174134799999));
#213923=CARTESIAN_POINT('Ctrl Pts',(5.39304647699994,15.2,8.95309731199998));
#213924=CARTESIAN_POINT('Ctrl Pts',(5.39304647699994,11.6,8.95309731199998));
#213925=CARTESIAN_POINT('Ctrl Pts',(5.39361196299994,15.2,8.95446135399999));
#213926=CARTESIAN_POINT('Ctrl Pts',(5.39361196299994,11.6,8.95446135399999));
#213927=CARTESIAN_POINT('Ctrl Pts',(5.39417926699994,15.2,8.95583345799999));
#213928=CARTESIAN_POINT('Ctrl Pts',(5.39417926699994,11.6,8.95583345799999));
#213929=CARTESIAN_POINT('Ctrl Pts',(5.39474836399994,15.2,8.95721361199998));
#213930=CARTESIAN_POINT('Ctrl Pts',(5.39474836399994,11.6,8.95721361199998));
#213931=CARTESIAN_POINT('Ctrl Pts',(5.39531923399994,15.2,8.95860180399998));
#213932=CARTESIAN_POINT('Ctrl Pts',(5.39531923399994,11.6,8.95860180399998));
#213933=CARTESIAN_POINT('Ctrl Pts',(5.39589185799994,15.2,8.95999802199999));
#213934=CARTESIAN_POINT('Ctrl Pts',(5.39589185799994,11.6,8.95999802199999));
#213935=CARTESIAN_POINT('Ctrl Pts',(5.39646621499994,15.2,8.96140224899998));
#213936=CARTESIAN_POINT('Ctrl Pts',(5.39646621499994,11.6,8.96140224899998));
#213937=CARTESIAN_POINT('Ctrl Pts',(5.39704228299994,15.2,8.96281447699998));
#213938=CARTESIAN_POINT('Ctrl Pts',(5.39704228299994,11.6,8.96281447699998));
#213939=CARTESIAN_POINT('Ctrl Pts',(5.39762004199994,15.2,8.96423468999998));
#213940=CARTESIAN_POINT('Ctrl Pts',(5.39762004199994,11.6,8.96423468999998));
#213941=CARTESIAN_POINT('Ctrl Pts',(5.39819947299994,15.2,8.96566287699999));
#213942=CARTESIAN_POINT('Ctrl Pts',(5.39819947299994,11.6,8.96566287699999));
#213943=CARTESIAN_POINT('Ctrl Pts',(5.39878055599995,15.2,8.96709902399999));
#213944=CARTESIAN_POINT('Ctrl Pts',(5.39878055599995,11.6,8.96709902399999));
#213945=CARTESIAN_POINT('Ctrl Pts',(5.39936326899994,15.2,8.96854311899999));
#213946=CARTESIAN_POINT('Ctrl Pts',(5.39936326899994,11.6,8.96854311899999));
#213947=CARTESIAN_POINT('Ctrl Pts',(5.39994759199994,15.2,8.96999514999998));
#213948=CARTESIAN_POINT('Ctrl Pts',(5.39994759199994,11.6,8.96999514999998));
#213949=CARTESIAN_POINT('Ctrl Pts',(5.40053350699995,15.2,8.97145510299998));
#213950=CARTESIAN_POINT('Ctrl Pts',(5.40053350699995,11.6,8.97145510299998));
#213951=CARTESIAN_POINT('Ctrl Pts',(5.40112099199994,15.2,8.97292296699998));
#213952=CARTESIAN_POINT('Ctrl Pts',(5.40112099199994,11.6,8.97292296699998));
#213953=CARTESIAN_POINT('Ctrl Pts',(5.40171002799994,15.2,8.97439872899999));
#213954=CARTESIAN_POINT('Ctrl Pts',(5.40171002799994,11.6,8.97439872899999));
#213955=CARTESIAN_POINT('Ctrl Pts',(5.40230059699994,15.2,8.97588237599999));
#213956=CARTESIAN_POINT('Ctrl Pts',(5.40230059699994,11.6,8.97588237599999));
#213957=CARTESIAN_POINT('Ctrl Pts',(5.40289267599994,15.2,8.97737389499999));
#213958=CARTESIAN_POINT('Ctrl Pts',(5.40289267599994,11.6,8.97737389499999));
#213959=CARTESIAN_POINT('Ctrl Pts',(5.40348624899995,15.2,8.97887327499999));
#213960=CARTESIAN_POINT('Ctrl Pts',(5.40348624899995,11.6,8.97887327499999));
#213961=CARTESIAN_POINT('Ctrl Pts',(5.40408129299994,15.2,8.98038050299999));
#213962=CARTESIAN_POINT('Ctrl Pts',(5.40408129299994,11.6,8.98038050299999));
#213963=CARTESIAN_POINT('Ctrl Pts',(5.40467779099994,15.2,8.98189556699998));
#213964=CARTESIAN_POINT('Ctrl Pts',(5.40467779099994,11.6,8.98189556699998));
#213965=CARTESIAN_POINT('Ctrl Pts',(5.40527572299994,15.2,8.98341845499999));
#213966=CARTESIAN_POINT('Ctrl Pts',(5.40527572299994,11.6,8.98341845499999));
#213967=CARTESIAN_POINT('Ctrl Pts',(5.40587506999994,15.2,8.98494915299998));
#213968=CARTESIAN_POINT('Ctrl Pts',(5.40587506999994,11.6,8.98494915299998));
#213969=CARTESIAN_POINT('Ctrl Pts',(5.40647581199994,15.2,8.98648765099999));
#213970=CARTESIAN_POINT('Ctrl Pts',(5.40647581199994,11.6,8.98648765099999));
#213971=CARTESIAN_POINT('Ctrl Pts',(5.40707793099994,15.2,8.98803393599999));
#213972=CARTESIAN_POINT('Ctrl Pts',(5.40707793099994,11.6,8.98803393599999));
#213973=CARTESIAN_POINT('Ctrl Pts',(5.40768140799995,15.2,8.98958799599999));
#213974=CARTESIAN_POINT('Ctrl Pts',(5.40768140799995,11.6,8.98958799599999));
#213975=CARTESIAN_POINT('Ctrl Pts',(5.40828622299994,15.2,8.99114981699999));
#213976=CARTESIAN_POINT('Ctrl Pts',(5.40828622299994,11.6,8.99114981699999));
#213977=CARTESIAN_POINT('Ctrl Pts',(5.40889235899994,15.2,8.99271938999998));
#213978=CARTESIAN_POINT('Ctrl Pts',(5.40889235899994,11.6,8.99271938999998));
#213979=CARTESIAN_POINT('Ctrl Pts',(5.40949979499994,15.2,8.99429669999999));
#213980=CARTESIAN_POINT('Ctrl Pts',(5.40949979499994,11.6,8.99429669999999));
#213981=CARTESIAN_POINT('Ctrl Pts',(5.41010851399994,15.2,8.99588173799999));
#213982=CARTESIAN_POINT('Ctrl Pts',(5.41010851399994,11.6,8.99588173799999));
#213983=CARTESIAN_POINT('Ctrl Pts',(5.41071849599994,15.2,8.99747448999998));
#213984=CARTESIAN_POINT('Ctrl Pts',(5.41071849599994,11.6,8.99747448999998));
#213985=CARTESIAN_POINT('Ctrl Pts',(5.41132972499994,15.2,8.99907494599999));
#213986=CARTESIAN_POINT('Ctrl Pts',(5.41132972499994,11.6,8.99907494599999));
#213987=CARTESIAN_POINT('Ctrl Pts',(5.41194217999994,15.2,9.00068309099998));
#213988=CARTESIAN_POINT('Ctrl Pts',(5.41194217999994,11.6,9.00068309099998));
#213989=CARTESIAN_POINT('Ctrl Pts',(5.41255584299994,15.2,9.00229891499999));
#213990=CARTESIAN_POINT('Ctrl Pts',(5.41255584299994,11.6,9.00229891499999));
#213991=CARTESIAN_POINT('Ctrl Pts',(5.41317069799994,15.2,9.00392240699999));
#213992=CARTESIAN_POINT('Ctrl Pts',(5.41317069799994,11.6,9.00392240699999));
#213993=CARTESIAN_POINT('Ctrl Pts',(5.41378672399994,15.2,9.00555355399998));
#213994=CARTESIAN_POINT('Ctrl Pts',(5.41378672399994,11.6,9.00555355399998));
#213995=CARTESIAN_POINT('Ctrl Pts',(5.41440390399995,15.2,9.00719234399999));
#213996=CARTESIAN_POINT('Ctrl Pts',(5.41440390399995,11.6,9.00719234399999));
#213997=CARTESIAN_POINT('Ctrl Pts',(5.41502221999994,15.2,9.00883876599998));
#213998=CARTESIAN_POINT('Ctrl Pts',(5.41502221999994,11.6,9.00883876599998));
#213999=CARTESIAN_POINT('Ctrl Pts',(5.41564165299994,15.2,9.01049280899999));
#214000=CARTESIAN_POINT('Ctrl Pts',(5.41564165299994,11.6,9.01049280899999));
#214001=CARTESIAN_POINT('Ctrl Pts',(5.41626218699994,15.2,9.01215445799998));
#214002=CARTESIAN_POINT('Ctrl Pts',(5.41626218699994,11.6,9.01215445799998));
#214003=CARTESIAN_POINT('Ctrl Pts',(5.41688380299994,15.2,9.01382370599999));
#214004=CARTESIAN_POINT('Ctrl Pts',(5.41688380299994,11.6,9.01382370599999));
#214005=CARTESIAN_POINT('Ctrl Pts',(5.41750648299994,15.2,9.01550053899999));
#214006=CARTESIAN_POINT('Ctrl Pts',(5.41750648299994,11.6,9.01550053899999));
#214007=CARTESIAN_POINT('Ctrl Pts',(5.41813020999994,15.2,9.01718494499999));
#214008=CARTESIAN_POINT('Ctrl Pts',(5.41813020999994,11.6,9.01718494499999));
#214009=CARTESIAN_POINT('Ctrl Pts',(5.41875496599994,15.2,9.01887691399999));
#214010=CARTESIAN_POINT('Ctrl Pts',(5.41875496599994,11.6,9.01887691399999));
#214011=CARTESIAN_POINT('Ctrl Pts',(5.41938073299994,15.2,9.02057643199999));
#214012=CARTESIAN_POINT('Ctrl Pts',(5.41938073299994,11.6,9.02057643199999));
#214013=CARTESIAN_POINT('Ctrl Pts',(5.42000749399994,15.2,9.02228348999999));
#214014=CARTESIAN_POINT('Ctrl Pts',(5.42000749399994,11.6,9.02228348999999));
#214015=CARTESIAN_POINT('Ctrl Pts',(5.42063523199994,15.2,9.02399807499998));
#214016=CARTESIAN_POINT('Ctrl Pts',(5.42063523199994,11.6,9.02399807499998));
#214017=CARTESIAN_POINT('Ctrl Pts',(5.42126392899994,15.2,9.02572017699999));
#214018=CARTESIAN_POINT('Ctrl Pts',(5.42126392899994,11.6,9.02572017699999));
#214019=CARTESIAN_POINT('Ctrl Pts',(5.42189356699994,15.2,9.02744978399999));
#214020=CARTESIAN_POINT('Ctrl Pts',(5.42189356699994,11.6,9.02744978399999));
#214021=CARTESIAN_POINT('Ctrl Pts',(5.42252413099994,15.2,9.02918688399998));
#214022=CARTESIAN_POINT('Ctrl Pts',(5.42252413099994,11.6,9.02918688399998));
#214023=CARTESIAN_POINT('Ctrl Pts',(5.42315560199994,15.2,9.03093146599998));
#214024=CARTESIAN_POINT('Ctrl Pts',(5.42315560199994,11.6,9.03093146599998));
#214025=CARTESIAN_POINT('Ctrl Pts',(5.42378796399994,15.2,9.03268351899998));
#214026=CARTESIAN_POINT('Ctrl Pts',(5.42378796399994,11.6,9.03268351899998));
#214027=CARTESIAN_POINT('Ctrl Pts',(5.42442119799994,15.2,9.03444303199999));
#214028=CARTESIAN_POINT('Ctrl Pts',(5.42442119799994,11.6,9.03444303199999));
#214029=CARTESIAN_POINT('Ctrl Pts',(5.42505528999994,15.2,9.03620999399998));
#214030=CARTESIAN_POINT('Ctrl Pts',(5.42505528999994,11.6,9.03620999399998));
#214031=CARTESIAN_POINT('Ctrl Pts',(5.42569022099994,15.2,9.03798439299998));
#214032=CARTESIAN_POINT('Ctrl Pts',(5.42569022099994,11.6,9.03798439299998));
#214033=CARTESIAN_POINT('Ctrl Pts',(5.42632597499994,15.2,9.03976621599998));
#214034=CARTESIAN_POINT('Ctrl Pts',(5.42632597499994,11.6,9.03976621599998));
#214035=CARTESIAN_POINT('Ctrl Pts',(5.42696253499994,15.2,9.04155545599998));
#214036=CARTESIAN_POINT('Ctrl Pts',(5.42696253499994,11.6,9.04155545599998));
#214037=CARTESIAN_POINT('Ctrl Pts',(5.42759988399994,15.2,9.04335209899998));
#214038=CARTESIAN_POINT('Ctrl Pts',(5.42759988399994,11.6,9.04335209899998));
#214039=CARTESIAN_POINT('Ctrl Pts',(5.42823800599994,15.2,9.04515613499999));
#214040=CARTESIAN_POINT('Ctrl Pts',(5.42823800599994,11.6,9.04515613499999));
#214041=CARTESIAN_POINT('Ctrl Pts',(5.42887688399994,15.2,9.04696755199998));
#214042=CARTESIAN_POINT('Ctrl Pts',(5.42887688399994,11.6,9.04696755199998));
#214043=CARTESIAN_POINT('Ctrl Pts',(5.42951650299995,15.2,9.04878633999999));
#214044=CARTESIAN_POINT('Ctrl Pts',(5.42951650299995,11.6,9.04878633999999));
#214045=CARTESIAN_POINT('Ctrl Pts',(5.43015684399994,15.2,9.05061248799999));
#214046=CARTESIAN_POINT('Ctrl Pts',(5.43015684399994,11.6,9.05061248799999));
#214047=CARTESIAN_POINT('Ctrl Pts',(5.43079789199994,15.2,9.05244598399998));
#214048=CARTESIAN_POINT('Ctrl Pts',(5.43079789199994,11.6,9.05244598399998));
#214049=CARTESIAN_POINT('Ctrl Pts',(5.43143963199994,15.2,9.05428681699998));
#214050=CARTESIAN_POINT('Ctrl Pts',(5.43143963199994,11.6,9.05428681699998));
#214051=CARTESIAN_POINT('Ctrl Pts',(5.43208204399994,15.2,9.05613497799998));
#214052=CARTESIAN_POINT('Ctrl Pts',(5.43208204399994,11.6,9.05613497799998));
#214053=CARTESIAN_POINT('Ctrl Pts',(5.43272511499994,15.2,9.05799045399998));
#214054=CARTESIAN_POINT('Ctrl Pts',(5.43272511499994,11.6,9.05799045399998));
#214055=CARTESIAN_POINT('Ctrl Pts',(5.43336882899994,15.2,9.05985323499999));
#214056=CARTESIAN_POINT('Ctrl Pts',(5.43336882899994,11.6,9.05985323499999));
#214057=CARTESIAN_POINT('Ctrl Pts',(5.43401316899994,15.2,9.06172330999999));
#214058=CARTESIAN_POINT('Ctrl Pts',(5.43401316899994,11.6,9.06172330999999));
#214059=CARTESIAN_POINT('Ctrl Pts',(5.43465811899994,15.2,9.06360066899998));
#214060=CARTESIAN_POINT('Ctrl Pts',(5.43465811899994,11.6,9.06360066899998));
#214061=CARTESIAN_POINT('Ctrl Pts',(5.43530366199994,15.2,9.06548529999998));
#214062=CARTESIAN_POINT('Ctrl Pts',(5.43530366199994,11.6,9.06548529999998));
#214063=CARTESIAN_POINT('Ctrl Pts',(5.43594978499994,15.2,9.06737719299999));
#214064=CARTESIAN_POINT('Ctrl Pts',(5.43594978499994,11.6,9.06737719299999));
#214065=CARTESIAN_POINT('Ctrl Pts',(5.43659646899994,15.2,9.06927633599998));
#214066=CARTESIAN_POINT('Ctrl Pts',(5.43659646899994,11.6,9.06927633599998));
#214067=CARTESIAN_POINT('Ctrl Pts',(5.43724370099994,15.2,9.07118272099999));
#214068=CARTESIAN_POINT('Ctrl Pts',(5.43724370099994,11.6,9.07118272099999));
#214069=CARTESIAN_POINT('Ctrl Pts',(5.43789146399994,15.2,9.07309633499998));
#214070=CARTESIAN_POINT('Ctrl Pts',(5.43789146399994,11.6,9.07309633499998));
#214071=CARTESIAN_POINT('Ctrl Pts',(5.43853974099994,15.2,9.07501716699999));
#214072=CARTESIAN_POINT('Ctrl Pts',(5.43853974099994,11.6,9.07501716699999));
#214073=CARTESIAN_POINT('Ctrl Pts',(5.43918851899994,15.2,9.07694520799998));
#214074=CARTESIAN_POINT('Ctrl Pts',(5.43918851899994,11.6,9.07694520799998));
#214075=CARTESIAN_POINT('Ctrl Pts',(5.43983778099994,15.2,9.07888044599999));
#214076=CARTESIAN_POINT('Ctrl Pts',(5.43983778099994,11.6,9.07888044599999));
#214077=CARTESIAN_POINT('Ctrl Pts',(5.44048751099994,15.2,9.08082287099998));
#214078=CARTESIAN_POINT('Ctrl Pts',(5.44048751099994,11.6,9.08082287099998));
#214079=CARTESIAN_POINT('Ctrl Pts',(5.44113769599995,15.2,9.08277247399998));
#214080=CARTESIAN_POINT('Ctrl Pts',(5.44113769599995,11.6,9.08277247399998));
#214081=CARTESIAN_POINT('Ctrl Pts',(5.44178831799995,15.2,9.08472924199998));
#214082=CARTESIAN_POINT('Ctrl Pts',(5.44178831799995,11.6,9.08472924199998));
#214083=CARTESIAN_POINT('Ctrl Pts',(5.44243936299995,15.2,9.08669316599998));
#214084=CARTESIAN_POINT('Ctrl Pts',(5.44243936299995,11.6,9.08669316599998));
#214085=CARTESIAN_POINT('Ctrl Pts',(5.44309081699994,15.2,9.08866423499998));
#214086=CARTESIAN_POINT('Ctrl Pts',(5.44309081699994,11.6,9.08866423499998));
#214087=CARTESIAN_POINT('Ctrl Pts',(5.44374266099994,15.2,9.09064243899999));
#214088=CARTESIAN_POINT('Ctrl Pts',(5.44374266099994,11.6,9.09064243899999));
#214089=CARTESIAN_POINT('Ctrl Pts',(5.44439488399994,15.2,9.09262776599999));
#214090=CARTESIAN_POINT('Ctrl Pts',(5.44439488399994,11.6,9.09262776599999));
#214091=CARTESIAN_POINT('Ctrl Pts',(5.44504746899994,15.2,9.09462020699999));
#214092=CARTESIAN_POINT('Ctrl Pts',(5.44504746899994,11.6,9.09462020699999));
#214093=CARTESIAN_POINT('Ctrl Pts',(5.44570040099994,15.2,9.09661975099999));
#214094=CARTESIAN_POINT('Ctrl Pts',(5.44570040099994,11.6,9.09661975099999));
#214095=CARTESIAN_POINT('Ctrl Pts',(5.44635366499994,15.2,9.09862638899998));
#214096=CARTESIAN_POINT('Ctrl Pts',(5.44635366499994,11.6,9.09862638899998));
#214097=CARTESIAN_POINT('Ctrl Pts',(5.44700724699994,15.2,9.10064010899998));
#214098=CARTESIAN_POINT('Ctrl Pts',(5.44700724699994,11.6,9.10064010899998));
#214099=CARTESIAN_POINT('Ctrl Pts',(5.44766113199994,15.2,9.10266090099999));
#214100=CARTESIAN_POINT('Ctrl Pts',(5.44766113199994,11.6,9.10266090099999));
#214101=CARTESIAN_POINT('Ctrl Pts',(5.44831530399994,15.2,9.10468875599998));
#214102=CARTESIAN_POINT('Ctrl Pts',(5.44831530399994,11.6,9.10468875599998));
#214103=CARTESIAN_POINT('Ctrl Pts',(5.44896974899994,15.2,9.10672366199999));
#214104=CARTESIAN_POINT('Ctrl Pts',(5.44896974899994,11.6,9.10672366199999));
#214105=CARTESIAN_POINT('Ctrl Pts',(5.44962445199995,15.2,9.10876560899998));
#214106=CARTESIAN_POINT('Ctrl Pts',(5.44962445199995,11.6,9.10876560899998));
#214107=CARTESIAN_POINT('Ctrl Pts',(5.45027939899994,15.2,9.11081458899999));
#214108=CARTESIAN_POINT('Ctrl Pts',(5.45027939899994,11.6,9.11081458899999));
#214109=CARTESIAN_POINT('Ctrl Pts',(5.45093457599994,15.2,9.11287058899998));
#214110=CARTESIAN_POINT('Ctrl Pts',(5.45093457599994,11.6,9.11287058899998));
#214111=CARTESIAN_POINT('Ctrl Pts',(5.45158996599994,15.2,9.11493359899998));
#214112=CARTESIAN_POINT('Ctrl Pts',(5.45158996599994,11.6,9.11493359899998));
#214113=CARTESIAN_POINT('Ctrl Pts',(5.45224555799994,15.2,9.11700361099999));
#214114=CARTESIAN_POINT('Ctrl Pts',(5.45224555799994,11.6,9.11700361099999));
#214115=CARTESIAN_POINT('Ctrl Pts',(5.45290133399994,15.2,9.11908061299999));
#214116=CARTESIAN_POINT('Ctrl Pts',(5.45290133399994,11.6,9.11908061299999));
#214117=CARTESIAN_POINT('Ctrl Pts',(5.45355728299994,15.2,9.12116459599999));
#214118=CARTESIAN_POINT('Ctrl Pts',(5.45355728299994,11.6,9.12116459599999));
#214119=CARTESIAN_POINT('Ctrl Pts',(5.45421338799994,15.2,9.12325554899999));
#214120=CARTESIAN_POINT('Ctrl Pts',(5.45421338799994,11.6,9.12325554899999));
#214121=CARTESIAN_POINT('Ctrl Pts',(5.45486963699994,15.2,9.12535346199999));
#214122=CARTESIAN_POINT('Ctrl Pts',(5.45486963699994,11.6,9.12535346199999));
#214123=CARTESIAN_POINT('Ctrl Pts',(5.45552601299994,15.2,9.12745832599999));
#214124=CARTESIAN_POINT('Ctrl Pts',(5.45552601299994,11.6,9.12745832599999));
#214125=CARTESIAN_POINT('Ctrl Pts',(5.45618250499994,15.2,9.12957012999998));
#214126=CARTESIAN_POINT('Ctrl Pts',(5.45618250499994,11.6,9.12957012999998));
#214127=CARTESIAN_POINT('Ctrl Pts',(5.45683909599994,15.2,9.13168886499999));
#214128=CARTESIAN_POINT('Ctrl Pts',(5.45683909599994,11.6,9.13168886499999));
#214129=CARTESIAN_POINT('Ctrl Pts',(5.45749577399994,15.2,9.13381451899999));
#214130=CARTESIAN_POINT('Ctrl Pts',(5.45749577399994,11.6,9.13381451899999));
#214131=CARTESIAN_POINT('Ctrl Pts',(5.45815252399994,15.2,9.13594708299998));
#214132=CARTESIAN_POINT('Ctrl Pts',(5.45815252399994,11.6,9.13594708299998));
#214133=CARTESIAN_POINT('Ctrl Pts',(5.45880933199994,15.2,9.13808654799999));
#214134=CARTESIAN_POINT('Ctrl Pts',(5.45880933199994,11.6,9.13808654799999));
#214135=CARTESIAN_POINT('Ctrl Pts',(5.45946618499994,15.2,9.14023290499999));
#214136=CARTESIAN_POINT('Ctrl Pts',(5.45946618499994,11.6,9.14023290499999));
#214137=CARTESIAN_POINT('Ctrl Pts',(5.46012306899994,15.2,9.14238613999999));
#214138=CARTESIAN_POINT('Ctrl Pts',(5.46012306899994,11.6,9.14238613999999));
#214139=CARTESIAN_POINT('Ctrl Pts',(5.46077996899994,15.2,9.14454624699999));
#214140=CARTESIAN_POINT('Ctrl Pts',(5.46077996899994,11.6,9.14454624699999));
#214141=CARTESIAN_POINT('Ctrl Pts',(5.46143687199994,15.2,9.14671321499998));
#214142=CARTESIAN_POINT('Ctrl Pts',(5.46143687199994,11.6,9.14671321499998));
#214143=CARTESIAN_POINT('Ctrl Pts',(5.46209376399994,15.2,9.14888703299999));
#214144=CARTESIAN_POINT('Ctrl Pts',(5.46209376399994,11.6,9.14888703299999));
#214145=CARTESIAN_POINT('Ctrl Pts',(5.46275063199994,15.2,9.15106769299998));
#214146=CARTESIAN_POINT('Ctrl Pts',(5.46275063199994,11.6,9.15106769299998));
#214147=CARTESIAN_POINT('Ctrl Pts',(5.46340746199994,15.2,9.15325518399998));
#214148=CARTESIAN_POINT('Ctrl Pts',(5.46340746199994,11.6,9.15325518399998));
#214149=CARTESIAN_POINT('Ctrl Pts',(5.46406423999994,15.2,9.15544949699999));
#214150=CARTESIAN_POINT('Ctrl Pts',(5.46406423999994,11.6,9.15544949699999));
#214151=CARTESIAN_POINT('Ctrl Pts',(5.46472095299994,15.2,9.15765062199998));
#214152=CARTESIAN_POINT('Ctrl Pts',(5.46472095299994,11.6,9.15765062199998));
#214153=CARTESIAN_POINT('Ctrl Pts',(5.46537758699994,15.2,9.15985854799998));
#214154=CARTESIAN_POINT('Ctrl Pts',(5.46537758699994,11.6,9.15985854799998));
#214155=CARTESIAN_POINT('Ctrl Pts',(5.46603412999994,15.2,9.16207326799999));
#214156=CARTESIAN_POINT('Ctrl Pts',(5.46603412999994,11.6,9.16207326799999));
#214157=CARTESIAN_POINT('Ctrl Pts',(5.46669056599994,15.2,9.16429476899999));
#214158=CARTESIAN_POINT('Ctrl Pts',(5.46669056599994,11.6,9.16429476899999));
#214159=CARTESIAN_POINT('Ctrl Pts',(5.46734688499994,15.2,9.16652304399998));
#214160=CARTESIAN_POINT('Ctrl Pts',(5.46734688499994,11.6,9.16652304399998));
#214161=CARTESIAN_POINT('Ctrl Pts',(5.46800306999994,15.2,9.16875808199999));
#214162=CARTESIAN_POINT('Ctrl Pts',(5.46800306999994,11.6,9.16875808199999));
#214163=CARTESIAN_POINT('Ctrl Pts',(5.46865911099994,15.2,9.17099987499999));
#214164=CARTESIAN_POINT('Ctrl Pts',(5.46865911099994,11.6,9.17099987499999));
#214165=CARTESIAN_POINT('Ctrl Pts',(5.46931499299994,15.2,9.17324841099998));
#214166=CARTESIAN_POINT('Ctrl Pts',(5.46931499299994,11.6,9.17324841099998));
#214167=CARTESIAN_POINT('Ctrl Pts',(5.46997070299994,15.2,9.17550368099998));
#214168=CARTESIAN_POINT('Ctrl Pts',(5.46997070299994,11.6,9.17550368099998));
#214169=CARTESIAN_POINT('Ctrl Pts',(5.47062622799994,15.2,9.17776567599999));
#214170=CARTESIAN_POINT('Ctrl Pts',(5.47062622799994,11.6,9.17776567599999));
#214171=CARTESIAN_POINT('Ctrl Pts',(5.47128155699994,15.2,9.18003438799998));
#214172=CARTESIAN_POINT('Ctrl Pts',(5.47128155699994,11.6,9.18003438799998));
#214173=CARTESIAN_POINT('Ctrl Pts',(5.47193667299994,15.2,9.18230980399999));
#214174=CARTESIAN_POINT('Ctrl Pts',(5.47193667299994,11.6,9.18230980399999));
#214175=CARTESIAN_POINT('Ctrl Pts',(5.47259156599995,15.2,9.18459191699998));
#214176=CARTESIAN_POINT('Ctrl Pts',(5.47259156599995,11.6,9.18459191699998));
#214177=CARTESIAN_POINT('Ctrl Pts',(5.47324622199994,15.2,9.18688071699999));
#214178=CARTESIAN_POINT('Ctrl Pts',(5.47324622199994,11.6,9.18688071699999));
#214179=CARTESIAN_POINT('Ctrl Pts',(5.47390062799994,15.2,9.18917619399998));
#214180=CARTESIAN_POINT('Ctrl Pts',(5.47390062799994,11.6,9.18917619399998));
#214181=CARTESIAN_POINT('Ctrl Pts',(5.47455477099994,15.2,9.19147833999999));
#214182=CARTESIAN_POINT('Ctrl Pts',(5.47455477099994,11.6,9.19147833999999));
#214183=CARTESIAN_POINT('Ctrl Pts',(5.47520863999994,15.2,9.19378714299998));
#214184=CARTESIAN_POINT('Ctrl Pts',(5.47520863999994,11.6,9.19378714299998));
#214185=CARTESIAN_POINT('Ctrl Pts',(5.47586222099994,15.2,9.19610259599999));
#214186=CARTESIAN_POINT('Ctrl Pts',(5.47586222099994,11.6,9.19610259599999));
#214187=CARTESIAN_POINT('Ctrl Pts',(5.47651549999994,15.2,9.19842468799999));
#214188=CARTESIAN_POINT('Ctrl Pts',(5.47651549999994,11.6,9.19842468799999));
#214189=CARTESIAN_POINT('Ctrl Pts',(5.47716846599994,15.2,9.20075340999999));
#214190=CARTESIAN_POINT('Ctrl Pts',(5.47716846599994,11.6,9.20075340999999));
#214191=CARTESIAN_POINT('Ctrl Pts',(5.47782110499995,15.2,9.20308875299998));
#214192=CARTESIAN_POINT('Ctrl Pts',(5.47782110499995,11.6,9.20308875299998));
#214193=CARTESIAN_POINT('Ctrl Pts',(5.47847340599994,15.2,9.20543070799998));
#214194=CARTESIAN_POINT('Ctrl Pts',(5.47847340599994,11.6,9.20543070799998));
#214195=CARTESIAN_POINT('Ctrl Pts',(5.47912535699994,15.2,9.20777926499999));
#214196=CARTESIAN_POINT('Ctrl Pts',(5.47912535699994,11.6,9.20777926499999));
#214197=CARTESIAN_POINT('Ctrl Pts',(5.47977694299994,15.2,9.21013441399998));
#214198=CARTESIAN_POINT('Ctrl Pts',(5.47977694299994,11.6,9.21013441399998));
#214199=CARTESIAN_POINT('Ctrl Pts',(5.48042815199994,15.2,9.21249614799999));
#214200=CARTESIAN_POINT('Ctrl Pts',(5.48042815199994,11.6,9.21249614799999));
#214201=CARTESIAN_POINT('Ctrl Pts',(5.48107897199994,15.2,9.21486445499998));
#214202=CARTESIAN_POINT('Ctrl Pts',(5.48107897199994,11.6,9.21486445499998));
#214203=CARTESIAN_POINT('Ctrl Pts',(5.48172939199994,15.2,9.21723932699998));
#214204=CARTESIAN_POINT('Ctrl Pts',(5.48172939199994,11.6,9.21723932699998));
#214205=CARTESIAN_POINT('Ctrl Pts',(5.48237939899994,15.2,9.21962075499999));
#214206=CARTESIAN_POINT('Ctrl Pts',(5.48237939899994,11.6,9.21962075499999));
#214207=CARTESIAN_POINT('Ctrl Pts',(5.48302897899994,15.2,9.22200872899998));
#214208=CARTESIAN_POINT('Ctrl Pts',(5.48302897899994,11.6,9.22200872899998));
#214209=CARTESIAN_POINT('Ctrl Pts',(5.48367812199994,15.2,9.22440324099998));
#214210=CARTESIAN_POINT('Ctrl Pts',(5.48367812199994,11.6,9.22440324099998));
#214211=CARTESIAN_POINT('Ctrl Pts',(5.48432681499994,15.2,9.22680428099999));
#214212=CARTESIAN_POINT('Ctrl Pts',(5.48432681499994,11.6,9.22680428099999));
#214213=CARTESIAN_POINT('Ctrl Pts',(5.48497504599994,15.2,9.22921183899999));
#214214=CARTESIAN_POINT('Ctrl Pts',(5.48497504599994,11.6,9.22921183899999));
#214215=CARTESIAN_POINT('Ctrl Pts',(5.48562280099994,15.2,9.23162590799999));
#214216=CARTESIAN_POINT('Ctrl Pts',(5.48562280099994,11.6,9.23162590799999));
#214217=CARTESIAN_POINT('Ctrl Pts',(5.48627006999994,15.2,9.23404647599998));
#214218=CARTESIAN_POINT('Ctrl Pts',(5.48627006999994,11.6,9.23404647599998));
#214219=CARTESIAN_POINT('Ctrl Pts',(5.48691684099994,15.2,9.23647353599998));
#214220=CARTESIAN_POINT('Ctrl Pts',(5.48691684099994,11.6,9.23647353599998));
#214221=CARTESIAN_POINT('Ctrl Pts',(5.48756310199994,15.2,9.23890707899999));
#214222=CARTESIAN_POINT('Ctrl Pts',(5.48756310199994,11.6,9.23890707899999));
#214223=CARTESIAN_POINT('Ctrl Pts',(5.48820883899994,15.2,9.24134709399999));
#214224=CARTESIAN_POINT('Ctrl Pts',(5.48820883899994,11.6,9.24134709399999));
#214225=CARTESIAN_POINT('Ctrl Pts',(5.48885404099994,15.2,9.24379357399999));
#214226=CARTESIAN_POINT('Ctrl Pts',(5.48885404099994,11.6,9.24379357399999));
#214227=CARTESIAN_POINT('Ctrl Pts',(5.48949869799994,15.2,9.24624650799998));
#214228=CARTESIAN_POINT('Ctrl Pts',(5.48949869799994,11.6,9.24624650799998));
#214229=CARTESIAN_POINT('Ctrl Pts',(5.49014279599994,15.2,9.24870588899999));
#214230=CARTESIAN_POINT('Ctrl Pts',(5.49014279599994,11.6,9.24870588899999));
#214231=CARTESIAN_POINT('Ctrl Pts',(5.49078632299994,15.2,9.25117170699998));
#214232=CARTESIAN_POINT('Ctrl Pts',(5.49078632299994,11.6,9.25117170699998));
#214233=CARTESIAN_POINT('Ctrl Pts',(5.49142926899994,15.2,9.25364395199999));
#214234=CARTESIAN_POINT('Ctrl Pts',(5.49142926899994,11.6,9.25364395199999));
#214235=CARTESIAN_POINT('Ctrl Pts',(5.49207162099994,15.2,9.25612261599999));
#214236=CARTESIAN_POINT('Ctrl Pts',(5.49207162099994,11.6,9.25612261599999));
#214237=CARTESIAN_POINT('Ctrl Pts',(5.49271336799994,15.2,9.25860769099998));
#214238=CARTESIAN_POINT('Ctrl Pts',(5.49271336799994,11.6,9.25860769099998));
#214239=CARTESIAN_POINT('Ctrl Pts',(5.49335449699995,15.2,9.26109916599999));
#214240=CARTESIAN_POINT('Ctrl Pts',(5.49335449699995,11.6,9.26109916599999));
#214241=CARTESIAN_POINT('Ctrl Pts',(5.49399499799994,15.2,9.26359703299998));
#214242=CARTESIAN_POINT('Ctrl Pts',(5.49399499799994,11.6,9.26359703299998));
#214243=CARTESIAN_POINT('Ctrl Pts',(5.49463485899994,15.2,9.26610128399999));
#214244=CARTESIAN_POINT('Ctrl Pts',(5.49463485899994,11.6,9.26610128399999));
#214245=CARTESIAN_POINT('Ctrl Pts',(5.49527406699994,15.2,9.26861190799999));
#214246=CARTESIAN_POINT('Ctrl Pts',(5.49527406699994,11.6,9.26861190799999));
#214247=CARTESIAN_POINT('Ctrl Pts',(5.49591261199994,15.2,9.27112889799999));
#214248=CARTESIAN_POINT('Ctrl Pts',(5.49591261199994,11.6,9.27112889799999));
#214249=CARTESIAN_POINT('Ctrl Pts',(5.49655048199994,15.2,9.27365224499999));
#214250=CARTESIAN_POINT('Ctrl Pts',(5.49655048199994,11.6,9.27365224499999));
#214251=CARTESIAN_POINT('Ctrl Pts',(5.49718766599994,15.2,9.27618193799999));
#214252=CARTESIAN_POINT('Ctrl Pts',(5.49718766599994,11.6,9.27618193799999));
#214253=CARTESIAN_POINT('Ctrl Pts',(5.49782415299994,15.2,9.27871796999998));
#214254=CARTESIAN_POINT('Ctrl Pts',(5.49782415299994,11.6,9.27871796999998));
#214255=CARTESIAN_POINT('Ctrl Pts',(5.49845992999995,15.2,9.28126033199998));
#214256=CARTESIAN_POINT('Ctrl Pts',(5.49845992999995,11.6,9.28126033199998));
#214257=CARTESIAN_POINT('Ctrl Pts',(5.49909498699994,15.2,9.28380901499999));
#214258=CARTESIAN_POINT('Ctrl Pts',(5.49909498699994,11.6,9.28380901499999));
#214259=CARTESIAN_POINT('Ctrl Pts',(5.49972931199994,15.2,9.28636400999999));
#214260=CARTESIAN_POINT('Ctrl Pts',(5.49972931199994,11.6,9.28636400999999));
#214261=CARTESIAN_POINT('Ctrl Pts',(5.50036289399994,15.2,9.28892530799999));
#214262=CARTESIAN_POINT('Ctrl Pts',(5.50036289399994,11.6,9.28892530799999));
#214263=CARTESIAN_POINT('Ctrl Pts',(5.50099572099994,15.2,9.29149289999998));
#214264=CARTESIAN_POINT('Ctrl Pts',(5.50099572099994,11.6,9.29149289999998));
#214265=CARTESIAN_POINT('Ctrl Pts',(5.50162778299994,15.2,9.29406677899999));
#214266=CARTESIAN_POINT('Ctrl Pts',(5.50162778299994,11.6,9.29406677899999));
#214267=CARTESIAN_POINT('Ctrl Pts',(5.50225906899994,15.2,9.29664693499999));
#214268=CARTESIAN_POINT('Ctrl Pts',(5.50225906899994,11.6,9.29664693499999));
#214269=CARTESIAN_POINT('Ctrl Pts',(5.50288956699994,15.2,9.29923335799998));
#214270=CARTESIAN_POINT('Ctrl Pts',(5.50288956699994,11.6,9.29923335799998));
#214271=CARTESIAN_POINT('Ctrl Pts',(5.50351926699994,15.2,9.30182604099999));
#214272=CARTESIAN_POINT('Ctrl Pts',(5.50351926699994,11.6,9.30182604099999));
#214273=CARTESIAN_POINT('Ctrl Pts',(5.50414815599994,15.2,9.30442497499998));
#214274=CARTESIAN_POINT('Ctrl Pts',(5.50414815599994,11.6,9.30442497499998));
#214275=CARTESIAN_POINT('Ctrl Pts',(5.50477622399995,15.2,9.30703015099999));
#214276=CARTESIAN_POINT('Ctrl Pts',(5.50477622399995,11.6,9.30703015099999));
#214277=CARTESIAN_POINT('Ctrl Pts',(5.50540345999995,15.2,9.30964156099999));
#214278=CARTESIAN_POINT('Ctrl Pts',(5.50540345999995,11.6,9.30964156099999));
#214279=CARTESIAN_POINT('Ctrl Pts',(5.50602985399995,15.2,9.31225919499998));
#214280=CARTESIAN_POINT('Ctrl Pts',(5.50602985399995,11.6,9.31225919499998));
#214281=CARTESIAN_POINT('Ctrl Pts',(5.50665539399994,15.2,9.31488304499998));
#214282=CARTESIAN_POINT('Ctrl Pts',(5.50665539399994,11.6,9.31488304499998));
#214283=CARTESIAN_POINT('Ctrl Pts',(5.50728006899995,15.2,9.31751310199999));
#214284=CARTESIAN_POINT('Ctrl Pts',(5.50728006899995,11.6,9.31751310199999));
#214285=CARTESIAN_POINT('Ctrl Pts',(5.50790386899994,15.2,9.32014935899998));
#214286=CARTESIAN_POINT('Ctrl Pts',(5.50790386899994,11.6,9.32014935899998));
#214287=CARTESIAN_POINT('Ctrl Pts',(5.50852678199995,15.2,9.32279180499999));
#214288=CARTESIAN_POINT('Ctrl Pts',(5.50852678199995,11.6,9.32279180499999));
#214289=CARTESIAN_POINT('Ctrl Pts',(5.50914879799994,15.2,9.32544043399999));
#214290=CARTESIAN_POINT('Ctrl Pts',(5.50914879799994,11.6,9.32544043399999));
#214291=CARTESIAN_POINT('Ctrl Pts',(5.50976990699994,15.2,9.32809523399998));
#214292=CARTESIAN_POINT('Ctrl Pts',(5.50976990699994,11.6,9.32809523399998));
#214293=CARTESIAN_POINT('Ctrl Pts',(5.51039009699994,15.2,9.33075619999999));
#214294=CARTESIAN_POINT('Ctrl Pts',(5.51039009699994,11.6,9.33075619999999));
#214295=CARTESIAN_POINT('Ctrl Pts',(5.51100935799995,15.2,9.33342332199998));
#214296=CARTESIAN_POINT('Ctrl Pts',(5.51100935799995,11.6,9.33342332199998));
#214297=CARTESIAN_POINT('Ctrl Pts',(5.51162767899994,15.2,9.33609658999998));
#214298=CARTESIAN_POINT('Ctrl Pts',(5.51162767899994,11.6,9.33609658999998));
#214299=CARTESIAN_POINT('Ctrl Pts',(5.51224504999994,15.2,9.33877599699999));
#214300=CARTESIAN_POINT('Ctrl Pts',(5.51224504999994,11.6,9.33877599699999));
#214301=CARTESIAN_POINT('Ctrl Pts',(5.51286145799994,15.2,9.34146153499999));
#214302=CARTESIAN_POINT('Ctrl Pts',(5.51286145799994,11.6,9.34146153499999));
#214303=CARTESIAN_POINT('Ctrl Pts',(5.51347689599995,15.2,9.34415319399999));
#214304=CARTESIAN_POINT('Ctrl Pts',(5.51347689599995,11.6,9.34415319399999));
#214305=CARTESIAN_POINT('Ctrl Pts',(5.51409135199994,15.2,9.34685096699998));
#214306=CARTESIAN_POINT('Ctrl Pts',(5.51409135199994,11.6,9.34685096699998));
#214307=CARTESIAN_POINT('Ctrl Pts',(5.51470481499994,15.2,9.34955484399998));
#214308=CARTESIAN_POINT('Ctrl Pts',(5.51470481499994,11.6,9.34955484399998));
#214309=CARTESIAN_POINT('Ctrl Pts',(5.51531727499994,15.2,9.35226481699999));
#214310=CARTESIAN_POINT('Ctrl Pts',(5.51531727499994,11.6,9.35226481699999));
#214311=CARTESIAN_POINT('Ctrl Pts',(5.51592872199994,15.2,9.35498087899998));
#214312=CARTESIAN_POINT('Ctrl Pts',(5.51592872199994,11.6,9.35498087899998));
#214313=CARTESIAN_POINT('Ctrl Pts',(5.51653914399994,15.2,9.35770301999998));
#214314=CARTESIAN_POINT('Ctrl Pts',(5.51653914399994,11.6,9.35770301999998));
#214315=CARTESIAN_POINT('Ctrl Pts',(5.51714853299995,15.2,9.36043123099999));
#214316=CARTESIAN_POINT('Ctrl Pts',(5.51714853299995,11.6,9.36043123099999));
#214317=CARTESIAN_POINT('Ctrl Pts',(5.51775687699994,15.2,9.36316550599999));
#214318=CARTESIAN_POINT('Ctrl Pts',(5.51775687699994,11.6,9.36316550599999));
#214319=CARTESIAN_POINT('Ctrl Pts',(5.51836416599994,15.2,9.36590583399998));
#214320=CARTESIAN_POINT('Ctrl Pts',(5.51836416599994,11.6,9.36590583399998));
#214321=CARTESIAN_POINT('Ctrl Pts',(5.51897038999994,15.2,9.36865220899998));
#214322=CARTESIAN_POINT('Ctrl Pts',(5.51897038999994,11.6,9.36865220899998));
#214323=CARTESIAN_POINT('Ctrl Pts',(5.51957553899994,15.2,9.37140461999999));
#214324=CARTESIAN_POINT('Ctrl Pts',(5.51957553899994,11.6,9.37140461999999));
#214325=CARTESIAN_POINT('Ctrl Pts',(5.52017960199994,15.2,9.37416306199999));
#214326=CARTESIAN_POINT('Ctrl Pts',(5.52017960199994,11.6,9.37416306199999));
#214327=CARTESIAN_POINT('Ctrl Pts',(5.52078256999994,15.2,9.37692752199998));
#214328=CARTESIAN_POINT('Ctrl Pts',(5.52078256999994,11.6,9.37692752199998));
#214329=CARTESIAN_POINT('Ctrl Pts',(5.52138443099994,15.2,9.37969799599998));
#214330=CARTESIAN_POINT('Ctrl Pts',(5.52138443099994,11.6,9.37969799599998));
#214331=CARTESIAN_POINT('Ctrl Pts',(5.52198517699994,15.2,9.38247447399998));
#214332=CARTESIAN_POINT('Ctrl Pts',(5.52198517699994,11.6,9.38247447399998));
#214333=CARTESIAN_POINT('Ctrl Pts',(5.52258479599995,15.2,9.38525694799999));
#214334=CARTESIAN_POINT('Ctrl Pts',(5.52258479599995,11.6,9.38525694799999));
#214335=CARTESIAN_POINT('Ctrl Pts',(5.52318327999994,15.2,9.38804540799998));
#214336=CARTESIAN_POINT('Ctrl Pts',(5.52318327999994,11.6,9.38804540799998));
#214337=CARTESIAN_POINT('Ctrl Pts',(5.52378061699994,15.2,9.39083984899998));
#214338=CARTESIAN_POINT('Ctrl Pts',(5.52378061699994,11.6,9.39083984899998));
#214339=CARTESIAN_POINT('Ctrl Pts',(5.52437679899994,15.2,9.39364025899999));
#214340=CARTESIAN_POINT('Ctrl Pts',(5.52437679899994,11.6,9.39364025899999));
#214341=CARTESIAN_POINT('Ctrl Pts',(5.52497181399994,15.2,9.39644663299998));
#214342=CARTESIAN_POINT('Ctrl Pts',(5.52497181399994,11.6,9.39644663299998));
#214343=CARTESIAN_POINT('Ctrl Pts',(5.52556565399994,15.2,9.39925895999998));
#214344=CARTESIAN_POINT('Ctrl Pts',(5.52556565399994,11.6,9.39925895999998));
#214345=CARTESIAN_POINT('Ctrl Pts',(5.52615830699994,15.2,9.40207723399999));
#214346=CARTESIAN_POINT('Ctrl Pts',(5.52615830699994,11.6,9.40207723399999));
#214347=CARTESIAN_POINT('Ctrl Pts',(5.52674976499994,15.2,9.40490144499999));
#214348=CARTESIAN_POINT('Ctrl Pts',(5.52674976499994,11.6,9.40490144499999));
#214349=CARTESIAN_POINT('Ctrl Pts',(5.52734001699994,15.2,9.40773158699999));
#214350=CARTESIAN_POINT('Ctrl Pts',(5.52734001699994,11.6,9.40773158699999));
#214351=CARTESIAN_POINT('Ctrl Pts',(5.52792905399994,15.2,9.41056764999999));
#214352=CARTESIAN_POINT('Ctrl Pts',(5.52792905399994,11.6,9.41056764999999));
#214353=CARTESIAN_POINT('Ctrl Pts',(5.52851686599994,15.2,9.41340962499999));
#214354=CARTESIAN_POINT('Ctrl Pts',(5.52851686599994,11.6,9.41340962499999));
#214355=CARTESIAN_POINT('Ctrl Pts',(5.52910344299995,15.2,9.41625750699998));
#214356=CARTESIAN_POINT('Ctrl Pts',(5.52910344299995,11.6,9.41625750699998));
#214357=CARTESIAN_POINT('Ctrl Pts',(5.52968877499994,15.2,9.41911128399998));
#214358=CARTESIAN_POINT('Ctrl Pts',(5.52968877499994,11.6,9.41911128399998));
#214359=CARTESIAN_POINT('Ctrl Pts',(5.53027285299994,15.2,9.42197095099999));
#214360=CARTESIAN_POINT('Ctrl Pts',(5.53027285299994,11.6,9.42197095099999));
#214361=CARTESIAN_POINT('Ctrl Pts',(5.53085566699995,15.2,9.42483649799998));
#214362=CARTESIAN_POINT('Ctrl Pts',(5.53085566699995,11.6,9.42483649799998));
#214363=CARTESIAN_POINT('Ctrl Pts',(5.53143720799994,15.2,9.42770791799998));
#214364=CARTESIAN_POINT('Ctrl Pts',(5.53143720799994,11.6,9.42770791799998));
#214365=CARTESIAN_POINT('Ctrl Pts',(5.53201746599995,15.2,9.43058520199998));
#214366=CARTESIAN_POINT('Ctrl Pts',(5.53201746599995,11.6,9.43058520199998));
#214367=CARTESIAN_POINT('Ctrl Pts',(5.53259642999994,15.2,9.43346834199998));
#214368=CARTESIAN_POINT('Ctrl Pts',(5.53259642999994,11.6,9.43346834199998));
#214369=CARTESIAN_POINT('Ctrl Pts',(5.53317409299994,15.2,9.43635733099999));
#214370=CARTESIAN_POINT('Ctrl Pts',(5.53317409299994,11.6,9.43635733099999));
#214371=CARTESIAN_POINT('Ctrl Pts',(5.53375044299995,15.2,9.43925215999998));
#214372=CARTESIAN_POINT('Ctrl Pts',(5.53375044299995,11.6,9.43925215999998));
#214373=CARTESIAN_POINT('Ctrl Pts',(5.53432547199994,15.2,9.44215281999998));
#214374=CARTESIAN_POINT('Ctrl Pts',(5.53432547199994,11.6,9.44215281999998));
#214375=CARTESIAN_POINT('Ctrl Pts',(5.53489916999995,15.2,9.44505930399998));
#214376=CARTESIAN_POINT('Ctrl Pts',(5.53489916999995,11.6,9.44505930399998));
#214377=CARTESIAN_POINT('Ctrl Pts',(5.53547152799994,15.2,9.44797160399999));
#214378=CARTESIAN_POINT('Ctrl Pts',(5.53547152799994,11.6,9.44797160399999));
#214379=CARTESIAN_POINT('Ctrl Pts',(5.53604253599995,15.2,9.45088971299998));
#214380=CARTESIAN_POINT('Ctrl Pts',(5.53604253599995,11.6,9.45088971299998));
#214381=CARTESIAN_POINT('Ctrl Pts',(5.53661218599995,15.2,9.45381362099998));
#214382=CARTESIAN_POINT('Ctrl Pts',(5.53661218599995,11.6,9.45381362099998));
#214383=CARTESIAN_POINT('Ctrl Pts',(5.53718046699994,15.2,9.45674331999999));
#214384=CARTESIAN_POINT('Ctrl Pts',(5.53718046699994,11.6,9.45674331999999));
#214385=CARTESIAN_POINT('Ctrl Pts',(5.53774736999994,15.2,9.45967880399999));
#214386=CARTESIAN_POINT('Ctrl Pts',(5.53774736999994,11.6,9.45967880399999));
#214387=CARTESIAN_POINT('Ctrl Pts',(5.53831288599994,15.2,9.46262006299998));
#214388=CARTESIAN_POINT('Ctrl Pts',(5.53831288599994,11.6,9.46262006299998));
#214389=CARTESIAN_POINT('Ctrl Pts',(5.53887700599994,15.2,9.46556708999999));
#214390=CARTESIAN_POINT('Ctrl Pts',(5.53887700599994,11.6,9.46556708999999));
#214391=CARTESIAN_POINT('Ctrl Pts',(5.53943972199994,15.2,9.46851987699999));
#214392=CARTESIAN_POINT('Ctrl Pts',(5.53943972199994,11.6,9.46851987699999));
#214393=CARTESIAN_POINT('Ctrl Pts',(5.54000102099995,15.2,9.47147841499999));
#214394=CARTESIAN_POINT('Ctrl Pts',(5.54000102099995,11.6,9.47147841499999));
#214395=CARTESIAN_POINT('Ctrl Pts',(5.54056089699994,15.2,9.47444269799998));
#214396=CARTESIAN_POINT('Ctrl Pts',(5.54056089699994,11.6,9.47444269799998));
#214397=CARTESIAN_POINT('Ctrl Pts',(5.54111933899994,15.2,9.47741271699999));
#214398=CARTESIAN_POINT('Ctrl Pts',(5.54111933899994,11.6,9.47741271699999));
#214399=CARTESIAN_POINT('Ctrl Pts',(5.54167633999994,15.2,9.48038846399999));
#214400=CARTESIAN_POINT('Ctrl Pts',(5.54167633999994,11.6,9.48038846399999));
#214401=CARTESIAN_POINT('Ctrl Pts',(5.54223188899994,15.2,9.48336992999998));
#214402=CARTESIAN_POINT('Ctrl Pts',(5.54223188899994,11.6,9.48336992999998));
#214403=CARTESIAN_POINT('Ctrl Pts',(5.54278597899994,15.2,9.48635710899998));
#214404=CARTESIAN_POINT('Ctrl Pts',(5.54278597899994,11.6,9.48635710899998));
#214405=CARTESIAN_POINT('Ctrl Pts',(5.54333859799994,15.2,9.48934999299999));
#214406=CARTESIAN_POINT('Ctrl Pts',(5.54333859799994,11.6,9.48934999299999));
#214407=CARTESIAN_POINT('Ctrl Pts',(5.54388973899995,15.2,9.49234857099999));
#214408=CARTESIAN_POINT('Ctrl Pts',(5.54388973899995,11.6,9.49234857099999));
#214409=CARTESIAN_POINT('Ctrl Pts',(5.54443939299994,15.2,9.49535283999998));
#214410=CARTESIAN_POINT('Ctrl Pts',(5.54443939299994,11.6,9.49535283999998));
#214411=CARTESIAN_POINT('Ctrl Pts',(5.54498754999995,15.2,9.49836278799999));
#214412=CARTESIAN_POINT('Ctrl Pts',(5.54498754999995,11.6,9.49836278799999));
#214413=CARTESIAN_POINT('Ctrl Pts',(5.54553420099994,15.2,9.50137841099998));
#214414=CARTESIAN_POINT('Ctrl Pts',(5.54553420099994,11.6,9.50137841099998));
#214415=CARTESIAN_POINT('Ctrl Pts',(5.54607933799995,15.2,9.50439969699998));
#214416=CARTESIAN_POINT('Ctrl Pts',(5.54607933799995,11.6,9.50439969699998));
#214417=CARTESIAN_POINT('Ctrl Pts',(5.54662295099994,15.2,9.50742664099998));
#214418=CARTESIAN_POINT('Ctrl Pts',(5.54662295099994,11.6,9.50742664099998));
#214419=CARTESIAN_POINT('Ctrl Pts',(5.54716503399994,15.2,9.51045923399998));
#214420=CARTESIAN_POINT('Ctrl Pts',(5.54716503399994,11.6,9.51045923399998));
#214421=CARTESIAN_POINT('Ctrl Pts',(5.54770557399995,15.2,9.51349746899999));
#214422=CARTESIAN_POINT('Ctrl Pts',(5.54770557399995,11.6,9.51349746899999));
#214423=CARTESIAN_POINT('Ctrl Pts',(5.54824456499994,15.2,9.51654133699999));
#214424=CARTESIAN_POINT('Ctrl Pts',(5.54824456499994,11.6,9.51654133699999));
#214425=CARTESIAN_POINT('Ctrl Pts',(5.54878199699995,15.2,9.51959082999998));
#214426=CARTESIAN_POINT('Ctrl Pts',(5.54878199699995,11.6,9.51959082999998));
#214427=CARTESIAN_POINT('Ctrl Pts',(5.54931786199995,15.2,9.52264594299999));
#214428=CARTESIAN_POINT('Ctrl Pts',(5.54931786199995,11.6,9.52264594299999));
#214429=CARTESIAN_POINT('Ctrl Pts',(5.54985214999995,15.2,9.52570666499999));
#214430=CARTESIAN_POINT('Ctrl Pts',(5.54985214999995,11.6,9.52570666499999));
#214431=CARTESIAN_POINT('Ctrl Pts',(5.55038485399994,15.2,9.52877299099999));
#214432=CARTESIAN_POINT('Ctrl Pts',(5.55038485399994,11.6,9.52877299099999));
#214433=CARTESIAN_POINT('Ctrl Pts',(5.55091596399994,15.2,9.53184491099999));
#214434=CARTESIAN_POINT('Ctrl Pts',(5.55091596399994,11.6,9.53184491099999));
#214435=CARTESIAN_POINT('Ctrl Pts',(5.55144547199995,15.2,9.53492241799999));
#214436=CARTESIAN_POINT('Ctrl Pts',(5.55144547199995,11.6,9.53492241799999));
#214437=CARTESIAN_POINT('Ctrl Pts',(5.55197336999995,15.2,9.53800550399999));
#214438=CARTESIAN_POINT('Ctrl Pts',(5.55197336999995,11.6,9.53800550399999));
#214439=CARTESIAN_POINT('Ctrl Pts',(5.55249964699994,15.2,9.54109416199999));
#214440=CARTESIAN_POINT('Ctrl Pts',(5.55249964699994,11.6,9.54109416199999));
#214441=CARTESIAN_POINT('Ctrl Pts',(5.55302429599994,15.2,9.54418838299999));
#214442=CARTESIAN_POINT('Ctrl Pts',(5.55302429599994,11.6,9.54418838299999));
#214443=CARTESIAN_POINT('Ctrl Pts',(5.55354730899994,15.2,9.54728816199999));
#214444=CARTESIAN_POINT('Ctrl Pts',(5.55354730899994,11.6,9.54728816199999));
#214445=CARTESIAN_POINT('Ctrl Pts',(5.55406867599994,15.2,9.55039348799998));
#214446=CARTESIAN_POINT('Ctrl Pts',(5.55406867599994,11.6,9.55039348799998));
#214447=CARTESIAN_POINT('Ctrl Pts',(5.55458838999994,15.2,9.55350435599998));
#214448=CARTESIAN_POINT('Ctrl Pts',(5.55458838999994,11.6,9.55350435599998));
#214449=CARTESIAN_POINT('Ctrl Pts',(5.55510644099994,15.2,9.55662075599999));
#214450=CARTESIAN_POINT('Ctrl Pts',(5.55510644099994,11.6,9.55662075599999));
#214451=CARTESIAN_POINT('Ctrl Pts',(5.55562282199994,15.2,9.55974268199999));
#214452=CARTESIAN_POINT('Ctrl Pts',(5.55562282199994,11.6,9.55974268199999));
#214453=CARTESIAN_POINT('Ctrl Pts',(5.55613752299994,15.2,9.56287012499999));
#214454=CARTESIAN_POINT('Ctrl Pts',(5.55613752299994,11.6,9.56287012499999));
#214455=CARTESIAN_POINT('Ctrl Pts',(5.55665053699995,15.2,9.56600307999998));
#214456=CARTESIAN_POINT('Ctrl Pts',(5.55665053699995,11.6,9.56600307999998));
#214457=CARTESIAN_POINT('Ctrl Pts',(5.55716185399994,15.2,9.56914153499999));
#214458=CARTESIAN_POINT('Ctrl Pts',(5.55716185399994,11.6,9.56914153499999));
#214459=CARTESIAN_POINT('Ctrl Pts',(5.55767146699995,15.2,9.57228548699998));
#214460=CARTESIAN_POINT('Ctrl Pts',(5.55767146699995,11.6,9.57228548699998));
#214461=CARTESIAN_POINT('Ctrl Pts',(5.55817936699994,15.2,9.57543492499998));
#214462=CARTESIAN_POINT('Ctrl Pts',(5.55817936699994,11.6,9.57543492499998));
#214463=CARTESIAN_POINT('Ctrl Pts',(5.55868554599994,15.2,9.57858984399999));
#214464=CARTESIAN_POINT('Ctrl Pts',(5.55868554599994,11.6,9.57858984399999));
#214465=CARTESIAN_POINT('Ctrl Pts',(5.55918999599994,15.2,9.58175023399999));
#214466=CARTESIAN_POINT('Ctrl Pts',(5.55918999599994,11.6,9.58175023399999));
#214467=CARTESIAN_POINT('Ctrl Pts',(5.55969270799994,15.2,9.58491608999999));
#214468=CARTESIAN_POINT('Ctrl Pts',(5.55969270799994,11.6,9.58491608999999));
#214469=CARTESIAN_POINT('Ctrl Pts',(5.56019367299994,15.2,9.58808740099999));
#214470=CARTESIAN_POINT('Ctrl Pts',(5.56019367299994,11.6,9.58808740099999));
#214471=CARTESIAN_POINT('Ctrl Pts',(5.56069288399994,15.2,9.59126416199998));
#214472=CARTESIAN_POINT('Ctrl Pts',(5.56069288399994,11.6,9.59126416199998));
#214473=CARTESIAN_POINT('Ctrl Pts',(5.56119033299994,15.2,9.59444636499999));
#214474=CARTESIAN_POINT('Ctrl Pts',(5.56119033299994,11.6,9.59444636499999));
#214475=CARTESIAN_POINT('Ctrl Pts',(5.56168601199994,15.2,9.59763400199999));
#214476=CARTESIAN_POINT('Ctrl Pts',(5.56168601199994,11.6,9.59763400199999));
#214477=CARTESIAN_POINT('Ctrl Pts',(5.56217990999994,15.2,9.60082706499998));
#214478=CARTESIAN_POINT('Ctrl Pts',(5.56217990999994,11.6,9.60082706499998));
#214479=CARTESIAN_POINT('Ctrl Pts',(5.56267202299994,15.2,9.60402554799998));
#214480=CARTESIAN_POINT('Ctrl Pts',(5.56267202299994,11.6,9.60402554799998));
#214481=CARTESIAN_POINT('Ctrl Pts',(5.56316233999994,15.2,9.60722944199999));
#214482=CARTESIAN_POINT('Ctrl Pts',(5.56316233999994,11.6,9.60722944199999));
#214483=CARTESIAN_POINT('Ctrl Pts',(5.56365085299994,15.2,9.61043873999999));
#214484=CARTESIAN_POINT('Ctrl Pts',(5.56365085299994,11.6,9.61043873999999));
#214485=CARTESIAN_POINT('Ctrl Pts',(5.56413755499994,15.2,9.61365343599999));
#214486=CARTESIAN_POINT('Ctrl Pts',(5.56413755499994,11.6,9.61365343599999));
#214487=CARTESIAN_POINT('Ctrl Pts',(5.56462243899994,15.2,9.61687351999998));
#214488=CARTESIAN_POINT('Ctrl Pts',(5.56462243899994,11.6,9.61687351999998));
#214489=CARTESIAN_POINT('Ctrl Pts',(5.56510549399994,15.2,9.62009898599998));
#214490=CARTESIAN_POINT('Ctrl Pts',(5.56510549399994,11.6,9.62009898599998));
#214491=CARTESIAN_POINT('Ctrl Pts',(5.56558671399994,15.2,9.62332982499999));
#214492=CARTESIAN_POINT('Ctrl Pts',(5.56558671399994,11.6,9.62332982499999));
#214493=CARTESIAN_POINT('Ctrl Pts',(5.56606608999994,15.2,9.62656603199999));
#214494=CARTESIAN_POINT('Ctrl Pts',(5.56606608999994,11.6,9.62656603199999));
#214495=CARTESIAN_POINT('Ctrl Pts',(5.56654361499994,15.2,9.62980759699999));
#214496=CARTESIAN_POINT('Ctrl Pts',(5.56654361499994,11.6,9.62980759699999));
#214497=CARTESIAN_POINT('Ctrl Pts',(5.56701928099995,15.2,9.63305451399999));
#214498=CARTESIAN_POINT('Ctrl Pts',(5.56701928099995,11.6,9.63305451399999));
#214499=CARTESIAN_POINT('Ctrl Pts',(5.56749307999994,15.2,9.63630677599999));
#214500=CARTESIAN_POINT('Ctrl Pts',(5.56749307999994,11.6,9.63630677599999));
#214501=CARTESIAN_POINT('Ctrl Pts',(5.56796500199994,15.2,9.63956437499998));
#214502=CARTESIAN_POINT('Ctrl Pts',(5.56796500199994,11.6,9.63956437499998));
#214503=CARTESIAN_POINT('Ctrl Pts',(5.56843504199994,15.2,9.64282730199999));
#214504=CARTESIAN_POINT('Ctrl Pts',(5.56843504199994,11.6,9.64282730199999));
#214505=CARTESIAN_POINT('Ctrl Pts',(5.56890318999995,15.2,9.64609555199999));
#214506=CARTESIAN_POINT('Ctrl Pts',(5.56890318999995,11.6,9.64609555199999));
#214507=CARTESIAN_POINT('Ctrl Pts',(5.56936943999994,15.2,9.64936911699999));
#214508=CARTESIAN_POINT('Ctrl Pts',(5.56936943999994,11.6,9.64936911699999));
#214509=CARTESIAN_POINT('Ctrl Pts',(5.56983378399994,15.2,9.65264798799998));
#214510=CARTESIAN_POINT('Ctrl Pts',(5.56983378399994,11.6,9.65264798799998));
#214511=CARTESIAN_POINT('Ctrl Pts',(5.57029621199994,15.2,9.65593215999998));
#214512=CARTESIAN_POINT('Ctrl Pts',(5.57029621199994,11.6,9.65593215999998));
#214513=CARTESIAN_POINT('Ctrl Pts',(5.57075671899995,15.2,9.65922162299999));
#214514=CARTESIAN_POINT('Ctrl Pts',(5.57075671899995,11.6,9.65922162299999));
#214515=CARTESIAN_POINT('Ctrl Pts',(5.57121529499994,15.2,9.66251637199999));
#214516=CARTESIAN_POINT('Ctrl Pts',(5.57121529499994,11.6,9.66251637199999));
#214517=CARTESIAN_POINT('Ctrl Pts',(5.57167193299994,15.2,9.66581639899999));
#214518=CARTESIAN_POINT('Ctrl Pts',(5.57167193299994,11.6,9.66581639899999));
#214519=CARTESIAN_POINT('Ctrl Pts',(5.57212662699994,15.2,9.66912169499999));
#214520=CARTESIAN_POINT('Ctrl Pts',(5.57212662699994,11.6,9.66912169499999));
#214521=CARTESIAN_POINT('Ctrl Pts',(5.57257936599994,15.2,9.67243225399999));
#214522=CARTESIAN_POINT('Ctrl Pts',(5.57257936599994,11.6,9.67243225399999));
#214523=CARTESIAN_POINT('Ctrl Pts',(5.57303014599994,15.2,9.67574806999998));
#214524=CARTESIAN_POINT('Ctrl Pts',(5.57303014599994,11.6,9.67574806999998));
#214525=CARTESIAN_POINT('Ctrl Pts',(5.57347895599994,15.2,9.67906913199998));
#214526=CARTESIAN_POINT('Ctrl Pts',(5.57347895599994,11.6,9.67906913199998));
#214527=CARTESIAN_POINT('Ctrl Pts',(5.57392578999995,15.2,9.68239543699998));
#214528=CARTESIAN_POINT('Ctrl Pts',(5.57392578999995,11.6,9.68239543699998));
#214529=CARTESIAN_POINT('Ctrl Pts',(5.57437064099994,15.2,9.68572697499999));
#214530=CARTESIAN_POINT('Ctrl Pts',(5.57437064099994,11.6,9.68572697499999));
#214531=CARTESIAN_POINT('Ctrl Pts',(5.57481349999994,15.2,9.68906373899999));
#214532=CARTESIAN_POINT('Ctrl Pts',(5.57481349999994,11.6,9.68906373899999));
#214533=CARTESIAN_POINT('Ctrl Pts',(5.57525436099994,15.2,9.69240572199999));
#214534=CARTESIAN_POINT('Ctrl Pts',(5.57525436099994,11.6,9.69240572199999));
#214535=CARTESIAN_POINT('Ctrl Pts',(5.57569321399994,15.2,9.69575291799998));
#214536=CARTESIAN_POINT('Ctrl Pts',(5.57569321399994,11.6,9.69575291799998));
#214537=CARTESIAN_POINT('Ctrl Pts',(5.57613005399994,15.2,9.69910531599999));
#214538=CARTESIAN_POINT('Ctrl Pts',(5.57613005399994,11.6,9.69910531599999));
#214539=CARTESIAN_POINT('Ctrl Pts',(5.57656487299995,15.2,9.70246291299999));
#214540=CARTESIAN_POINT('Ctrl Pts',(5.57656487299995,11.6,9.70246291299999));
#214541=CARTESIAN_POINT('Ctrl Pts',(5.57699766199995,15.2,9.70582569899998));
#214542=CARTESIAN_POINT('Ctrl Pts',(5.57699766199995,11.6,9.70582569899998));
#214543=CARTESIAN_POINT('Ctrl Pts',(5.57742841599994,15.2,9.70919366799999));
#214544=CARTESIAN_POINT('Ctrl Pts',(5.57742841599994,11.6,9.70919366799999));
#214545=CARTESIAN_POINT('Ctrl Pts',(5.57785712399995,15.2,9.71256681299998));
#214546=CARTESIAN_POINT('Ctrl Pts',(5.57785712399995,11.6,9.71256681299998));
#214547=CARTESIAN_POINT('Ctrl Pts',(5.57828378199994,15.2,9.71594512399999));
#214548=CARTESIAN_POINT('Ctrl Pts',(5.57828378199994,11.6,9.71594512399999));
#214549=CARTESIAN_POINT('Ctrl Pts',(5.57870838199994,15.2,9.71932859799999));
#214550=CARTESIAN_POINT('Ctrl Pts',(5.57870838199994,11.6,9.71932859799999));
#214551=CARTESIAN_POINT('Ctrl Pts',(5.57913091399994,15.2,9.72271722499999));
#214552=CARTESIAN_POINT('Ctrl Pts',(5.57913091399994,11.6,9.72271722499999));
#214553=CARTESIAN_POINT('Ctrl Pts',(5.57955137399994,15.2,9.72611099799998));
#214554=CARTESIAN_POINT('Ctrl Pts',(5.57955137399994,11.6,9.72611099799998));
#214555=CARTESIAN_POINT('Ctrl Pts',(5.57996975299995,15.2,9.72950991099999));
#214556=CARTESIAN_POINT('Ctrl Pts',(5.57996975299995,11.6,9.72950991099999));
#214557=CARTESIAN_POINT('Ctrl Pts',(5.58038604299995,15.2,9.73291395399999));
#214558=CARTESIAN_POINT('Ctrl Pts',(5.58038604299995,11.6,9.73291395399999));
#214559=CARTESIAN_POINT('Ctrl Pts',(5.58080023799994,15.2,9.73632312399998));
#214560=CARTESIAN_POINT('Ctrl Pts',(5.58080023799994,11.6,9.73632312399998));
#214561=CARTESIAN_POINT('Ctrl Pts',(5.58121232999994,15.2,9.73973741099999));
#214562=CARTESIAN_POINT('Ctrl Pts',(5.58121232999994,11.6,9.73973741099999));
#214563=CARTESIAN_POINT('Ctrl Pts',(5.58162231199995,15.2,9.74315680799998));
#214564=CARTESIAN_POINT('Ctrl Pts',(5.58162231199995,11.6,9.74315680799998));
#214565=CARTESIAN_POINT('Ctrl Pts',(5.58203017699994,15.2,9.74658130799998));
#214566=CARTESIAN_POINT('Ctrl Pts',(5.58203017699994,11.6,9.74658130799998));
#214567=CARTESIAN_POINT('Ctrl Pts',(5.58243591799994,15.2,9.75001090499998));
#214568=CARTESIAN_POINT('Ctrl Pts',(5.58243591799994,11.6,9.75001090499998));
#214569=CARTESIAN_POINT('Ctrl Pts',(5.58283952599995,15.2,9.75344558999998));
#214570=CARTESIAN_POINT('Ctrl Pts',(5.58283952599995,11.6,9.75344558999998));
#214571=CARTESIAN_POINT('Ctrl Pts',(5.58324099499995,15.2,9.75688535799998));
#214572=CARTESIAN_POINT('Ctrl Pts',(5.58324099499995,11.6,9.75688535799998));
#214573=CARTESIAN_POINT('Ctrl Pts',(5.58364031899995,15.2,9.76033019899998));
#214574=CARTESIAN_POINT('Ctrl Pts',(5.58364031899995,11.6,9.76033019899998));
#214575=CARTESIAN_POINT('Ctrl Pts',(5.58403748899994,15.2,9.76378010799999));
#214576=CARTESIAN_POINT('Ctrl Pts',(5.58403748899994,11.6,9.76378010799999));
#214577=CARTESIAN_POINT('Ctrl Pts',(5.58443249899994,15.2,9.76723507899998));
#214578=CARTESIAN_POINT('Ctrl Pts',(5.58443249899994,11.6,9.76723507899998));
#214579=CARTESIAN_POINT('Ctrl Pts',(5.58482534199994,15.2,9.77069510199998));
#214580=CARTESIAN_POINT('Ctrl Pts',(5.58482534199994,11.6,9.77069510199998));
#214581=CARTESIAN_POINT('Ctrl Pts',(5.58521600899994,15.2,9.77416016999998));
#214582=CARTESIAN_POINT('Ctrl Pts',(5.58521600899994,11.6,9.77416016999998));
#214583=CARTESIAN_POINT('Ctrl Pts',(5.58560449599995,15.2,9.77763027899999));
#214584=CARTESIAN_POINT('Ctrl Pts',(5.58560449599995,11.6,9.77763027899999));
#214585=CARTESIAN_POINT('Ctrl Pts',(5.58599079299994,15.2,9.78110541899999));
#214586=CARTESIAN_POINT('Ctrl Pts',(5.58599079299994,11.6,9.78110541899999));
#214587=CARTESIAN_POINT('Ctrl Pts',(5.58637489499994,15.2,9.78458558299998));
#214588=CARTESIAN_POINT('Ctrl Pts',(5.58637489499994,11.6,9.78458558299998));
#214589=CARTESIAN_POINT('Ctrl Pts',(5.58675679299995,15.2,9.78807076599999));
#214590=CARTESIAN_POINT('Ctrl Pts',(5.58675679299995,11.6,9.78807076599999));
#214591=CARTESIAN_POINT('Ctrl Pts',(5.58713648299995,15.2,9.79156095899998));
#214592=CARTESIAN_POINT('Ctrl Pts',(5.58713648299995,11.6,9.79156095899998));
#214593=CARTESIAN_POINT('Ctrl Pts',(5.58751395599995,15.2,9.79505615499999));
#214594=CARTESIAN_POINT('Ctrl Pts',(5.58751395599995,11.6,9.79505615499999));
#214595=CARTESIAN_POINT('Ctrl Pts',(5.58788920299994,15.2,9.79855634899998));
#214596=CARTESIAN_POINT('Ctrl Pts',(5.58788920299994,11.6,9.79855634899998));
#214597=CARTESIAN_POINT('Ctrl Pts',(5.58826222199994,15.2,9.80206153099999));
#214598=CARTESIAN_POINT('Ctrl Pts',(5.58826222199994,11.6,9.80206153099999));
#214599=CARTESIAN_POINT('Ctrl Pts',(5.58863300199994,15.2,9.80557169599999));
#214600=CARTESIAN_POINT('Ctrl Pts',(5.58863300199994,11.6,9.80557169599999));
#214601=CARTESIAN_POINT('Ctrl Pts',(5.58900153799994,15.2,9.80908683699998));
#214602=CARTESIAN_POINT('Ctrl Pts',(5.58900153799994,11.6,9.80908683699998));
#214603=CARTESIAN_POINT('Ctrl Pts',(5.58936782299994,15.2,9.81260694599998));
#214604=CARTESIAN_POINT('Ctrl Pts',(5.58936782299994,11.6,9.81260694599998));
#214605=CARTESIAN_POINT('Ctrl Pts',(5.58973184799994,15.2,9.81613201599998));
#214606=CARTESIAN_POINT('Ctrl Pts',(5.58973184799994,11.6,9.81613201599998));
#214607=CARTESIAN_POINT('Ctrl Pts',(5.59009360999994,15.2,9.81966203999999));
#214608=CARTESIAN_POINT('Ctrl Pts',(5.59009360999994,11.6,9.81966203999999));
#214609=CARTESIAN_POINT('Ctrl Pts',(5.59045309799994,15.2,9.82319701299998));
#214610=CARTESIAN_POINT('Ctrl Pts',(5.59045309799994,11.6,9.82319701299998));
#214611=CARTESIAN_POINT('Ctrl Pts',(5.59081030799994,15.2,9.82673692399998));
#214612=CARTESIAN_POINT('Ctrl Pts',(5.59081030799994,11.6,9.82673692399998));
#214613=CARTESIAN_POINT('Ctrl Pts',(5.59116523299994,15.2,9.83028176999999));
#214614=CARTESIAN_POINT('Ctrl Pts',(5.59116523299994,11.6,9.83028176999999));
#214615=CARTESIAN_POINT('Ctrl Pts',(5.59151786499994,15.2,9.83383154199998));
#214616=CARTESIAN_POINT('Ctrl Pts',(5.59151786499994,11.6,9.83383154199998));
#214617=CARTESIAN_POINT('Ctrl Pts',(5.59186819799995,15.2,9.83738623299999));
#214618=CARTESIAN_POINT('Ctrl Pts',(5.59186819799995,11.6,9.83738623299999));
#214619=CARTESIAN_POINT('Ctrl Pts',(5.59221622499994,15.2,9.84094583599998));
#214620=CARTESIAN_POINT('Ctrl Pts',(5.59221622499994,11.6,9.84094583599998));
#214621=CARTESIAN_POINT('Ctrl Pts',(5.59256193999994,15.2,9.84451034399999));
#214622=CARTESIAN_POINT('Ctrl Pts',(5.59256193999994,11.6,9.84451034399999));
#214623=CARTESIAN_POINT('Ctrl Pts',(5.59290533499994,15.2,9.84807975199999));
#214624=CARTESIAN_POINT('Ctrl Pts',(5.59290533499994,11.6,9.84807975199999));
#214625=CARTESIAN_POINT('Ctrl Pts',(5.59324640499995,15.2,9.85165404999999));
#214626=CARTESIAN_POINT('Ctrl Pts',(5.59324640499995,11.6,9.85165404999999));
#214627=CARTESIAN_POINT('Ctrl Pts',(5.59358513999994,15.2,9.85523323299999));
#214628=CARTESIAN_POINT('Ctrl Pts',(5.59358513999994,11.6,9.85523323299999));
#214629=CARTESIAN_POINT('Ctrl Pts',(5.59392153799994,15.2,9.85881729399999));
#214630=CARTESIAN_POINT('Ctrl Pts',(5.59392153799994,11.6,9.85881729399999));
#214631=CARTESIAN_POINT('Ctrl Pts',(5.59425558899994,15.2,9.86240622499999));
#214632=CARTESIAN_POINT('Ctrl Pts',(5.59425558899994,11.6,9.86240622499999));
#214633=CARTESIAN_POINT('Ctrl Pts',(5.59458728699994,15.2,9.86600001999999));
#214634=CARTESIAN_POINT('Ctrl Pts',(5.59458728699994,11.6,9.86600001999999));
#214635=CARTESIAN_POINT('Ctrl Pts',(5.59491662599994,15.2,9.86959867199998));
#214636=CARTESIAN_POINT('Ctrl Pts',(5.59491662599994,11.6,9.86959867199998));
#214637=CARTESIAN_POINT('Ctrl Pts',(5.59524359999994,15.2,9.87320217299999));
#214638=CARTESIAN_POINT('Ctrl Pts',(5.59524359999994,11.6,9.87320217299999));
#214639=CARTESIAN_POINT('Ctrl Pts',(5.59556819999995,15.2,9.87681051799999));
#214640=CARTESIAN_POINT('Ctrl Pts',(5.59556819999995,11.6,9.87681051799999));
#214641=CARTESIAN_POINT('Ctrl Pts',(5.59589042199995,15.2,9.88042369799999));
#214642=CARTESIAN_POINT('Ctrl Pts',(5.59589042199995,11.6,9.88042369799999));
#214643=CARTESIAN_POINT('Ctrl Pts',(5.59621025999995,15.2,9.88404170799999));
#214644=CARTESIAN_POINT('Ctrl Pts',(5.59621025999995,11.6,9.88404170799999));
#214645=CARTESIAN_POINT('Ctrl Pts',(5.59652770299994,15.2,9.88766453999999));
#214646=CARTESIAN_POINT('Ctrl Pts',(5.59652770299994,11.6,9.88766453999999));
#214647=CARTESIAN_POINT('Ctrl Pts',(5.59684274999994,15.2,9.89129218699999));
#214648=CARTESIAN_POINT('Ctrl Pts',(5.59684274999994,11.6,9.89129218699999));
#214649=CARTESIAN_POINT('Ctrl Pts',(5.59715539099994,15.2,9.89492464299998));
#214650=CARTESIAN_POINT('Ctrl Pts',(5.59715539099994,11.6,9.89492464299998));
#214651=CARTESIAN_POINT('Ctrl Pts',(5.59746561999994,15.2,9.89856189999998));
#214652=CARTESIAN_POINT('Ctrl Pts',(5.59746561999994,11.6,9.89856189999998));
#214653=CARTESIAN_POINT('Ctrl Pts',(5.59777343199994,15.2,9.90220395299998));
#214654=CARTESIAN_POINT('Ctrl Pts',(5.59777343199994,11.6,9.90220395299998));
#214655=CARTESIAN_POINT('Ctrl Pts',(5.59807881899995,15.2,9.90585079299999));
#214656=CARTESIAN_POINT('Ctrl Pts',(5.59807881899995,11.6,9.90585079299999));
#214657=CARTESIAN_POINT('Ctrl Pts',(5.59838177599995,15.2,9.90950241499998));
#214658=CARTESIAN_POINT('Ctrl Pts',(5.59838177599995,11.6,9.90950241499998));
#214659=CARTESIAN_POINT('Ctrl Pts',(5.59868229399994,15.2,9.91315880999998));
#214660=CARTESIAN_POINT('Ctrl Pts',(5.59868229399994,11.6,9.91315880999998));
#214661=CARTESIAN_POINT('Ctrl Pts',(5.59898037099994,15.2,9.91681997299998));
#214662=CARTESIAN_POINT('Ctrl Pts',(5.59898037099994,11.6,9.91681997299998));
#214663=CARTESIAN_POINT('Ctrl Pts',(5.59927599599994,15.2,9.92048589699999));
#214664=CARTESIAN_POINT('Ctrl Pts',(5.59927599599994,11.6,9.92048589699999));
#214665=CARTESIAN_POINT('Ctrl Pts',(5.59956916499995,15.2,9.92415657399999));
#214666=CARTESIAN_POINT('Ctrl Pts',(5.59956916499995,11.6,9.92415657399999));
#214667=CARTESIAN_POINT('Ctrl Pts',(5.59985987199994,15.2,9.92783199799998));
#214668=CARTESIAN_POINT('Ctrl Pts',(5.59985987199994,11.6,9.92783199799998));
#214669=CARTESIAN_POINT('Ctrl Pts',(5.60014810899994,15.2,9.93151216299999));
#214670=CARTESIAN_POINT('Ctrl Pts',(5.60014810899994,11.6,9.93151216299999));
#214671=CARTESIAN_POINT('Ctrl Pts',(5.60043387199994,15.2,9.93519705999999));
#214672=CARTESIAN_POINT('Ctrl Pts',(5.60043387199994,11.6,9.93519705999999));
#214673=CARTESIAN_POINT('Ctrl Pts',(5.60071715199995,15.2,9.93888668399999));
#214674=CARTESIAN_POINT('Ctrl Pts',(5.60071715199995,11.6,9.93888668399999));
#214675=CARTESIAN_POINT('Ctrl Pts',(5.60099794499994,15.2,9.94258102799999));
#214676=CARTESIAN_POINT('Ctrl Pts',(5.60099794499994,11.6,9.94258102799999));
#214677=CARTESIAN_POINT('Ctrl Pts',(5.60127624499994,15.2,9.94628008399999));
#214678=CARTESIAN_POINT('Ctrl Pts',(5.60127624499994,11.6,9.94628008399999));
#214679=CARTESIAN_POINT('Ctrl Pts',(5.60155204299994,15.2,9.94998384799998));
#214680=CARTESIAN_POINT('Ctrl Pts',(5.60155204299994,11.6,9.94998384799998));
#214681=CARTESIAN_POINT('Ctrl Pts',(5.60182533599995,15.2,9.95369231099998));
#214682=CARTESIAN_POINT('Ctrl Pts',(5.60182533599995,11.6,9.95369231099998));
#214683=CARTESIAN_POINT('Ctrl Pts',(5.60209611699994,15.2,9.95740546799999));
#214684=CARTESIAN_POINT('Ctrl Pts',(5.60209611699994,11.6,9.95740546799999));
#214685=CARTESIAN_POINT('Ctrl Pts',(5.60236437799994,15.2,9.96112330999999));
#214686=CARTESIAN_POINT('Ctrl Pts',(5.60236437799994,11.6,9.96112330999999));
#214687=CARTESIAN_POINT('Ctrl Pts',(5.60263011399995,15.2,9.96484582999998));
#214688=CARTESIAN_POINT('Ctrl Pts',(5.60263011399995,11.6,9.96484582999998));
#214689=CARTESIAN_POINT('Ctrl Pts',(5.60289331799994,15.2,9.96857302299999));
#214690=CARTESIAN_POINT('Ctrl Pts',(5.60289331799994,11.6,9.96857302299999));
#214691=CARTESIAN_POINT('Ctrl Pts',(5.60315398399994,15.2,9.97230487999998));
#214692=CARTESIAN_POINT('Ctrl Pts',(5.60315398399994,11.6,9.97230487999998));
#214693=CARTESIAN_POINT('Ctrl Pts',(5.60341210499995,15.2,9.97604139599999));
#214694=CARTESIAN_POINT('Ctrl Pts',(5.60341210499995,11.6,9.97604139599999));
#214695=CARTESIAN_POINT('Ctrl Pts',(5.60366767599994,15.2,9.97978256399998));
#214696=CARTESIAN_POINT('Ctrl Pts',(5.60366767599994,11.6,9.97978256399998));
#214697=CARTESIAN_POINT('Ctrl Pts',(5.60392069199994,15.2,9.98352837599998));
#214698=CARTESIAN_POINT('Ctrl Pts',(5.60392069199994,11.6,9.98352837599998));
#214699=CARTESIAN_POINT('Ctrl Pts',(5.60417114799994,15.2,9.98727882899999));
#214700=CARTESIAN_POINT('Ctrl Pts',(5.60417114799994,11.6,9.98727882899999));
#214701=CARTESIAN_POINT('Ctrl Pts',(5.60441903599994,15.2,9.99103391699999));
#214702=CARTESIAN_POINT('Ctrl Pts',(5.60441903599994,11.6,9.99103391699999));
#214703=CARTESIAN_POINT('Ctrl Pts',(5.60466435299994,15.2,9.99479363099999));
#214704=CARTESIAN_POINT('Ctrl Pts',(5.60466435299994,11.6,9.99479363099999));
#214705=CARTESIAN_POINT('Ctrl Pts',(5.60490709099994,15.2,9.99855796499999));
#214706=CARTESIAN_POINT('Ctrl Pts',(5.60490709099994,11.6,9.99855796499999));
#214707=CARTESIAN_POINT('Ctrl Pts',(5.60514724499994,15.2,10.002326911));
#214708=CARTESIAN_POINT('Ctrl Pts',(5.60514724499994,11.6,10.002326911));
#214709=CARTESIAN_POINT('Ctrl Pts',(5.60538480399994,15.2,10.006100462));
#214710=CARTESIAN_POINT('Ctrl Pts',(5.60538480399994,11.6,10.006100462));
#214711=CARTESIAN_POINT('Ctrl Pts',(5.60561976299994,15.2,10.009878609));
#214712=CARTESIAN_POINT('Ctrl Pts',(5.60561976299994,11.6,10.009878609));
#214713=CARTESIAN_POINT('Ctrl Pts',(5.60585211499995,15.2,10.013661345));
#214714=CARTESIAN_POINT('Ctrl Pts',(5.60585211499995,11.6,10.013661345));
#214715=CARTESIAN_POINT('Ctrl Pts',(5.60608185199994,15.2,10.01744866));
#214716=CARTESIAN_POINT('Ctrl Pts',(5.60608185199994,11.6,10.01744866));
#214717=CARTESIAN_POINT('Ctrl Pts',(5.60630896899994,15.2,10.021240551));
#214718=CARTESIAN_POINT('Ctrl Pts',(5.60630896899994,11.6,10.021240551));
#214719=CARTESIAN_POINT('Ctrl Pts',(5.60653346399994,15.2,10.025037011));
#214720=CARTESIAN_POINT('Ctrl Pts',(5.60653346399994,11.6,10.025037011));
#214721=CARTESIAN_POINT('Ctrl Pts',(5.60675533299994,15.2,10.028838039));
#214722=CARTESIAN_POINT('Ctrl Pts',(5.60675533299994,11.6,10.028838039));
#214723=CARTESIAN_POINT('Ctrl Pts',(5.60697457299995,15.2,10.032643632));
#214724=CARTESIAN_POINT('Ctrl Pts',(5.60697457299995,11.6,10.032643632));
#214725=CARTESIAN_POINT('Ctrl Pts',(5.60714786199994,15.2,10.035691756));
#214726=CARTESIAN_POINT('Ctrl Pts',(5.60714786199994,11.6,10.035691756));
#214727=CARTESIAN_POINT('Ctrl Pts',(5.60727664699994,15.2,10.037979905));
#214728=CARTESIAN_POINT('Ctrl Pts',(5.60727664699994,11.6,10.037979905));
#214729=CARTESIAN_POINT('Ctrl Pts',(5.60736197799995,15.2,10.039506249));
#214730=CARTESIAN_POINT('Ctrl Pts',(5.60736197799995,11.6,10.039506249));
#214731=CARTESIAN_POINT('Ctrl Pts',(5.60740451299995,15.2,10.04026965));
#214732=CARTESIAN_POINT('Ctrl Pts',(5.60740451299995,11.6,10.04026965));
#214733=CARTESIAN_POINT('Ctrl Pts',(5.36127880499994,15.2,8.88241603299999));
#214734=CARTESIAN_POINT('Ctrl Pts',(5.36206719568413,15.2,8.88401933383977));
#214735=CARTESIAN_POINT('Ctrl Pts',(5.3628759863957,15.2,8.88567631031983));
#214736=CARTESIAN_POINT('Ctrl Pts',(5.36370417391754,15.2,8.88738636482928));
#214737=CARTESIAN_POINT('Ctrl Pts',(5.36453635537823,15.2,8.88910466608596));
#214738=CARTESIAN_POINT('Ctrl Pts',(5.36538812011717,15.2,8.89087656335787));
#214739=CARTESIAN_POINT('Ctrl Pts',(5.36625847962582,15.2,8.89270147796823));
#214740=CARTESIAN_POINT('Ctrl Pts',(5.36712883905543,15.2,8.89452639241284));
#214741=CARTESIAN_POINT('Ctrl Pts',(5.36801779174953,15.2,8.89640432539507));
#214742=CARTESIAN_POINT('Ctrl Pts',(5.36892438021658,15.2,8.89833471374155));
#214743=CARTESIAN_POINT('Ctrl Pts',(5.36983096868362,15.2,8.90026510208804));
#214744=CARTESIAN_POINT('Ctrl Pts',(5.37075519224708,15.2,8.90224794602847));
#214745=CARTESIAN_POINT('Ctrl Pts',(5.3716961199256,15.2,8.90428269455318));
#214746=CARTESIAN_POINT('Ctrl Pts',(5.37263704768957,15.2,8.90631744326271));
#214747=CARTESIAN_POINT('Ctrl Pts',(5.37359468033524,15.2,8.9084040964046));
#214748=CARTESIAN_POINT('Ctrl Pts',(5.37456811338936,15.2,8.91054211894128));
#214749=CARTESIAN_POINT('Ctrl Pts',(5.37570378515322,15.2,8.91303647827611));
#214750=CARTESIAN_POINT('Ctrl Pts',(5.37686096291785,15.2,8.91560075447309));
#214751=CARTESIAN_POINT('Ctrl Pts',(5.37803825790234,15.2,8.91823411554835));
#214752=CARTESIAN_POINT('Ctrl Pts',(5.3790473680069,15.2,8.92049128244788));
#214753=CARTESIAN_POINT('Ctrl Pts',(5.38007125793053,15.2,8.92279920619165));
#214754=CARTESIAN_POINT('Ctrl Pts',(5.38110908007138,15.2,8.92515737499027));
#214755=CARTESIAN_POINT('Ctrl Pts',(5.38214690211796,15.2,8.92751554357471));
#214756=CARTESIAN_POINT('Ctrl Pts',(5.38319865533424,15.2,8.92992395694573));
#214757=CARTESIAN_POINT('Ctrl Pts',(5.38426351746707,15.2,8.93238211453435));
#214758=CARTESIAN_POINT('Ctrl Pts',(5.3853283795999,15.2,8.93484027212297));
#214759=CARTESIAN_POINT('Ctrl Pts',(5.3864063481307,15.2,8.93734817377245));
#214760=CARTESIAN_POINT('Ctrl Pts',(5.38749662325722,15.2,8.93990532934408));
#214761=CARTESIAN_POINT('Ctrl Pts',(5.38858689848278,15.2,8.94246248514798));
#214762=CARTESIAN_POINT('Ctrl Pts',(5.38968947790153,15.2,8.94506889477464));
#214763=CARTESIAN_POINT('Ctrl Pts',(5.39080358337969,15.2,8.94772407675599));
#214764=CARTESIAN_POINT('Ctrl Pts',(5.39191768875667,15.2,8.95037925849614));
#214765=CARTESIAN_POINT('Ctrl Pts',(5.39304331814439,15.2,8.95308321474799));
#214766=CARTESIAN_POINT('Ctrl Pts',(5.39417971535357,15.2,8.95583547065011));
#214767=CARTESIAN_POINT('Ctrl Pts',(5.39531611256277,15.2,8.95858772655223));
#214768=CARTESIAN_POINT('Ctrl Pts',(5.39646327322106,15.2,8.96138828550877));
#214769=CARTESIAN_POINT('Ctrl Pts',(5.39762045992857,15.2,8.96423668331986));
#214770=CARTESIAN_POINT('Ctrl Pts',(5.39877764663609,15.2,8.96708508113096));
#214771=CARTESIAN_POINT('Ctrl Pts',(5.39994486175675,15.2,8.96998131745591));
#214772=CARTESIAN_POINT('Ctrl Pts',(5.40112137963002,15.2,8.97292494117904));
#214773=CARTESIAN_POINT('Ctrl Pts',(5.40229789761017,15.2,8.97586856516956));
#214774=CARTESIAN_POINT('Ctrl Pts',(5.40348372275793,15.2,8.97885957314806));
#214775=CARTESIAN_POINT('Ctrl Pts',(5.40467814957339,15.2,8.981897523149));
#214776=CARTESIAN_POINT('Ctrl Pts',(5.40587257628037,15.2,8.98493547287399));
#214777=CARTESIAN_POINT('Ctrl Pts',(5.40707560536163,15.2,8.98802036289524));
#214778=CARTESIAN_POINT('Ctrl Pts',(5.40828655315064,15.2,8.99115175477944));
#214779=CARTESIAN_POINT('Ctrl Pts',(5.40949750093962,15.2,8.99428314666365));
#214780=CARTESIAN_POINT('Ctrl Pts',(5.41071636676135,15.2,8.99746104326049));
#214781=CARTESIAN_POINT('Ctrl Pts',(5.41194248188295,15.2,9.00068501039017));
#214782=CARTESIAN_POINT('Ctrl Pts',(5.41316859711593,15.2,9.00390897781269));
#214783=CARTESIAN_POINT('Ctrl Pts',(5.41440196414134,15.2,9.00717902039809));
#214784=CARTESIAN_POINT('Ctrl Pts',(5.41564192829254,15.2,9.01049471074747));
#214785=CARTESIAN_POINT('Ctrl Pts',(5.41688189233111,15.2,9.01381040079567));
#214786=CARTESIAN_POINT('Ctrl Pts',(5.41812845637254,15.2,9.01717174290682));
#214787=CARTESIAN_POINT('Ctrl Pts',(5.41938098149937,15.2,9.02057831696503));
#214788=CARTESIAN_POINT('Ctrl Pts',(5.42063350662618,15.2,9.02398489102326));
#214789=CARTESIAN_POINT('Ctrl Pts',(5.42189199455013,15.2,9.02743670033225));
#214790=CARTESIAN_POINT('Ctrl Pts',(5.42315582458718,15.2,9.03093333336878));
#214791=CARTESIAN_POINT('Ctrl Pts',(5.42441965473902,15.2,9.03442996672293));
#214792=CARTESIAN_POINT('Ctrl Pts',(5.42568882599815,15.2,9.03797142575305));
#214793=CARTESIAN_POINT('Ctrl Pts',(5.42696273238152,15.2,9.04155730713024));
#214794=CARTESIAN_POINT('Ctrl Pts',(5.42823663864917,15.2,9.04514318818172));
#214795=CARTESIAN_POINT('Ctrl Pts',(5.42951527992154,15.2,9.04877349106673));
#214796=CARTESIAN_POINT('Ctrl Pts',(5.43079806495827,15.2,9.05244781826656));
#214797=CARTESIAN_POINT('Ctrl Pts',(5.432080849995,15.2,9.0561221454664));
#214798=CARTESIAN_POINT('Ctrl Pts',(5.43336777664106,15.2,9.05984049843734));
#214799=CARTESIAN_POINT('Ctrl Pts',(5.43465826715844,15.2,9.06360248665276));
#214800=CARTESIAN_POINT('Ctrl Pts',(5.435733675962,15.2,9.06673747694619));
#214801=CARTESIAN_POINT('Ctrl Pts',(5.43681156121276,15.2,9.06990276903155));
#214802=CARTESIAN_POINT('Ctrl Pts',(5.43789159246265,15.2,9.07309813930779));
#214803=CARTESIAN_POINT('Ctrl Pts',(5.43897162371255,15.2,9.07629350958402));
#214804=CARTESIAN_POINT('Ctrl Pts',(5.44005380160138,15.2,9.0795189574332));
#214805=CARTESIAN_POINT('Ctrl Pts',(5.44113780521239,15.2,9.08277426507052));
#214806=CARTESIAN_POINT('Ctrl Pts',(5.44222180882341,15.2,9.08602957270784));
#214807=CARTESIAN_POINT('Ctrl Pts',(5.44330763673329,15.2,9.08931473918868));
#214808=CARTESIAN_POINT('Ctrl Pts',(5.44439497451602,15.2,9.09262954448144));
#214809=CARTESIAN_POINT('Ctrl Pts',(5.44548231229874,15.2,9.09594434977421));
#214810=CARTESIAN_POINT('Ctrl Pts',(5.44657115834994,15.2,9.09928879568325));
#214811=CARTESIAN_POINT('Ctrl Pts',(5.44766120376661,15.2,9.10266266672491));
#214812=CARTESIAN_POINT('Ctrl Pts',(5.44896925821909,15.2,9.1067113118278));
#214813=CARTESIAN_POINT('Ctrl Pts',(5.45027903671366,15.2,9.11080232867963));
#214814=CARTESIAN_POINT('Ctrl Pts',(5.45159001631479,15.2,9.11493534906686));
#214815=CARTESIAN_POINT('Ctrl Pts',(5.45268249935543,15.2,9.11837953284803));
#214816=CARTESIAN_POINT('Ctrl Pts',(5.45377581650622,15.2,9.12185288672812));
#214817=CARTESIAN_POINT('Ctrl Pts',(5.45486966872841,15.2,9.12535519950437));
#214818=CARTESIAN_POINT('Ctrl Pts',(5.45618229146657,15.2,9.12955797506492));
#214819=CARTESIAN_POINT('Ctrl Pts',(5.45749568456319,15.2,9.1338024511057));
#214820=CARTESIAN_POINT('Ctrl Pts',(5.4588093433848,15.2,9.13808827142541));
#214821=CARTESIAN_POINT('Ctrl Pts',(5.45990405889049,15.2,9.14165978777456));
#214822=CARTESIAN_POINT('Ctrl Pts',(5.46099895984273,15.2,9.14526001305091));
#214823=CARTESIAN_POINT('Ctrl Pts',(5.46209375784841,15.2,9.14888874300029));
#214824=CARTESIAN_POINT('Ctrl Pts',(5.46318855597342,15.2,9.1525174733452));
#214825=CARTESIAN_POINT('Ctrl Pts',(5.46428325185122,15.2,9.15617470902571));
#214826=CARTESIAN_POINT('Ctrl Pts',(5.46537756407347,15.2,9.15986024596785));
#214827=CARTESIAN_POINT('Ctrl Pts',(5.46647187629573,15.2,9.16354578290998));
#214828=CARTESIAN_POINT('Ctrl Pts',(5.46756580386281,15.2,9.16725962078066));
#214829=CARTESIAN_POINT('Ctrl Pts',(5.4686590711397,15.2,9.17100156034063));
#214830=CARTESIAN_POINT('Ctrl Pts',(5.46975233841657,15.2,9.1747434999006));
#214831=CARTESIAN_POINT('Ctrl Pts',(5.47084494464517,15.2,9.17851353832538));
#214832=CARTESIAN_POINT('Ctrl Pts',(5.47193661714521,15.2,9.1823114779767));
#214833=CARTESIAN_POINT('Ctrl Pts',(5.47302828964526,15.2,9.18610941762802));
#214834=CARTESIAN_POINT('Ctrl Pts',(5.4741190282064,15.2,9.18993525979951));
#214835=CARTESIAN_POINT('Ctrl Pts',(5.47520856792868,15.2,9.19378880521472));
#214836=CARTESIAN_POINT('Ctrl Pts',(5.47629810765096,15.2,9.19764235062994));
#214837=CARTESIAN_POINT('Ctrl Pts',(5.4773864436121,15.2,9.20152359963474));
#214838=CARTESIAN_POINT('Ctrl Pts',(5.47847331840386,15.2,9.20543235824444));
#214839=CARTESIAN_POINT('Ctrl Pts',(5.47956019319562,15.2,9.20934111685415));
#214840=CARTESIAN_POINT('Ctrl Pts',(5.48064560144443,15.2,9.21327738395761));
#214841=CARTESIAN_POINT('Ctrl Pts',(5.48172928874102,15.2,9.21724096598943));
#214842=CARTESIAN_POINT('Ctrl Pts',(5.4830297134497,15.2,9.2219972642548));
#214843=CARTESIAN_POINT('Ctrl Pts',(5.48432765722231,15.2,9.2267928970263));
#214844=CARTESIAN_POINT('Ctrl Pts',(5.48562267934213,15.2,9.23162753226462));
#214845=CARTESIAN_POINT('Ctrl Pts',(5.48648602750041,15.2,9.23485062271627));
#214846=CARTESIAN_POINT('Ctrl Pts',(5.48734808037473,15.2,9.23809104769311));
#214847=CARTESIAN_POINT('Ctrl Pts',(5.48820870525887,15.2,9.24134871021882));
#214848=CARTESIAN_POINT('Ctrl Pts',(5.48906933002574,15.2,9.24460637230066));
#214849=CARTESIAN_POINT('Ctrl Pts',(5.48992853026579,15.2,9.24788127249925));
#214850=CARTESIAN_POINT('Ctrl Pts',(5.49078617758473,15.2,9.25117331322835));
#214851=CARTESIAN_POINT('Ctrl Pts',(5.49164382502051,15.2,9.25446535440598));
#214852=CARTESIAN_POINT('Ctrl Pts',(5.49249992115894,15.2,9.25777453670752));
#214853=CARTESIAN_POINT('Ctrl Pts',(5.49335433998329,15.2,9.26110076399991));
#214854=CARTESIAN_POINT('Ctrl Pts',(5.49420875880763,15.2,9.2644269912923));
#214855=CARTESIAN_POINT('Ctrl Pts',(5.49506150129567,15.2,9.26777026404226));
#214856=CARTESIAN_POINT('Ctrl Pts',(5.49591244339741,15.2,9.27113048778265));
#214857=CARTESIAN_POINT('Ctrl Pts',(5.49676338538321,15.2,9.27449071106523));
#214858=CARTESIAN_POINT('Ctrl Pts',(5.49761252860366,15.2,9.27786788350966));
#214859=CARTESIAN_POINT('Ctrl Pts',(5.49845974998271,15.2,9.28126191224761));
#214860=CARTESIAN_POINT('Ctrl Pts',(5.49930697147719,15.2,9.28465594144798));
#214861=CARTESIAN_POINT('Ctrl Pts',(5.50015227166707,15.2,9.28806682570794));
#214862=CARTESIAN_POINT('Ctrl Pts',(5.50099552987949,15.2,9.29149447228535));
#214863=CARTESIAN_POINT('Ctrl Pts',(5.50183878797701,15.2,9.29492211839574));
#214864=CARTESIAN_POINT('Ctrl Pts',(5.50268000621923,15.2,9.29836652675115));
#214865=CARTESIAN_POINT('Ctrl Pts',(5.50351906420634,15.2,9.30182760346714));
#214866=CARTESIAN_POINT('Ctrl Pts',(5.50477765124416,15.2,9.30701921877689));
#214867=CARTESIAN_POINT('Ctrl Pts',(5.50603137697554,15.2,9.31224833908646));
#214868=CARTESIAN_POINT('Ctrl Pts',(5.5072798500972,15.2,9.31751465139257));
#214869=CARTESIAN_POINT('Ctrl Pts',(5.50811216558724,15.2,9.32102552658221));
#214870=CARTESIAN_POINT('Ctrl Pts',(5.50894214577708,15.2,9.32455293209843));
#214871=CARTESIAN_POINT('Ctrl Pts',(5.50976967726663,15.2,9.32809677545826));
#214872=CARTESIAN_POINT('Ctrl Pts',(5.51059720875617,15.2,9.33164061881809));
#214873=CARTESIAN_POINT('Ctrl Pts',(5.51142229116766,15.2,9.33520090112145));
#214874=CARTESIAN_POINT('Ctrl Pts',(5.51224480943444,15.2,9.33877753031806));
#214875=CARTESIAN_POINT('Ctrl Pts',(5.51306732758916,15.2,9.34235415902734));
#214876=CARTESIAN_POINT('Ctrl Pts',(5.51388728342361,15.2,9.34594713578453));
#214877=CARTESIAN_POINT('Ctrl Pts',(5.5147045642494,15.2,9.3495563680058));
#214878=CARTESIAN_POINT('Ctrl Pts',(5.51552184518655,15.2,9.35316560071883));
#214879=CARTESIAN_POINT('Ctrl Pts',(5.51633645107762,15.2,9.35679109096465));
#214880=CARTESIAN_POINT('Ctrl Pts',(5.51714827189936,15.2,9.36043274755369));
#214881=CARTESIAN_POINT('Ctrl Pts',(5.51796009261048,15.2,9.36407440364655));
#214882=CARTESIAN_POINT('Ctrl Pts',(5.51876912729418,15.2,9.36773222668446));
#214883=CARTESIAN_POINT('Ctrl Pts',(5.51957526745069,15.2,9.37140612738306));
#214884=CARTESIAN_POINT('Ctrl Pts',(5.52038140771703,15.2,9.37508002858223));
#214885=CARTESIAN_POINT('Ctrl Pts',(5.52118465309384,15.2,9.3787700061326));
#214886=CARTESIAN_POINT('Ctrl Pts',(5.52198489539939,15.2,9.38247597352111));
#214887=CARTESIAN_POINT('Ctrl Pts',(5.52278513759591,15.2,9.38618194040468));
#214888=CARTESIAN_POINT('Ctrl Pts',(5.52358237706084,15.2,9.38990389484001));
#214889=CARTESIAN_POINT('Ctrl Pts',(5.52437650721834,15.2,9.39364174964451));
#214890=CARTESIAN_POINT('Ctrl Pts',(5.52517063748404,15.2,9.39737960495828));
#214891=CARTESIAN_POINT('Ctrl Pts',(5.52596165798271,15.2,9.40113336004064));
#214892=CARTESIAN_POINT('Ctrl Pts',(5.526749463581,15.2,9.4049029280249));
#214893=CARTESIAN_POINT('Ctrl Pts',(5.52753726907194,15.2,9.40867249549554));
#214894=CARTESIAN_POINT('Ctrl Pts',(5.52832186005834,15.2,9.41245787532344));
#214895=CARTESIAN_POINT('Ctrl Pts',(5.5291031316449,15.2,9.41625898025678));
#214896=CARTESIAN_POINT('Ctrl Pts',(5.52988440333791,15.2,9.42006008570802));
#214897=CARTESIAN_POINT('Ctrl Pts',(5.53066235576293,15.2,9.42387691572295));
#214898=CARTESIAN_POINT('Ctrl Pts',(5.53143688730491,15.2,9.42770938432171));
#214899=CARTESIAN_POINT('Ctrl Pts',(5.53221141874136,15.2,9.4315418523983));
#214900=CARTESIAN_POINT('Ctrl Pts',(5.53298252767017,15.2,9.43538995900788));
#214901=CARTESIAN_POINT('Ctrl Pts',(5.53375011260779,15.2,9.43925361713489));
#214902=CARTESIAN_POINT('Ctrl Pts',(5.53451769764998,15.2,9.44311727578831));
#214903=CARTESIAN_POINT('Ctrl Pts',(5.53528175881948,15.2,9.44699648553922));
#214904=CARTESIAN_POINT('Ctrl Pts',(5.53604219647548,15.2,9.45089116276925));
#214905=CARTESIAN_POINT('Ctrl Pts',(5.53737296232167,15.2,9.45770684765646));
#214906=CARTESIAN_POINT('Ctrl Pts',(5.5386926294636,15.2,9.46456989538522));
#214907=CARTESIAN_POINT('Ctrl Pts',(5.5400006653305,15.2,9.47147985187053));
#214908=CARTESIAN_POINT('Ctrl Pts',(5.54112183887252,15.2,9.47740267140767));
#214909=CARTESIAN_POINT('Ctrl Pts',(5.54223446985674,15.2,9.48335995595096));
#214910=CARTESIAN_POINT('Ctrl Pts',(5.5433382284833,15.2,9.48935141656659));
#214911=CARTESIAN_POINT('Ctrl Pts',(5.54407406763451,15.2,9.49334572400649));
#214912=CARTESIAN_POINT('Ctrl Pts',(5.54480596489638,15.2,9.49735522218987));
#214913=CARTESIAN_POINT('Ctrl Pts',(5.5455338226023,15.2,9.50137982746629));
#214914=CARTESIAN_POINT('Ctrl Pts',(5.54626168020904,15.2,9.50540443219436));
#214915=CARTESIAN_POINT('Ctrl Pts',(5.54698550032724,15.2,9.50944414317971));
#214916=CARTESIAN_POINT('Ctrl Pts',(5.54770518671614,15.2,9.5134988772555));
#214917=CARTESIAN_POINT('Ctrl Pts',(5.54842487320309,15.2,9.51755361188376));
#214918=CARTESIAN_POINT('Ctrl Pts',(5.54914042699737,15.2,9.52162336856864));
#214919=CARTESIAN_POINT('Ctrl Pts',(5.54985175409126,15.2,9.52570806662612));
#214920=CARTESIAN_POINT('Ctrl Pts',(5.55056308108823,15.2,9.52979276412706));
#214921=CARTESIAN_POINT('Ctrl Pts',(5.55127018244964,15.2,9.53389240187326));
#214922=CARTESIAN_POINT('Ctrl Pts',(5.5519729647258,15.2,9.53800689664705));
#214923=CARTESIAN_POINT('Ctrl Pts',(5.55267574709771,15.2,9.54212139198143));
#214924=CARTESIAN_POINT('Ctrl Pts',(5.55337420969798,15.2,9.54625074512554));
#214925=CARTESIAN_POINT('Ctrl Pts',(5.55406826282565,15.2,9.55039487405968));
#214926=CARTESIAN_POINT('Ctrl Pts',(5.55476231585875,15.2,9.5545390024292));
#214927=CARTESIAN_POINT('Ctrl Pts',(5.55545195883573,15.2,9.55869790522049));
#214928=CARTESIAN_POINT('Ctrl Pts',(5.55613710116891,15.2,9.56287150260054));
#214929=CARTESIAN_POINT('Ctrl Pts',(5.55682224359543,15.2,9.56704510054923));
#214930=CARTESIAN_POINT('Ctrl Pts',(5.55750288499086,15.2,9.57123339148861));
#214931=CARTESIAN_POINT('Ctrl Pts',(5.55817893680519,15.2,9.57543629555199));
#214932=CARTESIAN_POINT('Ctrl Pts',(5.5588549885274,15.2,9.57963919904272));
#214933=CARTESIAN_POINT('Ctrl Pts',(5.55952645124896,15.2,9.58385671571892));
#214934=CARTESIAN_POINT('Ctrl Pts',(5.56019323439485,15.2,9.58808876286091));
#214935=CARTESIAN_POINT('Ctrl Pts',(5.56102671339534,15.2,9.59337882222087));
#214936=CARTESIAN_POINT('Ctrl Pts',(5.56185288362376,15.2,9.5986915873634));
#214937=CARTESIAN_POINT('Ctrl Pts',(5.56267157397138,15.2,9.60402690041779));
#214938=CARTESIAN_POINT('Ctrl Pts',(5.56349026431899,15.2,9.6093622134722));
#214939=CARTESIAN_POINT('Ctrl Pts',(5.56430147371364,15.2,9.61472007573824));
#214940=CARTESIAN_POINT('Ctrl Pts',(5.56510503517236,15.2,9.62010032893153));
#214941=CARTESIAN_POINT('Ctrl Pts',(5.5659085966311,15.2,9.6254805821248));
#214942=CARTESIAN_POINT('Ctrl Pts',(5.56670451099593,15.2,9.63088322722794));
#214943=CARTESIAN_POINT('Ctrl Pts',(5.5674926107912,15.2,9.63630811023865));
#214944=CARTESIAN_POINT('Ctrl Pts',(5.56812309066178,15.2,9.64064801688375));
#214945=CARTESIAN_POINT('Ctrl Pts',(5.56874856855144,15.2,9.64500215411906));
#214946=CARTESIAN_POINT('Ctrl Pts',(5.56936896358473,15.2,9.6493704442475));
#214947=CARTESIAN_POINT('Ctrl Pts',(5.57014445733409,15.2,9.65483080661045));
#214948=CARTESIAN_POINT('Ctrl Pts',(5.57091200490551,15.2,9.66031328220149));
#214949=CARTESIAN_POINT('Ctrl Pts',(5.57167144705763,15.2,9.66581771699492));
#214950=CARTESIAN_POINT('Ctrl Pts',(5.57227900072965,15.2,9.67022126446967));
#214951=CARTESIAN_POINT('Ctrl Pts',(5.57288136675953,15.2,9.674638865753));
#214952=CARTESIAN_POINT('Ctrl Pts',(5.57347846199122,15.2,9.67907044268858));
#214953=CARTESIAN_POINT('Ctrl Pts',(5.57407555730428,15.2,9.68350202022796));
#214954=CARTESIAN_POINT('Ctrl Pts',(5.57466738393944,15.2,9.68794757397072));
#214955=CARTESIAN_POINT('Ctrl Pts',(5.57525385913752,15.2,9.69240702593738));
#214956=CARTESIAN_POINT('Ctrl Pts',(5.57598695309516,15.2,9.69798134059192));
#214957=CARTESIAN_POINT('Ctrl Pts',(5.576711687361,15.2,9.70357736888849));
#214958=CARTESIAN_POINT('Ctrl Pts',(5.57742790465198,15.2,9.70919496270973));
#214959=CARTESIAN_POINT('Ctrl Pts',(5.57785763501095,15.2,9.71256551888001));
#214960=CARTESIAN_POINT('Ctrl Pts',(5.57828429970981,15.2,9.71594383709144));
#214961=CARTESIAN_POINT('Ctrl Pts',(5.57870786513189,15.2,9.71932988693013));
#214962=CARTESIAN_POINT('Ctrl Pts',(5.57941380752767,15.2,9.72497330353301));
#214963=CARTESIAN_POINT('Ctrl Pts',(5.58011114089075,15.2,9.73063819103081));
#214964=CARTESIAN_POINT('Ctrl Pts',(5.58079971234836,15.2,9.7363244040187));
#214965=CARTESIAN_POINT('Ctrl Pts',(5.58135056946943,15.2,9.74087337403714));
#214966=CARTESIAN_POINT('Ctrl Pts',(5.58189581960788,15.2,9.74543598981206));
#214967=CARTESIAN_POINT('Ctrl Pts',(5.5824353847308,15.2,9.75001217665929));
#214968=CARTESIAN_POINT('Ctrl Pts',(5.58284005859138,15.2,9.75344431695061));
#214969=CARTESIAN_POINT('Ctrl Pts',(5.58324153406708,15.2,9.75688409073694));
#214970=CARTESIAN_POINT('Ctrl Pts',(5.58363978044788,15.2,9.76033146532468));
#214971=CARTESIAN_POINT('Ctrl Pts',(5.58403802682868,15.2,9.76377883991242));
#214972=CARTESIAN_POINT('Ctrl Pts',(5.58443304351169,15.2,9.76723381760528));
#214973=CARTESIAN_POINT('Ctrl Pts',(5.58482479795623,15.2,9.7706963625201));
#214974=CARTESIAN_POINT('Ctrl Pts',(5.58521655247194,15.2,9.77415890806395));
#214975=CARTESIAN_POINT('Ctrl Pts',(5.5856050453284,15.2,9.77762902376828));
#214976=CARTESIAN_POINT('Ctrl Pts',(5.58599024430061,15.2,9.78110667577474));
#214977=CARTESIAN_POINT('Ctrl Pts',(5.58637544320283,15.2,9.78458432714942));
#214978=CARTESIAN_POINT('Ctrl Pts',(5.58675734805522,15.2,9.78806951627366));
#214979=CARTESIAN_POINT('Ctrl Pts',(5.58713592879118,15.2,9.79156221014743));
#214980=CARTESIAN_POINT('Ctrl Pts',(5.58776689670736,15.2,9.79738336681522));
#214981=CARTESIAN_POINT('Ctrl Pts',(5.58838862555219,15.2,9.80322537210294));
#214982=CARTESIAN_POINT('Ctrl Pts',(5.58900097530435,15.2,9.80908807968891));
#214983=CARTESIAN_POINT('Ctrl Pts',(5.58961332505651,15.2,9.81495078727488));
#214984=CARTESIAN_POINT('Ctrl Pts',(5.59021629202837,15.2,9.82083419513713));
#214985=CARTESIAN_POINT('Ctrl Pts',(5.59080973681925,15.2,9.82673815847218));
#214986=CARTESIAN_POINT('Ctrl Pts',(5.59116580368086,15.2,9.83028053634449));
#214987=CARTESIAN_POINT('Ctrl Pts',(5.59151844210096,15.2,9.83383031509972));
#214988=CARTESIAN_POINT('Ctrl Pts',(5.59186762154631,15.2,9.8373874613878));
#214989=CARTESIAN_POINT('Ctrl Pts',(5.59221680099165,15.2,9.84094460767589));
#214990=CARTESIAN_POINT('Ctrl Pts',(5.59256252184574,15.2,9.84450912229638));
#214991=CARTESIAN_POINT('Ctrl Pts',(5.59290475370831,15.2,9.84808097454161));
#214992=CARTESIAN_POINT('Ctrl Pts',(5.59324698557087,15.2,9.85165282678683));
#214993=CARTESIAN_POINT('Ctrl Pts',(5.59358572742524,15.2,9.85523201584012));
#214994=CARTESIAN_POINT('Ctrl Pts',(5.5939209512467,15.2,9.85881851112579));
#214995=CARTESIAN_POINT('Ctrl Pts',(5.59447965763609,15.2,9.86479600348576));
#214996=CARTESIAN_POINT('Ctrl Pts',(5.59502858784164,15.2,9.87079379022497));
#214997=CARTESIAN_POINT('Ctrl Pts',(5.59556760548301,15.2,9.87681172677999));
#214998=CARTESIAN_POINT('Ctrl Pts',(5.59589101605607,15.2,9.8804224885818));
#214999=CARTESIAN_POINT('Ctrl Pts',(5.59621085935995,15.2,9.88404050453726));
#215000=CARTESIAN_POINT('Ctrl Pts',(5.59652710389044,15.2,9.88766574336324));
#215001=CARTESIAN_POINT('Ctrl Pts',(5.59684334842093,15.2,9.89129098218923));
#215002=CARTESIAN_POINT('Ctrl Pts',(5.59715599571,15.2,9.89492344388971));
#215003=CARTESIAN_POINT('Ctrl Pts',(5.5974650156576,15.2,9.89856309817317));
#215004=CARTESIAN_POINT('Ctrl Pts',(5.59777403566135,15.2,9.90220275311783));
#215005=CARTESIAN_POINT('Ctrl Pts',(5.59807942928906,15.2,9.90584960063116));
#215006=CARTESIAN_POINT('Ctrl Pts',(5.59838116637408,15.2,9.90950360907985));
#215007=CARTESIAN_POINT('Ctrl Pts',(5.59878348239608,15.2,9.91437561923842));
#215008=CARTESIAN_POINT('Ctrl Pts',(5.59917929962418,15.2,9.91926036112476));
#215009=CARTESIAN_POINT('Ctrl Pts',(5.59956854948304,15.2,9.9241577607466));
#215010=CARTESIAN_POINT('Ctrl Pts',(5.59986048689044,15.2,9.92783081062981));
#215011=CARTESIAN_POINT('Ctrl Pts',(5.60014873031224,15.2,9.93151098146608));
#215012=CARTESIAN_POINT('Ctrl Pts',(5.60043325126056,15.2,9.93519824133148));
#215013=CARTESIAN_POINT('Ctrl Pts',(5.60071777220888,15.2,9.93888550119688));
#215014=CARTESIAN_POINT('Ctrl Pts',(5.60099857099912,15.2,9.9425798508285));
#215015=CARTESIAN_POINT('Ctrl Pts',(5.60127561948957,15.2,9.94628126015137));
#215016=CARTESIAN_POINT('Ctrl Pts',(5.60155266803035,15.2,9.94998267014666));
#215017=CARTESIAN_POINT('Ctrl Pts',(5.60182596658673,15.2,9.95369114070231));
#215018=CARTESIAN_POINT('Ctrl Pts',(5.60209548708372,15.2,9.9574066400766));
#215019=CARTESIAN_POINT('Ctrl Pts',(5.60245484766478,15.2,9.96236063811736));
#215020=CARTESIAN_POINT('Ctrl Pts',(5.60280749045975,15.2,9.96732713044767));
#215021=CARTESIAN_POINT('Ctrl Pts',(5.6031533477664,15.2,9.97230604472988));
#215022=CARTESIAN_POINT('Ctrl Pts',(5.60341274075817,15.2,9.97604023061113));
#215023=CARTESIAN_POINT('Ctrl Pts',(5.60366831649795,15.2,9.97978140382829));
#215024=CARTESIAN_POINT('Ctrl Pts',(5.60392005194747,15.2,9.98352953581651));
#215025=CARTESIAN_POINT('Ctrl Pts',(5.60417178739699,15.2,9.98727766780473));
#215026=CARTESIAN_POINT('Ctrl Pts',(5.60441968127177,15.2,9.99103276188411));
#215027=CARTESIAN_POINT('Ctrl Pts',(5.60466370822177,15.2,9.99479478516316));
#215028=CARTESIAN_POINT('Ctrl Pts',(5.6049077352161,15.2,9.99855680912564));
#215029=CARTESIAN_POINT('Ctrl Pts',(5.605147895501,15.2,10.0023257629567));
#215030=CARTESIAN_POINT('Ctrl Pts',(5.60538415403481,15.2,10.0061016118397));
#215031=CARTESIAN_POINT('Ctrl Pts',(5.60562041252569,15.2,10.0098774600368));
#215032=CARTESIAN_POINT('Ctrl Pts',(5.60585277035814,15.2,10.0136602020641));
#215033=CARTESIAN_POINT('Ctrl Pts',(5.60608119706913,15.2,10.0174498046999));
#215034=CARTESIAN_POINT('Ctrl Pts',(5.60630962378012,15.2,10.0212394073356));
#215035=CARTESIAN_POINT('Ctrl Pts',(5.60653412142436,15.2,10.0250358705591));
#215036=CARTESIAN_POINT('Ctrl Pts',(5.60675467580093,15.2,10.0288391806629));
#215037=CARTESIAN_POINT('Ctrl Pts',(5.6069752301775,15.2,10.0326424907666));
#215038=CARTESIAN_POINT('Ctrl Pts',(5.60719183796131,15.2,10.0364526443066));
#215039=CARTESIAN_POINT('Ctrl Pts',(5.60740451299995,15.2,10.04026965));
#215040=CARTESIAN_POINT('Ctrl Pts',(5.36127880499994,12.2,8.88241603299999));
#215041=CARTESIAN_POINT('Ctrl Pts',(5.36206719568413,12.2,8.88401933383977));
#215042=CARTESIAN_POINT('Ctrl Pts',(5.3628759863957,12.2,8.88567631031983));
#215043=CARTESIAN_POINT('Ctrl Pts',(5.36370417391754,12.2,8.88738636482928));
#215044=CARTESIAN_POINT('Ctrl Pts',(5.36453635537823,12.2,8.88910466608596));
#215045=CARTESIAN_POINT('Ctrl Pts',(5.36538812011717,12.2,8.89087656335787));
#215046=CARTESIAN_POINT('Ctrl Pts',(5.36625847962582,12.2,8.89270147796823));
#215047=CARTESIAN_POINT('Ctrl Pts',(5.36712883905543,12.2,8.89452639241284));
#215048=CARTESIAN_POINT('Ctrl Pts',(5.36801779174953,12.2,8.89640432539507));
#215049=CARTESIAN_POINT('Ctrl Pts',(5.36892438021658,12.2,8.89833471374155));
#215050=CARTESIAN_POINT('Ctrl Pts',(5.36983096868362,12.2,8.90026510208804));
#215051=CARTESIAN_POINT('Ctrl Pts',(5.37075519224708,12.2,8.90224794602847));
#215052=CARTESIAN_POINT('Ctrl Pts',(5.3716961199256,12.2,8.90428269455318));
#215053=CARTESIAN_POINT('Ctrl Pts',(5.37263704768957,12.2,8.90631744326271));
#215054=CARTESIAN_POINT('Ctrl Pts',(5.37359468033524,12.2,8.9084040964046));
#215055=CARTESIAN_POINT('Ctrl Pts',(5.37456811338936,12.2,8.91054211894128));
#215056=CARTESIAN_POINT('Ctrl Pts',(5.37570378515322,12.2,8.91303647827611));
#215057=CARTESIAN_POINT('Ctrl Pts',(5.37686096291785,12.2,8.91560075447309));
#215058=CARTESIAN_POINT('Ctrl Pts',(5.37803825790234,12.2,8.91823411554835));
#215059=CARTESIAN_POINT('Ctrl Pts',(5.3790473680069,12.2,8.92049128244788));
#215060=CARTESIAN_POINT('Ctrl Pts',(5.38007125793053,12.2,8.92279920619165));
#215061=CARTESIAN_POINT('Ctrl Pts',(5.38110908007138,12.2,8.92515737499027));
#215062=CARTESIAN_POINT('Ctrl Pts',(5.38214690211796,12.2,8.92751554357471));
#215063=CARTESIAN_POINT('Ctrl Pts',(5.38319865533422,12.2,8.9299239569457));
#215064=CARTESIAN_POINT('Ctrl Pts',(5.38426351746706,12.2,8.93238211453432));
#215065=CARTESIAN_POINT('Ctrl Pts',(5.38532837959989,12.2,8.93484027212294));
#215066=CARTESIAN_POINT('Ctrl Pts',(5.3864063481307,12.2,8.93734817377245));
#215067=CARTESIAN_POINT('Ctrl Pts',(5.38749662325722,12.2,8.93990532934408));
#215068=CARTESIAN_POINT('Ctrl Pts',(5.38858689848278,12.2,8.94246248514798));
#215069=CARTESIAN_POINT('Ctrl Pts',(5.38968947790153,12.2,8.94506889477464));
#215070=CARTESIAN_POINT('Ctrl Pts',(5.39080358337969,12.2,8.94772407675599));
#215071=CARTESIAN_POINT('Ctrl Pts',(5.39191768875667,12.2,8.95037925849614));
#215072=CARTESIAN_POINT('Ctrl Pts',(5.39304331814439,12.2,8.95308321474799));
#215073=CARTESIAN_POINT('Ctrl Pts',(5.39417971535357,12.2,8.95583547065011));
#215074=CARTESIAN_POINT('Ctrl Pts',(5.39531611256277,12.2,8.95858772655223));
#215075=CARTESIAN_POINT('Ctrl Pts',(5.39646327322106,12.2,8.96138828550877));
#215076=CARTESIAN_POINT('Ctrl Pts',(5.39762045992857,12.2,8.96423668331986));
#215077=CARTESIAN_POINT('Ctrl Pts',(5.39877764663609,12.2,8.96708508113096));
#215078=CARTESIAN_POINT('Ctrl Pts',(5.39994486175675,12.2,8.96998131745591));
#215079=CARTESIAN_POINT('Ctrl Pts',(5.40112137963002,12.2,8.97292494117905));
#215080=CARTESIAN_POINT('Ctrl Pts',(5.40229789761017,12.2,8.97586856516956));
#215081=CARTESIAN_POINT('Ctrl Pts',(5.40348372275793,12.2,8.97885957314806));
#215082=CARTESIAN_POINT('Ctrl Pts',(5.40467814957339,12.2,8.981897523149));
#215083=CARTESIAN_POINT('Ctrl Pts',(5.40587257628037,12.2,8.984935472874));
#215084=CARTESIAN_POINT('Ctrl Pts',(5.40707560536163,12.2,8.98802036289522));
#215085=CARTESIAN_POINT('Ctrl Pts',(5.40828655315063,12.2,8.99115175477942));
#215086=CARTESIAN_POINT('Ctrl Pts',(5.40949750093961,12.2,8.99428314666363));
#215087=CARTESIAN_POINT('Ctrl Pts',(5.41071636676135,12.2,8.99746104326049));
#215088=CARTESIAN_POINT('Ctrl Pts',(5.41194248188295,12.2,9.00068501039017));
#215089=CARTESIAN_POINT('Ctrl Pts',(5.41316859711593,12.2,9.00390897781269));
#215090=CARTESIAN_POINT('Ctrl Pts',(5.41440196414134,12.2,9.00717902039809));
#215091=CARTESIAN_POINT('Ctrl Pts',(5.41564192829254,12.2,9.01049471074747));
#215092=CARTESIAN_POINT('Ctrl Pts',(5.41688189233111,12.2,9.01381040079567));
#215093=CARTESIAN_POINT('Ctrl Pts',(5.41812845637254,12.2,9.01717174290682));
#215094=CARTESIAN_POINT('Ctrl Pts',(5.41938098149937,12.2,9.02057831696503));
#215095=CARTESIAN_POINT('Ctrl Pts',(5.42063350662618,12.2,9.02398489102326));
#215096=CARTESIAN_POINT('Ctrl Pts',(5.42189199455013,12.2,9.02743670033225));
#215097=CARTESIAN_POINT('Ctrl Pts',(5.42315582458718,12.2,9.03093333336878));
#215098=CARTESIAN_POINT('Ctrl Pts',(5.42441965473902,12.2,9.03442996672293));
#215099=CARTESIAN_POINT('Ctrl Pts',(5.42568882599815,12.2,9.03797142575305));
#215100=CARTESIAN_POINT('Ctrl Pts',(5.42696273238152,12.2,9.04155730713024));
#215101=CARTESIAN_POINT('Ctrl Pts',(5.42823663864917,12.2,9.04514318818172));
#215102=CARTESIAN_POINT('Ctrl Pts',(5.42951527992153,12.2,9.0487734910667));
#215103=CARTESIAN_POINT('Ctrl Pts',(5.43079806495826,12.2,9.05244781826653));
#215104=CARTESIAN_POINT('Ctrl Pts',(5.43208084999499,12.2,9.05612214546637));
#215105=CARTESIAN_POINT('Ctrl Pts',(5.43336777664106,12.2,9.05984049843734));
#215106=CARTESIAN_POINT('Ctrl Pts',(5.43465826715844,12.2,9.06360248665276));
#215107=CARTESIAN_POINT('Ctrl Pts',(5.435733675962,12.2,9.06673747694619));
#215108=CARTESIAN_POINT('Ctrl Pts',(5.43681156121276,12.2,9.06990276903155));
#215109=CARTESIAN_POINT('Ctrl Pts',(5.43789159246265,12.2,9.07309813930779));
#215110=CARTESIAN_POINT('Ctrl Pts',(5.43897162371255,12.2,9.07629350958402));
#215111=CARTESIAN_POINT('Ctrl Pts',(5.44005380160138,12.2,9.0795189574332));
#215112=CARTESIAN_POINT('Ctrl Pts',(5.44113780521239,12.2,9.08277426507052));
#215113=CARTESIAN_POINT('Ctrl Pts',(5.44222180882341,12.2,9.08602957270784));
#215114=CARTESIAN_POINT('Ctrl Pts',(5.44330763673329,12.2,9.08931473918867));
#215115=CARTESIAN_POINT('Ctrl Pts',(5.44439497451601,12.2,9.09262954448143));
#215116=CARTESIAN_POINT('Ctrl Pts',(5.44548231229873,12.2,9.09594434977421));
#215117=CARTESIAN_POINT('Ctrl Pts',(5.44657115834994,12.2,9.09928879568324));
#215118=CARTESIAN_POINT('Ctrl Pts',(5.44766120376661,12.2,9.10266266672491));
#215119=CARTESIAN_POINT('Ctrl Pts',(5.44875124918328,12.2,9.10603653776656));
#215120=CARTESIAN_POINT('Ctrl Pts',(5.44984249207336,12.2,9.10943983441946));
#215121=CARTESIAN_POINT('Ctrl Pts',(5.45093462930054,12.2,9.11287234151845));
#215122=CARTESIAN_POINT('Ctrl Pts',(5.45202676652772,12.2,9.11630484861744));
#215123=CARTESIAN_POINT('Ctrl Pts',(5.45311979771034,12.2,9.11976656888801));
#215124=CARTESIAN_POINT('Ctrl Pts',(5.4542134240298,12.2,9.12325728923671));
#215125=CARTESIAN_POINT('Ctrl Pts',(5.45530705034927,12.2,9.12674800958542));
#215126=CARTESIAN_POINT('Ctrl Pts',(5.45640127076041,12.2,9.13026773298068));
#215127=CARTESIAN_POINT('Ctrl Pts',(5.45749579207986,12.2,9.13381624673216));
#215128=CARTESIAN_POINT('Ctrl Pts',(5.45859031339931,12.2,9.13736476048364));
#215129=CARTESIAN_POINT('Ctrl Pts',(5.45968513585568,12.2,9.14094206818094));
#215130=CARTESIAN_POINT('Ctrl Pts',(5.4607799698687,12.2,9.14454796266859));
#215131=CARTESIAN_POINT('Ctrl Pts',(5.46187480388173,12.2,9.14815385715625));
#215132=CARTESIAN_POINT('Ctrl Pts',(5.46296964992647,12.2,9.1517883369267));
#215133=CARTESIAN_POINT('Ctrl Pts',(5.46406422388478,12.2,9.15545120047069));
#215134=CARTESIAN_POINT('Ctrl Pts',(5.4651587978431,12.2,9.15911406401468));
#215135=CARTESIAN_POINT('Ctrl Pts',(5.46625310024305,12.2,9.16280530907858));
#215136=CARTESIAN_POINT('Ctrl Pts',(5.46734685170134,12.2,9.16652473526142));
#215137=CARTESIAN_POINT('Ctrl Pts',(5.46844060304041,12.2,9.17024416103885));
#215138=CARTESIAN_POINT('Ctrl Pts',(5.46953380253719,12.2,9.17399176741993));
#215139=CARTESIAN_POINT('Ctrl Pts',(5.47062617880706,12.2,9.1777673547144));
#215140=CARTESIAN_POINT('Ctrl Pts',(5.471718555196,12.2,9.18154294242043));
#215141=CARTESIAN_POINT('Ctrl Pts',(5.47281010629056,12.2,9.18534650960661));
#215142=CARTESIAN_POINT('Ctrl Pts',(5.47390056212398,12.2,9.18917786071545));
#215143=CARTESIAN_POINT('Ctrl Pts',(5.47499101795739,12.2,9.19300921182428));
#215144=CARTESIAN_POINT('Ctrl Pts',(5.47608038170198,12.2,9.19686834516053));
#215145=CARTESIAN_POINT('Ctrl Pts',(5.47716838413264,12.2,9.20075506474153));
#215146=CARTESIAN_POINT('Ctrl Pts',(5.47825638656329,12.2,9.20464178432255));
#215147=CARTESIAN_POINT('Ctrl Pts',(5.47934303200856,12.2,9.20855609118631));
#215148=CARTESIAN_POINT('Ctrl Pts',(5.48042805463232,12.2,9.21249779082578));
#215149=CARTESIAN_POINT('Ctrl Pts',(5.48151307725608,12.2,9.21643949046523));
#215150=CARTESIAN_POINT('Ctrl Pts',(5.48259648117356,12.2,9.22040858079572));
#215151=CARTESIAN_POINT('Ctrl Pts',(5.48367800943754,12.2,9.22440487273872));
#215152=CARTESIAN_POINT('Ctrl Pts',(5.48475953770153,12.2,9.22840116468173));
#215153=CARTESIAN_POINT('Ctrl Pts',(5.48583918855158,12.2,9.23242465535882));
#215154=CARTESIAN_POINT('Ctrl Pts',(5.4869167134128,12.2,9.23647515646851));
#215155=CARTESIAN_POINT('Ctrl Pts',(5.48777873334876,12.2,9.23971555753287));
#215156=CARTESIAN_POINT('Ctrl Pts',(5.4886393897461,12.2,9.2429732441344));
#215157=CARTESIAN_POINT('Ctrl Pts',(5.48949855839128,12.2,9.24624812020022));
#215158=CARTESIAN_POINT('Ctrl Pts',(5.4903577269194,12.2,9.24952299581985));
#215159=CARTESIAN_POINT('Ctrl Pts',(5.4912154050665,12.2,9.25281506044842));
#215160=CARTESIAN_POINT('Ctrl Pts',(5.49207146966329,12.2,9.25612421845456));
#215161=CARTESIAN_POINT('Ctrl Pts',(5.49292753437671,12.2,9.25943337691156));
#215162=CARTESIAN_POINT('Ctrl Pts',(5.49378198440939,12.2,9.26275962837338));
#215163=CARTESIAN_POINT('Ctrl Pts',(5.49463469584464,12.2,9.26610287755673));
#215164=CARTESIAN_POINT('Ctrl Pts',(5.49548740716372,12.2,9.26944612628455));
#215165=CARTESIAN_POINT('Ctrl Pts',(5.49633837897022,12.2,9.27280637324101));
#215166=CARTESIAN_POINT('Ctrl Pts',(5.49718749161006,12.2,9.2761835222433));
#215167=CARTESIAN_POINT('Ctrl Pts',(5.4980366043656,12.2,9.27956067170573));
#215168=CARTESIAN_POINT('Ctrl Pts',(5.4988838562092,12.2,9.28295472484192));
#215169=CARTESIAN_POINT('Ctrl Pts',(5.4997291263107,12.2,9.28636558602892));
#215170=CARTESIAN_POINT('Ctrl Pts',(5.50057439629703,12.2,9.28977644675119));
#215171=CARTESIAN_POINT('Ctrl Pts',(5.50141768383653,12.2,9.29320411643952));
#215172=CARTESIAN_POINT('Ctrl Pts',(5.50225887187908,12.2,9.29664850121177));
#215173=CARTESIAN_POINT('Ctrl Pts',(5.50310006003624,12.2,9.3000928864533));
#215174=CARTESIAN_POINT('Ctrl Pts',(5.5039391477928,12.2,9.30355398628027));
#215175=CARTESIAN_POINT('Ctrl Pts',(5.50477601600886,12.2,9.30703170948562));
#215176=CARTESIAN_POINT('Ctrl Pts',(5.50561288411089,12.2,9.31050943221713));
#215177=CARTESIAN_POINT('Ctrl Pts',(5.50644753472056,12.2,9.31400377668128));
#215178=CARTESIAN_POINT('Ctrl Pts',(5.5072798500972,12.2,9.31751465139257));
#215179=CARTESIAN_POINT('Ctrl Pts',(5.50811216558724,12.2,9.32102552658221));
#215180=CARTESIAN_POINT('Ctrl Pts',(5.50894214577708,12.2,9.32455293209843));
#215181=CARTESIAN_POINT('Ctrl Pts',(5.50976967726663,12.2,9.32809677545826));
#215182=CARTESIAN_POINT('Ctrl Pts',(5.51059720875617,12.2,9.33164061881809));
#215183=CARTESIAN_POINT('Ctrl Pts',(5.51142229116766,12.2,9.33520090112145));
#215184=CARTESIAN_POINT('Ctrl Pts',(5.51224480943444,12.2,9.33877753031806));
#215185=CARTESIAN_POINT('Ctrl Pts',(5.51306732758916,12.2,9.34235415902734));
#215186=CARTESIAN_POINT('Ctrl Pts',(5.51388728342361,12.2,9.34594713578453));
#215187=CARTESIAN_POINT('Ctrl Pts',(5.5147045642494,12.2,9.3495563680058));
#215188=CARTESIAN_POINT('Ctrl Pts',(5.51552184518655,12.2,9.35316560071883));
#215189=CARTESIAN_POINT('Ctrl Pts',(5.51633645107762,12.2,9.35679109096465));
#215190=CARTESIAN_POINT('Ctrl Pts',(5.51714827189936,12.2,9.36043274755369));
#215191=CARTESIAN_POINT('Ctrl Pts',(5.51796009261048,12.2,9.36407440364655));
#215192=CARTESIAN_POINT('Ctrl Pts',(5.51876912729418,12.2,9.36773222668446));
#215193=CARTESIAN_POINT('Ctrl Pts',(5.51957526745069,12.2,9.37140612738306));
#215194=CARTESIAN_POINT('Ctrl Pts',(5.52038140771703,12.2,9.37508002858223));
#215195=CARTESIAN_POINT('Ctrl Pts',(5.52118465309384,12.2,9.3787700061326));
#215196=CARTESIAN_POINT('Ctrl Pts',(5.52198489539939,12.2,9.38247597352111));
#215197=CARTESIAN_POINT('Ctrl Pts',(5.52278513759591,12.2,9.38618194040468));
#215198=CARTESIAN_POINT('Ctrl Pts',(5.52358237706084,12.2,9.38990389484001));
#215199=CARTESIAN_POINT('Ctrl Pts',(5.52437650721834,12.2,9.39364174964451));
#215200=CARTESIAN_POINT('Ctrl Pts',(5.52517063748404,12.2,9.39737960495828));
#215201=CARTESIAN_POINT('Ctrl Pts',(5.52596165798271,12.2,9.40113336004065));
#215202=CARTESIAN_POINT('Ctrl Pts',(5.526749463581,12.2,9.4049029280249));
#215203=CARTESIAN_POINT('Ctrl Pts',(5.52753726907195,12.2,9.40867249549555));
#215204=CARTESIAN_POINT('Ctrl Pts',(5.52832186005834,12.2,9.41245787532344));
#215205=CARTESIAN_POINT('Ctrl Pts',(5.52910313164491,12.2,9.41625898025678));
#215206=CARTESIAN_POINT('Ctrl Pts',(5.52988440333791,12.2,9.42006008570802));
#215207=CARTESIAN_POINT('Ctrl Pts',(5.53066235576293,12.2,9.42387691572295));
#215208=CARTESIAN_POINT('Ctrl Pts',(5.53143688730491,12.2,9.42770938432171));
#215209=CARTESIAN_POINT('Ctrl Pts',(5.53221141874136,12.2,9.4315418523983));
#215210=CARTESIAN_POINT('Ctrl Pts',(5.53298252767017,12.2,9.43538995900788));
#215211=CARTESIAN_POINT('Ctrl Pts',(5.53375011260779,12.2,9.43925361713489));
#215212=CARTESIAN_POINT('Ctrl Pts',(5.53451769764998,12.2,9.44311727578831));
#215213=CARTESIAN_POINT('Ctrl Pts',(5.53528175881948,12.2,9.44699648553922));
#215214=CARTESIAN_POINT('Ctrl Pts',(5.53604219647548,12.2,9.45089116276925));
#215215=CARTESIAN_POINT('Ctrl Pts',(5.53680263402787,12.2,9.45478583946862));
#215216=CARTESIAN_POINT('Ctrl Pts',(5.53755944722412,12.2,9.45869598150561));
#215217=CARTESIAN_POINT('Ctrl Pts',(5.53831253688516,12.2,9.46262150434977));
#215218=CARTESIAN_POINT('Ctrl Pts',(5.5390656266488,12.2,9.46654702772878));
#215219=CARTESIAN_POINT('Ctrl Pts',(5.53981499415934,12.2,9.47048793140378));
#215220=CARTESIAN_POINT('Ctrl Pts',(5.54056053853329,12.2,9.47444413200825));
#215221=CARTESIAN_POINT('Ctrl Pts',(5.54149246894995,12.2,9.47938938249433));
#215222=CARTESIAN_POINT('Ctrl Pts',(5.54241842959441,12.2,9.48435853253883));
#215223=CARTESIAN_POINT('Ctrl Pts',(5.5433382284833,12.2,9.48935141656659));
#215224=CARTESIAN_POINT('Ctrl Pts',(5.54407406763451,12.2,9.49334572400649));
#215225=CARTESIAN_POINT('Ctrl Pts',(5.54480596489638,12.2,9.49735522218987));
#215226=CARTESIAN_POINT('Ctrl Pts',(5.5455338226023,12.2,9.50137982746629));
#215227=CARTESIAN_POINT('Ctrl Pts',(5.54626168020904,12.2,9.50540443219436));
#215228=CARTESIAN_POINT('Ctrl Pts',(5.54698550032724,12.2,9.50944414317971));
#215229=CARTESIAN_POINT('Ctrl Pts',(5.54770518671614,12.2,9.5134988772555));
#215230=CARTESIAN_POINT('Ctrl Pts',(5.54842487320309,12.2,9.51755361188376));
#215231=CARTESIAN_POINT('Ctrl Pts',(5.54914042699737,12.2,9.52162336856864));
#215232=CARTESIAN_POINT('Ctrl Pts',(5.54985175409126,12.2,9.52570806662612));
#215233=CARTESIAN_POINT('Ctrl Pts',(5.55056308108823,12.2,9.52979276412706));
#215234=CARTESIAN_POINT('Ctrl Pts',(5.55127018244964,12.2,9.53389240187326));
#215235=CARTESIAN_POINT('Ctrl Pts',(5.5519729647258,12.2,9.53800689664705));
#215236=CARTESIAN_POINT('Ctrl Pts',(5.55267574709771,12.2,9.54212139198143));
#215237=CARTESIAN_POINT('Ctrl Pts',(5.55337420969798,12.2,9.54625074512554));
#215238=CARTESIAN_POINT('Ctrl Pts',(5.55406826282565,12.2,9.55039487405968));
#215239=CARTESIAN_POINT('Ctrl Pts',(5.55476231585875,12.2,9.5545390024292));
#215240=CARTESIAN_POINT('Ctrl Pts',(5.55545195883573,12.2,9.55869790522049));
#215241=CARTESIAN_POINT('Ctrl Pts',(5.55613710116891,12.2,9.56287150260054));
#215242=CARTESIAN_POINT('Ctrl Pts',(5.55682224359543,12.2,9.56704510054923));
#215243=CARTESIAN_POINT('Ctrl Pts',(5.55750288499086,12.2,9.57123339148861));
#215244=CARTESIAN_POINT('Ctrl Pts',(5.55817893680519,12.2,9.57543629555199));
#215245=CARTESIAN_POINT('Ctrl Pts',(5.5588549885274,12.2,9.57963919904272));
#215246=CARTESIAN_POINT('Ctrl Pts',(5.55952645124896,12.2,9.58385671571892));
#215247=CARTESIAN_POINT('Ctrl Pts',(5.56019323439485,12.2,9.58808876286091));
#215248=CARTESIAN_POINT('Ctrl Pts',(5.56102671339534,12.2,9.59337882222087));
#215249=CARTESIAN_POINT('Ctrl Pts',(5.56185288362376,12.2,9.5986915873634));
#215250=CARTESIAN_POINT('Ctrl Pts',(5.56267157397138,12.2,9.6040269004178));
#215251=CARTESIAN_POINT('Ctrl Pts',(5.56332652628516,12.2,9.60829515109394));
#215252=CARTESIAN_POINT('Ctrl Pts',(5.56397669008727,12.2,9.61257783309124));
#215253=CARTESIAN_POINT('Ctrl Pts',(5.56462198184434,12.2,9.61687486582635));
#215254=CARTESIAN_POINT('Ctrl Pts',(5.56526727351349,12.2,9.621171897976));
#215255=CARTESIAN_POINT('Ctrl Pts',(5.56590769039972,12.2,9.6254832805583));
#215256=CARTESIAN_POINT('Ctrl Pts',(5.56654315015773,12.2,9.629808934364));
#215257=CARTESIAN_POINT('Ctrl Pts',(5.56717861000232,12.2,9.63413458875908));
#215258=CARTESIAN_POINT('Ctrl Pts',(5.56780911127284,12.2,9.63847451556499));
#215259=CARTESIAN_POINT('Ctrl Pts',(5.56843456908438,12.2,9.64282863308101));
#215260=CARTESIAN_POINT('Ctrl Pts',(5.5690600268107,12.2,9.64718275000377));
#215261=CARTESIAN_POINT('Ctrl Pts',(5.5696804424908,12.2,9.65155105993478));
#215262=CARTESIAN_POINT('Ctrl Pts',(5.57029573160769,12.2,9.65593348207507));
#215263=CARTESIAN_POINT('Ctrl Pts',(5.57091102080842,12.2,9.66031590481246));
#215264=CARTESIAN_POINT('Ctrl Pts',(5.57152118377301,12.2,9.66471244115915));
#215265=CARTESIAN_POINT('Ctrl Pts',(5.57212613830871,12.2,9.66912301075294));
#215266=CARTESIAN_POINT('Ctrl Pts',(5.57257985416927,12.2,9.67243093764781));
#215267=CARTESIAN_POINT('Ctrl Pts',(5.57303064054712,12.2,9.67574675983595));
#215268=CARTESIAN_POINT('Ctrl Pts',(5.57347846199122,12.2,9.67907044268858));
#215269=CARTESIAN_POINT('Ctrl Pts',(5.57392628343534,12.2,9.68239412554122));
#215270=CARTESIAN_POINT('Ctrl Pts',(5.57437114110088,12.2,9.68572567055809));
#215271=CARTESIAN_POINT('Ctrl Pts',(5.57481300041842,12.2,9.6890650433944));
#215272=CARTESIAN_POINT('Ctrl Pts',(5.57525485973595,12.2,9.69240441623071));
#215273=CARTESIAN_POINT('Ctrl Pts',(5.57569371987037,12.2,9.69575161812483));
#215274=CARTESIAN_POINT('Ctrl Pts',(5.57612954864662,12.2,9.69910661496022));
#215275=CARTESIAN_POINT('Ctrl Pts',(5.57656537750204,12.2,9.7024616124051));
#215276=CARTESIAN_POINT('Ctrl Pts',(5.57699817421494,12.2,9.70582440592713));
#215277=CARTESIAN_POINT('Ctrl Pts',(5.57742790465198,12.2,9.70919496270973));
#215278=CARTESIAN_POINT('Ctrl Pts',(5.57785763501095,12.2,9.71256551888001));
#215279=CARTESIAN_POINT('Ctrl Pts',(5.57828429970981,12.2,9.71594383709144));
#215280=CARTESIAN_POINT('Ctrl Pts',(5.57870786513189,12.2,9.71932988693013));
#215281=CARTESIAN_POINT('Ctrl Pts',(5.57913143055397,12.2,9.72271593676883));
#215282=CARTESIAN_POINT('Ctrl Pts',(5.57955189691084,12.2,9.72610971659373));
#215283=CARTESIAN_POINT('Ctrl Pts',(5.57996923081207,12.2,9.72951119392916));
#215284=CARTESIAN_POINT('Ctrl Pts',(5.5803865647133,12.2,9.73291267126461));
#215285=CARTESIAN_POINT('Ctrl Pts',(5.58080076609824,12.2,9.7363218472074));
#215286=CARTESIAN_POINT('Ctrl Pts',(5.58121180249997,12.2,9.73973868849992));
#215287=CARTESIAN_POINT('Ctrl Pts',(5.5816228389017,12.2,9.74315552979245));
#215288=CARTESIAN_POINT('Ctrl Pts',(5.58203071087023,12.2,9.74658003636799));
#215289=CARTESIAN_POINT('Ctrl Pts',(5.5824353847308,12.2,9.75001217665929));
#215290=CARTESIAN_POINT('Ctrl Pts',(5.58284005859138,12.2,9.75344431695061));
#215291=CARTESIAN_POINT('Ctrl Pts',(5.58324153406708,12.2,9.75688409073694));
#215292=CARTESIAN_POINT('Ctrl Pts',(5.58363978044788,12.2,9.76033146532468));
#215293=CARTESIAN_POINT('Ctrl Pts',(5.58403802682868,12.2,9.76377883991242));
#215294=CARTESIAN_POINT('Ctrl Pts',(5.58443304351169,12.2,9.76723381760528));
#215295=CARTESIAN_POINT('Ctrl Pts',(5.58482479795623,12.2,9.7706963625201));
#215296=CARTESIAN_POINT('Ctrl Pts',(5.58521655247194,12.2,9.77415890806395));
#215297=CARTESIAN_POINT('Ctrl Pts',(5.5856050453284,12.2,9.77762902376828));
#215298=CARTESIAN_POINT('Ctrl Pts',(5.58599024430061,12.2,9.78110667577474));
#215299=CARTESIAN_POINT('Ctrl Pts',(5.58637544320283,12.2,9.78458432714942));
#215300=CARTESIAN_POINT('Ctrl Pts',(5.58675734805522,12.2,9.78806951627366));
#215301=CARTESIAN_POINT('Ctrl Pts',(5.58713592879118,12.2,9.79156221014743));
#215302=CARTESIAN_POINT('Ctrl Pts',(5.58764070308286,12.2,9.79621913510096));
#215303=CARTESIAN_POINT('Ctrl Pts',(5.58813956426023,12.2,9.80088940296212));
#215304=CARTESIAN_POINT('Ctrl Pts',(5.58863244091175,12.2,9.80557293931206));
#215305=CARTESIAN_POINT('Ctrl Pts',(5.58900209841717,12.2,9.80908559173404));
#215306=CARTESIAN_POINT('Ctrl Pts',(5.58936838920025,12.2,9.81260570737679));
#215307=CARTESIAN_POINT('Ctrl Pts',(5.58973128210419,12.2,9.8161332537476));
#215308=CARTESIAN_POINT('Ctrl Pts',(5.59009417507406,12.2,9.81966080075924));
#215309=CARTESIAN_POINT('Ctrl Pts',(5.59045366989297,12.2,9.82319577995633));
#215310=CARTESIAN_POINT('Ctrl Pts',(5.59080973681925,12.2,9.82673815847218));
#215311=CARTESIAN_POINT('Ctrl Pts',(5.59116580368086,12.2,9.83028053634449));
#215312=CARTESIAN_POINT('Ctrl Pts',(5.59151844210096,12.2,9.83383031509972));
#215313=CARTESIAN_POINT('Ctrl Pts',(5.59186762154631,12.2,9.8373874613878));
#215314=CARTESIAN_POINT('Ctrl Pts',(5.59221680099165,12.2,9.84094460767589));
#215315=CARTESIAN_POINT('Ctrl Pts',(5.59256252184574,12.2,9.84450912229638));
#215316=CARTESIAN_POINT('Ctrl Pts',(5.59290475370831,12.2,9.84808097454161));
#215317=CARTESIAN_POINT('Ctrl Pts',(5.59324698557087,12.2,9.85165282678683));
#215318=CARTESIAN_POINT('Ctrl Pts',(5.59358572742524,12.2,9.85523201584012));
#215319=CARTESIAN_POINT('Ctrl Pts',(5.5939209512467,12.2,9.85881851112579));
#215320=CARTESIAN_POINT('Ctrl Pts',(5.59425617506815,12.2,9.86240500641146));
#215321=CARTESIAN_POINT('Ctrl Pts',(5.59458787878156,12.2,9.86599880757176));
#215322=CARTESIAN_POINT('Ctrl Pts',(5.59491603466144,12.2,9.86959988357828));
#215323=CARTESIAN_POINT('Ctrl Pts',(5.59524419054132,12.2,9.87320095958478));
#215324=CARTESIAN_POINT('Ctrl Pts',(5.59556879660783,12.2,9.87680931036078));
#215325=CARTESIAN_POINT('Ctrl Pts',(5.59588982588831,12.2,9.88042490468673));
#215326=CARTESIAN_POINT('Ctrl Pts',(5.59631786496785,12.2,9.88524569755923));
#215327=CARTESIAN_POINT('Ctrl Pts',(5.59673954193012,12.2,9.89007936839968));
#215328=CARTESIAN_POINT('Ctrl Pts',(5.59715478800831,12.2,9.89492584327494));
#215329=CARTESIAN_POINT('Ctrl Pts',(5.59746622253866,12.2,9.89856069910121));
#215330=CARTESIAN_POINT('Ctrl Pts',(5.59777404002748,12.2,9.9022027577855));
#215331=CARTESIAN_POINT('Ctrl Pts',(5.59807821143342,12.2,9.90585198806896));
#215332=CARTESIAN_POINT('Ctrl Pts',(5.59838238283935,12.2,9.90950121835242));
#215333=CARTESIAN_POINT('Ctrl Pts',(5.59868290762136,12.2,9.91315761960878));
#215334=CARTESIAN_POINT('Ctrl Pts',(5.59897975800084,12.2,9.91682116253287));
#215335=CARTESIAN_POINT('Ctrl Pts',(5.5992766083803,12.2,9.92048470545697));
#215336=CARTESIAN_POINT('Ctrl Pts',(5.59956978298021,12.2,9.92415538868278));
#215337=CARTESIAN_POINT('Ctrl Pts',(5.5998592544702,12.2,9.92783318242318));
#215338=CARTESIAN_POINT('Ctrl Pts',(5.60014872601277,12.2,9.9315109768317));
#215339=CARTESIAN_POINT('Ctrl Pts',(5.60043449417097,12.2,9.93519588088392));
#215340=CARTESIAN_POINT('Ctrl Pts',(5.60071653029478,12.2,9.93888786479647));
#215341=CARTESIAN_POINT('Ctrl Pts',(5.60109257837447,12.2,9.94381050889536));
#215342=CARTESIAN_POINT('Ctrl Pts',(5.60146199282447,12.2,9.94874573857864));
#215343=CARTESIAN_POINT('Ctrl Pts',(5.60182470796192,12.2,9.95369348406225));
#215344=CARTESIAN_POINT('Ctrl Pts',(5.60209674432737,12.2,9.95740429334348));
#215345=CARTESIAN_POINT('Ctrl Pts',(5.60236501149473,12.2,9.96112214152942));
#215346=CARTESIAN_POINT('Ctrl Pts',(5.6026294809571,12.2,9.964846997496));
#215347=CARTESIAN_POINT('Ctrl Pts',(5.60289395041948,12.2,9.96857185346258));
#215348=CARTESIAN_POINT('Ctrl Pts',(5.60315462186946,12.2,9.97230371693833));
#215349=CARTESIAN_POINT('Ctrl Pts',(5.60341146744397,12.2,9.97604255817653));
#215350=CARTESIAN_POINT('Ctrl Pts',(5.60366831306516,12.2,9.97978140009396));
#215351=CARTESIAN_POINT('Ctrl Pts',(5.6039213345186,12.2,9.9835272181217));
#215352=CARTESIAN_POINT('Ctrl Pts',(5.60417050609595,12.2,9.98727998854306));
#215353=CARTESIAN_POINT('Ctrl Pts',(5.60441967762805,12.2,9.99103275828267));
#215354=CARTESIAN_POINT('Ctrl Pts',(5.604664999652,12.2,9.99479247918021));
#215355=CARTESIAN_POINT('Ctrl Pts',(5.60490644497622,12.2,9.99855911841896));
#215356=CARTESIAN_POINT('Ctrl Pts',(5.60514789030045,12.2,10.0023257576577));
#215357=CARTESIAN_POINT('Ctrl Pts',(5.6053854563743,12.2,10.0060993155569));
#215358=CARTESIAN_POINT('Ctrl Pts',(5.60561911124185,12.2,10.0098797562284));
#215359=CARTESIAN_POINT('Ctrl Pts',(5.60585276610941,12.2,10.0136601968999));
#215360=CARTESIAN_POINT('Ctrl Pts',(5.60608250774026,12.2,10.0174475182505));
#215361=CARTESIAN_POINT('Ctrl Pts',(5.6063083134831,12.2,10.0212416932965));
#215362=CARTESIAN_POINT('Ctrl Pts',(5.6066846564015,12.2,10.0275653186029));
#215363=CARTESIAN_POINT('Ctrl Pts',(5.60705005458934,12.2,10.0339079736131));
#215364=CARTESIAN_POINT('Ctrl Pts',(5.60740451299995,12.2,10.04026965));
#215365=CARTESIAN_POINT('Ctrl Pts',(5.26939701799994,15.2,10.221714878));
#215366=CARTESIAN_POINT('Ctrl Pts',(5.26939701799994,11.6,10.221714878));
#215367=CARTESIAN_POINT('Ctrl Pts',(5.26878426899994,15.2,10.221257575));
#215368=CARTESIAN_POINT('Ctrl Pts',(5.26878426899994,11.6,10.221257575));
#215369=CARTESIAN_POINT('Ctrl Pts',(5.26755929399994,15.2,10.220343));
#215370=CARTESIAN_POINT('Ctrl Pts',(5.26755929399994,11.6,10.220343));
#215371=CARTESIAN_POINT('Ctrl Pts',(5.26572340899994,15.2,10.218971238));
#215372=CARTESIAN_POINT('Ctrl Pts',(5.26572340899994,11.6,10.218971238));
#215373=CARTESIAN_POINT('Ctrl Pts',(5.26327871499994,15.2,10.217142421));
#215374=CARTESIAN_POINT('Ctrl Pts',(5.26327871499994,11.6,10.217142421));
#215375=CARTESIAN_POINT('Ctrl Pts',(5.26022810499994,15.2,10.214856731));
#215376=CARTESIAN_POINT('Ctrl Pts',(5.26022810499994,11.6,10.214856731));
#215377=CARTESIAN_POINT('Ctrl Pts',(5.25718275199995,15.2,10.212571374));
#215378=CARTESIAN_POINT('Ctrl Pts',(5.25718275199995,11.6,10.212571374));
#215379=CARTESIAN_POINT('Ctrl Pts',(5.25414265599994,15.2,10.210286353));
#215380=CARTESIAN_POINT('Ctrl Pts',(5.25414265599994,11.6,10.210286353));
#215381=CARTESIAN_POINT('Ctrl Pts',(5.25110781899994,15.2,10.208001669));
#215382=CARTESIAN_POINT('Ctrl Pts',(5.25110781899994,11.6,10.208001669));
#215383=CARTESIAN_POINT('Ctrl Pts',(5.24807824099994,15.2,10.205717331));
#215384=CARTESIAN_POINT('Ctrl Pts',(5.24807824099994,11.6,10.205717331));
#215385=CARTESIAN_POINT('Ctrl Pts',(5.24505392599994,15.2,10.203433344));
#215386=CARTESIAN_POINT('Ctrl Pts',(5.24505392599994,11.6,10.203433344));
#215387=CARTESIAN_POINT('Ctrl Pts',(5.24203487699994,15.2,10.20114972));
#215388=CARTESIAN_POINT('Ctrl Pts',(5.24203487699994,11.6,10.20114972));
#215389=CARTESIAN_POINT('Ctrl Pts',(5.23902109399994,15.2,10.198866469));
#215390=CARTESIAN_POINT('Ctrl Pts',(5.23902109399994,11.6,10.198866469));
#215391=CARTESIAN_POINT('Ctrl Pts',(5.23601258199994,15.2,10.1965836));
#215392=CARTESIAN_POINT('Ctrl Pts',(5.23601258199994,11.6,10.1965836));
#215393=CARTESIAN_POINT('Ctrl Pts',(5.23300934399994,15.2,10.194301126));
#215394=CARTESIAN_POINT('Ctrl Pts',(5.23300934399994,11.6,10.194301126));
#215395=CARTESIAN_POINT('Ctrl Pts',(5.23001137999994,15.2,10.192019056));
#215396=CARTESIAN_POINT('Ctrl Pts',(5.23001137999994,11.6,10.192019056));
#215397=CARTESIAN_POINT('Ctrl Pts',(5.22701869399994,15.2,10.189737398));
#215398=CARTESIAN_POINT('Ctrl Pts',(5.22701869399994,11.6,10.189737398));
#215399=CARTESIAN_POINT('Ctrl Pts',(5.22403128899994,15.2,10.187456163));
#215400=CARTESIAN_POINT('Ctrl Pts',(5.22403128899994,11.6,10.187456163));
#215401=CARTESIAN_POINT('Ctrl Pts',(5.22104916599995,15.2,10.185175356));
#215402=CARTESIAN_POINT('Ctrl Pts',(5.22104916599995,11.6,10.185175356));
#215403=CARTESIAN_POINT('Ctrl Pts',(5.21807232699994,15.2,10.182894988));
#215404=CARTESIAN_POINT('Ctrl Pts',(5.21807232699994,11.6,10.182894988));
#215405=CARTESIAN_POINT('Ctrl Pts',(5.21510077399994,15.2,10.180615065));
#215406=CARTESIAN_POINT('Ctrl Pts',(5.21510077399994,11.6,10.180615065));
#215407=CARTESIAN_POINT('Ctrl Pts',(5.21213450999994,15.2,10.178335595));
#215408=CARTESIAN_POINT('Ctrl Pts',(5.21213450999994,11.6,10.178335595));
#215409=CARTESIAN_POINT('Ctrl Pts',(5.20917353599994,15.2,10.176056588));
#215410=CARTESIAN_POINT('Ctrl Pts',(5.20917353599994,11.6,10.176056588));
#215411=CARTESIAN_POINT('Ctrl Pts',(5.20621785499994,15.2,10.173778052));
#215412=CARTESIAN_POINT('Ctrl Pts',(5.20621785499994,11.6,10.173778052));
#215413=CARTESIAN_POINT('Ctrl Pts',(5.20326746799994,15.2,10.171499997));
#215414=CARTESIAN_POINT('Ctrl Pts',(5.20326746799994,11.6,10.171499997));
#215415=CARTESIAN_POINT('Ctrl Pts',(5.20032237999994,15.2,10.169222432));
#215416=CARTESIAN_POINT('Ctrl Pts',(5.20032237999994,11.6,10.169222432));
#215417=CARTESIAN_POINT('Ctrl Pts',(5.19738259199994,15.2,10.166945366));
#215418=CARTESIAN_POINT('Ctrl Pts',(5.19738259199994,11.6,10.166945366));
#215419=CARTESIAN_POINT('Ctrl Pts',(5.19444810399994,15.2,10.164668808));
#215420=CARTESIAN_POINT('Ctrl Pts',(5.19444810399994,11.6,10.164668808));
#215421=CARTESIAN_POINT('Ctrl Pts',(5.19151892099995,15.2,10.162392767));
#215422=CARTESIAN_POINT('Ctrl Pts',(5.19151892099995,11.6,10.162392767));
#215423=CARTESIAN_POINT('Ctrl Pts',(5.18859504499994,15.2,10.160117253));
#215424=CARTESIAN_POINT('Ctrl Pts',(5.18859504499994,11.6,10.160117253));
#215425=CARTESIAN_POINT('Ctrl Pts',(5.18567647699994,15.2,10.157842273));
#215426=CARTESIAN_POINT('Ctrl Pts',(5.18567647699994,11.6,10.157842273));
#215427=CARTESIAN_POINT('Ctrl Pts',(5.18276321899994,15.2,10.155567837));
#215428=CARTESIAN_POINT('Ctrl Pts',(5.18276321899994,11.6,10.155567837));
#215429=CARTESIAN_POINT('Ctrl Pts',(5.17985527399994,15.2,10.153293953));
#215430=CARTESIAN_POINT('Ctrl Pts',(5.17985527399994,11.6,10.153293953));
#215431=CARTESIAN_POINT('Ctrl Pts',(5.17695264399994,15.2,10.151020631));
#215432=CARTESIAN_POINT('Ctrl Pts',(5.17695264399994,11.6,10.151020631));
#215433=CARTESIAN_POINT('Ctrl Pts',(5.17405533099994,15.2,10.14874788));
#215434=CARTESIAN_POINT('Ctrl Pts',(5.17405533099994,11.6,10.14874788));
#215435=CARTESIAN_POINT('Ctrl Pts',(5.17116333899994,15.2,10.146475708));
#215436=CARTESIAN_POINT('Ctrl Pts',(5.17116333899994,11.6,10.146475708));
#215437=CARTESIAN_POINT('Ctrl Pts',(5.16827666699994,15.2,10.144204125));
#215438=CARTESIAN_POINT('Ctrl Pts',(5.16827666699994,11.6,10.144204125));
#215439=CARTESIAN_POINT('Ctrl Pts',(5.16539531799994,15.2,10.141933139));
#215440=CARTESIAN_POINT('Ctrl Pts',(5.16539531799994,11.6,10.141933139));
#215441=CARTESIAN_POINT('Ctrl Pts',(5.16251929599994,15.2,10.139662761));
#215442=CARTESIAN_POINT('Ctrl Pts',(5.16251929599994,11.6,10.139662761));
#215443=CARTESIAN_POINT('Ctrl Pts',(5.15964860199994,15.2,10.137392999));
#215444=CARTESIAN_POINT('Ctrl Pts',(5.15964860199994,11.6,10.137392999));
#215445=CARTESIAN_POINT('Ctrl Pts',(5.15678323799994,15.2,10.135123862));
#215446=CARTESIAN_POINT('Ctrl Pts',(5.15678323799994,11.6,10.135123862));
#215447=CARTESIAN_POINT('Ctrl Pts',(5.15392320699994,15.2,10.132855359));
#215448=CARTESIAN_POINT('Ctrl Pts',(5.15392320699994,11.6,10.132855359));
#215449=CARTESIAN_POINT('Ctrl Pts',(5.15106850999994,15.2,10.130587501));
#215450=CARTESIAN_POINT('Ctrl Pts',(5.15106850999994,11.6,10.130587501));
#215451=CARTESIAN_POINT('Ctrl Pts',(5.14821914899994,15.2,10.128320294));
#215452=CARTESIAN_POINT('Ctrl Pts',(5.14821914899994,11.6,10.128320294));
#215453=CARTESIAN_POINT('Ctrl Pts',(5.14537512799994,15.2,10.12605375));
#215454=CARTESIAN_POINT('Ctrl Pts',(5.14537512799994,11.6,10.12605375));
#215455=CARTESIAN_POINT('Ctrl Pts',(5.14253644699994,15.2,10.123787877));
#215456=CARTESIAN_POINT('Ctrl Pts',(5.14253644699994,11.6,10.123787877));
#215457=CARTESIAN_POINT('Ctrl Pts',(5.13970310899994,15.2,10.121522684));
#215458=CARTESIAN_POINT('Ctrl Pts',(5.13970310899994,11.6,10.121522684));
#215459=CARTESIAN_POINT('Ctrl Pts',(5.13687511699994,15.2,10.119258181));
#215460=CARTESIAN_POINT('Ctrl Pts',(5.13687511699994,11.6,10.119258181));
#215461=CARTESIAN_POINT('Ctrl Pts',(5.13405247199994,15.2,10.116994376));
#215462=CARTESIAN_POINT('Ctrl Pts',(5.13405247199994,11.6,10.116994376));
#215463=CARTESIAN_POINT('Ctrl Pts',(5.13123517599994,15.2,10.114731281));
#215464=CARTESIAN_POINT('Ctrl Pts',(5.13123517599994,11.6,10.114731281));
#215465=CARTESIAN_POINT('Ctrl Pts',(5.12842323199994,15.2,10.112468902));
#215466=CARTESIAN_POINT('Ctrl Pts',(5.12842323199994,11.6,10.112468902));
#215467=CARTESIAN_POINT('Ctrl Pts',(5.12561664199994,15.2,10.11020725));
#215468=CARTESIAN_POINT('Ctrl Pts',(5.12561664199994,11.6,10.11020725));
#215469=CARTESIAN_POINT('Ctrl Pts',(5.12281540699994,15.2,10.107946335));
#215470=CARTESIAN_POINT('Ctrl Pts',(5.12281540699994,11.6,10.107946335));
#215471=CARTESIAN_POINT('Ctrl Pts',(5.12001953099994,15.2,10.105686165));
#215472=CARTESIAN_POINT('Ctrl Pts',(5.12001953099994,11.6,10.105686165));
#215473=CARTESIAN_POINT('Ctrl Pts',(5.11722901399994,15.2,10.103426751));
#215474=CARTESIAN_POINT('Ctrl Pts',(5.11722901399994,11.6,10.103426751));
#215475=CARTESIAN_POINT('Ctrl Pts',(5.11444385999994,15.2,10.101168101));
#215476=CARTESIAN_POINT('Ctrl Pts',(5.11444385999994,11.6,10.101168101));
#215477=CARTESIAN_POINT('Ctrl Pts',(5.11166406899994,15.2,10.098910224));
#215478=CARTESIAN_POINT('Ctrl Pts',(5.11166406899994,11.6,10.098910224));
#215479=CARTESIAN_POINT('Ctrl Pts',(5.10888964499994,15.2,10.09665313));
#215480=CARTESIAN_POINT('Ctrl Pts',(5.10888964499994,11.6,10.09665313));
#215481=CARTESIAN_POINT('Ctrl Pts',(5.10612058999994,15.2,10.094396829));
#215482=CARTESIAN_POINT('Ctrl Pts',(5.10612058999994,11.6,10.094396829));
#215483=CARTESIAN_POINT('Ctrl Pts',(5.10335690499994,15.2,10.092141331));
#215484=CARTESIAN_POINT('Ctrl Pts',(5.10335690499994,11.6,10.092141331));
#215485=CARTESIAN_POINT('Ctrl Pts',(5.10059859199994,15.2,10.089886644));
#215486=CARTESIAN_POINT('Ctrl Pts',(5.10059859199994,11.6,10.089886644));
#215487=CARTESIAN_POINT('Ctrl Pts',(5.09784565399994,15.2,10.087632778));
#215488=CARTESIAN_POINT('Ctrl Pts',(5.09784565399994,11.6,10.087632778));
#215489=CARTESIAN_POINT('Ctrl Pts',(5.09509809299994,15.2,10.085379743));
#215490=CARTESIAN_POINT('Ctrl Pts',(5.09509809299994,11.6,10.085379743));
#215491=CARTESIAN_POINT('Ctrl Pts',(5.09235591199994,15.2,10.083127549));
#215492=CARTESIAN_POINT('Ctrl Pts',(5.09235591199994,11.6,10.083127549));
#215493=CARTESIAN_POINT('Ctrl Pts',(5.08961910999994,15.2,10.080876204));
#215494=CARTESIAN_POINT('Ctrl Pts',(5.08961910999994,11.6,10.080876204));
#215495=CARTESIAN_POINT('Ctrl Pts',(5.08688769099994,15.2,10.078625719));
#215496=CARTESIAN_POINT('Ctrl Pts',(5.08688769099994,11.6,10.078625719));
#215497=CARTESIAN_POINT('Ctrl Pts',(5.08416165799994,15.2,10.076376103));
#215498=CARTESIAN_POINT('Ctrl Pts',(5.08416165799994,11.6,10.076376103));
#215499=CARTESIAN_POINT('Ctrl Pts',(5.08144101099994,15.2,10.074127366));
#215500=CARTESIAN_POINT('Ctrl Pts',(5.08144101099994,11.6,10.074127366));
#215501=CARTESIAN_POINT('Ctrl Pts',(5.07872575399994,15.2,10.071879516));
#215502=CARTESIAN_POINT('Ctrl Pts',(5.07872575399994,11.6,10.071879516));
#215503=CARTESIAN_POINT('Ctrl Pts',(5.07601588799994,15.2,10.069632566));
#215504=CARTESIAN_POINT('Ctrl Pts',(5.07601588799994,11.6,10.069632566));
#215505=CARTESIAN_POINT('Ctrl Pts',(5.07331141499994,15.2,10.067386522));
#215506=CARTESIAN_POINT('Ctrl Pts',(5.07331141499994,11.6,10.067386522));
#215507=CARTESIAN_POINT('Ctrl Pts',(5.07061233699994,15.2,10.065141396));
#215508=CARTESIAN_POINT('Ctrl Pts',(5.07061233699994,11.6,10.065141396));
#215509=CARTESIAN_POINT('Ctrl Pts',(5.06791865699994,15.2,10.062897197));
#215510=CARTESIAN_POINT('Ctrl Pts',(5.06791865699994,11.6,10.062897197));
#215511=CARTESIAN_POINT('Ctrl Pts',(5.06523037499995,15.2,10.060653934));
#215512=CARTESIAN_POINT('Ctrl Pts',(5.06523037499995,11.6,10.060653934));
#215513=CARTESIAN_POINT('Ctrl Pts',(5.06254749499995,15.2,10.058411619));
#215514=CARTESIAN_POINT('Ctrl Pts',(5.06254749499995,11.6,10.058411619));
#215515=CARTESIAN_POINT('Ctrl Pts',(5.05987001799994,15.2,10.056170261));
#215516=CARTESIAN_POINT('Ctrl Pts',(5.05987001799994,11.6,10.056170261));
#215517=CARTESIAN_POINT('Ctrl Pts',(5.05719794699994,15.2,10.053929868));
#215518=CARTESIAN_POINT('Ctrl Pts',(5.05719794699994,11.6,10.053929868));
#215519=CARTESIAN_POINT('Ctrl Pts',(5.05453128299994,15.2,10.051690451));
#215520=CARTESIAN_POINT('Ctrl Pts',(5.05453128299994,11.6,10.051690451));
#215521=CARTESIAN_POINT('Ctrl Pts',(5.05187002799994,15.2,10.04945202));
#215522=CARTESIAN_POINT('Ctrl Pts',(5.05187002799994,11.6,10.04945202));
#215523=CARTESIAN_POINT('Ctrl Pts',(5.04921418499994,15.2,10.047214586));
#215524=CARTESIAN_POINT('Ctrl Pts',(5.04921418499994,11.6,10.047214586));
#215525=CARTESIAN_POINT('Ctrl Pts',(5.04656375499994,15.2,10.044978156));
#215526=CARTESIAN_POINT('Ctrl Pts',(5.04656375499994,11.6,10.044978156));
#215527=CARTESIAN_POINT('Ctrl Pts',(5.04391874099994,15.2,10.042742743));
#215528=CARTESIAN_POINT('Ctrl Pts',(5.04391874099994,11.6,10.042742743));
#215529=CARTESIAN_POINT('Ctrl Pts',(5.04127914399994,15.2,10.040508354));
#215530=CARTESIAN_POINT('Ctrl Pts',(5.04127914399994,11.6,10.040508354));
#215531=CARTESIAN_POINT('Ctrl Pts',(5.03864496599994,15.2,10.038275002));
#215532=CARTESIAN_POINT('Ctrl Pts',(5.03864496599994,11.6,10.038275002));
#215533=CARTESIAN_POINT('Ctrl Pts',(5.03601620899994,15.2,10.036042695));
#215534=CARTESIAN_POINT('Ctrl Pts',(5.03601620899994,11.6,10.036042695));
#215535=CARTESIAN_POINT('Ctrl Pts',(5.03339287499994,15.2,10.033811443));
#215536=CARTESIAN_POINT('Ctrl Pts',(5.03339287499994,11.6,10.033811443));
#215537=CARTESIAN_POINT('Ctrl Pts',(5.03077496799994,15.2,10.031581256));
#215538=CARTESIAN_POINT('Ctrl Pts',(5.03077496799994,11.6,10.031581256));
#215539=CARTESIAN_POINT('Ctrl Pts',(5.02816248699994,15.2,10.029352145));
#215540=CARTESIAN_POINT('Ctrl Pts',(5.02816248699994,11.6,10.029352145));
#215541=CARTESIAN_POINT('Ctrl Pts',(5.02555543499994,15.2,10.027124119));
#215542=CARTESIAN_POINT('Ctrl Pts',(5.02555543499994,11.6,10.027124119));
#215543=CARTESIAN_POINT('Ctrl Pts',(5.02295381499994,15.2,10.024897189));
#215544=CARTESIAN_POINT('Ctrl Pts',(5.02295381499994,11.6,10.024897189));
#215545=CARTESIAN_POINT('Ctrl Pts',(5.02035762799994,15.2,10.022671365));
#215546=CARTESIAN_POINT('Ctrl Pts',(5.02035762799994,11.6,10.022671365));
#215547=CARTESIAN_POINT('Ctrl Pts',(5.01776687499994,15.2,10.020446656));
#215548=CARTESIAN_POINT('Ctrl Pts',(5.01776687499994,11.6,10.020446656));
#215549=CARTESIAN_POINT('Ctrl Pts',(5.01518155999994,15.2,10.018223073));
#215550=CARTESIAN_POINT('Ctrl Pts',(5.01518155999994,11.6,10.018223073));
#215551=CARTESIAN_POINT('Ctrl Pts',(5.01260168399994,15.2,10.016000626));
#215552=CARTESIAN_POINT('Ctrl Pts',(5.01260168399994,11.6,10.016000626));
#215553=CARTESIAN_POINT('Ctrl Pts',(5.01002724899994,15.2,10.013779325));
#215554=CARTESIAN_POINT('Ctrl Pts',(5.01002724899994,11.6,10.013779325));
#215555=CARTESIAN_POINT('Ctrl Pts',(5.00745825699994,15.2,10.011559181));
#215556=CARTESIAN_POINT('Ctrl Pts',(5.00745825699994,11.6,10.011559181));
#215557=CARTESIAN_POINT('Ctrl Pts',(5.00489470899994,15.2,10.009340204));
#215558=CARTESIAN_POINT('Ctrl Pts',(5.00489470899994,11.6,10.009340204));
#215559=CARTESIAN_POINT('Ctrl Pts',(5.00233660699994,15.2,10.007122403));
#215560=CARTESIAN_POINT('Ctrl Pts',(5.00233660699994,11.6,10.007122403));
#215561=CARTESIAN_POINT('Ctrl Pts',(4.99978395499994,15.2,10.00490579));
#215562=CARTESIAN_POINT('Ctrl Pts',(4.99978395499994,11.6,10.00490579));
#215563=CARTESIAN_POINT('Ctrl Pts',(4.99723675399994,15.2,10.002690374));
#215564=CARTESIAN_POINT('Ctrl Pts',(4.99723675399994,11.6,10.002690374));
#215565=CARTESIAN_POINT('Ctrl Pts',(4.99469500299994,15.2,10.000476165));
#215566=CARTESIAN_POINT('Ctrl Pts',(4.99469500299994,11.6,10.000476165));
#215567=CARTESIAN_POINT('Ctrl Pts',(4.99215870799994,15.2,9.99826317399998));
#215568=CARTESIAN_POINT('Ctrl Pts',(4.99215870799994,11.6,9.99826317399998));
#215569=CARTESIAN_POINT('Ctrl Pts',(4.98962786999994,15.2,9.99605141199999));
#215570=CARTESIAN_POINT('Ctrl Pts',(4.98962786999994,11.6,9.99605141199999));
#215571=CARTESIAN_POINT('Ctrl Pts',(4.98710248999994,15.2,9.99384088899999));
#215572=CARTESIAN_POINT('Ctrl Pts',(4.98710248999994,11.6,9.99384088899999));
#215573=CARTESIAN_POINT('Ctrl Pts',(4.98458256799994,15.2,9.99163161499999));
#215574=CARTESIAN_POINT('Ctrl Pts',(4.98458256799994,11.6,9.99163161499999));
#215575=CARTESIAN_POINT('Ctrl Pts',(4.98206810999994,15.2,9.98942359999998));
#215576=CARTESIAN_POINT('Ctrl Pts',(4.98206810999994,11.6,9.98942359999998));
#215577=CARTESIAN_POINT('Ctrl Pts',(4.97955911499994,15.2,9.98721685499999));
#215578=CARTESIAN_POINT('Ctrl Pts',(4.97955911499994,11.6,9.98721685499999));
#215579=CARTESIAN_POINT('Ctrl Pts',(4.97705558599994,15.2,9.98501139099999));
#215580=CARTESIAN_POINT('Ctrl Pts',(4.97705558599994,11.6,9.98501139099999));
#215581=CARTESIAN_POINT('Ctrl Pts',(4.97455752499994,15.2,9.98280721799999));
#215582=CARTESIAN_POINT('Ctrl Pts',(4.97455752499994,11.6,9.98280721799999));
#215583=CARTESIAN_POINT('Ctrl Pts',(4.97206493199994,15.2,9.98060434499998));
#215584=CARTESIAN_POINT('Ctrl Pts',(4.97206493199994,11.6,9.98060434499998));
#215585=CARTESIAN_POINT('Ctrl Pts',(4.96957781099994,15.2,9.97840278399998));
#215586=CARTESIAN_POINT('Ctrl Pts',(4.96957781099994,11.6,9.97840278399998));
#215587=CARTESIAN_POINT('Ctrl Pts',(4.96709616399994,15.2,9.97620254699999));
#215588=CARTESIAN_POINT('Ctrl Pts',(4.96709616399994,11.6,9.97620254699999));
#215589=CARTESIAN_POINT('Ctrl Pts',(4.96461999099994,15.2,9.97400364199999));
#215590=CARTESIAN_POINT('Ctrl Pts',(4.96461999099994,11.6,9.97400364199999));
#215591=CARTESIAN_POINT('Ctrl Pts',(4.96214929499994,15.2,9.97180608099999));
#215592=CARTESIAN_POINT('Ctrl Pts',(4.96214929499994,11.6,9.97180608099999));
#215593=CARTESIAN_POINT('Ctrl Pts',(4.95968407799994,15.2,9.96960987399999));
#215594=CARTESIAN_POINT('Ctrl Pts',(4.95968407799994,11.6,9.96960987399999));
#215595=CARTESIAN_POINT('Ctrl Pts',(4.95722434099994,15.2,9.96741503199999));
#215596=CARTESIAN_POINT('Ctrl Pts',(4.95722434099994,11.6,9.96741503199999));
#215597=CARTESIAN_POINT('Ctrl Pts',(4.95477008699994,15.2,9.96522156599998));
#215598=CARTESIAN_POINT('Ctrl Pts',(4.95477008699994,11.6,9.96522156599998));
#215599=CARTESIAN_POINT('Ctrl Pts',(4.95232131799995,15.2,9.96302948599999));
#215600=CARTESIAN_POINT('Ctrl Pts',(4.95232131799995,11.6,9.96302948599999));
#215601=CARTESIAN_POINT('Ctrl Pts',(4.94987803399994,15.2,9.96083880199999));
#215602=CARTESIAN_POINT('Ctrl Pts',(4.94987803399994,11.6,9.96083880199999));
#215603=CARTESIAN_POINT('Ctrl Pts',(4.94744023799994,15.2,9.95864952599998));
#215604=CARTESIAN_POINT('Ctrl Pts',(4.94744023799994,11.6,9.95864952599998));
#215605=CARTESIAN_POINT('Ctrl Pts',(4.94500793199994,15.2,9.95646166799999));
#215606=CARTESIAN_POINT('Ctrl Pts',(4.94500793199994,11.6,9.95646166799999));
#215607=CARTESIAN_POINT('Ctrl Pts',(4.94258111699994,15.2,9.95427523999999));
#215608=CARTESIAN_POINT('Ctrl Pts',(4.94258111699994,11.6,9.95427523999999));
#215609=CARTESIAN_POINT('Ctrl Pts',(4.94015979599994,15.2,9.95209025199999));
#215610=CARTESIAN_POINT('Ctrl Pts',(4.94015979599994,11.6,9.95209025199999));
#215611=CARTESIAN_POINT('Ctrl Pts',(4.93774396999994,15.2,9.94990671399999));
#215612=CARTESIAN_POINT('Ctrl Pts',(4.93774396999994,11.6,9.94990671399999));
#215613=CARTESIAN_POINT('Ctrl Pts',(4.93533364099994,15.2,9.94772463799999));
#215614=CARTESIAN_POINT('Ctrl Pts',(4.93533364099994,11.6,9.94772463799999));
#215615=CARTESIAN_POINT('Ctrl Pts',(4.93292880999994,15.2,9.94554403399999));
#215616=CARTESIAN_POINT('Ctrl Pts',(4.93292880999994,11.6,9.94554403399999));
#215617=CARTESIAN_POINT('Ctrl Pts',(4.93052947999994,15.2,9.94336491299999));
#215618=CARTESIAN_POINT('Ctrl Pts',(4.93052947999994,11.6,9.94336491299999));
#215619=CARTESIAN_POINT('Ctrl Pts',(4.92813565299994,15.2,9.94118728699998));
#215620=CARTESIAN_POINT('Ctrl Pts',(4.92813565299994,11.6,9.94118728699998));
#215621=CARTESIAN_POINT('Ctrl Pts',(4.92574732899994,15.2,9.93901116599999));
#215622=CARTESIAN_POINT('Ctrl Pts',(4.92574732899994,11.6,9.93901116599999));
#215623=CARTESIAN_POINT('Ctrl Pts',(4.92336451099994,15.2,9.93683656199998));
#215624=CARTESIAN_POINT('Ctrl Pts',(4.92336451099994,11.6,9.93683656199998));
#215625=CARTESIAN_POINT('Ctrl Pts',(4.92098720099994,15.2,9.93466348399998));
#215626=CARTESIAN_POINT('Ctrl Pts',(4.92098720099994,11.6,9.93466348399998));
#215627=CARTESIAN_POINT('Ctrl Pts',(4.91861540099994,15.2,9.93249194499998));
#215628=CARTESIAN_POINT('Ctrl Pts',(4.91861540099994,11.6,9.93249194499998));
#215629=CARTESIAN_POINT('Ctrl Pts',(4.91624911099994,15.2,9.93032195499998));
#215630=CARTESIAN_POINT('Ctrl Pts',(4.91624911099994,11.6,9.93032195499998));
#215631=CARTESIAN_POINT('Ctrl Pts',(4.91388833399994,15.2,9.92815352399998));
#215632=CARTESIAN_POINT('Ctrl Pts',(4.91388833399994,11.6,9.92815352399998));
#215633=CARTESIAN_POINT('Ctrl Pts',(4.91153307199994,15.2,9.92598666599999));
#215634=CARTESIAN_POINT('Ctrl Pts',(4.91153307199994,11.6,9.92598666599999));
#215635=CARTESIAN_POINT('Ctrl Pts',(4.90918332699994,15.2,9.92382138899998));
#215636=CARTESIAN_POINT('Ctrl Pts',(4.90918332699994,11.6,9.92382138899998));
#215637=CARTESIAN_POINT('Ctrl Pts',(4.90683909899994,15.2,9.92165770599998));
#215638=CARTESIAN_POINT('Ctrl Pts',(4.90683909899994,11.6,9.92165770599998));
#215639=CARTESIAN_POINT('Ctrl Pts',(4.90450039099994,15.2,9.91949562899999));
#215640=CARTESIAN_POINT('Ctrl Pts',(4.90450039099994,11.6,9.91949562899999));
#215641=CARTESIAN_POINT('Ctrl Pts',(4.90216720599994,15.2,9.91733516599999));
#215642=CARTESIAN_POINT('Ctrl Pts',(4.90216720599994,11.6,9.91733516599999));
#215643=CARTESIAN_POINT('Ctrl Pts',(4.89983954199994,15.2,9.91517633099999));
#215644=CARTESIAN_POINT('Ctrl Pts',(4.89983954199994,11.6,9.91517633099999));
#215645=CARTESIAN_POINT('Ctrl Pts',(4.89751740499994,15.2,9.91301913399998));
#215646=CARTESIAN_POINT('Ctrl Pts',(4.89751740499994,11.6,9.91301913399998));
#215647=CARTESIAN_POINT('Ctrl Pts',(4.89520079399994,15.2,9.91086358699998));
#215648=CARTESIAN_POINT('Ctrl Pts',(4.89520079399994,11.6,9.91086358699998));
#215649=CARTESIAN_POINT('Ctrl Pts',(4.89288971099994,15.2,9.90870969999998));
#215650=CARTESIAN_POINT('Ctrl Pts',(4.89288971099994,11.6,9.90870969999998));
#215651=CARTESIAN_POINT('Ctrl Pts',(4.89058415899994,15.2,9.90655748699999));
#215652=CARTESIAN_POINT('Ctrl Pts',(4.89058415899994,11.6,9.90655748699999));
#215653=CARTESIAN_POINT('Ctrl Pts',(4.88828413899994,15.2,9.90440695499998));
#215654=CARTESIAN_POINT('Ctrl Pts',(4.88828413899994,11.6,9.90440695499998));
#215655=CARTESIAN_POINT('Ctrl Pts',(4.88598965099994,15.2,9.90225811999998));
#215656=CARTESIAN_POINT('Ctrl Pts',(4.88598965099994,11.6,9.90225811999998));
#215657=CARTESIAN_POINT('Ctrl Pts',(4.88370069999994,15.2,9.90011098999998));
#215658=CARTESIAN_POINT('Ctrl Pts',(4.88370069999994,11.6,9.90011098999998));
#215659=CARTESIAN_POINT('Ctrl Pts',(4.88141728599994,15.2,9.89796557799998));
#215660=CARTESIAN_POINT('Ctrl Pts',(4.88141728599994,11.6,9.89796557799998));
#215661=CARTESIAN_POINT('Ctrl Pts',(4.87913940899994,15.2,9.89582189499998));
#215662=CARTESIAN_POINT('Ctrl Pts',(4.87913940899994,11.6,9.89582189499998));
#215663=CARTESIAN_POINT('Ctrl Pts',(4.87686707299994,15.2,9.89367995299999));
#215664=CARTESIAN_POINT('Ctrl Pts',(4.87686707299994,11.6,9.89367995299999));
#215665=CARTESIAN_POINT('Ctrl Pts',(4.87460027899994,15.2,9.89153976199999));
#215666=CARTESIAN_POINT('Ctrl Pts',(4.87460027899994,11.6,9.89153976199999));
#215667=CARTESIAN_POINT('Ctrl Pts',(4.87233902799994,15.2,9.88940133499998));
#215668=CARTESIAN_POINT('Ctrl Pts',(4.87233902799994,11.6,9.88940133499998));
#215669=CARTESIAN_POINT('Ctrl Pts',(4.87008332399994,15.2,9.88726468299999));
#215670=CARTESIAN_POINT('Ctrl Pts',(4.87008332399994,11.6,9.88726468299999));
#215671=CARTESIAN_POINT('Ctrl Pts',(4.86783316499994,15.2,9.88512981799998));
#215672=CARTESIAN_POINT('Ctrl Pts',(4.86783316499994,11.6,9.88512981799998));
#215673=CARTESIAN_POINT('Ctrl Pts',(4.86558855599994,15.2,9.88299675099999));
#215674=CARTESIAN_POINT('Ctrl Pts',(4.86558855599994,11.6,9.88299675099999));
#215675=CARTESIAN_POINT('Ctrl Pts',(4.86334949599994,15.2,9.88086549299998));
#215676=CARTESIAN_POINT('Ctrl Pts',(4.86334949599994,11.6,9.88086549299998));
#215677=CARTESIAN_POINT('Ctrl Pts',(4.86111598899994,15.2,9.87873605699999));
#215678=CARTESIAN_POINT('Ctrl Pts',(4.86111598899994,11.6,9.87873605699999));
#215679=CARTESIAN_POINT('Ctrl Pts',(4.85888803499994,15.2,9.87660845499999));
#215680=CARTESIAN_POINT('Ctrl Pts',(4.85888803499994,11.6,9.87660845499999));
#215681=CARTESIAN_POINT('Ctrl Pts',(4.85666563599994,15.2,9.87448269699998));
#215682=CARTESIAN_POINT('Ctrl Pts',(4.85666563599994,11.6,9.87448269699998));
#215683=CARTESIAN_POINT('Ctrl Pts',(4.85444879299994,15.2,9.87235879599999));
#215684=CARTESIAN_POINT('Ctrl Pts',(4.85444879299994,11.6,9.87235879599999));
#215685=CARTESIAN_POINT('Ctrl Pts',(4.85223750899994,15.2,9.87023676299999));
#215686=CARTESIAN_POINT('Ctrl Pts',(4.85223750899994,11.6,9.87023676299999));
#215687=CARTESIAN_POINT('Ctrl Pts',(4.85003178499994,15.2,9.86811660999999));
#215688=CARTESIAN_POINT('Ctrl Pts',(4.85003178499994,11.6,9.86811660999999));
#215689=CARTESIAN_POINT('Ctrl Pts',(4.84783162099994,15.2,9.86599834899998));
#215690=CARTESIAN_POINT('Ctrl Pts',(4.84783162099994,11.6,9.86599834899998));
#215691=CARTESIAN_POINT('Ctrl Pts',(4.84563702199994,15.2,9.86388199099999));
#215692=CARTESIAN_POINT('Ctrl Pts',(4.84563702199994,11.6,9.86388199099999));
#215693=CARTESIAN_POINT('Ctrl Pts',(4.84344798699994,15.2,9.86176754899999));
#215694=CARTESIAN_POINT('Ctrl Pts',(4.84344798699994,11.6,9.86176754899999));
#215695=CARTESIAN_POINT('Ctrl Pts',(4.84126451799994,15.2,9.85965503499998));
#215696=CARTESIAN_POINT('Ctrl Pts',(4.84126451799994,11.6,9.85965503499998));
#215697=CARTESIAN_POINT('Ctrl Pts',(4.83908661699994,15.2,9.85754446099998));
#215698=CARTESIAN_POINT('Ctrl Pts',(4.83908661699994,11.6,9.85754446099998));
#215699=CARTESIAN_POINT('Ctrl Pts',(4.83691428499994,15.2,9.85543583699998));
#215700=CARTESIAN_POINT('Ctrl Pts',(4.83691428499994,11.6,9.85543583699998));
#215701=CARTESIAN_POINT('Ctrl Pts',(4.83474752499994,15.2,9.85332917699999));
#215702=CARTESIAN_POINT('Ctrl Pts',(4.83474752499994,11.6,9.85332917699999));
#215703=CARTESIAN_POINT('Ctrl Pts',(4.83258633699994,15.2,9.85122449099999));
#215704=CARTESIAN_POINT('Ctrl Pts',(4.83258633699994,11.6,9.85122449099999));
#215705=CARTESIAN_POINT('Ctrl Pts',(4.83043072399994,15.2,9.84912179399998));
#215706=CARTESIAN_POINT('Ctrl Pts',(4.83043072399994,11.6,9.84912179399998));
#215707=CARTESIAN_POINT('Ctrl Pts',(4.82828068499994,15.2,9.84702109599999));
#215708=CARTESIAN_POINT('Ctrl Pts',(4.82828068499994,11.6,9.84702109599999));
#215709=CARTESIAN_POINT('Ctrl Pts',(4.82613622399994,15.2,9.84492240899998));
#215710=CARTESIAN_POINT('Ctrl Pts',(4.82613622399994,11.6,9.84492240899998));
#215711=CARTESIAN_POINT('Ctrl Pts',(4.82399734199994,15.2,9.84282574499998));
#215712=CARTESIAN_POINT('Ctrl Pts',(4.82399734199994,11.6,9.84282574499998));
#215713=CARTESIAN_POINT('Ctrl Pts',(4.82186403999994,15.2,9.84073111799999));
#215714=CARTESIAN_POINT('Ctrl Pts',(4.82186403999994,11.6,9.84073111799999));
#215715=CARTESIAN_POINT('Ctrl Pts',(4.81973631899994,15.2,9.83863853799999));
#215716=CARTESIAN_POINT('Ctrl Pts',(4.81973631899994,11.6,9.83863853799999));
#215717=CARTESIAN_POINT('Ctrl Pts',(4.81761418199994,15.2,9.83654801799998));
#215718=CARTESIAN_POINT('Ctrl Pts',(4.81761418199994,11.6,9.83654801799998));
#215719=CARTESIAN_POINT('Ctrl Pts',(4.81549763099994,15.2,9.83445957099999));
#215720=CARTESIAN_POINT('Ctrl Pts',(4.81549763099994,11.6,9.83445957099999));
#215721=CARTESIAN_POINT('Ctrl Pts',(4.81338666499994,15.2,9.83237320799999));
#215722=CARTESIAN_POINT('Ctrl Pts',(4.81338666499994,11.6,9.83237320799999));
#215723=CARTESIAN_POINT('Ctrl Pts',(4.81128128599994,15.2,9.83028894199999));
#215724=CARTESIAN_POINT('Ctrl Pts',(4.81128128599994,11.6,9.83028894199999));
#215725=CARTESIAN_POINT('Ctrl Pts',(4.80918149799994,15.2,9.82820678499999));
#215726=CARTESIAN_POINT('Ctrl Pts',(4.80918149799994,11.6,9.82820678499999));
#215727=CARTESIAN_POINT('Ctrl Pts',(4.80708729999994,15.2,9.82612674999999));
#215728=CARTESIAN_POINT('Ctrl Pts',(4.80708729999994,11.6,9.82612674999999));
#215729=CARTESIAN_POINT('Ctrl Pts',(4.80499869399994,15.2,9.82404884799998));
#215730=CARTESIAN_POINT('Ctrl Pts',(4.80499869399994,11.6,9.82404884799998));
#215731=CARTESIAN_POINT('Ctrl Pts',(4.80291568299994,15.2,9.82197309199999));
#215732=CARTESIAN_POINT('Ctrl Pts',(4.80291568299994,11.6,9.82197309199999));
#215733=CARTESIAN_POINT('Ctrl Pts',(4.80083826599994,15.2,9.81989949599999));
#215734=CARTESIAN_POINT('Ctrl Pts',(4.80083826599994,11.6,9.81989949599999));
#215735=CARTESIAN_POINT('Ctrl Pts',(4.79876644599994,15.2,9.81782807099999));
#215736=CARTESIAN_POINT('Ctrl Pts',(4.79876644599994,11.6,9.81782807099999));
#215737=CARTESIAN_POINT('Ctrl Pts',(4.79670022499994,15.2,9.81575882899998));
#215738=CARTESIAN_POINT('Ctrl Pts',(4.79670022499994,11.6,9.81575882899998));
#215739=CARTESIAN_POINT('Ctrl Pts',(4.79463960199994,15.2,9.81369178299998));
#215740=CARTESIAN_POINT('Ctrl Pts',(4.79463960199994,11.6,9.81369178299998));
#215741=CARTESIAN_POINT('Ctrl Pts',(4.79258458199994,15.2,9.81162694599998));
#215742=CARTESIAN_POINT('Ctrl Pts',(4.79258458199994,11.6,9.81162694599998));
#215743=CARTESIAN_POINT('Ctrl Pts',(4.79053516299994,15.2,9.80956433099998));
#215744=CARTESIAN_POINT('Ctrl Pts',(4.79053516299994,11.6,9.80956433099998));
#215745=CARTESIAN_POINT('Ctrl Pts',(4.78849134899994,15.2,9.80750394899999));
#215746=CARTESIAN_POINT('Ctrl Pts',(4.78849134899994,11.6,9.80750394899999));
#215747=CARTESIAN_POINT('Ctrl Pts',(4.78645313999994,15.2,9.80544581399998));
#215748=CARTESIAN_POINT('Ctrl Pts',(4.78645313999994,11.6,9.80544581399998));
#215749=CARTESIAN_POINT('Ctrl Pts',(4.78442053799994,15.2,9.80338993799998));
#215750=CARTESIAN_POINT('Ctrl Pts',(4.78442053799994,11.6,9.80338993799998));
#215751=CARTESIAN_POINT('Ctrl Pts',(4.78239354399994,15.2,9.80133633399999));
#215752=CARTESIAN_POINT('Ctrl Pts',(4.78239354399994,11.6,9.80133633399999));
#215753=CARTESIAN_POINT('Ctrl Pts',(4.78037215899994,15.2,9.79928501499998));
#215754=CARTESIAN_POINT('Ctrl Pts',(4.78037215899994,11.6,9.79928501499998));
#215755=CARTESIAN_POINT('Ctrl Pts',(4.77835638599994,15.2,9.79723599399998));
#215756=CARTESIAN_POINT('Ctrl Pts',(4.77835638599994,11.6,9.79723599399998));
#215757=CARTESIAN_POINT('Ctrl Pts',(4.77634622499994,15.2,9.79518928099999));
#215758=CARTESIAN_POINT('Ctrl Pts',(4.77634622499994,11.6,9.79518928099999));
#215759=CARTESIAN_POINT('Ctrl Pts',(4.77434167799994,15.2,9.79314489299998));
#215760=CARTESIAN_POINT('Ctrl Pts',(4.77434167799994,11.6,9.79314489299998));
#215761=CARTESIAN_POINT('Ctrl Pts',(4.77234274699994,15.2,9.79110284099999));
#215762=CARTESIAN_POINT('Ctrl Pts',(4.77234274699994,11.6,9.79110284099999));
#215763=CARTESIAN_POINT('Ctrl Pts',(4.77034943099994,15.2,9.78906313699999));
#215764=CARTESIAN_POINT('Ctrl Pts',(4.77034943099994,11.6,9.78906313699999));
#215765=CARTESIAN_POINT('Ctrl Pts',(4.76836173399994,15.2,9.78702579499998));
#215766=CARTESIAN_POINT('Ctrl Pts',(4.76836173399994,11.6,9.78702579499998));
#215767=CARTESIAN_POINT('Ctrl Pts',(4.76637965599994,15.2,9.78499082799999));
#215768=CARTESIAN_POINT('Ctrl Pts',(4.76637965599994,11.6,9.78499082799999));
#215769=CARTESIAN_POINT('Ctrl Pts',(4.76440319899994,15.2,9.78295824899998));
#215770=CARTESIAN_POINT('Ctrl Pts',(4.76440319899994,11.6,9.78295824899998));
#215771=CARTESIAN_POINT('Ctrl Pts',(4.76243236299994,15.2,9.78092806999998));
#215772=CARTESIAN_POINT('Ctrl Pts',(4.76243236299994,11.6,9.78092806999998));
#215773=CARTESIAN_POINT('Ctrl Pts',(4.76046715199994,15.2,9.77890030499999));
#215774=CARTESIAN_POINT('Ctrl Pts',(4.76046715199994,11.6,9.77890030499999));
#215775=CARTESIAN_POINT('Ctrl Pts',(4.75850756399994,15.2,9.77687496799999));
#215776=CARTESIAN_POINT('Ctrl Pts',(4.75850756399994,11.6,9.77687496799999));
#215777=CARTESIAN_POINT('Ctrl Pts',(4.75655360399994,15.2,9.77485206899999));
#215778=CARTESIAN_POINT('Ctrl Pts',(4.75655360399994,11.6,9.77485206899999));
#215779=CARTESIAN_POINT('Ctrl Pts',(4.75460526999994,15.2,9.77283162499998));
#215780=CARTESIAN_POINT('Ctrl Pts',(4.75460526999994,11.6,9.77283162499998));
#215781=CARTESIAN_POINT('Ctrl Pts',(4.75266256599994,15.2,9.77081364599999));
#215782=CARTESIAN_POINT('Ctrl Pts',(4.75266256599994,11.6,9.77081364599999));
#215783=CARTESIAN_POINT('Ctrl Pts',(4.75072549099994,15.2,9.76879814799998));
#215784=CARTESIAN_POINT('Ctrl Pts',(4.75072549099994,11.6,9.76879814799998));
#215785=CARTESIAN_POINT('Ctrl Pts',(4.74879404699994,15.2,9.76678514099999));
#215786=CARTESIAN_POINT('Ctrl Pts',(4.74879404699994,11.6,9.76678514099999));
#215787=CARTESIAN_POINT('Ctrl Pts',(4.74686823599995,15.2,9.76477464199998));
#215788=CARTESIAN_POINT('Ctrl Pts',(4.74686823599995,11.6,9.76477464199998));
#215789=CARTESIAN_POINT('Ctrl Pts',(4.74494805999994,15.2,9.76276666099999));
#215790=CARTESIAN_POINT('Ctrl Pts',(4.74494805999994,11.6,9.76276666099999));
#215791=CARTESIAN_POINT('Ctrl Pts',(4.74303351799994,15.2,9.76076121399998));
#215792=CARTESIAN_POINT('Ctrl Pts',(4.74303351799994,11.6,9.76076121399998));
#215793=CARTESIAN_POINT('Ctrl Pts',(4.74112461299994,15.2,9.75875831199998));
#215794=CARTESIAN_POINT('Ctrl Pts',(4.74112461299994,11.6,9.75875831199998));
#215795=CARTESIAN_POINT('Ctrl Pts',(4.73922134499994,15.2,9.75675797099999));
#215796=CARTESIAN_POINT('Ctrl Pts',(4.73922134499994,11.6,9.75675797099999));
#215797=CARTESIAN_POINT('Ctrl Pts',(4.73732371699994,15.2,9.75476020199999));
#215798=CARTESIAN_POINT('Ctrl Pts',(4.73732371699994,11.6,9.75476020199999));
#215799=CARTESIAN_POINT('Ctrl Pts',(4.73543172899995,15.2,9.75276501999998));
#215800=CARTESIAN_POINT('Ctrl Pts',(4.73543172899995,11.6,9.75276501999998));
#215801=CARTESIAN_POINT('Ctrl Pts',(4.73354538299994,15.2,9.75077243799999));
#215802=CARTESIAN_POINT('Ctrl Pts',(4.73354538299994,11.6,9.75077243799999));
#215803=CARTESIAN_POINT('Ctrl Pts',(4.73166467999994,15.2,9.74878246999998));
#215804=CARTESIAN_POINT('Ctrl Pts',(4.73166467999994,11.6,9.74878246999998));
#215805=CARTESIAN_POINT('Ctrl Pts',(4.72978961999994,15.2,9.74679512799998));
#215806=CARTESIAN_POINT('Ctrl Pts',(4.72978961999994,11.6,9.74679512799998));
#215807=CARTESIAN_POINT('Ctrl Pts',(4.72792020499994,15.2,9.74481042899999));
#215808=CARTESIAN_POINT('Ctrl Pts',(4.72792020499994,11.6,9.74481042899999));
#215809=CARTESIAN_POINT('Ctrl Pts',(4.72605643799994,15.2,9.74282838299998));
#215810=CARTESIAN_POINT('Ctrl Pts',(4.72605643799994,11.6,9.74282838299998));
#215811=CARTESIAN_POINT('Ctrl Pts',(4.72419831899995,15.2,9.74084900499999));
#215812=CARTESIAN_POINT('Ctrl Pts',(4.72419831899995,11.6,9.74084900499999));
#215813=CARTESIAN_POINT('Ctrl Pts',(4.72234584699994,15.2,9.73887231099998));
#215814=CARTESIAN_POINT('Ctrl Pts',(4.72234584699994,11.6,9.73887231099998));
#215815=CARTESIAN_POINT('Ctrl Pts',(4.72049902599994,15.2,9.73689831099998));
#215816=CARTESIAN_POINT('Ctrl Pts',(4.72049902599994,11.6,9.73689831099998));
#215817=CARTESIAN_POINT('Ctrl Pts',(4.71865785699994,15.2,9.73492701999999));
#215818=CARTESIAN_POINT('Ctrl Pts',(4.71865785699994,11.6,9.73492701999999));
#215819=CARTESIAN_POINT('Ctrl Pts',(4.71682233899994,15.2,9.73295845299998));
#215820=CARTESIAN_POINT('Ctrl Pts',(4.71682233899994,11.6,9.73295845299998));
#215821=CARTESIAN_POINT('Ctrl Pts',(4.71499247599994,15.2,9.73099262399998));
#215822=CARTESIAN_POINT('Ctrl Pts',(4.71499247599994,11.6,9.73099262399998));
#215823=CARTESIAN_POINT('Ctrl Pts',(4.71316826799994,15.2,9.72902954599999));
#215824=CARTESIAN_POINT('Ctrl Pts',(4.71316826799994,11.6,9.72902954599999));
#215825=CARTESIAN_POINT('Ctrl Pts',(4.71134971599994,15.2,9.72706923299998));
#215826=CARTESIAN_POINT('Ctrl Pts',(4.71134971599994,11.6,9.72706923299998));
#215827=CARTESIAN_POINT('Ctrl Pts',(4.70953681999994,15.2,9.72511169999999));
#215828=CARTESIAN_POINT('Ctrl Pts',(4.70953681999994,11.6,9.72511169999999));
#215829=CARTESIAN_POINT('Ctrl Pts',(4.70772958299994,15.2,9.72315695899999));
#215830=CARTESIAN_POINT('Ctrl Pts',(4.70772958299994,11.6,9.72315695899999));
#215831=CARTESIAN_POINT('Ctrl Pts',(4.70592800699994,15.2,9.72120502599999));
#215832=CARTESIAN_POINT('Ctrl Pts',(4.70592800699994,11.6,9.72120502599999));
#215833=CARTESIAN_POINT('Ctrl Pts',(4.70413208999994,15.2,9.71925591399999));
#215834=CARTESIAN_POINT('Ctrl Pts',(4.70413208999994,11.6,9.71925591399999));
#215835=CARTESIAN_POINT('Ctrl Pts',(4.70234183499994,15.2,9.71730963799999));
#215836=CARTESIAN_POINT('Ctrl Pts',(4.70234183499994,11.6,9.71730963799999));
#215837=CARTESIAN_POINT('Ctrl Pts',(4.70055724399994,15.2,9.71536621099998));
#215838=CARTESIAN_POINT('Ctrl Pts',(4.70055724399994,11.6,9.71536621099998));
#215839=CARTESIAN_POINT('Ctrl Pts',(4.69877831599994,15.2,9.71342564899999));
#215840=CARTESIAN_POINT('Ctrl Pts',(4.69877831599994,11.6,9.71342564899999));
#215841=CARTESIAN_POINT('Ctrl Pts',(4.69700505299994,15.2,9.71148796399999));
#215842=CARTESIAN_POINT('Ctrl Pts',(4.69700505299994,11.6,9.71148796399999));
#215843=CARTESIAN_POINT('Ctrl Pts',(4.69523745699994,15.2,9.70955317299998));
#215844=CARTESIAN_POINT('Ctrl Pts',(4.69523745699994,11.6,9.70955317299998));
#215845=CARTESIAN_POINT('Ctrl Pts',(4.69347552899994,15.2,9.70762128699998));
#215846=CARTESIAN_POINT('Ctrl Pts',(4.69347552899994,11.6,9.70762128699998));
#215847=CARTESIAN_POINT('Ctrl Pts',(4.69171926699994,15.2,9.70569232299999));
#215848=CARTESIAN_POINT('Ctrl Pts',(4.69171926699994,11.6,9.70569232299999));
#215849=CARTESIAN_POINT('Ctrl Pts',(4.68996867699994,15.2,9.70376629399999));
#215850=CARTESIAN_POINT('Ctrl Pts',(4.68996867699994,11.6,9.70376629399999));
#215851=CARTESIAN_POINT('Ctrl Pts',(4.68822375699994,15.2,9.70184321599999));
#215852=CARTESIAN_POINT('Ctrl Pts',(4.68822375699994,11.6,9.70184321599999));
#215853=CARTESIAN_POINT('Ctrl Pts',(4.68648450799994,15.2,9.69992310099999));
#215854=CARTESIAN_POINT('Ctrl Pts',(4.68648450799994,11.6,9.69992310099999));
#215855=CARTESIAN_POINT('Ctrl Pts',(4.68475093199994,15.2,9.69800596699999));
#215856=CARTESIAN_POINT('Ctrl Pts',(4.68475093199994,11.6,9.69800596699999));
#215857=CARTESIAN_POINT('Ctrl Pts',(4.68302303099994,15.2,9.69609182599999));
#215858=CARTESIAN_POINT('Ctrl Pts',(4.68302303099994,11.6,9.69609182599999));
#215859=CARTESIAN_POINT('Ctrl Pts',(4.68130080299994,15.2,9.69418069199998));
#215860=CARTESIAN_POINT('Ctrl Pts',(4.68130080299994,11.6,9.69418069199998));
#215861=CARTESIAN_POINT('Ctrl Pts',(4.67958425099994,15.2,9.69227258199999));
#215862=CARTESIAN_POINT('Ctrl Pts',(4.67958425099994,11.6,9.69227258199999));
#215863=CARTESIAN_POINT('Ctrl Pts',(4.67787337699994,15.2,9.69036750899999));
#215864=CARTESIAN_POINT('Ctrl Pts',(4.67787337699994,11.6,9.69036750899999));
#215865=CARTESIAN_POINT('Ctrl Pts',(4.67616818099994,15.2,9.68846548899998));
#215866=CARTESIAN_POINT('Ctrl Pts',(4.67616818099994,11.6,9.68846548899998));
#215867=CARTESIAN_POINT('Ctrl Pts',(4.67446866299994,15.2,9.68656653599999));
#215868=CARTESIAN_POINT('Ctrl Pts',(4.67446866299994,11.6,9.68656653599999));
#215869=CARTESIAN_POINT('Ctrl Pts',(4.67277482599994,15.2,9.68467066399998));
#215870=CARTESIAN_POINT('Ctrl Pts',(4.67277482599994,11.6,9.68467066399998));
#215871=CARTESIAN_POINT('Ctrl Pts',(4.67108666899994,15.2,9.68277788899999));
#215872=CARTESIAN_POINT('Ctrl Pts',(4.67108666899994,11.6,9.68277788899999));
#215873=CARTESIAN_POINT('Ctrl Pts',(4.66940419399994,15.2,9.68088822599999));
#215874=CARTESIAN_POINT('Ctrl Pts',(4.66940419399994,11.6,9.68088822599999));
#215875=CARTESIAN_POINT('Ctrl Pts',(4.66772740199994,15.2,9.67900168899998));
#215876=CARTESIAN_POINT('Ctrl Pts',(4.66772740199994,11.6,9.67900168899998));
#215877=CARTESIAN_POINT('Ctrl Pts',(4.66605629399994,15.2,9.67711829299999));
#215878=CARTESIAN_POINT('Ctrl Pts',(4.66605629399994,11.6,9.67711829299999));
#215879=CARTESIAN_POINT('Ctrl Pts',(4.66439087099994,15.2,9.67523805499999));
#215880=CARTESIAN_POINT('Ctrl Pts',(4.66439087099994,11.6,9.67523805499999));
#215881=CARTESIAN_POINT('Ctrl Pts',(4.66273113299994,15.2,9.67336098699998));
#215882=CARTESIAN_POINT('Ctrl Pts',(4.66273113299994,11.6,9.67336098699998));
#215883=CARTESIAN_POINT('Ctrl Pts',(4.66107708199994,15.2,9.67148710599999));
#215884=CARTESIAN_POINT('Ctrl Pts',(4.66107708199994,11.6,9.67148710599999));
#215885=CARTESIAN_POINT('Ctrl Pts',(4.65942871899994,15.2,9.66961642799999));
#215886=CARTESIAN_POINT('Ctrl Pts',(4.65942871899994,11.6,9.66961642799999));
#215887=CARTESIAN_POINT('Ctrl Pts',(4.65778604399994,15.2,9.66774896599999));
#215888=CARTESIAN_POINT('Ctrl Pts',(4.65778604399994,11.6,9.66774896599999));
#215889=CARTESIAN_POINT('Ctrl Pts',(4.65614905999994,15.2,9.66588473699998));
#215890=CARTESIAN_POINT('Ctrl Pts',(4.65614905999994,11.6,9.66588473699998));
#215891=CARTESIAN_POINT('Ctrl Pts',(4.65451776499994,15.2,9.66402375399999));
#215892=CARTESIAN_POINT('Ctrl Pts',(4.65451776499994,11.6,9.66402375399999));
#215893=CARTESIAN_POINT('Ctrl Pts',(4.65289216199994,15.2,9.66216603499999));
#215894=CARTESIAN_POINT('Ctrl Pts',(4.65289216199994,11.6,9.66216603499999));
#215895=CARTESIAN_POINT('Ctrl Pts',(4.65127225199994,15.2,9.66031159299998));
#215896=CARTESIAN_POINT('Ctrl Pts',(4.65127225199994,11.6,9.66031159299998));
#215897=CARTESIAN_POINT('Ctrl Pts',(4.64965803299994,15.2,9.65846044499998));
#215898=CARTESIAN_POINT('Ctrl Pts',(4.64965803299994,11.6,9.65846044499998));
#215899=CARTESIAN_POINT('Ctrl Pts',(4.64804950999994,15.2,9.65661260499999));
#215900=CARTESIAN_POINT('Ctrl Pts',(4.64804950999994,11.6,9.65661260499999));
#215901=CARTESIAN_POINT('Ctrl Pts',(4.64644668199994,15.2,9.65476809099999));
#215902=CARTESIAN_POINT('Ctrl Pts',(4.64644668199994,11.6,9.65476809099999));
#215903=CARTESIAN_POINT('Ctrl Pts',(4.64484954799994,15.2,9.65292691699998));
#215904=CARTESIAN_POINT('Ctrl Pts',(4.64484954799994,11.6,9.65292691699998));
#215905=CARTESIAN_POINT('Ctrl Pts',(4.64325811199994,15.2,9.65108909799999));
#215906=CARTESIAN_POINT('Ctrl Pts',(4.64325811199994,11.6,9.65108909799999));
#215907=CARTESIAN_POINT('Ctrl Pts',(4.64167237399994,15.2,9.64925464899999));
#215908=CARTESIAN_POINT('Ctrl Pts',(4.64167237399994,11.6,9.64925464899999));
#215909=CARTESIAN_POINT('Ctrl Pts',(4.64009233299994,15.2,9.64742358899999));
#215910=CARTESIAN_POINT('Ctrl Pts',(4.64009233299994,11.6,9.64742358899999));
#215911=CARTESIAN_POINT('Ctrl Pts',(4.63851799199994,15.2,9.64559592999999));
#215912=CARTESIAN_POINT('Ctrl Pts',(4.63851799199994,11.6,9.64559592999999));
#215913=CARTESIAN_POINT('Ctrl Pts',(4.63694935099994,15.2,9.64377168999999));
#215914=CARTESIAN_POINT('Ctrl Pts',(4.63694935099994,11.6,9.64377168999999));
#215915=CARTESIAN_POINT('Ctrl Pts',(4.63538641099994,15.2,9.64195088399999));
#215916=CARTESIAN_POINT('Ctrl Pts',(4.63538641099994,11.6,9.64195088399999));
#215917=CARTESIAN_POINT('Ctrl Pts',(4.63382917099994,15.2,9.64013352699999));
#215918=CARTESIAN_POINT('Ctrl Pts',(4.63382917099994,11.6,9.64013352699999));
#215919=CARTESIAN_POINT('Ctrl Pts',(4.63227763499994,15.2,9.63831963699998));
#215920=CARTESIAN_POINT('Ctrl Pts',(4.63227763499994,11.6,9.63831963699998));
#215921=CARTESIAN_POINT('Ctrl Pts',(4.63073180199994,15.2,9.63650922899999));
#215922=CARTESIAN_POINT('Ctrl Pts',(4.63073180199994,11.6,9.63650922899999));
#215923=CARTESIAN_POINT('Ctrl Pts',(4.62919167299994,15.2,9.63470231799998));
#215924=CARTESIAN_POINT('Ctrl Pts',(4.62919167299994,11.6,9.63470231799998));
#215925=CARTESIAN_POINT('Ctrl Pts',(4.62765724799994,15.2,9.63289892099999));
#215926=CARTESIAN_POINT('Ctrl Pts',(4.62765724799994,11.6,9.63289892099999));
#215927=CARTESIAN_POINT('Ctrl Pts',(4.62612852999994,15.2,9.63109905299999));
#215928=CARTESIAN_POINT('Ctrl Pts',(4.62612852999994,11.6,9.63109905299999));
#215929=CARTESIAN_POINT('Ctrl Pts',(4.62460551699994,15.2,9.62930273299998));
#215930=CARTESIAN_POINT('Ctrl Pts',(4.62460551699994,11.6,9.62930273299998));
#215931=CARTESIAN_POINT('Ctrl Pts',(4.62308821099994,15.2,9.62750997299998));
#215932=CARTESIAN_POINT('Ctrl Pts',(4.62308821099994,11.6,9.62750997299998));
#215933=CARTESIAN_POINT('Ctrl Pts',(4.62157661299994,15.2,9.62572079199998));
#215934=CARTESIAN_POINT('Ctrl Pts',(4.62157661299994,11.6,9.62572079199998));
#215935=CARTESIAN_POINT('Ctrl Pts',(4.62007072299994,15.2,9.62393520599999));
#215936=CARTESIAN_POINT('Ctrl Pts',(4.62007072299994,11.6,9.62393520599999));
#215937=CARTESIAN_POINT('Ctrl Pts',(4.61857054399994,15.2,9.62215323199998));
#215938=CARTESIAN_POINT('Ctrl Pts',(4.61857054399994,11.6,9.62215323199998));
#215939=CARTESIAN_POINT('Ctrl Pts',(4.61707607299994,15.2,9.62037488299998));
#215940=CARTESIAN_POINT('Ctrl Pts',(4.61707607299994,11.6,9.62037488299998));
#215941=CARTESIAN_POINT('Ctrl Pts',(4.61558731299994,15.2,9.61860017899999));
#215942=CARTESIAN_POINT('Ctrl Pts',(4.61558731299994,11.6,9.61860017899999));
#215943=CARTESIAN_POINT('Ctrl Pts',(4.61410426499994,15.2,9.61682913599999));
#215944=CARTESIAN_POINT('Ctrl Pts',(4.61410426499994,11.6,9.61682913599999));
#215945=CARTESIAN_POINT('Ctrl Pts',(4.61262692899994,15.2,9.61506176899999));
#215946=CARTESIAN_POINT('Ctrl Pts',(4.61262692899994,11.6,9.61506176899999));
#215947=CARTESIAN_POINT('Ctrl Pts',(4.61115530499994,15.2,9.61329809499999));
#215948=CARTESIAN_POINT('Ctrl Pts',(4.61115530499994,11.6,9.61329809499999));
#215949=CARTESIAN_POINT('Ctrl Pts',(4.60968939499994,15.2,9.61153813099998));
#215950=CARTESIAN_POINT('Ctrl Pts',(4.60968939499994,11.6,9.61153813099998));
#215951=CARTESIAN_POINT('Ctrl Pts',(4.60822919899994,15.2,9.60978189399999));
#215952=CARTESIAN_POINT('Ctrl Pts',(4.60822919899994,11.6,9.60978189399999));
#215953=CARTESIAN_POINT('Ctrl Pts',(4.60677471599994,15.2,9.60802939999999));
#215954=CARTESIAN_POINT('Ctrl Pts',(4.60677471599994,11.6,9.60802939999999));
#215955=CARTESIAN_POINT('Ctrl Pts',(4.60532594999994,15.2,9.60628066599998));
#215956=CARTESIAN_POINT('Ctrl Pts',(4.60532594999994,11.6,9.60628066599998));
#215957=CARTESIAN_POINT('Ctrl Pts',(4.60388289999994,15.2,9.60453570899999));
#215958=CARTESIAN_POINT('Ctrl Pts',(4.60388289999994,11.6,9.60453570899999));
#215959=CARTESIAN_POINT('Ctrl Pts',(4.60244556499994,15.2,9.60279454499998));
#215960=CARTESIAN_POINT('Ctrl Pts',(4.60244556499994,11.6,9.60279454499998));
#215961=CARTESIAN_POINT('Ctrl Pts',(4.60101394899994,15.2,9.60105719299998));
#215962=CARTESIAN_POINT('Ctrl Pts',(4.60101394899994,11.6,9.60105719299998));
#215963=CARTESIAN_POINT('Ctrl Pts',(4.59958804899994,15.2,9.59932366799999));
#215964=CARTESIAN_POINT('Ctrl Pts',(4.59958804899994,11.6,9.59932366799999));
#215965=CARTESIAN_POINT('Ctrl Pts',(4.59816786799994,15.2,9.59759398699998));
#215966=CARTESIAN_POINT('Ctrl Pts',(4.59816786799994,11.6,9.59759398699998));
#215967=CARTESIAN_POINT('Ctrl Pts',(4.59675340599994,15.2,9.59586816899998));
#215968=CARTESIAN_POINT('Ctrl Pts',(4.59675340599994,11.6,9.59586816899998));
#215969=CARTESIAN_POINT('Ctrl Pts',(4.59534466399994,15.2,9.59414622899999));
#215970=CARTESIAN_POINT('Ctrl Pts',(4.59534466399994,11.6,9.59414622899999));
#215971=CARTESIAN_POINT('Ctrl Pts',(4.59394164099994,15.2,9.59242818499998));
#215972=CARTESIAN_POINT('Ctrl Pts',(4.59394164099994,11.6,9.59242818499998));
#215973=CARTESIAN_POINT('Ctrl Pts',(4.59254433799994,15.2,9.59071405499999));
#215974=CARTESIAN_POINT('Ctrl Pts',(4.59254433799994,11.6,9.59071405499999));
#215975=CARTESIAN_POINT('Ctrl Pts',(4.59115275799994,15.2,9.58900385399998));
#215976=CARTESIAN_POINT('Ctrl Pts',(4.59115275799994,11.6,9.58900385399998));
#215977=CARTESIAN_POINT('Ctrl Pts',(4.58976689799994,15.2,9.58729760299999));
#215978=CARTESIAN_POINT('Ctrl Pts',(4.58976689799994,11.6,9.58729760299999));
#215979=CARTESIAN_POINT('Ctrl Pts',(4.58838676199994,15.2,9.58559531599998));
#215980=CARTESIAN_POINT('Ctrl Pts',(4.58838676199994,11.6,9.58559531599998));
#215981=CARTESIAN_POINT('Ctrl Pts',(4.58701234599994,15.2,9.58389701199999));
#215982=CARTESIAN_POINT('Ctrl Pts',(4.58701234599994,11.6,9.58389701199999));
#215983=CARTESIAN_POINT('Ctrl Pts',(4.58564365499994,15.2,9.58220270799998));
#215984=CARTESIAN_POINT('Ctrl Pts',(4.58564365499994,11.6,9.58220270799998));
#215985=CARTESIAN_POINT('Ctrl Pts',(4.58428068699994,15.2,9.58051242199998));
#215986=CARTESIAN_POINT('Ctrl Pts',(4.58428068699994,11.6,9.58051242199998));
#215987=CARTESIAN_POINT('Ctrl Pts',(4.58292344399994,15.2,9.57882617199999));
#215988=CARTESIAN_POINT('Ctrl Pts',(4.58292344399994,11.6,9.57882617199999));
#215989=CARTESIAN_POINT('Ctrl Pts',(4.58157192499994,15.2,9.57714397399998));
#215990=CARTESIAN_POINT('Ctrl Pts',(4.58157192499994,11.6,9.57714397399998));
#215991=CARTESIAN_POINT('Ctrl Pts',(4.58022613099994,15.2,9.57546584699998));
#215992=CARTESIAN_POINT('Ctrl Pts',(4.58022613099994,11.6,9.57546584699998));
#215993=CARTESIAN_POINT('Ctrl Pts',(4.57888606199994,15.2,9.57379180899999));
#215994=CARTESIAN_POINT('Ctrl Pts',(4.57888606199994,11.6,9.57379180899999));
#215995=CARTESIAN_POINT('Ctrl Pts',(4.57755171999994,15.2,9.57212187799998));
#215996=CARTESIAN_POINT('Ctrl Pts',(4.57755171999994,11.6,9.57212187799998));
#215997=CARTESIAN_POINT('Ctrl Pts',(4.57622310299994,15.2,9.57045607099998));
#215998=CARTESIAN_POINT('Ctrl Pts',(4.57622310299994,11.6,9.57045607099998));
#215999=CARTESIAN_POINT('Ctrl Pts',(4.57490021399994,15.2,9.56879440499998));
#216000=CARTESIAN_POINT('Ctrl Pts',(4.57490021399994,11.6,9.56879440499998));
#216001=CARTESIAN_POINT('Ctrl Pts',(4.57358305099994,15.2,9.56713690099999));
#216002=CARTESIAN_POINT('Ctrl Pts',(4.57358305099994,11.6,9.56713690099999));
#216003=CARTESIAN_POINT('Ctrl Pts',(4.57227161699994,15.2,9.56548357499998));
#216004=CARTESIAN_POINT('Ctrl Pts',(4.57227161699994,11.6,9.56548357499998));
#216005=CARTESIAN_POINT('Ctrl Pts',(4.57096591099994,15.2,9.56383444499998));
#216006=CARTESIAN_POINT('Ctrl Pts',(4.57096591099994,11.6,9.56383444499998));
#216007=CARTESIAN_POINT('Ctrl Pts',(4.56966593299994,15.2,9.56218952999999));
#216008=CARTESIAN_POINT('Ctrl Pts',(4.56966593299994,11.6,9.56218952999999));
#216009=CARTESIAN_POINT('Ctrl Pts',(4.56837168299994,15.2,9.56054884799999));
#216010=CARTESIAN_POINT('Ctrl Pts',(4.56837168299994,11.6,9.56054884799999));
#216011=CARTESIAN_POINT('Ctrl Pts',(4.56708316199994,15.2,9.55891241699998));
#216012=CARTESIAN_POINT('Ctrl Pts',(4.56708316199994,11.6,9.55891241699998));
#216013=CARTESIAN_POINT('Ctrl Pts',(4.56580037199994,15.2,9.55728025599999));
#216014=CARTESIAN_POINT('Ctrl Pts',(4.56580037199994,11.6,9.55728025599999));
#216015=CARTESIAN_POINT('Ctrl Pts',(4.56452330999994,15.2,9.55565238299998));
#216016=CARTESIAN_POINT('Ctrl Pts',(4.56452330999994,11.6,9.55565238299998));
#216017=CARTESIAN_POINT('Ctrl Pts',(4.56325197899994,15.2,9.55402881599999));
#216018=CARTESIAN_POINT('Ctrl Pts',(4.56325197899994,11.6,9.55402881599999));
#216019=CARTESIAN_POINT('Ctrl Pts',(4.56198637899994,15.2,9.55240957399998));
#216020=CARTESIAN_POINT('Ctrl Pts',(4.56198637899994,11.6,9.55240957399998));
#216021=CARTESIAN_POINT('Ctrl Pts',(4.56072650899994,15.2,9.55079467699999));
#216022=CARTESIAN_POINT('Ctrl Pts',(4.56072650899994,11.6,9.55079467699999));
#216023=CARTESIAN_POINT('Ctrl Pts',(4.55947236999994,15.2,9.54918414099998));
#216024=CARTESIAN_POINT('Ctrl Pts',(4.55947236999994,11.6,9.54918414099998));
#216025=CARTESIAN_POINT('Ctrl Pts',(4.55822396199994,15.2,9.54757798599999));
#216026=CARTESIAN_POINT('Ctrl Pts',(4.55822396199994,11.6,9.54757798599999));
#216027=CARTESIAN_POINT('Ctrl Pts',(4.55698128499994,15.2,9.54597623199999));
#216028=CARTESIAN_POINT('Ctrl Pts',(4.55698128499994,11.6,9.54597623199999));
#216029=CARTESIAN_POINT('Ctrl Pts',(4.55574434099994,15.2,9.54437889699999));
#216030=CARTESIAN_POINT('Ctrl Pts',(4.55574434099994,11.6,9.54437889699999));
#216031=CARTESIAN_POINT('Ctrl Pts',(4.55451312799994,15.2,9.54278599799999));
#216032=CARTESIAN_POINT('Ctrl Pts',(4.55451312799994,11.6,9.54278599799999));
#216033=CARTESIAN_POINT('Ctrl Pts',(4.55328764899994,15.2,9.54119755699999));
#216034=CARTESIAN_POINT('Ctrl Pts',(4.55328764899994,11.6,9.54119755699999));
#216035=CARTESIAN_POINT('Ctrl Pts',(4.55206790099994,15.2,9.53961359099999));
#216036=CARTESIAN_POINT('Ctrl Pts',(4.55206790099994,11.6,9.53961359099999));
#216037=CARTESIAN_POINT('Ctrl Pts',(4.55085388599994,15.2,9.53803411999999));
#216038=CARTESIAN_POINT('Ctrl Pts',(4.55085388599994,11.6,9.53803411999999));
#216039=CARTESIAN_POINT('Ctrl Pts',(4.54964560399994,15.2,9.53645916199999));
#216040=CARTESIAN_POINT('Ctrl Pts',(4.54964560399994,11.6,9.53645916199999));
#216041=CARTESIAN_POINT('Ctrl Pts',(4.54844305499994,15.2,9.53488873799999));
#216042=CARTESIAN_POINT('Ctrl Pts',(4.54844305499994,11.6,9.53488873799999));
#216043=CARTESIAN_POINT('Ctrl Pts',(4.54724623999994,15.2,9.53332286699998));
#216044=CARTESIAN_POINT('Ctrl Pts',(4.54724623999994,11.6,9.53332286699998));
#216045=CARTESIAN_POINT('Ctrl Pts',(4.54605515799994,15.2,9.53176156799999));
#216046=CARTESIAN_POINT('Ctrl Pts',(4.54605515799994,11.6,9.53176156799999));
#216047=CARTESIAN_POINT('Ctrl Pts',(4.54486980899994,15.2,9.53020485899999));
#216048=CARTESIAN_POINT('Ctrl Pts',(4.54486980899994,11.6,9.53020485899999));
#216049=CARTESIAN_POINT('Ctrl Pts',(4.54369019399994,15.2,9.52865276099999));
#216050=CARTESIAN_POINT('Ctrl Pts',(4.54369019399994,11.6,9.52865276099999));
#216051=CARTESIAN_POINT('Ctrl Pts',(4.54251631299994,15.2,9.52710529499999));
#216052=CARTESIAN_POINT('Ctrl Pts',(4.54251631299994,11.6,9.52710529499999));
#216053=CARTESIAN_POINT('Ctrl Pts',(4.54134816699994,15.2,9.52556247699999));
#216054=CARTESIAN_POINT('Ctrl Pts',(4.54134816699994,11.6,9.52556247699999));
#216055=CARTESIAN_POINT('Ctrl Pts',(4.54018575499994,15.2,9.52402432999998));
#216056=CARTESIAN_POINT('Ctrl Pts',(4.54018575499994,11.6,9.52402432999998));
#216057=CARTESIAN_POINT('Ctrl Pts',(4.53902907599994,15.2,9.52249087299998));
#216058=CARTESIAN_POINT('Ctrl Pts',(4.53902907599994,11.6,9.52249087299998));
#216059=CARTESIAN_POINT('Ctrl Pts',(4.53787813099994,15.2,9.52096212399999));
#216060=CARTESIAN_POINT('Ctrl Pts',(4.53787813099994,11.6,9.52096212399999));
#216061=CARTESIAN_POINT('Ctrl Pts',(4.53673292199994,15.2,9.51943810399998));
#216062=CARTESIAN_POINT('Ctrl Pts',(4.53673292199994,11.6,9.51943810399998));
#216063=CARTESIAN_POINT('Ctrl Pts',(4.53559344599994,15.2,9.51791883399999));
#216064=CARTESIAN_POINT('Ctrl Pts',(4.53559344599994,11.6,9.51791883399999));
#216065=CARTESIAN_POINT('Ctrl Pts',(4.53445970499994,15.2,9.51640433299998));
#216066=CARTESIAN_POINT('Ctrl Pts',(4.53445970499994,11.6,9.51640433299998));
#216067=CARTESIAN_POINT('Ctrl Pts',(4.53333169799994,15.2,9.51489462199999));
#216068=CARTESIAN_POINT('Ctrl Pts',(4.53333169799994,11.6,9.51489462199999));
#216069=CARTESIAN_POINT('Ctrl Pts',(4.53220942699994,15.2,9.51338971999999));
#216070=CARTESIAN_POINT('Ctrl Pts',(4.53220942699994,11.6,9.51338971999999));
#216071=CARTESIAN_POINT('Ctrl Pts',(4.53109288899994,15.2,9.51188964799999));
#216072=CARTESIAN_POINT('Ctrl Pts',(4.53109288899994,11.6,9.51188964799999));
#216073=CARTESIAN_POINT('Ctrl Pts',(4.52998208699994,15.2,9.51039442599999));
#216074=CARTESIAN_POINT('Ctrl Pts',(4.52998208699994,11.6,9.51039442599999));
#216075=CARTESIAN_POINT('Ctrl Pts',(4.52887701799994,15.2,9.50890407399999));
#216076=CARTESIAN_POINT('Ctrl Pts',(4.52887701799994,11.6,9.50890407399999));
#216077=CARTESIAN_POINT('Ctrl Pts',(4.52777768499994,15.2,9.50741861399998));
#216078=CARTESIAN_POINT('Ctrl Pts',(4.52777768499994,11.6,9.50741861399998));
#216079=CARTESIAN_POINT('Ctrl Pts',(4.52668408499994,15.2,9.50593806499998));
#216080=CARTESIAN_POINT('Ctrl Pts',(4.52668408499994,11.6,9.50593806499998));
#216081=CARTESIAN_POINT('Ctrl Pts',(4.52559621999994,15.2,9.50446244899998));
#216082=CARTESIAN_POINT('Ctrl Pts',(4.52559621999994,11.6,9.50446244899998));
#216083=CARTESIAN_POINT('Ctrl Pts',(4.52451408999994,15.2,9.50299178399998));
#216084=CARTESIAN_POINT('Ctrl Pts',(4.52451408999994,11.6,9.50299178399998));
#216085=CARTESIAN_POINT('Ctrl Pts',(4.52343769299994,15.2,9.50152609499998));
#216086=CARTESIAN_POINT('Ctrl Pts',(4.52343769299994,11.6,9.50152609499998));
#216087=CARTESIAN_POINT('Ctrl Pts',(4.52236703099994,15.2,9.50006539899999));
#216088=CARTESIAN_POINT('Ctrl Pts',(4.52236703099994,11.6,9.50006539899999));
#216089=CARTESIAN_POINT('Ctrl Pts',(4.52130210399995,15.2,9.49860971899999));
#216090=CARTESIAN_POINT('Ctrl Pts',(4.52130210399995,11.6,9.49860971899999));
#216091=CARTESIAN_POINT('Ctrl Pts',(4.52024290899994,15.2,9.49715907499998));
#216092=CARTESIAN_POINT('Ctrl Pts',(4.52024290899994,11.6,9.49715907499998));
#216093=CARTESIAN_POINT('Ctrl Pts',(4.51918944899994,15.2,9.49571348899998));
#216094=CARTESIAN_POINT('Ctrl Pts',(4.51918944899994,11.6,9.49571348899998));
#216095=CARTESIAN_POINT('Ctrl Pts',(4.51814172299994,15.2,9.49427298099998));
#216096=CARTESIAN_POINT('Ctrl Pts',(4.51814172299994,11.6,9.49427298099998));
#216097=CARTESIAN_POINT('Ctrl Pts',(4.51709972999994,15.2,9.49283757399999));
#216098=CARTESIAN_POINT('Ctrl Pts',(4.51709972999994,11.6,9.49283757399999));
#216099=CARTESIAN_POINT('Ctrl Pts',(4.51606346999994,15.2,9.49140728699999));
#216100=CARTESIAN_POINT('Ctrl Pts',(4.51606346999994,11.6,9.49140728699999));
#216101=CARTESIAN_POINT('Ctrl Pts',(4.51503294399994,15.2,9.48998214299999));
#216102=CARTESIAN_POINT('Ctrl Pts',(4.51503294399994,11.6,9.48998214299999));
#216103=CARTESIAN_POINT('Ctrl Pts',(4.51400814999994,15.2,9.48856216299999));
#216104=CARTESIAN_POINT('Ctrl Pts',(4.51400814999994,11.6,9.48856216299999));
#216105=CARTESIAN_POINT('Ctrl Pts',(4.51298909099994,15.2,9.48714736799998));
#216106=CARTESIAN_POINT('Ctrl Pts',(4.51298909099994,11.6,9.48714736799998));
#216107=CARTESIAN_POINT('Ctrl Pts',(4.51197576199994,15.2,9.48573778099998));
#216108=CARTESIAN_POINT('Ctrl Pts',(4.51197576199994,11.6,9.48573778099998));
#216109=CARTESIAN_POINT('Ctrl Pts',(4.51096816599994,15.2,9.48433342299998));
#216110=CARTESIAN_POINT('Ctrl Pts',(4.51096816599994,11.6,9.48433342299998));
#216111=CARTESIAN_POINT('Ctrl Pts',(4.50996630399994,15.2,9.48293431499999));
#216112=CARTESIAN_POINT('Ctrl Pts',(4.50996630399994,11.6,9.48293431499999));
#216113=CARTESIAN_POINT('Ctrl Pts',(4.50897017099994,15.2,9.48154047899998));
#216114=CARTESIAN_POINT('Ctrl Pts',(4.50897017099994,11.6,9.48154047899998));
#216115=CARTESIAN_POINT('Ctrl Pts',(4.50797977099994,15.2,9.48015193799998));
#216116=CARTESIAN_POINT('Ctrl Pts',(4.50797977099994,11.6,9.48015193799998));
#216117=CARTESIAN_POINT('Ctrl Pts',(4.50699510299994,15.2,9.47876871399998));
#216118=CARTESIAN_POINT('Ctrl Pts',(4.50699510299994,11.6,9.47876871399998));
#216119=CARTESIAN_POINT('Ctrl Pts',(4.50601616399994,15.2,9.47739082699999));
#216120=CARTESIAN_POINT('Ctrl Pts',(4.50601616399994,11.6,9.47739082699999));
#216121=CARTESIAN_POINT('Ctrl Pts',(4.50504295699994,15.2,9.47601830199999));
#216122=CARTESIAN_POINT('Ctrl Pts',(4.50504295699994,11.6,9.47601830199999));
#216123=CARTESIAN_POINT('Ctrl Pts',(4.50407547999994,15.2,9.47465115999999));
#216124=CARTESIAN_POINT('Ctrl Pts',(4.50407547999994,11.6,9.47465115999999));
#216125=CARTESIAN_POINT('Ctrl Pts',(4.50311373299994,15.2,9.47328942299999));
#216126=CARTESIAN_POINT('Ctrl Pts',(4.50311373299994,11.6,9.47328942299999));
#216127=CARTESIAN_POINT('Ctrl Pts',(4.50215771599994,15.2,9.47193311399998));
#216128=CARTESIAN_POINT('Ctrl Pts',(4.50215771599994,11.6,9.47193311399998));
#216129=CARTESIAN_POINT('Ctrl Pts',(4.50120742799994,15.2,9.47058225599999));
#216130=CARTESIAN_POINT('Ctrl Pts',(4.50120742799994,11.6,9.47058225599999));
#216131=CARTESIAN_POINT('Ctrl Pts',(4.50026286899994,15.2,9.46923686999998));
#216132=CARTESIAN_POINT('Ctrl Pts',(4.50026286899994,11.6,9.46923686999998));
#216133=CARTESIAN_POINT('Ctrl Pts',(4.49932403799994,15.2,9.46789697899998));
#216134=CARTESIAN_POINT('Ctrl Pts',(4.49932403799994,11.6,9.46789697899998));
#216135=CARTESIAN_POINT('Ctrl Pts',(4.49839093499994,15.2,9.46656260799998));
#216136=CARTESIAN_POINT('Ctrl Pts',(4.49839093499994,11.6,9.46656260799998));
#216137=CARTESIAN_POINT('Ctrl Pts',(4.49746355999994,15.2,9.46523377799998));
#216138=CARTESIAN_POINT('Ctrl Pts',(4.49746355999994,11.6,9.46523377799998));
#216139=CARTESIAN_POINT('Ctrl Pts',(4.49654191199994,15.2,9.46391051099998));
#216140=CARTESIAN_POINT('Ctrl Pts',(4.49654191199994,11.6,9.46391051099998));
#216141=CARTESIAN_POINT('Ctrl Pts',(4.49562599099994,15.2,9.46259283199998));
#216142=CARTESIAN_POINT('Ctrl Pts',(4.49562599099994,11.6,9.46259283199998));
#216143=CARTESIAN_POINT('Ctrl Pts',(4.49471579599994,15.2,9.46128076399999));
#216144=CARTESIAN_POINT('Ctrl Pts',(4.49471579599994,11.6,9.46128076399999));
#216145=CARTESIAN_POINT('Ctrl Pts',(4.49381132699994,15.2,9.45997432999999));
#216146=CARTESIAN_POINT('Ctrl Pts',(4.49381132699994,11.6,9.45997432999999));
#216147=CARTESIAN_POINT('Ctrl Pts',(4.49291258199994,15.2,9.45867355199999));
#216148=CARTESIAN_POINT('Ctrl Pts',(4.49291258199994,11.6,9.45867355199999));
#216149=CARTESIAN_POINT('Ctrl Pts',(4.49201956299994,15.2,9.45737845499998));
#216150=CARTESIAN_POINT('Ctrl Pts',(4.49201956299994,11.6,9.45737845499998));
#216151=CARTESIAN_POINT('Ctrl Pts',(4.49113226699995,15.2,9.45608906199999));
#216152=CARTESIAN_POINT('Ctrl Pts',(4.49113226699995,11.6,9.45608906199999));
#216153=CARTESIAN_POINT('Ctrl Pts',(4.49025069599994,15.2,9.45480539599998));
#216154=CARTESIAN_POINT('Ctrl Pts',(4.49025069599994,11.6,9.45480539599998));
#216155=CARTESIAN_POINT('Ctrl Pts',(4.48937484699994,15.2,9.45352748299998));
#216156=CARTESIAN_POINT('Ctrl Pts',(4.48937484699994,11.6,9.45352748299998));
#216157=CARTESIAN_POINT('Ctrl Pts',(4.48850472099994,15.2,9.45225534399999));
#216158=CARTESIAN_POINT('Ctrl Pts',(4.48850472099994,11.6,9.45225534399999));
#216159=CARTESIAN_POINT('Ctrl Pts',(4.48764031599994,15.2,9.45098900299998));
#216160=CARTESIAN_POINT('Ctrl Pts',(4.48764031599994,11.6,9.45098900299998));
#216161=CARTESIAN_POINT('Ctrl Pts',(4.48678163299994,15.2,9.44972848599999));
#216162=CARTESIAN_POINT('Ctrl Pts',(4.48678163299994,11.6,9.44972848599999));
#216163=CARTESIAN_POINT('Ctrl Pts',(4.48592867099994,15.2,9.44847381599999));
#216164=CARTESIAN_POINT('Ctrl Pts',(4.48592867099994,11.6,9.44847381599999));
#216165=CARTESIAN_POINT('Ctrl Pts',(4.48508142799994,15.2,9.44722501699999));
#216166=CARTESIAN_POINT('Ctrl Pts',(4.48508142799994,11.6,9.44722501699999));
#216167=CARTESIAN_POINT('Ctrl Pts',(4.48423990499994,15.2,9.44598211299999));
#216168=CARTESIAN_POINT('Ctrl Pts',(4.48423990499994,11.6,9.44598211299999));
#216169=CARTESIAN_POINT('Ctrl Pts',(4.48340409999994,15.2,9.44474512999999));
#216170=CARTESIAN_POINT('Ctrl Pts',(4.48340409999994,11.6,9.44474512999999));
#216171=CARTESIAN_POINT('Ctrl Pts',(4.48257401299994,15.2,9.44351408899998));
#216172=CARTESIAN_POINT('Ctrl Pts',(4.48257401299994,11.6,9.44351408899998));
#216173=CARTESIAN_POINT('Ctrl Pts',(4.48174964399994,15.2,9.44228901799999));
#216174=CARTESIAN_POINT('Ctrl Pts',(4.48174964399994,11.6,9.44228901799999));
#216175=CARTESIAN_POINT('Ctrl Pts',(4.48093099099994,15.2,9.44106994099998));
#216176=CARTESIAN_POINT('Ctrl Pts',(4.48093099099994,11.6,9.44106994099998));
#216177=CARTESIAN_POINT('Ctrl Pts',(4.48011805399995,15.2,9.43985688299998));
#216178=CARTESIAN_POINT('Ctrl Pts',(4.48011805399995,11.6,9.43985688299998));
#216179=CARTESIAN_POINT('Ctrl Pts',(4.47931083199994,15.2,9.43864986699998));
#216180=CARTESIAN_POINT('Ctrl Pts',(4.47931083199994,11.6,9.43864986699998));
#216181=CARTESIAN_POINT('Ctrl Pts',(4.47850932399994,15.2,9.43744891999999));
#216182=CARTESIAN_POINT('Ctrl Pts',(4.47850932399994,11.6,9.43744891999999));
#216183=CARTESIAN_POINT('Ctrl Pts',(4.47771352899994,15.2,9.43625406599999));
#216184=CARTESIAN_POINT('Ctrl Pts',(4.47771352899994,11.6,9.43625406599999));
#216185=CARTESIAN_POINT('Ctrl Pts',(4.47692344799994,15.2,9.43506532899999));
#216186=CARTESIAN_POINT('Ctrl Pts',(4.47692344799994,11.6,9.43506532899999));
#216187=CARTESIAN_POINT('Ctrl Pts',(4.47613907699994,15.2,9.43388273699998));
#216188=CARTESIAN_POINT('Ctrl Pts',(4.47613907699994,11.6,9.43388273699998));
#216189=CARTESIAN_POINT('Ctrl Pts',(4.47536041799994,15.2,9.43270631399999));
#216190=CARTESIAN_POINT('Ctrl Pts',(4.47536041799994,11.6,9.43270631399999));
#216191=CARTESIAN_POINT('Ctrl Pts',(4.47458746999994,15.2,9.43153608499999));
#216192=CARTESIAN_POINT('Ctrl Pts',(4.47458746999994,11.6,9.43153608499999));
#216193=CARTESIAN_POINT('Ctrl Pts',(4.47382022999994,15.2,9.43037207699999));
#216194=CARTESIAN_POINT('Ctrl Pts',(4.47382022999994,11.6,9.43037207699999));
#216195=CARTESIAN_POINT('Ctrl Pts',(4.47305869799994,15.2,9.42921431399999));
#216196=CARTESIAN_POINT('Ctrl Pts',(4.47305869799994,11.6,9.42921431399999));
#216197=CARTESIAN_POINT('Ctrl Pts',(4.47230287399994,15.2,9.42806282299999));
#216198=CARTESIAN_POINT('Ctrl Pts',(4.47230287399994,11.6,9.42806282299999));
#216199=CARTESIAN_POINT('Ctrl Pts',(4.47155275699994,15.2,9.42691763099998));
#216200=CARTESIAN_POINT('Ctrl Pts',(4.47155275699994,11.6,9.42691763099998));
#216201=CARTESIAN_POINT('Ctrl Pts',(4.47080834499994,15.2,9.42577875999999));
#216202=CARTESIAN_POINT('Ctrl Pts',(4.47080834499994,11.6,9.42577875999999));
#216203=CARTESIAN_POINT('Ctrl Pts',(4.47006963599994,15.2,9.42464624099999));
#216204=CARTESIAN_POINT('Ctrl Pts',(4.47006963599994,11.6,9.42464624099999));
#216205=CARTESIAN_POINT('Ctrl Pts',(4.46933663299994,15.2,9.42352009699999));
#216206=CARTESIAN_POINT('Ctrl Pts',(4.46933663299994,11.6,9.42352009699999));
#216207=CARTESIAN_POINT('Ctrl Pts',(4.46860933199994,15.2,9.42240035599998));
#216208=CARTESIAN_POINT('Ctrl Pts',(4.46860933199994,11.6,9.42240035599998));
#216209=CARTESIAN_POINT('Ctrl Pts',(4.46788773299994,15.2,9.42128704399998));
#216210=CARTESIAN_POINT('Ctrl Pts',(4.46788773299994,11.6,9.42128704399998));
#216211=CARTESIAN_POINT('Ctrl Pts',(4.46717183399994,15.2,9.42018018699999));
#216212=CARTESIAN_POINT('Ctrl Pts',(4.46717183399994,11.6,9.42018018699999));
#216213=CARTESIAN_POINT('Ctrl Pts',(4.46646163399994,15.2,9.41907981299998));
#216214=CARTESIAN_POINT('Ctrl Pts',(4.46646163399994,11.6,9.41907981299998));
#216215=CARTESIAN_POINT('Ctrl Pts',(4.46575713299994,15.2,9.41798594799998));
#216216=CARTESIAN_POINT('Ctrl Pts',(4.46575713299994,11.6,9.41798594799998));
#216217=CARTESIAN_POINT('Ctrl Pts',(4.46505832899994,15.2,9.41689861899999));
#216218=CARTESIAN_POINT('Ctrl Pts',(4.46505832899994,11.6,9.41689861899999));
#216219=CARTESIAN_POINT('Ctrl Pts',(4.46436522199994,15.2,9.41581785299999));
#216220=CARTESIAN_POINT('Ctrl Pts',(4.46436522199994,11.6,9.41581785299999));
#216221=CARTESIAN_POINT('Ctrl Pts',(4.46367780899994,15.2,9.41474367799999));
#216222=CARTESIAN_POINT('Ctrl Pts',(4.46367780899994,11.6,9.41474367799999));
#216223=CARTESIAN_POINT('Ctrl Pts',(4.46299609099994,15.2,9.41367611999999));
#216224=CARTESIAN_POINT('Ctrl Pts',(4.46299609099994,11.6,9.41367611999999));
#216225=CARTESIAN_POINT('Ctrl Pts',(4.46232006499994,15.2,9.41261520599999));
#216226=CARTESIAN_POINT('Ctrl Pts',(4.46232006499994,11.6,9.41261520599999));
#216227=CARTESIAN_POINT('Ctrl Pts',(4.46164973199994,15.2,9.41156096599999));
#216228=CARTESIAN_POINT('Ctrl Pts',(4.46164973199994,11.6,9.41156096599999));
#216229=CARTESIAN_POINT('Ctrl Pts',(4.46098508699994,15.2,9.41051342599999));
#216230=CARTESIAN_POINT('Ctrl Pts',(4.46098508699994,11.6,9.41051342599999));
#216231=CARTESIAN_POINT('Ctrl Pts',(4.46032613299994,15.2,9.40947261499998));
#216232=CARTESIAN_POINT('Ctrl Pts',(4.46032613299994,11.6,9.40947261499998));
#216233=CARTESIAN_POINT('Ctrl Pts',(4.45967286699995,15.2,9.40843855999999));
#216234=CARTESIAN_POINT('Ctrl Pts',(4.45967286699995,11.6,9.40843855999999));
#216235=CARTESIAN_POINT('Ctrl Pts',(4.45902528699994,15.2,9.40741128699998));
#216236=CARTESIAN_POINT('Ctrl Pts',(4.45902528699994,11.6,9.40741128699998));
#216237=CARTESIAN_POINT('Ctrl Pts',(4.45838339299994,15.2,9.40639082799999));
#216238=CARTESIAN_POINT('Ctrl Pts',(4.45838339299994,11.6,9.40639082799999));
#216239=CARTESIAN_POINT('Ctrl Pts',(4.45774718199995,15.2,9.40537720999998));
#216240=CARTESIAN_POINT('Ctrl Pts',(4.45774718199995,11.6,9.40537720999998));
#216241=CARTESIAN_POINT('Ctrl Pts',(4.45711665599995,15.2,9.40437045999998));
#216242=CARTESIAN_POINT('Ctrl Pts',(4.45711665599995,11.6,9.40437045999998));
#216243=CARTESIAN_POINT('Ctrl Pts',(4.45649180899994,15.2,9.40337060799998));
#216244=CARTESIAN_POINT('Ctrl Pts',(4.45649180899994,11.6,9.40337060799998));
#216245=CARTESIAN_POINT('Ctrl Pts',(4.45587264399994,15.2,9.40237768199999));
#216246=CARTESIAN_POINT('Ctrl Pts',(4.45587264399994,11.6,9.40237768199999));
#216247=CARTESIAN_POINT('Ctrl Pts',(4.45525915699994,15.2,9.40139171099998));
#216248=CARTESIAN_POINT('Ctrl Pts',(4.45525915699994,11.6,9.40139171099998));
#216249=CARTESIAN_POINT('Ctrl Pts',(4.45465134699994,15.2,9.40041272399998));
#216250=CARTESIAN_POINT('Ctrl Pts',(4.45465134699994,11.6,9.40041272399998));
#216251=CARTESIAN_POINT('Ctrl Pts',(4.45404921299995,15.2,9.39944075099999));
#216252=CARTESIAN_POINT('Ctrl Pts',(4.45404921299995,11.6,9.39944075099999));
#216253=CARTESIAN_POINT('Ctrl Pts',(4.45345275399994,15.2,9.39847581999998));
#216254=CARTESIAN_POINT('Ctrl Pts',(4.45345275399994,11.6,9.39847581999998));
#216255=CARTESIAN_POINT('Ctrl Pts',(4.45286196799994,15.2,9.39751795999998));
#216256=CARTESIAN_POINT('Ctrl Pts',(4.45286196799994,11.6,9.39751795999998));
#216257=CARTESIAN_POINT('Ctrl Pts',(4.45227685199994,15.2,9.39656720199999));
#216258=CARTESIAN_POINT('Ctrl Pts',(4.45227685199994,11.6,9.39656720199999));
#216259=CARTESIAN_POINT('Ctrl Pts',(4.45169740799995,15.2,9.39562357499998));
#216260=CARTESIAN_POINT('Ctrl Pts',(4.45169740799995,11.6,9.39562357499998));
#216261=CARTESIAN_POINT('Ctrl Pts',(4.45112363199994,15.2,9.39468710799999));
#216262=CARTESIAN_POINT('Ctrl Pts',(4.45112363199994,11.6,9.39468710799999));
#216263=CARTESIAN_POINT('Ctrl Pts',(4.45055552199995,15.2,9.39375783199999));
#216264=CARTESIAN_POINT('Ctrl Pts',(4.45055552199995,11.6,9.39375783199999));
#216265=CARTESIAN_POINT('Ctrl Pts',(4.44999307799994,15.2,9.39283577599999));
#216266=CARTESIAN_POINT('Ctrl Pts',(4.44999307799994,11.6,9.39283577599999));
#216267=CARTESIAN_POINT('Ctrl Pts',(4.44943629699995,15.2,9.39192097099999));
#216268=CARTESIAN_POINT('Ctrl Pts',(4.44943629699995,11.6,9.39192097099999));
#216269=CARTESIAN_POINT('Ctrl Pts',(4.44888517999994,15.2,9.39101344799998));
#216270=CARTESIAN_POINT('Ctrl Pts',(4.44888517999994,11.6,9.39101344799998));
#216271=CARTESIAN_POINT('Ctrl Pts',(4.44833972299994,15.2,9.39011323599999));
#216272=CARTESIAN_POINT('Ctrl Pts',(4.44833972299994,11.6,9.39011323599999));
#216273=CARTESIAN_POINT('Ctrl Pts',(4.44779992399994,15.2,9.38922036599998));
#216274=CARTESIAN_POINT('Ctrl Pts',(4.44779992399994,11.6,9.38922036599998));
#216275=CARTESIAN_POINT('Ctrl Pts',(4.44726578199994,15.2,9.38833486899998));
#216276=CARTESIAN_POINT('Ctrl Pts',(4.44726578199994,11.6,9.38833486899998));
#216277=CARTESIAN_POINT('Ctrl Pts',(4.44673729699994,15.2,9.38745677599999));
#216278=CARTESIAN_POINT('Ctrl Pts',(4.44673729699994,11.6,9.38745677599999));
#216279=CARTESIAN_POINT('Ctrl Pts',(4.44621446499994,15.2,9.38658611899999));
#216280=CARTESIAN_POINT('Ctrl Pts',(4.44621446499994,11.6,9.38658611899999));
#216281=CARTESIAN_POINT('Ctrl Pts',(4.44569728499994,15.2,9.38572292699998));
#216282=CARTESIAN_POINT('Ctrl Pts',(4.44569728499994,11.6,9.38572292699998));
#216283=CARTESIAN_POINT('Ctrl Pts',(4.44518575599994,15.2,9.38486723299999));
#216284=CARTESIAN_POINT('Ctrl Pts',(4.44518575599994,11.6,9.38486723299999));
#216285=CARTESIAN_POINT('Ctrl Pts',(4.44467987499995,15.2,9.38401906899998));
#216286=CARTESIAN_POINT('Ctrl Pts',(4.44467987499995,11.6,9.38401906899998));
#216287=CARTESIAN_POINT('Ctrl Pts',(4.44417963999994,15.2,9.38317846499999));
#216288=CARTESIAN_POINT('Ctrl Pts',(4.44417963999994,11.6,9.38317846499999));
#216289=CARTESIAN_POINT('Ctrl Pts',(4.44368505199995,15.2,9.38234545399999));
#216290=CARTESIAN_POINT('Ctrl Pts',(4.44368505199995,11.6,9.38234545399999));
#216291=CARTESIAN_POINT('Ctrl Pts',(4.44319610499995,15.2,9.38152006799999));
#216292=CARTESIAN_POINT('Ctrl Pts',(4.44319610499995,11.6,9.38152006799999));
#216293=CARTESIAN_POINT('Ctrl Pts',(4.44271279899994,15.2,9.38070233899998));
#216294=CARTESIAN_POINT('Ctrl Pts',(4.44271279899994,11.6,9.38070233899998));
#216295=CARTESIAN_POINT('Ctrl Pts',(4.44223513299994,15.2,9.37989229799999));
#216296=CARTESIAN_POINT('Ctrl Pts',(4.44223513299994,11.6,9.37989229799999));
#216297=CARTESIAN_POINT('Ctrl Pts',(4.44176310499994,15.2,9.37908997999998));
#216298=CARTESIAN_POINT('Ctrl Pts',(4.44176310499994,11.6,9.37908997999998));
#216299=CARTESIAN_POINT('Ctrl Pts',(4.44129939799994,15.2,9.37829999199998));
#216300=CARTESIAN_POINT('Ctrl Pts',(4.44129939799994,11.6,9.37829999199998));
#216301=CARTESIAN_POINT('Ctrl Pts',(4.44093341099994,15.2,9.37767505799999));
#216302=CARTESIAN_POINT('Ctrl Pts',(4.44093341099994,11.6,9.37767505799999));
#216303=CARTESIAN_POINT('Ctrl Pts',(4.44066206999994,15.2,9.37721094199999));
#216304=CARTESIAN_POINT('Ctrl Pts',(4.44066206999994,11.6,9.37721094199999));
#216305=CARTESIAN_POINT('Ctrl Pts',(4.44048314699994,15.2,9.37690455399999));
#216306=CARTESIAN_POINT('Ctrl Pts',(4.44048314699994,11.6,9.37690455399999));
#216307=CARTESIAN_POINT('Ctrl Pts',(4.44039525799994,15.2,9.37675396799998));
#216308=CARTESIAN_POINT('Ctrl Pts',(4.44039525799994,11.6,9.37675396799998));
#216309=CARTESIAN_POINT('',(4.44039525799994,12.2,9.37675396699999));
#216310=CARTESIAN_POINT('',(4.44039525799994,15.2,9.37675396699999));
#216311=CARTESIAN_POINT('',(4.44039525799994,12.2,9.37675396699999));
#216312=CARTESIAN_POINT('Ctrl Pts',(5.26939701799994,12.2,10.221714878));
#216313=CARTESIAN_POINT('Ctrl Pts',(5.2653120205644,12.2,10.2186661882717));
#216314=CARTESIAN_POINT('Ctrl Pts',(5.26124103171183,12.2,10.2156183760956));
#216315=CARTESIAN_POINT('Ctrl Pts',(5.25718406560325,12.2,10.2125714574851));
#216316=CARTESIAN_POINT('Ctrl Pts',(5.25312710004742,12.2,10.2095245392899));
#216317=CARTESIAN_POINT('Ctrl Pts',(5.24908415133328,12.2,10.2064785072781));
#216318=CARTESIAN_POINT('Ctrl Pts',(5.24505524247764,12.2,10.2034334347354));
#216319=CARTESIAN_POINT('Ctrl Pts',(5.24203356069867,12.2,10.2011496302247));
#216320=CARTESIAN_POINT('Ctrl Pts',(5.23901977556914,12.2,10.1988663694659));
#216321=CARTESIAN_POINT('Ctrl Pts',(5.23601390080266,12.2,10.1965836989655));
#216322=CARTESIAN_POINT('Ctrl Pts',(5.23300802603618,12.2,10.194301028465));
#216323=CARTESIAN_POINT('Ctrl Pts',(5.23001006011084,12.2,10.1920189499479));
#216324=CARTESIAN_POINT('Ctrl Pts',(5.22702001488506,12.2,10.1897375041973));
#216325=CARTESIAN_POINT('Ctrl Pts',(5.22402996911608,12.2,10.1874560580323));
#216326=CARTESIAN_POINT('Ctrl Pts',(5.22104784408269,12.2,10.1851752440175));
#216327=CARTESIAN_POINT('Ctrl Pts',(5.21807364785986,12.2,10.1828950987696));
#216328=CARTESIAN_POINT('Ctrl Pts',(5.21509945217735,12.2,10.1806149539359));
#216329=CARTESIAN_POINT('Ctrl Pts',(5.21213318603366,12.2,10.1783354761067));
#216330=CARTESIAN_POINT('Ctrl Pts',(5.20917485866094,12.2,10.1760567053258));
#216331=CARTESIAN_POINT('Ctrl Pts',(5.20621653128821,12.2,10.1737779345448));
#216332=CARTESIAN_POINT('Ctrl Pts',(5.2032661425217,12.2,10.171499871169));
#216333=CARTESIAN_POINT('Ctrl Pts',(5.20032370467096,12.2,10.1692225565018));
#216334=CARTESIAN_POINT('Ctrl Pts',(5.19738126682022,12.2,10.1669452418346));
#216335=CARTESIAN_POINT('Ctrl Pts',(5.19444677701023,12.2,10.164668675434));
#216336=CARTESIAN_POINT('Ctrl Pts',(5.19152024774155,12.2,10.162392898725));
#216337=CARTESIAN_POINT('Ctrl Pts',(5.18859371847288,12.2,10.160117122016));
#216338=CARTESIAN_POINT('Ctrl Pts',(5.18567514874556,12.2,10.157842134432));
#216339=CARTESIAN_POINT('Ctrl Pts',(5.18276454755894,12.2,10.1555679752645));
#216340=CARTESIAN_POINT('Ctrl Pts',(5.17985394637232,12.2,10.1532938160971));
#216341=CARTESIAN_POINT('Ctrl Pts',(5.17695131418371,12.2,10.1510204859874));
#216342=CARTESIAN_POINT('Ctrl Pts',(5.17405666176834,12.2,10.1487480252063));
#216343=CARTESIAN_POINT('Ctrl Pts',(5.17019712486394,12.2,10.145718077223));
#216344=CARTESIAN_POINT('Ctrl Pts',(5.16635177173637,12.2,10.1426896739813));
#216345=CARTESIAN_POINT('Ctrl Pts',(5.16252062769516,12.2,10.1396629147609));
#216346=CARTESIAN_POINT('Ctrl Pts',(5.15964726992526,12.2,10.1373928455518));
#216347=CARTESIAN_POINT('Ctrl Pts',(5.1567819042794,12.2,10.1351236999176));
#216348=CARTESIAN_POINT('Ctrl Pts',(5.15392454050822,12.2,10.1328555202083));
#216349=CARTESIAN_POINT('Ctrl Pts',(5.15106717673703,12.2,10.130587340499));
#216350=CARTESIAN_POINT('Ctrl Pts',(5.14821781410719,12.2,10.1283201257148));
#216351=CARTESIAN_POINT('Ctrl Pts',(5.14537646333473,12.2,10.1260539180053));
#216352=CARTESIAN_POINT('Ctrl Pts',(5.14253511256228,12.2,10.1237877102959));
#216353=CARTESIAN_POINT('Ctrl Pts',(5.13970177271935,12.2,10.121522509169));
#216354=CARTESIAN_POINT('Ctrl Pts',(5.13687645430493,12.2,10.1192583559714));
#216355=CARTESIAN_POINT('Ctrl Pts',(5.13405113589052,12.2,10.1169942027738));
#216356=CARTESIAN_POINT('Ctrl Pts',(5.13123383787802,12.2,10.1147310987777));
#216357=CARTESIAN_POINT('Ctrl Pts',(5.12842457110398,12.2,10.1124690842348));
#216358=CARTESIAN_POINT('Ctrl Pts',(5.12561530381961,12.2,10.1102070692809));
#216359=CARTESIAN_POINT('Ctrl Pts',(5.1228140669125,12.2,10.1079461450189));
#216360=CARTESIAN_POINT('Ctrl Pts',(5.12002087017431,12.2,10.1056863534823));
#216361=CARTESIAN_POINT('Ctrl Pts',(5.11722767394355,12.2,10.1034265623563));
#216362=CARTESIAN_POINT('Ctrl Pts',(5.11444251757905,12.2,10.1011679040885));
#216363=CARTESIAN_POINT('Ctrl Pts',(5.11166541043065,12.2,10.0989104195039));
#216364=CARTESIAN_POINT('Ctrl Pts',(5.10888830328225,12.2,10.0966529349194));
#216365=CARTESIAN_POINT('Ctrl Pts',(5.10611924669956,12.2,10.0943966254347));
#216366=CARTESIAN_POINT('Ctrl Pts',(5.10335824800821,12.2,10.0921415337666));
#216367=CARTESIAN_POINT('Ctrl Pts',(5.10059724931687,12.2,10.0898864420986));
#216368=CARTESIAN_POINT('Ctrl Pts',(5.09784430908352,12.2,10.0876325671471));
#216369=CARTESIAN_POINT('Ctrl Pts',(5.09509943826588,12.2,10.0853799534789));
#216370=CARTESIAN_POINT('Ctrl Pts',(5.09235456744824,12.2,10.0831273398106));
#216371=CARTESIAN_POINT('Ctrl Pts',(5.08961776391601,12.2,10.0808759864328));
#216372=CARTESIAN_POINT('Ctrl Pts',(5.08688903800291,12.2,10.0786259366937));
#216373=CARTESIAN_POINT('Ctrl Pts',(5.0841603120898,12.2,10.0763758869545));
#216374=CARTESIAN_POINT('Ctrl Pts',(5.0814396636271,12.2,10.0741271405584));
#216375=CARTESIAN_POINT('Ctrl Pts',(5.07872710234957,12.2,10.0718797414316));
#216376=CARTESIAN_POINT('Ctrl Pts',(5.07601454057925,12.2,10.0696323418964));
#216377=CARTESIAN_POINT('Ctrl Pts',(5.07331006515285,12.2,10.0673862893367));
#216378=CARTESIAN_POINT('Ctrl Pts',(5.07061368588709,12.2,10.0651416272606));
#216379=CARTESIAN_POINT('Ctrl Pts',(5.06791730711117,12.2,10.0628969655924));
#216380=CARTESIAN_POINT('Ctrl Pts',(5.0652290237098,12.2,10.0606536937074));
#216381=CARTESIAN_POINT('Ctrl Pts',(5.06254884547455,12.2,10.0584118579973));
#216382=CARTESIAN_POINT('Ctrl Pts',(5.0598686672393,12.2,10.0561700222872));
#216383=CARTESIAN_POINT('Ctrl Pts',(5.05719659446274,12.2,10.0539296205601));
#216384=CARTESIAN_POINT('Ctrl Pts',(5.05453263525581,12.2,10.0516906975063));
#216385=CARTESIAN_POINT('Ctrl Pts',(5.05186867604886,12.2,10.0494517744525));
#216386=CARTESIAN_POINT('Ctrl Pts',(5.04921283073482,12.2,10.0472143307976));
#216387=CARTESIAN_POINT('Ctrl Pts',(5.04656510898563,12.2,10.044978410202));
#216388=CARTESIAN_POINT('Ctrl Pts',(5.04391738723644,12.2,10.0427424896064));
#216389=CARTESIAN_POINT('Ctrl Pts',(5.04127778877529,12.2,10.0405080921791));
#216390=CARTESIAN_POINT('Ctrl Pts',(5.03864632153685,12.2,10.03827526351));
#216391=CARTESIAN_POINT('Ctrl Pts',(5.03601485429843,12.2,10.036042434841));
#216392=CARTESIAN_POINT('Ctrl Pts',(5.03339151892609,12.2,10.0338111735552));
#216393=CARTESIAN_POINT('Ctrl Pts',(5.03077632510334,12.2,10.0315815254694));
#216394=CARTESIAN_POINT('Ctrl Pts',(5.02816113080549,12.2,10.0293518769784));
#216395=CARTESIAN_POINT('Ctrl Pts',(5.0255540764766,12.2,10.027123841538));
#216396=CARTESIAN_POINT('Ctrl Pts',(5.02295517268333,12.2,10.0248974650063));
#216397=CARTESIAN_POINT('Ctrl Pts',(5.01948996841253,12.2,10.0219289636381));
#216398=CARTESIAN_POINT('Ctrl Pts',(5.01603925109809,12.2,10.0189634097816));
#216399=CARTESIAN_POINT('Ctrl Pts',(5.01260304425224,12.2,10.0160009125103));
#216400=CARTESIAN_POINT('Ctrl Pts',(5.01002588900081,12.2,10.013779039456));
#216401=CARTESIAN_POINT('Ctrl Pts',(5.0074568954535,12.2,10.0115588863114));
#216402=CARTESIAN_POINT('Ctrl Pts',(5.00489607079582,12.2,10.0093404982668));
#216403=CARTESIAN_POINT('Ctrl Pts',(5.00233524613813,12.2,10.0071221102222));
#216404=CARTESIAN_POINT('Ctrl Pts',(4.99978259281325,12.2,10.0049054877859));
#216405=CARTESIAN_POINT('Ctrl Pts',(4.99723811711292,12.2,10.0026906762411));
#216406=CARTESIAN_POINT('Ctrl Pts',(4.99469364095034,12.2,10.000475864294));
#216407=CARTESIAN_POINT('Ctrl Pts',(4.99215734326508,12.2,9.99826286325572));
#216408=CARTESIAN_POINT('Ctrl Pts',(4.98962923394044,12.2,9.99605172126795));
#216409=CARTESIAN_POINT('Ctrl Pts',(4.98625842227304,12.2,9.9931035326204));
#216410=CARTESIAN_POINT('Ctrl Pts',(4.98290216362476,12.2,9.99015864651654));
#216411=CARTESIAN_POINT('Ctrl Pts',(4.97956048149383,12.2,9.98721717524364));
#216412=CARTESIAN_POINT('Ctrl Pts',(4.97621879890759,12.2,9.98427570356997));
#216413=CARTESIAN_POINT('Ctrl Pts',(4.97289169100956,12.2,9.9813376455353));
#216414=CARTESIAN_POINT('Ctrl Pts',(4.96957917894164,12.2,9.97840311448685));
#216415=CARTESIAN_POINT('Ctrl Pts',(4.96626666732504,12.2,9.97546858383822));
#216416=CARTESIAN_POINT('Ctrl Pts',(4.9629687504621,12.2,9.97253758002802));
#216417=CARTESIAN_POINT('Ctrl Pts',(4.9596854482851,12.2,9.96961021548932));
#216418=CARTESIAN_POINT('Ctrl Pts',(4.95640214566075,12.2,9.96668285055175));
#216419=CARTESIAN_POINT('Ctrl Pts',(4.95313345891366,12.2,9.96375912597543));
#216420=CARTESIAN_POINT('Ctrl Pts',(4.94987940551945,12.2,9.96083915355961));
#216421=CARTESIAN_POINT('Ctrl Pts',(4.9466253525686,12.2,9.95791918154165));
#216422=CARTESIAN_POINT('Ctrl Pts',(4.94338593425932,12.2,9.95500296396137));
#216423=CARTESIAN_POINT('Ctrl Pts',(4.94016117002198,12.2,9.95209061475476));
#216424=CARTESIAN_POINT('Ctrl Pts',(4.93693640534528,12.2,9.94917826515134));
#216425=CARTESIAN_POINT('Ctrl Pts',(4.93372629353421,12.2,9.94626978343171));
#216426=CARTESIAN_POINT('Ctrl Pts',(4.93053085547213,12.2,9.9433652864959));
#216427=CARTESIAN_POINT('Ctrl Pts',(4.92733541784544,12.2,9.94046078995584));
#216428=CARTESIAN_POINT('Ctrl Pts',(4.92415465206556,12.2,9.93756027910911));
#216429=CARTESIAN_POINT('Ctrl Pts',(4.92098857894272,12.2,9.93466386914528));
#216430=CARTESIAN_POINT('Ctrl Pts',(4.9178225053885,12.2,9.93176745878681));
#216431=CARTESIAN_POINT('Ctrl Pts',(4.91467112236914,12.2,9.92887515004603));
#216432=CARTESIAN_POINT('Ctrl Pts',(4.91153445097694,12.2,9.92598706105558));
#216433=CARTESIAN_POINT('Ctrl Pts',(4.90839778001212,12.2,9.92309897245864));
#216434=CARTESIAN_POINT('Ctrl Pts',(4.90527581901654,12.2,9.92021510386916));
#216435=CARTESIAN_POINT('Ctrl Pts',(4.9021685868246,12.2,9.91733557343745));
#216436=CARTESIAN_POINT('Ctrl Pts',(4.89906135420929,12.2,9.91445604261339));
#216437=CARTESIAN_POINT('Ctrl Pts',(4.89596885035724,12.2,9.91158085077582));
#216438=CARTESIAN_POINT('Ctrl Pts',(4.89289109373113,12.2,9.90871011843968));
#216439=CARTESIAN_POINT('Ctrl Pts',(4.88981333752437,12.2,9.90583938649468));
#216440=CARTESIAN_POINT('Ctrl Pts',(4.88675032783394,12.2,9.90297311305106));
#216441=CARTESIAN_POINT('Ctrl Pts',(4.88370208474828,12.2,9.90011141995119));
#216442=CARTESIAN_POINT('Ctrl Pts',(4.8806538412473,12.2,9.89724972646141));
#216443=CARTESIAN_POINT('Ctrl Pts',(4.87762036132828,12.2,9.89439261380542));
#216444=CARTESIAN_POINT('Ctrl Pts',(4.87460166477489,12.2,9.89154020298331));
#216445=CARTESIAN_POINT('Ctrl Pts',(4.87158296822151,12.2,9.88868779216121));
#216446=CARTESIAN_POINT('Ctrl Pts',(4.86857905546424,12.2,9.88584008495627));
#216447=CARTESIAN_POINT('Ctrl Pts',(4.86558994280284,12.2,9.88299720280183));
#216448=CARTESIAN_POINT('Ctrl Pts',(4.86110627421802,12.2,9.8787328799575));
#216449=CARTESIAN_POINT('Ctrl Pts',(4.8566559065057,12.2,9.87447941661418));
#216450=CARTESIAN_POINT('Ctrl Pts',(4.85223889875095,12.2,9.8702372327688));
#216451=CARTESIAN_POINT('Ctrl Pts',(4.84929422704819,12.2,9.86740911033366));
#216452=CARTESIAN_POINT('Ctrl Pts',(4.84636438118417,12.2,9.8645860005642));
#216453=CARTESIAN_POINT('Ctrl Pts',(4.8434493789765,12.2,9.86176803146071));
#216454=CARTESIAN_POINT('Ctrl Pts',(4.84053437637165,12.2,9.85895006197325));
#216455=CARTESIAN_POINT('Ctrl Pts',(4.83763421668213,12.2,9.85613723330575));
#216456=CARTESIAN_POINT('Ctrl Pts',(4.83474891802488,12.2,9.85332967054163));
#216457=CARTESIAN_POINT('Ctrl Pts',(4.83186361936764,12.2,9.85052210777752));
#216458=CARTESIAN_POINT('Ctrl Pts',(4.82899318032601,12.2,9.84771981368344));
#216459=CARTESIAN_POINT('Ctrl Pts',(4.82613761828301,12.2,9.84492291430934));
#216460=CARTESIAN_POINT('Ctrl Pts',(4.82328205662909,12.2,9.84212601531632));
#216461=CARTESIAN_POINT('Ctrl Pts',(4.82044137020316,12.2,9.8393345126868));
#216462=CARTESIAN_POINT('Ctrl Pts',(4.81761557847681,12.2,9.8365485362352));
#216463=CARTESIAN_POINT('Ctrl Pts',(4.81478978636546,12.2,9.83376255940399));
#216464=CARTESIAN_POINT('Ctrl Pts',(4.81197888582972,12.2,9.8309821085136));
#216465=CARTESIAN_POINT('Ctrl Pts',(4.80918289506775,12.2,9.82820731502962));
#216466=CARTESIAN_POINT('Ctrl Pts',(4.80638690468674,12.2,9.82543252192371));
#216467=CARTESIAN_POINT('Ctrl Pts',(4.80360582296489,12.2,9.82266338481429));
#216468=CARTESIAN_POINT('Ctrl Pts',(4.80083966546783,12.2,9.81990003898426));
#216469=CARTESIAN_POINT('Ctrl Pts',(4.79807350759388,12.2,9.81713669277772));
#216470=CARTESIAN_POINT('Ctrl Pts',(4.79532227474298,12.2,9.81437913470427));
#216471=CARTESIAN_POINT('Ctrl Pts',(4.79258598190291,12.2,9.81162750108404));
#216472=CARTESIAN_POINT('Ctrl Pts',(4.78984968943566,12.2,9.80887586783873));
#216473=CARTESIAN_POINT('Ctrl Pts',(4.78712833722324,12.2,9.80613015788931));
#216474=CARTESIAN_POINT('Ctrl Pts',(4.78442194022127,12.2,9.80339050622398));
#216475=CARTESIAN_POINT('Ctrl Pts',(4.78171554285056,12.2,9.80065085418537));
#216476=CARTESIAN_POINT('Ctrl Pts',(4.77902410020388,12.2,9.7979172612364));
#216477=CARTESIAN_POINT('Ctrl Pts',(4.77634762828123,12.2,9.79518986197706));
#216478=CARTESIAN_POINT('Ctrl Pts',(4.77367115672325,12.2,9.79246246308933));
#216479=CARTESIAN_POINT('Ctrl Pts',(4.77100965562339,12.2,9.7897412602804));
#216480=CARTESIAN_POINT('Ctrl Pts',(4.76836313915066,12.2,9.78702638914394));
#216481=CARTESIAN_POINT('Ctrl Pts',(4.76505499328931,12.2,9.78363279994593));
#216482=CARTESIAN_POINT('Ctrl Pts',(4.76177026094788,12.2,9.78024910590453));
#216483=CARTESIAN_POINT('Ctrl Pts',(4.75850897115498,12.2,9.77687557777898));
#216484=CARTESIAN_POINT('Ctrl Pts',(4.75589993917847,12.2,9.77417675513147));
#216485=CARTESIAN_POINT('Ctrl Pts',(4.75330591112321,12.2,9.77148443923473));
#216486=CARTESIAN_POINT('Ctrl Pts',(4.75072689853919,12.2,9.7687987705888));
#216487=CARTESIAN_POINT('Ctrl Pts',(4.74814788630656,12.2,9.76611310230878));
#216488=CARTESIAN_POINT('Ctrl Pts',(4.74558389201512,12.2,9.76343408176174));
#216489=CARTESIAN_POINT('Ctrl Pts',(4.74303492759484,12.2,9.76076185067942));
#216490=CARTESIAN_POINT('Ctrl Pts',(4.74048596282725,12.2,9.758089619233));
#216491=CARTESIAN_POINT('Ctrl Pts',(4.73795202858875,12.2,9.7554241777688));
#216492=CARTESIAN_POINT('Ctrl Pts',(4.73543313928577,12.2,9.75276566979102));
#216493=CARTESIAN_POINT('Ctrl Pts',(4.732914250326,12.2,9.75010716217546));
#216494=CARTESIAN_POINT('Ctrl Pts',(4.73041040501321,12.2,9.74745558778629));
#216495=CARTESIAN_POINT('Ctrl Pts',(4.72792161738181,12.2,9.744811092724));
#216496=CARTESIAN_POINT('Ctrl Pts',(4.72543282941131,12.2,9.74216659730139));
#216497=CARTESIAN_POINT('Ctrl Pts',(4.72295909912665,12.2,9.73952918073676));
#216498=CARTESIAN_POINT('Ctrl Pts',(4.72050043898155,12.2,9.73689898824816));
#216499=CARTESIAN_POINT('Ctrl Pts',(4.71804177917144,12.2,9.73426879611794));
#216500=CARTESIAN_POINT('Ctrl Pts',(4.71559818880275,12.2,9.73164582986177));
#216501=CARTESIAN_POINT('Ctrl Pts',(4.71316968238862,12.2,9.72903023768594));
#216502=CARTESIAN_POINT('Ctrl Pts',(4.71074117564361,12.2,9.72641464515374));
#216503=CARTESIAN_POINT('Ctrl Pts',(4.70832775053337,12.2,9.72380642651948));
#216504=CARTESIAN_POINT('Ctrl Pts',(4.70592942179155,12.2,9.72120573126663));
#216505=CARTESIAN_POINT('Ctrl Pts',(4.70353109304973,12.2,9.71860503601378));
#216506=CARTESIAN_POINT('Ctrl Pts',(4.70114785910134,12.2,9.71601186439792));
#216507=CARTESIAN_POINT('Ctrl Pts',(4.69877973186271,12.2,9.7134263678689));
#216508=CARTESIAN_POINT('Ctrl Pts',(4.69641160494673,12.2,9.71084087169215));
#216509=CARTESIAN_POINT('Ctrl Pts',(4.69405858586547,12.2,9.70826305030053));
#216510=CARTESIAN_POINT('Ctrl Pts',(4.69172068493481,12.2,9.70569305677671));
#216511=CARTESIAN_POINT('Ctrl Pts',(4.68938278368562,12.2,9.70312306290272));
#216512=CARTESIAN_POINT('Ctrl Pts',(4.68706000179682,12.2,9.7005608968763));
#216513=CARTESIAN_POINT('Ctrl Pts',(4.68475235033926,12.2,9.69800671484902));
#216514=CARTESIAN_POINT('Ctrl Pts',(4.68244469919612,12.2,9.69545253316975));
#216515=CARTESIAN_POINT('Ctrl Pts',(4.68015217650101,12.2,9.69290633256723));
#216516=CARTESIAN_POINT('Ctrl Pts',(4.67787479668621,12.2,9.69036827244086));
#216517=CARTESIAN_POINT('Ctrl Pts',(4.67559741656112,12.2,9.68783021196868));
#216518=CARTESIAN_POINT('Ctrl Pts',(4.67333517723231,12.2,9.68530029061066));
#216519=CARTESIAN_POINT('Ctrl Pts',(4.67108808916556,12.2,9.68277866662575));
#216520=CARTESIAN_POINT('Ctrl Pts',(4.66884100140499,12.2,9.68025704298442));
#216521=CARTESIAN_POINT('Ctrl Pts',(4.6666090661566,12.2,9.67774371659783));
#216522=CARTESIAN_POINT('Ctrl Pts',(4.66439229244791,12.2,9.67523884774647));
#216523=CARTESIAN_POINT('Ctrl Pts',(4.66162132508552,12.2,9.67210776142629));
#216524=CARTESIAN_POINT('Ctrl Pts',(4.65887404823495,12.2,9.66898988992599));
#216525=CARTESIAN_POINT('Ctrl Pts',(4.65615048246981,12.2,9.66588554874472));
#216526=CARTESIAN_POINT('Ctrl Pts',(4.65342691670467,12.2,9.66278120756344));
#216527=CARTESIAN_POINT('Ctrl Pts',(4.6507270597358,12.2,9.65969039592677));
#216528=CARTESIAN_POINT('Ctrl Pts',(4.64805093375135,12.2,9.6566134364683));
#216529=CARTESIAN_POINT('Ctrl Pts',(4.64537480776689,12.2,9.65353647700981));
#216530=CARTESIAN_POINT('Ctrl Pts',(4.64272240943322,12.2,9.65047336971662));
#216531=CARTESIAN_POINT('Ctrl Pts',(4.64009375797488,12.2,9.64742443929995));
#216532=CARTESIAN_POINT('Ctrl Pts',(4.63746510651654,12.2,9.64437550888329));
#216533=CARTESIAN_POINT('Ctrl Pts',(4.63486020159988,12.2,9.64134075374995));
#216534=CARTESIAN_POINT('Ctrl Pts',(4.63227906076654,12.2,9.63832050749994));
#216535=CARTESIAN_POINT('Ctrl Pts',(4.6296979199332,12.2,9.63530026124993));
#216536=CARTESIAN_POINT('Ctrl Pts',(4.62714054270995,12.2,9.63229452091742));
#216537=CARTESIAN_POINT('Ctrl Pts',(4.62460694374017,12.2,9.62930362305665));
#216538=CARTESIAN_POINT('Ctrl Pts',(4.62207334477039,12.2,9.62631272519588));
#216539=CARTESIAN_POINT('Ctrl Pts',(4.61956352612509,12.2,9.62333666902227));
#216540=CARTESIAN_POINT('Ctrl Pts',(4.61707750057077,12.2,9.62037579402306));
#216541=CARTESIAN_POINT('Ctrl Pts',(4.61459147501646,12.2,9.61741491902385));
#216542=CARTESIAN_POINT('Ctrl Pts',(4.61212924506708,12.2,9.61446922775758));
#216543=CARTESIAN_POINT('Ctrl Pts',(4.60969082333222,12.2,9.61153906255007));
#216544=CARTESIAN_POINT('Ctrl Pts',(4.60725240159737,12.2,9.60860889734257));
#216545=CARTESIAN_POINT('Ctrl Pts',(4.60483778696246,12.2,9.60569425874612));
#216546=CARTESIAN_POINT('Ctrl Pts',(4.6024469944141,12.2,9.60279549763016));
#216547=CARTESIAN_POINT('Ctrl Pts',(4.5995780434603,12.2,9.59931698441738));
#216548=CARTESIAN_POINT('Ctrl Pts',(4.59674339658148,12.2,9.59586133460025));
#216549=CARTESIAN_POINT('Ctrl Pts',(4.59394307101654,12.2,9.59242916347494));
#216550=CARTESIAN_POINT('Ctrl Pts',(4.59160946629431,12.2,9.5895690207666));
#216551=CARTESIAN_POINT('Ctrl Pts',(4.58929969949227,12.2,9.58672518292228));
#216552=CARTESIAN_POINT('Ctrl Pts',(4.58701377719031,12.2,9.58389801200673));
#216553=CARTESIAN_POINT('Ctrl Pts',(4.58472785488834,12.2,9.58107084109118));
#216554=CARTESIAN_POINT('Ctrl Pts',(4.58246578114682,12.2,9.57826033739977));
#216555=CARTESIAN_POINT('Ctrl Pts',(4.5802275621203,12.2,9.57546686906734));
#216556=CARTESIAN_POINT('Ctrl Pts',(4.57798934309378,12.2,9.5726734007349));
#216557=CARTESIAN_POINT('Ctrl Pts',(4.57577498043331,12.2,9.56989696797427));
#216558=CARTESIAN_POINT('Ctrl Pts',(4.57358448307344,12.2,9.56713794533627));
#216559=CARTESIAN_POINT('Ctrl Pts',(4.57139398571357,12.2,9.56437892269829));
#216560=CARTESIAN_POINT('Ctrl Pts',(4.56922735380106,12.2,9.56163730840754));
#216561=CARTESIAN_POINT('Ctrl Pts',(4.56708459445956,12.2,9.55891348417547));
#216562=CARTESIAN_POINT('Ctrl Pts',(4.56494183511805,12.2,9.5561896599434));
#216563=CARTESIAN_POINT('Ctrl Pts',(4.56282294889613,12.2,9.55348362526355));
#216564=CARTESIAN_POINT('Ctrl Pts',(4.56072794146753,12.2,9.55079576693171));
#216565=CARTESIAN_POINT('Ctrl Pts',(4.55863293403893,12.2,9.54810790859987));
#216566=CARTESIAN_POINT('Ctrl Pts',(4.55656180451348,12.2,9.54543822606832));
#216567=CARTESIAN_POINT('Ctrl Pts',(4.55451456118211,12.2,9.54278711211152));
#216568=CARTESIAN_POINT('Ctrl Pts',(4.55205786927373,12.2,9.53960577547894));
#216569=CARTESIAN_POINT('Ctrl Pts',(4.54963557012329,12.2,9.53645117662313));
#216570=CARTESIAN_POINT('Ctrl Pts',(4.54724767312822,12.2,9.53332400982129));
#216571=CARTESIAN_POINT('Ctrl Pts',(4.54485977613314,12.2,9.53019684301944));
#216572=CARTESIAN_POINT('Ctrl Pts',(4.54250627931032,12.2,9.52709710346541));
#216573=CARTESIAN_POINT('Ctrl Pts',(4.54018718839309,12.2,9.52402550265912));
#216574=CARTESIAN_POINT('Ctrl Pts',(4.53786809747585,12.2,9.52095390185282));
#216575=CARTESIAN_POINT('Ctrl Pts',(4.53558341020743,12.2,9.51791043415431));
#216576=CARTESIAN_POINT('Ctrl Pts',(4.53333313220351,12.2,9.5148958245952));
#216577=CARTESIAN_POINT('Ctrl Pts',(4.53070780772933,12.2,9.51137877992701));
#216578=CARTESIAN_POINT('Ctrl Pts',(4.52812931492057,12.2,9.50790101067677));
#216579=CARTESIAN_POINT('Ctrl Pts',(4.52559765385162,12.2,9.50446368696895));
#216580=CARTESIAN_POINT('Ctrl Pts',(4.52342765876229,12.2,9.50151740965803));
#216581=CARTESIAN_POINT('Ctrl Pts',(4.5212920688216,12.2,9.49860084915342));
#216582=CARTESIAN_POINT('Ctrl Pts',(4.51919088272892,12.2,9.49571475883952));
#216583=CARTESIAN_POINT('Ctrl Pts',(4.51708969644538,12.2,9.49282866826346));
#216584=CARTESIAN_POINT('Ctrl Pts',(4.51502291173186,12.2,9.48997304831535));
#216585=CARTESIAN_POINT('Ctrl Pts',(4.51299052345593,12.2,9.48714866982946));
#216586=CARTESIAN_POINT('Ctrl Pts',(4.5109581353646,12.2,9.48432429160011));
#216587=CARTESIAN_POINT('Ctrl Pts',(4.50896014223842,12.2,9.48153115545513));
#216588=CARTESIAN_POINT('Ctrl Pts',(4.50699653530078,12.2,9.47877004829285));
#216589=CARTESIAN_POINT('Ctrl Pts',(4.50503292836314,12.2,9.47600894113057));
#216590=CARTESIAN_POINT('Ctrl Pts',(4.50310370746493,12.2,9.4732798645481));
#216591=CARTESIAN_POINT('Ctrl Pts',(4.5012088604481,12.2,9.47058362431049));
#216592=CARTESIAN_POINT('Ctrl Pts',(4.49931401325915,12.2,9.46788738382798));
#216593=CARTESIAN_POINT('Ctrl Pts',(4.49745353859021,12.2,9.46522397791527));
#216594=CARTESIAN_POINT('Ctrl Pts',(4.49562742240884,12.2,9.46259423460674));
#216595=CARTESIAN_POINT('Ctrl Pts',(4.49380130639334,12.2,9.45996449153708));
#216596=CARTESIAN_POINT('Ctrl Pts',(4.49200954664489,12.2,9.4573684092114));
#216597=CARTESIAN_POINT('Ctrl Pts',(4.49025212653402,12.2,9.45480683420942));
#216598=CARTESIAN_POINT('Ctrl Pts',(4.48849470642314,12.2,9.45224525920745));
#216599=CARTESIAN_POINT('Ctrl Pts',(4.48677162418329,12.2,9.44971818978343));
#216600=CARTESIAN_POINT('Ctrl Pts',(4.48508285815897,12.2,9.44722649103819));
#216601=CARTESIAN_POINT('Ctrl Pts',(4.48339409198124,12.2,9.44473479206662));
#216602=CARTESIAN_POINT('Ctrl Pts',(4.48173964192714,12.2,9.44227846338324));
#216603=CARTESIAN_POINT('Ctrl Pts',(4.48011948259323,12.2,9.43985839329923));
#216604=CARTESIAN_POINT('Ctrl Pts',(4.47849932340649,12.2,9.43743832343503));
#216605=CARTESIAN_POINT('Ctrl Pts',(4.47691345301017,12.2,9.435054510098));
#216606=CARTESIAN_POINT('Ctrl Pts',(4.47536184573321,12.2,9.43270786251658));
#216607=CARTESIAN_POINT('Ctrl Pts',(4.47381023845626,12.2,9.43036121493518));
#216608=CARTESIAN_POINT('Ctrl Pts',(4.47229289187397,12.2,9.42805173368623));
#216609=CARTESIAN_POINT('Ctrl Pts',(4.47080977093511,12.2,9.42578034815307));
#216610=CARTESIAN_POINT('Ctrl Pts',(4.46932664986153,12.2,9.42350896241359));
#216611=CARTESIAN_POINT('Ctrl Pts',(4.46787775982046,12.2,9.42127567471935));
#216612=CARTESIAN_POINT('Ctrl Pts',(4.46646305857902,12.2,9.41908144001909));
#216613=CARTESIAN_POINT('Ctrl Pts',(4.46504835746609,12.2,9.41688720551812));
#216614=CARTESIAN_POINT('Ctrl Pts',(4.46366784748975,12.2,9.41473202373166));
#216615=CARTESIAN_POINT('Ctrl Pts',(4.46232148819927,12.2,9.41261687446562));
#216616=CARTESIAN_POINT('Ctrl Pts',(4.4609751289088,12.2,9.41050172519959));
#216617=CARTESIAN_POINT('Ctrl Pts',(4.45966291889973,12.2,9.40842661078881));
#216618=CARTESIAN_POINT('Ctrl Pts',(4.45838481386135,12.2,9.40639253836094));
#216619=CARTESIAN_POINT('Ctrl Pts',(4.45710670870688,12.2,9.40435846574831));
#216620=CARTESIAN_POINT('Ctrl Pts',(4.45586271009828,12.2,9.4023654325407));
#216621=CARTESIAN_POINT('Ctrl Pts',(4.45465276586801,12.2,9.4004144772706));
#216622=CARTESIAN_POINT('Ctrl Pts',(4.45344282174763,12.2,9.39846352217771));
#216623=CARTESIAN_POINT('Ctrl Pts',(4.45226693457815,12.2,9.39655464356205));
#216624=CARTESIAN_POINT('Ctrl Pts',(4.45112504845446,12.2,9.39468890563175));
#216625=CARTESIAN_POINT('Ctrl Pts',(4.44998316233077,12.2,9.39282316770143));
#216626=CARTESIAN_POINT('Ctrl Pts',(4.44887527936268,12.2,9.39100057111765));
#216627=CARTESIAN_POINT('Ctrl Pts',(4.44780133831689,12.2,9.38922220934701));
#216628=CARTESIAN_POINT('Ctrl Pts',(4.44672739727111,12.2,9.38744384757638));
#216629=CARTESIAN_POINT('Ctrl Pts',(4.44568740268365,12.2,9.38570972190072));
#216630=CARTESIAN_POINT('Ctrl Pts',(4.44468128663456,12.2,9.38402095920899));
#216631=CARTESIAN_POINT('Ctrl Pts',(4.44317694109225,12.2,9.38149591984635));
#216632=CARTESIAN_POINT('Ctrl Pts',(4.44174833406917,12.2,9.37907228215719));
#216633=CARTESIAN_POINT('Ctrl Pts',(4.44039525799994,12.2,9.37675396799998));
#216634=CARTESIAN_POINT('Ctrl Pts',(4.44039525799994,15.2,9.37675396799998));
#216635=CARTESIAN_POINT('Ctrl Pts',(4.44129586096445,15.2,9.37829703024913));
#216636=CARTESIAN_POINT('Ctrl Pts',(4.44222992819487,15.2,9.37988675810253));
#216637=CARTESIAN_POINT('Ctrl Pts',(4.44319751513558,15.2,9.38152198206248));
#216638=CARTESIAN_POINT('Ctrl Pts',(4.44416976826961,15.2,9.38316509189892));
#216639=CARTESIAN_POINT('Ctrl Pts',(4.4451758658233,15.2,9.38485414143403));
#216640=CARTESIAN_POINT('Ctrl Pts',(4.44621587810058,15.2,9.38658798545109));
#216641=CARTESIAN_POINT('Ctrl Pts',(4.4472558902834,15.2,9.38832182931068));
#216642=CARTESIAN_POINT('Ctrl Pts',(4.44832981474848,15.2,9.39010046854946));
#216643=CARTESIAN_POINT('Ctrl Pts',(4.44943771295822,15.2,9.39192279148324));
#216644=CARTESIAN_POINT('Ctrl Pts',(4.45054561116795,15.2,9.39374511441702));
#216645=CARTESIAN_POINT('Ctrl Pts',(4.45168748333048,15.2,9.39561112227516));
#216646=CARTESIAN_POINT('Ctrl Pts',(4.45286338542788,15.2,9.39751973529871));
#216647=CARTESIAN_POINT('Ctrl Pts',(4.45403928763209,15.2,9.39942834849564));
#216648=CARTESIAN_POINT('Ctrl Pts',(4.45524921742371,15.2,9.40137956636406));
#216649=CARTESIAN_POINT('Ctrl Pts',(4.45649322957716,15.2,9.40337233972547));
#216650=CARTESIAN_POINT('Ctrl Pts',(4.4577372416176,15.2,9.40536511290588));
#216651=CARTESIAN_POINT('Ctrl Pts',(4.45901533463377,15.2,9.40739944247505));
#216652=CARTESIAN_POINT('Ctrl Pts',(4.46032755500882,15.2,9.40947430399253));
#216653=CARTESIAN_POINT('Ctrl Pts',(4.46163977538387,15.2,9.41154916551003));
#216654=CARTESIAN_POINT('Ctrl Pts',(4.4629861253431,15.2,9.413664564196));
#216655=CARTESIAN_POINT('Ctrl Pts',(4.46436664545812,15.2,9.41581950061597));
#216656=CARTESIAN_POINT('Ctrl Pts',(4.46574716569854,15.2,9.41797443723169));
#216657=CARTESIAN_POINT('Ctrl Pts',(4.46716185739318,15.2,9.42016891470231));
#216658=CARTESIAN_POINT('Ctrl Pts',(4.46861075764116,15.2,9.42240196349333));
#216659=CARTESIAN_POINT('Ctrl Pts',(4.47005965775753,15.2,9.42463501208152));
#216660=CARTESIAN_POINT('Ctrl Pts',(4.47154276904471,15.2,9.42690663270821));
#216661=CARTESIAN_POINT('Ctrl Pts',(4.47306012507439,15.2,9.42921588212593));
#216662=CARTESIAN_POINT('Ctrl Pts',(4.47457748110407,15.2,9.43152513154365));
#216663=CARTESIAN_POINT('Ctrl Pts',(4.47612908118104,15.2,9.43387200857503));
#216664=CARTESIAN_POINT('Ctrl Pts',(4.47771495737194,15.2,9.43625559515351));
#216665=CARTESIAN_POINT('Ctrl Pts',(4.47930083356283,15.2,9.43863918173199));
#216666=CARTESIAN_POINT('Ctrl Pts',(4.48092098619868,15.2,9.4410594736239));
#216667=CARTESIAN_POINT('Ctrl Pts',(4.48257544230289,15.2,9.44351558119889));
#216668=CARTESIAN_POINT('Ctrl Pts',(4.48422989855739,15.2,9.44597168899697));
#216669=CARTESIAN_POINT('Ctrl Pts',(4.48591865848186,15.2,9.44846360505688));
#216670=CARTESIAN_POINT('Ctrl Pts',(4.48764174657727,15.2,9.45099045911279));
#216671=CARTESIAN_POINT('Ctrl Pts',(4.48936483451616,15.2,9.45351731293916));
#216672=CARTESIAN_POINT('Ctrl Pts',(4.49112224943113,15.2,9.4560791013147));
#216673=CARTESIAN_POINT('Ctrl Pts',(4.49291401345741,15.2,9.45867497223209));
#216674=CARTESIAN_POINT('Ctrl Pts',(4.49470577748369,15.2,9.46127084314946));
#216675=CARTESIAN_POINT('Ctrl Pts',(4.49653188877539,15.2,9.46390079565037));
#216676=CARTESIAN_POINT('Ctrl Pts',(4.49839236678877,15.2,9.46656399296798));
#216677=CARTESIAN_POINT('Ctrl Pts',(4.50025284497113,15.2,9.4692271905275));
#216678=CARTESIAN_POINT('Ctrl Pts',(4.50214768849854,15.2,9.47192363600699));
#216679=CARTESIAN_POINT('Ctrl Pts',(4.50407691260518,15.2,9.47465251140713));
#216680=CARTESIAN_POINT('Ctrl Pts',(4.50600613653657,15.2,9.47738138655938));
#216681=CARTESIAN_POINT('Ctrl Pts',(4.50796974130426,15.2,9.48014269284589));
#216682=CARTESIAN_POINT('Ctrl Pts',(4.50996773632398,15.2,9.482935633007));
#216683=CARTESIAN_POINT('Ctrl Pts',(4.51196573134371,15.2,9.48572857316812));
#216684=CARTESIAN_POINT('Ctrl Pts',(4.51399811724373,15.2,9.48855314519458));
#216685=CARTESIAN_POINT('Ctrl Pts',(4.51606490324962,15.2,9.49140857242204));
#216686=CARTESIAN_POINT('Ctrl Pts',(4.51813168944324,15.2,9.49426399990887));
#216687=CARTESIAN_POINT('Ctrl Pts',(4.52023287545651,15.2,9.49715028053412));
#216688=CARTESIAN_POINT('Ctrl Pts',(4.52236846493156,15.2,9.50006665325712));
#216689=CARTESIAN_POINT('Ctrl Pts',(4.52450405421262,15.2,9.50298302571523));
#216690=CARTESIAN_POINT('Ctrl Pts',(4.52667405002997,15.2,9.50592948849973));
#216691=CARTESIAN_POINT('Ctrl Pts',(4.52887845194988,15.2,9.50890529697493));
#216692=CARTESIAN_POINT('Ctrl Pts',(4.53108285386978,15.2,9.51188110545013));
#216693=CARTESIAN_POINT('Ctrl Pts',(4.53332166255942,15.2,9.51488625826685));
#216694=CARTESIAN_POINT('Ctrl Pts',(4.53559487950507,15.2,9.5179200259732));
#216695=CARTESIAN_POINT('Ctrl Pts',(4.53824696607933,15.2,9.52145942181432));
#216696=CARTESIAN_POINT('Ctrl Pts',(4.54094588222936,15.2,9.52503776449918));
#216697=CARTESIAN_POINT('Ctrl Pts',(4.54369162750822,15.2,9.52865391895827));
#216698=CARTESIAN_POINT('Ctrl Pts',(4.54604512333937,15.2,9.53175347976232));
#216699=CARTESIAN_POINT('Ctrl Pts',(4.54843302198461,15.2,9.53488082217843));
#216700=CARTESIAN_POINT('Ctrl Pts',(4.55085531901565,15.2,9.53803524796986));
#216701=CARTESIAN_POINT('Ctrl Pts',(4.55287389994818,15.2,9.5406639362249));
#216702=CARTESIAN_POINT('Ctrl Pts',(4.55491636724948,15.2,9.5433114314989));
#216703=CARTESIAN_POINT('Ctrl Pts',(4.55698271808156,15.2,9.54597733656737));
#216704=CARTESIAN_POINT('Ctrl Pts',(4.55904906891363,15.2,9.54864324163583));
#216705=CARTESIAN_POINT('Ctrl Pts',(4.56113930236859,15.2,9.55132755895761));
#216706=CARTESIAN_POINT('Ctrl Pts',(4.56325341160343,15.2,9.55402989708165));
#216707=CARTESIAN_POINT('Ctrl Pts',(4.56579034259306,15.2,9.55727270271265));
#216708=CARTESIAN_POINT('Ctrl Pts',(4.56836165881291,15.2,9.56054145658733));
#216709=CARTESIAN_POINT('Ctrl Pts',(4.57096734271587,15.2,9.56383549838256));
#216710=CARTESIAN_POINT('Ctrl Pts',(4.57313874604725,15.2,9.56658053331167));
#216711=CARTESIAN_POINT('Ctrl Pts',(4.57533401857269,15.2,9.56934312933219));
#216712=CARTESIAN_POINT('Ctrl Pts',(4.5775531510013,15.2,9.57212290863635));
#216713=CARTESIAN_POINT('Ctrl Pts',(4.57977228342991,15.2,9.57490268794052));
#216714=CARTESIAN_POINT('Ctrl Pts',(4.58201527541966,15.2,9.57769965287838));
#216715=CARTESIAN_POINT('Ctrl Pts',(4.58428211796182,15.2,9.5805134306567));
#216716=CARTESIAN_POINT('Ctrl Pts',(4.58654896050399,15.2,9.58332720843501));
#216717=CARTESIAN_POINT('Ctrl Pts',(4.58883965464435,15.2,9.58615780035358));
#216718=CARTESIAN_POINT('Ctrl Pts',(4.59115418790699,15.2,9.58900484125551));
#216719=CARTESIAN_POINT('Ctrl Pts',(4.59346872116964,15.2,9.59185188215743));
#216720=CARTESIAN_POINT('Ctrl Pts',(4.59580709517458,15.2,9.59471537239036));
#216721=CARTESIAN_POINT('Ctrl Pts',(4.59816929760388,15.2,9.59759495252839));
#216722=CARTESIAN_POINT('Ctrl Pts',(4.60053150003318,15.2,9.60047453266643));
#216723=CARTESIAN_POINT('Ctrl Pts',(4.60291753218211,15.2,9.60337020335182));
#216724=CARTESIAN_POINT('Ctrl Pts',(4.60532737899857,15.2,9.60628161024002));
#216725=CARTESIAN_POINT('Ctrl Pts',(4.60773722581503,15.2,9.60919301712823));
#216726=CARTESIAN_POINT('Ctrl Pts',(4.61017089048876,15.2,9.61212016044438));
#216727=CARTESIAN_POINT('Ctrl Pts',(4.61262835701655,15.2,9.61506269224995));
#216728=CARTESIAN_POINT('Ctrl Pts',(4.61606881020903,15.2,9.6191822368419));
#216729=CARTESIAN_POINT('Ctrl Pts',(4.61955591681464,15.2,9.62333194003229));
#216730=CARTESIAN_POINT('Ctrl Pts',(4.62308963828464,15.2,9.62751086807151));
#216731=CARTESIAN_POINT('Ctrl Pts',(4.62561372500964,15.2,9.63049581662447));
#216732=CARTESIAN_POINT('Ctrl Pts',(4.62816159339544,15.2,9.63349567338195));
#216733=CARTESIAN_POINT('Ctrl Pts',(4.63073322832793,15.2,9.6365101036609));
#216734=CARTESIAN_POINT('Ctrl Pts',(4.63330486326042,15.2,9.63952453393987));
#216735=CARTESIAN_POINT('Ctrl Pts',(4.63590026575164,15.2,9.64255353824684));
#216736=CARTESIAN_POINT('Ctrl Pts',(4.63851941735081,15.2,9.64559678512302));
#216737=CARTESIAN_POINT('Ctrl Pts',(4.64113856894998,15.2,9.64864003199919));
#216738=CARTESIAN_POINT('Ctrl Pts',(4.64378147109676,15.2,9.65169752175614));
#216739=CARTESIAN_POINT('Ctrl Pts',(4.64644810589035,15.2,9.65476892641003));
#216740=CARTESIAN_POINT('Ctrl Pts',(4.64911474039328,15.2,9.65784033072913));
#216741=CARTESIAN_POINT('Ctrl Pts',(4.65180510653709,15.2,9.66092565371126));
#216742=CARTESIAN_POINT('Ctrl Pts',(4.65451918762822,15.2,9.66402456955295));
#216743=CARTESIAN_POINT('Ctrl Pts',(4.65723326901519,15.2,9.66712348573241));
#216744=CARTESIAN_POINT('Ctrl Pts',(4.65997106375728,15.2,9.67023599479217));
#216745=CARTESIAN_POINT('Ctrl Pts',(4.66273255438036,15.2,9.67336178333277));
#216746=CARTESIAN_POINT('Ctrl Pts',(4.66494174699921,15.2,9.67586241430154));
#216747=CARTESIAN_POINT('Ctrl Pts',(4.66716610339692,15.2,9.67837154230579));
#216748=CARTESIAN_POINT('Ctrl Pts',(4.66940561475142,15.2,9.68088900751001));
#216749=CARTESIAN_POINT('Ctrl Pts',(4.67164512580078,15.2,9.68340647237122));
#216750=CARTESIAN_POINT('Ctrl Pts',(4.67389979117421,15.2,9.68593227509919));
#216751=CARTESIAN_POINT('Ctrl Pts',(4.67616960015378,15.2,9.68846625533565));
#216752=CARTESIAN_POINT('Ctrl Pts',(4.6784394094426,15.2,9.69100023591736));
#216753=CARTESIAN_POINT('Ctrl Pts',(4.68072436322175,15.2,9.69354239602485));
#216754=CARTESIAN_POINT('Ctrl Pts',(4.68302444929155,15.2,9.69609257777496));
#216755=CARTESIAN_POINT('Ctrl Pts',(4.6858995567221,15.2,9.69928030478884));
#216756=CARTESIAN_POINT('Ctrl Pts',(4.68879830853259,15.2,9.7024805646093));
#216757=CARTESIAN_POINT('Ctrl Pts',(4.69172068493481,15.2,9.70569305677671));
#216758=CARTESIAN_POINT('Ctrl Pts',(4.69405858586547,15.2,9.70826305030053));
#216759=CARTESIAN_POINT('Ctrl Pts',(4.69641160494672,15.2,9.71084087169215));
#216760=CARTESIAN_POINT('Ctrl Pts',(4.6987797318627,15.2,9.7134263678689));
#216761=CARTESIAN_POINT('Ctrl Pts',(4.70114785910134,15.2,9.71601186439792));
#216762=CARTESIAN_POINT('Ctrl Pts',(4.70353109304973,15.2,9.71860503601378));
#216763=CARTESIAN_POINT('Ctrl Pts',(4.70592942179154,15.2,9.72120573126662));
#216764=CARTESIAN_POINT('Ctrl Pts',(4.70892733255542,15.2,9.7244566001555));
#216765=CARTESIAN_POINT('Ctrl Pts',(4.71194883064877,15.2,9.72771922445351));
#216766=CARTESIAN_POINT('Ctrl Pts',(4.71499388975988,15.2,9.73099331176007));
#216767=CARTESIAN_POINT('Ctrl Pts',(4.71803894887099,15.2,9.73426739906664));
#216768=CARTESIAN_POINT('Ctrl Pts',(4.72110757203435,15.2,9.73755295130394));
#216769=CARTESIAN_POINT('Ctrl Pts',(4.72419973099392,15.2,9.74084967616563));
#216770=CARTESIAN_POINT('Ctrl Pts',(4.72667345795934,15.2,9.74348705583938));
#216771=CARTESIAN_POINT('Ctrl Pts',(4.72916224867453,15.2,9.7461315879367));
#216772=CARTESIAN_POINT('Ctrl Pts',(4.73166609035718,15.2,9.7487831261081));
#216773=CARTESIAN_POINT('Ctrl Pts',(4.73416993238098,15.2,9.75143466464077));
#216774=CARTESIAN_POINT('Ctrl Pts',(4.73668882432696,15.2,9.7540932086555));
#216775=CARTESIAN_POINT('Ctrl Pts',(4.73922275497661,15.2,9.75675861403511));
#216776=CARTESIAN_POINT('Ctrl Pts',(4.74175668528101,15.2,9.75942401905156));
#216777=CARTESIAN_POINT('Ctrl Pts',(4.74430565323905,15.2,9.76209628610942));
#216778=CARTESIAN_POINT('Ctrl Pts',(4.74686964430567,15.2,9.76477527111195));
#216779=CARTESIAN_POINT('Ctrl Pts',(4.74943363572164,15.2,9.76745425647947));
#216780=CARTESIAN_POINT('Ctrl Pts',(4.75201265215018,15.2,9.77013996059767));
#216781=CARTESIAN_POINT('Ctrl Pts',(4.75460667745821,15.2,9.77283224129996));
#216782=CARTESIAN_POINT('Ctrl Pts',(4.75720070276625,15.2,9.77552452200223));
#216783=CARTESIAN_POINT('Ctrl Pts',(4.75980973826216,15.2,9.77822337934974));
#216784=CARTESIAN_POINT('Ctrl Pts',(4.76243376962892,15.2,9.78092867394228));
#216785=CARTESIAN_POINT('Ctrl Pts',(4.76505780063815,15.2,9.78363396816621));
#216786=CARTESIAN_POINT('Ctrl Pts',(4.76769682747524,15.2,9.78634569853296));
#216787=CARTESIAN_POINT('Ctrl Pts',(4.77035083571475,15.2,9.78906372748978));
#216788=CARTESIAN_POINT('Ctrl Pts',(4.77300484431586,15.2,9.79178175681692));
#216789=CARTESIAN_POINT('Ctrl Pts',(4.77567383341869,15.2,9.79450608352196));
#216790=CARTESIAN_POINT('Ctrl Pts',(4.77835778945539,15.2,9.79723657150473));
#216791=CARTESIAN_POINT('Ctrl Pts',(4.7810417451264,15.2,9.79996705911548));
#216792=CARTESIAN_POINT('Ctrl Pts',(4.78374066790933,15.2,9.80270370614763));
#216793=CARTESIAN_POINT('Ctrl Pts',(4.78645454151983,15.2,9.80544637853414));
#216794=CARTESIAN_POINT('Ctrl Pts',(4.78984688381027,15.2,9.80887471929753));
#216795=CARTESIAN_POINT('Ctrl Pts',(4.79326258814358,15.2,9.81231247312135));
#216796=CARTESIAN_POINT('Ctrl Pts',(4.79670162454801,15.2,9.81575937799808));
#216797=CARTESIAN_POINT('Ctrl Pts',(4.79945285382151,15.2,9.81851690204976));
#216798=CARTESIAN_POINT('Ctrl Pts',(4.80221901512927,15.2,9.8212802809762));
#216799=CARTESIAN_POINT('Ctrl Pts',(4.80500009317127,15.2,9.82404938496105));
#216800=CARTESIAN_POINT('Ctrl Pts',(4.8084764405343,15.2,9.82751076475346));
#216801=CARTESIAN_POINT('Ctrl Pts',(4.81197609696989,15.2,9.83098108580431));
#216802=CARTESIAN_POINT('Ctrl Pts',(4.8154990277357,15.2,9.83446009247169));
#216803=CARTESIAN_POINT('Ctrl Pts',(4.8190219581175,15.2,9.83793909875986));
#216804=CARTESIAN_POINT('Ctrl Pts',(4.82256816631288,15.2,9.84142679066334));
#216805=CARTESIAN_POINT('Ctrl Pts',(4.82613761828301,15.2,9.84492291430934));
#216806=CARTESIAN_POINT('Ctrl Pts',(4.82899318032599,15.2,9.84771981368343));
#216807=CARTESIAN_POINT('Ctrl Pts',(4.83186361936764,15.2,9.85052210777751));
#216808=CARTESIAN_POINT('Ctrl Pts',(4.83474891802488,15.2,9.85332967054163));
#216809=CARTESIAN_POINT('Ctrl Pts',(4.83763421668212,15.2,9.85613723330575));
#216810=CARTESIAN_POINT('Ctrl Pts',(4.84053437637169,15.2,9.85895006197329));
#216811=CARTESIAN_POINT('Ctrl Pts',(4.8434493789765,15.2,9.86176803146071));
#216812=CARTESIAN_POINT('Ctrl Pts',(4.84636438118414,15.2,9.86458600056417));
#216813=CARTESIAN_POINT('Ctrl Pts',(4.8492942270482,15.2,9.86740911033366));
#216814=CARTESIAN_POINT('Ctrl Pts',(4.85223889875097,15.2,9.87023723276882));
#216815=CARTESIAN_POINT('Ctrl Pts',(4.85665590650573,15.2,9.87447941661421));
#216816=CARTESIAN_POINT('Ctrl Pts',(4.86110627421804,15.2,9.87873287995751));
#216817=CARTESIAN_POINT('Ctrl Pts',(4.86558994280284,15.2,9.88299720280182));
#216818=CARTESIAN_POINT('Ctrl Pts',(4.86932633342592,15.2,9.88655080530119));
#216819=CARTESIAN_POINT('Ctrl Pts',(4.87308584981257,15.2,9.89011194773937));
#216820=CARTESIAN_POINT('Ctrl Pts',(4.87686845800512,15.2,9.89368039030822));
#216821=CARTESIAN_POINT('Ctrl Pts',(4.88065106619768,15.2,9.89724883287706));
#216822=CARTESIAN_POINT('Ctrl Pts',(4.88445676508805,15.2,9.90082457442224));
#216823=CARTESIAN_POINT('Ctrl Pts',(4.88828552159717,15.2,9.90440737876741));
#216824=CARTESIAN_POINT('Ctrl Pts',(4.8913485269714,15.2,9.90727362239975));
#216825=CARTESIAN_POINT('Ctrl Pts',(4.89442628799722,15.2,9.91014438511696));
#216826=CARTESIAN_POINT('Ctrl Pts',(4.89751878677784,15.2,9.91301954671838));
#216827=CARTESIAN_POINT('Ctrl Pts',(4.90061128513711,15.2,9.91589470792809));
#216828=CARTESIAN_POINT('Ctrl Pts',(4.90371852174617,15.2,9.91877426834242));
#216829=CARTESIAN_POINT('Ctrl Pts',(4.90684047848945,15.2,9.92165810699513));
#216830=CARTESIAN_POINT('Ctrl Pts',(4.91074292473758,15.2,9.9252629056057));
#216831=CARTESIAN_POINT('Ctrl Pts',(4.91466836974595,15.2,9.92887439220526));
#216832=CARTESIAN_POINT('Ctrl Pts',(4.91861677806661,15.2,9.93249233183));
#216833=CARTESIAN_POINT('Ctrl Pts',(4.9217755048953,15.2,9.93538668368754));
#216834=CARTESIAN_POINT('Ctrl Pts',(4.92494892836094,15.2,9.93828516656772));
#216835=CARTESIAN_POINT('Ctrl Pts',(4.92813702903565,15.2,9.94118766350395));
#216836=CARTESIAN_POINT('Ctrl Pts',(4.93132512927599,15.2,9.94409016004472));
#216837=CARTESIAN_POINT('Ctrl Pts',(4.93452790748004,15.2,9.94699667113466));
#216838=CARTESIAN_POINT('Ctrl Pts',(4.93774534371551,15.2,9.94990707900746));
#216839=CARTESIAN_POINT('Ctrl Pts',(4.94096278038937,15.2,9.95281748727679));
#216840=CARTESIAN_POINT('Ctrl Pts',(4.94419487580203,15.2,9.95573179223521));
#216841=CARTESIAN_POINT('Ctrl Pts',(4.94744161049377,15.2,9.95864988051863));
#216842=CARTESIAN_POINT('Ctrl Pts',(4.95068834474315,15.2,9.96156796840446));
#216843=CARTESIAN_POINT('Ctrl Pts',(4.95394971775303,15.2,9.96448983825286));
#216844=CARTESIAN_POINT('Ctrl Pts',(4.95722571120594,15.2,9.96741537551332));
#216845=CARTESIAN_POINT('Ctrl Pts',(4.96132070335684,15.2,9.97107229738784));
#216846=CARTESIAN_POINT('Ctrl Pts',(4.96543853908239,15.2,9.97473495087619));
#216847=CARTESIAN_POINT('Ctrl Pts',(4.96957917894163,15.2,9.97840311448684));
#216848=CARTESIAN_POINT('Ctrl Pts',(4.97289169100955,15.2,9.98133764553529));
#216849=CARTESIAN_POINT('Ctrl Pts',(4.97621879890759,15.2,9.98427570356997));
#216850=CARTESIAN_POINT('Ctrl Pts',(4.97956048149383,15.2,9.98721717524365));
#216851=CARTESIAN_POINT('Ctrl Pts',(4.98290216362477,15.2,9.99015864651655));
#216852=CARTESIAN_POINT('Ctrl Pts',(4.98625842227304,15.2,9.99310353262039));
#216853=CARTESIAN_POINT('Ctrl Pts',(4.98962923394043,15.2,9.99605172126794));
#216854=CARTESIAN_POINT('Ctrl Pts',(4.99215734326506,15.2,9.99826286325571));
#216855=CARTESIAN_POINT('Ctrl Pts',(4.99469364095036,15.2,10.000475864294));
#216856=CARTESIAN_POINT('Ctrl Pts',(4.99723811711292,15.2,10.0026906762411));
#216857=CARTESIAN_POINT('Ctrl Pts',(4.99978259281324,15.2,10.0049054877859));
#216858=CARTESIAN_POINT('Ctrl Pts',(5.00233524613814,15.2,10.0071221102223));
#216859=CARTESIAN_POINT('Ctrl Pts',(5.00489607079583,15.2,10.0093404982668));
#216860=CARTESIAN_POINT('Ctrl Pts',(5.00916411204702,15.2,10.0130378118087));
#216861=CARTESIAN_POINT('Ctrl Pts',(5.01345484510585,15.2,10.0167400291948));
#216862=CARTESIAN_POINT('Ctrl Pts',(5.01776823497569,15.2,10.020446937922));
#216863=CARTESIAN_POINT('Ctrl Pts',(5.02121894658947,15.2,10.0234124646613));
#216864=CARTESIAN_POINT('Ctrl Pts',(5.02468415591764,15.2,10.0263809927113));
#216865=CARTESIAN_POINT('Ctrl Pts',(5.02816384396556,15.2,10.0293524160238));
#216866=CARTESIAN_POINT('Ctrl Pts',(5.03164353248757,15.2,10.0323238397411));
#216867=CARTESIAN_POINT('Ctrl Pts',(5.03513769823358,15.2,10.0352981583476));
#216868=CARTESIAN_POINT('Ctrl Pts',(5.03864632153686,15.2,10.03827526351));
#216869=CARTESIAN_POINT('Ctrl Pts',(5.04127778877529,15.2,10.0405080921791));
#216870=CARTESIAN_POINT('Ctrl Pts',(5.04391738723644,15.2,10.0427424896064));
#216871=CARTESIAN_POINT('Ctrl Pts',(5.04656510898563,15.2,10.044978410202));
#216872=CARTESIAN_POINT('Ctrl Pts',(5.04921283073482,15.2,10.0472143307976));
#216873=CARTESIAN_POINT('Ctrl Pts',(5.05186867604886,15.2,10.0494517744525));
#216874=CARTESIAN_POINT('Ctrl Pts',(5.0545326352558,15.2,10.0516906975063));
#216875=CARTESIAN_POINT('Ctrl Pts',(5.05719659446274,15.2,10.0539296205601));
#216876=CARTESIAN_POINT('Ctrl Pts',(5.0598686672393,15.2,10.0561700222872));
#216877=CARTESIAN_POINT('Ctrl Pts',(5.06254884547455,15.2,10.0584118579973));
#216878=CARTESIAN_POINT('Ctrl Pts',(5.0652290237098,15.2,10.0606536937074));
#216879=CARTESIAN_POINT('Ctrl Pts',(5.06791730711116,15.2,10.0628969655924));
#216880=CARTESIAN_POINT('Ctrl Pts',(5.07061368588708,15.2,10.0651416272606));
#216881=CARTESIAN_POINT('Ctrl Pts',(5.0751076506769,15.2,10.068882730177));
#216882=CARTESIAN_POINT('Ctrl Pts',(5.07962410405897,15.2,10.0726276958612));
#216883=CARTESIAN_POINT('Ctrl Pts',(5.0841630040064,15.2,10.0763763222982));
#216884=CARTESIAN_POINT('Ctrl Pts',(5.08688634387591,15.2,10.0786254980787));
#216885=CARTESIAN_POINT('Ctrl Pts',(5.08961776491998,15.2,10.0808759921577));
#216886=CARTESIAN_POINT('Ctrl Pts',(5.09235725619435,15.2,10.0831277607841));
#216887=CARTESIAN_POINT('Ctrl Pts',(5.09509674796639,15.2,10.0853795298195));
#216888=CARTESIAN_POINT('Ctrl Pts',(5.09784431064905,15.2,10.087632573747));
#216889=CARTESIAN_POINT('Ctrl Pts',(5.10059993634229,15.2,10.0898868497414));
#216890=CARTESIAN_POINT('Ctrl Pts',(5.10427410309893,15.2,10.0928925503848));
#216891=CARTESIAN_POINT('Ctrl Pts',(5.10796260106763,15.2,10.0959004401946));
#216892=CARTESIAN_POINT('Ctrl Pts',(5.11166541043065,15.2,10.0989104195039));
#216893=CARTESIAN_POINT('Ctrl Pts',(5.11444251757904,15.2,10.1011679040885));
#216894=CARTESIAN_POINT('Ctrl Pts',(5.11722767394358,15.2,10.1034265623563));
#216895=CARTESIAN_POINT('Ctrl Pts',(5.12002087017431,15.2,10.1056863534823));
#216896=CARTESIAN_POINT('Ctrl Pts',(5.12374513215358,15.2,10.1086994085908));
#216897=CARTESIAN_POINT('Ctrl Pts',(5.12748368738361,15.2,10.1117144781433));
#216898=CARTESIAN_POINT('Ctrl Pts',(5.13123651399412,15.2,10.1147314600437));
#216899=CARTESIAN_POINT('Ctrl Pts',(5.13405113369634,15.2,10.1169941962634));
#216900=CARTESIAN_POINT('Ctrl Pts',(5.13687378073734,15.2,10.1192580093033));
#216901=CARTESIAN_POINT('Ctrl Pts',(5.13970444548066,15.2,10.1215228564813));
#216902=CARTESIAN_POINT('Ctrl Pts',(5.14253511022397,15.2,10.1237877036593));
#216903=CARTESIAN_POINT('Ctrl Pts',(5.14537379292719,15.2,10.1260535848853));
#216904=CARTESIAN_POINT('Ctrl Pts',(5.1482204836564,15.2,10.1283204594696));
#216905=CARTESIAN_POINT('Ctrl Pts',(5.15106717438561,15.2,10.1305873340538));
#216906=CARTESIAN_POINT('Ctrl Pts',(5.15392187338094,15.2,10.1328552009379));
#216907=CARTESIAN_POINT('Ctrl Pts',(5.15678457060916,15.2,10.135124020022));
#216908=CARTESIAN_POINT('Ctrl Pts',(5.16060150059348,15.2,10.1381491124089));
#216909=CARTESIAN_POINT('Ctrl Pts',(5.16443265058931,15.2,10.1411758958205));
#216910=CARTESIAN_POINT('Ctrl Pts',(5.16827799776085,15.2,10.144204274277));
#216911=CARTESIAN_POINT('Ctrl Pts',(5.17212334440845,15.2,10.147232652321));
#216912=CARTESIAN_POINT('Ctrl Pts',(5.17598288599022,15.2,10.1502626236329));
#216913=CARTESIAN_POINT('Ctrl Pts',(5.17985660211654,15.2,10.153294092996));
#216914=CARTESIAN_POINT('Ctrl Pts',(5.18373031877066,15.2,10.1563255627722));
#216915=CARTESIAN_POINT('Ctrl Pts',(5.18761820836222,15.2,10.1593585295041));
#216916=CARTESIAN_POINT('Ctrl Pts',(5.19152024774155,15.2,10.162392898725));
#216917=CARTESIAN_POINT('Ctrl Pts',(5.19444677701023,15.2,10.164668675434));
#216918=CARTESIAN_POINT('Ctrl Pts',(5.19738126682024,15.2,10.1669452418346));
#216919=CARTESIAN_POINT('Ctrl Pts',(5.20032370467096,15.2,10.1692225565018));
#216920=CARTESIAN_POINT('Ctrl Pts',(5.20326614252168,15.2,10.171499871169));
#216921=CARTESIAN_POINT('Ctrl Pts',(5.2062165312882,15.2,10.1737779345448));
#216922=CARTESIAN_POINT('Ctrl Pts',(5.20917485866094,15.2,10.1760567053258));
#216923=CARTESIAN_POINT('Ctrl Pts',(5.21213318603366,15.2,10.1783354761067));
#216924=CARTESIAN_POINT('Ctrl Pts',(5.21509945217733,15.2,10.1806149539358));
#216925=CARTESIAN_POINT('Ctrl Pts',(5.21807364785985,15.2,10.1828950987696));
#216926=CARTESIAN_POINT('Ctrl Pts',(5.2210478440827,15.2,10.1851752440175));
#216927=CARTESIAN_POINT('Ctrl Pts',(5.22402996911609,15.2,10.1874560580323));
#216928=CARTESIAN_POINT('Ctrl Pts',(5.22702001488507,15.2,10.1897375041973));
#216929=CARTESIAN_POINT('Ctrl Pts',(5.23001006011085,15.2,10.1920189499479));
#216930=CARTESIAN_POINT('Ctrl Pts',(5.23300802603619,15.2,10.194301028465));
#216931=CARTESIAN_POINT('Ctrl Pts',(5.23601390080267,15.2,10.1965836989655));
#216932=CARTESIAN_POINT('Ctrl Pts',(5.24102369226215,15.2,10.2003881499378));
#216933=CARTESIAN_POINT('Ctrl Pts',(5.24605545522705,15.2,10.2041942383572));
#216934=CARTESIAN_POINT('Ctrl Pts',(5.25110913436996,15.2,10.2080017559086));
#216935=CARTESIAN_POINT('Ctrl Pts',(5.25414134174553,15.2,10.2102862663565));
#216936=CARTESIAN_POINT('Ctrl Pts',(5.25718143818119,15.2,10.2125712912946));
#216937=CARTESIAN_POINT('Ctrl Pts',(5.26022941958503,15.2,10.2148568145085));
#216938=CARTESIAN_POINT('Ctrl Pts',(5.26327740098887,15.2,10.2171423377224));
#216939=CARTESIAN_POINT('Ctrl Pts',(5.26633327020158,15.2,10.2194283609115));
#216940=CARTESIAN_POINT('Ctrl Pts',(5.26939701799994,15.2,10.221714878));
#216941=CARTESIAN_POINT('Origin',(-5.66257110645729E-14,15.2,-1.77635683940025E-14));
#216942=CARTESIAN_POINT('',(4.0426091163045,15.2,9.55499537093196));
#216943=CARTESIAN_POINT('',(4.0426091163045,12.2,9.55499537093196));
#216944=CARTESIAN_POINT('',(4.04260911599994,15.2,9.55499537099998));
#216945=CARTESIAN_POINT('Origin',(-5.66257110645729E-14,12.2,-1.77635683940025E-14));
#216946=CARTESIAN_POINT('Origin',(-5.66257110645729E-14,15.2,-1.77635683940025E-14));
#216947=CARTESIAN_POINT('Origin',(-5.66257110645729E-14,15.2,-1.77635683940025E-14));
#216948=CARTESIAN_POINT('',(4.12144986799994,15.2,10.736091048));
#216949=CARTESIAN_POINT('',(3.76106045499994,15.2,10.867585944));
#216950=CARTESIAN_POINT('Origin',(-5.66257110645729E-14,15.2,-1.77635683940025E-14));
#216951=CARTESIAN_POINT('',(3.76106045499994,12.2,10.867585944));
#216952=CARTESIAN_POINT('',(3.76106045499994,15.2,10.867585944));
#216953=CARTESIAN_POINT('',(4.12144986799994,12.2,10.736091048));
#216954=CARTESIAN_POINT('Origin',(-5.66257110645729E-14,12.2,-1.77635683940025E-14));
#216955=CARTESIAN_POINT('',(4.12144986799994,15.2,10.736091048));
#216956=CARTESIAN_POINT('Ctrl Pts',(3.76106045499994,15.2,10.867585944));
#216957=CARTESIAN_POINT('Ctrl Pts',(3.76106045499994,11.6,10.867585944));
#216958=CARTESIAN_POINT('Ctrl Pts',(3.76051902299994,15.2,10.867046091));
#216959=CARTESIAN_POINT('Ctrl Pts',(3.76051902299994,11.6,10.867046091));
#216960=CARTESIAN_POINT('Ctrl Pts',(3.75943667399994,15.2,10.865966495));
#216961=CARTESIAN_POINT('Ctrl Pts',(3.75943667399994,11.6,10.865966495));
#216962=CARTESIAN_POINT('Ctrl Pts',(3.75781469799994,15.2,10.864347421));
#216963=CARTESIAN_POINT('Ctrl Pts',(3.75781469799994,11.6,10.864347421));
#216964=CARTESIAN_POINT('Ctrl Pts',(3.75565515599994,15.2,10.862189302));
#216965=CARTESIAN_POINT('Ctrl Pts',(3.75565515599994,11.6,10.862189302));
#216966=CARTESIAN_POINT('Ctrl Pts',(3.75296088399994,15.2,10.85949273));
#216967=CARTESIAN_POINT('Ctrl Pts',(3.75296088399994,11.6,10.85949273));
#216968=CARTESIAN_POINT('Ctrl Pts',(3.75027176799994,15.2,10.856797236));
#216969=CARTESIAN_POINT('Ctrl Pts',(3.75027176799994,11.6,10.856797236));
#216970=CARTESIAN_POINT('Ctrl Pts',(3.74758780799994,15.2,10.854102822));
#216971=CARTESIAN_POINT('Ctrl Pts',(3.74758780799994,11.6,10.854102822));
#216972=CARTESIAN_POINT('Ctrl Pts',(3.74490900499994,15.2,10.85140949));
#216973=CARTESIAN_POINT('Ctrl Pts',(3.74490900499994,11.6,10.85140949));
#216974=CARTESIAN_POINT('Ctrl Pts',(3.74223535999994,15.2,10.84871725));
#216975=CARTESIAN_POINT('Ctrl Pts',(3.74223535999994,11.6,10.84871725));
#216976=CARTESIAN_POINT('Ctrl Pts',(3.73956687399994,15.2,10.846026106));
#216977=CARTESIAN_POINT('Ctrl Pts',(3.73956687399994,11.6,10.846026106));
#216978=CARTESIAN_POINT('Ctrl Pts',(3.73690354699994,15.2,10.843336071));
#216979=CARTESIAN_POINT('Ctrl Pts',(3.73690354699994,11.6,10.843336071));
#216980=CARTESIAN_POINT('Ctrl Pts',(3.73424538199994,15.2,10.840647153));
#216981=CARTESIAN_POINT('Ctrl Pts',(3.73424538199994,11.6,10.840647153));
#216982=CARTESIAN_POINT('Ctrl Pts',(3.73159237799995,15.2,10.837959365));
#216983=CARTESIAN_POINT('Ctrl Pts',(3.73159237799995,11.6,10.837959365));
#216984=CARTESIAN_POINT('Ctrl Pts',(3.72894453699994,15.2,10.835272717));
#216985=CARTESIAN_POINT('Ctrl Pts',(3.72894453699994,11.6,10.835272717));
#216986=CARTESIAN_POINT('Ctrl Pts',(3.72630186199994,15.2,10.832587221));
#216987=CARTESIAN_POINT('Ctrl Pts',(3.72630186199994,11.6,10.832587221));
#216988=CARTESIAN_POINT('Ctrl Pts',(3.72366435199994,15.2,10.829902884));
#216989=CARTESIAN_POINT('Ctrl Pts',(3.72366435199994,11.6,10.829902884));
#216990=CARTESIAN_POINT('Ctrl Pts',(3.72103200699994,15.2,10.827219716));
#216991=CARTESIAN_POINT('Ctrl Pts',(3.72103200699994,11.6,10.827219716));
#216992=CARTESIAN_POINT('Ctrl Pts',(3.71840482999994,15.2,10.824537725));
#216993=CARTESIAN_POINT('Ctrl Pts',(3.71840482999994,11.6,10.824537725));
#216994=CARTESIAN_POINT('Ctrl Pts',(3.71578282099994,15.2,10.821856919));
#216995=CARTESIAN_POINT('Ctrl Pts',(3.71578282099994,11.6,10.821856919));
#216996=CARTESIAN_POINT('Ctrl Pts',(3.71316598199994,15.2,10.819177306));
#216997=CARTESIAN_POINT('Ctrl Pts',(3.71316598199994,11.6,10.819177306));
#216998=CARTESIAN_POINT('Ctrl Pts',(3.71055431199994,15.2,10.816498895));
#216999=CARTESIAN_POINT('Ctrl Pts',(3.71055431199994,11.6,10.816498895));
#217000=CARTESIAN_POINT('Ctrl Pts',(3.70794781299994,15.2,10.813821695));
#217001=CARTESIAN_POINT('Ctrl Pts',(3.70794781299994,11.6,10.813821695));
#217002=CARTESIAN_POINT('Ctrl Pts',(3.70534648499994,15.2,10.811145713));
#217003=CARTESIAN_POINT('Ctrl Pts',(3.70534648499994,11.6,10.811145713));
#217004=CARTESIAN_POINT('Ctrl Pts',(3.70275033099994,15.2,10.808470961));
#217005=CARTESIAN_POINT('Ctrl Pts',(3.70275033099994,11.6,10.808470961));
#217006=CARTESIAN_POINT('Ctrl Pts',(3.70015935099994,15.2,10.805797449));
#217007=CARTESIAN_POINT('Ctrl Pts',(3.70015935099994,11.6,10.805797449));
#217008=CARTESIAN_POINT('Ctrl Pts',(3.69757354499994,15.2,10.803125184));
#217009=CARTESIAN_POINT('Ctrl Pts',(3.69757354499994,11.6,10.803125184));
#217010=CARTESIAN_POINT('Ctrl Pts',(3.69499291499995,15.2,10.800454179));
#217011=CARTESIAN_POINT('Ctrl Pts',(3.69499291499995,11.6,10.800454179));
#217012=CARTESIAN_POINT('Ctrl Pts',(3.69241746099994,15.2,10.797784438));
#217013=CARTESIAN_POINT('Ctrl Pts',(3.69241746099994,11.6,10.797784438));
#217014=CARTESIAN_POINT('Ctrl Pts',(3.68984718499994,15.2,10.795115974));
#217015=CARTESIAN_POINT('Ctrl Pts',(3.68984718499994,11.6,10.795115974));
#217016=CARTESIAN_POINT('Ctrl Pts',(3.68728208699994,15.2,10.792448794));
#217017=CARTESIAN_POINT('Ctrl Pts',(3.68728208699994,11.6,10.792448794));
#217018=CARTESIAN_POINT('Ctrl Pts',(3.68472216799994,15.2,10.789782909));
#217019=CARTESIAN_POINT('Ctrl Pts',(3.68472216799994,11.6,10.789782909));
#217020=CARTESIAN_POINT('Ctrl Pts',(3.68216742899994,15.2,10.787118327));
#217021=CARTESIAN_POINT('Ctrl Pts',(3.68216742899994,11.6,10.787118327));
#217022=CARTESIAN_POINT('Ctrl Pts',(3.67961787099994,15.2,10.784455057));
#217023=CARTESIAN_POINT('Ctrl Pts',(3.67961787099994,11.6,10.784455057));
#217024=CARTESIAN_POINT('Ctrl Pts',(3.67707349599994,15.2,10.781793108));
#217025=CARTESIAN_POINT('Ctrl Pts',(3.67707349599994,11.6,10.781793108));
#217026=CARTESIAN_POINT('Ctrl Pts',(3.67453430199994,15.2,10.77913249));
#217027=CARTESIAN_POINT('Ctrl Pts',(3.67453430199994,11.6,10.77913249));
#217028=CARTESIAN_POINT('Ctrl Pts',(3.67200029299994,15.2,10.776473211));
#217029=CARTESIAN_POINT('Ctrl Pts',(3.67200029299994,11.6,10.776473211));
#217030=CARTESIAN_POINT('Ctrl Pts',(3.66947146699994,15.2,10.773815282));
#217031=CARTESIAN_POINT('Ctrl Pts',(3.66947146699994,11.6,10.773815282));
#217032=CARTESIAN_POINT('Ctrl Pts',(3.66694782699994,15.2,10.771158713));
#217033=CARTESIAN_POINT('Ctrl Pts',(3.66694782699994,11.6,10.771158713));
#217034=CARTESIAN_POINT('Ctrl Pts',(3.66442937399994,15.2,10.768503511));
#217035=CARTESIAN_POINT('Ctrl Pts',(3.66442937399994,11.6,10.768503511));
#217036=CARTESIAN_POINT('Ctrl Pts',(3.66191610699994,15.2,10.765849687));
#217037=CARTESIAN_POINT('Ctrl Pts',(3.66191610699994,11.6,10.765849687));
#217038=CARTESIAN_POINT('Ctrl Pts',(3.65940802899994,15.2,10.76319725));
#217039=CARTESIAN_POINT('Ctrl Pts',(3.65940802899994,11.6,10.76319725));
#217040=CARTESIAN_POINT('Ctrl Pts',(3.65690513699994,15.2,10.760546208));
#217041=CARTESIAN_POINT('Ctrl Pts',(3.65690513699994,11.6,10.760546208));
#217042=CARTESIAN_POINT('Ctrl Pts',(3.65440743699994,15.2,10.757896573));
#217043=CARTESIAN_POINT('Ctrl Pts',(3.65440743699994,11.6,10.757896573));
#217044=CARTESIAN_POINT('Ctrl Pts',(3.65191492599994,15.2,10.755248353));
#217045=CARTESIAN_POINT('Ctrl Pts',(3.65191492599994,11.6,10.755248353));
#217046=CARTESIAN_POINT('Ctrl Pts',(3.64942760599994,15.2,10.752601556));
#217047=CARTESIAN_POINT('Ctrl Pts',(3.64942760599994,11.6,10.752601556));
#217048=CARTESIAN_POINT('Ctrl Pts',(3.64694547899994,15.2,10.749956194));
#217049=CARTESIAN_POINT('Ctrl Pts',(3.64694547899994,11.6,10.749956194));
#217050=CARTESIAN_POINT('Ctrl Pts',(3.64446854399994,15.2,10.747312275));
#217051=CARTESIAN_POINT('Ctrl Pts',(3.64446854399994,11.6,10.747312275));
#217052=CARTESIAN_POINT('Ctrl Pts',(3.64199680199994,15.2,10.744669808));
#217053=CARTESIAN_POINT('Ctrl Pts',(3.64199680199994,11.6,10.744669808));
#217054=CARTESIAN_POINT('Ctrl Pts',(3.63953025499994,15.2,10.742028805));
#217055=CARTESIAN_POINT('Ctrl Pts',(3.63953025499994,11.6,10.742028805));
#217056=CARTESIAN_POINT('Ctrl Pts',(3.63706890199994,15.2,10.739389272));
#217057=CARTESIAN_POINT('Ctrl Pts',(3.63706890199994,11.6,10.739389272));
#217058=CARTESIAN_POINT('Ctrl Pts',(3.63461274499994,15.2,10.736751222));
#217059=CARTESIAN_POINT('Ctrl Pts',(3.63461274499994,11.6,10.736751222));
#217060=CARTESIAN_POINT('Ctrl Pts',(3.63216178499994,15.2,10.734114662));
#217061=CARTESIAN_POINT('Ctrl Pts',(3.63216178499994,11.6,10.734114662));
#217062=CARTESIAN_POINT('Ctrl Pts',(3.62971602199994,15.2,10.731479602));
#217063=CARTESIAN_POINT('Ctrl Pts',(3.62971602199994,11.6,10.731479602));
#217064=CARTESIAN_POINT('Ctrl Pts',(3.62727545699994,15.2,10.728846054));
#217065=CARTESIAN_POINT('Ctrl Pts',(3.62727545699994,11.6,10.728846054));
#217066=CARTESIAN_POINT('Ctrl Pts',(3.62484009099994,15.2,10.726214025));
#217067=CARTESIAN_POINT('Ctrl Pts',(3.62484009099994,11.6,10.726214025));
#217068=CARTESIAN_POINT('Ctrl Pts',(3.62240992399994,15.2,10.723583524));
#217069=CARTESIAN_POINT('Ctrl Pts',(3.62240992399994,11.6,10.723583524));
#217070=CARTESIAN_POINT('Ctrl Pts',(3.61998495799994,15.2,10.720954563));
#217071=CARTESIAN_POINT('Ctrl Pts',(3.61998495799994,11.6,10.720954563));
#217072=CARTESIAN_POINT('Ctrl Pts',(3.61756519199994,15.2,10.718327151));
#217073=CARTESIAN_POINT('Ctrl Pts',(3.61756519199994,11.6,10.718327151));
#217074=CARTESIAN_POINT('Ctrl Pts',(3.61515062899994,15.2,10.715701296));
#217075=CARTESIAN_POINT('Ctrl Pts',(3.61515062899994,11.6,10.715701296));
#217076=CARTESIAN_POINT('Ctrl Pts',(3.61274126699994,15.2,10.71307701));
#217077=CARTESIAN_POINT('Ctrl Pts',(3.61274126699994,11.6,10.71307701));
#217078=CARTESIAN_POINT('Ctrl Pts',(3.61033710899994,15.2,10.710454302));
#217079=CARTESIAN_POINT('Ctrl Pts',(3.61033710899994,11.6,10.710454302));
#217080=CARTESIAN_POINT('Ctrl Pts',(3.60793815399994,15.2,10.707833181));
#217081=CARTESIAN_POINT('Ctrl Pts',(3.60793815399994,11.6,10.707833181));
#217082=CARTESIAN_POINT('Ctrl Pts',(3.60554440399994,15.2,10.705213657));
#217083=CARTESIAN_POINT('Ctrl Pts',(3.60554440399994,11.6,10.705213657));
#217084=CARTESIAN_POINT('Ctrl Pts',(3.60315585899994,15.2,10.702595741));
#217085=CARTESIAN_POINT('Ctrl Pts',(3.60315585899994,11.6,10.702595741));
#217086=CARTESIAN_POINT('Ctrl Pts',(3.60077251999994,15.2,10.699979441));
#217087=CARTESIAN_POINT('Ctrl Pts',(3.60077251999994,11.6,10.699979441));
#217088=CARTESIAN_POINT('Ctrl Pts',(3.59839438799994,15.2,10.697364767));
#217089=CARTESIAN_POINT('Ctrl Pts',(3.59839438799994,11.6,10.697364767));
#217090=CARTESIAN_POINT('Ctrl Pts',(3.59602146199994,15.2,10.694751731));
#217091=CARTESIAN_POINT('Ctrl Pts',(3.59602146199994,11.6,10.694751731));
#217092=CARTESIAN_POINT('Ctrl Pts',(3.59365374499994,15.2,10.692140339));
#217093=CARTESIAN_POINT('Ctrl Pts',(3.59365374499994,11.6,10.692140339));
#217094=CARTESIAN_POINT('Ctrl Pts',(3.59129123599994,15.2,10.689530605));
#217095=CARTESIAN_POINT('Ctrl Pts',(3.59129123599994,11.6,10.689530605));
#217096=CARTESIAN_POINT('Ctrl Pts',(3.58893393499994,15.2,10.686922536));
#217097=CARTESIAN_POINT('Ctrl Pts',(3.58893393499994,11.6,10.686922536));
#217098=CARTESIAN_POINT('Ctrl Pts',(3.58658184499994,15.2,10.684316143));
#217099=CARTESIAN_POINT('Ctrl Pts',(3.58658184499994,11.6,10.684316143));
#217100=CARTESIAN_POINT('Ctrl Pts',(3.58423496399995,15.2,10.681711437));
#217101=CARTESIAN_POINT('Ctrl Pts',(3.58423496399995,11.6,10.681711437));
#217102=CARTESIAN_POINT('Ctrl Pts',(3.58189329599994,15.2,10.679108425));
#217103=CARTESIAN_POINT('Ctrl Pts',(3.58189329599994,11.6,10.679108425));
#217104=CARTESIAN_POINT('Ctrl Pts',(3.57955683799994,15.2,10.67650712));
#217105=CARTESIAN_POINT('Ctrl Pts',(3.57955683799994,11.6,10.67650712));
#217106=CARTESIAN_POINT('Ctrl Pts',(3.57722559299994,15.2,10.673907531));
#217107=CARTESIAN_POINT('Ctrl Pts',(3.57722559299994,11.6,10.673907531));
#217108=CARTESIAN_POINT('Ctrl Pts',(3.57489956099994,15.2,10.671309666));
#217109=CARTESIAN_POINT('Ctrl Pts',(3.57489956099994,11.6,10.671309666));
#217110=CARTESIAN_POINT('Ctrl Pts',(3.57257874199994,15.2,10.668713538));
#217111=CARTESIAN_POINT('Ctrl Pts',(3.57257874199994,11.6,10.668713538));
#217112=CARTESIAN_POINT('Ctrl Pts',(3.57026313699994,15.2,10.666119155));
#217113=CARTESIAN_POINT('Ctrl Pts',(3.57026313699994,11.6,10.666119155));
#217114=CARTESIAN_POINT('Ctrl Pts',(3.56795274699994,15.2,10.663526528));
#217115=CARTESIAN_POINT('Ctrl Pts',(3.56795274699994,11.6,10.663526528));
#217116=CARTESIAN_POINT('Ctrl Pts',(3.56564757099994,15.2,10.660935667));
#217117=CARTESIAN_POINT('Ctrl Pts',(3.56564757099994,11.6,10.660935667));
#217118=CARTESIAN_POINT('Ctrl Pts',(3.56334761099994,15.2,10.658346581));
#217119=CARTESIAN_POINT('Ctrl Pts',(3.56334761099994,11.6,10.658346581));
#217120=CARTESIAN_POINT('Ctrl Pts',(3.56105286799994,15.2,10.655759282));
#217121=CARTESIAN_POINT('Ctrl Pts',(3.56105286799994,11.6,10.655759282));
#217122=CARTESIAN_POINT('Ctrl Pts',(3.55876334099994,15.2,10.653173779));
#217123=CARTESIAN_POINT('Ctrl Pts',(3.55876334099994,11.6,10.653173779));
#217124=CARTESIAN_POINT('Ctrl Pts',(3.55647903199994,15.2,10.650590083));
#217125=CARTESIAN_POINT('Ctrl Pts',(3.55647903199994,11.6,10.650590083));
#217126=CARTESIAN_POINT('Ctrl Pts',(3.55419994099994,15.2,10.648008202));
#217127=CARTESIAN_POINT('Ctrl Pts',(3.55419994099994,11.6,10.648008202));
#217128=CARTESIAN_POINT('Ctrl Pts',(3.55192606799994,15.2,10.645428149));
#217129=CARTESIAN_POINT('Ctrl Pts',(3.55192606799994,11.6,10.645428149));
#217130=CARTESIAN_POINT('Ctrl Pts',(3.54965741499994,15.2,10.642849932));
#217131=CARTESIAN_POINT('Ctrl Pts',(3.54965741499994,11.6,10.642849932));
#217132=CARTESIAN_POINT('Ctrl Pts',(3.54739397999994,15.2,10.640273563));
#217133=CARTESIAN_POINT('Ctrl Pts',(3.54739397999994,11.6,10.640273563));
#217134=CARTESIAN_POINT('Ctrl Pts',(3.54513576499994,15.2,10.637699051));
#217135=CARTESIAN_POINT('Ctrl Pts',(3.54513576499994,11.6,10.637699051));
#217136=CARTESIAN_POINT('Ctrl Pts',(3.54288277099994,15.2,10.635126406));
#217137=CARTESIAN_POINT('Ctrl Pts',(3.54288277099994,11.6,10.635126406));
#217138=CARTESIAN_POINT('Ctrl Pts',(3.54063499799994,15.2,10.632555639));
#217139=CARTESIAN_POINT('Ctrl Pts',(3.54063499799994,11.6,10.632555639));
#217140=CARTESIAN_POINT('Ctrl Pts',(3.53839244699994,15.2,10.62998676));
#217141=CARTESIAN_POINT('Ctrl Pts',(3.53839244699994,11.6,10.62998676));
#217142=CARTESIAN_POINT('Ctrl Pts',(3.53615511699994,15.2,10.62741978));
#217143=CARTESIAN_POINT('Ctrl Pts',(3.53615511699994,11.6,10.62741978));
#217144=CARTESIAN_POINT('Ctrl Pts',(3.53392300999994,15.2,10.624854709));
#217145=CARTESIAN_POINT('Ctrl Pts',(3.53392300999994,11.6,10.624854709));
#217146=CARTESIAN_POINT('Ctrl Pts',(3.53169612599994,15.2,10.622291557));
#217147=CARTESIAN_POINT('Ctrl Pts',(3.53169612599994,11.6,10.622291557));
#217148=CARTESIAN_POINT('Ctrl Pts',(3.52947446499994,15.2,10.619730334));
#217149=CARTESIAN_POINT('Ctrl Pts',(3.52947446499994,11.6,10.619730334));
#217150=CARTESIAN_POINT('Ctrl Pts',(3.52725802799994,15.2,10.617171051));
#217151=CARTESIAN_POINT('Ctrl Pts',(3.52725802799994,11.6,10.617171051));
#217152=CARTESIAN_POINT('Ctrl Pts',(3.52504681399994,15.2,10.61461372));
#217153=CARTESIAN_POINT('Ctrl Pts',(3.52504681399994,11.6,10.61461372));
#217154=CARTESIAN_POINT('Ctrl Pts',(3.52284082599994,15.2,10.612058349));
#217155=CARTESIAN_POINT('Ctrl Pts',(3.52284082599994,11.6,10.612058349));
#217156=CARTESIAN_POINT('Ctrl Pts',(3.52064006199994,15.2,10.609504948));
#217157=CARTESIAN_POINT('Ctrl Pts',(3.52064006199994,11.6,10.609504948));
#217158=CARTESIAN_POINT('Ctrl Pts',(3.51844452399994,15.2,10.606953531));
#217159=CARTESIAN_POINT('Ctrl Pts',(3.51844452399994,11.6,10.606953531));
#217160=CARTESIAN_POINT('Ctrl Pts',(3.51625421199994,15.2,10.604404106));
#217161=CARTESIAN_POINT('Ctrl Pts',(3.51625421199994,11.6,10.604404106));
#217162=CARTESIAN_POINT('Ctrl Pts',(3.51406912699994,15.2,10.601856683));
#217163=CARTESIAN_POINT('Ctrl Pts',(3.51406912699994,11.6,10.601856683));
#217164=CARTESIAN_POINT('Ctrl Pts',(3.51188926799994,15.2,10.599311274));
#217165=CARTESIAN_POINT('Ctrl Pts',(3.51188926799994,11.6,10.599311274));
#217166=CARTESIAN_POINT('Ctrl Pts',(3.50971463599994,15.2,10.596767889));
#217167=CARTESIAN_POINT('Ctrl Pts',(3.50971463599994,11.6,10.596767889));
#217168=CARTESIAN_POINT('Ctrl Pts',(3.50754523199994,15.2,10.594226538));
#217169=CARTESIAN_POINT('Ctrl Pts',(3.50754523199994,11.6,10.594226538));
#217170=CARTESIAN_POINT('Ctrl Pts',(3.50538105499994,15.2,10.591687233));
#217171=CARTESIAN_POINT('Ctrl Pts',(3.50538105499994,11.6,10.591687233));
#217172=CARTESIAN_POINT('Ctrl Pts',(3.50322210699994,15.2,10.589149983));
#217173=CARTESIAN_POINT('Ctrl Pts',(3.50322210699994,11.6,10.589149983));
#217174=CARTESIAN_POINT('Ctrl Pts',(3.50106838699995,15.2,10.5866148));
#217175=CARTESIAN_POINT('Ctrl Pts',(3.50106838699995,11.6,10.5866148));
#217176=CARTESIAN_POINT('Ctrl Pts',(3.49891989599994,15.2,10.584081694));
#217177=CARTESIAN_POINT('Ctrl Pts',(3.49891989599994,11.6,10.584081694));
#217178=CARTESIAN_POINT('Ctrl Pts',(3.49677663399994,15.2,10.581550676));
#217179=CARTESIAN_POINT('Ctrl Pts',(3.49677663399994,11.6,10.581550676));
#217180=CARTESIAN_POINT('Ctrl Pts',(3.49463860199994,15.2,10.579021758));
#217181=CARTESIAN_POINT('Ctrl Pts',(3.49463860199994,11.6,10.579021758));
#217182=CARTESIAN_POINT('Ctrl Pts',(3.49250580099994,15.2,10.576494948));
#217183=CARTESIAN_POINT('Ctrl Pts',(3.49250580099994,11.6,10.576494948));
#217184=CARTESIAN_POINT('Ctrl Pts',(3.49037822899994,15.2,10.573970259));
#217185=CARTESIAN_POINT('Ctrl Pts',(3.49037822899994,11.6,10.573970259));
#217186=CARTESIAN_POINT('Ctrl Pts',(3.48825588699994,15.2,10.571447699));
#217187=CARTESIAN_POINT('Ctrl Pts',(3.48825588699994,11.6,10.571447699));
#217188=CARTESIAN_POINT('Ctrl Pts',(3.48613877699994,15.2,10.568927282));
#217189=CARTESIAN_POINT('Ctrl Pts',(3.48613877699994,11.6,10.568927282));
#217190=CARTESIAN_POINT('Ctrl Pts',(3.48402689799994,15.2,10.566409018));
#217191=CARTESIAN_POINT('Ctrl Pts',(3.48402689799994,11.6,10.566409018));
#217192=CARTESIAN_POINT('Ctrl Pts',(3.48192024899994,15.2,10.563892917));
#217193=CARTESIAN_POINT('Ctrl Pts',(3.48192024899994,11.6,10.563892917));
#217194=CARTESIAN_POINT('Ctrl Pts',(3.47981883399994,15.2,10.561378991));
#217195=CARTESIAN_POINT('Ctrl Pts',(3.47981883399994,11.6,10.561378991));
#217196=CARTESIAN_POINT('Ctrl Pts',(3.47772264999994,15.2,10.558867249));
#217197=CARTESIAN_POINT('Ctrl Pts',(3.47772264999994,11.6,10.558867249));
#217198=CARTESIAN_POINT('Ctrl Pts',(3.47563169699994,15.2,10.556357703));
#217199=CARTESIAN_POINT('Ctrl Pts',(3.47563169699994,11.6,10.556357703));
#217200=CARTESIAN_POINT('Ctrl Pts',(3.47354597799994,15.2,10.553850365));
#217201=CARTESIAN_POINT('Ctrl Pts',(3.47354597799994,11.6,10.553850365));
#217202=CARTESIAN_POINT('Ctrl Pts',(3.47146549099994,15.2,10.551345244));
#217203=CARTESIAN_POINT('Ctrl Pts',(3.47146549099994,11.6,10.551345244));
#217204=CARTESIAN_POINT('Ctrl Pts',(3.46939023699994,15.2,10.548842353));
#217205=CARTESIAN_POINT('Ctrl Pts',(3.46939023699994,11.6,10.548842353));
#217206=CARTESIAN_POINT('Ctrl Pts',(3.46732021699995,15.2,10.546341702));
#217207=CARTESIAN_POINT('Ctrl Pts',(3.46732021699995,11.6,10.546341702));
#217208=CARTESIAN_POINT('Ctrl Pts',(3.46525542999994,15.2,10.543843302));
#217209=CARTESIAN_POINT('Ctrl Pts',(3.46525542999994,11.6,10.543843302));
#217210=CARTESIAN_POINT('Ctrl Pts',(3.46319587599994,15.2,10.541347163));
#217211=CARTESIAN_POINT('Ctrl Pts',(3.46319587599994,11.6,10.541347163));
#217212=CARTESIAN_POINT('Ctrl Pts',(3.46114155699994,15.2,10.538853298));
#217213=CARTESIAN_POINT('Ctrl Pts',(3.46114155699994,11.6,10.538853298));
#217214=CARTESIAN_POINT('Ctrl Pts',(3.45909247099994,15.2,10.536361718));
#217215=CARTESIAN_POINT('Ctrl Pts',(3.45909247099994,11.6,10.536361718));
#217216=CARTESIAN_POINT('Ctrl Pts',(3.45704861999995,15.2,10.533872432));
#217217=CARTESIAN_POINT('Ctrl Pts',(3.45704861999995,11.6,10.533872432));
#217218=CARTESIAN_POINT('Ctrl Pts',(3.45501000299994,15.2,10.531385453));
#217219=CARTESIAN_POINT('Ctrl Pts',(3.45501000299994,11.6,10.531385453));
#217220=CARTESIAN_POINT('Ctrl Pts',(3.45297662099994,15.2,10.528900792));
#217221=CARTESIAN_POINT('Ctrl Pts',(3.45297662099994,11.6,10.528900792));
#217222=CARTESIAN_POINT('Ctrl Pts',(3.45094847299994,15.2,10.526418461));
#217223=CARTESIAN_POINT('Ctrl Pts',(3.45094847299994,11.6,10.526418461));
#217224=CARTESIAN_POINT('Ctrl Pts',(3.44892555999994,15.2,10.523938468));
#217225=CARTESIAN_POINT('Ctrl Pts',(3.44892555999994,11.6,10.523938468));
#217226=CARTESIAN_POINT('Ctrl Pts',(3.44690788299994,15.2,10.521460827));
#217227=CARTESIAN_POINT('Ctrl Pts',(3.44690788299994,11.6,10.521460827));
#217228=CARTESIAN_POINT('Ctrl Pts',(3.44489543999994,15.2,10.51898555));
#217229=CARTESIAN_POINT('Ctrl Pts',(3.44489543999994,11.6,10.51898555));
#217230=CARTESIAN_POINT('Ctrl Pts',(3.44288823299994,15.2,10.516512645));
#217231=CARTESIAN_POINT('Ctrl Pts',(3.44288823299994,11.6,10.516512645));
#217232=CARTESIAN_POINT('Ctrl Pts',(3.44088626199994,15.2,10.514042126));
#217233=CARTESIAN_POINT('Ctrl Pts',(3.44088626199994,11.6,10.514042126));
#217234=CARTESIAN_POINT('Ctrl Pts',(3.43888952499994,15.2,10.511574004));
#217235=CARTESIAN_POINT('Ctrl Pts',(3.43888952499994,11.6,10.511574004));
#217236=CARTESIAN_POINT('Ctrl Pts',(3.43689802499994,15.2,10.50910829));
#217237=CARTESIAN_POINT('Ctrl Pts',(3.43689802499994,11.6,10.50910829));
#217238=CARTESIAN_POINT('Ctrl Pts',(3.43491175999994,15.2,10.506644995));
#217239=CARTESIAN_POINT('Ctrl Pts',(3.43491175999994,11.6,10.506644995));
#217240=CARTESIAN_POINT('Ctrl Pts',(3.43293072999994,15.2,10.504184131));
#217241=CARTESIAN_POINT('Ctrl Pts',(3.43293072999994,11.6,10.504184131));
#217242=CARTESIAN_POINT('Ctrl Pts',(3.43095493699995,15.2,10.501725709));
#217243=CARTESIAN_POINT('Ctrl Pts',(3.43095493699995,11.6,10.501725709));
#217244=CARTESIAN_POINT('Ctrl Pts',(3.42898437999994,15.2,10.49926974));
#217245=CARTESIAN_POINT('Ctrl Pts',(3.42898437999994,11.6,10.49926974));
#217246=CARTESIAN_POINT('Ctrl Pts',(3.42701905899994,15.2,10.496816237));
#217247=CARTESIAN_POINT('Ctrl Pts',(3.42701905899994,11.6,10.496816237));
#217248=CARTESIAN_POINT('Ctrl Pts',(3.42505897399994,15.2,10.49436521));
#217249=CARTESIAN_POINT('Ctrl Pts',(3.42505897399994,11.6,10.49436521));
#217250=CARTESIAN_POINT('Ctrl Pts',(3.42310412599995,15.2,10.491916672));
#217251=CARTESIAN_POINT('Ctrl Pts',(3.42310412599995,11.6,10.491916672));
#217252=CARTESIAN_POINT('Ctrl Pts',(3.42115451199994,15.2,10.489470632));
#217253=CARTESIAN_POINT('Ctrl Pts',(3.42115451199994,11.6,10.489470632));
#217254=CARTESIAN_POINT('Ctrl Pts',(3.41921013599995,15.2,10.487027105));
#217255=CARTESIAN_POINT('Ctrl Pts',(3.41921013599995,11.6,10.487027105));
#217256=CARTESIAN_POINT('Ctrl Pts',(3.41727099499994,15.2,10.4845861));
#217257=CARTESIAN_POINT('Ctrl Pts',(3.41727099499994,11.6,10.4845861));
#217258=CARTESIAN_POINT('Ctrl Pts',(3.41533709199994,15.2,10.482147629));
#217259=CARTESIAN_POINT('Ctrl Pts',(3.41533709199994,11.6,10.482147629));
#217260=CARTESIAN_POINT('Ctrl Pts',(3.41340842399994,15.2,10.479711706));
#217261=CARTESIAN_POINT('Ctrl Pts',(3.41340842399994,11.6,10.479711706));
#217262=CARTESIAN_POINT('Ctrl Pts',(3.41148499199994,15.2,10.477278339));
#217263=CARTESIAN_POINT('Ctrl Pts',(3.41148499199994,11.6,10.477278339));
#217264=CARTESIAN_POINT('Ctrl Pts',(3.40956679599994,15.2,10.474847543));
#217265=CARTESIAN_POINT('Ctrl Pts',(3.40956679599994,11.6,10.474847543));
#217266=CARTESIAN_POINT('Ctrl Pts',(3.40765383599994,15.2,10.472419326));
#217267=CARTESIAN_POINT('Ctrl Pts',(3.40765383599994,11.6,10.472419326));
#217268=CARTESIAN_POINT('Ctrl Pts',(3.40574611299994,15.2,10.469993704));
#217269=CARTESIAN_POINT('Ctrl Pts',(3.40574611299994,11.6,10.469993704));
#217270=CARTESIAN_POINT('Ctrl Pts',(3.40384362599994,15.2,10.467570687));
#217271=CARTESIAN_POINT('Ctrl Pts',(3.40384362599994,11.6,10.467570687));
#217272=CARTESIAN_POINT('Ctrl Pts',(3.40194637399994,15.2,10.465150286));
#217273=CARTESIAN_POINT('Ctrl Pts',(3.40194637399994,11.6,10.465150286));
#217274=CARTESIAN_POINT('Ctrl Pts',(3.40005435899994,15.2,10.462732513));
#217275=CARTESIAN_POINT('Ctrl Pts',(3.40005435899994,11.6,10.462732513));
#217276=CARTESIAN_POINT('Ctrl Pts',(3.39816757899994,15.2,10.460317381));
#217277=CARTESIAN_POINT('Ctrl Pts',(3.39816757899994,11.6,10.460317381));
#217278=CARTESIAN_POINT('Ctrl Pts',(3.39628603499994,15.2,10.4579049));
#217279=CARTESIAN_POINT('Ctrl Pts',(3.39628603499994,11.6,10.4579049));
#217280=CARTESIAN_POINT('Ctrl Pts',(3.39440972599995,15.2,10.455495084));
#217281=CARTESIAN_POINT('Ctrl Pts',(3.39440972599995,11.6,10.455495084));
#217282=CARTESIAN_POINT('Ctrl Pts',(3.39253865299994,15.2,10.453087944));
#217283=CARTESIAN_POINT('Ctrl Pts',(3.39253865299994,11.6,10.453087944));
#217284=CARTESIAN_POINT('Ctrl Pts',(3.39067281599994,15.2,10.450683492));
#217285=CARTESIAN_POINT('Ctrl Pts',(3.39067281599994,11.6,10.450683492));
#217286=CARTESIAN_POINT('Ctrl Pts',(3.38881221399994,15.2,10.448281741));
#217287=CARTESIAN_POINT('Ctrl Pts',(3.38881221399994,11.6,10.448281741));
#217288=CARTESIAN_POINT('Ctrl Pts',(3.38695684699994,15.2,10.445882701));
#217289=CARTESIAN_POINT('Ctrl Pts',(3.38695684699994,11.6,10.445882701));
#217290=CARTESIAN_POINT('Ctrl Pts',(3.38510671499994,15.2,10.443486385));
#217291=CARTESIAN_POINT('Ctrl Pts',(3.38510671499994,11.6,10.443486385));
#217292=CARTESIAN_POINT('Ctrl Pts',(3.38326181899995,15.2,10.441092806));
#217293=CARTESIAN_POINT('Ctrl Pts',(3.38326181899995,11.6,10.441092806));
#217294=CARTESIAN_POINT('Ctrl Pts',(3.38142215599994,15.2,10.438701973));
#217295=CARTESIAN_POINT('Ctrl Pts',(3.38142215599994,11.6,10.438701973));
#217296=CARTESIAN_POINT('Ctrl Pts',(3.37958772799994,15.2,10.436313903));
#217297=CARTESIAN_POINT('Ctrl Pts',(3.37958772799994,11.6,10.436313903));
#217298=CARTESIAN_POINT('Ctrl Pts',(3.37775853499994,15.2,10.433928604));
#217299=CARTESIAN_POINT('Ctrl Pts',(3.37775853499994,11.6,10.433928604));
#217300=CARTESIAN_POINT('Ctrl Pts',(3.37593457599994,15.2,10.43154609));
#217301=CARTESIAN_POINT('Ctrl Pts',(3.37593457599994,11.6,10.43154609));
#217302=CARTESIAN_POINT('Ctrl Pts',(3.37411584999994,15.2,10.429166374));
#217303=CARTESIAN_POINT('Ctrl Pts',(3.37411584999994,11.6,10.429166374));
#217304=CARTESIAN_POINT('Ctrl Pts',(3.37230235899994,15.2,10.426789465));
#217305=CARTESIAN_POINT('Ctrl Pts',(3.37230235899994,11.6,10.426789465));
#217306=CARTESIAN_POINT('Ctrl Pts',(3.37049410099994,15.2,10.424415378));
#217307=CARTESIAN_POINT('Ctrl Pts',(3.37049410099994,11.6,10.424415378));
#217308=CARTESIAN_POINT('Ctrl Pts',(3.36869107699994,15.2,10.422044126));
#217309=CARTESIAN_POINT('Ctrl Pts',(3.36869107699994,11.6,10.422044126));
#217310=CARTESIAN_POINT('Ctrl Pts',(3.36689328399994,15.2,10.419675719));
#217311=CARTESIAN_POINT('Ctrl Pts',(3.36689328399994,11.6,10.419675719));
#217312=CARTESIAN_POINT('Ctrl Pts',(3.36510072599994,15.2,10.417310171));
#217313=CARTESIAN_POINT('Ctrl Pts',(3.36510072599994,11.6,10.417310171));
#217314=CARTESIAN_POINT('Ctrl Pts',(3.36331339899994,15.2,10.414947493));
#217315=CARTESIAN_POINT('Ctrl Pts',(3.36331339899994,11.6,10.414947493));
#217316=CARTESIAN_POINT('Ctrl Pts',(3.36153130499994,15.2,10.412587698));
#217317=CARTESIAN_POINT('Ctrl Pts',(3.36153130499994,11.6,10.412587698));
#217318=CARTESIAN_POINT('Ctrl Pts',(3.35975444299994,15.2,10.410230799));
#217319=CARTESIAN_POINT('Ctrl Pts',(3.35975444299994,11.6,10.410230799));
#217320=CARTESIAN_POINT('Ctrl Pts',(3.35798281299994,15.2,10.407876808));
#217321=CARTESIAN_POINT('Ctrl Pts',(3.35798281299994,11.6,10.407876808));
#217322=CARTESIAN_POINT('Ctrl Pts',(3.35621641399994,15.2,10.405525737));
#217323=CARTESIAN_POINT('Ctrl Pts',(3.35621641399994,11.6,10.405525737));
#217324=CARTESIAN_POINT('Ctrl Pts',(3.35445524599994,15.2,10.4031776));
#217325=CARTESIAN_POINT('Ctrl Pts',(3.35445524599994,11.6,10.4031776));
#217326=CARTESIAN_POINT('Ctrl Pts',(3.35269930899994,15.2,10.400832408));
#217327=CARTESIAN_POINT('Ctrl Pts',(3.35269930899994,11.6,10.400832408));
#217328=CARTESIAN_POINT('Ctrl Pts',(3.35094860199994,15.2,10.398490174));
#217329=CARTESIAN_POINT('Ctrl Pts',(3.35094860199994,11.6,10.398490174));
#217330=CARTESIAN_POINT('Ctrl Pts',(3.34920312499994,15.2,10.396150911));
#217331=CARTESIAN_POINT('Ctrl Pts',(3.34920312499994,11.6,10.396150911));
#217332=CARTESIAN_POINT('Ctrl Pts',(3.34746287999995,15.2,10.393814631));
#217333=CARTESIAN_POINT('Ctrl Pts',(3.34746287999995,11.6,10.393814631));
#217334=CARTESIAN_POINT('Ctrl Pts',(3.34572786099995,15.2,10.391481347));
#217335=CARTESIAN_POINT('Ctrl Pts',(3.34572786099995,11.6,10.391481347));
#217336=CARTESIAN_POINT('Ctrl Pts',(3.34399807299994,15.2,10.389151072));
#217337=CARTESIAN_POINT('Ctrl Pts',(3.34399807299994,11.6,10.389151072));
#217338=CARTESIAN_POINT('Ctrl Pts',(3.34227351299994,15.2,10.386823818));
#217339=CARTESIAN_POINT('Ctrl Pts',(3.34227351299994,11.6,10.386823818));
#217340=CARTESIAN_POINT('Ctrl Pts',(3.34055418199994,15.2,10.384499599));
#217341=CARTESIAN_POINT('Ctrl Pts',(3.34055418199994,11.6,10.384499599));
#217342=CARTESIAN_POINT('Ctrl Pts',(3.33884007799994,15.2,10.382178427));
#217343=CARTESIAN_POINT('Ctrl Pts',(3.33884007799994,11.6,10.382178427));
#217344=CARTESIAN_POINT('Ctrl Pts',(3.33713120199994,15.2,10.379860313));
#217345=CARTESIAN_POINT('Ctrl Pts',(3.33713120199994,11.6,10.379860313));
#217346=CARTESIAN_POINT('Ctrl Pts',(3.33542755199994,15.2,10.377545274));
#217347=CARTESIAN_POINT('Ctrl Pts',(3.33542755199994,11.6,10.377545274));
#217348=CARTESIAN_POINT('Ctrl Pts',(3.33372912899994,15.2,10.375233319));
#217349=CARTESIAN_POINT('Ctrl Pts',(3.33372912899994,11.6,10.375233319));
#217350=CARTESIAN_POINT('Ctrl Pts',(3.33203593199995,15.2,10.372924463));
#217351=CARTESIAN_POINT('Ctrl Pts',(3.33203593199995,11.6,10.372924463));
#217352=CARTESIAN_POINT('Ctrl Pts',(3.33034796099994,15.2,10.370618718));
#217353=CARTESIAN_POINT('Ctrl Pts',(3.33034796099994,11.6,10.370618718));
#217354=CARTESIAN_POINT('Ctrl Pts',(3.32866521499994,15.2,10.368316097));
#217355=CARTESIAN_POINT('Ctrl Pts',(3.32866521499994,11.6,10.368316097));
#217356=CARTESIAN_POINT('Ctrl Pts',(3.32698769299994,15.2,10.366016614));
#217357=CARTESIAN_POINT('Ctrl Pts',(3.32698769299994,11.6,10.366016614));
#217358=CARTESIAN_POINT('Ctrl Pts',(3.32531539599994,15.2,10.36372028));
#217359=CARTESIAN_POINT('Ctrl Pts',(3.32531539599994,11.6,10.36372028));
#217360=CARTESIAN_POINT('Ctrl Pts',(3.32364832199994,15.2,10.36142711));
#217361=CARTESIAN_POINT('Ctrl Pts',(3.32364832199994,11.6,10.36142711));
#217362=CARTESIAN_POINT('Ctrl Pts',(3.32198647199994,15.2,10.359137117));
#217363=CARTESIAN_POINT('Ctrl Pts',(3.32198647199994,11.6,10.359137117));
#217364=CARTESIAN_POINT('Ctrl Pts',(3.32032984499994,15.2,10.356850313));
#217365=CARTESIAN_POINT('Ctrl Pts',(3.32032984499994,11.6,10.356850313));
#217366=CARTESIAN_POINT('Ctrl Pts',(3.31867843899994,15.2,10.354566712));
#217367=CARTESIAN_POINT('Ctrl Pts',(3.31867843899994,11.6,10.354566712));
#217368=CARTESIAN_POINT('Ctrl Pts',(3.31703225499994,15.2,10.352286327));
#217369=CARTESIAN_POINT('Ctrl Pts',(3.31703225499994,11.6,10.352286327));
#217370=CARTESIAN_POINT('Ctrl Pts',(3.31539129199995,15.2,10.35000917));
#217371=CARTESIAN_POINT('Ctrl Pts',(3.31539129199995,11.6,10.35000917));
#217372=CARTESIAN_POINT('Ctrl Pts',(3.31375554899994,15.2,10.347735256));
#217373=CARTESIAN_POINT('Ctrl Pts',(3.31375554899994,11.6,10.347735256));
#217374=CARTESIAN_POINT('Ctrl Pts',(3.31212502599994,15.2,10.345464598));
#217375=CARTESIAN_POINT('Ctrl Pts',(3.31212502599994,11.6,10.345464598));
#217376=CARTESIAN_POINT('Ctrl Pts',(3.31049972299994,15.2,10.343197209));
#217377=CARTESIAN_POINT('Ctrl Pts',(3.31049972299994,11.6,10.343197209));
#217378=CARTESIAN_POINT('Ctrl Pts',(3.30887963899994,15.2,10.340933102));
#217379=CARTESIAN_POINT('Ctrl Pts',(3.30887963899994,11.6,10.340933102));
#217380=CARTESIAN_POINT('Ctrl Pts',(3.30726477099994,15.2,10.33867229));
#217381=CARTESIAN_POINT('Ctrl Pts',(3.30726477099994,11.6,10.33867229));
#217382=CARTESIAN_POINT('Ctrl Pts',(3.30565512199994,15.2,10.336414786));
#217383=CARTESIAN_POINT('Ctrl Pts',(3.30565512199994,11.6,10.336414786));
#217384=CARTESIAN_POINT('Ctrl Pts',(3.30405068899994,15.2,10.334160606));
#217385=CARTESIAN_POINT('Ctrl Pts',(3.30405068899994,11.6,10.334160606));
#217386=CARTESIAN_POINT('Ctrl Pts',(3.30245147199994,15.2,10.331909762));
#217387=CARTESIAN_POINT('Ctrl Pts',(3.30245147199994,11.6,10.331909762));
#217388=CARTESIAN_POINT('Ctrl Pts',(3.30085747199994,15.2,10.329662268));
#217389=CARTESIAN_POINT('Ctrl Pts',(3.30085747199994,11.6,10.329662268));
#217390=CARTESIAN_POINT('Ctrl Pts',(3.29926868599994,15.2,10.327418135));
#217391=CARTESIAN_POINT('Ctrl Pts',(3.29926868599994,11.6,10.327418135));
#217392=CARTESIAN_POINT('Ctrl Pts',(3.29768511299994,15.2,10.325177379));
#217393=CARTESIAN_POINT('Ctrl Pts',(3.29768511299994,11.6,10.325177379));
#217394=CARTESIAN_POINT('Ctrl Pts',(3.29610675499994,15.2,10.322940014));
#217395=CARTESIAN_POINT('Ctrl Pts',(3.29610675499994,11.6,10.322940014));
#217396=CARTESIAN_POINT('Ctrl Pts',(3.29453360899994,15.2,10.320706052));
#217397=CARTESIAN_POINT('Ctrl Pts',(3.29453360899994,11.6,10.320706052));
#217398=CARTESIAN_POINT('Ctrl Pts',(3.29296567499994,15.2,10.318475509));
#217399=CARTESIAN_POINT('Ctrl Pts',(3.29296567499994,11.6,10.318475509));
#217400=CARTESIAN_POINT('Ctrl Pts',(3.29140295199994,15.2,10.316248395));
#217401=CARTESIAN_POINT('Ctrl Pts',(3.29140295199994,11.6,10.316248395));
#217402=CARTESIAN_POINT('Ctrl Pts',(3.28984543999994,15.2,10.314024727));
#217403=CARTESIAN_POINT('Ctrl Pts',(3.28984543999994,11.6,10.314024727));
#217404=CARTESIAN_POINT('Ctrl Pts',(3.28829313699994,15.2,10.311804518));
#217405=CARTESIAN_POINT('Ctrl Pts',(3.28829313699994,11.6,10.311804518));
#217406=CARTESIAN_POINT('Ctrl Pts',(3.28674604399994,15.2,10.30958778));
#217407=CARTESIAN_POINT('Ctrl Pts',(3.28674604399994,11.6,10.30958778));
#217408=CARTESIAN_POINT('Ctrl Pts',(3.28520415899995,15.2,10.307374529));
#217409=CARTESIAN_POINT('Ctrl Pts',(3.28520415899995,11.6,10.307374529));
#217410=CARTESIAN_POINT('Ctrl Pts',(3.28366748099994,15.2,10.305164779));
#217411=CARTESIAN_POINT('Ctrl Pts',(3.28366748099994,11.6,10.305164779));
#217412=CARTESIAN_POINT('Ctrl Pts',(3.28213600999995,15.2,10.302958542));
#217413=CARTESIAN_POINT('Ctrl Pts',(3.28213600999995,11.6,10.302958542));
#217414=CARTESIAN_POINT('Ctrl Pts',(3.28060974399994,15.2,10.300755834));
#217415=CARTESIAN_POINT('Ctrl Pts',(3.28060974399994,11.6,10.300755834));
#217416=CARTESIAN_POINT('Ctrl Pts',(3.27908868399994,15.2,10.298556666));
#217417=CARTESIAN_POINT('Ctrl Pts',(3.27908868399994,11.6,10.298556666));
#217418=CARTESIAN_POINT('Ctrl Pts',(3.27757282699995,15.2,10.296361056));
#217419=CARTESIAN_POINT('Ctrl Pts',(3.27757282699995,11.6,10.296361056));
#217420=CARTESIAN_POINT('Ctrl Pts',(3.27606217499994,15.2,10.294169016));
#217421=CARTESIAN_POINT('Ctrl Pts',(3.27606217499994,11.6,10.294169016));
#217422=CARTESIAN_POINT('Ctrl Pts',(3.27455672399994,15.2,10.291980559));
#217423=CARTESIAN_POINT('Ctrl Pts',(3.27455672399994,11.6,10.291980559));
#217424=CARTESIAN_POINT('Ctrl Pts',(3.27305647499994,15.2,10.2897957));
#217425=CARTESIAN_POINT('Ctrl Pts',(3.27305647499994,11.6,10.2897957));
#217426=CARTESIAN_POINT('Ctrl Pts',(3.27156142599994,15.2,10.287614454));
#217427=CARTESIAN_POINT('Ctrl Pts',(3.27156142599994,11.6,10.287614454));
#217428=CARTESIAN_POINT('Ctrl Pts',(3.27007157799994,15.2,10.285436836));
#217429=CARTESIAN_POINT('Ctrl Pts',(3.27007157799994,11.6,10.285436836));
#217430=CARTESIAN_POINT('Ctrl Pts',(3.26858692799994,15.2,10.283262858));
#217431=CARTESIAN_POINT('Ctrl Pts',(3.26858692799994,11.6,10.283262858));
#217432=CARTESIAN_POINT('Ctrl Pts',(3.26710747499994,15.2,10.281092534));
#217433=CARTESIAN_POINT('Ctrl Pts',(3.26710747499994,11.6,10.281092534));
#217434=CARTESIAN_POINT('Ctrl Pts',(3.26563321999994,15.2,10.27892588));
#217435=CARTESIAN_POINT('Ctrl Pts',(3.26563321999994,11.6,10.27892588));
#217436=CARTESIAN_POINT('Ctrl Pts',(3.26416416099994,15.2,10.276762911));
#217437=CARTESIAN_POINT('Ctrl Pts',(3.26416416099994,11.6,10.276762911));
#217438=CARTESIAN_POINT('Ctrl Pts',(3.26270029699995,15.2,10.274603639));
#217439=CARTESIAN_POINT('Ctrl Pts',(3.26270029699995,11.6,10.274603639));
#217440=CARTESIAN_POINT('Ctrl Pts',(3.26124162699994,15.2,10.272448079));
#217441=CARTESIAN_POINT('Ctrl Pts',(3.26124162699994,11.6,10.272448079));
#217442=CARTESIAN_POINT('Ctrl Pts',(3.25978815099994,15.2,10.270296246));
#217443=CARTESIAN_POINT('Ctrl Pts',(3.25978815099994,11.6,10.270296246));
#217444=CARTESIAN_POINT('Ctrl Pts',(3.25833986599994,15.2,10.268148156));
#217445=CARTESIAN_POINT('Ctrl Pts',(3.25833986599994,11.6,10.268148156));
#217446=CARTESIAN_POINT('Ctrl Pts',(3.25689677199994,15.2,10.266003821));
#217447=CARTESIAN_POINT('Ctrl Pts',(3.25689677199994,11.6,10.266003821));
#217448=CARTESIAN_POINT('Ctrl Pts',(3.25545886799994,15.2,10.263863257));
#217449=CARTESIAN_POINT('Ctrl Pts',(3.25545886799994,11.6,10.263863257));
#217450=CARTESIAN_POINT('Ctrl Pts',(3.25402615299994,15.2,10.261726478));
#217451=CARTESIAN_POINT('Ctrl Pts',(3.25402615299994,11.6,10.261726478));
#217452=CARTESIAN_POINT('Ctrl Pts',(3.25259862599995,15.2,10.259593498));
#217453=CARTESIAN_POINT('Ctrl Pts',(3.25259862599995,11.6,10.259593498));
#217454=CARTESIAN_POINT('Ctrl Pts',(3.25117628599994,15.2,10.257464334));
#217455=CARTESIAN_POINT('Ctrl Pts',(3.25117628599994,11.6,10.257464334));
#217456=CARTESIAN_POINT('Ctrl Pts',(3.24975913199995,15.2,10.255338999));
#217457=CARTESIAN_POINT('Ctrl Pts',(3.24975913199995,11.6,10.255338999));
#217458=CARTESIAN_POINT('Ctrl Pts',(3.24834716199994,15.2,10.253217507));
#217459=CARTESIAN_POINT('Ctrl Pts',(3.24834716199994,11.6,10.253217507));
#217460=CARTESIAN_POINT('Ctrl Pts',(3.24694037599994,15.2,10.251099875));
#217461=CARTESIAN_POINT('Ctrl Pts',(3.24694037599994,11.6,10.251099875));
#217462=CARTESIAN_POINT('Ctrl Pts',(3.24553877199994,15.2,10.248986116));
#217463=CARTESIAN_POINT('Ctrl Pts',(3.24553877199994,11.6,10.248986116));
#217464=CARTESIAN_POINT('Ctrl Pts',(3.24414234999994,15.2,10.246876245));
#217465=CARTESIAN_POINT('Ctrl Pts',(3.24414234999994,11.6,10.246876245));
#217466=CARTESIAN_POINT('Ctrl Pts',(3.24275110699995,15.2,10.244770278));
#217467=CARTESIAN_POINT('Ctrl Pts',(3.24275110699995,11.6,10.244770278));
#217468=CARTESIAN_POINT('Ctrl Pts',(3.24136504399994,15.2,10.242668229));
#217469=CARTESIAN_POINT('Ctrl Pts',(3.24136504399994,11.6,10.242668229));
#217470=CARTESIAN_POINT('Ctrl Pts',(3.23998415799994,15.2,10.240570115));
#217471=CARTESIAN_POINT('Ctrl Pts',(3.23998415799994,11.6,10.240570115));
#217472=CARTESIAN_POINT('Ctrl Pts',(3.23860844899994,15.2,10.238475948));
#217473=CARTESIAN_POINT('Ctrl Pts',(3.23860844899994,11.6,10.238475948));
#217474=CARTESIAN_POINT('Ctrl Pts',(3.23723791499994,15.2,10.236385745));
#217475=CARTESIAN_POINT('Ctrl Pts',(3.23723791499994,11.6,10.236385745));
#217476=CARTESIAN_POINT('Ctrl Pts',(3.23587255499994,15.2,10.23429952));
#217477=CARTESIAN_POINT('Ctrl Pts',(3.23587255499994,11.6,10.23429952));
#217478=CARTESIAN_POINT('Ctrl Pts',(3.23451236799994,15.2,10.232217288));
#217479=CARTESIAN_POINT('Ctrl Pts',(3.23451236799994,11.6,10.232217288));
#217480=CARTESIAN_POINT('Ctrl Pts',(3.23315735299994,15.2,10.230139067));
#217481=CARTESIAN_POINT('Ctrl Pts',(3.23315735299994,11.6,10.230139067));
#217482=CARTESIAN_POINT('Ctrl Pts',(3.23180750799994,15.2,10.228064869));
#217483=CARTESIAN_POINT('Ctrl Pts',(3.23180750799994,11.6,10.228064869));
#217484=CARTESIAN_POINT('Ctrl Pts',(3.23046283199994,15.2,10.225994711));
#217485=CARTESIAN_POINT('Ctrl Pts',(3.23046283199994,11.6,10.225994711));
#217486=CARTESIAN_POINT('Ctrl Pts',(3.22912332499994,15.2,10.223928608));
#217487=CARTESIAN_POINT('Ctrl Pts',(3.22912332499994,11.6,10.223928608));
#217488=CARTESIAN_POINT('Ctrl Pts',(3.22778898299994,15.2,10.221866575));
#217489=CARTESIAN_POINT('Ctrl Pts',(3.22778898299994,11.6,10.221866575));
#217490=CARTESIAN_POINT('Ctrl Pts',(3.22645980699994,15.2,10.219808628));
#217491=CARTESIAN_POINT('Ctrl Pts',(3.22645980699994,11.6,10.219808628));
#217492=CARTESIAN_POINT('Ctrl Pts',(3.22513579399994,15.2,10.217754781));
#217493=CARTESIAN_POINT('Ctrl Pts',(3.22513579399994,11.6,10.217754781));
#217494=CARTESIAN_POINT('Ctrl Pts',(3.22381694499994,15.2,10.215705052));
#217495=CARTESIAN_POINT('Ctrl Pts',(3.22381694499994,11.6,10.215705052));
#217496=CARTESIAN_POINT('Ctrl Pts',(3.22250325599994,15.2,10.213659454));
#217497=CARTESIAN_POINT('Ctrl Pts',(3.22250325599994,11.6,10.213659454));
#217498=CARTESIAN_POINT('Ctrl Pts',(3.22119472699995,15.2,10.211618004));
#217499=CARTESIAN_POINT('Ctrl Pts',(3.22119472699995,11.6,10.211618004));
#217500=CARTESIAN_POINT('Ctrl Pts',(3.21989135599994,15.2,10.209580717));
#217501=CARTESIAN_POINT('Ctrl Pts',(3.21989135599994,11.6,10.209580717));
#217502=CARTESIAN_POINT('Ctrl Pts',(3.21859314299994,15.2,10.20754761));
#217503=CARTESIAN_POINT('Ctrl Pts',(3.21859314299994,11.6,10.20754761));
#217504=CARTESIAN_POINT('Ctrl Pts',(3.21730008399994,15.2,10.205518696));
#217505=CARTESIAN_POINT('Ctrl Pts',(3.21730008399994,11.6,10.205518696));
#217506=CARTESIAN_POINT('Ctrl Pts',(3.21601217999994,15.2,10.203493994));
#217507=CARTESIAN_POINT('Ctrl Pts',(3.21601217999994,11.6,10.203493994));
#217508=CARTESIAN_POINT('Ctrl Pts',(3.21472942799994,15.2,10.201473517));
#217509=CARTESIAN_POINT('Ctrl Pts',(3.21472942799994,11.6,10.201473517));
#217510=CARTESIAN_POINT('Ctrl Pts',(3.21345182799994,15.2,10.199457283));
#217511=CARTESIAN_POINT('Ctrl Pts',(3.21345182799994,11.6,10.199457283));
#217512=CARTESIAN_POINT('Ctrl Pts',(3.21217937699994,15.2,10.197445307));
#217513=CARTESIAN_POINT('Ctrl Pts',(3.21217937699994,11.6,10.197445307));
#217514=CARTESIAN_POINT('Ctrl Pts',(3.21091207399995,15.2,10.195437604));
#217515=CARTESIAN_POINT('Ctrl Pts',(3.21091207399995,11.6,10.195437604));
#217516=CARTESIAN_POINT('Ctrl Pts',(3.20964991799995,15.2,10.193434192));
#217517=CARTESIAN_POINT('Ctrl Pts',(3.20964991799995,11.6,10.193434192));
#217518=CARTESIAN_POINT('Ctrl Pts',(3.20839290699994,15.2,10.191435086));
#217519=CARTESIAN_POINT('Ctrl Pts',(3.20839290699994,11.6,10.191435086));
#217520=CARTESIAN_POINT('Ctrl Pts',(3.20714103999994,15.2,10.189440301));
#217521=CARTESIAN_POINT('Ctrl Pts',(3.20714103999994,11.6,10.189440301));
#217522=CARTESIAN_POINT('Ctrl Pts',(3.20589431499994,15.2,10.187449854));
#217523=CARTESIAN_POINT('Ctrl Pts',(3.20589431499994,11.6,10.187449854));
#217524=CARTESIAN_POINT('Ctrl Pts',(3.20465272999995,15.2,10.185463762));
#217525=CARTESIAN_POINT('Ctrl Pts',(3.20465272999995,11.6,10.185463762));
#217526=CARTESIAN_POINT('Ctrl Pts',(3.20341628299994,15.2,10.183482041));
#217527=CARTESIAN_POINT('Ctrl Pts',(3.20341628299994,11.6,10.183482041));
#217528=CARTESIAN_POINT('Ctrl Pts',(3.20218497399994,15.2,10.181504705));
#217529=CARTESIAN_POINT('Ctrl Pts',(3.20218497399994,11.6,10.181504705));
#217530=CARTESIAN_POINT('Ctrl Pts',(3.20095880099994,15.2,10.179531773));
#217531=CARTESIAN_POINT('Ctrl Pts',(3.20095880099994,11.6,10.179531773));
#217532=CARTESIAN_POINT('Ctrl Pts',(3.19973776199994,15.2,10.17756326));
#217533=CARTESIAN_POINT('Ctrl Pts',(3.19973776199994,11.6,10.17756326));
#217534=CARTESIAN_POINT('Ctrl Pts',(3.19852185399994,15.2,10.175599184));
#217535=CARTESIAN_POINT('Ctrl Pts',(3.19852185399994,11.6,10.175599184));
#217536=CARTESIAN_POINT('Ctrl Pts',(3.19731107699994,15.2,10.173639559));
#217537=CARTESIAN_POINT('Ctrl Pts',(3.19731107699994,11.6,10.173639559));
#217538=CARTESIAN_POINT('Ctrl Pts',(3.19610542999994,15.2,10.171684403));
#217539=CARTESIAN_POINT('Ctrl Pts',(3.19610542999994,11.6,10.171684403));
#217540=CARTESIAN_POINT('Ctrl Pts',(3.19490490899994,15.2,10.169733732));
#217541=CARTESIAN_POINT('Ctrl Pts',(3.19490490899994,11.6,10.169733732));
#217542=CARTESIAN_POINT('Ctrl Pts',(3.19370951399994,15.2,10.167787564));
#217543=CARTESIAN_POINT('Ctrl Pts',(3.19370951399994,11.6,10.167787564));
#217544=CARTESIAN_POINT('Ctrl Pts',(3.19251924199994,15.2,10.165845913));
#217545=CARTESIAN_POINT('Ctrl Pts',(3.19251924199994,11.6,10.165845913));
#217546=CARTESIAN_POINT('Ctrl Pts',(3.19133409399994,15.2,10.163908798));
#217547=CARTESIAN_POINT('Ctrl Pts',(3.19133409399994,11.6,10.163908798));
#217548=CARTESIAN_POINT('Ctrl Pts',(3.19015406399994,15.2,10.161976234));
#217549=CARTESIAN_POINT('Ctrl Pts',(3.19015406399994,11.6,10.161976234));
#217550=CARTESIAN_POINT('Ctrl Pts',(3.18897915299994,15.2,10.160048239));
#217551=CARTESIAN_POINT('Ctrl Pts',(3.18897915299994,11.6,10.160048239));
#217552=CARTESIAN_POINT('Ctrl Pts',(3.18780935899994,15.2,10.158124831));
#217553=CARTESIAN_POINT('Ctrl Pts',(3.18780935899994,11.6,10.158124831));
#217554=CARTESIAN_POINT('Ctrl Pts',(3.18664467899994,15.2,10.156206023));
#217555=CARTESIAN_POINT('Ctrl Pts',(3.18664467899994,11.6,10.156206023));
#217556=CARTESIAN_POINT('Ctrl Pts',(3.18548511399994,15.2,10.154291836));
#217557=CARTESIAN_POINT('Ctrl Pts',(3.18548511399994,11.6,10.154291836));
#217558=CARTESIAN_POINT('Ctrl Pts',(3.18433065699995,15.2,10.152382285));
#217559=CARTESIAN_POINT('Ctrl Pts',(3.18433065699995,11.6,10.152382285));
#217560=CARTESIAN_POINT('Ctrl Pts',(3.18318131199995,15.2,10.150477387));
#217561=CARTESIAN_POINT('Ctrl Pts',(3.18318131199995,11.6,10.150477387));
#217562=CARTESIAN_POINT('Ctrl Pts',(3.18203707299994,15.2,10.148577159));
#217563=CARTESIAN_POINT('Ctrl Pts',(3.18203707299994,11.6,10.148577159));
#217564=CARTESIAN_POINT('Ctrl Pts',(3.18089793999994,15.2,10.146681619));
#217565=CARTESIAN_POINT('Ctrl Pts',(3.18089793999994,11.6,10.146681619));
#217566=CARTESIAN_POINT('Ctrl Pts',(3.17976390999994,15.2,10.144790784));
#217567=CARTESIAN_POINT('Ctrl Pts',(3.17976390999994,11.6,10.144790784));
#217568=CARTESIAN_POINT('Ctrl Pts',(3.17863498099995,15.2,10.142904671));
#217569=CARTESIAN_POINT('Ctrl Pts',(3.17863498099995,11.6,10.142904671));
#217570=CARTESIAN_POINT('Ctrl Pts',(3.17751115299994,15.2,10.141023297));
#217571=CARTESIAN_POINT('Ctrl Pts',(3.17751115299994,11.6,10.141023297));
#217572=CARTESIAN_POINT('Ctrl Pts',(3.17639242199995,15.2,10.13914668));
#217573=CARTESIAN_POINT('Ctrl Pts',(3.17639242199995,11.6,10.13914668));
#217574=CARTESIAN_POINT('Ctrl Pts',(3.17527878599994,15.2,10.137274836));
#217575=CARTESIAN_POINT('Ctrl Pts',(3.17527878599994,11.6,10.137274836));
#217576=CARTESIAN_POINT('Ctrl Pts',(3.17417024399994,15.2,10.135407784));
#217577=CARTESIAN_POINT('Ctrl Pts',(3.17417024399994,11.6,10.135407784));
#217578=CARTESIAN_POINT('Ctrl Pts',(3.17306679399994,15.2,10.133545542));
#217579=CARTESIAN_POINT('Ctrl Pts',(3.17306679399994,11.6,10.133545542));
#217580=CARTESIAN_POINT('Ctrl Pts',(3.17196843199994,15.2,10.131688125));
#217581=CARTESIAN_POINT('Ctrl Pts',(3.17196843199994,11.6,10.131688125));
#217582=CARTESIAN_POINT('Ctrl Pts',(3.17087515899994,15.2,10.129835553));
#217583=CARTESIAN_POINT('Ctrl Pts',(3.17087515899994,11.6,10.129835553));
#217584=CARTESIAN_POINT('Ctrl Pts',(3.16978697099994,15.2,10.127987842));
#217585=CARTESIAN_POINT('Ctrl Pts',(3.16978697099994,11.6,10.127987842));
#217586=CARTESIAN_POINT('Ctrl Pts',(3.16870386699994,15.2,10.126145011));
#217587=CARTESIAN_POINT('Ctrl Pts',(3.16870386699994,11.6,10.126145011));
#217588=CARTESIAN_POINT('Ctrl Pts',(3.16762584299994,15.2,10.124307078));
#217589=CARTESIAN_POINT('Ctrl Pts',(3.16762584299994,11.6,10.124307078));
#217590=CARTESIAN_POINT('Ctrl Pts',(3.16655289799994,15.2,10.12247406));
#217591=CARTESIAN_POINT('Ctrl Pts',(3.16655289799994,11.6,10.12247406));
#217592=CARTESIAN_POINT('Ctrl Pts',(3.16548502999995,15.2,10.120645975));
#217593=CARTESIAN_POINT('Ctrl Pts',(3.16548502999995,11.6,10.120645975));
#217594=CARTESIAN_POINT('Ctrl Pts',(3.16442223699994,15.2,10.11882284));
#217595=CARTESIAN_POINT('Ctrl Pts',(3.16442223699994,11.6,10.11882284));
#217596=CARTESIAN_POINT('Ctrl Pts',(3.16336451599994,15.2,10.117004675));
#217597=CARTESIAN_POINT('Ctrl Pts',(3.16336451599994,11.6,10.117004675));
#217598=CARTESIAN_POINT('Ctrl Pts',(3.16231186499994,15.2,10.115191496));
#217599=CARTESIAN_POINT('Ctrl Pts',(3.16231186499994,11.6,10.115191496));
#217600=CARTESIAN_POINT('Ctrl Pts',(3.16126428299994,15.2,10.113383323));
#217601=CARTESIAN_POINT('Ctrl Pts',(3.16126428299994,11.6,10.113383323));
#217602=CARTESIAN_POINT('Ctrl Pts',(3.16022176599994,15.2,10.111580173));
#217603=CARTESIAN_POINT('Ctrl Pts',(3.16022176599994,11.6,10.111580173));
#217604=CARTESIAN_POINT('Ctrl Pts',(3.15918431399994,15.2,10.109782065));
#217605=CARTESIAN_POINT('Ctrl Pts',(3.15918431399994,11.6,10.109782065));
#217606=CARTESIAN_POINT('Ctrl Pts',(3.15815192199994,15.2,10.107989016));
#217607=CARTESIAN_POINT('Ctrl Pts',(3.15815192199994,11.6,10.107989016));
#217608=CARTESIAN_POINT('Ctrl Pts',(3.15712458699994,15.2,10.106201046));
#217609=CARTESIAN_POINT('Ctrl Pts',(3.15712458699994,11.6,10.106201046));
#217610=CARTESIAN_POINT('Ctrl Pts',(3.15610231199994,15.2,10.104418172));
#217611=CARTESIAN_POINT('Ctrl Pts',(3.15610231199994,11.6,10.104418172));
#217612=CARTESIAN_POINT('Ctrl Pts',(3.15508508899994,15.2,10.102640413));
#217613=CARTESIAN_POINT('Ctrl Pts',(3.15508508899994,11.6,10.102640413));
#217614=CARTESIAN_POINT('Ctrl Pts',(3.15407291799994,15.2,10.100867788));
#217615=CARTESIAN_POINT('Ctrl Pts',(3.15407291799994,11.6,10.100867788));
#217616=CARTESIAN_POINT('Ctrl Pts',(3.15306579799994,15.2,10.099100315));
#217617=CARTESIAN_POINT('Ctrl Pts',(3.15306579799994,11.6,10.099100315));
#217618=CARTESIAN_POINT('Ctrl Pts',(3.15206372299994,15.2,10.097338013));
#217619=CARTESIAN_POINT('Ctrl Pts',(3.15206372299994,11.6,10.097338013));
#217620=CARTESIAN_POINT('Ctrl Pts',(3.15106669299994,15.2,10.0955809));
#217621=CARTESIAN_POINT('Ctrl Pts',(3.15106669299994,11.6,10.0955809));
#217622=CARTESIAN_POINT('Ctrl Pts',(3.15007470599994,15.2,10.093828996));
#217623=CARTESIAN_POINT('Ctrl Pts',(3.15007470599994,11.6,10.093828996));
#217624=CARTESIAN_POINT('Ctrl Pts',(3.14908775899994,15.2,10.092082318));
#217625=CARTESIAN_POINT('Ctrl Pts',(3.14908775899994,11.6,10.092082318));
#217626=CARTESIAN_POINT('Ctrl Pts',(3.14810584799994,15.2,10.090340886));
#217627=CARTESIAN_POINT('Ctrl Pts',(3.14810584799994,11.6,10.090340886));
#217628=CARTESIAN_POINT('Ctrl Pts',(3.14712897199994,15.2,10.08860472));
#217629=CARTESIAN_POINT('Ctrl Pts',(3.14712897199994,11.6,10.08860472));
#217630=CARTESIAN_POINT('Ctrl Pts',(3.14615712899994,15.2,10.086873837));
#217631=CARTESIAN_POINT('Ctrl Pts',(3.14615712899994,11.6,10.086873837));
#217632=CARTESIAN_POINT('Ctrl Pts',(3.14519031499994,15.2,10.085148257));
#217633=CARTESIAN_POINT('Ctrl Pts',(3.14519031499994,11.6,10.085148257));
#217634=CARTESIAN_POINT('Ctrl Pts',(3.14422852799995,15.2,10.083427999));
#217635=CARTESIAN_POINT('Ctrl Pts',(3.14422852799995,11.6,10.083427999));
#217636=CARTESIAN_POINT('Ctrl Pts',(3.14327176599994,15.2,10.081713083));
#217637=CARTESIAN_POINT('Ctrl Pts',(3.14327176599994,11.6,10.081713083));
#217638=CARTESIAN_POINT('Ctrl Pts',(3.14232002399994,15.2,10.080003527));
#217639=CARTESIAN_POINT('Ctrl Pts',(3.14232002399994,11.6,10.080003527));
#217640=CARTESIAN_POINT('Ctrl Pts',(3.14137330399994,15.2,10.078299351));
#217641=CARTESIAN_POINT('Ctrl Pts',(3.14137330399994,11.6,10.078299351));
#217642=CARTESIAN_POINT('Ctrl Pts',(3.14043159899994,15.2,10.076600574));
#217643=CARTESIAN_POINT('Ctrl Pts',(3.14043159899994,11.6,10.076600574));
#217644=CARTESIAN_POINT('Ctrl Pts',(3.13949490699994,15.2,10.074907216));
#217645=CARTESIAN_POINT('Ctrl Pts',(3.13949490699994,11.6,10.074907216));
#217646=CARTESIAN_POINT('Ctrl Pts',(3.13856322699994,15.2,10.073219296));
#217647=CARTESIAN_POINT('Ctrl Pts',(3.13856322699994,11.6,10.073219296));
#217648=CARTESIAN_POINT('Ctrl Pts',(3.13763655599994,15.2,10.071536834));
#217649=CARTESIAN_POINT('Ctrl Pts',(3.13763655599994,11.6,10.071536834));
#217650=CARTESIAN_POINT('Ctrl Pts',(3.13671488999994,15.2,10.069859849));
#217651=CARTESIAN_POINT('Ctrl Pts',(3.13671488999994,11.6,10.069859849));
#217652=CARTESIAN_POINT('Ctrl Pts',(3.13579822699994,15.2,10.068188362));
#217653=CARTESIAN_POINT('Ctrl Pts',(3.13579822699994,11.6,10.068188362));
#217654=CARTESIAN_POINT('Ctrl Pts',(3.13488656499994,15.2,10.066522392));
#217655=CARTESIAN_POINT('Ctrl Pts',(3.13488656499994,11.6,10.066522392));
#217656=CARTESIAN_POINT('Ctrl Pts',(3.13397989999994,15.2,10.064861958));
#217657=CARTESIAN_POINT('Ctrl Pts',(3.13397989999994,11.6,10.064861958));
#217658=CARTESIAN_POINT('Ctrl Pts',(3.13307822999994,15.2,10.063207081));
#217659=CARTESIAN_POINT('Ctrl Pts',(3.13307822999994,11.6,10.063207081));
#217660=CARTESIAN_POINT('Ctrl Pts',(3.13218154999995,15.2,10.061557781));
#217661=CARTESIAN_POINT('Ctrl Pts',(3.13218154999995,11.6,10.061557781));
#217662=CARTESIAN_POINT('Ctrl Pts',(3.13128985999994,15.2,10.059914077));
#217663=CARTESIAN_POINT('Ctrl Pts',(3.13128985999994,11.6,10.059914077));
#217664=CARTESIAN_POINT('Ctrl Pts',(3.13040315599994,15.2,10.058275991));
#217665=CARTESIAN_POINT('Ctrl Pts',(3.13040315599994,11.6,10.058275991));
#217666=CARTESIAN_POINT('Ctrl Pts',(3.12952143499994,15.2,10.056643542));
#217667=CARTESIAN_POINT('Ctrl Pts',(3.12952143499994,11.6,10.056643542));
#217668=CARTESIAN_POINT('Ctrl Pts',(3.12864469399994,15.2,10.05501675));
#217669=CARTESIAN_POINT('Ctrl Pts',(3.12864469399994,11.6,10.05501675));
#217670=CARTESIAN_POINT('Ctrl Pts',(3.12777292999994,15.2,10.053395635));
#217671=CARTESIAN_POINT('Ctrl Pts',(3.12777292999994,11.6,10.053395635));
#217672=CARTESIAN_POINT('Ctrl Pts',(3.12690613999994,15.2,10.051780219));
#217673=CARTESIAN_POINT('Ctrl Pts',(3.12690613999994,11.6,10.051780219));
#217674=CARTESIAN_POINT('Ctrl Pts',(3.12604432099994,15.2,10.050170521));
#217675=CARTESIAN_POINT('Ctrl Pts',(3.12604432099994,11.6,10.050170521));
#217676=CARTESIAN_POINT('Ctrl Pts',(3.12518747099995,15.2,10.048566563));
#217677=CARTESIAN_POINT('Ctrl Pts',(3.12518747099995,11.6,10.048566563));
#217678=CARTESIAN_POINT('Ctrl Pts',(3.12433558499994,15.2,10.046968364));
#217679=CARTESIAN_POINT('Ctrl Pts',(3.12433558499994,11.6,10.046968364));
#217680=CARTESIAN_POINT('Ctrl Pts',(3.12348866099994,15.2,10.045375946));
#217681=CARTESIAN_POINT('Ctrl Pts',(3.12348866099994,11.6,10.045375946));
#217682=CARTESIAN_POINT('Ctrl Pts',(3.12264669699994,15.2,10.043789328));
#217683=CARTESIAN_POINT('Ctrl Pts',(3.12264669699994,11.6,10.043789328));
#217684=CARTESIAN_POINT('Ctrl Pts',(3.12180968799994,15.2,10.042208533));
#217685=CARTESIAN_POINT('Ctrl Pts',(3.12180968799994,11.6,10.042208533));
#217686=CARTESIAN_POINT('Ctrl Pts',(3.12097763099994,15.2,10.040633581));
#217687=CARTESIAN_POINT('Ctrl Pts',(3.12097763099994,11.6,10.040633581));
#217688=CARTESIAN_POINT('Ctrl Pts',(3.12015052399994,15.2,10.039064492));
#217689=CARTESIAN_POINT('Ctrl Pts',(3.12015052399994,11.6,10.039064492));
#217690=CARTESIAN_POINT('Ctrl Pts',(3.11932836299994,15.2,10.037501289));
#217691=CARTESIAN_POINT('Ctrl Pts',(3.11932836299994,11.6,10.037501289));
#217692=CARTESIAN_POINT('Ctrl Pts',(3.11851114499994,15.2,10.035943991));
#217693=CARTESIAN_POINT('Ctrl Pts',(3.11851114499994,11.6,10.035943991));
#217694=CARTESIAN_POINT('Ctrl Pts',(3.11769886699994,15.2,10.034392622));
#217695=CARTESIAN_POINT('Ctrl Pts',(3.11769886699994,11.6,10.034392622));
#217696=CARTESIAN_POINT('Ctrl Pts',(3.11689152499994,15.2,10.0328472));
#217697=CARTESIAN_POINT('Ctrl Pts',(3.11689152499994,11.6,10.0328472));
#217698=CARTESIAN_POINT('Ctrl Pts',(3.11608911699994,15.2,10.031307748));
#217699=CARTESIAN_POINT('Ctrl Pts',(3.11608911699994,11.6,10.031307748));
#217700=CARTESIAN_POINT('Ctrl Pts',(3.11529163799994,15.2,10.029774289));
#217701=CARTESIAN_POINT('Ctrl Pts',(3.11529163799994,11.6,10.029774289));
#217702=CARTESIAN_POINT('Ctrl Pts',(3.11449908499994,15.2,10.028246841));
#217703=CARTESIAN_POINT('Ctrl Pts',(3.11449908499994,11.6,10.028246841));
#217704=CARTESIAN_POINT('Ctrl Pts',(3.11371145699994,15.2,10.026725429));
#217705=CARTESIAN_POINT('Ctrl Pts',(3.11371145699994,11.6,10.026725429));
#217706=CARTESIAN_POINT('Ctrl Pts',(3.11292874799994,15.2,10.025210072));
#217707=CARTESIAN_POINT('Ctrl Pts',(3.11292874799994,11.6,10.025210072));
#217708=CARTESIAN_POINT('Ctrl Pts',(3.11215095499994,15.2,10.023700794));
#217709=CARTESIAN_POINT('Ctrl Pts',(3.11215095499994,11.6,10.023700794));
#217710=CARTESIAN_POINT('Ctrl Pts',(3.11137807399994,15.2,10.022197616));
#217711=CARTESIAN_POINT('Ctrl Pts',(3.11137807399994,11.6,10.022197616));
#217712=CARTESIAN_POINT('Ctrl Pts',(3.11061010399994,15.2,10.020700559));
#217713=CARTESIAN_POINT('Ctrl Pts',(3.11061010399994,11.6,10.020700559));
#217714=CARTESIAN_POINT('Ctrl Pts',(3.10984703899994,15.2,10.019209646));
#217715=CARTESIAN_POINT('Ctrl Pts',(3.10984703899994,11.6,10.019209646));
#217716=CARTESIAN_POINT('Ctrl Pts',(3.10908887599994,15.2,10.017724899));
#217717=CARTESIAN_POINT('Ctrl Pts',(3.10908887599994,11.6,10.017724899));
#217718=CARTESIAN_POINT('Ctrl Pts',(3.10833561299994,15.2,10.01624634));
#217719=CARTESIAN_POINT('Ctrl Pts',(3.10833561299994,11.6,10.01624634));
#217720=CARTESIAN_POINT('Ctrl Pts',(3.10758724499994,15.2,10.01477399));
#217721=CARTESIAN_POINT('Ctrl Pts',(3.10758724499994,11.6,10.01477399));
#217722=CARTESIAN_POINT('Ctrl Pts',(3.10684376799994,15.2,10.013307874));
#217723=CARTESIAN_POINT('Ctrl Pts',(3.10684376799994,11.6,10.013307874));
#217724=CARTESIAN_POINT('Ctrl Pts',(3.10610517999995,15.2,10.011848013));
#217725=CARTESIAN_POINT('Ctrl Pts',(3.10610517999995,11.6,10.011848013));
#217726=CARTESIAN_POINT('Ctrl Pts',(3.10537147499995,15.2,10.010394428));
#217727=CARTESIAN_POINT('Ctrl Pts',(3.10537147499995,11.6,10.010394428));
#217728=CARTESIAN_POINT('Ctrl Pts',(3.10464265199994,15.2,10.008947144));
#217729=CARTESIAN_POINT('Ctrl Pts',(3.10464265199994,11.6,10.008947144));
#217730=CARTESIAN_POINT('Ctrl Pts',(3.10391870499994,15.2,10.007506183));
#217731=CARTESIAN_POINT('Ctrl Pts',(3.10391870499994,11.6,10.007506183));
#217732=CARTESIAN_POINT('Ctrl Pts',(3.10319963199994,15.2,10.006071567));
#217733=CARTESIAN_POINT('Ctrl Pts',(3.10319963199994,11.6,10.006071567));
#217734=CARTESIAN_POINT('Ctrl Pts',(3.10248542799994,15.2,10.00464332));
#217735=CARTESIAN_POINT('Ctrl Pts',(3.10248542799994,11.6,10.00464332));
#217736=CARTESIAN_POINT('Ctrl Pts',(3.10177608999994,15.2,10.003221464));
#217737=CARTESIAN_POINT('Ctrl Pts',(3.10177608999994,11.6,10.003221464));
#217738=CARTESIAN_POINT('Ctrl Pts',(3.10107161399995,15.2,10.001806022));
#217739=CARTESIAN_POINT('Ctrl Pts',(3.10107161399995,11.6,10.001806022));
#217740=CARTESIAN_POINT('Ctrl Pts',(3.10037199499994,15.2,10.000397017));
#217741=CARTESIAN_POINT('Ctrl Pts',(3.10037199499994,11.6,10.000397017));
#217742=CARTESIAN_POINT('Ctrl Pts',(3.09967723099994,15.2,9.99899447299999));
#217743=CARTESIAN_POINT('Ctrl Pts',(3.09967723099994,11.6,9.99899447299999));
#217744=CARTESIAN_POINT('Ctrl Pts',(3.09898731599994,15.2,9.99759841199998));
#217745=CARTESIAN_POINT('Ctrl Pts',(3.09898731599994,11.6,9.99759841199998));
#217746=CARTESIAN_POINT('Ctrl Pts',(3.09830224899994,15.2,9.99620885899999));
#217747=CARTESIAN_POINT('Ctrl Pts',(3.09830224899994,11.6,9.99620885899999));
#217748=CARTESIAN_POINT('Ctrl Pts',(3.09762202399994,15.2,9.99482583699999));
#217749=CARTESIAN_POINT('Ctrl Pts',(3.09762202399994,11.6,9.99482583699999));
#217750=CARTESIAN_POINT('Ctrl Pts',(3.09694663699994,15.2,9.99344936799999));
#217751=CARTESIAN_POINT('Ctrl Pts',(3.09694663699994,11.6,9.99344936799999));
#217752=CARTESIAN_POINT('Ctrl Pts',(3.09627608499994,15.2,9.99207947799999));
#217753=CARTESIAN_POINT('Ctrl Pts',(3.09627608499994,11.6,9.99207947799999));
#217754=CARTESIAN_POINT('Ctrl Pts',(3.09561036199994,15.2,9.99071618899999));
#217755=CARTESIAN_POINT('Ctrl Pts',(3.09561036199994,11.6,9.99071618899999));
#217756=CARTESIAN_POINT('Ctrl Pts',(3.09494946499994,15.2,9.98935952599999));
#217757=CARTESIAN_POINT('Ctrl Pts',(3.09494946499994,11.6,9.98935952599999));
#217758=CARTESIAN_POINT('Ctrl Pts',(3.09429339099994,15.2,9.98800951199998));
#217759=CARTESIAN_POINT('Ctrl Pts',(3.09429339099994,11.6,9.98800951199998));
#217760=CARTESIAN_POINT('Ctrl Pts',(3.09364213499994,15.2,9.98666617199999));
#217761=CARTESIAN_POINT('Ctrl Pts',(3.09364213499994,11.6,9.98666617199999));
#217762=CARTESIAN_POINT('Ctrl Pts',(3.09299569299994,15.2,9.98532952799999));
#217763=CARTESIAN_POINT('Ctrl Pts',(3.09299569299994,11.6,9.98532952799999));
#217764=CARTESIAN_POINT('Ctrl Pts',(3.09235405999994,15.2,9.98399960799999));
#217765=CARTESIAN_POINT('Ctrl Pts',(3.09235405999994,11.6,9.98399960799999));
#217766=CARTESIAN_POINT('Ctrl Pts',(3.09171723299994,15.2,9.98267643199998));
#217767=CARTESIAN_POINT('Ctrl Pts',(3.09171723299994,11.6,9.98267643199998));
#217768=CARTESIAN_POINT('Ctrl Pts',(3.09108520699994,15.2,9.98136002699999));
#217769=CARTESIAN_POINT('Ctrl Pts',(3.09108520699994,11.6,9.98136002699999));
#217770=CARTESIAN_POINT('Ctrl Pts',(3.09045797699994,15.2,9.98005041799999));
#217771=CARTESIAN_POINT('Ctrl Pts',(3.09045797699994,11.6,9.98005041799999));
#217772=CARTESIAN_POINT('Ctrl Pts',(3.08983553999994,15.2,9.97874762799999));
#217773=CARTESIAN_POINT('Ctrl Pts',(3.08983553999994,11.6,9.97874762799999));
#217774=CARTESIAN_POINT('Ctrl Pts',(3.08921789099994,15.2,9.97745168099998));
#217775=CARTESIAN_POINT('Ctrl Pts',(3.08921789099994,11.6,9.97745168099998));
#217776=CARTESIAN_POINT('Ctrl Pts',(3.08860502499994,15.2,9.97616260499999));
#217777=CARTESIAN_POINT('Ctrl Pts',(3.08860502499994,11.6,9.97616260499999));
#217778=CARTESIAN_POINT('Ctrl Pts',(3.08799693999994,15.2,9.97488042299998));
#217779=CARTESIAN_POINT('Ctrl Pts',(3.08799693999994,11.6,9.97488042299998));
#217780=CARTESIAN_POINT('Ctrl Pts',(3.08739362899995,15.2,9.97360515799999));
#217781=CARTESIAN_POINT('Ctrl Pts',(3.08739362899995,11.6,9.97360515799999));
#217782=CARTESIAN_POINT('Ctrl Pts',(3.08679508799994,15.2,9.97233683899999));
#217783=CARTESIAN_POINT('Ctrl Pts',(3.08679508799994,11.6,9.97233683899999));
#217784=CARTESIAN_POINT('Ctrl Pts',(3.08620131299994,15.2,9.97107548899999));
#217785=CARTESIAN_POINT('Ctrl Pts',(3.08620131299994,11.6,9.97107548899999));
#217786=CARTESIAN_POINT('Ctrl Pts',(3.08561229999994,15.2,9.96982113299998));
#217787=CARTESIAN_POINT('Ctrl Pts',(3.08561229999994,11.6,9.96982113299998));
#217788=CARTESIAN_POINT('Ctrl Pts',(3.08502804299994,15.2,9.96857379799999));
#217789=CARTESIAN_POINT('Ctrl Pts',(3.08502804299994,11.6,9.96857379799999));
#217790=CARTESIAN_POINT('Ctrl Pts',(3.08444853899994,15.2,9.96733350799998));
#217791=CARTESIAN_POINT('Ctrl Pts',(3.08444853899994,11.6,9.96733350799998));
#217792=CARTESIAN_POINT('Ctrl Pts',(3.08387378199994,15.2,9.96610028999999));
#217793=CARTESIAN_POINT('Ctrl Pts',(3.08387378199994,11.6,9.96610028999999));
#217794=CARTESIAN_POINT('Ctrl Pts',(3.08330376799994,15.2,9.96487416799998));
#217795=CARTESIAN_POINT('Ctrl Pts',(3.08330376799994,11.6,9.96487416799998));
#217796=CARTESIAN_POINT('Ctrl Pts',(3.08273849199994,15.2,9.96365516999998));
#217797=CARTESIAN_POINT('Ctrl Pts',(3.08273849199994,11.6,9.96365516999998));
#217798=CARTESIAN_POINT('Ctrl Pts',(3.08217794999994,15.2,9.96244332099998));
#217799=CARTESIAN_POINT('Ctrl Pts',(3.08217794999994,11.6,9.96244332099998));
#217800=CARTESIAN_POINT('Ctrl Pts',(3.08162213499994,15.2,9.96123864599999));
#217801=CARTESIAN_POINT('Ctrl Pts',(3.08162213499994,11.6,9.96123864599999));
#217802=CARTESIAN_POINT('Ctrl Pts',(3.08107104499994,15.2,9.96004117299999));
#217803=CARTESIAN_POINT('Ctrl Pts',(3.08107104499994,11.6,9.96004117299999));
#217804=CARTESIAN_POINT('Ctrl Pts',(3.08052467399994,15.2,9.95885092599998));
#217805=CARTESIAN_POINT('Ctrl Pts',(3.08052467399994,11.6,9.95885092599998));
#217806=CARTESIAN_POINT('Ctrl Pts',(3.07998301799994,15.2,9.95766793499998));
#217807=CARTESIAN_POINT('Ctrl Pts',(3.07998301799994,11.6,9.95766793499998));
#217808=CARTESIAN_POINT('Ctrl Pts',(3.07944606999994,15.2,9.95649222299999));
#217809=CARTESIAN_POINT('Ctrl Pts',(3.07944606999994,11.6,9.95649222299999));
#217810=CARTESIAN_POINT('Ctrl Pts',(3.07891382499994,15.2,9.95532381799999));
#217811=CARTESIAN_POINT('Ctrl Pts',(3.07891382499994,11.6,9.95532381799999));
#217812=CARTESIAN_POINT('Ctrl Pts',(3.07838628099995,15.2,9.95416274699998));
#217813=CARTESIAN_POINT('Ctrl Pts',(3.07838628099995,11.6,9.95416274699998));
#217814=CARTESIAN_POINT('Ctrl Pts',(3.07786343199994,15.2,9.95300903699999));
#217815=CARTESIAN_POINT('Ctrl Pts',(3.07786343199994,11.6,9.95300903699999));
#217816=CARTESIAN_POINT('Ctrl Pts',(3.07734526999994,15.2,9.95186271399999));
#217817=CARTESIAN_POINT('Ctrl Pts',(3.07734526999994,11.6,9.95186271399999));
#217818=CARTESIAN_POINT('Ctrl Pts',(3.07683179299994,15.2,9.95072380599998));
#217819=CARTESIAN_POINT('Ctrl Pts',(3.07683179299994,11.6,9.95072380599998));
#217820=CARTESIAN_POINT('Ctrl Pts',(3.07632299499994,15.2,9.94959233999998));
#217821=CARTESIAN_POINT('Ctrl Pts',(3.07632299499994,11.6,9.94959233999998));
#217822=CARTESIAN_POINT('Ctrl Pts',(3.07581887099994,15.2,9.94846834399999));
#217823=CARTESIAN_POINT('Ctrl Pts',(3.07581887099994,11.6,9.94846834399999));
#217824=CARTESIAN_POINT('Ctrl Pts',(3.07531941599994,15.2,9.94735184399998));
#217825=CARTESIAN_POINT('Ctrl Pts',(3.07531941599994,11.6,9.94735184399998));
#217826=CARTESIAN_POINT('Ctrl Pts',(3.07482462299994,15.2,9.94624286799999));
#217827=CARTESIAN_POINT('Ctrl Pts',(3.07482462299994,11.6,9.94624286799999));
#217828=CARTESIAN_POINT('Ctrl Pts',(3.07433448899994,15.2,9.94514144399999));
#217829=CARTESIAN_POINT('Ctrl Pts',(3.07433448899994,11.6,9.94514144399999));
#217830=CARTESIAN_POINT('Ctrl Pts',(3.07384900699994,15.2,9.94404759999998));
#217831=CARTESIAN_POINT('Ctrl Pts',(3.07384900699994,11.6,9.94404759999998));
#217832=CARTESIAN_POINT('Ctrl Pts',(3.07336817399994,15.2,9.94296136499998));
#217833=CARTESIAN_POINT('Ctrl Pts',(3.07336817399994,11.6,9.94296136499998));
#217834=CARTESIAN_POINT('Ctrl Pts',(3.07289198199994,15.2,9.94188276499998));
#217835=CARTESIAN_POINT('Ctrl Pts',(3.07289198199994,11.6,9.94188276499998));
#217836=CARTESIAN_POINT('Ctrl Pts',(3.07242042599994,15.2,9.94081182999999));
#217837=CARTESIAN_POINT('Ctrl Pts',(3.07242042599994,11.6,9.94081182999999));
#217838=CARTESIAN_POINT('Ctrl Pts',(3.07195350199994,15.2,9.93974858599999));
#217839=CARTESIAN_POINT('Ctrl Pts',(3.07195350199994,11.6,9.93974858599999));
#217840=CARTESIAN_POINT('Ctrl Pts',(3.07149120299994,15.2,9.93869306299998));
#217841=CARTESIAN_POINT('Ctrl Pts',(3.07149120299994,11.6,9.93869306299998));
#217842=CARTESIAN_POINT('Ctrl Pts',(3.07103352399994,15.2,9.93764528999998));
#217843=CARTESIAN_POINT('Ctrl Pts',(3.07103352399994,11.6,9.93764528999998));
#217844=CARTESIAN_POINT('Ctrl Pts',(3.07058045999994,15.2,9.93660529599998));
#217845=CARTESIAN_POINT('Ctrl Pts',(3.07058045999994,11.6,9.93660529599998));
#217846=CARTESIAN_POINT('Ctrl Pts',(3.07013200399994,15.2,9.93557310899998));
#217847=CARTESIAN_POINT('Ctrl Pts',(3.07013200399994,11.6,9.93557310899998));
#217848=CARTESIAN_POINT('Ctrl Pts',(3.06968815199995,15.2,9.93454875599999));
#217849=CARTESIAN_POINT('Ctrl Pts',(3.06968815199995,11.6,9.93454875599999));
#217850=CARTESIAN_POINT('Ctrl Pts',(3.06924889699994,15.2,9.93353227099998));
#217851=CARTESIAN_POINT('Ctrl Pts',(3.06924889699994,11.6,9.93353227099998));
#217852=CARTESIAN_POINT('Ctrl Pts',(3.06881423399994,15.2,9.93252367899998));
#217853=CARTESIAN_POINT('Ctrl Pts',(3.06881423399994,11.6,9.93252367899998));
#217854=CARTESIAN_POINT('Ctrl Pts',(3.06838415699994,15.2,9.93152301099999));
#217855=CARTESIAN_POINT('Ctrl Pts',(3.06838415699994,11.6,9.93152301099999));
#217856=CARTESIAN_POINT('Ctrl Pts',(3.06795865999994,15.2,9.93053029599999));
#217857=CARTESIAN_POINT('Ctrl Pts',(3.06795865999994,11.6,9.93053029599999));
#217858=CARTESIAN_POINT('Ctrl Pts',(3.06753773799994,15.2,9.92954556499999));
#217859=CARTESIAN_POINT('Ctrl Pts',(3.06753773799994,11.6,9.92954556499999));
#217860=CARTESIAN_POINT('Ctrl Pts',(3.06712138399994,15.2,9.92856884599998));
#217861=CARTESIAN_POINT('Ctrl Pts',(3.06712138399994,11.6,9.92856884599998));
#217862=CARTESIAN_POINT('Ctrl Pts',(3.06670959199994,15.2,9.92760017099998));
#217863=CARTESIAN_POINT('Ctrl Pts',(3.06670959199994,11.6,9.92760017099998));
#217864=CARTESIAN_POINT('Ctrl Pts',(3.06630235599994,15.2,9.92663956799999));
#217865=CARTESIAN_POINT('Ctrl Pts',(3.06630235599994,11.6,9.92663956799999));
#217866=CARTESIAN_POINT('Ctrl Pts',(3.06589967099994,15.2,9.92568706699998));
#217867=CARTESIAN_POINT('Ctrl Pts',(3.06589967099994,11.6,9.92568706699998));
#217868=CARTESIAN_POINT('Ctrl Pts',(3.06550152999994,15.2,9.92474270099999));
#217869=CARTESIAN_POINT('Ctrl Pts',(3.06550152999994,11.6,9.92474270099999));
#217870=CARTESIAN_POINT('Ctrl Pts',(3.06510792699994,15.2,9.92380649899999));
#217871=CARTESIAN_POINT('Ctrl Pts',(3.06510792699994,11.6,9.92380649899999));
#217872=CARTESIAN_POINT('Ctrl Pts',(3.06471885599994,15.2,9.92287849099998));
#217873=CARTESIAN_POINT('Ctrl Pts',(3.06471885599994,11.6,9.92287849099998));
#217874=CARTESIAN_POINT('Ctrl Pts',(3.06433431199994,15.2,9.92195870799998));
#217875=CARTESIAN_POINT('Ctrl Pts',(3.06433431199994,11.6,9.92195870799998));
#217876=CARTESIAN_POINT('Ctrl Pts',(3.06395428599994,15.2,9.92104718299998));
#217877=CARTESIAN_POINT('Ctrl Pts',(3.06395428599994,11.6,9.92104718299998));
#217878=CARTESIAN_POINT('Ctrl Pts',(3.06357877399994,15.2,9.92014394499999));
#217879=CARTESIAN_POINT('Ctrl Pts',(3.06357877399994,11.6,9.92014394499999));
#217880=CARTESIAN_POINT('Ctrl Pts',(3.06320776799994,15.2,9.91924902499999));
#217881=CARTESIAN_POINT('Ctrl Pts',(3.06320776799994,11.6,9.91924902499999));
#217882=CARTESIAN_POINT('Ctrl Pts',(3.06284126399994,15.2,9.91836245599998));
#217883=CARTESIAN_POINT('Ctrl Pts',(3.06284126399994,11.6,9.91836245599998));
#217884=CARTESIAN_POINT('Ctrl Pts',(3.06247925299994,15.2,9.91748426799998));
#217885=CARTESIAN_POINT('Ctrl Pts',(3.06247925299994,11.6,9.91748426799998));
#217886=CARTESIAN_POINT('Ctrl Pts',(3.06212172999994,15.2,9.91661449399999));
#217887=CARTESIAN_POINT('Ctrl Pts',(3.06212172999994,11.6,9.91661449399999));
#217888=CARTESIAN_POINT('Ctrl Pts',(3.06176868699994,15.2,9.91575316599998));
#217889=CARTESIAN_POINT('Ctrl Pts',(3.06176868699994,11.6,9.91575316599998));
#217890=CARTESIAN_POINT('Ctrl Pts',(3.06142212599994,15.2,9.91490522599998));
#217891=CARTESIAN_POINT('Ctrl Pts',(3.06142212599994,11.6,9.91490522599998));
#217892=CARTESIAN_POINT('Ctrl Pts',(3.06114880299994,15.2,9.91423456699999));
#217893=CARTESIAN_POINT('Ctrl Pts',(3.06114880299994,11.6,9.91423456699999));
#217894=CARTESIAN_POINT('Ctrl Pts',(3.06094627499994,15.2,9.91373655899999));
#217895=CARTESIAN_POINT('Ctrl Pts',(3.06094627499994,11.6,9.91373655899999));
#217896=CARTESIAN_POINT('Ctrl Pts',(3.06081277599994,15.2,9.91340782599998));
#217897=CARTESIAN_POINT('Ctrl Pts',(3.06081277599994,11.6,9.91340782599998));
#217898=CARTESIAN_POINT('Ctrl Pts',(3.06074721199994,15.2,9.91324626499999));
#217899=CARTESIAN_POINT('Ctrl Pts',(3.06074721199994,11.6,9.91324626499999));
#217900=CARTESIAN_POINT('',(3.06074721199994,12.2,9.91324626499999));
#217901=CARTESIAN_POINT('',(3.06074721199994,15.2,9.91324626499999));
#217902=CARTESIAN_POINT('',(3.06074721199994,12.2,9.91324626499999));
#217903=CARTESIAN_POINT('Ctrl Pts',(3.76106045499994,12.2,10.867585944));
#217904=CARTESIAN_POINT('Ctrl Pts',(3.76051902299994,12.2,10.867046091));
#217905=CARTESIAN_POINT('Ctrl Pts',(3.75943667399994,12.2,10.865966495));
#217906=CARTESIAN_POINT('Ctrl Pts',(3.75781469799994,12.2,10.864347421));
#217907=CARTESIAN_POINT('Ctrl Pts',(3.75565515599994,12.2,10.862189302));
#217908=CARTESIAN_POINT('Ctrl Pts',(3.75296088399994,12.2,10.85949273));
#217909=CARTESIAN_POINT('Ctrl Pts',(3.75027176799994,12.2,10.856797236));
#217910=CARTESIAN_POINT('Ctrl Pts',(3.74758780799994,12.2,10.854102822));
#217911=CARTESIAN_POINT('Ctrl Pts',(3.74490900499994,12.2,10.85140949));
#217912=CARTESIAN_POINT('Ctrl Pts',(3.74223535999994,12.2,10.84871725));
#217913=CARTESIAN_POINT('Ctrl Pts',(3.73956687399994,12.2,10.846026106));
#217914=CARTESIAN_POINT('Ctrl Pts',(3.73690354699994,12.2,10.843336071));
#217915=CARTESIAN_POINT('Ctrl Pts',(3.73424538199994,12.2,10.840647153));
#217916=CARTESIAN_POINT('Ctrl Pts',(3.73159237799995,12.2,10.837959365));
#217917=CARTESIAN_POINT('Ctrl Pts',(3.72894453699994,12.2,10.835272717));
#217918=CARTESIAN_POINT('Ctrl Pts',(3.72630186199994,12.2,10.832587221));
#217919=CARTESIAN_POINT('Ctrl Pts',(3.72366435199994,12.2,10.829902884));
#217920=CARTESIAN_POINT('Ctrl Pts',(3.72103200699994,12.2,10.827219716));
#217921=CARTESIAN_POINT('Ctrl Pts',(3.71840482999994,12.2,10.824537725));
#217922=CARTESIAN_POINT('Ctrl Pts',(3.71578282099994,12.2,10.821856919));
#217923=CARTESIAN_POINT('Ctrl Pts',(3.71316598199994,12.2,10.819177306));
#217924=CARTESIAN_POINT('Ctrl Pts',(3.71055431199994,12.2,10.816498895));
#217925=CARTESIAN_POINT('Ctrl Pts',(3.70794781299994,12.2,10.813821695));
#217926=CARTESIAN_POINT('Ctrl Pts',(3.70534648499994,12.2,10.811145713));
#217927=CARTESIAN_POINT('Ctrl Pts',(3.70275033099994,12.2,10.808470961));
#217928=CARTESIAN_POINT('Ctrl Pts',(3.70015935099994,12.2,10.805797449));
#217929=CARTESIAN_POINT('Ctrl Pts',(3.69757354499994,12.2,10.803125184));
#217930=CARTESIAN_POINT('Ctrl Pts',(3.69499291499995,12.2,10.800454179));
#217931=CARTESIAN_POINT('Ctrl Pts',(3.69241746099994,12.2,10.797784438));
#217932=CARTESIAN_POINT('Ctrl Pts',(3.68984718499994,12.2,10.795115974));
#217933=CARTESIAN_POINT('Ctrl Pts',(3.68728208699994,12.2,10.792448794));
#217934=CARTESIAN_POINT('Ctrl Pts',(3.68472216799994,12.2,10.789782909));
#217935=CARTESIAN_POINT('Ctrl Pts',(3.68216742899994,12.2,10.787118327));
#217936=CARTESIAN_POINT('Ctrl Pts',(3.67961787099994,12.2,10.784455057));
#217937=CARTESIAN_POINT('Ctrl Pts',(3.67707349599994,12.2,10.781793108));
#217938=CARTESIAN_POINT('Ctrl Pts',(3.67453430199994,12.2,10.77913249));
#217939=CARTESIAN_POINT('Ctrl Pts',(3.67200029299994,12.2,10.776473211));
#217940=CARTESIAN_POINT('Ctrl Pts',(3.66947146699994,12.2,10.773815282));
#217941=CARTESIAN_POINT('Ctrl Pts',(3.66694782699994,12.2,10.771158713));
#217942=CARTESIAN_POINT('Ctrl Pts',(3.66442937399994,12.2,10.768503511));
#217943=CARTESIAN_POINT('Ctrl Pts',(3.66191610699994,12.2,10.765849687));
#217944=CARTESIAN_POINT('Ctrl Pts',(3.65940802899994,12.2,10.76319725));
#217945=CARTESIAN_POINT('Ctrl Pts',(3.65690513699994,12.2,10.760546208));
#217946=CARTESIAN_POINT('Ctrl Pts',(3.65440743699994,12.2,10.757896573));
#217947=CARTESIAN_POINT('Ctrl Pts',(3.65191492599994,12.2,10.755248353));
#217948=CARTESIAN_POINT('Ctrl Pts',(3.64942760599994,12.2,10.752601556));
#217949=CARTESIAN_POINT('Ctrl Pts',(3.64694547899994,12.2,10.749956194));
#217950=CARTESIAN_POINT('Ctrl Pts',(3.64446854399994,12.2,10.747312275));
#217951=CARTESIAN_POINT('Ctrl Pts',(3.64199680199994,12.2,10.744669808));
#217952=CARTESIAN_POINT('Ctrl Pts',(3.63953025499994,12.2,10.742028805));
#217953=CARTESIAN_POINT('Ctrl Pts',(3.63706890199994,12.2,10.739389272));
#217954=CARTESIAN_POINT('Ctrl Pts',(3.63461274499994,12.2,10.736751222));
#217955=CARTESIAN_POINT('Ctrl Pts',(3.63216178499994,12.2,10.734114662));
#217956=CARTESIAN_POINT('Ctrl Pts',(3.62971602199994,12.2,10.731479602));
#217957=CARTESIAN_POINT('Ctrl Pts',(3.62727545699994,12.2,10.728846054));
#217958=CARTESIAN_POINT('Ctrl Pts',(3.62484009099994,12.2,10.726214025));
#217959=CARTESIAN_POINT('Ctrl Pts',(3.62240992399994,12.2,10.723583524));
#217960=CARTESIAN_POINT('Ctrl Pts',(3.61998495799994,12.2,10.720954563));
#217961=CARTESIAN_POINT('Ctrl Pts',(3.61756519199994,12.2,10.718327151));
#217962=CARTESIAN_POINT('Ctrl Pts',(3.61515062899994,12.2,10.715701296));
#217963=CARTESIAN_POINT('Ctrl Pts',(3.61274126699994,12.2,10.71307701));
#217964=CARTESIAN_POINT('Ctrl Pts',(3.61033710899994,12.2,10.710454302));
#217965=CARTESIAN_POINT('Ctrl Pts',(3.60793815399994,12.2,10.707833181));
#217966=CARTESIAN_POINT('Ctrl Pts',(3.60554440399994,12.2,10.705213657));
#217967=CARTESIAN_POINT('Ctrl Pts',(3.60315585899994,12.2,10.702595741));
#217968=CARTESIAN_POINT('Ctrl Pts',(3.60077251999994,12.2,10.699979441));
#217969=CARTESIAN_POINT('Ctrl Pts',(3.59839438799994,12.2,10.697364767));
#217970=CARTESIAN_POINT('Ctrl Pts',(3.59602146199994,12.2,10.694751731));
#217971=CARTESIAN_POINT('Ctrl Pts',(3.59365374499994,12.2,10.692140339));
#217972=CARTESIAN_POINT('Ctrl Pts',(3.59129123599994,12.2,10.689530605));
#217973=CARTESIAN_POINT('Ctrl Pts',(3.58893393499994,12.2,10.686922536));
#217974=CARTESIAN_POINT('Ctrl Pts',(3.58658184499994,12.2,10.684316143));
#217975=CARTESIAN_POINT('Ctrl Pts',(3.58423496399995,12.2,10.681711437));
#217976=CARTESIAN_POINT('Ctrl Pts',(3.58189329599994,12.2,10.679108425));
#217977=CARTESIAN_POINT('Ctrl Pts',(3.57955683799994,12.2,10.67650712));
#217978=CARTESIAN_POINT('Ctrl Pts',(3.57722559299994,12.2,10.673907531));
#217979=CARTESIAN_POINT('Ctrl Pts',(3.57489956099994,12.2,10.671309666));
#217980=CARTESIAN_POINT('Ctrl Pts',(3.57257874199994,12.2,10.668713538));
#217981=CARTESIAN_POINT('Ctrl Pts',(3.57026313699994,12.2,10.666119155));
#217982=CARTESIAN_POINT('Ctrl Pts',(3.56795274699994,12.2,10.663526528));
#217983=CARTESIAN_POINT('Ctrl Pts',(3.56564757099994,12.2,10.660935667));
#217984=CARTESIAN_POINT('Ctrl Pts',(3.56334761099994,12.2,10.658346581));
#217985=CARTESIAN_POINT('Ctrl Pts',(3.56105286799994,12.2,10.655759282));
#217986=CARTESIAN_POINT('Ctrl Pts',(3.55876334099994,12.2,10.653173779));
#217987=CARTESIAN_POINT('Ctrl Pts',(3.55647903199994,12.2,10.650590083));
#217988=CARTESIAN_POINT('Ctrl Pts',(3.55419994099994,12.2,10.648008202));
#217989=CARTESIAN_POINT('Ctrl Pts',(3.55192606799994,12.2,10.645428149));
#217990=CARTESIAN_POINT('Ctrl Pts',(3.54965741499994,12.2,10.642849932));
#217991=CARTESIAN_POINT('Ctrl Pts',(3.54739397999994,12.2,10.640273563));
#217992=CARTESIAN_POINT('Ctrl Pts',(3.54513576499994,12.2,10.637699051));
#217993=CARTESIAN_POINT('Ctrl Pts',(3.54288277099994,12.2,10.635126406));
#217994=CARTESIAN_POINT('Ctrl Pts',(3.54063499799994,12.2,10.632555639));
#217995=CARTESIAN_POINT('Ctrl Pts',(3.53839244699994,12.2,10.62998676));
#217996=CARTESIAN_POINT('Ctrl Pts',(3.53615511699994,12.2,10.62741978));
#217997=CARTESIAN_POINT('Ctrl Pts',(3.53392300999994,12.2,10.624854709));
#217998=CARTESIAN_POINT('Ctrl Pts',(3.53169612599994,12.2,10.622291557));
#217999=CARTESIAN_POINT('Ctrl Pts',(3.52947446499994,12.2,10.619730334));
#218000=CARTESIAN_POINT('Ctrl Pts',(3.52725802799994,12.2,10.617171051));
#218001=CARTESIAN_POINT('Ctrl Pts',(3.52504681399994,12.2,10.61461372));
#218002=CARTESIAN_POINT('Ctrl Pts',(3.52284082599994,12.2,10.612058349));
#218003=CARTESIAN_POINT('Ctrl Pts',(3.52064006199994,12.2,10.609504948));
#218004=CARTESIAN_POINT('Ctrl Pts',(3.51844452399994,12.2,10.606953531));
#218005=CARTESIAN_POINT('Ctrl Pts',(3.51625421199994,12.2,10.604404106));
#218006=CARTESIAN_POINT('Ctrl Pts',(3.51406912699994,12.2,10.601856683));
#218007=CARTESIAN_POINT('Ctrl Pts',(3.51188926799994,12.2,10.599311274));
#218008=CARTESIAN_POINT('Ctrl Pts',(3.50971463599994,12.2,10.596767889));
#218009=CARTESIAN_POINT('Ctrl Pts',(3.50754523199994,12.2,10.594226538));
#218010=CARTESIAN_POINT('Ctrl Pts',(3.50538105499994,12.2,10.591687233));
#218011=CARTESIAN_POINT('Ctrl Pts',(3.50322210699994,12.2,10.589149983));
#218012=CARTESIAN_POINT('Ctrl Pts',(3.50106838699995,12.2,10.5866148));
#218013=CARTESIAN_POINT('Ctrl Pts',(3.49891989599994,12.2,10.584081694));
#218014=CARTESIAN_POINT('Ctrl Pts',(3.49677663399994,12.2,10.581550676));
#218015=CARTESIAN_POINT('Ctrl Pts',(3.49463860199994,12.2,10.579021758));
#218016=CARTESIAN_POINT('Ctrl Pts',(3.49250580099994,12.2,10.576494948));
#218017=CARTESIAN_POINT('Ctrl Pts',(3.49037822899994,12.2,10.573970259));
#218018=CARTESIAN_POINT('Ctrl Pts',(3.48825588699994,12.2,10.571447699));
#218019=CARTESIAN_POINT('Ctrl Pts',(3.48613877699994,12.2,10.568927282));
#218020=CARTESIAN_POINT('Ctrl Pts',(3.48402689799994,12.2,10.566409018));
#218021=CARTESIAN_POINT('Ctrl Pts',(3.48192024899994,12.2,10.563892917));
#218022=CARTESIAN_POINT('Ctrl Pts',(3.47981883399994,12.2,10.561378991));
#218023=CARTESIAN_POINT('Ctrl Pts',(3.47772264999994,12.2,10.558867249));
#218024=CARTESIAN_POINT('Ctrl Pts',(3.47563169699994,12.2,10.556357703));
#218025=CARTESIAN_POINT('Ctrl Pts',(3.47354597799994,12.2,10.553850365));
#218026=CARTESIAN_POINT('Ctrl Pts',(3.47146549099994,12.2,10.551345244));
#218027=CARTESIAN_POINT('Ctrl Pts',(3.46939023699994,12.2,10.548842353));
#218028=CARTESIAN_POINT('Ctrl Pts',(3.46732021699995,12.2,10.546341702));
#218029=CARTESIAN_POINT('Ctrl Pts',(3.46525542999994,12.2,10.543843302));
#218030=CARTESIAN_POINT('Ctrl Pts',(3.46319587599994,12.2,10.541347163));
#218031=CARTESIAN_POINT('Ctrl Pts',(3.46114155699994,12.2,10.538853298));
#218032=CARTESIAN_POINT('Ctrl Pts',(3.45909247099994,12.2,10.536361718));
#218033=CARTESIAN_POINT('Ctrl Pts',(3.45704861999995,12.2,10.533872432));
#218034=CARTESIAN_POINT('Ctrl Pts',(3.45501000299994,12.2,10.531385453));
#218035=CARTESIAN_POINT('Ctrl Pts',(3.45297662099994,12.2,10.528900792));
#218036=CARTESIAN_POINT('Ctrl Pts',(3.45094847299994,12.2,10.526418461));
#218037=CARTESIAN_POINT('Ctrl Pts',(3.44892555999994,12.2,10.523938468));
#218038=CARTESIAN_POINT('Ctrl Pts',(3.44690788299994,12.2,10.521460827));
#218039=CARTESIAN_POINT('Ctrl Pts',(3.44489543999994,12.2,10.51898555));
#218040=CARTESIAN_POINT('Ctrl Pts',(3.44288823299994,12.2,10.516512645));
#218041=CARTESIAN_POINT('Ctrl Pts',(3.44088626199994,12.2,10.514042126));
#218042=CARTESIAN_POINT('Ctrl Pts',(3.43888952499994,12.2,10.511574004));
#218043=CARTESIAN_POINT('Ctrl Pts',(3.43689802499994,12.2,10.50910829));
#218044=CARTESIAN_POINT('Ctrl Pts',(3.43491175999994,12.2,10.506644995));
#218045=CARTESIAN_POINT('Ctrl Pts',(3.43293072999994,12.2,10.504184131));
#218046=CARTESIAN_POINT('Ctrl Pts',(3.43095493699995,12.2,10.501725709));
#218047=CARTESIAN_POINT('Ctrl Pts',(3.42898437999994,12.2,10.49926974));
#218048=CARTESIAN_POINT('Ctrl Pts',(3.42701905899994,12.2,10.496816237));
#218049=CARTESIAN_POINT('Ctrl Pts',(3.42505897399994,12.2,10.49436521));
#218050=CARTESIAN_POINT('Ctrl Pts',(3.42310412599995,12.2,10.491916672));
#218051=CARTESIAN_POINT('Ctrl Pts',(3.42115451199994,12.2,10.489470632));
#218052=CARTESIAN_POINT('Ctrl Pts',(3.41921013599995,12.2,10.487027105));
#218053=CARTESIAN_POINT('Ctrl Pts',(3.41727099499994,12.2,10.4845861));
#218054=CARTESIAN_POINT('Ctrl Pts',(3.41533709199994,12.2,10.482147629));
#218055=CARTESIAN_POINT('Ctrl Pts',(3.41340842399994,12.2,10.479711706));
#218056=CARTESIAN_POINT('Ctrl Pts',(3.41148499199994,12.2,10.477278339));
#218057=CARTESIAN_POINT('Ctrl Pts',(3.40956679599994,12.2,10.474847543));
#218058=CARTESIAN_POINT('Ctrl Pts',(3.40765383599994,12.2,10.472419326));
#218059=CARTESIAN_POINT('Ctrl Pts',(3.40574611299994,12.2,10.469993704));
#218060=CARTESIAN_POINT('Ctrl Pts',(3.40384362599994,12.2,10.467570687));
#218061=CARTESIAN_POINT('Ctrl Pts',(3.40194637399994,12.2,10.465150286));
#218062=CARTESIAN_POINT('Ctrl Pts',(3.40005435899994,12.2,10.462732513));
#218063=CARTESIAN_POINT('Ctrl Pts',(3.39816757899994,12.2,10.460317381));
#218064=CARTESIAN_POINT('Ctrl Pts',(3.39628603499994,12.2,10.4579049));
#218065=CARTESIAN_POINT('Ctrl Pts',(3.39440972599995,12.2,10.455495084));
#218066=CARTESIAN_POINT('Ctrl Pts',(3.39253865299994,12.2,10.453087944));
#218067=CARTESIAN_POINT('Ctrl Pts',(3.39067281599994,12.2,10.450683492));
#218068=CARTESIAN_POINT('Ctrl Pts',(3.38881221399994,12.2,10.448281741));
#218069=CARTESIAN_POINT('Ctrl Pts',(3.38695684699994,12.2,10.445882701));
#218070=CARTESIAN_POINT('Ctrl Pts',(3.38510671499994,12.2,10.443486385));
#218071=CARTESIAN_POINT('Ctrl Pts',(3.38326181899995,12.2,10.441092806));
#218072=CARTESIAN_POINT('Ctrl Pts',(3.38142215599994,12.2,10.438701973));
#218073=CARTESIAN_POINT('Ctrl Pts',(3.37958772799994,12.2,10.436313903));
#218074=CARTESIAN_POINT('Ctrl Pts',(3.37775853499994,12.2,10.433928604));
#218075=CARTESIAN_POINT('Ctrl Pts',(3.37593457599994,12.2,10.43154609));
#218076=CARTESIAN_POINT('Ctrl Pts',(3.37411584999994,12.2,10.429166374));
#218077=CARTESIAN_POINT('Ctrl Pts',(3.37230235899994,12.2,10.426789465));
#218078=CARTESIAN_POINT('Ctrl Pts',(3.37049410099994,12.2,10.424415378));
#218079=CARTESIAN_POINT('Ctrl Pts',(3.36869107699994,12.2,10.422044126));
#218080=CARTESIAN_POINT('Ctrl Pts',(3.36689328399994,12.2,10.419675719));
#218081=CARTESIAN_POINT('Ctrl Pts',(3.36510072599994,12.2,10.417310171));
#218082=CARTESIAN_POINT('Ctrl Pts',(3.36331339899994,12.2,10.414947493));
#218083=CARTESIAN_POINT('Ctrl Pts',(3.36153130499994,12.2,10.412587698));
#218084=CARTESIAN_POINT('Ctrl Pts',(3.35975444299994,12.2,10.410230799));
#218085=CARTESIAN_POINT('Ctrl Pts',(3.35798281299994,12.2,10.407876808));
#218086=CARTESIAN_POINT('Ctrl Pts',(3.35621641399994,12.2,10.405525737));
#218087=CARTESIAN_POINT('Ctrl Pts',(3.35445524599994,12.2,10.4031776));
#218088=CARTESIAN_POINT('Ctrl Pts',(3.35269930899994,12.2,10.400832408));
#218089=CARTESIAN_POINT('Ctrl Pts',(3.35094860199994,12.2,10.398490174));
#218090=CARTESIAN_POINT('Ctrl Pts',(3.34920312499994,12.2,10.396150911));
#218091=CARTESIAN_POINT('Ctrl Pts',(3.34746287999995,12.2,10.393814631));
#218092=CARTESIAN_POINT('Ctrl Pts',(3.34572786099995,12.2,10.391481347));
#218093=CARTESIAN_POINT('Ctrl Pts',(3.34399807299994,12.2,10.389151072));
#218094=CARTESIAN_POINT('Ctrl Pts',(3.34227351299994,12.2,10.386823818));
#218095=CARTESIAN_POINT('Ctrl Pts',(3.34055418199994,12.2,10.384499599));
#218096=CARTESIAN_POINT('Ctrl Pts',(3.33884007799994,12.2,10.382178427));
#218097=CARTESIAN_POINT('Ctrl Pts',(3.33713120199994,12.2,10.379860313));
#218098=CARTESIAN_POINT('Ctrl Pts',(3.33542755199994,12.2,10.377545274));
#218099=CARTESIAN_POINT('Ctrl Pts',(3.33372912899994,12.2,10.375233319));
#218100=CARTESIAN_POINT('Ctrl Pts',(3.33203593199995,12.2,10.372924463));
#218101=CARTESIAN_POINT('Ctrl Pts',(3.33034796099994,12.2,10.370618718));
#218102=CARTESIAN_POINT('Ctrl Pts',(3.32866521499994,12.2,10.368316097));
#218103=CARTESIAN_POINT('Ctrl Pts',(3.32698769299994,12.2,10.366016614));
#218104=CARTESIAN_POINT('Ctrl Pts',(3.32531539599994,12.2,10.36372028));
#218105=CARTESIAN_POINT('Ctrl Pts',(3.32364832199994,12.2,10.36142711));
#218106=CARTESIAN_POINT('Ctrl Pts',(3.32198647199994,12.2,10.359137117));
#218107=CARTESIAN_POINT('Ctrl Pts',(3.32032984499994,12.2,10.356850313));
#218108=CARTESIAN_POINT('Ctrl Pts',(3.31867843899994,12.2,10.354566712));
#218109=CARTESIAN_POINT('Ctrl Pts',(3.31703225499994,12.2,10.352286327));
#218110=CARTESIAN_POINT('Ctrl Pts',(3.31506309947149,12.2,10.3495537386993));
#218111=CARTESIAN_POINT('Ctrl Pts',(3.31310177376417,12.2,10.3468260146503));
#218112=CARTESIAN_POINT('Ctrl Pts',(3.31114827823572,12.2,10.3441031813496));
#218113=CARTESIAN_POINT('Ctrl Pts',(3.30920261270513,12.2,10.3413852645476));
#218114=CARTESIAN_POINT('Ctrl Pts',(3.30726477099994,12.2,10.33867229));
#218115=CARTESIAN_POINT('Ctrl Pts',(3.30565512199994,12.2,10.336414786));
#218116=CARTESIAN_POINT('Ctrl Pts',(3.30405068899994,12.2,10.334160606));
#218117=CARTESIAN_POINT('Ctrl Pts',(3.30245147199994,12.2,10.331909762));
#218118=CARTESIAN_POINT('Ctrl Pts',(3.30085747199994,12.2,10.329662268));
#218119=CARTESIAN_POINT('Ctrl Pts',(3.29926868599994,12.2,10.327418135));
#218120=CARTESIAN_POINT('Ctrl Pts',(3.29768511299994,12.2,10.325177379));
#218121=CARTESIAN_POINT('Ctrl Pts',(3.29610675499994,12.2,10.322940014));
#218122=CARTESIAN_POINT('Ctrl Pts',(3.29453360899994,12.2,10.320706052));
#218123=CARTESIAN_POINT('Ctrl Pts',(3.29296567499994,12.2,10.318475509));
#218124=CARTESIAN_POINT('Ctrl Pts',(3.29140295199994,12.2,10.316248395));
#218125=CARTESIAN_POINT('Ctrl Pts',(3.28984543999994,12.2,10.314024727));
#218126=CARTESIAN_POINT('Ctrl Pts',(3.28829313699994,12.2,10.311804518));
#218127=CARTESIAN_POINT('Ctrl Pts',(3.28674604399994,12.2,10.30958778));
#218128=CARTESIAN_POINT('Ctrl Pts',(3.28520415899995,12.2,10.307374529));
#218129=CARTESIAN_POINT('Ctrl Pts',(3.28366748099994,12.2,10.305164779));
#218130=CARTESIAN_POINT('Ctrl Pts',(3.28213600999995,12.2,10.302958542));
#218131=CARTESIAN_POINT('Ctrl Pts',(3.28060974399994,12.2,10.300755834));
#218132=CARTESIAN_POINT('Ctrl Pts',(3.27908868399994,12.2,10.298556666));
#218133=CARTESIAN_POINT('Ctrl Pts',(3.27757282699995,12.2,10.296361056));
#218134=CARTESIAN_POINT('Ctrl Pts',(3.27606217499994,12.2,10.294169016));
#218135=CARTESIAN_POINT('Ctrl Pts',(3.27455672399994,12.2,10.291980559));
#218136=CARTESIAN_POINT('Ctrl Pts',(3.27305647499994,12.2,10.2897957));
#218137=CARTESIAN_POINT('Ctrl Pts',(3.27156142599994,12.2,10.287614454));
#218138=CARTESIAN_POINT('Ctrl Pts',(3.27007157799994,12.2,10.285436836));
#218139=CARTESIAN_POINT('Ctrl Pts',(3.26858692799994,12.2,10.283262858));
#218140=CARTESIAN_POINT('Ctrl Pts',(3.26710747499994,12.2,10.281092534));
#218141=CARTESIAN_POINT('Ctrl Pts',(3.26563321999994,12.2,10.27892588));
#218142=CARTESIAN_POINT('Ctrl Pts',(3.26416416099994,12.2,10.276762911));
#218143=CARTESIAN_POINT('Ctrl Pts',(3.26270029699995,12.2,10.274603639));
#218144=CARTESIAN_POINT('Ctrl Pts',(3.26124162699994,12.2,10.272448079));
#218145=CARTESIAN_POINT('Ctrl Pts',(3.25978815099994,12.2,10.270296246));
#218146=CARTESIAN_POINT('Ctrl Pts',(3.25833986599994,12.2,10.268148156));
#218147=CARTESIAN_POINT('Ctrl Pts',(3.25689677199994,12.2,10.266003821));
#218148=CARTESIAN_POINT('Ctrl Pts',(3.25545886799994,12.2,10.263863257));
#218149=CARTESIAN_POINT('Ctrl Pts',(3.25402615299994,12.2,10.261726478));
#218150=CARTESIAN_POINT('Ctrl Pts',(3.25259862599995,12.2,10.259593498));
#218151=CARTESIAN_POINT('Ctrl Pts',(3.25117628599994,12.2,10.257464334));
#218152=CARTESIAN_POINT('Ctrl Pts',(3.24975913199995,12.2,10.255338999));
#218153=CARTESIAN_POINT('Ctrl Pts',(3.24834716199994,12.2,10.253217507));
#218154=CARTESIAN_POINT('Ctrl Pts',(3.24694037599994,12.2,10.251099875));
#218155=CARTESIAN_POINT('Ctrl Pts',(3.24553877199994,12.2,10.248986116));
#218156=CARTESIAN_POINT('Ctrl Pts',(3.24414234999994,12.2,10.246876245));
#218157=CARTESIAN_POINT('Ctrl Pts',(3.24275110699995,12.2,10.244770278));
#218158=CARTESIAN_POINT('Ctrl Pts',(3.24136504399994,12.2,10.242668229));
#218159=CARTESIAN_POINT('Ctrl Pts',(3.23998415799994,12.2,10.240570115));
#218160=CARTESIAN_POINT('Ctrl Pts',(3.23860844899994,12.2,10.238475948));
#218161=CARTESIAN_POINT('Ctrl Pts',(3.23723791499994,12.2,10.236385745));
#218162=CARTESIAN_POINT('Ctrl Pts',(3.23587255499994,12.2,10.23429952));
#218163=CARTESIAN_POINT('Ctrl Pts',(3.23451236799994,12.2,10.232217288));
#218164=CARTESIAN_POINT('Ctrl Pts',(3.23315735299994,12.2,10.230139067));
#218165=CARTESIAN_POINT('Ctrl Pts',(3.23180750799994,12.2,10.228064869));
#218166=CARTESIAN_POINT('Ctrl Pts',(3.23046283199994,12.2,10.225994711));
#218167=CARTESIAN_POINT('Ctrl Pts',(3.22912332499994,12.2,10.223928608));
#218168=CARTESIAN_POINT('Ctrl Pts',(3.22778898299994,12.2,10.221866575));
#218169=CARTESIAN_POINT('Ctrl Pts',(3.22645980699994,12.2,10.219808628));
#218170=CARTESIAN_POINT('Ctrl Pts',(3.22513579399994,12.2,10.217754781));
#218171=CARTESIAN_POINT('Ctrl Pts',(3.22381694499994,12.2,10.215705052));
#218172=CARTESIAN_POINT('Ctrl Pts',(3.22250325599994,12.2,10.213659454));
#218173=CARTESIAN_POINT('Ctrl Pts',(3.22119472699995,12.2,10.211618004));
#218174=CARTESIAN_POINT('Ctrl Pts',(3.21989135599994,12.2,10.209580717));
#218175=CARTESIAN_POINT('Ctrl Pts',(3.21859314299994,12.2,10.20754761));
#218176=CARTESIAN_POINT('Ctrl Pts',(3.21730008399994,12.2,10.205518696));
#218177=CARTESIAN_POINT('Ctrl Pts',(3.21601217999994,12.2,10.203493994));
#218178=CARTESIAN_POINT('Ctrl Pts',(3.21472942799994,12.2,10.201473517));
#218179=CARTESIAN_POINT('Ctrl Pts',(3.21345182799994,12.2,10.199457283));
#218180=CARTESIAN_POINT('Ctrl Pts',(3.21217937699994,12.2,10.197445307));
#218181=CARTESIAN_POINT('Ctrl Pts',(3.21091207399995,12.2,10.195437604));
#218182=CARTESIAN_POINT('Ctrl Pts',(3.20964991799995,12.2,10.193434192));
#218183=CARTESIAN_POINT('Ctrl Pts',(3.20839290699994,12.2,10.191435086));
#218184=CARTESIAN_POINT('Ctrl Pts',(3.20714103999994,12.2,10.189440301));
#218185=CARTESIAN_POINT('Ctrl Pts',(3.20589431499994,12.2,10.187449854));
#218186=CARTESIAN_POINT('Ctrl Pts',(3.20465272999995,12.2,10.185463762));
#218187=CARTESIAN_POINT('Ctrl Pts',(3.20341628299994,12.2,10.183482041));
#218188=CARTESIAN_POINT('Ctrl Pts',(3.20218497399994,12.2,10.181504705));
#218189=CARTESIAN_POINT('Ctrl Pts',(3.20095880099994,12.2,10.179531773));
#218190=CARTESIAN_POINT('Ctrl Pts',(3.19973776199994,12.2,10.17756326));
#218191=CARTESIAN_POINT('Ctrl Pts',(3.19852185399994,12.2,10.175599184));
#218192=CARTESIAN_POINT('Ctrl Pts',(3.19731107699994,12.2,10.173639559));
#218193=CARTESIAN_POINT('Ctrl Pts',(3.19610542999994,12.2,10.171684403));
#218194=CARTESIAN_POINT('Ctrl Pts',(3.19490490899994,12.2,10.169733732));
#218195=CARTESIAN_POINT('Ctrl Pts',(3.19370951399994,12.2,10.167787564));
#218196=CARTESIAN_POINT('Ctrl Pts',(3.19251924199994,12.2,10.165845913));
#218197=CARTESIAN_POINT('Ctrl Pts',(3.19133409399994,12.2,10.163908798));
#218198=CARTESIAN_POINT('Ctrl Pts',(3.19015406399994,12.2,10.161976234));
#218199=CARTESIAN_POINT('Ctrl Pts',(3.18897915299994,12.2,10.160048239));
#218200=CARTESIAN_POINT('Ctrl Pts',(3.18780935899994,12.2,10.158124831));
#218201=CARTESIAN_POINT('Ctrl Pts',(3.18664467899994,12.2,10.156206023));
#218202=CARTESIAN_POINT('Ctrl Pts',(3.18548511399994,12.2,10.154291836));
#218203=CARTESIAN_POINT('Ctrl Pts',(3.18433065699995,12.2,10.152382285));
#218204=CARTESIAN_POINT('Ctrl Pts',(3.18318131199995,12.2,10.150477387));
#218205=CARTESIAN_POINT('Ctrl Pts',(3.18203707299994,12.2,10.148577159));
#218206=CARTESIAN_POINT('Ctrl Pts',(3.18089793999994,12.2,10.146681619));
#218207=CARTESIAN_POINT('Ctrl Pts',(3.17976390999994,12.2,10.144790784));
#218208=CARTESIAN_POINT('Ctrl Pts',(3.17863498099995,12.2,10.142904671));
#218209=CARTESIAN_POINT('Ctrl Pts',(3.17751115299994,12.2,10.141023297));
#218210=CARTESIAN_POINT('Ctrl Pts',(3.17639242199995,12.2,10.13914668));
#218211=CARTESIAN_POINT('Ctrl Pts',(3.17527878599994,12.2,10.137274836));
#218212=CARTESIAN_POINT('Ctrl Pts',(3.17417024399994,12.2,10.135407784));
#218213=CARTESIAN_POINT('Ctrl Pts',(3.17306679399994,12.2,10.133545542));
#218214=CARTESIAN_POINT('Ctrl Pts',(3.17196843199994,12.2,10.131688125));
#218215=CARTESIAN_POINT('Ctrl Pts',(3.17087515899994,12.2,10.129835553));
#218216=CARTESIAN_POINT('Ctrl Pts',(3.16978697099994,12.2,10.127987842));
#218217=CARTESIAN_POINT('Ctrl Pts',(3.16870386699994,12.2,10.126145011));
#218218=CARTESIAN_POINT('Ctrl Pts',(3.16762584299994,12.2,10.124307078));
#218219=CARTESIAN_POINT('Ctrl Pts',(3.16655289799994,12.2,10.12247406));
#218220=CARTESIAN_POINT('Ctrl Pts',(3.16548502999995,12.2,10.120645975));
#218221=CARTESIAN_POINT('Ctrl Pts',(3.16442223699994,12.2,10.11882284));
#218222=CARTESIAN_POINT('Ctrl Pts',(3.16336451599994,12.2,10.117004675));
#218223=CARTESIAN_POINT('Ctrl Pts',(3.16231186499994,12.2,10.115191496));
#218224=CARTESIAN_POINT('Ctrl Pts',(3.16126428299994,12.2,10.113383323));
#218225=CARTESIAN_POINT('Ctrl Pts',(3.16022176599994,12.2,10.111580173));
#218226=CARTESIAN_POINT('Ctrl Pts',(3.15918431399994,12.2,10.109782065));
#218227=CARTESIAN_POINT('Ctrl Pts',(3.15815192199994,12.2,10.107989016));
#218228=CARTESIAN_POINT('Ctrl Pts',(3.15712458699994,12.2,10.106201046));
#218229=CARTESIAN_POINT('Ctrl Pts',(3.15610231199994,12.2,10.104418172));
#218230=CARTESIAN_POINT('Ctrl Pts',(3.15508508899994,12.2,10.102640413));
#218231=CARTESIAN_POINT('Ctrl Pts',(3.15407291799994,12.2,10.100867788));
#218232=CARTESIAN_POINT('Ctrl Pts',(3.15306579799994,12.2,10.099100315));
#218233=CARTESIAN_POINT('Ctrl Pts',(3.15206372299994,12.2,10.097338013));
#218234=CARTESIAN_POINT('Ctrl Pts',(3.15106669299994,12.2,10.0955809));
#218235=CARTESIAN_POINT('Ctrl Pts',(3.15007470599994,12.2,10.093828996));
#218236=CARTESIAN_POINT('Ctrl Pts',(3.14908775899994,12.2,10.092082318));
#218237=CARTESIAN_POINT('Ctrl Pts',(3.14810584799994,12.2,10.090340886));
#218238=CARTESIAN_POINT('Ctrl Pts',(3.14712897199994,12.2,10.08860472));
#218239=CARTESIAN_POINT('Ctrl Pts',(3.14615712899994,12.2,10.086873837));
#218240=CARTESIAN_POINT('Ctrl Pts',(3.14519031499994,12.2,10.085148257));
#218241=CARTESIAN_POINT('Ctrl Pts',(3.14422852799995,12.2,10.083427999));
#218242=CARTESIAN_POINT('Ctrl Pts',(3.14327176599994,12.2,10.081713083));
#218243=CARTESIAN_POINT('Ctrl Pts',(3.14232002399994,12.2,10.080003527));
#218244=CARTESIAN_POINT('Ctrl Pts',(3.14137330399994,12.2,10.078299351));
#218245=CARTESIAN_POINT('Ctrl Pts',(3.14043159899994,12.2,10.076600574));
#218246=CARTESIAN_POINT('Ctrl Pts',(3.13949490699994,12.2,10.074907216));
#218247=CARTESIAN_POINT('Ctrl Pts',(3.13856322699994,12.2,10.073219296));
#218248=CARTESIAN_POINT('Ctrl Pts',(3.13763655599994,12.2,10.071536834));
#218249=CARTESIAN_POINT('Ctrl Pts',(3.13671488999994,12.2,10.069859849));
#218250=CARTESIAN_POINT('Ctrl Pts',(3.13579822699994,12.2,10.068188362));
#218251=CARTESIAN_POINT('Ctrl Pts',(3.13488656499994,12.2,10.066522392));
#218252=CARTESIAN_POINT('Ctrl Pts',(3.13397989999994,12.2,10.064861958));
#218253=CARTESIAN_POINT('Ctrl Pts',(3.13307822999994,12.2,10.063207081));
#218254=CARTESIAN_POINT('Ctrl Pts',(3.13218154999995,12.2,10.061557781));
#218255=CARTESIAN_POINT('Ctrl Pts',(3.13128985999994,12.2,10.059914077));
#218256=CARTESIAN_POINT('Ctrl Pts',(3.13040315599994,12.2,10.058275991));
#218257=CARTESIAN_POINT('Ctrl Pts',(3.12952143499994,12.2,10.056643542));
#218258=CARTESIAN_POINT('Ctrl Pts',(3.12864469399994,12.2,10.05501675));
#218259=CARTESIAN_POINT('Ctrl Pts',(3.12777292999994,12.2,10.053395635));
#218260=CARTESIAN_POINT('Ctrl Pts',(3.12690613999994,12.2,10.051780219));
#218261=CARTESIAN_POINT('Ctrl Pts',(3.12604432099994,12.2,10.050170521));
#218262=CARTESIAN_POINT('Ctrl Pts',(3.12518747099995,12.2,10.048566563));
#218263=CARTESIAN_POINT('Ctrl Pts',(3.12433558499994,12.2,10.046968364));
#218264=CARTESIAN_POINT('Ctrl Pts',(3.12348866099994,12.2,10.045375946));
#218265=CARTESIAN_POINT('Ctrl Pts',(3.12264669699994,12.2,10.043789328));
#218266=CARTESIAN_POINT('Ctrl Pts',(3.12180968799994,12.2,10.042208533));
#218267=CARTESIAN_POINT('Ctrl Pts',(3.12097763099994,12.2,10.040633581));
#218268=CARTESIAN_POINT('Ctrl Pts',(3.12015052399994,12.2,10.039064492));
#218269=CARTESIAN_POINT('Ctrl Pts',(3.11932836299994,12.2,10.037501289));
#218270=CARTESIAN_POINT('Ctrl Pts',(3.11851114499994,12.2,10.035943991));
#218271=CARTESIAN_POINT('Ctrl Pts',(3.11769886699994,12.2,10.034392622));
#218272=CARTESIAN_POINT('Ctrl Pts',(3.11689152499994,12.2,10.0328472));
#218273=CARTESIAN_POINT('Ctrl Pts',(3.11608911699994,12.2,10.031307748));
#218274=CARTESIAN_POINT('Ctrl Pts',(3.11529163799994,12.2,10.029774289));
#218275=CARTESIAN_POINT('Ctrl Pts',(3.11449908499994,12.2,10.028246841));
#218276=CARTESIAN_POINT('Ctrl Pts',(3.11371145699994,12.2,10.026725429));
#218277=CARTESIAN_POINT('Ctrl Pts',(3.11292874799994,12.2,10.025210072));
#218278=CARTESIAN_POINT('Ctrl Pts',(3.11215095499994,12.2,10.023700794));
#218279=CARTESIAN_POINT('Ctrl Pts',(3.11137807399994,12.2,10.022197616));
#218280=CARTESIAN_POINT('Ctrl Pts',(3.11061010399994,12.2,10.020700559));
#218281=CARTESIAN_POINT('Ctrl Pts',(3.10984703899994,12.2,10.019209646));
#218282=CARTESIAN_POINT('Ctrl Pts',(3.10908887599994,12.2,10.017724899));
#218283=CARTESIAN_POINT('Ctrl Pts',(3.10833561299994,12.2,10.01624634));
#218284=CARTESIAN_POINT('Ctrl Pts',(3.10758724499994,12.2,10.01477399));
#218285=CARTESIAN_POINT('Ctrl Pts',(3.10684376799994,12.2,10.013307874));
#218286=CARTESIAN_POINT('Ctrl Pts',(3.10610517999995,12.2,10.011848013));
#218287=CARTESIAN_POINT('Ctrl Pts',(3.10537147499995,12.2,10.010394428));
#218288=CARTESIAN_POINT('Ctrl Pts',(3.10464265199994,12.2,10.008947144));
#218289=CARTESIAN_POINT('Ctrl Pts',(3.10391870499994,12.2,10.007506183));
#218290=CARTESIAN_POINT('Ctrl Pts',(3.10319963199994,12.2,10.006071567));
#218291=CARTESIAN_POINT('Ctrl Pts',(3.10248542799994,12.2,10.00464332));
#218292=CARTESIAN_POINT('Ctrl Pts',(3.10177608999994,12.2,10.003221464));
#218293=CARTESIAN_POINT('Ctrl Pts',(3.10107161399995,12.2,10.001806022));
#218294=CARTESIAN_POINT('Ctrl Pts',(3.10037199499994,12.2,10.000397017));
#218295=CARTESIAN_POINT('Ctrl Pts',(3.09967723099994,12.2,9.99899447299999));
#218296=CARTESIAN_POINT('Ctrl Pts',(3.09898731599994,12.2,9.99759841199998));
#218297=CARTESIAN_POINT('Ctrl Pts',(3.09830224899994,12.2,9.99620885899999));
#218298=CARTESIAN_POINT('Ctrl Pts',(3.09762202399994,12.2,9.99482583699999));
#218299=CARTESIAN_POINT('Ctrl Pts',(3.09694663699994,12.2,9.99344936799999));
#218300=CARTESIAN_POINT('Ctrl Pts',(3.09627608499994,12.2,9.99207947799999));
#218301=CARTESIAN_POINT('Ctrl Pts',(3.09561036199994,12.2,9.99071618899999));
#218302=CARTESIAN_POINT('Ctrl Pts',(3.09494946499994,12.2,9.98935952599999));
#218303=CARTESIAN_POINT('Ctrl Pts',(3.09429339099994,12.2,9.98800951199998));
#218304=CARTESIAN_POINT('Ctrl Pts',(3.09364213499994,12.2,9.98666617199999));
#218305=CARTESIAN_POINT('Ctrl Pts',(3.09299569299994,12.2,9.98532952799999));
#218306=CARTESIAN_POINT('Ctrl Pts',(3.09235405999994,12.2,9.98399960799999));
#218307=CARTESIAN_POINT('Ctrl Pts',(3.09171723299994,12.2,9.98267643199998));
#218308=CARTESIAN_POINT('Ctrl Pts',(3.09108520699994,12.2,9.98136002699999));
#218309=CARTESIAN_POINT('Ctrl Pts',(3.09045797699994,12.2,9.98005041799999));
#218310=CARTESIAN_POINT('Ctrl Pts',(3.08983553999994,12.2,9.97874762799999));
#218311=CARTESIAN_POINT('Ctrl Pts',(3.08921789099994,12.2,9.97745168099998));
#218312=CARTESIAN_POINT('Ctrl Pts',(3.08860502499994,12.2,9.97616260499999));
#218313=CARTESIAN_POINT('Ctrl Pts',(3.08799693999994,12.2,9.97488042299998));
#218314=CARTESIAN_POINT('Ctrl Pts',(3.08739362899995,12.2,9.97360515799999));
#218315=CARTESIAN_POINT('Ctrl Pts',(3.08679508799994,12.2,9.97233683899999));
#218316=CARTESIAN_POINT('Ctrl Pts',(3.08620131299994,12.2,9.97107548899999));
#218317=CARTESIAN_POINT('Ctrl Pts',(3.08561229999994,12.2,9.96982113299998));
#218318=CARTESIAN_POINT('Ctrl Pts',(3.08502804299994,12.2,9.96857379799999));
#218319=CARTESIAN_POINT('Ctrl Pts',(3.08444853899994,12.2,9.96733350799998));
#218320=CARTESIAN_POINT('Ctrl Pts',(3.08387378199994,12.2,9.96610028999999));
#218321=CARTESIAN_POINT('Ctrl Pts',(3.08330376799994,12.2,9.96487416799998));
#218322=CARTESIAN_POINT('Ctrl Pts',(3.08273849199994,12.2,9.96365516999998));
#218323=CARTESIAN_POINT('Ctrl Pts',(3.08217794999994,12.2,9.96244332099998));
#218324=CARTESIAN_POINT('Ctrl Pts',(3.08162213499994,12.2,9.96123864599999));
#218325=CARTESIAN_POINT('Ctrl Pts',(3.08107104499994,12.2,9.96004117299999));
#218326=CARTESIAN_POINT('Ctrl Pts',(3.08052467399994,12.2,9.95885092599998));
#218327=CARTESIAN_POINT('Ctrl Pts',(3.07998301799994,12.2,9.95766793499998));
#218328=CARTESIAN_POINT('Ctrl Pts',(3.07944606999994,12.2,9.95649222299999));
#218329=CARTESIAN_POINT('Ctrl Pts',(3.07891382499994,12.2,9.95532381799999));
#218330=CARTESIAN_POINT('Ctrl Pts',(3.07838628099995,12.2,9.95416274699998));
#218331=CARTESIAN_POINT('Ctrl Pts',(3.07786343199994,12.2,9.95300903699999));
#218332=CARTESIAN_POINT('Ctrl Pts',(3.07734526999994,12.2,9.95186271399999));
#218333=CARTESIAN_POINT('Ctrl Pts',(3.07683179299994,12.2,9.95072380599998));
#218334=CARTESIAN_POINT('Ctrl Pts',(3.07632299499994,12.2,9.94959233999998));
#218335=CARTESIAN_POINT('Ctrl Pts',(3.07581887099994,12.2,9.94846834399999));
#218336=CARTESIAN_POINT('Ctrl Pts',(3.07531941599994,12.2,9.94735184399998));
#218337=CARTESIAN_POINT('Ctrl Pts',(3.07482462299994,12.2,9.94624286799999));
#218338=CARTESIAN_POINT('Ctrl Pts',(3.07433448899994,12.2,9.94514144399999));
#218339=CARTESIAN_POINT('Ctrl Pts',(3.07384900699994,12.2,9.94404759999998));
#218340=CARTESIAN_POINT('Ctrl Pts',(3.07336817399994,12.2,9.94296136499998));
#218341=CARTESIAN_POINT('Ctrl Pts',(3.07289198199994,12.2,9.94188276499998));
#218342=CARTESIAN_POINT('Ctrl Pts',(3.07242042599994,12.2,9.94081182999999));
#218343=CARTESIAN_POINT('Ctrl Pts',(3.07195350199994,12.2,9.93974858599999));
#218344=CARTESIAN_POINT('Ctrl Pts',(3.07149120299994,12.2,9.93869306299998));
#218345=CARTESIAN_POINT('Ctrl Pts',(3.07103352399994,12.2,9.93764528999998));
#218346=CARTESIAN_POINT('Ctrl Pts',(3.07058045999994,12.2,9.93660529599998));
#218347=CARTESIAN_POINT('Ctrl Pts',(3.07013200399994,12.2,9.93557310899998));
#218348=CARTESIAN_POINT('Ctrl Pts',(3.06968815199995,12.2,9.93454875599999));
#218349=CARTESIAN_POINT('Ctrl Pts',(3.06924889699994,12.2,9.93353227099998));
#218350=CARTESIAN_POINT('Ctrl Pts',(3.06881423399994,12.2,9.93252367899998));
#218351=CARTESIAN_POINT('Ctrl Pts',(3.06838415699994,12.2,9.93152301099999));
#218352=CARTESIAN_POINT('Ctrl Pts',(3.06795865999994,12.2,9.93053029599999));
#218353=CARTESIAN_POINT('Ctrl Pts',(3.06753773799994,12.2,9.92954556499999));
#218354=CARTESIAN_POINT('Ctrl Pts',(3.06712138399994,12.2,9.92856884599998));
#218355=CARTESIAN_POINT('Ctrl Pts',(3.06670959199994,12.2,9.92760017099998));
#218356=CARTESIAN_POINT('Ctrl Pts',(3.06630235599994,12.2,9.92663956799999));
#218357=CARTESIAN_POINT('Ctrl Pts',(3.06589967099994,12.2,9.92568706699998));
#218358=CARTESIAN_POINT('Ctrl Pts',(3.06550152999994,12.2,9.92474270099999));
#218359=CARTESIAN_POINT('Ctrl Pts',(3.06510792699994,12.2,9.92380649899999));
#218360=CARTESIAN_POINT('Ctrl Pts',(3.06471885599994,12.2,9.92287849099998));
#218361=CARTESIAN_POINT('Ctrl Pts',(3.06433431199994,12.2,9.92195870799998));
#218362=CARTESIAN_POINT('Ctrl Pts',(3.06395428599994,12.2,9.92104718299998));
#218363=CARTESIAN_POINT('Ctrl Pts',(3.06357877399994,12.2,9.92014394499999));
#218364=CARTESIAN_POINT('Ctrl Pts',(3.06320776799994,12.2,9.91924902499999));
#218365=CARTESIAN_POINT('Ctrl Pts',(3.06284126399994,12.2,9.91836245599998));
#218366=CARTESIAN_POINT('Ctrl Pts',(3.06247925299994,12.2,9.91748426799998));
#218367=CARTESIAN_POINT('Ctrl Pts',(3.06212172999994,12.2,9.91661449399999));
#218368=CARTESIAN_POINT('Ctrl Pts',(3.06176868699994,12.2,9.91575316599998));
#218369=CARTESIAN_POINT('Ctrl Pts',(3.06142212599994,12.2,9.91490522599998));
#218370=CARTESIAN_POINT('Ctrl Pts',(3.06114880299994,12.2,9.91423456699999));
#218371=CARTESIAN_POINT('Ctrl Pts',(3.06094627499994,12.2,9.91373655899999));
#218372=CARTESIAN_POINT('Ctrl Pts',(3.06081277599994,12.2,9.91340782599998));
#218373=CARTESIAN_POINT('Ctrl Pts',(3.06074721199994,12.2,9.91324626499999));
#218374=CARTESIAN_POINT('Ctrl Pts',(3.06074721199994,15.2,9.91324626499999));
#218375=CARTESIAN_POINT('Ctrl Pts',(3.06081277599994,15.2,9.91340782599998));
#218376=CARTESIAN_POINT('Ctrl Pts',(3.06094627499994,15.2,9.91373655899999));
#218377=CARTESIAN_POINT('Ctrl Pts',(3.06114880299994,15.2,9.91423456699999));
#218378=CARTESIAN_POINT('Ctrl Pts',(3.06142212599994,15.2,9.91490522599998));
#218379=CARTESIAN_POINT('Ctrl Pts',(3.06176868699994,15.2,9.91575316599998));
#218380=CARTESIAN_POINT('Ctrl Pts',(3.06212172999994,15.2,9.91661449399999));
#218381=CARTESIAN_POINT('Ctrl Pts',(3.06247925299994,15.2,9.91748426799998));
#218382=CARTESIAN_POINT('Ctrl Pts',(3.06284126399994,15.2,9.91836245599998));
#218383=CARTESIAN_POINT('Ctrl Pts',(3.06320776799994,15.2,9.91924902499999));
#218384=CARTESIAN_POINT('Ctrl Pts',(3.06357877399994,15.2,9.92014394499999));
#218385=CARTESIAN_POINT('Ctrl Pts',(3.06395428599994,15.2,9.92104718299998));
#218386=CARTESIAN_POINT('Ctrl Pts',(3.06433431199994,15.2,9.92195870799998));
#218387=CARTESIAN_POINT('Ctrl Pts',(3.06471885599994,15.2,9.92287849099998));
#218388=CARTESIAN_POINT('Ctrl Pts',(3.06510792699994,15.2,9.92380649899999));
#218389=CARTESIAN_POINT('Ctrl Pts',(3.06550152999994,15.2,9.92474270099999));
#218390=CARTESIAN_POINT('Ctrl Pts',(3.06589967099994,15.2,9.92568706699998));
#218391=CARTESIAN_POINT('Ctrl Pts',(3.06630235599994,15.2,9.92663956799999));
#218392=CARTESIAN_POINT('Ctrl Pts',(3.06670959199994,15.2,9.92760017099998));
#218393=CARTESIAN_POINT('Ctrl Pts',(3.06712138399994,15.2,9.92856884599998));
#218394=CARTESIAN_POINT('Ctrl Pts',(3.06753773799994,15.2,9.92954556499999));
#218395=CARTESIAN_POINT('Ctrl Pts',(3.06795865999994,15.2,9.93053029599999));
#218396=CARTESIAN_POINT('Ctrl Pts',(3.06838415699994,15.2,9.93152301099999));
#218397=CARTESIAN_POINT('Ctrl Pts',(3.06881423399994,15.2,9.93252367899998));
#218398=CARTESIAN_POINT('Ctrl Pts',(3.06924889699994,15.2,9.93353227099998));
#218399=CARTESIAN_POINT('Ctrl Pts',(3.06968815199995,15.2,9.93454875599999));
#218400=CARTESIAN_POINT('Ctrl Pts',(3.07013200399994,15.2,9.93557310899998));
#218401=CARTESIAN_POINT('Ctrl Pts',(3.07058045999994,15.2,9.93660529599998));
#218402=CARTESIAN_POINT('Ctrl Pts',(3.07103352399994,15.2,9.93764528999998));
#218403=CARTESIAN_POINT('Ctrl Pts',(3.07149120299994,15.2,9.93869306299998));
#218404=CARTESIAN_POINT('Ctrl Pts',(3.07195350199994,15.2,9.93974858599999));
#218405=CARTESIAN_POINT('Ctrl Pts',(3.07242042599994,15.2,9.94081182999999));
#218406=CARTESIAN_POINT('Ctrl Pts',(3.07289198199994,15.2,9.94188276499998));
#218407=CARTESIAN_POINT('Ctrl Pts',(3.07336817399994,15.2,9.94296136499998));
#218408=CARTESIAN_POINT('Ctrl Pts',(3.07384900699994,15.2,9.94404759999998));
#218409=CARTESIAN_POINT('Ctrl Pts',(3.07433448899994,15.2,9.94514144399999));
#218410=CARTESIAN_POINT('Ctrl Pts',(3.07482462299994,15.2,9.94624286799999));
#218411=CARTESIAN_POINT('Ctrl Pts',(3.07531941599994,15.2,9.94735184399998));
#218412=CARTESIAN_POINT('Ctrl Pts',(3.07581887099994,15.2,9.94846834399999));
#218413=CARTESIAN_POINT('Ctrl Pts',(3.07632299499994,15.2,9.94959233999998));
#218414=CARTESIAN_POINT('Ctrl Pts',(3.07683179299994,15.2,9.95072380599998));
#218415=CARTESIAN_POINT('Ctrl Pts',(3.07734526999994,15.2,9.95186271399999));
#218416=CARTESIAN_POINT('Ctrl Pts',(3.07786343199994,15.2,9.95300903699999));
#218417=CARTESIAN_POINT('Ctrl Pts',(3.07838628099995,15.2,9.95416274699998));
#218418=CARTESIAN_POINT('Ctrl Pts',(3.07891382499994,15.2,9.95532381799999));
#218419=CARTESIAN_POINT('Ctrl Pts',(3.07944606999994,15.2,9.95649222299999));
#218420=CARTESIAN_POINT('Ctrl Pts',(3.07998301799994,15.2,9.95766793499998));
#218421=CARTESIAN_POINT('Ctrl Pts',(3.08052467399994,15.2,9.95885092599998));
#218422=CARTESIAN_POINT('Ctrl Pts',(3.08107104499994,15.2,9.96004117299999));
#218423=CARTESIAN_POINT('Ctrl Pts',(3.08162213499994,15.2,9.96123864599999));
#218424=CARTESIAN_POINT('Ctrl Pts',(3.08217794999994,15.2,9.96244332099998));
#218425=CARTESIAN_POINT('Ctrl Pts',(3.08273849199994,15.2,9.96365516999998));
#218426=CARTESIAN_POINT('Ctrl Pts',(3.08330376799994,15.2,9.96487416799998));
#218427=CARTESIAN_POINT('Ctrl Pts',(3.08387378199994,15.2,9.96610028999999));
#218428=CARTESIAN_POINT('Ctrl Pts',(3.08444853899994,15.2,9.96733350799998));
#218429=CARTESIAN_POINT('Ctrl Pts',(3.08502804299994,15.2,9.96857379799999));
#218430=CARTESIAN_POINT('Ctrl Pts',(3.08561229999994,15.2,9.96982113299998));
#218431=CARTESIAN_POINT('Ctrl Pts',(3.08620131299994,15.2,9.97107548899999));
#218432=CARTESIAN_POINT('Ctrl Pts',(3.08679508799994,15.2,9.97233683899999));
#218433=CARTESIAN_POINT('Ctrl Pts',(3.08739362899995,15.2,9.97360515799999));
#218434=CARTESIAN_POINT('Ctrl Pts',(3.08799693999994,15.2,9.97488042299998));
#218435=CARTESIAN_POINT('Ctrl Pts',(3.08860502499994,15.2,9.97616260499999));
#218436=CARTESIAN_POINT('Ctrl Pts',(3.08921789099994,15.2,9.97745168099998));
#218437=CARTESIAN_POINT('Ctrl Pts',(3.08983553999994,15.2,9.97874762799999));
#218438=CARTESIAN_POINT('Ctrl Pts',(3.09045797699994,15.2,9.98005041799999));
#218439=CARTESIAN_POINT('Ctrl Pts',(3.09108520699994,15.2,9.98136002699999));
#218440=CARTESIAN_POINT('Ctrl Pts',(3.09171723299994,15.2,9.98267643199998));
#218441=CARTESIAN_POINT('Ctrl Pts',(3.09235405999994,15.2,9.98399960799999));
#218442=CARTESIAN_POINT('Ctrl Pts',(3.09299569299994,15.2,9.98532952799999));
#218443=CARTESIAN_POINT('Ctrl Pts',(3.09364213499994,15.2,9.98666617199999));
#218444=CARTESIAN_POINT('Ctrl Pts',(3.09429339099994,15.2,9.98800951199998));
#218445=CARTESIAN_POINT('Ctrl Pts',(3.09494946499994,15.2,9.98935952599999));
#218446=CARTESIAN_POINT('Ctrl Pts',(3.09561036199994,15.2,9.99071618899999));
#218447=CARTESIAN_POINT('Ctrl Pts',(3.09627608499994,15.2,9.99207947799999));
#218448=CARTESIAN_POINT('Ctrl Pts',(3.09694663699994,15.2,9.99344936799999));
#218449=CARTESIAN_POINT('Ctrl Pts',(3.09762202399994,15.2,9.99482583699999));
#218450=CARTESIAN_POINT('Ctrl Pts',(3.09830224899994,15.2,9.99620885899999));
#218451=CARTESIAN_POINT('Ctrl Pts',(3.09898731599994,15.2,9.99759841199998));
#218452=CARTESIAN_POINT('Ctrl Pts',(3.09967723099994,15.2,9.99899447299999));
#218453=CARTESIAN_POINT('Ctrl Pts',(3.10037199499994,15.2,10.000397017));
#218454=CARTESIAN_POINT('Ctrl Pts',(3.10107161399995,15.2,10.001806022));
#218455=CARTESIAN_POINT('Ctrl Pts',(3.10177608999994,15.2,10.003221464));
#218456=CARTESIAN_POINT('Ctrl Pts',(3.10248542799994,15.2,10.00464332));
#218457=CARTESIAN_POINT('Ctrl Pts',(3.10319963199994,15.2,10.006071567));
#218458=CARTESIAN_POINT('Ctrl Pts',(3.10391870499994,15.2,10.007506183));
#218459=CARTESIAN_POINT('Ctrl Pts',(3.10464265199994,15.2,10.008947144));
#218460=CARTESIAN_POINT('Ctrl Pts',(3.10537147499995,15.2,10.010394428));
#218461=CARTESIAN_POINT('Ctrl Pts',(3.10610517999995,15.2,10.011848013));
#218462=CARTESIAN_POINT('Ctrl Pts',(3.10684376799994,15.2,10.013307874));
#218463=CARTESIAN_POINT('Ctrl Pts',(3.10758724499994,15.2,10.01477399));
#218464=CARTESIAN_POINT('Ctrl Pts',(3.10833561299994,15.2,10.01624634));
#218465=CARTESIAN_POINT('Ctrl Pts',(3.10908887599994,15.2,10.017724899));
#218466=CARTESIAN_POINT('Ctrl Pts',(3.10984703899994,15.2,10.019209646));
#218467=CARTESIAN_POINT('Ctrl Pts',(3.11061010399994,15.2,10.020700559));
#218468=CARTESIAN_POINT('Ctrl Pts',(3.11137807399994,15.2,10.022197616));
#218469=CARTESIAN_POINT('Ctrl Pts',(3.11215095499994,15.2,10.023700794));
#218470=CARTESIAN_POINT('Ctrl Pts',(3.11292874799994,15.2,10.025210072));
#218471=CARTESIAN_POINT('Ctrl Pts',(3.11371145699994,15.2,10.026725429));
#218472=CARTESIAN_POINT('Ctrl Pts',(3.11449908499994,15.2,10.028246841));
#218473=CARTESIAN_POINT('Ctrl Pts',(3.11529163799994,15.2,10.029774289));
#218474=CARTESIAN_POINT('Ctrl Pts',(3.11608911699994,15.2,10.031307748));
#218475=CARTESIAN_POINT('Ctrl Pts',(3.11689152499994,15.2,10.0328472));
#218476=CARTESIAN_POINT('Ctrl Pts',(3.11769886699994,15.2,10.034392622));
#218477=CARTESIAN_POINT('Ctrl Pts',(3.11851114499994,15.2,10.035943991));
#218478=CARTESIAN_POINT('Ctrl Pts',(3.11932836299994,15.2,10.037501289));
#218479=CARTESIAN_POINT('Ctrl Pts',(3.12015052399994,15.2,10.039064492));
#218480=CARTESIAN_POINT('Ctrl Pts',(3.12097763099994,15.2,10.040633581));
#218481=CARTESIAN_POINT('Ctrl Pts',(3.12180968799994,15.2,10.042208533));
#218482=CARTESIAN_POINT('Ctrl Pts',(3.12264669699994,15.2,10.043789328));
#218483=CARTESIAN_POINT('Ctrl Pts',(3.12348866099994,15.2,10.045375946));
#218484=CARTESIAN_POINT('Ctrl Pts',(3.12433558499994,15.2,10.046968364));
#218485=CARTESIAN_POINT('Ctrl Pts',(3.12518747099995,15.2,10.048566563));
#218486=CARTESIAN_POINT('Ctrl Pts',(3.12604432099994,15.2,10.050170521));
#218487=CARTESIAN_POINT('Ctrl Pts',(3.12690613999994,15.2,10.051780219));
#218488=CARTESIAN_POINT('Ctrl Pts',(3.12777292999994,15.2,10.053395635));
#218489=CARTESIAN_POINT('Ctrl Pts',(3.12864469399994,15.2,10.05501675));
#218490=CARTESIAN_POINT('Ctrl Pts',(3.12952143499994,15.2,10.056643542));
#218491=CARTESIAN_POINT('Ctrl Pts',(3.13040315599994,15.2,10.058275991));
#218492=CARTESIAN_POINT('Ctrl Pts',(3.13128985999994,15.2,10.059914077));
#218493=CARTESIAN_POINT('Ctrl Pts',(3.13218154999995,15.2,10.061557781));
#218494=CARTESIAN_POINT('Ctrl Pts',(3.13307822999994,15.2,10.063207081));
#218495=CARTESIAN_POINT('Ctrl Pts',(3.13397989999994,15.2,10.064861958));
#218496=CARTESIAN_POINT('Ctrl Pts',(3.13488656499994,15.2,10.066522392));
#218497=CARTESIAN_POINT('Ctrl Pts',(3.13579822699994,15.2,10.068188362));
#218498=CARTESIAN_POINT('Ctrl Pts',(3.13671488999994,15.2,10.069859849));
#218499=CARTESIAN_POINT('Ctrl Pts',(3.13763655599994,15.2,10.071536834));
#218500=CARTESIAN_POINT('Ctrl Pts',(3.13856322699994,15.2,10.073219296));
#218501=CARTESIAN_POINT('Ctrl Pts',(3.13949490699994,15.2,10.074907216));
#218502=CARTESIAN_POINT('Ctrl Pts',(3.14043159899994,15.2,10.076600574));
#218503=CARTESIAN_POINT('Ctrl Pts',(3.14137330399994,15.2,10.078299351));
#218504=CARTESIAN_POINT('Ctrl Pts',(3.14232002399994,15.2,10.080003527));
#218505=CARTESIAN_POINT('Ctrl Pts',(3.14327176599994,15.2,10.081713083));
#218506=CARTESIAN_POINT('Ctrl Pts',(3.14422852799995,15.2,10.083427999));
#218507=CARTESIAN_POINT('Ctrl Pts',(3.14519031499994,15.2,10.085148257));
#218508=CARTESIAN_POINT('Ctrl Pts',(3.14615712899994,15.2,10.086873837));
#218509=CARTESIAN_POINT('Ctrl Pts',(3.14712897199994,15.2,10.08860472));
#218510=CARTESIAN_POINT('Ctrl Pts',(3.14810584799994,15.2,10.090340886));
#218511=CARTESIAN_POINT('Ctrl Pts',(3.14908775899994,15.2,10.092082318));
#218512=CARTESIAN_POINT('Ctrl Pts',(3.15007470599994,15.2,10.093828996));
#218513=CARTESIAN_POINT('Ctrl Pts',(3.15106669299994,15.2,10.0955809));
#218514=CARTESIAN_POINT('Ctrl Pts',(3.15206372299994,15.2,10.097338013));
#218515=CARTESIAN_POINT('Ctrl Pts',(3.15306579799994,15.2,10.099100315));
#218516=CARTESIAN_POINT('Ctrl Pts',(3.15407291799994,15.2,10.100867788));
#218517=CARTESIAN_POINT('Ctrl Pts',(3.15508508899994,15.2,10.102640413));
#218518=CARTESIAN_POINT('Ctrl Pts',(3.15610231199994,15.2,10.104418172));
#218519=CARTESIAN_POINT('Ctrl Pts',(3.15712458699994,15.2,10.106201046));
#218520=CARTESIAN_POINT('Ctrl Pts',(3.15815192199994,15.2,10.107989016));
#218521=CARTESIAN_POINT('Ctrl Pts',(3.15918431399994,15.2,10.109782065));
#218522=CARTESIAN_POINT('Ctrl Pts',(3.16022176599994,15.2,10.111580173));
#218523=CARTESIAN_POINT('Ctrl Pts',(3.16126428299994,15.2,10.113383323));
#218524=CARTESIAN_POINT('Ctrl Pts',(3.16231186499994,15.2,10.115191496));
#218525=CARTESIAN_POINT('Ctrl Pts',(3.16336451599994,15.2,10.117004675));
#218526=CARTESIAN_POINT('Ctrl Pts',(3.16442223699994,15.2,10.11882284));
#218527=CARTESIAN_POINT('Ctrl Pts',(3.16548502999995,15.2,10.120645975));
#218528=CARTESIAN_POINT('Ctrl Pts',(3.16655289799994,15.2,10.12247406));
#218529=CARTESIAN_POINT('Ctrl Pts',(3.16762584299994,15.2,10.124307078));
#218530=CARTESIAN_POINT('Ctrl Pts',(3.16870386699994,15.2,10.126145011));
#218531=CARTESIAN_POINT('Ctrl Pts',(3.16978697099994,15.2,10.127987842));
#218532=CARTESIAN_POINT('Ctrl Pts',(3.17087515899994,15.2,10.129835553));
#218533=CARTESIAN_POINT('Ctrl Pts',(3.17196843199994,15.2,10.131688125));
#218534=CARTESIAN_POINT('Ctrl Pts',(3.17306679399994,15.2,10.133545542));
#218535=CARTESIAN_POINT('Ctrl Pts',(3.17417024399994,15.2,10.135407784));
#218536=CARTESIAN_POINT('Ctrl Pts',(3.17527878599994,15.2,10.137274836));
#218537=CARTESIAN_POINT('Ctrl Pts',(3.17639242199995,15.2,10.13914668));
#218538=CARTESIAN_POINT('Ctrl Pts',(3.17751115299994,15.2,10.141023297));
#218539=CARTESIAN_POINT('Ctrl Pts',(3.17863498099995,15.2,10.142904671));
#218540=CARTESIAN_POINT('Ctrl Pts',(3.17976390999994,15.2,10.144790784));
#218541=CARTESIAN_POINT('Ctrl Pts',(3.18089793999994,15.2,10.146681619));
#218542=CARTESIAN_POINT('Ctrl Pts',(3.18203707299994,15.2,10.148577159));
#218543=CARTESIAN_POINT('Ctrl Pts',(3.18318131199995,15.2,10.150477387));
#218544=CARTESIAN_POINT('Ctrl Pts',(3.18433065699995,15.2,10.152382285));
#218545=CARTESIAN_POINT('Ctrl Pts',(3.18548511399994,15.2,10.154291836));
#218546=CARTESIAN_POINT('Ctrl Pts',(3.18664467899994,15.2,10.156206023));
#218547=CARTESIAN_POINT('Ctrl Pts',(3.18780935899994,15.2,10.158124831));
#218548=CARTESIAN_POINT('Ctrl Pts',(3.18897915299994,15.2,10.160048239));
#218549=CARTESIAN_POINT('Ctrl Pts',(3.19015406399994,15.2,10.161976234));
#218550=CARTESIAN_POINT('Ctrl Pts',(3.19133409399994,15.2,10.163908798));
#218551=CARTESIAN_POINT('Ctrl Pts',(3.19251924199994,15.2,10.165845913));
#218552=CARTESIAN_POINT('Ctrl Pts',(3.19370951399994,15.2,10.167787564));
#218553=CARTESIAN_POINT('Ctrl Pts',(3.19490490899994,15.2,10.169733732));
#218554=CARTESIAN_POINT('Ctrl Pts',(3.19610542999994,15.2,10.171684403));
#218555=CARTESIAN_POINT('Ctrl Pts',(3.19731107699994,15.2,10.173639559));
#218556=CARTESIAN_POINT('Ctrl Pts',(3.19852185399994,15.2,10.175599184));
#218557=CARTESIAN_POINT('Ctrl Pts',(3.19973776199994,15.2,10.17756326));
#218558=CARTESIAN_POINT('Ctrl Pts',(3.20095880099994,15.2,10.179531773));
#218559=CARTESIAN_POINT('Ctrl Pts',(3.20218497399994,15.2,10.181504705));
#218560=CARTESIAN_POINT('Ctrl Pts',(3.20341628299994,15.2,10.183482041));
#218561=CARTESIAN_POINT('Ctrl Pts',(3.20465272999995,15.2,10.185463762));
#218562=CARTESIAN_POINT('Ctrl Pts',(3.20589431499994,15.2,10.187449854));
#218563=CARTESIAN_POINT('Ctrl Pts',(3.20714103999994,15.2,10.189440301));
#218564=CARTESIAN_POINT('Ctrl Pts',(3.20839290699994,15.2,10.191435086));
#218565=CARTESIAN_POINT('Ctrl Pts',(3.20964991799995,15.2,10.193434192));
#218566=CARTESIAN_POINT('Ctrl Pts',(3.21091207399995,15.2,10.195437604));
#218567=CARTESIAN_POINT('Ctrl Pts',(3.21217937699994,15.2,10.197445307));
#218568=CARTESIAN_POINT('Ctrl Pts',(3.21345182799994,15.2,10.199457283));
#218569=CARTESIAN_POINT('Ctrl Pts',(3.21472942799994,15.2,10.201473517));
#218570=CARTESIAN_POINT('Ctrl Pts',(3.21601217999994,15.2,10.203493994));
#218571=CARTESIAN_POINT('Ctrl Pts',(3.21730008399994,15.2,10.205518696));
#218572=CARTESIAN_POINT('Ctrl Pts',(3.21859314299994,15.2,10.20754761));
#218573=CARTESIAN_POINT('Ctrl Pts',(3.21989135599994,15.2,10.209580717));
#218574=CARTESIAN_POINT('Ctrl Pts',(3.22119472699995,15.2,10.211618004));
#218575=CARTESIAN_POINT('Ctrl Pts',(3.22250325599994,15.2,10.213659454));
#218576=CARTESIAN_POINT('Ctrl Pts',(3.22381694499994,15.2,10.215705052));
#218577=CARTESIAN_POINT('Ctrl Pts',(3.22513579399994,15.2,10.217754781));
#218578=CARTESIAN_POINT('Ctrl Pts',(3.22645980699994,15.2,10.219808628));
#218579=CARTESIAN_POINT('Ctrl Pts',(3.22778898299994,15.2,10.221866575));
#218580=CARTESIAN_POINT('Ctrl Pts',(3.22912332499994,15.2,10.223928608));
#218581=CARTESIAN_POINT('Ctrl Pts',(3.23046283199994,15.2,10.225994711));
#218582=CARTESIAN_POINT('Ctrl Pts',(3.23180750799994,15.2,10.228064869));
#218583=CARTESIAN_POINT('Ctrl Pts',(3.23315735299994,15.2,10.230139067));
#218584=CARTESIAN_POINT('Ctrl Pts',(3.23451236799994,15.2,10.232217288));
#218585=CARTESIAN_POINT('Ctrl Pts',(3.23587255499994,15.2,10.23429952));
#218586=CARTESIAN_POINT('Ctrl Pts',(3.23723791499994,15.2,10.236385745));
#218587=CARTESIAN_POINT('Ctrl Pts',(3.23860844899994,15.2,10.238475948));
#218588=CARTESIAN_POINT('Ctrl Pts',(3.23998415799994,15.2,10.240570115));
#218589=CARTESIAN_POINT('Ctrl Pts',(3.24136504399994,15.2,10.242668229));
#218590=CARTESIAN_POINT('Ctrl Pts',(3.24275110699995,15.2,10.244770278));
#218591=CARTESIAN_POINT('Ctrl Pts',(3.24414234999994,15.2,10.246876245));
#218592=CARTESIAN_POINT('Ctrl Pts',(3.24553877199994,15.2,10.248986116));
#218593=CARTESIAN_POINT('Ctrl Pts',(3.24694037599994,15.2,10.251099875));
#218594=CARTESIAN_POINT('Ctrl Pts',(3.24834716199994,15.2,10.253217507));
#218595=CARTESIAN_POINT('Ctrl Pts',(3.24975913199995,15.2,10.255338999));
#218596=CARTESIAN_POINT('Ctrl Pts',(3.25117628599994,15.2,10.257464334));
#218597=CARTESIAN_POINT('Ctrl Pts',(3.25259862599995,15.2,10.259593498));
#218598=CARTESIAN_POINT('Ctrl Pts',(3.25402615299994,15.2,10.261726478));
#218599=CARTESIAN_POINT('Ctrl Pts',(3.25545886799994,15.2,10.263863257));
#218600=CARTESIAN_POINT('Ctrl Pts',(3.25689677199994,15.2,10.266003821));
#218601=CARTESIAN_POINT('Ctrl Pts',(3.25833986599994,15.2,10.268148156));
#218602=CARTESIAN_POINT('Ctrl Pts',(3.25978815099994,15.2,10.270296246));
#218603=CARTESIAN_POINT('Ctrl Pts',(3.26124162699994,15.2,10.272448079));
#218604=CARTESIAN_POINT('Ctrl Pts',(3.26270029699995,15.2,10.274603639));
#218605=CARTESIAN_POINT('Ctrl Pts',(3.26416416099994,15.2,10.276762911));
#218606=CARTESIAN_POINT('Ctrl Pts',(3.26563321999994,15.2,10.27892588));
#218607=CARTESIAN_POINT('Ctrl Pts',(3.26710747499994,15.2,10.281092534));
#218608=CARTESIAN_POINT('Ctrl Pts',(3.26858692799994,15.2,10.283262858));
#218609=CARTESIAN_POINT('Ctrl Pts',(3.27007157799994,15.2,10.285436836));
#218610=CARTESIAN_POINT('Ctrl Pts',(3.27156142599994,15.2,10.287614454));
#218611=CARTESIAN_POINT('Ctrl Pts',(3.27305647499994,15.2,10.2897957));
#218612=CARTESIAN_POINT('Ctrl Pts',(3.27455672399994,15.2,10.291980559));
#218613=CARTESIAN_POINT('Ctrl Pts',(3.27606217499994,15.2,10.294169016));
#218614=CARTESIAN_POINT('Ctrl Pts',(3.27757282699995,15.2,10.296361056));
#218615=CARTESIAN_POINT('Ctrl Pts',(3.27908868399994,15.2,10.298556666));
#218616=CARTESIAN_POINT('Ctrl Pts',(3.28060974399994,15.2,10.300755834));
#218617=CARTESIAN_POINT('Ctrl Pts',(3.28213600999995,15.2,10.302958542));
#218618=CARTESIAN_POINT('Ctrl Pts',(3.28366748099994,15.2,10.305164779));
#218619=CARTESIAN_POINT('Ctrl Pts',(3.28520415899995,15.2,10.307374529));
#218620=CARTESIAN_POINT('Ctrl Pts',(3.28674604399994,15.2,10.30958778));
#218621=CARTESIAN_POINT('Ctrl Pts',(3.28829313699994,15.2,10.311804518));
#218622=CARTESIAN_POINT('Ctrl Pts',(3.28984543999994,15.2,10.314024727));
#218623=CARTESIAN_POINT('Ctrl Pts',(3.29140295199994,15.2,10.316248395));
#218624=CARTESIAN_POINT('Ctrl Pts',(3.29296567499994,15.2,10.318475509));
#218625=CARTESIAN_POINT('Ctrl Pts',(3.29453360899994,15.2,10.320706052));
#218626=CARTESIAN_POINT('Ctrl Pts',(3.29610675499994,15.2,10.322940014));
#218627=CARTESIAN_POINT('Ctrl Pts',(3.29768511299994,15.2,10.325177379));
#218628=CARTESIAN_POINT('Ctrl Pts',(3.29926868599994,15.2,10.327418135));
#218629=CARTESIAN_POINT('Ctrl Pts',(3.30085747199994,15.2,10.329662268));
#218630=CARTESIAN_POINT('Ctrl Pts',(3.30245147199994,15.2,10.331909762));
#218631=CARTESIAN_POINT('Ctrl Pts',(3.30405068899994,15.2,10.334160606));
#218632=CARTESIAN_POINT('Ctrl Pts',(3.30565512199994,15.2,10.336414786));
#218633=CARTESIAN_POINT('Ctrl Pts',(3.30726477099994,15.2,10.33867229));
#218634=CARTESIAN_POINT('Ctrl Pts',(3.30920261270556,15.2,10.3413852645478));
#218635=CARTESIAN_POINT('Ctrl Pts',(3.3111482782355,15.2,10.3441031813495));
#218636=CARTESIAN_POINT('Ctrl Pts',(3.31310177376438,15.2,10.3468260146505));
#218637=CARTESIAN_POINT('Ctrl Pts',(3.31506309947107,15.2,10.349553738699));
#218638=CARTESIAN_POINT('Ctrl Pts',(3.31703225499994,15.2,10.352286327));
#218639=CARTESIAN_POINT('Ctrl Pts',(3.31867843899994,15.2,10.354566712));
#218640=CARTESIAN_POINT('Ctrl Pts',(3.32032984499994,15.2,10.356850313));
#218641=CARTESIAN_POINT('Ctrl Pts',(3.32198647199994,15.2,10.359137117));
#218642=CARTESIAN_POINT('Ctrl Pts',(3.32364832199994,15.2,10.36142711));
#218643=CARTESIAN_POINT('Ctrl Pts',(3.32531539599994,15.2,10.36372028));
#218644=CARTESIAN_POINT('Ctrl Pts',(3.32698769299994,15.2,10.366016614));
#218645=CARTESIAN_POINT('Ctrl Pts',(3.32866521499994,15.2,10.368316097));
#218646=CARTESIAN_POINT('Ctrl Pts',(3.33034796099994,15.2,10.370618718));
#218647=CARTESIAN_POINT('Ctrl Pts',(3.33203593199995,15.2,10.372924463));
#218648=CARTESIAN_POINT('Ctrl Pts',(3.33372912899994,15.2,10.375233319));
#218649=CARTESIAN_POINT('Ctrl Pts',(3.33542755199994,15.2,10.377545274));
#218650=CARTESIAN_POINT('Ctrl Pts',(3.33713120199994,15.2,10.379860313));
#218651=CARTESIAN_POINT('Ctrl Pts',(3.33884007799994,15.2,10.382178427));
#218652=CARTESIAN_POINT('Ctrl Pts',(3.34055418199994,15.2,10.384499599));
#218653=CARTESIAN_POINT('Ctrl Pts',(3.34227351299994,15.2,10.386823818));
#218654=CARTESIAN_POINT('Ctrl Pts',(3.34399807299994,15.2,10.389151072));
#218655=CARTESIAN_POINT('Ctrl Pts',(3.34572786099995,15.2,10.391481347));
#218656=CARTESIAN_POINT('Ctrl Pts',(3.34746287999995,15.2,10.393814631));
#218657=CARTESIAN_POINT('Ctrl Pts',(3.34920312499994,15.2,10.396150911));
#218658=CARTESIAN_POINT('Ctrl Pts',(3.35094860199994,15.2,10.398490174));
#218659=CARTESIAN_POINT('Ctrl Pts',(3.35269930899994,15.2,10.400832408));
#218660=CARTESIAN_POINT('Ctrl Pts',(3.35445524599994,15.2,10.4031776));
#218661=CARTESIAN_POINT('Ctrl Pts',(3.35621641399994,15.2,10.405525737));
#218662=CARTESIAN_POINT('Ctrl Pts',(3.35798281299994,15.2,10.407876808));
#218663=CARTESIAN_POINT('Ctrl Pts',(3.35975444299994,15.2,10.410230799));
#218664=CARTESIAN_POINT('Ctrl Pts',(3.36153130499994,15.2,10.412587698));
#218665=CARTESIAN_POINT('Ctrl Pts',(3.36331339899994,15.2,10.414947493));
#218666=CARTESIAN_POINT('Ctrl Pts',(3.36510072599994,15.2,10.417310171));
#218667=CARTESIAN_POINT('Ctrl Pts',(3.36689328399994,15.2,10.419675719));
#218668=CARTESIAN_POINT('Ctrl Pts',(3.36869107699994,15.2,10.422044126));
#218669=CARTESIAN_POINT('Ctrl Pts',(3.37049410099994,15.2,10.424415378));
#218670=CARTESIAN_POINT('Ctrl Pts',(3.37230235899994,15.2,10.426789465));
#218671=CARTESIAN_POINT('Ctrl Pts',(3.37411584999994,15.2,10.429166374));
#218672=CARTESIAN_POINT('Ctrl Pts',(3.37593457599994,15.2,10.43154609));
#218673=CARTESIAN_POINT('Ctrl Pts',(3.37775853499994,15.2,10.433928604));
#218674=CARTESIAN_POINT('Ctrl Pts',(3.37958772799994,15.2,10.436313903));
#218675=CARTESIAN_POINT('Ctrl Pts',(3.38142215599994,15.2,10.438701973));
#218676=CARTESIAN_POINT('Ctrl Pts',(3.38326181899995,15.2,10.441092806));
#218677=CARTESIAN_POINT('Ctrl Pts',(3.38510671499994,15.2,10.443486385));
#218678=CARTESIAN_POINT('Ctrl Pts',(3.38695684699994,15.2,10.445882701));
#218679=CARTESIAN_POINT('Ctrl Pts',(3.38881221399994,15.2,10.448281741));
#218680=CARTESIAN_POINT('Ctrl Pts',(3.39067281599994,15.2,10.450683492));
#218681=CARTESIAN_POINT('Ctrl Pts',(3.39253865299994,15.2,10.453087944));
#218682=CARTESIAN_POINT('Ctrl Pts',(3.39440972599995,15.2,10.455495084));
#218683=CARTESIAN_POINT('Ctrl Pts',(3.39628603499994,15.2,10.4579049));
#218684=CARTESIAN_POINT('Ctrl Pts',(3.39816757899994,15.2,10.460317381));
#218685=CARTESIAN_POINT('Ctrl Pts',(3.40005435899994,15.2,10.462732513));
#218686=CARTESIAN_POINT('Ctrl Pts',(3.40194637399994,15.2,10.465150286));
#218687=CARTESIAN_POINT('Ctrl Pts',(3.40384362599994,15.2,10.467570687));
#218688=CARTESIAN_POINT('Ctrl Pts',(3.40574611299994,15.2,10.469993704));
#218689=CARTESIAN_POINT('Ctrl Pts',(3.40765383599994,15.2,10.472419326));
#218690=CARTESIAN_POINT('Ctrl Pts',(3.40956679599994,15.2,10.474847543));
#218691=CARTESIAN_POINT('Ctrl Pts',(3.41148499199994,15.2,10.477278339));
#218692=CARTESIAN_POINT('Ctrl Pts',(3.41340842399994,15.2,10.479711706));
#218693=CARTESIAN_POINT('Ctrl Pts',(3.41533709199994,15.2,10.482147629));
#218694=CARTESIAN_POINT('Ctrl Pts',(3.41727099499994,15.2,10.4845861));
#218695=CARTESIAN_POINT('Ctrl Pts',(3.41921013599995,15.2,10.487027105));
#218696=CARTESIAN_POINT('Ctrl Pts',(3.42115451199994,15.2,10.489470632));
#218697=CARTESIAN_POINT('Ctrl Pts',(3.42310412599995,15.2,10.491916672));
#218698=CARTESIAN_POINT('Ctrl Pts',(3.42505897399994,15.2,10.49436521));
#218699=CARTESIAN_POINT('Ctrl Pts',(3.42701905899994,15.2,10.496816237));
#218700=CARTESIAN_POINT('Ctrl Pts',(3.42898437999994,15.2,10.49926974));
#218701=CARTESIAN_POINT('Ctrl Pts',(3.43095493699995,15.2,10.501725709));
#218702=CARTESIAN_POINT('Ctrl Pts',(3.43293072999994,15.2,10.504184131));
#218703=CARTESIAN_POINT('Ctrl Pts',(3.43491175999994,15.2,10.506644995));
#218704=CARTESIAN_POINT('Ctrl Pts',(3.43689802499994,15.2,10.50910829));
#218705=CARTESIAN_POINT('Ctrl Pts',(3.43888952499994,15.2,10.511574004));
#218706=CARTESIAN_POINT('Ctrl Pts',(3.44088626199994,15.2,10.514042126));
#218707=CARTESIAN_POINT('Ctrl Pts',(3.44288823299994,15.2,10.516512645));
#218708=CARTESIAN_POINT('Ctrl Pts',(3.44489543999994,15.2,10.51898555));
#218709=CARTESIAN_POINT('Ctrl Pts',(3.44690788299994,15.2,10.521460827));
#218710=CARTESIAN_POINT('Ctrl Pts',(3.44892555999994,15.2,10.523938468));
#218711=CARTESIAN_POINT('Ctrl Pts',(3.45094847299994,15.2,10.526418461));
#218712=CARTESIAN_POINT('Ctrl Pts',(3.45297662099994,15.2,10.528900792));
#218713=CARTESIAN_POINT('Ctrl Pts',(3.45501000299994,15.2,10.531385453));
#218714=CARTESIAN_POINT('Ctrl Pts',(3.45704861999995,15.2,10.533872432));
#218715=CARTESIAN_POINT('Ctrl Pts',(3.45909247099994,15.2,10.536361718));
#218716=CARTESIAN_POINT('Ctrl Pts',(3.46114155699994,15.2,10.538853298));
#218717=CARTESIAN_POINT('Ctrl Pts',(3.46319587599994,15.2,10.541347163));
#218718=CARTESIAN_POINT('Ctrl Pts',(3.46525542999994,15.2,10.543843302));
#218719=CARTESIAN_POINT('Ctrl Pts',(3.46732021699995,15.2,10.546341702));
#218720=CARTESIAN_POINT('Ctrl Pts',(3.46939023699994,15.2,10.548842353));
#218721=CARTESIAN_POINT('Ctrl Pts',(3.47146549099994,15.2,10.551345244));
#218722=CARTESIAN_POINT('Ctrl Pts',(3.47354597799994,15.2,10.553850365));
#218723=CARTESIAN_POINT('Ctrl Pts',(3.47563169699994,15.2,10.556357703));
#218724=CARTESIAN_POINT('Ctrl Pts',(3.47772264999994,15.2,10.558867249));
#218725=CARTESIAN_POINT('Ctrl Pts',(3.47981883399994,15.2,10.561378991));
#218726=CARTESIAN_POINT('Ctrl Pts',(3.48192024899994,15.2,10.563892917));
#218727=CARTESIAN_POINT('Ctrl Pts',(3.48402689799994,15.2,10.566409018));
#218728=CARTESIAN_POINT('Ctrl Pts',(3.48613877699994,15.2,10.568927282));
#218729=CARTESIAN_POINT('Ctrl Pts',(3.48825588699994,15.2,10.571447699));
#218730=CARTESIAN_POINT('Ctrl Pts',(3.49037822899994,15.2,10.573970259));
#218731=CARTESIAN_POINT('Ctrl Pts',(3.49250580099994,15.2,10.576494948));
#218732=CARTESIAN_POINT('Ctrl Pts',(3.49463860199994,15.2,10.579021758));
#218733=CARTESIAN_POINT('Ctrl Pts',(3.49677663399994,15.2,10.581550676));
#218734=CARTESIAN_POINT('Ctrl Pts',(3.49891989599994,15.2,10.584081694));
#218735=CARTESIAN_POINT('Ctrl Pts',(3.50106838699995,15.2,10.5866148));
#218736=CARTESIAN_POINT('Ctrl Pts',(3.50322210699994,15.2,10.589149983));
#218737=CARTESIAN_POINT('Ctrl Pts',(3.50538105499994,15.2,10.591687233));
#218738=CARTESIAN_POINT('Ctrl Pts',(3.50754523199994,15.2,10.594226538));
#218739=CARTESIAN_POINT('Ctrl Pts',(3.50971463599994,15.2,10.596767889));
#218740=CARTESIAN_POINT('Ctrl Pts',(3.51188926799994,15.2,10.599311274));
#218741=CARTESIAN_POINT('Ctrl Pts',(3.51406912699994,15.2,10.601856683));
#218742=CARTESIAN_POINT('Ctrl Pts',(3.51625421199994,15.2,10.604404106));
#218743=CARTESIAN_POINT('Ctrl Pts',(3.51844452399994,15.2,10.606953531));
#218744=CARTESIAN_POINT('Ctrl Pts',(3.52064006199994,15.2,10.609504948));
#218745=CARTESIAN_POINT('Ctrl Pts',(3.52284082599994,15.2,10.612058349));
#218746=CARTESIAN_POINT('Ctrl Pts',(3.52504681399994,15.2,10.61461372));
#218747=CARTESIAN_POINT('Ctrl Pts',(3.52725802799994,15.2,10.617171051));
#218748=CARTESIAN_POINT('Ctrl Pts',(3.52947446499994,15.2,10.619730334));
#218749=CARTESIAN_POINT('Ctrl Pts',(3.53169612599994,15.2,10.622291557));
#218750=CARTESIAN_POINT('Ctrl Pts',(3.53392300999994,15.2,10.624854709));
#218751=CARTESIAN_POINT('Ctrl Pts',(3.53615511699994,15.2,10.62741978));
#218752=CARTESIAN_POINT('Ctrl Pts',(3.53839244699994,15.2,10.62998676));
#218753=CARTESIAN_POINT('Ctrl Pts',(3.54063499799994,15.2,10.632555639));
#218754=CARTESIAN_POINT('Ctrl Pts',(3.54288277099994,15.2,10.635126406));
#218755=CARTESIAN_POINT('Ctrl Pts',(3.54513576499994,15.2,10.637699051));
#218756=CARTESIAN_POINT('Ctrl Pts',(3.54739397999994,15.2,10.640273563));
#218757=CARTESIAN_POINT('Ctrl Pts',(3.54965741499994,15.2,10.642849932));
#218758=CARTESIAN_POINT('Ctrl Pts',(3.55192606799994,15.2,10.645428149));
#218759=CARTESIAN_POINT('Ctrl Pts',(3.55419994099994,15.2,10.648008202));
#218760=CARTESIAN_POINT('Ctrl Pts',(3.55647903199994,15.2,10.650590083));
#218761=CARTESIAN_POINT('Ctrl Pts',(3.55876334099994,15.2,10.653173779));
#218762=CARTESIAN_POINT('Ctrl Pts',(3.56105286799994,15.2,10.655759282));
#218763=CARTESIAN_POINT('Ctrl Pts',(3.56334761099994,15.2,10.658346581));
#218764=CARTESIAN_POINT('Ctrl Pts',(3.56564757099994,15.2,10.660935667));
#218765=CARTESIAN_POINT('Ctrl Pts',(3.56795274699994,15.2,10.663526528));
#218766=CARTESIAN_POINT('Ctrl Pts',(3.57026313699994,15.2,10.666119155));
#218767=CARTESIAN_POINT('Ctrl Pts',(3.57257874199994,15.2,10.668713538));
#218768=CARTESIAN_POINT('Ctrl Pts',(3.57489956099994,15.2,10.671309666));
#218769=CARTESIAN_POINT('Ctrl Pts',(3.57722559299994,15.2,10.673907531));
#218770=CARTESIAN_POINT('Ctrl Pts',(3.57955683799994,15.2,10.67650712));
#218771=CARTESIAN_POINT('Ctrl Pts',(3.58189329599994,15.2,10.679108425));
#218772=CARTESIAN_POINT('Ctrl Pts',(3.58423496399995,15.2,10.681711437));
#218773=CARTESIAN_POINT('Ctrl Pts',(3.58658184499994,15.2,10.684316143));
#218774=CARTESIAN_POINT('Ctrl Pts',(3.58893393499994,15.2,10.686922536));
#218775=CARTESIAN_POINT('Ctrl Pts',(3.59129123599994,15.2,10.689530605));
#218776=CARTESIAN_POINT('Ctrl Pts',(3.59365374499994,15.2,10.692140339));
#218777=CARTESIAN_POINT('Ctrl Pts',(3.59602146199994,15.2,10.694751731));
#218778=CARTESIAN_POINT('Ctrl Pts',(3.59839438799994,15.2,10.697364767));
#218779=CARTESIAN_POINT('Ctrl Pts',(3.60077251999994,15.2,10.699979441));
#218780=CARTESIAN_POINT('Ctrl Pts',(3.60315585899994,15.2,10.702595741));
#218781=CARTESIAN_POINT('Ctrl Pts',(3.60554440399994,15.2,10.705213657));
#218782=CARTESIAN_POINT('Ctrl Pts',(3.60793815399994,15.2,10.707833181));
#218783=CARTESIAN_POINT('Ctrl Pts',(3.61033710899994,15.2,10.710454302));
#218784=CARTESIAN_POINT('Ctrl Pts',(3.61274126699994,15.2,10.71307701));
#218785=CARTESIAN_POINT('Ctrl Pts',(3.61515062899994,15.2,10.715701296));
#218786=CARTESIAN_POINT('Ctrl Pts',(3.61756519199994,15.2,10.718327151));
#218787=CARTESIAN_POINT('Ctrl Pts',(3.61998495799994,15.2,10.720954563));
#218788=CARTESIAN_POINT('Ctrl Pts',(3.62240992399994,15.2,10.723583524));
#218789=CARTESIAN_POINT('Ctrl Pts',(3.62484009099994,15.2,10.726214025));
#218790=CARTESIAN_POINT('Ctrl Pts',(3.62727545699994,15.2,10.728846054));
#218791=CARTESIAN_POINT('Ctrl Pts',(3.62971602199994,15.2,10.731479602));
#218792=CARTESIAN_POINT('Ctrl Pts',(3.63216178499994,15.2,10.734114662));
#218793=CARTESIAN_POINT('Ctrl Pts',(3.63461274499994,15.2,10.736751222));
#218794=CARTESIAN_POINT('Ctrl Pts',(3.63706890199994,15.2,10.739389272));
#218795=CARTESIAN_POINT('Ctrl Pts',(3.63953025499994,15.2,10.742028805));
#218796=CARTESIAN_POINT('Ctrl Pts',(3.64199680199994,15.2,10.744669808));
#218797=CARTESIAN_POINT('Ctrl Pts',(3.64446854399994,15.2,10.747312275));
#218798=CARTESIAN_POINT('Ctrl Pts',(3.64694547899994,15.2,10.749956194));
#218799=CARTESIAN_POINT('Ctrl Pts',(3.64942760599994,15.2,10.752601556));
#218800=CARTESIAN_POINT('Ctrl Pts',(3.65191492599994,15.2,10.755248353));
#218801=CARTESIAN_POINT('Ctrl Pts',(3.65440743699994,15.2,10.757896573));
#218802=CARTESIAN_POINT('Ctrl Pts',(3.65690513699994,15.2,10.760546208));
#218803=CARTESIAN_POINT('Ctrl Pts',(3.65940802899994,15.2,10.76319725));
#218804=CARTESIAN_POINT('Ctrl Pts',(3.66191610699994,15.2,10.765849687));
#218805=CARTESIAN_POINT('Ctrl Pts',(3.66442937399994,15.2,10.768503511));
#218806=CARTESIAN_POINT('Ctrl Pts',(3.66694782699994,15.2,10.771158713));
#218807=CARTESIAN_POINT('Ctrl Pts',(3.66947146699994,15.2,10.773815282));
#218808=CARTESIAN_POINT('Ctrl Pts',(3.67200029299994,15.2,10.776473211));
#218809=CARTESIAN_POINT('Ctrl Pts',(3.67453430199994,15.2,10.77913249));
#218810=CARTESIAN_POINT('Ctrl Pts',(3.67707349599994,15.2,10.781793108));
#218811=CARTESIAN_POINT('Ctrl Pts',(3.67961787099994,15.2,10.784455057));
#218812=CARTESIAN_POINT('Ctrl Pts',(3.68216742899994,15.2,10.787118327));
#218813=CARTESIAN_POINT('Ctrl Pts',(3.68472216799994,15.2,10.789782909));
#218814=CARTESIAN_POINT('Ctrl Pts',(3.68728208699994,15.2,10.792448794));
#218815=CARTESIAN_POINT('Ctrl Pts',(3.68984718499994,15.2,10.795115974));
#218816=CARTESIAN_POINT('Ctrl Pts',(3.69241746099994,15.2,10.797784438));
#218817=CARTESIAN_POINT('Ctrl Pts',(3.69499291499995,15.2,10.800454179));
#218818=CARTESIAN_POINT('Ctrl Pts',(3.69757354499994,15.2,10.803125184));
#218819=CARTESIAN_POINT('Ctrl Pts',(3.70015935099994,15.2,10.805797449));
#218820=CARTESIAN_POINT('Ctrl Pts',(3.70275033099994,15.2,10.808470961));
#218821=CARTESIAN_POINT('Ctrl Pts',(3.70534648499994,15.2,10.811145713));
#218822=CARTESIAN_POINT('Ctrl Pts',(3.70794781299994,15.2,10.813821695));
#218823=CARTESIAN_POINT('Ctrl Pts',(3.71055431199994,15.2,10.816498895));
#218824=CARTESIAN_POINT('Ctrl Pts',(3.71316598199994,15.2,10.819177306));
#218825=CARTESIAN_POINT('Ctrl Pts',(3.71578282099994,15.2,10.821856919));
#218826=CARTESIAN_POINT('Ctrl Pts',(3.71840482999994,15.2,10.824537725));
#218827=CARTESIAN_POINT('Ctrl Pts',(3.72103200699994,15.2,10.827219716));
#218828=CARTESIAN_POINT('Ctrl Pts',(3.72366435199994,15.2,10.829902884));
#218829=CARTESIAN_POINT('Ctrl Pts',(3.72630186199994,15.2,10.832587221));
#218830=CARTESIAN_POINT('Ctrl Pts',(3.72894453699994,15.2,10.835272717));
#218831=CARTESIAN_POINT('Ctrl Pts',(3.73159237799995,15.2,10.837959365));
#218832=CARTESIAN_POINT('Ctrl Pts',(3.73424538199994,15.2,10.840647153));
#218833=CARTESIAN_POINT('Ctrl Pts',(3.73690354699994,15.2,10.843336071));
#218834=CARTESIAN_POINT('Ctrl Pts',(3.73956687399994,15.2,10.846026106));
#218835=CARTESIAN_POINT('Ctrl Pts',(3.74223535999994,15.2,10.84871725));
#218836=CARTESIAN_POINT('Ctrl Pts',(3.74490900499994,15.2,10.85140949));
#218837=CARTESIAN_POINT('Ctrl Pts',(3.74758780799994,15.2,10.854102822));
#218838=CARTESIAN_POINT('Ctrl Pts',(3.75027176799994,15.2,10.856797236));
#218839=CARTESIAN_POINT('Ctrl Pts',(3.75296088399994,15.2,10.85949273));
#218840=CARTESIAN_POINT('Ctrl Pts',(3.75565515599994,15.2,10.862189302));
#218841=CARTESIAN_POINT('Ctrl Pts',(3.75781469799994,15.2,10.864347421));
#218842=CARTESIAN_POINT('Ctrl Pts',(3.75943667399994,15.2,10.865966495));
#218843=CARTESIAN_POINT('Ctrl Pts',(3.76051902299994,15.2,10.867046091));
#218844=CARTESIAN_POINT('Ctrl Pts',(3.76106045499994,15.2,10.867585944));
#218845=CARTESIAN_POINT('Ctrl Pts',(4.04260911699994,15.2,9.55499537099998));
#218846=CARTESIAN_POINT('Ctrl Pts',(4.04260911699994,11.6,9.55499537099998));
#218847=CARTESIAN_POINT('Ctrl Pts',(4.04266300399994,15.2,9.55516119299999));
#218848=CARTESIAN_POINT('Ctrl Pts',(4.04266300399994,11.6,9.55516119299999));
#218849=CARTESIAN_POINT('Ctrl Pts',(4.04277257899994,15.2,9.55549865399998));
#218850=CARTESIAN_POINT('Ctrl Pts',(4.04277257899994,11.6,9.55549865399998));
#218851=CARTESIAN_POINT('Ctrl Pts',(4.04293835799994,15.2,9.55601007199999));
#218852=CARTESIAN_POINT('Ctrl Pts',(4.04293835799994,11.6,9.55601007199999));
#218853=CARTESIAN_POINT('Ctrl Pts',(4.04316116499994,15.2,9.55669916199999));
#218854=CARTESIAN_POINT('Ctrl Pts',(4.04316116499994,11.6,9.55669916199999));
#218855=CARTESIAN_POINT('Ctrl Pts',(4.04344211299995,15.2,9.55757104199999));
#218856=CARTESIAN_POINT('Ctrl Pts',(4.04344211299995,11.6,9.55757104199999));
#218857=CARTESIAN_POINT('Ctrl Pts',(4.04372672499994,15.2,9.55845733799999));
#218858=CARTESIAN_POINT('Ctrl Pts',(4.04372672499994,11.6,9.55845733799999));
#218859=CARTESIAN_POINT('Ctrl Pts',(4.04401334799994,15.2,9.55935298199999));
#218860=CARTESIAN_POINT('Ctrl Pts',(4.04401334799994,11.6,9.55935298199999));
#218861=CARTESIAN_POINT('Ctrl Pts',(4.04430195599994,15.2,9.56025795199999));
#218862=CARTESIAN_POINT('Ctrl Pts',(4.04430195599994,11.6,9.56025795199999));
#218863=CARTESIAN_POINT('Ctrl Pts',(4.04459252299994,15.2,9.56117222799998));
#218864=CARTESIAN_POINT('Ctrl Pts',(4.04459252299994,11.6,9.56117222799998));
#218865=CARTESIAN_POINT('Ctrl Pts',(4.04488502599994,15.2,9.56209579099998));
#218866=CARTESIAN_POINT('Ctrl Pts',(4.04488502599994,11.6,9.56209579099998));
#218867=CARTESIAN_POINT('Ctrl Pts',(4.04517943799994,15.2,9.56302861999998));
#218868=CARTESIAN_POINT('Ctrl Pts',(4.04517943799994,11.6,9.56302861999998));
#218869=CARTESIAN_POINT('Ctrl Pts',(4.04547573399994,15.2,9.56397069599999));
#218870=CARTESIAN_POINT('Ctrl Pts',(4.04547573399994,11.6,9.56397069599999));
#218871=CARTESIAN_POINT('Ctrl Pts',(4.04577388999994,15.2,9.56492199899999));
#218872=CARTESIAN_POINT('Ctrl Pts',(4.04577388999994,11.6,9.56492199899999));
#218873=CARTESIAN_POINT('Ctrl Pts',(4.04607388099994,15.2,9.56588250899999));
#218874=CARTESIAN_POINT('Ctrl Pts',(4.04607388099994,11.6,9.56588250899999));
#218875=CARTESIAN_POINT('Ctrl Pts',(4.04637568199994,15.2,9.56685220699999));
#218876=CARTESIAN_POINT('Ctrl Pts',(4.04637568199994,11.6,9.56685220699999));
#218877=CARTESIAN_POINT('Ctrl Pts',(4.04667926799995,15.2,9.56783107399998));
#218878=CARTESIAN_POINT('Ctrl Pts',(4.04667926799995,11.6,9.56783107399998));
#218879=CARTESIAN_POINT('Ctrl Pts',(4.04698461699994,15.2,9.56881908899998));
#218880=CARTESIAN_POINT('Ctrl Pts',(4.04698461699994,11.6,9.56881908899998));
#218881=CARTESIAN_POINT('Ctrl Pts',(4.04729170299994,15.2,9.56981623299999));
#218882=CARTESIAN_POINT('Ctrl Pts',(4.04729170299994,11.6,9.56981623299999));
#218883=CARTESIAN_POINT('Ctrl Pts',(4.04760050099994,15.2,9.57082248799999));
#218884=CARTESIAN_POINT('Ctrl Pts',(4.04760050099994,11.6,9.57082248799999));
#218885=CARTESIAN_POINT('Ctrl Pts',(4.04791098999994,15.2,9.57183783399999));
#218886=CARTESIAN_POINT('Ctrl Pts',(4.04791098999994,11.6,9.57183783399999));
#218887=CARTESIAN_POINT('Ctrl Pts',(4.04822314399994,15.2,9.57286225199999));
#218888=CARTESIAN_POINT('Ctrl Pts',(4.04822314399994,11.6,9.57286225199999));
#218889=CARTESIAN_POINT('Ctrl Pts',(4.04853693799994,15.2,9.57389572199999));
#218890=CARTESIAN_POINT('Ctrl Pts',(4.04853693799994,11.6,9.57389572199999));
#218891=CARTESIAN_POINT('Ctrl Pts',(4.04885235199994,15.2,9.57493822799999));
#218892=CARTESIAN_POINT('Ctrl Pts',(4.04885235199994,11.6,9.57493822799999));
#218893=CARTESIAN_POINT('Ctrl Pts',(4.04916935999994,15.2,9.57598974799998));
#218894=CARTESIAN_POINT('Ctrl Pts',(4.04916935999994,11.6,9.57598974799998));
#218895=CARTESIAN_POINT('Ctrl Pts',(4.04948793899994,15.2,9.57705026599999));
#218896=CARTESIAN_POINT('Ctrl Pts',(4.04948793899994,11.6,9.57705026599999));
#218897=CARTESIAN_POINT('Ctrl Pts',(4.04980806699994,15.2,9.57811975999999));
#218898=CARTESIAN_POINT('Ctrl Pts',(4.04980806699994,11.6,9.57811975999999));
#218899=CARTESIAN_POINT('Ctrl Pts',(4.05012971799994,15.2,9.57919821499999));
#218900=CARTESIAN_POINT('Ctrl Pts',(4.05012971799994,11.6,9.57919821499999));
#218901=CARTESIAN_POINT('Ctrl Pts',(4.05045287199994,15.2,9.58028560899999));
#218902=CARTESIAN_POINT('Ctrl Pts',(4.05045287199994,11.6,9.58028560899999));
#218903=CARTESIAN_POINT('Ctrl Pts',(4.05077750499994,15.2,9.58138192699998));
#218904=CARTESIAN_POINT('Ctrl Pts',(4.05077750499994,11.6,9.58138192699998));
#218905=CARTESIAN_POINT('Ctrl Pts',(4.05110359499994,15.2,9.58248714699998));
#218906=CARTESIAN_POINT('Ctrl Pts',(4.05110359499994,11.6,9.58248714699998));
#218907=CARTESIAN_POINT('Ctrl Pts',(4.05143111699994,15.2,9.58360125399999));
#218908=CARTESIAN_POINT('Ctrl Pts',(4.05143111699994,11.6,9.58360125399999));
#218909=CARTESIAN_POINT('Ctrl Pts',(4.05176005199994,15.2,9.58472422799998));
#218910=CARTESIAN_POINT('Ctrl Pts',(4.05176005199994,11.6,9.58472422799998));
#218911=CARTESIAN_POINT('Ctrl Pts',(4.05209037399994,15.2,9.58585605099999));
#218912=CARTESIAN_POINT('Ctrl Pts',(4.05209037399994,11.6,9.58585605099999));
#218913=CARTESIAN_POINT('Ctrl Pts',(4.05242206299994,15.2,9.58699670499998));
#218914=CARTESIAN_POINT('Ctrl Pts',(4.05242206299994,11.6,9.58699670499998));
#218915=CARTESIAN_POINT('Ctrl Pts',(4.05275509599995,15.2,9.58814617299998));
#218916=CARTESIAN_POINT('Ctrl Pts',(4.05275509599995,11.6,9.58814617299998));
#218917=CARTESIAN_POINT('Ctrl Pts',(4.05308945099994,15.2,9.58930443499998));
#218918=CARTESIAN_POINT('Ctrl Pts',(4.05308945099994,11.6,9.58930443499998));
#218919=CARTESIAN_POINT('Ctrl Pts',(4.05342510599994,15.2,9.59047147499999));
#218920=CARTESIAN_POINT('Ctrl Pts',(4.05342510599994,11.6,9.59047147499999));
#218921=CARTESIAN_POINT('Ctrl Pts',(4.05376203899994,15.2,9.59164727399998));
#218922=CARTESIAN_POINT('Ctrl Pts',(4.05376203899994,11.6,9.59164727399998));
#218923=CARTESIAN_POINT('Ctrl Pts',(4.05410022799995,15.2,9.59283181599999));
#218924=CARTESIAN_POINT('Ctrl Pts',(4.05410022799995,11.6,9.59283181599999));
#218925=CARTESIAN_POINT('Ctrl Pts',(4.05443965299995,15.2,9.59402508099998));
#218926=CARTESIAN_POINT('Ctrl Pts',(4.05443965299995,11.6,9.59402508099998));
#218927=CARTESIAN_POINT('Ctrl Pts',(4.05478029099995,15.2,9.59522705199999));
#218928=CARTESIAN_POINT('Ctrl Pts',(4.05478029099995,11.6,9.59522705199999));
#218929=CARTESIAN_POINT('Ctrl Pts',(4.05512211899994,15.2,9.59643771299999));
#218930=CARTESIAN_POINT('Ctrl Pts',(4.05512211899994,11.6,9.59643771299999));
#218931=CARTESIAN_POINT('Ctrl Pts',(4.05546511799994,15.2,9.59765704599998));
#218932=CARTESIAN_POINT('Ctrl Pts',(4.05546511799994,11.6,9.59765704599998));
#218933=CARTESIAN_POINT('Ctrl Pts',(4.05580926699994,15.2,9.59888503199998));
#218934=CARTESIAN_POINT('Ctrl Pts',(4.05580926699994,11.6,9.59888503199998));
#218935=CARTESIAN_POINT('Ctrl Pts',(4.05615454399994,15.2,9.60012165499998));
#218936=CARTESIAN_POINT('Ctrl Pts',(4.05615454399994,11.6,9.60012165499998));
#218937=CARTESIAN_POINT('Ctrl Pts',(4.05650092699995,15.2,9.60136689799998));
#218938=CARTESIAN_POINT('Ctrl Pts',(4.05650092699995,11.6,9.60136689799998));
#218939=CARTESIAN_POINT('Ctrl Pts',(4.05684839499994,15.2,9.60262074399999));
#218940=CARTESIAN_POINT('Ctrl Pts',(4.05684839499994,11.6,9.60262074399999));
#218941=CARTESIAN_POINT('Ctrl Pts',(4.05719692999994,15.2,9.60388317399998));
#218942=CARTESIAN_POINT('Ctrl Pts',(4.05719692999994,11.6,9.60388317399998));
#218943=CARTESIAN_POINT('Ctrl Pts',(4.05754650899994,15.2,9.60515417299998));
#218944=CARTESIAN_POINT('Ctrl Pts',(4.05754650899994,11.6,9.60515417299998));
#218945=CARTESIAN_POINT('Ctrl Pts',(4.05789711099994,15.2,9.60643372199998));
#218946=CARTESIAN_POINT('Ctrl Pts',(4.05789711099994,11.6,9.60643372199998));
#218947=CARTESIAN_POINT('Ctrl Pts',(4.05824871699994,15.2,9.60772180699998));
#218948=CARTESIAN_POINT('Ctrl Pts',(4.05824871699994,11.6,9.60772180699998));
#218949=CARTESIAN_POINT('Ctrl Pts',(4.05860130599994,15.2,9.60901840899999));
#218950=CARTESIAN_POINT('Ctrl Pts',(4.05860130599994,11.6,9.60901840899999));
#218951=CARTESIAN_POINT('Ctrl Pts',(4.05895485599994,15.2,9.61032350999999));
#218952=CARTESIAN_POINT('Ctrl Pts',(4.05895485599994,11.6,9.61032350999999));
#218953=CARTESIAN_POINT('Ctrl Pts',(4.05930934899995,15.2,9.61163709599998));
#218954=CARTESIAN_POINT('Ctrl Pts',(4.05930934899995,11.6,9.61163709599998));
#218955=CARTESIAN_POINT('Ctrl Pts',(4.05966476299994,15.2,9.61295914899999));
#218956=CARTESIAN_POINT('Ctrl Pts',(4.05966476299994,11.6,9.61295914899999));
#218957=CARTESIAN_POINT('Ctrl Pts',(4.06002107999995,15.2,9.61428965199998));
#218958=CARTESIAN_POINT('Ctrl Pts',(4.06002107999995,11.6,9.61428965199998));
#218959=CARTESIAN_POINT('Ctrl Pts',(4.06037827899994,15.2,9.61562858999999));
#218960=CARTESIAN_POINT('Ctrl Pts',(4.06037827899994,11.6,9.61562858999999));
#218961=CARTESIAN_POINT('Ctrl Pts',(4.06073633899994,15.2,9.61697594399999));
#218962=CARTESIAN_POINT('Ctrl Pts',(4.06073633899994,11.6,9.61697594399999));
#218963=CARTESIAN_POINT('Ctrl Pts',(4.06109524299994,15.2,9.61833170099998));
#218964=CARTESIAN_POINT('Ctrl Pts',(4.06109524299994,11.6,9.61833170099998));
#218965=CARTESIAN_POINT('Ctrl Pts',(4.06145496899994,15.2,9.61969584099998));
#218966=CARTESIAN_POINT('Ctrl Pts',(4.06145496899994,11.6,9.61969584099998));
#218967=CARTESIAN_POINT('Ctrl Pts',(4.06181549599994,15.2,9.62106834999998));
#218968=CARTESIAN_POINT('Ctrl Pts',(4.06181549599994,11.6,9.62106834999998));
#218969=CARTESIAN_POINT('Ctrl Pts',(4.06217680899995,15.2,9.62244920999998));
#218970=CARTESIAN_POINT('Ctrl Pts',(4.06217680899995,11.6,9.62244920999998));
#218971=CARTESIAN_POINT('Ctrl Pts',(4.06253888499994,15.2,9.62383840699999));
#218972=CARTESIAN_POINT('Ctrl Pts',(4.06253888499994,11.6,9.62383840699999));
#218973=CARTESIAN_POINT('Ctrl Pts',(4.06290170499994,15.2,9.62523592299998));
#218974=CARTESIAN_POINT('Ctrl Pts',(4.06290170499994,11.6,9.62523592299998));
#218975=CARTESIAN_POINT('Ctrl Pts',(4.06326525199994,15.2,9.62664174299999));
#218976=CARTESIAN_POINT('Ctrl Pts',(4.06326525199994,11.6,9.62664174299999));
#218977=CARTESIAN_POINT('Ctrl Pts',(4.06362950399994,15.2,9.62805584999998));
#218978=CARTESIAN_POINT('Ctrl Pts',(4.06362950399994,11.6,9.62805584999998));
#218979=CARTESIAN_POINT('Ctrl Pts',(4.06399444399994,15.2,9.62947822899999));
#218980=CARTESIAN_POINT('Ctrl Pts',(4.06399444399994,11.6,9.62947822899999));
#218981=CARTESIAN_POINT('Ctrl Pts',(4.06436005099994,15.2,9.63090886299998));
#218982=CARTESIAN_POINT('Ctrl Pts',(4.06436005099994,11.6,9.63090886299998));
#218983=CARTESIAN_POINT('Ctrl Pts',(4.06472630999995,15.2,9.63234773599999));
#218984=CARTESIAN_POINT('Ctrl Pts',(4.06472630999995,11.6,9.63234773599999));
#218985=CARTESIAN_POINT('Ctrl Pts',(4.06509319699994,15.2,9.63379483399999));
#218986=CARTESIAN_POINT('Ctrl Pts',(4.06509319699994,11.6,9.63379483399999));
#218987=CARTESIAN_POINT('Ctrl Pts',(4.06546069699994,15.2,9.63525013999998));
#218988=CARTESIAN_POINT('Ctrl Pts',(4.06546069699994,11.6,9.63525013999998));
#218989=CARTESIAN_POINT('Ctrl Pts',(4.06582878999994,15.2,9.63671363799998));
#218990=CARTESIAN_POINT('Ctrl Pts',(4.06582878999994,11.6,9.63671363799998));
#218991=CARTESIAN_POINT('Ctrl Pts',(4.06619745799994,15.2,9.63818531199998));
#218992=CARTESIAN_POINT('Ctrl Pts',(4.06619745799994,11.6,9.63818531199998));
#218993=CARTESIAN_POINT('Ctrl Pts',(4.06656668099994,15.2,9.63966514799999));
#218994=CARTESIAN_POINT('Ctrl Pts',(4.06656668099994,11.6,9.63966514799999));
#218995=CARTESIAN_POINT('Ctrl Pts',(4.06693644299994,15.2,9.64115312899999));
#218996=CARTESIAN_POINT('Ctrl Pts',(4.06693644299994,11.6,9.64115312899999));
#218997=CARTESIAN_POINT('Ctrl Pts',(4.06730672399994,15.2,9.64264924199998));
#218998=CARTESIAN_POINT('Ctrl Pts',(4.06730672399994,11.6,9.64264924199998));
#218999=CARTESIAN_POINT('Ctrl Pts',(4.06767750699994,15.2,9.64415346799999));
#219000=CARTESIAN_POINT('Ctrl Pts',(4.06767750699994,11.6,9.64415346799999));
#219001=CARTESIAN_POINT('Ctrl Pts',(4.06804877199994,15.2,9.64566579199998));
#219002=CARTESIAN_POINT('Ctrl Pts',(4.06804877199994,11.6,9.64566579199998));
#219003=CARTESIAN_POINT('Ctrl Pts',(4.06842050299994,15.2,9.64718620099998));
#219004=CARTESIAN_POINT('Ctrl Pts',(4.06842050299994,11.6,9.64718620099998));
#219005=CARTESIAN_POINT('Ctrl Pts',(4.06879268099994,15.2,9.64871467899999));
#219006=CARTESIAN_POINT('Ctrl Pts',(4.06879268099994,11.6,9.64871467899999));
#219007=CARTESIAN_POINT('Ctrl Pts',(4.06916528699994,15.2,9.65025120999999));
#219008=CARTESIAN_POINT('Ctrl Pts',(4.06916528699994,11.6,9.65025120999999));
#219009=CARTESIAN_POINT('Ctrl Pts',(4.06953830599995,15.2,9.65179577899999));
#219010=CARTESIAN_POINT('Ctrl Pts',(4.06953830599995,11.6,9.65179577899999));
#219011=CARTESIAN_POINT('Ctrl Pts',(4.06991171799994,15.2,9.65334837099999));
#219012=CARTESIAN_POINT('Ctrl Pts',(4.06991171799994,11.6,9.65334837099999));
#219013=CARTESIAN_POINT('Ctrl Pts',(4.07028550499995,15.2,9.65490897099999));
#219014=CARTESIAN_POINT('Ctrl Pts',(4.07028550499995,11.6,9.65490897099999));
#219015=CARTESIAN_POINT('Ctrl Pts',(4.07065965199994,15.2,9.65647756299998));
#219016=CARTESIAN_POINT('Ctrl Pts',(4.07065965199994,11.6,9.65647756299998));
#219017=CARTESIAN_POINT('Ctrl Pts',(4.07103413799994,15.2,9.65805413399998));
#219018=CARTESIAN_POINT('Ctrl Pts',(4.07103413799994,11.6,9.65805413399998));
#219019=CARTESIAN_POINT('Ctrl Pts',(4.07140894899995,15.2,9.65963866699998));
#219020=CARTESIAN_POINT('Ctrl Pts',(4.07140894899995,11.6,9.65963866699998));
#219021=CARTESIAN_POINT('Ctrl Pts',(4.07178406499995,15.2,9.66123114899998));
#219022=CARTESIAN_POINT('Ctrl Pts',(4.07178406499995,11.6,9.66123114899998));
#219023=CARTESIAN_POINT('Ctrl Pts',(4.07215946999994,15.2,9.66283156199999));
#219024=CARTESIAN_POINT('Ctrl Pts',(4.07215946999994,11.6,9.66283156199999));
#219025=CARTESIAN_POINT('Ctrl Pts',(4.07253514699994,15.2,9.66443989599998));
#219026=CARTESIAN_POINT('Ctrl Pts',(4.07253514699994,11.6,9.66443989599998));
#219027=CARTESIAN_POINT('Ctrl Pts',(4.07291107799994,15.2,9.66605613199999));
#219028=CARTESIAN_POINT('Ctrl Pts',(4.07291107799994,11.6,9.66605613199999));
#219029=CARTESIAN_POINT('Ctrl Pts',(4.07328724699994,15.2,9.66768025699999));
#219030=CARTESIAN_POINT('Ctrl Pts',(4.07328724699994,11.6,9.66768025699999));
#219031=CARTESIAN_POINT('Ctrl Pts',(4.07366363499994,15.2,9.66931225599998));
#219032=CARTESIAN_POINT('Ctrl Pts',(4.07366363499994,11.6,9.66931225599998));
#219033=CARTESIAN_POINT('Ctrl Pts',(4.07404022799995,15.2,9.67095211499998));
#219034=CARTESIAN_POINT('Ctrl Pts',(4.07404022799995,11.6,9.67095211499998));
#219035=CARTESIAN_POINT('Ctrl Pts',(4.07441700599994,15.2,9.67259981799998));
#219036=CARTESIAN_POINT('Ctrl Pts',(4.07441700599994,11.6,9.67259981799998));
#219037=CARTESIAN_POINT('Ctrl Pts',(4.07479395499994,15.2,9.67425535199999));
#219038=CARTESIAN_POINT('Ctrl Pts',(4.07479395499994,11.6,9.67425535199999));
#219039=CARTESIAN_POINT('Ctrl Pts',(4.07517105699994,15.2,9.67591870199998));
#219040=CARTESIAN_POINT('Ctrl Pts',(4.07517105699994,11.6,9.67591870199998));
#219041=CARTESIAN_POINT('Ctrl Pts',(4.07554829499994,15.2,9.67758985299999));
#219042=CARTESIAN_POINT('Ctrl Pts',(4.07554829499994,11.6,9.67758985299999));
#219043=CARTESIAN_POINT('Ctrl Pts',(4.07592565399994,15.2,9.67926879099998));
#219044=CARTESIAN_POINT('Ctrl Pts',(4.07592565399994,11.6,9.67926879099998));
#219045=CARTESIAN_POINT('Ctrl Pts',(4.07630311499994,15.2,9.68095550299999));
#219046=CARTESIAN_POINT('Ctrl Pts',(4.07630311499994,11.6,9.68095550299999));
#219047=CARTESIAN_POINT('Ctrl Pts',(4.07668066299994,15.2,9.68264997199999));
#219048=CARTESIAN_POINT('Ctrl Pts',(4.07668066299994,11.6,9.68264997199999));
#219049=CARTESIAN_POINT('Ctrl Pts',(4.07705828299994,15.2,9.68435218599998));
#219050=CARTESIAN_POINT('Ctrl Pts',(4.07705828299994,11.6,9.68435218599998));
#219051=CARTESIAN_POINT('Ctrl Pts',(4.07743595699994,15.2,9.68606212899999));
#219052=CARTESIAN_POINT('Ctrl Pts',(4.07743595699994,11.6,9.68606212899999));
#219053=CARTESIAN_POINT('Ctrl Pts',(4.07781366899994,15.2,9.68777978899999));
#219054=CARTESIAN_POINT('Ctrl Pts',(4.07781366899994,11.6,9.68777978899999));
#219055=CARTESIAN_POINT('Ctrl Pts',(4.07819140299994,15.2,9.68950514999998));
#219056=CARTESIAN_POINT('Ctrl Pts',(4.07819140299994,11.6,9.68950514999998));
#219057=CARTESIAN_POINT('Ctrl Pts',(4.07856914299995,15.2,9.69123819799999));
#219058=CARTESIAN_POINT('Ctrl Pts',(4.07856914299995,11.6,9.69123819799999));
#219059=CARTESIAN_POINT('Ctrl Pts',(4.07894687299994,15.2,9.69297891999998));
#219060=CARTESIAN_POINT('Ctrl Pts',(4.07894687299994,11.6,9.69297891999998));
#219061=CARTESIAN_POINT('Ctrl Pts',(4.07932457699994,15.2,9.69472730199998));
#219062=CARTESIAN_POINT('Ctrl Pts',(4.07932457699994,11.6,9.69472730199998));
#219063=CARTESIAN_POINT('Ctrl Pts',(4.07970223899994,15.2,9.69648332799999));
#219064=CARTESIAN_POINT('Ctrl Pts',(4.07970223899994,11.6,9.69648332799999));
#219065=CARTESIAN_POINT('Ctrl Pts',(4.08007984399995,15.2,9.69824698699998));
#219066=CARTESIAN_POINT('Ctrl Pts',(4.08007984399995,11.6,9.69824698699998));
#219067=CARTESIAN_POINT('Ctrl Pts',(4.08045737499994,15.2,9.70001826299999));
#219068=CARTESIAN_POINT('Ctrl Pts',(4.08045737499994,11.6,9.70001826299999));
#219069=CARTESIAN_POINT('Ctrl Pts',(4.08083481699994,15.2,9.70179714299999));
#219070=CARTESIAN_POINT('Ctrl Pts',(4.08083481699994,11.6,9.70179714299999));
#219071=CARTESIAN_POINT('Ctrl Pts',(4.08121215399994,15.2,9.70358361299999));
#219072=CARTESIAN_POINT('Ctrl Pts',(4.08121215399994,11.6,9.70358361299999));
#219073=CARTESIAN_POINT('Ctrl Pts',(4.08158937099994,15.2,9.70537765899999));
#219074=CARTESIAN_POINT('Ctrl Pts',(4.08158937099994,11.6,9.70537765899999));
#219075=CARTESIAN_POINT('Ctrl Pts',(4.08196645199994,15.2,9.70717926799999));
#219076=CARTESIAN_POINT('Ctrl Pts',(4.08196645199994,11.6,9.70717926799999));
#219077=CARTESIAN_POINT('Ctrl Pts',(4.08234338299994,15.2,9.70898842499999));
#219078=CARTESIAN_POINT('Ctrl Pts',(4.08234338299994,11.6,9.70898842499999));
#219079=CARTESIAN_POINT('Ctrl Pts',(4.08272014699994,15.2,9.71080511799999));
#219080=CARTESIAN_POINT('Ctrl Pts',(4.08272014699994,11.6,9.71080511799999));
#219081=CARTESIAN_POINT('Ctrl Pts',(4.08309672799995,15.2,9.71262933199998));
#219082=CARTESIAN_POINT('Ctrl Pts',(4.08309672799995,11.6,9.71262933199998));
#219083=CARTESIAN_POINT('Ctrl Pts',(4.08347311299995,15.2,9.71446105499999));
#219084=CARTESIAN_POINT('Ctrl Pts',(4.08347311299995,11.6,9.71446105499999));
#219085=CARTESIAN_POINT('Ctrl Pts',(4.08384928499994,15.2,9.71630027099998));
#219086=CARTESIAN_POINT('Ctrl Pts',(4.08384928499994,11.6,9.71630027099998));
#219087=CARTESIAN_POINT('Ctrl Pts',(4.08422522999994,15.2,9.71814696999999));
#219088=CARTESIAN_POINT('Ctrl Pts',(4.08422522999994,11.6,9.71814696999999));
#219089=CARTESIAN_POINT('Ctrl Pts',(4.08460093299994,15.2,9.72000113399999));
#219090=CARTESIAN_POINT('Ctrl Pts',(4.08460093299994,11.6,9.72000113399999));
#219091=CARTESIAN_POINT('Ctrl Pts',(4.08497637899994,15.2,9.72186275399999));
#219092=CARTESIAN_POINT('Ctrl Pts',(4.08497637899994,11.6,9.72186275399999));
#219093=CARTESIAN_POINT('Ctrl Pts',(4.08535155199994,15.2,9.72373181399998));
#219094=CARTESIAN_POINT('Ctrl Pts',(4.08535155199994,11.6,9.72373181399998));
#219095=CARTESIAN_POINT('Ctrl Pts',(4.08572643699994,15.2,9.72560830099999));
#219096=CARTESIAN_POINT('Ctrl Pts',(4.08572643699994,11.6,9.72560830099999));
#219097=CARTESIAN_POINT('Ctrl Pts',(4.08610102099995,15.2,9.72749220299999));
#219098=CARTESIAN_POINT('Ctrl Pts',(4.08610102099995,11.6,9.72749220299999));
#219099=CARTESIAN_POINT('Ctrl Pts',(4.08647528899994,15.2,9.72938350599998));
#219100=CARTESIAN_POINT('Ctrl Pts',(4.08647528899994,11.6,9.72938350599998));
#219101=CARTESIAN_POINT('Ctrl Pts',(4.08684922499994,15.2,9.73128219599998));
#219102=CARTESIAN_POINT('Ctrl Pts',(4.08684922499994,11.6,9.73128219599998));
#219103=CARTESIAN_POINT('Ctrl Pts',(4.08722281399994,15.2,9.73318826099998));
#219104=CARTESIAN_POINT('Ctrl Pts',(4.08722281399994,11.6,9.73318826099998));
#219105=CARTESIAN_POINT('Ctrl Pts',(4.08759604299994,15.2,9.73510168599999));
#219106=CARTESIAN_POINT('Ctrl Pts',(4.08759604299994,11.6,9.73510168599999));
#219107=CARTESIAN_POINT('Ctrl Pts',(4.08796889599994,15.2,9.73702245899998));
#219108=CARTESIAN_POINT('Ctrl Pts',(4.08796889599994,11.6,9.73702245899998));
#219109=CARTESIAN_POINT('Ctrl Pts',(4.08834136099994,15.2,9.73895056799999));
#219110=CARTESIAN_POINT('Ctrl Pts',(4.08834136099994,11.6,9.73895056799999));
#219111=CARTESIAN_POINT('Ctrl Pts',(4.08871342099994,15.2,9.74088599899999));
#219112=CARTESIAN_POINT('Ctrl Pts',(4.08871342099994,11.6,9.74088599899999));
#219113=CARTESIAN_POINT('Ctrl Pts',(4.08908506299994,15.2,9.74282873799999));
#219114=CARTESIAN_POINT('Ctrl Pts',(4.08908506299994,11.6,9.74282873799999));
#219115=CARTESIAN_POINT('Ctrl Pts',(4.08945627199994,15.2,9.74477877499999));
#219116=CARTESIAN_POINT('Ctrl Pts',(4.08945627199994,11.6,9.74477877499999));
#219117=CARTESIAN_POINT('Ctrl Pts',(4.08982703399994,15.2,9.74673609299998));
#219118=CARTESIAN_POINT('Ctrl Pts',(4.08982703399994,11.6,9.74673609299998));
#219119=CARTESIAN_POINT('Ctrl Pts',(4.09019733499994,15.2,9.74870068099998));
#219120=CARTESIAN_POINT('Ctrl Pts',(4.09019733499994,11.6,9.74870068099998));
#219121=CARTESIAN_POINT('Ctrl Pts',(4.09056716099994,15.2,9.75067252799998));
#219122=CARTESIAN_POINT('Ctrl Pts',(4.09056716099994,11.6,9.75067252799998));
#219123=CARTESIAN_POINT('Ctrl Pts',(4.09093649799994,15.2,9.75265161799998));
#219124=CARTESIAN_POINT('Ctrl Pts',(4.09093649799994,11.6,9.75265161799998));
#219125=CARTESIAN_POINT('Ctrl Pts',(4.09130533199995,15.2,9.75463793999998));
#219126=CARTESIAN_POINT('Ctrl Pts',(4.09130533199995,11.6,9.75463793999998));
#219127=CARTESIAN_POINT('Ctrl Pts',(4.09167364799994,15.2,9.75663148099999));
#219128=CARTESIAN_POINT('Ctrl Pts',(4.09167364799994,11.6,9.75663148099999));
#219129=CARTESIAN_POINT('Ctrl Pts',(4.09204143299995,15.2,9.75863222699999));
#219130=CARTESIAN_POINT('Ctrl Pts',(4.09204143299995,11.6,9.75863222699999));
#219131=CARTESIAN_POINT('Ctrl Pts',(4.09240867299994,15.2,9.76064016799998));
#219132=CARTESIAN_POINT('Ctrl Pts',(4.09240867299994,11.6,9.76064016799998));
#219133=CARTESIAN_POINT('Ctrl Pts',(4.09277535499994,15.2,9.76265528899999));
#219134=CARTESIAN_POINT('Ctrl Pts',(4.09277535499994,11.6,9.76265528899999));
#219135=CARTESIAN_POINT('Ctrl Pts',(4.09314146399994,15.2,9.76467757799998));
#219136=CARTESIAN_POINT('Ctrl Pts',(4.09314146399994,11.6,9.76467757799998));
#219137=CARTESIAN_POINT('Ctrl Pts',(4.09350698699994,15.2,9.76670702199998));
#219138=CARTESIAN_POINT('Ctrl Pts',(4.09350698699994,11.6,9.76670702199998));
#219139=CARTESIAN_POINT('Ctrl Pts',(4.09387190999994,15.2,9.76874360899998));
#219140=CARTESIAN_POINT('Ctrl Pts',(4.09387190999994,11.6,9.76874360899998));
#219141=CARTESIAN_POINT('Ctrl Pts',(4.09423621899994,15.2,9.77078732699999));
#219142=CARTESIAN_POINT('Ctrl Pts',(4.09423621899994,11.6,9.77078732699999));
#219143=CARTESIAN_POINT('Ctrl Pts',(4.09459990199994,15.2,9.77283816299998));
#219144=CARTESIAN_POINT('Ctrl Pts',(4.09459990199994,11.6,9.77283816299998));
#219145=CARTESIAN_POINT('Ctrl Pts',(4.09496294399994,15.2,9.77489610299998));
#219146=CARTESIAN_POINT('Ctrl Pts',(4.09496294399994,11.6,9.77489610299998));
#219147=CARTESIAN_POINT('Ctrl Pts',(4.09532533299994,15.2,9.77696113599999));
#219148=CARTESIAN_POINT('Ctrl Pts',(4.09532533299994,11.6,9.77696113599999));
#219149=CARTESIAN_POINT('Ctrl Pts',(4.09568705399994,15.2,9.77903324999998));
#219150=CARTESIAN_POINT('Ctrl Pts',(4.09568705399994,11.6,9.77903324999998));
#219151=CARTESIAN_POINT('Ctrl Pts',(4.09604809499994,15.2,9.78111243199999));
#219152=CARTESIAN_POINT('Ctrl Pts',(4.09604809499994,11.6,9.78111243199999));
#219153=CARTESIAN_POINT('Ctrl Pts',(4.09640844199994,15.2,9.78319866999998));
#219154=CARTESIAN_POINT('Ctrl Pts',(4.09640844199994,11.6,9.78319866999998));
#219155=CARTESIAN_POINT('Ctrl Pts',(4.09676808199994,15.2,9.78529195099998));
#219156=CARTESIAN_POINT('Ctrl Pts',(4.09676808199994,11.6,9.78529195099998));
#219157=CARTESIAN_POINT('Ctrl Pts',(4.09712700199994,15.2,9.78739226399998));
#219158=CARTESIAN_POINT('Ctrl Pts',(4.09712700199994,11.6,9.78739226399998));
#219159=CARTESIAN_POINT('Ctrl Pts',(4.09748518799994,15.2,9.78949959399999));
#219160=CARTESIAN_POINT('Ctrl Pts',(4.09748518799994,11.6,9.78949959399999));
#219161=CARTESIAN_POINT('Ctrl Pts',(4.09784262799994,15.2,9.79161393199998));
#219162=CARTESIAN_POINT('Ctrl Pts',(4.09784262799994,11.6,9.79161393199998));
#219163=CARTESIAN_POINT('Ctrl Pts',(4.09819930899994,15.2,9.79373526399998));
#219164=CARTESIAN_POINT('Ctrl Pts',(4.09819930899994,11.6,9.79373526399998));
#219165=CARTESIAN_POINT('Ctrl Pts',(4.09855521699994,15.2,9.79586357899999));
#219166=CARTESIAN_POINT('Ctrl Pts',(4.09855521699994,11.6,9.79586357899999));
#219167=CARTESIAN_POINT('Ctrl Pts',(4.09891033999994,15.2,9.79799886199999));
#219168=CARTESIAN_POINT('Ctrl Pts',(4.09891033999994,11.6,9.79799886199999));
#219169=CARTESIAN_POINT('Ctrl Pts',(4.09926466499994,15.2,9.80014110499998));
#219170=CARTESIAN_POINT('Ctrl Pts',(4.09926466499994,11.6,9.80014110499998));
#219171=CARTESIAN_POINT('Ctrl Pts',(4.09961817899995,15.2,9.80229029299998));
#219172=CARTESIAN_POINT('Ctrl Pts',(4.09961817899995,11.6,9.80229029299998));
#219173=CARTESIAN_POINT('Ctrl Pts',(4.09997086899994,15.2,9.80444641499999));
#219174=CARTESIAN_POINT('Ctrl Pts',(4.09997086899994,11.6,9.80444641499999));
#219175=CARTESIAN_POINT('Ctrl Pts',(4.10032272299994,15.2,9.80660945799999));
#219176=CARTESIAN_POINT('Ctrl Pts',(4.10032272299994,11.6,9.80660945799999));
#219177=CARTESIAN_POINT('Ctrl Pts',(4.10067372699995,15.2,9.80877941199999));
#219178=CARTESIAN_POINT('Ctrl Pts',(4.10067372699995,11.6,9.80877941199999));
#219179=CARTESIAN_POINT('Ctrl Pts',(4.10102386899994,15.2,9.81095626399998));
#219180=CARTESIAN_POINT('Ctrl Pts',(4.10102386899994,11.6,9.81095626399998));
#219181=CARTESIAN_POINT('Ctrl Pts',(4.10137313699994,15.2,9.81314000099999));
#219182=CARTESIAN_POINT('Ctrl Pts',(4.10137313699994,11.6,9.81314000099999));
#219183=CARTESIAN_POINT('Ctrl Pts',(4.10172151799994,15.2,9.81533061199999));
#219184=CARTESIAN_POINT('Ctrl Pts',(4.10172151799994,11.6,9.81533061199999));
#219185=CARTESIAN_POINT('Ctrl Pts',(4.10206899999995,15.2,9.81752808499999));
#219186=CARTESIAN_POINT('Ctrl Pts',(4.10206899999995,11.6,9.81752808499999));
#219187=CARTESIAN_POINT('Ctrl Pts',(4.10241556999994,15.2,9.81973240899999));
#219188=CARTESIAN_POINT('Ctrl Pts',(4.10241556999994,11.6,9.81973240899999));
#219189=CARTESIAN_POINT('Ctrl Pts',(4.10276121599995,15.2,9.82194357099999));
#219190=CARTESIAN_POINT('Ctrl Pts',(4.10276121599995,11.6,9.82194357099999));
#219191=CARTESIAN_POINT('Ctrl Pts',(4.10310592399994,15.2,9.82416155899998));
#219192=CARTESIAN_POINT('Ctrl Pts',(4.10310592399994,11.6,9.82416155899998));
#219193=CARTESIAN_POINT('Ctrl Pts',(4.10344968399994,15.2,9.82638636299999));
#219194=CARTESIAN_POINT('Ctrl Pts',(4.10344968399994,11.6,9.82638636299999));
#219195=CARTESIAN_POINT('Ctrl Pts',(4.10379248299995,15.2,9.82861796999998));
#219196=CARTESIAN_POINT('Ctrl Pts',(4.10379248299995,11.6,9.82861796999998));
#219197=CARTESIAN_POINT('Ctrl Pts',(4.10413430799994,15.2,9.83085636799998));
#219198=CARTESIAN_POINT('Ctrl Pts',(4.10413430799994,11.6,9.83085636799998));
#219199=CARTESIAN_POINT('Ctrl Pts',(4.10447514699994,15.2,9.83310154499998));
#219200=CARTESIAN_POINT('Ctrl Pts',(4.10447514699994,11.6,9.83310154499998));
#219201=CARTESIAN_POINT('Ctrl Pts',(4.10481498799994,15.2,9.83535349199999));
#219202=CARTESIAN_POINT('Ctrl Pts',(4.10481498799994,11.6,9.83535349199999));
#219203=CARTESIAN_POINT('Ctrl Pts',(4.10515382099994,15.2,9.83761219399998));
#219204=CARTESIAN_POINT('Ctrl Pts',(4.10515382099994,11.6,9.83761219399998));
#219205=CARTESIAN_POINT('Ctrl Pts',(4.10549163099994,15.2,9.83987764099999));
#219206=CARTESIAN_POINT('Ctrl Pts',(4.10549163099994,11.6,9.83987764099999));
#219207=CARTESIAN_POINT('Ctrl Pts',(4.10582840599994,15.2,9.84214982099999));
#219208=CARTESIAN_POINT('Ctrl Pts',(4.10582840599994,11.6,9.84214982099999));
#219209=CARTESIAN_POINT('Ctrl Pts',(4.10616413599994,15.2,9.84442872299999));
#219210=CARTESIAN_POINT('Ctrl Pts',(4.10616413599994,11.6,9.84442872299999));
#219211=CARTESIAN_POINT('Ctrl Pts',(4.10649880899994,15.2,9.84671433499998));
#219212=CARTESIAN_POINT('Ctrl Pts',(4.10649880899994,11.6,9.84671433499998));
#219213=CARTESIAN_POINT('Ctrl Pts',(4.10683241099994,15.2,9.84900664599999));
#219214=CARTESIAN_POINT('Ctrl Pts',(4.10683241099994,11.6,9.84900664599999));
#219215=CARTESIAN_POINT('Ctrl Pts',(4.10716493199994,15.2,9.85130564399999));
#219216=CARTESIAN_POINT('Ctrl Pts',(4.10716493199994,11.6,9.85130564399999));
#219217=CARTESIAN_POINT('Ctrl Pts',(4.10749635899994,15.2,9.85361131699998));
#219218=CARTESIAN_POINT('Ctrl Pts',(4.10749635899994,11.6,9.85361131699998));
#219219=CARTESIAN_POINT('Ctrl Pts',(4.10782668199994,15.2,9.85592365499999));
#219220=CARTESIAN_POINT('Ctrl Pts',(4.10782668199994,11.6,9.85592365499999));
#219221=CARTESIAN_POINT('Ctrl Pts',(4.10815588799994,15.2,9.85824264699998));
#219222=CARTESIAN_POINT('Ctrl Pts',(4.10815588799994,11.6,9.85824264699998));
#219223=CARTESIAN_POINT('Ctrl Pts',(4.10848396599994,15.2,9.86056827999998));
#219224=CARTESIAN_POINT('Ctrl Pts',(4.10848396599994,11.6,9.86056827999998));
#219225=CARTESIAN_POINT('Ctrl Pts',(4.10881090399995,15.2,9.86290054199999));
#219226=CARTESIAN_POINT('Ctrl Pts',(4.10881090399995,11.6,9.86290054199999));
#219227=CARTESIAN_POINT('Ctrl Pts',(4.10913668999994,15.2,9.86523942399998));
#219228=CARTESIAN_POINT('Ctrl Pts',(4.10913668999994,11.6,9.86523942399998));
#219229=CARTESIAN_POINT('Ctrl Pts',(4.10946131299994,15.2,9.86758491299998));
#219230=CARTESIAN_POINT('Ctrl Pts',(4.10946131299994,11.6,9.86758491299998));
#219231=CARTESIAN_POINT('Ctrl Pts',(4.10978476099995,15.2,9.86993699799999));
#219232=CARTESIAN_POINT('Ctrl Pts',(4.10978476099995,11.6,9.86993699799999));
#219233=CARTESIAN_POINT('Ctrl Pts',(4.11010702299994,15.2,9.87229566899998));
#219234=CARTESIAN_POINT('Ctrl Pts',(4.11010702299994,11.6,9.87229566899998));
#219235=CARTESIAN_POINT('Ctrl Pts',(4.11042808799994,15.2,9.87466091399998));
#219236=CARTESIAN_POINT('Ctrl Pts',(4.11042808799994,11.6,9.87466091399998));
#219237=CARTESIAN_POINT('Ctrl Pts',(4.11074794399994,15.2,9.87703271999998));
#219238=CARTESIAN_POINT('Ctrl Pts',(4.11074794399994,11.6,9.87703271999998));
#219239=CARTESIAN_POINT('Ctrl Pts',(4.11106657999994,15.2,9.87941107899999));
#219240=CARTESIAN_POINT('Ctrl Pts',(4.11106657999994,11.6,9.87941107899999));
#219241=CARTESIAN_POINT('Ctrl Pts',(4.11138398399994,15.2,9.88179597699999));
#219242=CARTESIAN_POINT('Ctrl Pts',(4.11138398399994,11.6,9.88179597699999));
#219243=CARTESIAN_POINT('Ctrl Pts',(4.11170014699994,15.2,9.88418740499998));
#219244=CARTESIAN_POINT('Ctrl Pts',(4.11170014699994,11.6,9.88418740499998));
#219245=CARTESIAN_POINT('Ctrl Pts',(4.11201505399994,15.2,9.88658535199999));
#219246=CARTESIAN_POINT('Ctrl Pts',(4.11201505399994,11.6,9.88658535199999));
#219247=CARTESIAN_POINT('Ctrl Pts',(4.11232869799994,15.2,9.88898980399998));
#219248=CARTESIAN_POINT('Ctrl Pts',(4.11232869799994,11.6,9.88898980399998));
#219249=CARTESIAN_POINT('Ctrl Pts',(4.11264106399994,15.2,9.89140075399998));
#219250=CARTESIAN_POINT('Ctrl Pts',(4.11264106399994,11.6,9.89140075399998));
#219251=CARTESIAN_POINT('Ctrl Pts',(4.11295214299995,15.2,9.89381818699999));
#219252=CARTESIAN_POINT('Ctrl Pts',(4.11295214299995,11.6,9.89381818699999));
#219253=CARTESIAN_POINT('Ctrl Pts',(4.11326192499994,15.2,9.89624209499999));
#219254=CARTESIAN_POINT('Ctrl Pts',(4.11326192499994,11.6,9.89624209499999));
#219255=CARTESIAN_POINT('Ctrl Pts',(4.11357039599995,15.2,9.89867246599999));
#219256=CARTESIAN_POINT('Ctrl Pts',(4.11357039599995,11.6,9.89867246599999));
#219257=CARTESIAN_POINT('Ctrl Pts',(4.11387754699994,15.2,9.90110928899998));
#219258=CARTESIAN_POINT('Ctrl Pts',(4.11387754699994,11.6,9.90110928899998));
#219259=CARTESIAN_POINT('Ctrl Pts',(4.11418336699994,15.2,9.90355255299999));
#219260=CARTESIAN_POINT('Ctrl Pts',(4.11418336699994,11.6,9.90355255299999));
#219261=CARTESIAN_POINT('Ctrl Pts',(4.11448784499994,15.2,9.90600224699998));
#219262=CARTESIAN_POINT('Ctrl Pts',(4.11448784499994,11.6,9.90600224699998));
#219263=CARTESIAN_POINT('Ctrl Pts',(4.11479096999994,15.2,9.90845835999998));
#219264=CARTESIAN_POINT('Ctrl Pts',(4.11479096999994,11.6,9.90845835999998));
#219265=CARTESIAN_POINT('Ctrl Pts',(4.11509273099994,15.2,9.91092088199998));
#219266=CARTESIAN_POINT('Ctrl Pts',(4.11509273099994,11.6,9.91092088199998));
#219267=CARTESIAN_POINT('Ctrl Pts',(4.11539311699994,15.2,9.91338979999998));
#219268=CARTESIAN_POINT('Ctrl Pts',(4.11539311699994,11.6,9.91338979999998));
#219269=CARTESIAN_POINT('Ctrl Pts',(4.11569211799994,15.2,9.91586510699998));
#219270=CARTESIAN_POINT('Ctrl Pts',(4.11569211799994,11.6,9.91586510699998));
#219271=CARTESIAN_POINT('Ctrl Pts',(4.11598972299995,15.2,9.91834678799999));
#219272=CARTESIAN_POINT('Ctrl Pts',(4.11598972299995,11.6,9.91834678799999));
#219273=CARTESIAN_POINT('Ctrl Pts',(4.11628592199994,15.2,9.92083483499999));
#219274=CARTESIAN_POINT('Ctrl Pts',(4.11628592199994,11.6,9.92083483499999));
#219275=CARTESIAN_POINT('Ctrl Pts',(4.11658070199994,15.2,9.92332923599999));
#219276=CARTESIAN_POINT('Ctrl Pts',(4.11658070199994,11.6,9.92332923599999));
#219277=CARTESIAN_POINT('Ctrl Pts',(4.11687405499995,15.2,9.92582998099999));
#219278=CARTESIAN_POINT('Ctrl Pts',(4.11687405499995,11.6,9.92582998099999));
#219279=CARTESIAN_POINT('Ctrl Pts',(4.11716596799994,15.2,9.92833705899999));
#219280=CARTESIAN_POINT('Ctrl Pts',(4.11716596799994,11.6,9.92833705899999));
#219281=CARTESIAN_POINT('Ctrl Pts',(4.11745643399995,15.2,9.93085045899999));
#219282=CARTESIAN_POINT('Ctrl Pts',(4.11745643399995,11.6,9.93085045899999));
#219283=CARTESIAN_POINT('Ctrl Pts',(4.11774543899995,15.2,9.93337017099999));
#219284=CARTESIAN_POINT('Ctrl Pts',(4.11774543899995,11.6,9.93337017099999));
#219285=CARTESIAN_POINT('Ctrl Pts',(4.11803297499994,15.2,9.93589618299998));
#219286=CARTESIAN_POINT('Ctrl Pts',(4.11803297499994,11.6,9.93589618299998));
#219287=CARTESIAN_POINT('Ctrl Pts',(4.11831903099994,15.2,9.93842848499998));
#219288=CARTESIAN_POINT('Ctrl Pts',(4.11831903099994,11.6,9.93842848499998));
#219289=CARTESIAN_POINT('Ctrl Pts',(4.11860359399994,15.2,9.94096706799999));
#219290=CARTESIAN_POINT('Ctrl Pts',(4.11860359399994,11.6,9.94096706799999));
#219291=CARTESIAN_POINT('Ctrl Pts',(4.11888665799994,15.2,9.94351191999998));
#219292=CARTESIAN_POINT('Ctrl Pts',(4.11888665799994,11.6,9.94351191999998));
#219293=CARTESIAN_POINT('Ctrl Pts',(4.11916820899994,15.2,9.94606302999999));
#219294=CARTESIAN_POINT('Ctrl Pts',(4.11916820899994,11.6,9.94606302999999));
#219295=CARTESIAN_POINT('Ctrl Pts',(4.11944823799994,15.2,9.94862038699999));
#219296=CARTESIAN_POINT('Ctrl Pts',(4.11944823799994,11.6,9.94862038699999));
#219297=CARTESIAN_POINT('Ctrl Pts',(4.11972673699994,15.2,9.95118398199999));
#219298=CARTESIAN_POINT('Ctrl Pts',(4.11972673699994,11.6,9.95118398199999));
#219299=CARTESIAN_POINT('Ctrl Pts',(4.12000369199994,15.2,9.95375380499999));
#219300=CARTESIAN_POINT('Ctrl Pts',(4.12000369199994,11.6,9.95375380499999));
#219301=CARTESIAN_POINT('Ctrl Pts',(4.12027909599994,15.2,9.95632984399998));
#219302=CARTESIAN_POINT('Ctrl Pts',(4.12027909599994,11.6,9.95632984399998));
#219303=CARTESIAN_POINT('Ctrl Pts',(4.12055293699995,15.2,9.95891208799998));
#219304=CARTESIAN_POINT('Ctrl Pts',(4.12055293699995,11.6,9.95891208799998));
#219305=CARTESIAN_POINT('Ctrl Pts',(4.12082520399994,15.2,9.96150052899999));
#219306=CARTESIAN_POINT('Ctrl Pts',(4.12082520399994,11.6,9.96150052899999));
#219307=CARTESIAN_POINT('Ctrl Pts',(4.12109588999995,15.2,9.96409515399998));
#219308=CARTESIAN_POINT('Ctrl Pts',(4.12109588999995,11.6,9.96409515399998));
#219309=CARTESIAN_POINT('Ctrl Pts',(4.12136498299995,15.2,9.96669595499998));
#219310=CARTESIAN_POINT('Ctrl Pts',(4.12136498299995,11.6,9.96669595499998));
#219311=CARTESIAN_POINT('Ctrl Pts',(4.12163247299994,15.2,9.96930291999998));
#219312=CARTESIAN_POINT('Ctrl Pts',(4.12163247299994,11.6,9.96930291999998));
#219313=CARTESIAN_POINT('Ctrl Pts',(4.12189834999994,15.2,9.97191603899999));
#219314=CARTESIAN_POINT('Ctrl Pts',(4.12189834999994,11.6,9.97191603899999));
#219315=CARTESIAN_POINT('Ctrl Pts',(4.12216260499994,15.2,9.97453530099998));
#219316=CARTESIAN_POINT('Ctrl Pts',(4.12216260499994,11.6,9.97453530099998));
#219317=CARTESIAN_POINT('Ctrl Pts',(4.12242522799994,15.2,9.97716069699998));
#219318=CARTESIAN_POINT('Ctrl Pts',(4.12242522799994,11.6,9.97716069699998));
#219319=CARTESIAN_POINT('Ctrl Pts',(4.12268620699995,15.2,9.97979221699998));
#219320=CARTESIAN_POINT('Ctrl Pts',(4.12268620699995,11.6,9.97979221699998));
#219321=CARTESIAN_POINT('Ctrl Pts',(4.12294553499994,15.2,9.98242984899999));
#219322=CARTESIAN_POINT('Ctrl Pts',(4.12294553499994,11.6,9.98242984899999));
#219323=CARTESIAN_POINT('Ctrl Pts',(4.12320319999994,15.2,9.98507358299998));
#219324=CARTESIAN_POINT('Ctrl Pts',(4.12320319999994,11.6,9.98507358299998));
#219325=CARTESIAN_POINT('Ctrl Pts',(4.12345919399994,15.2,9.98772340999999));
#219326=CARTESIAN_POINT('Ctrl Pts',(4.12345919399994,11.6,9.98772340999999));
#219327=CARTESIAN_POINT('Ctrl Pts',(4.12371350699994,15.2,9.99037931899998));
#219328=CARTESIAN_POINT('Ctrl Pts',(4.12371350699994,11.6,9.99037931899998));
#219329=CARTESIAN_POINT('Ctrl Pts',(4.12396612799994,15.2,9.99304129999998));
#219330=CARTESIAN_POINT('Ctrl Pts',(4.12396612799994,11.6,9.99304129999998));
#219331=CARTESIAN_POINT('Ctrl Pts',(4.12421704799994,15.2,9.99570934199999));
#219332=CARTESIAN_POINT('Ctrl Pts',(4.12421704799994,11.6,9.99570934199999));
#219333=CARTESIAN_POINT('Ctrl Pts',(4.12446625799994,15.2,9.99838343599999));
#219334=CARTESIAN_POINT('Ctrl Pts',(4.12446625799994,11.6,9.99838343599999));
#219335=CARTESIAN_POINT('Ctrl Pts',(4.12471374799994,15.2,10.001063571));
#219336=CARTESIAN_POINT('Ctrl Pts',(4.12471374799994,11.6,10.001063571));
#219337=CARTESIAN_POINT('Ctrl Pts',(4.12495950799994,15.2,10.003749739));
#219338=CARTESIAN_POINT('Ctrl Pts',(4.12495950799994,11.6,10.003749739));
#219339=CARTESIAN_POINT('Ctrl Pts',(4.12520352799994,15.2,10.006441926));
#219340=CARTESIAN_POINT('Ctrl Pts',(4.12520352799994,11.6,10.006441926));
#219341=CARTESIAN_POINT('Ctrl Pts',(4.12544579999994,15.2,10.009140125));
#219342=CARTESIAN_POINT('Ctrl Pts',(4.12544579999994,11.6,10.009140125));
#219343=CARTESIAN_POINT('Ctrl Pts',(4.12568631399994,15.2,10.011844325));
#219344=CARTESIAN_POINT('Ctrl Pts',(4.12568631399994,11.6,10.011844325));
#219345=CARTESIAN_POINT('Ctrl Pts',(4.12592505999995,15.2,10.014554516));
#219346=CARTESIAN_POINT('Ctrl Pts',(4.12592505999995,11.6,10.014554516));
#219347=CARTESIAN_POINT('Ctrl Pts',(4.12616202899994,15.2,10.017270688));
#219348=CARTESIAN_POINT('Ctrl Pts',(4.12616202899994,11.6,10.017270688));
#219349=CARTESIAN_POINT('Ctrl Pts',(4.12639721099994,15.2,10.01999283));
#219350=CARTESIAN_POINT('Ctrl Pts',(4.12639721099994,11.6,10.01999283));
#219351=CARTESIAN_POINT('Ctrl Pts',(4.12663059799994,15.2,10.022720935));
#219352=CARTESIAN_POINT('Ctrl Pts',(4.12663059799994,11.6,10.022720935));
#219353=CARTESIAN_POINT('Ctrl Pts',(4.12686217999994,15.2,10.02545499));
#219354=CARTESIAN_POINT('Ctrl Pts',(4.12686217999994,11.6,10.02545499));
#219355=CARTESIAN_POINT('Ctrl Pts',(4.12709194699994,15.2,10.028194985));
#219356=CARTESIAN_POINT('Ctrl Pts',(4.12709194699994,11.6,10.028194985));
#219357=CARTESIAN_POINT('Ctrl Pts',(4.12731988999994,15.2,10.030940912));
#219358=CARTESIAN_POINT('Ctrl Pts',(4.12731988999994,11.6,10.030940912));
#219359=CARTESIAN_POINT('Ctrl Pts',(4.12754600099994,15.2,10.03369276));
#219360=CARTESIAN_POINT('Ctrl Pts',(4.12754600099994,11.6,10.03369276));
#219361=CARTESIAN_POINT('Ctrl Pts',(4.12777026999995,15.2,10.03645052));
#219362=CARTESIAN_POINT('Ctrl Pts',(4.12777026999995,11.6,10.03645052));
#219363=CARTESIAN_POINT('Ctrl Pts',(4.12799268599994,15.2,10.03921418));
#219364=CARTESIAN_POINT('Ctrl Pts',(4.12799268599994,11.6,10.03921418));
#219365=CARTESIAN_POINT('Ctrl Pts',(4.12821324299994,15.2,10.041983733));
#219366=CARTESIAN_POINT('Ctrl Pts',(4.12821324299994,11.6,10.041983733));
#219367=CARTESIAN_POINT('Ctrl Pts',(4.12843192999994,15.2,10.044759166));
#219368=CARTESIAN_POINT('Ctrl Pts',(4.12843192999994,11.6,10.044759166));
#219369=CARTESIAN_POINT('Ctrl Pts',(4.12864873899994,15.2,10.047540472));
#219370=CARTESIAN_POINT('Ctrl Pts',(4.12864873899994,11.6,10.047540472));
#219371=CARTESIAN_POINT('Ctrl Pts',(4.12886365999994,15.2,10.050327639));
#219372=CARTESIAN_POINT('Ctrl Pts',(4.12886365999994,11.6,10.050327639));
#219373=CARTESIAN_POINT('Ctrl Pts',(4.12907668299995,15.2,10.053120659));
#219374=CARTESIAN_POINT('Ctrl Pts',(4.12907668299995,11.6,10.053120659));
#219375=CARTESIAN_POINT('Ctrl Pts',(4.12928780099994,15.2,10.055919521));
#219376=CARTESIAN_POINT('Ctrl Pts',(4.12928780099994,11.6,10.055919521));
#219377=CARTESIAN_POINT('Ctrl Pts',(4.12949700599994,15.2,10.058724216));
#219378=CARTESIAN_POINT('Ctrl Pts',(4.12949700599994,11.6,10.058724216));
#219379=CARTESIAN_POINT('Ctrl Pts',(4.12970428599994,15.2,10.061534734));
#219380=CARTESIAN_POINT('Ctrl Pts',(4.12970428599994,11.6,10.061534734));
#219381=CARTESIAN_POINT('Ctrl Pts',(4.12990963199994,15.2,10.064351065));
#219382=CARTESIAN_POINT('Ctrl Pts',(4.12990963199994,11.6,10.064351065));
#219383=CARTESIAN_POINT('Ctrl Pts',(4.13011303899994,15.2,10.067173199));
#219384=CARTESIAN_POINT('Ctrl Pts',(4.13011303899994,11.6,10.067173199));
#219385=CARTESIAN_POINT('Ctrl Pts',(4.13031449499994,15.2,10.070001128));
#219386=CARTESIAN_POINT('Ctrl Pts',(4.13031449499994,11.6,10.070001128));
#219387=CARTESIAN_POINT('Ctrl Pts',(4.13051399199994,15.2,10.072834839));
#219388=CARTESIAN_POINT('Ctrl Pts',(4.13051399199994,11.6,10.072834839));
#219389=CARTESIAN_POINT('Ctrl Pts',(4.13071152099994,15.2,10.075674326));
#219390=CARTESIAN_POINT('Ctrl Pts',(4.13071152099994,11.6,10.075674326));
#219391=CARTESIAN_POINT('Ctrl Pts',(4.13090707399994,15.2,10.078519578));
#219392=CARTESIAN_POINT('Ctrl Pts',(4.13090707399994,11.6,10.078519578));
#219393=CARTESIAN_POINT('Ctrl Pts',(4.13110064099994,15.2,10.081370584));
#219394=CARTESIAN_POINT('Ctrl Pts',(4.13110064099994,11.6,10.081370584));
#219395=CARTESIAN_POINT('Ctrl Pts',(4.13129221399995,15.2,10.084227337));
#219396=CARTESIAN_POINT('Ctrl Pts',(4.13129221399995,11.6,10.084227337));
#219397=CARTESIAN_POINT('Ctrl Pts',(4.13148178399994,15.2,10.087089825));
#219398=CARTESIAN_POINT('Ctrl Pts',(4.13148178399994,11.6,10.087089825));
#219399=CARTESIAN_POINT('Ctrl Pts',(4.13166934299994,15.2,10.089958039));
#219400=CARTESIAN_POINT('Ctrl Pts',(4.13166934299994,11.6,10.089958039));
#219401=CARTESIAN_POINT('Ctrl Pts',(4.13185488199994,15.2,10.09283197));
#219402=CARTESIAN_POINT('Ctrl Pts',(4.13185488199994,11.6,10.09283197));
#219403=CARTESIAN_POINT('Ctrl Pts',(4.13203839299995,15.2,10.095711608));
#219404=CARTESIAN_POINT('Ctrl Pts',(4.13203839299995,11.6,10.095711608));
#219405=CARTESIAN_POINT('Ctrl Pts',(4.13221986599994,15.2,10.098596945));
#219406=CARTESIAN_POINT('Ctrl Pts',(4.13221986599994,11.6,10.098596945));
#219407=CARTESIAN_POINT('Ctrl Pts',(4.13239929399994,15.2,10.101487969));
#219408=CARTESIAN_POINT('Ctrl Pts',(4.13239929399994,11.6,10.101487969));
#219409=CARTESIAN_POINT('Ctrl Pts',(4.13257666799994,15.2,10.104384672));
#219410=CARTESIAN_POINT('Ctrl Pts',(4.13257666799994,11.6,10.104384672));
#219411=CARTESIAN_POINT('Ctrl Pts',(4.13275197799994,15.2,10.107287045));
#219412=CARTESIAN_POINT('Ctrl Pts',(4.13275197799994,11.6,10.107287045));
#219413=CARTESIAN_POINT('Ctrl Pts',(4.13292521699994,15.2,10.110195076));
#219414=CARTESIAN_POINT('Ctrl Pts',(4.13292521699994,11.6,10.110195076));
#219415=CARTESIAN_POINT('Ctrl Pts',(4.13309637699994,15.2,10.113108759));
#219416=CARTESIAN_POINT('Ctrl Pts',(4.13309637699994,11.6,10.113108759));
#219417=CARTESIAN_POINT('Ctrl Pts',(4.13326544899994,15.2,10.116028082));
#219418=CARTESIAN_POINT('Ctrl Pts',(4.13326544899994,11.6,10.116028082));
#219419=CARTESIAN_POINT('Ctrl Pts',(4.13343242499994,15.2,10.118953037));
#219420=CARTESIAN_POINT('Ctrl Pts',(4.13343242499994,11.6,10.118953037));
#219421=CARTESIAN_POINT('Ctrl Pts',(4.13359729599994,15.2,10.121883614));
#219422=CARTESIAN_POINT('Ctrl Pts',(4.13359729599994,11.6,10.121883614));
#219423=CARTESIAN_POINT('Ctrl Pts',(4.13376005399994,15.2,10.124819803));
#219424=CARTESIAN_POINT('Ctrl Pts',(4.13376005399994,11.6,10.124819803));
#219425=CARTESIAN_POINT('Ctrl Pts',(4.13392068999994,15.2,10.127761596));
#219426=CARTESIAN_POINT('Ctrl Pts',(4.13392068999994,11.6,10.127761596));
#219427=CARTESIAN_POINT('Ctrl Pts',(4.13407919799995,15.2,10.130708982));
#219428=CARTESIAN_POINT('Ctrl Pts',(4.13407919799995,11.6,10.130708982));
#219429=CARTESIAN_POINT('Ctrl Pts',(4.13423556699995,15.2,10.133661953));
#219430=CARTESIAN_POINT('Ctrl Pts',(4.13423556699995,11.6,10.133661953));
#219431=CARTESIAN_POINT('Ctrl Pts',(4.13438978999995,15.2,10.136620499));
#219432=CARTESIAN_POINT('Ctrl Pts',(4.13438978999995,11.6,10.136620499));
#219433=CARTESIAN_POINT('Ctrl Pts',(4.13454185899994,15.2,10.139584612));
#219434=CARTESIAN_POINT('Ctrl Pts',(4.13454185899994,11.6,10.139584612));
#219435=CARTESIAN_POINT('Ctrl Pts',(4.13469176399994,15.2,10.142554281));
#219436=CARTESIAN_POINT('Ctrl Pts',(4.13469176399994,11.6,10.142554281));
#219437=CARTESIAN_POINT('Ctrl Pts',(4.13483949999994,15.2,10.145529497));
#219438=CARTESIAN_POINT('Ctrl Pts',(4.13483949999994,11.6,10.145529497));
#219439=CARTESIAN_POINT('Ctrl Pts',(4.13498505699994,15.2,10.148510252));
#219440=CARTESIAN_POINT('Ctrl Pts',(4.13498505699994,11.6,10.148510252));
#219441=CARTESIAN_POINT('Ctrl Pts',(4.13512842699994,15.2,10.151496535));
#219442=CARTESIAN_POINT('Ctrl Pts',(4.13512842699994,11.6,10.151496535));
#219443=CARTESIAN_POINT('Ctrl Pts',(4.13526960299994,15.2,10.154488338));
#219444=CARTESIAN_POINT('Ctrl Pts',(4.13526960299994,11.6,10.154488338));
#219445=CARTESIAN_POINT('Ctrl Pts',(4.13540857599994,15.2,10.157485651));
#219446=CARTESIAN_POINT('Ctrl Pts',(4.13540857599994,11.6,10.157485651));
#219447=CARTESIAN_POINT('Ctrl Pts',(4.13554533699994,15.2,10.160488465));
#219448=CARTESIAN_POINT('Ctrl Pts',(4.13554533699994,11.6,10.160488465));
#219449=CARTESIAN_POINT('Ctrl Pts',(4.13567987999994,15.2,10.163496772));
#219450=CARTESIAN_POINT('Ctrl Pts',(4.13567987999994,11.6,10.163496772));
#219451=CARTESIAN_POINT('Ctrl Pts',(4.13581219499994,15.2,10.166510561));
#219452=CARTESIAN_POINT('Ctrl Pts',(4.13581219499994,11.6,10.166510561));
#219453=CARTESIAN_POINT('Ctrl Pts',(4.13594227699994,15.2,10.169529823));
#219454=CARTESIAN_POINT('Ctrl Pts',(4.13594227699994,11.6,10.169529823));
#219455=CARTESIAN_POINT('Ctrl Pts',(4.13607011399994,15.2,10.172554551));
#219456=CARTESIAN_POINT('Ctrl Pts',(4.13607011399994,11.6,10.172554551));
#219457=CARTESIAN_POINT('Ctrl Pts',(4.13619570299994,15.2,10.175584734));
#219458=CARTESIAN_POINT('Ctrl Pts',(4.13619570299994,11.6,10.175584734));
#219459=CARTESIAN_POINT('Ctrl Pts',(4.13631903099995,15.2,10.178620362));
#219460=CARTESIAN_POINT('Ctrl Pts',(4.13631903099995,11.6,10.178620362));
#219461=CARTESIAN_POINT('Ctrl Pts',(4.13644009399994,15.2,10.181661428));
#219462=CARTESIAN_POINT('Ctrl Pts',(4.13644009399994,11.6,10.181661428));
#219463=CARTESIAN_POINT('Ctrl Pts',(4.13655888299994,15.2,10.184707922));
#219464=CARTESIAN_POINT('Ctrl Pts',(4.13655888299994,11.6,10.184707922));
#219465=CARTESIAN_POINT('Ctrl Pts',(4.13667538999994,15.2,10.187759835));
#219466=CARTESIAN_POINT('Ctrl Pts',(4.13667538999994,11.6,10.187759835));
#219467=CARTESIAN_POINT('Ctrl Pts',(4.13678960699994,15.2,10.190817157));
#219468=CARTESIAN_POINT('Ctrl Pts',(4.13678960699994,11.6,10.190817157));
#219469=CARTESIAN_POINT('Ctrl Pts',(4.13690152699994,15.2,10.193879881));
#219470=CARTESIAN_POINT('Ctrl Pts',(4.13690152699994,11.6,10.193879881));
#219471=CARTESIAN_POINT('Ctrl Pts',(4.13701114099995,15.2,10.196947997));
#219472=CARTESIAN_POINT('Ctrl Pts',(4.13701114099995,11.6,10.196947997));
#219473=CARTESIAN_POINT('Ctrl Pts',(4.13711844299994,15.2,10.200021495));
#219474=CARTESIAN_POINT('Ctrl Pts',(4.13711844299994,11.6,10.200021495));
#219475=CARTESIAN_POINT('Ctrl Pts',(4.13722342399994,15.2,10.203100367));
#219476=CARTESIAN_POINT('Ctrl Pts',(4.13722342399994,11.6,10.203100367));
#219477=CARTESIAN_POINT('Ctrl Pts',(4.13732607699994,15.2,10.206184603));
#219478=CARTESIAN_POINT('Ctrl Pts',(4.13732607699994,11.6,10.206184603));
#219479=CARTESIAN_POINT('Ctrl Pts',(4.13742639399994,15.2,10.209274196));
#219480=CARTESIAN_POINT('Ctrl Pts',(4.13742639399994,11.6,10.209274196));
#219481=CARTESIAN_POINT('Ctrl Pts',(4.13752436799994,15.2,10.212369135));
#219482=CARTESIAN_POINT('Ctrl Pts',(4.13752436799994,11.6,10.212369135));
#219483=CARTESIAN_POINT('Ctrl Pts',(4.13761998999994,15.2,10.215469412));
#219484=CARTESIAN_POINT('Ctrl Pts',(4.13761998999994,11.6,10.215469412));
#219485=CARTESIAN_POINT('Ctrl Pts',(4.13771325399995,15.2,10.218575018));
#219486=CARTESIAN_POINT('Ctrl Pts',(4.13771325399995,11.6,10.218575018));
#219487=CARTESIAN_POINT('Ctrl Pts',(4.13780415199995,15.2,10.221685944));
#219488=CARTESIAN_POINT('Ctrl Pts',(4.13780415199995,11.6,10.221685944));
#219489=CARTESIAN_POINT('Ctrl Pts',(4.13789267699994,15.2,10.224802182));
#219490=CARTESIAN_POINT('Ctrl Pts',(4.13789267699994,11.6,10.224802182));
#219491=CARTESIAN_POINT('Ctrl Pts',(4.13797881999994,15.2,10.22792372));
#219492=CARTESIAN_POINT('Ctrl Pts',(4.13797881999994,11.6,10.22792372));
#219493=CARTESIAN_POINT('Ctrl Pts',(4.13806257499994,15.2,10.231050553));
#219494=CARTESIAN_POINT('Ctrl Pts',(4.13806257499994,11.6,10.231050553));
#219495=CARTESIAN_POINT('Ctrl Pts',(4.13814393399994,15.2,10.23418267));
#219496=CARTESIAN_POINT('Ctrl Pts',(4.13814393399994,11.6,10.23418267));
#219497=CARTESIAN_POINT('Ctrl Pts',(4.13822288999994,15.2,10.237320063));
#219498=CARTESIAN_POINT('Ctrl Pts',(4.13822288999994,11.6,10.237320063));
#219499=CARTESIAN_POINT('Ctrl Pts',(4.13829943399994,15.2,10.240462722));
#219500=CARTESIAN_POINT('Ctrl Pts',(4.13829943399994,11.6,10.240462722));
#219501=CARTESIAN_POINT('Ctrl Pts',(4.13837356099994,15.2,10.243610638));
#219502=CARTESIAN_POINT('Ctrl Pts',(4.13837356099994,11.6,10.243610638));
#219503=CARTESIAN_POINT('Ctrl Pts',(4.13844526199994,15.2,10.246763804));
#219504=CARTESIAN_POINT('Ctrl Pts',(4.13844526199994,11.6,10.246763804));
#219505=CARTESIAN_POINT('Ctrl Pts',(4.13851452999995,15.2,10.249922211));
#219506=CARTESIAN_POINT('Ctrl Pts',(4.13851452999995,11.6,10.249922211));
#219507=CARTESIAN_POINT('Ctrl Pts',(4.13858135799994,15.2,10.253085849));
#219508=CARTESIAN_POINT('Ctrl Pts',(4.13858135799994,11.6,10.253085849));
#219509=CARTESIAN_POINT('Ctrl Pts',(4.13864573899995,15.2,10.256254709));
#219510=CARTESIAN_POINT('Ctrl Pts',(4.13864573899995,11.6,10.256254709));
#219511=CARTESIAN_POINT('Ctrl Pts',(4.13870766499994,15.2,10.259428783));
#219512=CARTESIAN_POINT('Ctrl Pts',(4.13870766499994,11.6,10.259428783));
#219513=CARTESIAN_POINT('Ctrl Pts',(4.13876712899994,15.2,10.262608063));
#219514=CARTESIAN_POINT('Ctrl Pts',(4.13876712899994,11.6,10.262608063));
#219515=CARTESIAN_POINT('Ctrl Pts',(4.13882412399994,15.2,10.265792539));
#219516=CARTESIAN_POINT('Ctrl Pts',(4.13882412399994,11.6,10.265792539));
#219517=CARTESIAN_POINT('Ctrl Pts',(4.13887864299994,15.2,10.268982203));
#219518=CARTESIAN_POINT('Ctrl Pts',(4.13887864299994,11.6,10.268982203));
#219519=CARTESIAN_POINT('Ctrl Pts',(4.13893067799994,15.2,10.272177045));
#219520=CARTESIAN_POINT('Ctrl Pts',(4.13893067799994,11.6,10.272177045));
#219521=CARTESIAN_POINT('Ctrl Pts',(4.13898022299994,15.2,10.275377058));
#219522=CARTESIAN_POINT('Ctrl Pts',(4.13898022299994,11.6,10.275377058));
#219523=CARTESIAN_POINT('Ctrl Pts',(4.13902726899994,15.2,10.278582233));
#219524=CARTESIAN_POINT('Ctrl Pts',(4.13902726899994,11.6,10.278582233));
#219525=CARTESIAN_POINT('Ctrl Pts',(4.13907180999994,15.2,10.281792559));
#219526=CARTESIAN_POINT('Ctrl Pts',(4.13907180999994,11.6,10.281792559));
#219527=CARTESIAN_POINT('Ctrl Pts',(4.13911384099994,15.2,10.285008031));
#219528=CARTESIAN_POINT('Ctrl Pts',(4.13911384099994,11.6,10.285008031));
#219529=CARTESIAN_POINT('Ctrl Pts',(4.13915335099994,15.2,10.288228638));
#219530=CARTESIAN_POINT('Ctrl Pts',(4.13915335099994,11.6,10.288228638));
#219531=CARTESIAN_POINT('Ctrl Pts',(4.13919033599994,15.2,10.291454371));
#219532=CARTESIAN_POINT('Ctrl Pts',(4.13919033599994,11.6,10.291454371));
#219533=CARTESIAN_POINT('Ctrl Pts',(4.13922478799994,15.2,10.294685223));
#219534=CARTESIAN_POINT('Ctrl Pts',(4.13922478799994,11.6,10.294685223));
#219535=CARTESIAN_POINT('Ctrl Pts',(4.13925669999994,15.2,10.297921185));
#219536=CARTESIAN_POINT('Ctrl Pts',(4.13925669999994,11.6,10.297921185));
#219537=CARTESIAN_POINT('Ctrl Pts',(4.13928606399994,15.2,10.301162247));
#219538=CARTESIAN_POINT('Ctrl Pts',(4.13928606399994,11.6,10.301162247));
#219539=CARTESIAN_POINT('Ctrl Pts',(4.13931287499994,15.2,10.304408403));
#219540=CARTESIAN_POINT('Ctrl Pts',(4.13931287499994,11.6,10.304408403));
#219541=CARTESIAN_POINT('Ctrl Pts',(4.13933712499994,15.2,10.307659642));
#219542=CARTESIAN_POINT('Ctrl Pts',(4.13933712499994,11.6,10.307659642));
#219543=CARTESIAN_POINT('Ctrl Pts',(4.13935880599994,15.2,10.310915956));
#219544=CARTESIAN_POINT('Ctrl Pts',(4.13935880599994,11.6,10.310915956));
#219545=CARTESIAN_POINT('Ctrl Pts',(4.13937791299994,15.2,10.314177338));
#219546=CARTESIAN_POINT('Ctrl Pts',(4.13937791299994,11.6,10.314177338));
#219547=CARTESIAN_POINT('Ctrl Pts',(4.13939443899995,15.2,10.317443777));
#219548=CARTESIAN_POINT('Ctrl Pts',(4.13939443899995,11.6,10.317443777));
#219549=CARTESIAN_POINT('Ctrl Pts',(4.13940837499994,15.2,10.320715266));
#219550=CARTESIAN_POINT('Ctrl Pts',(4.13940837499994,11.6,10.320715266));
#219551=CARTESIAN_POINT('Ctrl Pts',(4.13941971699994,15.2,10.323991796));
#219552=CARTESIAN_POINT('Ctrl Pts',(4.13941971699994,11.6,10.323991796));
#219553=CARTESIAN_POINT('Ctrl Pts',(4.13942845599994,15.2,10.327273358));
#219554=CARTESIAN_POINT('Ctrl Pts',(4.13942845599994,11.6,10.327273358));
#219555=CARTESIAN_POINT('Ctrl Pts',(4.13943458699995,15.2,10.330559945));
#219556=CARTESIAN_POINT('Ctrl Pts',(4.13943458699995,11.6,10.330559945));
#219557=CARTESIAN_POINT('Ctrl Pts',(4.13943810199994,15.2,10.333851547));
#219558=CARTESIAN_POINT('Ctrl Pts',(4.13943810199994,11.6,10.333851547));
#219559=CARTESIAN_POINT('Ctrl Pts',(4.13943899399994,15.2,10.337148157));
#219560=CARTESIAN_POINT('Ctrl Pts',(4.13943899399994,11.6,10.337148157));
#219561=CARTESIAN_POINT('Ctrl Pts',(4.13943725799994,15.2,10.340449765));
#219562=CARTESIAN_POINT('Ctrl Pts',(4.13943725799994,11.6,10.340449765));
#219563=CARTESIAN_POINT('Ctrl Pts',(4.13943288499994,15.2,10.343756363));
#219564=CARTESIAN_POINT('Ctrl Pts',(4.13943288499994,11.6,10.343756363));
#219565=CARTESIAN_POINT('Ctrl Pts',(4.13942586899995,15.2,10.347067944));
#219566=CARTESIAN_POINT('Ctrl Pts',(4.13942586899995,11.6,10.347067944));
#219567=CARTESIAN_POINT('Ctrl Pts',(4.13941620499994,15.2,10.350384497));
#219568=CARTESIAN_POINT('Ctrl Pts',(4.13941620499994,11.6,10.350384497));
#219569=CARTESIAN_POINT('Ctrl Pts',(4.13940388399994,15.2,10.353706016));
#219570=CARTESIAN_POINT('Ctrl Pts',(4.13940388399994,11.6,10.353706016));
#219571=CARTESIAN_POINT('Ctrl Pts',(4.13938890099994,15.2,10.357032491));
#219572=CARTESIAN_POINT('Ctrl Pts',(4.13938890099994,11.6,10.357032491));
#219573=CARTESIAN_POINT('Ctrl Pts',(4.13937124999994,15.2,10.360363915));
#219574=CARTESIAN_POINT('Ctrl Pts',(4.13937124999994,11.6,10.360363915));
#219575=CARTESIAN_POINT('Ctrl Pts',(4.13935092099995,15.2,10.363700278));
#219576=CARTESIAN_POINT('Ctrl Pts',(4.13935092099995,11.6,10.363700278));
#219577=CARTESIAN_POINT('Ctrl Pts',(4.13932791199994,15.2,10.367041572));
#219578=CARTESIAN_POINT('Ctrl Pts',(4.13932791199994,11.6,10.367041572));
#219579=CARTESIAN_POINT('Ctrl Pts',(4.13930221199994,15.2,10.370387789));
#219580=CARTESIAN_POINT('Ctrl Pts',(4.13930221199994,11.6,10.370387789));
#219581=CARTESIAN_POINT('Ctrl Pts',(4.13927381799994,15.2,10.373738921));
#219582=CARTESIAN_POINT('Ctrl Pts',(4.13927381799994,11.6,10.373738921));
#219583=CARTESIAN_POINT('Ctrl Pts',(4.13924272199994,15.2,10.37709496));
#219584=CARTESIAN_POINT('Ctrl Pts',(4.13924272199994,11.6,10.37709496));
#219585=CARTESIAN_POINT('Ctrl Pts',(4.13920891699994,15.2,10.380455897));
#219586=CARTESIAN_POINT('Ctrl Pts',(4.13920891699994,11.6,10.380455897));
#219587=CARTESIAN_POINT('Ctrl Pts',(4.13917239799994,15.2,10.383821722));
#219588=CARTESIAN_POINT('Ctrl Pts',(4.13917239799994,11.6,10.383821722));
#219589=CARTESIAN_POINT('Ctrl Pts',(4.13913315699994,15.2,10.38719243));
#219590=CARTESIAN_POINT('Ctrl Pts',(4.13913315699994,11.6,10.38719243));
#219591=CARTESIAN_POINT('Ctrl Pts',(4.13909118899995,15.2,10.39056801));
#219592=CARTESIAN_POINT('Ctrl Pts',(4.13909118899995,11.6,10.39056801));
#219593=CARTESIAN_POINT('Ctrl Pts',(4.13904648599994,15.2,10.393948456));
#219594=CARTESIAN_POINT('Ctrl Pts',(4.13904648599994,11.6,10.393948456));
#219595=CARTESIAN_POINT('Ctrl Pts',(4.13899904399995,15.2,10.397333758));
#219596=CARTESIAN_POINT('Ctrl Pts',(4.13899904399995,11.6,10.397333758));
#219597=CARTESIAN_POINT('Ctrl Pts',(4.13894885299994,15.2,10.400723909));
#219598=CARTESIAN_POINT('Ctrl Pts',(4.13894885299994,11.6,10.400723909));
#219599=CARTESIAN_POINT('Ctrl Pts',(4.13889590999994,15.2,10.4041189));
#219600=CARTESIAN_POINT('Ctrl Pts',(4.13889590999994,11.6,10.4041189));
#219601=CARTESIAN_POINT('Ctrl Pts',(4.13884020599994,15.2,10.407518721));
#219602=CARTESIAN_POINT('Ctrl Pts',(4.13884020599994,11.6,10.407518721));
#219603=CARTESIAN_POINT('Ctrl Pts',(4.13878173799994,15.2,10.410923367));
#219604=CARTESIAN_POINT('Ctrl Pts',(4.13878173799994,11.6,10.410923367));
#219605=CARTESIAN_POINT('Ctrl Pts',(4.13872049699994,15.2,10.414332828));
#219606=CARTESIAN_POINT('Ctrl Pts',(4.13872049699994,11.6,10.414332828));
#219607=CARTESIAN_POINT('Ctrl Pts',(4.13865647599994,15.2,10.417747096));
#219608=CARTESIAN_POINT('Ctrl Pts',(4.13865647599994,11.6,10.417747096));
#219609=CARTESIAN_POINT('Ctrl Pts',(4.13858967199995,15.2,10.421166163));
#219610=CARTESIAN_POINT('Ctrl Pts',(4.13858967199995,11.6,10.421166163));
#219611=CARTESIAN_POINT('Ctrl Pts',(4.13852007699994,15.2,10.424590021));
#219612=CARTESIAN_POINT('Ctrl Pts',(4.13852007699994,11.6,10.424590021));
#219613=CARTESIAN_POINT('Ctrl Pts',(4.13844768399994,15.2,10.428018661));
#219614=CARTESIAN_POINT('Ctrl Pts',(4.13844768399994,11.6,10.428018661));
#219615=CARTESIAN_POINT('Ctrl Pts',(4.13837248699994,15.2,10.431452077));
#219616=CARTESIAN_POINT('Ctrl Pts',(4.13837248699994,11.6,10.431452077));
#219617=CARTESIAN_POINT('Ctrl Pts',(4.13829448099994,15.2,10.434890258));
#219618=CARTESIAN_POINT('Ctrl Pts',(4.13829448099994,11.6,10.434890258));
#219619=CARTESIAN_POINT('Ctrl Pts',(4.13821365899994,15.2,10.438333197));
#219620=CARTESIAN_POINT('Ctrl Pts',(4.13821365899994,11.6,10.438333197));
#219621=CARTESIAN_POINT('Ctrl Pts',(4.13813001599994,15.2,10.441780886));
#219622=CARTESIAN_POINT('Ctrl Pts',(4.13813001599994,11.6,10.441780886));
#219623=CARTESIAN_POINT('Ctrl Pts',(4.13804354399994,15.2,10.445233317));
#219624=CARTESIAN_POINT('Ctrl Pts',(4.13804354399994,11.6,10.445233317));
#219625=CARTESIAN_POINT('Ctrl Pts',(4.13795423699994,15.2,10.448690482));
#219626=CARTESIAN_POINT('Ctrl Pts',(4.13795423699994,11.6,10.448690482));
#219627=CARTESIAN_POINT('Ctrl Pts',(4.13786209099994,15.2,10.452152373));
#219628=CARTESIAN_POINT('Ctrl Pts',(4.13786209099994,11.6,10.452152373));
#219629=CARTESIAN_POINT('Ctrl Pts',(4.13776709699994,15.2,10.45561898));
#219630=CARTESIAN_POINT('Ctrl Pts',(4.13776709699994,11.6,10.45561898));
#219631=CARTESIAN_POINT('Ctrl Pts',(4.13766925199995,15.2,10.459090298));
#219632=CARTESIAN_POINT('Ctrl Pts',(4.13766925199995,11.6,10.459090298));
#219633=CARTESIAN_POINT('Ctrl Pts',(4.13756854799994,15.2,10.462566317));
#219634=CARTESIAN_POINT('Ctrl Pts',(4.13756854799994,11.6,10.462566317));
#219635=CARTESIAN_POINT('Ctrl Pts',(4.13746497999994,15.2,10.466047029));
#219636=CARTESIAN_POINT('Ctrl Pts',(4.13746497999994,11.6,10.466047029));
#219637=CARTESIAN_POINT('Ctrl Pts',(4.13735853899994,15.2,10.469532426));
#219638=CARTESIAN_POINT('Ctrl Pts',(4.13735853899994,11.6,10.469532426));
#219639=CARTESIAN_POINT('Ctrl Pts',(4.13724922399994,15.2,10.473022501));
#219640=CARTESIAN_POINT('Ctrl Pts',(4.13724922399994,11.6,10.473022501));
#219641=CARTESIAN_POINT('Ctrl Pts',(4.13713702599994,15.2,10.476517245));
#219642=CARTESIAN_POINT('Ctrl Pts',(4.13713702599994,11.6,10.476517245));
#219643=CARTESIAN_POINT('Ctrl Pts',(4.13702193799994,15.2,10.48001665));
#219644=CARTESIAN_POINT('Ctrl Pts',(4.13702193799994,11.6,10.48001665));
#219645=CARTESIAN_POINT('Ctrl Pts',(4.13690395699994,15.2,10.483520709));
#219646=CARTESIAN_POINT('Ctrl Pts',(4.13690395699994,11.6,10.483520709));
#219647=CARTESIAN_POINT('Ctrl Pts',(4.13678307499994,15.2,10.487029411));
#219648=CARTESIAN_POINT('Ctrl Pts',(4.13678307499994,11.6,10.487029411));
#219649=CARTESIAN_POINT('Ctrl Pts',(4.13665928599994,15.2,10.490542752));
#219650=CARTESIAN_POINT('Ctrl Pts',(4.13665928599994,11.6,10.490542752));
#219651=CARTESIAN_POINT('Ctrl Pts',(4.13653258699994,15.2,10.494060722));
#219652=CARTESIAN_POINT('Ctrl Pts',(4.13653258699994,11.6,10.494060722));
#219653=CARTESIAN_POINT('Ctrl Pts',(4.13640296799994,15.2,10.497583313));
#219654=CARTESIAN_POINT('Ctrl Pts',(4.13640296799994,11.6,10.497583313));
#219655=CARTESIAN_POINT('Ctrl Pts',(4.13627042599995,15.2,10.501110517));
#219656=CARTESIAN_POINT('Ctrl Pts',(4.13627042599995,11.6,10.501110517));
#219657=CARTESIAN_POINT('Ctrl Pts',(4.13613495399995,15.2,10.504642327));
#219658=CARTESIAN_POINT('Ctrl Pts',(4.13613495399995,11.6,10.504642327));
#219659=CARTESIAN_POINT('Ctrl Pts',(4.13599654599994,15.2,10.508178734));
#219660=CARTESIAN_POINT('Ctrl Pts',(4.13599654599994,11.6,10.508178734));
#219661=CARTESIAN_POINT('Ctrl Pts',(4.13585519699994,15.2,10.51171973));
#219662=CARTESIAN_POINT('Ctrl Pts',(4.13585519699994,11.6,10.51171973));
#219663=CARTESIAN_POINT('Ctrl Pts',(4.13571090199994,15.2,10.515265308));
#219664=CARTESIAN_POINT('Ctrl Pts',(4.13571090199994,11.6,10.515265308));
#219665=CARTESIAN_POINT('Ctrl Pts',(4.13556365199994,15.2,10.518815459));
#219666=CARTESIAN_POINT('Ctrl Pts',(4.13556365199994,11.6,10.518815459));
#219667=CARTESIAN_POINT('Ctrl Pts',(4.13541344499994,15.2,10.522370177));
#219668=CARTESIAN_POINT('Ctrl Pts',(4.13541344499994,11.6,10.522370177));
#219669=CARTESIAN_POINT('Ctrl Pts',(4.13526027299994,15.2,10.525929452));
#219670=CARTESIAN_POINT('Ctrl Pts',(4.13526027299994,11.6,10.525929452));
#219671=CARTESIAN_POINT('Ctrl Pts',(4.13510412999995,15.2,10.529493277));
#219672=CARTESIAN_POINT('Ctrl Pts',(4.13510412999995,11.6,10.529493277));
#219673=CARTESIAN_POINT('Ctrl Pts',(4.13494501199995,15.2,10.533061644));
#219674=CARTESIAN_POINT('Ctrl Pts',(4.13494501199995,11.6,10.533061644));
#219675=CARTESIAN_POINT('Ctrl Pts',(4.13478291299994,15.2,10.536634545));
#219676=CARTESIAN_POINT('Ctrl Pts',(4.13478291299994,11.6,10.536634545));
#219677=CARTESIAN_POINT('Ctrl Pts',(4.13461782599994,15.2,10.540211972));
#219678=CARTESIAN_POINT('Ctrl Pts',(4.13461782599994,11.6,10.540211972));
#219679=CARTESIAN_POINT('Ctrl Pts',(4.13444974499994,15.2,10.543793918));
#219680=CARTESIAN_POINT('Ctrl Pts',(4.13444974499994,11.6,10.543793918));
#219681=CARTESIAN_POINT('Ctrl Pts',(4.13427866799995,15.2,10.547380374));
#219682=CARTESIAN_POINT('Ctrl Pts',(4.13427866799995,11.6,10.547380374));
#219683=CARTESIAN_POINT('Ctrl Pts',(4.13410458499994,15.2,10.550971333));
#219684=CARTESIAN_POINT('Ctrl Pts',(4.13410458499994,11.6,10.550971333));
#219685=CARTESIAN_POINT('Ctrl Pts',(4.13392749299994,15.2,10.554566788));
#219686=CARTESIAN_POINT('Ctrl Pts',(4.13392749299994,11.6,10.554566788));
#219687=CARTESIAN_POINT('Ctrl Pts',(4.13374738599994,15.2,10.55816673));
#219688=CARTESIAN_POINT('Ctrl Pts',(4.13374738599994,11.6,10.55816673));
#219689=CARTESIAN_POINT('Ctrl Pts',(4.13356425899994,15.2,10.561771151));
#219690=CARTESIAN_POINT('Ctrl Pts',(4.13356425899994,11.6,10.561771151));
#219691=CARTESIAN_POINT('Ctrl Pts',(4.13337810299994,15.2,10.565380043));
#219692=CARTESIAN_POINT('Ctrl Pts',(4.13337810299994,11.6,10.565380043));
#219693=CARTESIAN_POINT('Ctrl Pts',(4.13318891699994,15.2,10.568993399));
#219694=CARTESIAN_POINT('Ctrl Pts',(4.13318891699994,11.6,10.568993399));
#219695=CARTESIAN_POINT('Ctrl Pts',(4.13299669299994,15.2,10.572611211));
#219696=CARTESIAN_POINT('Ctrl Pts',(4.13299669299994,11.6,10.572611211));
#219697=CARTESIAN_POINT('Ctrl Pts',(4.13280142599994,15.2,10.576233472));
#219698=CARTESIAN_POINT('Ctrl Pts',(4.13280142599994,11.6,10.576233472));
#219699=CARTESIAN_POINT('Ctrl Pts',(4.13260311099994,15.2,10.579860173));
#219700=CARTESIAN_POINT('Ctrl Pts',(4.13260311099994,11.6,10.579860173));
#219701=CARTESIAN_POINT('Ctrl Pts',(4.13240174099994,15.2,10.583491307));
#219702=CARTESIAN_POINT('Ctrl Pts',(4.13240174099994,11.6,10.583491307));
#219703=CARTESIAN_POINT('Ctrl Pts',(4.13219731199994,15.2,10.587126865));
#219704=CARTESIAN_POINT('Ctrl Pts',(4.13219731199994,11.6,10.587126865));
#219705=CARTESIAN_POINT('Ctrl Pts',(4.13198981899995,15.2,10.590766842));
#219706=CARTESIAN_POINT('Ctrl Pts',(4.13198981899995,11.6,10.590766842));
#219707=CARTESIAN_POINT('Ctrl Pts',(4.13177925499994,15.2,10.594411227));
#219708=CARTESIAN_POINT('Ctrl Pts',(4.13177925499994,11.6,10.594411227));
#219709=CARTESIAN_POINT('Ctrl Pts',(4.13156561499994,15.2,10.598060015));
#219710=CARTESIAN_POINT('Ctrl Pts',(4.13156561499994,11.6,10.598060015));
#219711=CARTESIAN_POINT('Ctrl Pts',(4.13134889399995,15.2,10.601713197));
#219712=CARTESIAN_POINT('Ctrl Pts',(4.13134889399995,11.6,10.601713197));
#219713=CARTESIAN_POINT('Ctrl Pts',(4.13112908699994,15.2,10.605370765));
#219714=CARTESIAN_POINT('Ctrl Pts',(4.13112908699994,11.6,10.605370765));
#219715=CARTESIAN_POINT('Ctrl Pts',(4.13090618799994,15.2,10.609032712));
#219716=CARTESIAN_POINT('Ctrl Pts',(4.13090618799994,11.6,10.609032712));
#219717=CARTESIAN_POINT('Ctrl Pts',(4.13068019199994,15.2,10.612699031));
#219718=CARTESIAN_POINT('Ctrl Pts',(4.13068019199994,11.6,10.612699031));
#219719=CARTESIAN_POINT('Ctrl Pts',(4.13045109399994,15.2,10.616369713));
#219720=CARTESIAN_POINT('Ctrl Pts',(4.13045109399994,11.6,10.616369713));
#219721=CARTESIAN_POINT('Ctrl Pts',(4.13021888699994,15.2,10.62004475));
#219722=CARTESIAN_POINT('Ctrl Pts',(4.13021888699994,11.6,10.62004475));
#219723=CARTESIAN_POINT('Ctrl Pts',(4.12998356799995,15.2,10.623724135));
#219724=CARTESIAN_POINT('Ctrl Pts',(4.12998356799995,11.6,10.623724135));
#219725=CARTESIAN_POINT('Ctrl Pts',(4.12974512999994,15.2,10.627407862));
#219726=CARTESIAN_POINT('Ctrl Pts',(4.12974512999994,11.6,10.627407862));
#219727=CARTESIAN_POINT('Ctrl Pts',(4.12950356699994,15.2,10.63109592));
#219728=CARTESIAN_POINT('Ctrl Pts',(4.12950356699994,11.6,10.63109592));
#219729=CARTESIAN_POINT('Ctrl Pts',(4.12925887599994,15.2,10.634788304));
#219730=CARTESIAN_POINT('Ctrl Pts',(4.12925887599994,11.6,10.634788304));
#219731=CARTESIAN_POINT('Ctrl Pts',(4.12901105099994,15.2,10.638485005));
#219732=CARTESIAN_POINT('Ctrl Pts',(4.12901105099994,11.6,10.638485005));
#219733=CARTESIAN_POINT('Ctrl Pts',(4.12876008699994,15.2,10.642186018));
#219734=CARTESIAN_POINT('Ctrl Pts',(4.12876008699994,11.6,10.642186018));
#219735=CARTESIAN_POINT('Ctrl Pts',(4.12850597799994,15.2,10.645891332));
#219736=CARTESIAN_POINT('Ctrl Pts',(4.12850597799994,11.6,10.645891332));
#219737=CARTESIAN_POINT('Ctrl Pts',(4.12824871999994,15.2,10.649600943));
#219738=CARTESIAN_POINT('Ctrl Pts',(4.12824871999994,11.6,10.649600943));
#219739=CARTESIAN_POINT('Ctrl Pts',(4.12798830699994,15.2,10.65331484));
#219740=CARTESIAN_POINT('Ctrl Pts',(4.12798830699994,11.6,10.65331484));
#219741=CARTESIAN_POINT('Ctrl Pts',(4.12772473399994,15.2,10.657033018));
#219742=CARTESIAN_POINT('Ctrl Pts',(4.12772473399994,11.6,10.657033018));
#219743=CARTESIAN_POINT('Ctrl Pts',(4.12745799499994,15.2,10.660755467));
#219744=CARTESIAN_POINT('Ctrl Pts',(4.12745799499994,11.6,10.660755467));
#219745=CARTESIAN_POINT('Ctrl Pts',(4.12718808399995,15.2,10.66448218));
#219746=CARTESIAN_POINT('Ctrl Pts',(4.12718808399995,11.6,10.66448218));
#219747=CARTESIAN_POINT('Ctrl Pts',(4.12691499899995,15.2,10.668213149));
#219748=CARTESIAN_POINT('Ctrl Pts',(4.12691499899995,11.6,10.668213149));
#219749=CARTESIAN_POINT('Ctrl Pts',(4.12663873099994,15.2,10.671948366));
#219750=CARTESIAN_POINT('Ctrl Pts',(4.12663873099994,11.6,10.671948366));
#219751=CARTESIAN_POINT('Ctrl Pts',(4.12635927699994,15.2,10.675687826));
#219752=CARTESIAN_POINT('Ctrl Pts',(4.12635927699994,11.6,10.675687826));
#219753=CARTESIAN_POINT('Ctrl Pts',(4.12607663299995,15.2,10.679431519));
#219754=CARTESIAN_POINT('Ctrl Pts',(4.12607663299995,11.6,10.679431519));
#219755=CARTESIAN_POINT('Ctrl Pts',(4.12579079399995,15.2,10.683179442));
#219756=CARTESIAN_POINT('Ctrl Pts',(4.12579079399995,11.6,10.683179442));
#219757=CARTESIAN_POINT('Ctrl Pts',(4.12550175599994,15.2,10.686931586));
#219758=CARTESIAN_POINT('Ctrl Pts',(4.12550175599994,11.6,10.686931586));
#219759=CARTESIAN_POINT('Ctrl Pts',(4.12520951199994,15.2,10.690687944));
#219760=CARTESIAN_POINT('Ctrl Pts',(4.12520951199994,11.6,10.690687944));
#219761=CARTESIAN_POINT('Ctrl Pts',(4.12491405899994,15.2,10.694448508));
#219762=CARTESIAN_POINT('Ctrl Pts',(4.12491405899994,11.6,10.694448508));
#219763=CARTESIAN_POINT('Ctrl Pts',(4.12461539099994,15.2,10.698213269));
#219764=CARTESIAN_POINT('Ctrl Pts',(4.12461539099994,11.6,10.698213269));
#219765=CARTESIAN_POINT('Ctrl Pts',(4.12431349899994,15.2,10.70198222));
#219766=CARTESIAN_POINT('Ctrl Pts',(4.12431349899994,11.6,10.70198222));
#219767=CARTESIAN_POINT('Ctrl Pts',(4.12400838099995,15.2,10.705755348));
#219768=CARTESIAN_POINT('Ctrl Pts',(4.12400838099995,11.6,10.705755348));
#219769=CARTESIAN_POINT('Ctrl Pts',(4.12370002799994,15.2,10.709532648));
#219770=CARTESIAN_POINT('Ctrl Pts',(4.12370002799994,11.6,10.709532648));
#219771=CARTESIAN_POINT('Ctrl Pts',(4.12338843599994,15.2,10.713314109));
#219772=CARTESIAN_POINT('Ctrl Pts',(4.12338843599994,11.6,10.713314109));
#219773=CARTESIAN_POINT('Ctrl Pts',(4.12307359999994,15.2,10.717099726));
#219774=CARTESIAN_POINT('Ctrl Pts',(4.12307359999994,11.6,10.717099726));
#219775=CARTESIAN_POINT('Ctrl Pts',(4.12275551699994,15.2,10.720889492));
#219776=CARTESIAN_POINT('Ctrl Pts',(4.12275551699994,11.6,10.720889492));
#219777=CARTESIAN_POINT('Ctrl Pts',(4.12243418399994,15.2,10.724683406));
#219778=CARTESIAN_POINT('Ctrl Pts',(4.12243418399994,11.6,10.724683406));
#219779=CARTESIAN_POINT('Ctrl Pts',(4.12210959999994,15.2,10.728481465));
#219780=CARTESIAN_POINT('Ctrl Pts',(4.12210959999994,11.6,10.728481465));
#219781=CARTESIAN_POINT('Ctrl Pts',(4.12184733299994,15.2,10.731523226));
#219782=CARTESIAN_POINT('Ctrl Pts',(4.12184733299994,11.6,10.731523226));
#219783=CARTESIAN_POINT('Ctrl Pts',(4.12164916999994,15.2,10.733806412));
#219784=CARTESIAN_POINT('Ctrl Pts',(4.12164916999994,11.6,10.733806412));
#219785=CARTESIAN_POINT('Ctrl Pts',(4.12151640999994,15.2,10.735329364));
#219786=CARTESIAN_POINT('Ctrl Pts',(4.12151640999994,11.6,10.735329364));
#219787=CARTESIAN_POINT('Ctrl Pts',(4.12144986799994,15.2,10.736091048));
#219788=CARTESIAN_POINT('Ctrl Pts',(4.12144986799994,11.6,10.736091048));
#219789=CARTESIAN_POINT('Ctrl Pts',(4.04260911699994,15.2,9.55499537099998));
#219790=CARTESIAN_POINT('Ctrl Pts',(4.0431612978139,15.2,9.55669455126485));
#219791=CARTESIAN_POINT('Ctrl Pts',(4.04372605441455,15.2,9.55844976666689));
#219792=CARTESIAN_POINT('Ctrl Pts',(4.0443024457118,15.2,9.56026027830994));
#219793=CARTESIAN_POINT('Ctrl Pts',(4.04488161665923,15.2,9.56207952115529));
#219794=CARTESIAN_POINT('Ctrl Pts',(4.04547254566134,15.2,9.5639546011486));
#219795=CARTESIAN_POINT('Ctrl Pts',(4.04607433355817,15.2,9.56588480618675));
#219796=CARTESIAN_POINT('Ctrl Pts',(4.04667612140033,15.2,9.56781501104957));
#219797=CARTESIAN_POINT('Ctrl Pts',(4.0472887675309,15.2,9.56980034131573));
#219798=CARTESIAN_POINT('Ctrl Pts',(4.04791140625826,15.2,9.57184010199156));
#219799=CARTESIAN_POINT('Ctrl Pts',(4.04853404498562,15.2,9.57387986266738));
#219800=CARTESIAN_POINT('Ctrl Pts',(4.04916667256298,15.2,9.57597405404105));
#219801=CARTESIAN_POINT('Ctrl Pts',(4.04980844773787,15.2,9.5781219999839));
#219802=CARTESIAN_POINT('Ctrl Pts',(4.05045022297105,15.2,9.58026994612186));
#219803=CARTESIAN_POINT('Ctrl Pts',(4.05110114566863,15.2,9.58247164636916));
#219804=CARTESIAN_POINT('Ctrl Pts',(4.05176039887179,15.2,9.58472644049568));
#219805=CARTESIAN_POINT('Ctrl Pts',(4.05241965201507,15.2,9.58698123441737));
#219806=CARTESIAN_POINT('Ctrl Pts',(4.05308723453836,15.2,9.58928912179259));
#219807=CARTESIAN_POINT('Ctrl Pts',(4.05376235301691,15.2,9.59164945971764));
#219808=CARTESIAN_POINT('Ctrl Pts',(4.05443747149546,15.2,9.59400979764269));
#219809=CARTESIAN_POINT('Ctrl Pts',(4.05512012665439,15.2,9.59642258494925));
#219810=CARTESIAN_POINT('Ctrl Pts',(4.05580954896239,15.2,9.59888719110747));
#219811=CARTESIAN_POINT('Ctrl Pts',(4.05649897133301,15.2,9.60135179748954));
#219812=CARTESIAN_POINT('Ctrl Pts',(4.05719515735446,15.2,9.60386822484468));
#219813=CARTESIAN_POINT('Ctrl Pts',(4.05789736205981,15.2,9.60643585623811));
#219814=CARTESIAN_POINT('Ctrl Pts',(4.05859956670138,15.2,9.60900348739833));
#219815=CARTESIAN_POINT('Ctrl Pts',(4.05930778806454,15.2,9.6116223227904));
#219816=CARTESIAN_POINT('Ctrl Pts',(4.06002130053884,15.2,9.61429176086226));
#219817=CARTESIAN_POINT('Ctrl Pts',(4.06073481301314,15.2,9.61696119893412));
#219818=CARTESIAN_POINT('Ctrl Pts',(4.06145361427035,15.2,9.6196812398353));
#219819=CARTESIAN_POINT('Ctrl Pts',(4.06217699974386,15.2,9.62245129406581));
#219820=CARTESIAN_POINT('Ctrl Pts',(4.06290038521737,15.2,9.6252213482963));
#219821=CARTESIAN_POINT('Ctrl Pts',(4.06362835112202,15.2,9.62804141806142));
#219822=CARTESIAN_POINT('Ctrl Pts',(4.06436021384517,15.2,9.6309109224538));
#219823=CARTESIAN_POINT('Ctrl Pts',(4.06509207663479,15.2,9.63378042710684));
#219824=CARTESIAN_POINT('Ctrl Pts',(4.06582783371649,15.2,9.63669936978133));
#219825=CARTESIAN_POINT('Ctrl Pts',(4.06656681575689,15.2,9.63966718444519));
#219826=CARTESIAN_POINT('Ctrl Pts',(4.06730579773018,15.2,9.64263499883946));
#219827=CARTESIAN_POINT('Ctrl Pts',(4.06804800688995,15.2,9.64565168593773));
#219828=CARTESIAN_POINT('Ctrl Pts',(4.06879278803294,15.2,9.64871669225685));
#219829=CARTESIAN_POINT('Ctrl Pts',(4.06953756917591,15.2,9.65178169857597));
#219830=CARTESIAN_POINT('Ctrl Pts',(4.07028492497895,15.2,9.65489502280677));
#219831=CARTESIAN_POINT('Ctrl Pts',(4.07103421911827,15.2,9.65805612418869));
#219832=CARTESIAN_POINT('Ctrl Pts',(4.07178351332565,15.2,9.66121722585776));
#219833=CARTESIAN_POINT('Ctrl Pts',(4.07253474754156,15.2,9.66442610392306));
#219834=CARTESIAN_POINT('Ctrl Pts',(4.07328730183263,15.2,9.6676822256859));
#219835=CARTESIAN_POINT('Ctrl Pts',(4.07403985605534,15.2,9.67093834715298));
#219836=CARTESIAN_POINT('Ctrl Pts',(4.07479373107359,15.2,9.67424171311334));
#219837=CARTESIAN_POINT('Ctrl Pts',(4.07554832521627,15.2,9.67759179975672));
#219838=CARTESIAN_POINT('Ctrl Pts',(4.07630291935894,15.2,9.68094188640011));
#219839=CARTESIAN_POINT('Ctrl Pts',(4.07705823111172,15.2,9.68433869551952));
#219840=CARTESIAN_POINT('Ctrl Pts',(4.0778136744176,15.2,9.6877817138913));
#219841=CARTESIAN_POINT('Ctrl Pts',(4.07869502498687,15.2,9.69179856886687));
#219842=CARTESIAN_POINT('Ctrl Pts',(4.0795765539041,15.2,9.69587831786509));
#219843=CARTESIAN_POINT('Ctrl Pts',(4.08045735274127,15.2,9.70002016398996));
#219844=CARTESIAN_POINT('Ctrl Pts',(4.08121232313394,15.2,9.70357031762702));
#219845=CARTESIAN_POINT('Ctrl Pts',(4.0819667586368,15.2,9.70716609326345));
#219846=CARTESIAN_POINT('Ctrl Pts',(4.08272010119283,15.2,9.71080699787805));
#219847=CARTESIAN_POINT('Ctrl Pts',(4.08347344381729,15.2,9.71444790282339));
#219848=CARTESIAN_POINT('Ctrl Pts',(4.08422569433591,15.2,9.71813393641028));
#219849=CARTESIAN_POINT('Ctrl Pts',(4.08497631083089,15.2,9.72186461438592));
#219850=CARTESIAN_POINT('Ctrl Pts',(4.0857269272577,15.2,9.72559529202268));
#219851=CARTESIAN_POINT('Ctrl Pts',(4.08647590841874,15.2,9.72937061341363));
#219852=CARTESIAN_POINT('Ctrl Pts',(4.08722272397495,15.2,9.7331901010249));
#219853=CARTESIAN_POINT('Ctrl Pts',(4.08796953953115,15.2,9.73700958863618));
#219854=CARTESIAN_POINT('Ctrl Pts',(4.08871419150124,15.2,9.74087324220468));
#219855=CARTESIAN_POINT('Ctrl Pts',(4.08945616017817,15.2,9.74478059492203));
#219856=CARTESIAN_POINT('Ctrl Pts',(4.09007446743141,15.2,9.74803672230481));
#219857=CARTESIAN_POINT('Ctrl Pts',(4.09069091275409,15.2,9.75132319390142));
#219858=CARTESIAN_POINT('Ctrl Pts',(4.09130520247643,15.2,9.75463974452485));
#219859=CARTESIAN_POINT('Ctrl Pts',(4.09191949219876,15.2,9.75795629514829));
#219860=CARTESIAN_POINT('Ctrl Pts',(4.09253162599326,15.2,9.76130292410859));
#219861=CARTESIAN_POINT('Ctrl Pts',(4.09314131745173,15.2,9.76467936653761));
#219862=CARTESIAN_POINT('Ctrl Pts',(4.0938729471753,15.2,9.7687310973052));
#219863=CARTESIAN_POINT('Ctrl Pts',(4.09460105822206,15.2,9.77282576102715));
#219864=CARTESIAN_POINT('Ctrl Pts',(4.09532516594602,15.2,9.77696290579064));
#219865=CARTESIAN_POINT('Ctrl Pts',(4.09592858907126,15.2,9.78041052655215));
#219866=CARTESIAN_POINT('Ctrl Pts',(4.09652923191043,15.2,9.7838876503437));
#219867=CARTESIAN_POINT('Ctrl Pts',(4.09712681843845,15.2,9.78739401784129));
#219868=CARTESIAN_POINT('Ctrl Pts',(4.09784392231117,15.2,9.79160165906773));
#219869=CARTESIAN_POINT('Ctrl Pts',(4.09855662541143,15.2,9.79585141241445));
#219870=CARTESIAN_POINT('Ctrl Pts',(4.09926446231842,15.2,9.80014284169849));
#219871=CARTESIAN_POINT('Ctrl Pts',(4.09985432637543,15.2,9.80371903257362));
#219872=CARTESIAN_POINT('Ctrl Pts',(4.1004408106376,15.2,9.80732416323955));
#219873=CARTESIAN_POINT('Ctrl Pts',(4.10102365056785,15.2,9.81095798574189));
#219874=CARTESIAN_POINT('Ctrl Pts',(4.10160649049811,15.2,9.81459180824422));
#219875=CARTESIAN_POINT('Ctrl Pts',(4.10218568827552,15.2,9.81825432119145));
#219876=CARTESIAN_POINT('Ctrl Pts',(4.10276098160853,15.2,9.82194527799936));
#219877=CARTESIAN_POINT('Ctrl Pts',(4.10333627487884,15.2,9.82563623440494));
#219878=CARTESIAN_POINT('Ctrl Pts',(4.10390766569836,15.2,9.82935563570384));
#219879=CARTESIAN_POINT('Ctrl Pts',(4.10447489744243,15.2,9.83310323695974));
#219880=CARTESIAN_POINT('Ctrl Pts',(4.10504212924833,15.2,9.83685083862413));
#219881=CARTESIAN_POINT('Ctrl Pts',(4.10560520429875,15.2,9.8406266399436));
#219882=CARTESIAN_POINT('Ctrl Pts',(4.10616387166021,15.2,9.84443040001072));
#219883=CARTESIAN_POINT('Ctrl Pts',(4.1068342725305,15.2,9.84899491234003));
#219884=CARTESIAN_POINT('Ctrl Pts',(4.10749832390359,15.2,9.85359968430348));
#219885=CARTESIAN_POINT('Ctrl Pts',(4.10815560605519,15.2,9.85824430770765));
#219886=CARTESIAN_POINT('Ctrl Pts',(4.10903198219763,15.2,9.86443713849133));
#219887=CARTESIAN_POINT('Ctrl Pts',(4.1098963189273,15.2,9.87070080765411));
#219888=CARTESIAN_POINT('Ctrl Pts',(4.11074763902639,15.2,9.87703435845896));
#219889=CARTESIAN_POINT('Ctrl Pts',(4.11149254413484,15.2,9.88257621557503));
#219890=CARTESIAN_POINT('Ctrl Pts',(4.11222748327364,15.2,9.88817157693104));
#219891=CARTESIAN_POINT('Ctrl Pts',(4.1129518187843,15.2,9.8938198062443));
#219892=CARTESIAN_POINT('Ctrl Pts',(4.11346920122746,15.2,9.89785425525118));
#219893=CARTESIAN_POINT('Ctrl Pts',(4.1139811724329,15.2,9.90191568062968));
#219894=CARTESIAN_POINT('Ctrl Pts',(4.11448750668373,15.2,9.90600385122352));
#219895=CARTESIAN_POINT('Ctrl Pts',(4.11499384098974,15.2,9.91009202226297));
#219896=CARTESIAN_POINT('Ctrl Pts',(4.11549453634031,15.2,9.91420694031595));
#219897=CARTESIAN_POINT('Ctrl Pts',(4.11598937141023,15.2,9.9183483789249));
#219898=CARTESIAN_POINT('Ctrl Pts',(4.11648420648016,15.2,9.92248981753384));
#219899=CARTESIAN_POINT('Ctrl Pts',(4.11697317774711,15.2,9.92665777781657));
#219900=CARTESIAN_POINT('Ctrl Pts',(4.11745606874388,15.2,9.93085203649644));
#219901=CARTESIAN_POINT('Ctrl Pts',(4.11793895974064,15.2,9.93504629517632));
#219902=CARTESIAN_POINT('Ctrl Pts',(4.11841576885771,15.2,9.93926685075148));
#219903=CARTESIAN_POINT('Ctrl Pts',(4.11888627976082,15.2,9.94351348422233));
#219904=CARTESIAN_POINT('Ctrl Pts',(4.11926268850381,15.2,9.94691079118418));
#219905=CARTESIAN_POINT('Ctrl Pts',(4.11963506594078,15.2,9.95032478571192));
#219906=CARTESIAN_POINT('Ctrl Pts',(4.12000330423836,15.2,9.95375535928887));
#219907=CARTESIAN_POINT('Ctrl Pts',(4.12046360208525,15.2,9.95804357602636));
#219908=CARTESIAN_POINT('Ctrl Pts',(4.12091743116886,15.2,9.96235769282965));
#219909=CARTESIAN_POINT('Ctrl Pts',(4.12136458230185,15.2,9.96669749652046));
#219910=CARTESIAN_POINT('Ctrl Pts',(4.12172230317899,15.2,9.97016933918929));
#219911=CARTESIAN_POINT('Ctrl Pts',(4.12207575009686,15.2,9.97365761854002));
#219912=CARTESIAN_POINT('Ctrl Pts',(4.12242481701305,15.2,9.9771622276969));
#219913=CARTESIAN_POINT('Ctrl Pts',(4.12286115069396,15.2,9.98154298950111));
#219914=CARTESIAN_POINT('Ctrl Pts',(4.12329064037748,15.2,9.98594926316156));
#219915=CARTESIAN_POINT('Ctrl Pts',(4.12371308398896,15.2,9.99038083670192));
#219916=CARTESIAN_POINT('Ctrl Pts',(4.12413552760045,15.2,9.99481241024228));
#219917=CARTESIAN_POINT('Ctrl Pts',(4.12455092426453,15.2,9.99926928274387));
#219918=CARTESIAN_POINT('Ctrl Pts',(4.12495907301641,15.2,10.0037512438058));
#219919=CARTESIAN_POINT('Ctrl Pts',(4.1252855920357,15.2,10.0073368128508));
#219920=CARTESIAN_POINT('Ctrl Pts',(4.1256074734989,15.2,10.0109384374676));
#219921=CARTESIAN_POINT('Ctrl Pts',(4.12592461579348,15.2,10.0145560118331));
#219922=CARTESIAN_POINT('Ctrl Pts',(4.12624175804484,15.2,10.0181735857056));
#219923=CARTESIAN_POINT('Ctrl Pts',(4.12655416131349,15.2,10.0218071093511));
#219924=CARTESIAN_POINT('Ctrl Pts',(4.12686172623311,15.2,10.0254564747184));
#219925=CARTESIAN_POINT('Ctrl Pts',(4.12724618241406,15.2,10.0300181818004));
#219926=CARTESIAN_POINT('Ctrl Pts',(4.12762307822029,15.2,10.034604643732));
#219927=CARTESIAN_POINT('Ctrl Pts',(4.1279922212081,15.2,10.0392156531974));
#219928=CARTESIAN_POINT('Ctrl Pts',(4.12828753561444,15.2,10.0429044609708));
#219929=CARTESIAN_POINT('Ctrl Pts',(4.12857789050102,15.2,10.0466089790177));
#219930=CARTESIAN_POINT('Ctrl Pts',(4.12886318557161,15.2,10.0503291028332));
#219931=CARTESIAN_POINT('Ctrl Pts',(4.12914848060332,15.2,10.0540492261418));
#219932=CARTESIAN_POINT('Ctrl Pts',(4.12942871931069,15.2,10.0577849556955));
#219933=CARTESIAN_POINT('Ctrl Pts',(4.12970380251076,15.2,10.0615361869434));
#219934=CARTESIAN_POINT('Ctrl Pts',(4.13004765653896,15.2,10.0662252263866));
#219935=CARTESIAN_POINT('Ctrl Pts',(4.13038345989827,15.2,10.0709384862537));
#219936=CARTESIAN_POINT('Ctrl Pts',(4.13071102698312,15.2,10.0756757672474));
#219937=CARTESIAN_POINT('Ctrl Pts',(4.13103859406796,15.2,10.080413048241));
#219938=CARTESIAN_POINT('Ctrl Pts',(4.13135792418885,15.2,10.0851743487277));
#219939=CARTESIAN_POINT('Ctrl Pts',(4.1316688380083,15.2,10.0899594682416));
#219940=CARTESIAN_POINT('Ctrl Pts',(4.13191756907742,15.2,10.0937875640614));
#219941=CARTESIAN_POINT('Ctrl Pts',(4.13216091357368,15.2,10.0976309054384));
#219942=CARTESIAN_POINT('Ctrl Pts',(4.13239878053052,15.2,10.1014893893725));
#219943=CARTESIAN_POINT('Ctrl Pts',(4.13281504765639,15.2,10.1082417354685));
#219944=CARTESIAN_POINT('Ctrl Pts',(4.13321453556633,15.2,10.1150404585417));
#219945=CARTESIAN_POINT('Ctrl Pts',(4.13359676772372,15.2,10.121885016697));
#219946=CARTESIAN_POINT('Ctrl Pts',(4.13392439532547,15.2,10.1277517815153));
#219947=CARTESIAN_POINT('Ctrl Pts',(4.13423934530897,15.2,10.1336522210044));
#219948=CARTESIAN_POINT('Ctrl Pts',(4.13454131807455,15.2,10.1395860016634));
#219949=CARTESIAN_POINT('Ctrl Pts',(4.13474263322417,15.2,10.1435418548971));
#219950=CARTESIAN_POINT('Ctrl Pts',(4.13493818205335,15.2,10.1475125256216));
#219951=CARTESIAN_POINT('Ctrl Pts',(4.13512787848317,15.2,10.1514979149806));
#219952=CARTESIAN_POINT('Ctrl Pts',(4.13531757493884,15.2,10.1554833048825));
#219953=CARTESIAN_POINT('Ctrl Pts',(4.13550141856163,15.2,10.1594834133972));
#219954=CARTESIAN_POINT('Ctrl Pts',(4.13567932307072,15.2,10.163498143173));
#219955=CARTESIAN_POINT('Ctrl Pts',(4.13585722755556,15.2,10.1675128724018));
#219956=CARTESIAN_POINT('Ctrl Pts',(4.13602919410229,15.2,10.1715422222205));
#219957=CARTESIAN_POINT('Ctrl Pts',(4.13619513781135,15.2,10.1755860949445));
#219958=CARTESIAN_POINT('Ctrl Pts',(4.13640256746461,15.2,10.1806409362627));
#219959=CARTESIAN_POINT('Ctrl Pts',(4.13660058633153,15.2,10.1857184699899));
#219960=CARTESIAN_POINT('Ctrl Pts',(4.13678903272092,15.2,10.1908185071415));
#219961=CARTESIAN_POINT('Ctrl Pts',(4.13693978984065,15.2,10.1948985370852));
#219962=CARTESIAN_POINT('Ctrl Pts',(4.13708442016443,15.2,10.1989929704685));
#219963=CARTESIAN_POINT('Ctrl Pts',(4.13722284201169,15.2,10.2031017086212));
#219964=CARTESIAN_POINT('Ctrl Pts',(4.13739586931133,15.2,10.2082376310322));
#219965=CARTESIAN_POINT('Ctrl Pts',(4.13755919523751,15.2,10.2133959065313));
#219966=CARTESIAN_POINT('Ctrl Pts',(4.13771266252837,15.2,10.2185763486859));
#219967=CARTESIAN_POINT('Ctrl Pts',(4.13783543635102,15.2,10.2227207020708));
#219968=CARTESIAN_POINT('Ctrl Pts',(4.13795190084116,15.2,10.2268792417482));
#219969=CARTESIAN_POINT('Ctrl Pts',(4.13806197599924,15.2,10.2310518736839));
#219970=CARTESIAN_POINT('Ctrl Pts',(4.13817205117233,15.2,10.2352245061882));
#219971=CARTESIAN_POINT('Ctrl Pts',(4.13827573674334,15.2,10.2394112302085));
#219972=CARTESIAN_POINT('Ctrl Pts',(4.13837295453071,15.2,10.2436119510929));
#219973=CARTESIAN_POINT('Ctrl Pts',(4.13847017230483,15.2,10.247812671405));
#219974=CARTESIAN_POINT('Ctrl Pts',(4.13856092142448,15.2,10.2520273907232));
#219975=CARTESIAN_POINT('Ctrl Pts',(4.13864512525136,15.2,10.2562560121544));
#219976=CARTESIAN_POINT('Ctrl Pts',(4.13875038004356,15.2,10.2615417893755));
#219977=CARTESIAN_POINT('Ctrl Pts',(4.13884540651049,15.2,10.2668492926638));
#219978=CARTESIAN_POINT('Ctrl Pts',(4.13893005546937,15.2,10.2721783373849));
#219979=CARTESIAN_POINT('Ctrl Pts',(4.13904856401364,15.2,10.2796390001105));
#219980=CARTESIAN_POINT('Ctrl Pts',(4.13914672978642,15.2,10.287141886239));
#219981=CARTESIAN_POINT('Ctrl Pts',(4.13922415299519,15.2,10.2946865008442));
#219982=CARTESIAN_POINT('Ctrl Pts',(4.1392794552863,15.2,10.3000755111925));
#219983=CARTESIAN_POINT('Ctrl Pts',(4.13932417331936,15.2,10.3054858112375));
#219984=CARTESIAN_POINT('Ctrl Pts',(4.13935816248546,15.2,10.3109172233219));
#219985=CARTESIAN_POINT('Ctrl Pts',(4.13940574731505,15.2,10.3185211997665));
#219986=CARTESIAN_POINT('Ctrl Pts',(4.13943230593189,15.2,10.3261665530574));
#219987=CARTESIAN_POINT('Ctrl Pts',(4.13943744626615,15.2,10.3338527982568));
#219988=CARTESIAN_POINT('Ctrl Pts',(4.13944038360036,15.2,10.3382449388837));
#219989=CARTESIAN_POINT('Ctrl Pts',(4.13943632774502,15.2,10.3426504317452));
#219990=CARTESIAN_POINT('Ctrl Pts',(4.13942520696664,15.2,10.3470691870416));
#219991=CARTESIAN_POINT('Ctrl Pts',(4.13941408618825,15.2,10.351487942338));
#219992=CARTESIAN_POINT('Ctrl Pts',(4.13939590123127,15.2,10.3559199599165));
#219993=CARTESIAN_POINT('Ctrl Pts',(4.1393705805625,15.2,10.3603651504934));
#219994=CARTESIAN_POINT('Ctrl Pts',(4.13935159006264,15.2,10.3636990431232));
#219995=CARTESIAN_POINT('Ctrl Pts',(4.1393285859122,15.2,10.3670403445181));
#219996=CARTESIAN_POINT('Ctrl Pts',(4.13930153845303,15.2,10.3703890183979));
#219997=CARTESIAN_POINT('Ctrl Pts',(4.13927449099386,15.2,10.3737376922777));
#219998=CARTESIAN_POINT('Ctrl Pts',(4.13924340101181,15.2,10.3770937391549));
#219999=CARTESIAN_POINT('Ctrl Pts',(4.13920823847107,15.2,10.3804571194083));
#220000=CARTESIAN_POINT('Ctrl Pts',(4.13917307593033,15.2,10.3838204996618));
#220001=CARTESIAN_POINT('Ctrl Pts',(4.13913384128174,15.2,10.387191214256));
#220002=CARTESIAN_POINT('Ctrl Pts',(4.13909050528331,15.2,10.3905692264666));
#220003=CARTESIAN_POINT('Ctrl Pts',(4.13903272394683,15.2,10.3950732431565));
#220004=CARTESIAN_POINT('Ctrl Pts',(4.13896765179283,15.2,10.3995902342007));
#220005=CARTESIAN_POINT('Ctrl Pts',(4.13889521978813,15.2,10.4041201082823));
#220006=CARTESIAN_POINT('Ctrl Pts',(4.13884089578953,15.2,10.4075175135348));
#220007=CARTESIAN_POINT('Ctrl Pts',(4.13878243343915,15.2,10.4109221665295));
#220008=CARTESIAN_POINT('Ctrl Pts',(4.13871980202115,15.2,10.4143340304101));
#220009=CARTESIAN_POINT('Ctrl Pts',(4.1386362934676,15.2,10.4188831820444));
#220010=CARTESIAN_POINT('Ctrl Pts',(4.13854537695219,15.2,10.4234451519036));
#220011=CARTESIAN_POINT('Ctrl Pts',(4.13844698301628,15.2,10.4280198545844));
#220012=CARTESIAN_POINT('Ctrl Pts',(4.138373187561,15.2,10.4314508817508));
#220013=CARTESIAN_POINT('Ctrl Pts',(4.138295186781,15.2,10.4348890705417));
#220014=CARTESIAN_POINT('Ctrl Pts',(4.1382129537429,15.2,10.4383343837489));
#220015=CARTESIAN_POINT('Ctrl Pts',(4.13813072068985,15.2,10.4417796975819));
#220016=CARTESIAN_POINT('Ctrl Pts',(4.13804425424396,15.2,10.4452321364837));
#220017=CARTESIAN_POINT('Ctrl Pts',(4.13795352718853,15.2,10.4486916642374));
#220018=CARTESIAN_POINT('Ctrl Pts',(4.13783255780875,15.2,10.4533043668616));
#220019=CARTESIAN_POINT('Ctrl Pts',(4.13770401406731,15.2,10.4579296708271));
#220020=CARTESIAN_POINT('Ctrl Pts',(4.13756783196673,15.2,10.4625674902468));
#220021=CARTESIAN_POINT('Ctrl Pts',(4.13746569538666,15.2,10.4660458549695));
#220022=CARTESIAN_POINT('Ctrl Pts',(4.13735926044091,15.2,10.4695312592136));
#220023=CARTESIAN_POINT('Ctrl Pts',(4.13724850327864,15.2,10.4730236678777));
#220024=CARTESIAN_POINT('Ctrl Pts',(4.13713774611637,15.2,10.4765160765419));
#220025=CARTESIAN_POINT('Ctrl Pts',(4.13702266387107,15.2,10.4800154892972));
#220026=CARTESIAN_POINT('Ctrl Pts',(4.13690323179267,15.2,10.4835218690439));
#220027=CARTESIAN_POINT('Ctrl Pts',(4.13678379969258,15.2,10.4870282494276));
#220028=CARTESIAN_POINT('Ctrl Pts',(4.13666001659125,15.2,10.4905415976715));
#220029=CARTESIAN_POINT('Ctrl Pts',(4.13653185703036,15.2,10.4940618780174));
#220030=CARTESIAN_POINT('Ctrl Pts',(4.13640369749276,15.2,10.4975821577237));
#220031=CARTESIAN_POINT('Ctrl Pts',(4.13627116044248,15.2,10.5011093691015));
#220032=CARTESIAN_POINT('Ctrl Pts',(4.13613421998177,15.2,10.5046434769421));
#220033=CARTESIAN_POINT('Ctrl Pts',(4.13599727952106,15.2,10.5081775847827));
#220034=CARTESIAN_POINT('Ctrl Pts',(4.13585593624577,15.2,10.511718587915));
#220035=CARTESIAN_POINT('Ctrl Pts',(4.13571016329234,15.2,10.5152664516618));
#220036=CARTESIAN_POINT('Ctrl Pts',(4.13556439033892,15.2,10.5188143154085));
#220037=CARTESIAN_POINT('Ctrl Pts',(4.13541418817769,15.2,10.522369040246));
#220038=CARTESIAN_POINT('Ctrl Pts',(4.13525953026665,15.2,10.5259305894916));
#220039=CARTESIAN_POINT('Ctrl Pts',(4.1351048723556,15.2,10.5294921387373));
#220040=CARTESIAN_POINT('Ctrl Pts',(4.1349457595614,15.2,10.5330605128742));
#220041=CARTESIAN_POINT('Ctrl Pts',(4.13478216602607,15.2,10.5366356761187));
#220042=CARTESIAN_POINT('Ctrl Pts',(4.13461857249073,15.2,10.5402108393632));
#220043=CARTESIAN_POINT('Ctrl Pts',(4.13445049713071,15.2,10.5437927921822));
#220044=CARTESIAN_POINT('Ctrl Pts',(4.13427791659593,15.2,10.5473814989676));
#220045=CARTESIAN_POINT('Ctrl Pts',(4.13410533602979,15.2,10.5509702064049));
#220046=CARTESIAN_POINT('Ctrl Pts',(4.13392824853739,15.2,10.5545656691775));
#220047=CARTESIAN_POINT('Ctrl Pts',(4.13374663092704,15.2,10.5581678505352));
#220048=CARTESIAN_POINT('Ctrl Pts',(4.13356501334969,15.2,10.5617700312386));
#220049=CARTESIAN_POINT('Ctrl Pts',(4.13337886303283,15.2,10.5653789302828));
#220050=CARTESIAN_POINT('Ctrl Pts',(4.13318815748803,15.2,10.5689945137079));
#220051=CARTESIAN_POINT('Ctrl Pts',(4.13293388343986,15.2,10.573815291389));
#220052=CARTESIAN_POINT('Ctrl Pts',(4.1326715094077,15.2,10.5786479524786));
#220053=CARTESIAN_POINT('Ctrl Pts',(4.13240097626368,15.2,10.5834924126374));
#220054=CARTESIAN_POINT('Ctrl Pts',(4.13219807639645,15.2,10.5871257579214));
#220055=CARTESIAN_POINT('Ctrl Pts',(4.13199058845455,15.2,10.5907657411383));
#220056=CARTESIAN_POINT('Ctrl Pts',(4.13177848604621,15.2,10.5944123269217));
#220057=CARTESIAN_POINT('Ctrl Pts',(4.13156638359935,15.2,10.5980589133674));
#220058=CARTESIAN_POINT('Ctrl Pts',(4.13134966745119,15.2,10.6017121030983));
#220059=CARTESIAN_POINT('Ctrl Pts',(4.13112831396005,15.2,10.6053718605478));
#220060=CARTESIAN_POINT('Ctrl Pts',(4.13090696050913,15.2,10.6090316173324));
#220061=CARTESIAN_POINT('Ctrl Pts',(4.13068096965899,15.2,10.6126979435431));
#220062=CARTESIAN_POINT('Ctrl Pts',(4.13045031673864,15.2,10.6163708024689));
#220063=CARTESIAN_POINT('Ctrl Pts',(4.13006589519075,15.2,10.6224922342344));
#220064=CARTESIAN_POINT('Ctrl Pts',(4.12966852321958,15.2,10.6286318142261));
#220065=CARTESIAN_POINT('Ctrl Pts',(4.12925809245462,15.2,10.6347893840887));
#220066=CARTESIAN_POINT('Ctrl Pts',(4.12901183400459,15.2,10.638483925872));
#220067=CARTESIAN_POINT('Ctrl Pts',(4.12876087461315,15.2,10.642184944855));
#220068=CARTESIAN_POINT('Ctrl Pts',(4.12850519070536,15.2,10.6458924065958));
#220069=CARTESIAN_POINT('Ctrl Pts',(4.12824950679757,15.2,10.6495998683367));
#220070=CARTESIAN_POINT('Ctrl Pts',(4.12798909899133,15.2,10.6533137731049));
#220071=CARTESIAN_POINT('Ctrl Pts',(4.12772394249973,15.2,10.6570340857783));
#220072=CARTESIAN_POINT('Ctrl Pts',(4.12745878600814,15.2,10.6607543984518));
#220073=CARTESIAN_POINT('Ctrl Pts',(4.12718888029147,15.2,10.6644811186819));
#220074=CARTESIAN_POINT('Ctrl Pts',(4.12691420330023,15.2,10.6682142110215));
#220075=CARTESIAN_POINT('Ctrl Pts',(4.12663952630898,15.2,10.6719473033612));
#220076=CARTESIAN_POINT('Ctrl Pts',(4.12636007615346,15.2,10.6756867686784));
#220077=CARTESIAN_POINT('Ctrl Pts',(4.12607583428921,15.2,10.6794325760418));
#220078=CARTESIAN_POINT('Ctrl Pts',(4.12569684510245,15.2,10.6844269863132));
#220079=CARTESIAN_POINT('Ctrl Pts',(4.12530933671467,15.2,10.6894326749582));
#220080=CARTESIAN_POINT('Ctrl Pts',(4.12491325519252,15.2,10.6944495576769));
#220081=CARTESIAN_POINT('Ctrl Pts',(4.12461619407789,15.2,10.698212219374));
#220082=CARTESIAN_POINT('Ctrl Pts',(4.1243143083233,15.2,10.7019811777401));
#220083=CARTESIAN_POINT('Ctrl Pts',(4.12400757229137,15.2,10.7057563909534));
#220084=CARTESIAN_POINT('Ctrl Pts',(4.1234963455529,15.2,10.7120484132042));
#220085=CARTESIAN_POINT('Ctrl Pts',(4.12297163538237,15.2,10.7183577989103));
#220086=CARTESIAN_POINT('Ctrl Pts',(4.12243337123359,15.2,10.7246844426642));
#220087=CARTESIAN_POINT('Ctrl Pts',(4.12211041275606,15.2,10.7284804287786));
#220088=CARTESIAN_POINT('Ctrl Pts',(4.12178257806039,15.2,10.7322826273081));
#220089=CARTESIAN_POINT('Ctrl Pts',(4.12144986799994,15.2,10.736091048));
#220090=CARTESIAN_POINT('Ctrl Pts',(4.04260911699994,12.2,9.55499537099998));
#220091=CARTESIAN_POINT('Ctrl Pts',(4.0431612978139,12.2,9.55669455126485));
#220092=CARTESIAN_POINT('Ctrl Pts',(4.04372605441455,12.2,9.55844976666689));
#220093=CARTESIAN_POINT('Ctrl Pts',(4.0443024457118,12.2,9.56026027830994));
#220094=CARTESIAN_POINT('Ctrl Pts',(4.04488161665923,12.2,9.56207952115529));
#220095=CARTESIAN_POINT('Ctrl Pts',(4.04547254566134,12.2,9.5639546011486));
#220096=CARTESIAN_POINT('Ctrl Pts',(4.04607433355817,12.2,9.56588480618675));
#220097=CARTESIAN_POINT('Ctrl Pts',(4.04667612140033,12.2,9.56781501104957));
#220098=CARTESIAN_POINT('Ctrl Pts',(4.0472887675309,12.2,9.56980034131573));
#220099=CARTESIAN_POINT('Ctrl Pts',(4.04791140625826,12.2,9.57184010199156));
#220100=CARTESIAN_POINT('Ctrl Pts',(4.04853404498562,12.2,9.57387986266738));
#220101=CARTESIAN_POINT('Ctrl Pts',(4.04916667256298,12.2,9.57597405404106));
#220102=CARTESIAN_POINT('Ctrl Pts',(4.04980844773787,12.2,9.5781219999839));
#220103=CARTESIAN_POINT('Ctrl Pts',(4.05045022297105,12.2,9.58026994612186));
#220104=CARTESIAN_POINT('Ctrl Pts',(4.05110114566863,12.2,9.58247164636916));
#220105=CARTESIAN_POINT('Ctrl Pts',(4.05176039887179,12.2,9.58472644049568));
#220106=CARTESIAN_POINT('Ctrl Pts',(4.05241965201507,12.2,9.58698123441737));
#220107=CARTESIAN_POINT('Ctrl Pts',(4.05308723453836,12.2,9.58928912179259));
#220108=CARTESIAN_POINT('Ctrl Pts',(4.05376235301691,12.2,9.59164945971764));
#220109=CARTESIAN_POINT('Ctrl Pts',(4.05443747149546,12.2,9.59400979764269));
#220110=CARTESIAN_POINT('Ctrl Pts',(4.05512012665439,12.2,9.59642258494925));
#220111=CARTESIAN_POINT('Ctrl Pts',(4.05580954896239,12.2,9.59888719110747));
#220112=CARTESIAN_POINT('Ctrl Pts',(4.05649897133301,12.2,9.60135179748954));
#220113=CARTESIAN_POINT('Ctrl Pts',(4.05719515735446,12.2,9.60386822484468));
#220114=CARTESIAN_POINT('Ctrl Pts',(4.05789736205981,12.2,9.60643585623811));
#220115=CARTESIAN_POINT('Ctrl Pts',(4.05859956670138,12.2,9.60900348739833));
#220116=CARTESIAN_POINT('Ctrl Pts',(4.05930778806454,12.2,9.6116223227904));
#220117=CARTESIAN_POINT('Ctrl Pts',(4.06002130053884,12.2,9.61429176086226));
#220118=CARTESIAN_POINT('Ctrl Pts',(4.06073481301314,12.2,9.61696119893412));
#220119=CARTESIAN_POINT('Ctrl Pts',(4.06145361427035,12.2,9.6196812398353));
#220120=CARTESIAN_POINT('Ctrl Pts',(4.06217699974386,12.2,9.62245129406581));
#220121=CARTESIAN_POINT('Ctrl Pts',(4.06290038521737,12.2,9.6252213482963));
#220122=CARTESIAN_POINT('Ctrl Pts',(4.06362835112202,12.2,9.62804141806142));
#220123=CARTESIAN_POINT('Ctrl Pts',(4.06436021384517,12.2,9.6309109224538));
#220124=CARTESIAN_POINT('Ctrl Pts',(4.06509207663479,12.2,9.63378042710684));
#220125=CARTESIAN_POINT('Ctrl Pts',(4.06582783371649,12.2,9.63669936978133));
#220126=CARTESIAN_POINT('Ctrl Pts',(4.06656681575689,12.2,9.63966718444519));
#220127=CARTESIAN_POINT('Ctrl Pts',(4.06730579773018,12.2,9.64263499883946));
#220128=CARTESIAN_POINT('Ctrl Pts',(4.06804800688995,12.2,9.64565168593774));
#220129=CARTESIAN_POINT('Ctrl Pts',(4.06879278803294,12.2,9.64871669225687));
#220130=CARTESIAN_POINT('Ctrl Pts',(4.06953756917592,12.2,9.65178169857599));
#220131=CARTESIAN_POINT('Ctrl Pts',(4.07028492497895,12.2,9.65489502280677));
#220132=CARTESIAN_POINT('Ctrl Pts',(4.07103421911827,12.2,9.65805612418869));
#220133=CARTESIAN_POINT('Ctrl Pts',(4.07178351332565,12.2,9.66121722585776));
#220134=CARTESIAN_POINT('Ctrl Pts',(4.07253474754156,12.2,9.66442610392306));
#220135=CARTESIAN_POINT('Ctrl Pts',(4.07328730183263,12.2,9.6676822256859));
#220136=CARTESIAN_POINT('Ctrl Pts',(4.07403985605534,12.2,9.67093834715298));
#220137=CARTESIAN_POINT('Ctrl Pts',(4.07479373107359,12.2,9.67424171311334));
#220138=CARTESIAN_POINT('Ctrl Pts',(4.07554832521627,12.2,9.67759179975672));
#220139=CARTESIAN_POINT('Ctrl Pts',(4.07630291935894,12.2,9.68094188640011));
#220140=CARTESIAN_POINT('Ctrl Pts',(4.07705823111172,12.2,9.68433869551952));
#220141=CARTESIAN_POINT('Ctrl Pts',(4.0778136744176,12.2,9.6877817138913));
#220142=CARTESIAN_POINT('Ctrl Pts',(4.0785691177921,12.2,9.69122473257582));
#220143=CARTESIAN_POINT('Ctrl Pts',(4.07932469217746,12.2,9.6947139586617));
#220144=CARTESIAN_POINT('Ctrl Pts',(4.08007982558966,12.2,9.69824889161697));
#220145=CARTESIAN_POINT('Ctrl Pts',(4.08083495893326,12.2,9.70178382425116));
#220146=CARTESIAN_POINT('Ctrl Pts',(4.08158964903567,12.2,9.70536446135665));
#220147=CARTESIAN_POINT('Ctrl Pts',(4.08234334125828,12.2,9.70899030897491));
#220148=CARTESIAN_POINT('Ctrl Pts',(4.0830970334809,12.2,9.71261615659317));
#220149=CARTESIAN_POINT('Ctrl Pts',(4.08384972224196,12.2,9.71628721561753));
#220150=CARTESIAN_POINT('Ctrl Pts',(4.08460086866894,12.2,9.72000299758223));
#220151=CARTESIAN_POINT('Ctrl Pts',(4.08535201516417,12.2,9.72371877988444));
#220152=CARTESIAN_POINT('Ctrl Pts',(4.08610161564083,12.2,9.72747928717927));
#220153=CARTESIAN_POINT('Ctrl Pts',(4.08684913834809,12.2,9.73128404013963));
#220154=CARTESIAN_POINT('Ctrl Pts',(4.08759666098745,12.2,9.73508879275439));
#220155=CARTESIAN_POINT('Ctrl Pts',(4.08834210619891,12.2,9.738937788817));
#220156=CARTESIAN_POINT('Ctrl Pts',(4.08908495475862,12.2,9.74283056244335));
#220157=CARTESIAN_POINT('Ctrl Pts',(4.08982780331833,12.2,9.74672333606969));
#220158=CARTESIAN_POINT('Ctrl Pts',(4.09056805483641,12.2,9.75065988392134));
#220159=CARTESIAN_POINT('Ctrl Pts',(4.09130520247643,12.2,9.75463974452485));
#220160=CARTESIAN_POINT('Ctrl Pts',(4.09191949219876,12.2,9.75795629514829));
#220161=CARTESIAN_POINT('Ctrl Pts',(4.09253162599326,12.2,9.76130292410859));
#220162=CARTESIAN_POINT('Ctrl Pts',(4.09314131745173,12.2,9.76467936653761));
#220163=CARTESIAN_POINT('Ctrl Pts',(4.0938729471753,12.2,9.7687310973052));
#220164=CARTESIAN_POINT('Ctrl Pts',(4.09460105822206,12.2,9.77282576102715));
#220165=CARTESIAN_POINT('Ctrl Pts',(4.09532516594602,12.2,9.77696290579064));
#220166=CARTESIAN_POINT('Ctrl Pts',(4.09592858907126,12.2,9.78041052655215));
#220167=CARTESIAN_POINT('Ctrl Pts',(4.09652923191043,12.2,9.7838876503437));
#220168=CARTESIAN_POINT('Ctrl Pts',(4.09712681843845,12.2,9.78739401784129));
#220169=CARTESIAN_POINT('Ctrl Pts',(4.09772440496648,12.2,9.79090038533889));
#220170=CARTESIAN_POINT('Ctrl Pts',(4.09831893554042,12.2,9.794435997949));
#220171=CARTESIAN_POINT('Ctrl Pts',(4.09891014043131,12.2,9.79800060152789));
#220172=CARTESIAN_POINT('Ctrl Pts',(4.09950134532219,12.2,9.80156520510676));
#220173=CARTESIAN_POINT('Ctrl Pts',(4.10008922479487,12.2,9.80515879973693));
#220174=CARTESIAN_POINT('Ctrl Pts',(4.10067351146172,12.2,9.80878113626318));
#220175=CARTESIAN_POINT('Ctrl Pts',(4.10125779812857,12.2,9.81240347278944));
#220176=CARTESIAN_POINT('Ctrl Pts',(4.10183849408423,12.2,9.81605454833873));
#220177=CARTESIAN_POINT('Ctrl Pts',(4.10241533894554,12.2,9.81973411826777));
#220178=CARTESIAN_POINT('Ctrl Pts',(4.10299218380685,12.2,9.82341368819682));
#220179=CARTESIAN_POINT('Ctrl Pts',(4.10356517649705,12.2,9.82712175171432));
#220180=CARTESIAN_POINT('Ctrl Pts',(4.10413406149964,12.2,9.83085806277287));
#220181=CARTESIAN_POINT('Ctrl Pts',(4.10470294650224,12.2,9.83459437383143));
#220182=CARTESIAN_POINT('Ctrl Pts',(4.10526772542774,12.2,9.83835893475549));
#220183=CARTESIAN_POINT('Ctrl Pts',(4.10582814473329,12.2,9.84215150149158));
#220184=CARTESIAN_POINT('Ctrl Pts',(4.10638856403884,12.2,9.84594406822768));
#220185=CARTESIAN_POINT('Ctrl Pts',(4.10694462623665,12.2,9.84976464218446));
#220186=CARTESIAN_POINT('Ctrl Pts',(4.10749608297526,12.2,9.85361298324368));
#220187=CARTESIAN_POINT('Ctrl Pts',(4.10804753971386,12.2,9.8574613243029));
#220188=CARTESIAN_POINT('Ctrl Pts',(4.10859439337452,12.2,9.86133743518729));
#220189=CARTESIAN_POINT('Ctrl Pts',(4.10913639927704,12.2,9.86524107602204));
#220190=CARTESIAN_POINT('Ctrl Pts',(4.10967840517957,12.2,9.86914471685678));
#220191=CARTESIAN_POINT('Ctrl Pts',(4.11021556395721,12.2,9.87307588915198));
#220192=CARTESIAN_POINT('Ctrl Pts',(4.11074763902639,12.2,9.87703435845895));
#220193=CARTESIAN_POINT('Ctrl Pts',(4.1113861290862,12.2,9.88178452145474));
#220194=CARTESIAN_POINT('Ctrl Pts',(4.11201729881327,12.2,9.88657399363908));
#220195=CARTESIAN_POINT('Ctrl Pts',(4.11264074220761,12.2,9.89140237454526));
#220196=CARTESIAN_POINT('Ctrl Pts',(4.11316027838845,12.2,9.89542602544662));
#220197=CARTESIAN_POINT('Ctrl Pts',(4.11367445135847,12.2,9.89947669700703));
#220198=CARTESIAN_POINT('Ctrl Pts',(4.11418303149968,12.2,9.9035541604977));
#220199=CARTESIAN_POINT('Ctrl Pts',(4.1146916116409,12.2,9.90763162398837));
#220200=CARTESIAN_POINT('Ctrl Pts',(4.11519459879996,12.2,9.9117358788221));
#220201=CARTESIAN_POINT('Ctrl Pts',(4.1156917690083,12.2,9.91586670055825));
#220202=CARTESIAN_POINT('Ctrl Pts',(4.11608950519664,12.2,9.91917135812728));
#220203=CARTESIAN_POINT('Ctrl Pts',(4.11648351887066,12.2,9.92249301716767));
#220204=CARTESIAN_POINT('Ctrl Pts',(4.11687369511375,12.2,9.92583156479579));
#220205=CARTESIAN_POINT('Ctrl Pts',(4.11726387130368,12.2,9.92917011196903));
#220206=CARTESIAN_POINT('Ctrl Pts',(4.11765021167921,12.2,9.93252554748861));
#220207=CARTESIAN_POINT('Ctrl Pts',(4.11803260498303,12.2,9.93589775550596));
#220208=CARTESIAN_POINT('Ctrl Pts',(4.11841499833896,12.2,9.93926996398276));
#220209=CARTESIAN_POINT('Ctrl Pts',(4.11879344282729,12.2,9.94265894858054));
#220210=CARTESIAN_POINT('Ctrl Pts',(4.1191678285695,12.2,9.94606459232342));
#220211=CARTESIAN_POINT('Ctrl Pts',(4.11954221426071,12.2,9.94947023560229));
#220212=CARTESIAN_POINT('Ctrl Pts',(4.11991254320243,12.2,9.95289254099839));
#220213=CARTESIAN_POINT('Ctrl Pts',(4.12027870522832,12.2,9.95633139499395));
#220214=CARTESIAN_POINT('Ctrl Pts',(4.1206448673041,12.2,9.95977024945805));
#220215=CARTESIAN_POINT('Ctrl Pts',(4.12100686137596,12.2,9.9632256533786));
#220216=CARTESIAN_POINT('Ctrl Pts',(4.12136458230185,12.2,9.96669749652046));
#220217=CARTESIAN_POINT('Ctrl Pts',(4.12172230317899,12.2,9.97016933918929));
#220218=CARTESIAN_POINT('Ctrl Pts',(4.12207575009686,12.2,9.97365761854002));
#220219=CARTESIAN_POINT('Ctrl Pts',(4.12242481701305,12.2,9.9771622276969));
#220220=CARTESIAN_POINT('Ctrl Pts',(4.12286115069396,12.2,9.98154298950111));
#220221=CARTESIAN_POINT('Ctrl Pts',(4.12329064037748,12.2,9.98594926316156));
#220222=CARTESIAN_POINT('Ctrl Pts',(4.12371308398896,12.2,9.99038083670192));
#220223=CARTESIAN_POINT('Ctrl Pts',(4.12405103889657,12.2,9.99392609572743));
#220224=CARTESIAN_POINT('Ctrl Pts',(4.12438448329148,12.2,9.99748754523291));
#220225=CARTESIAN_POINT('Ctrl Pts',(4.12471331554765,12.2,10.0010650797191));
#220226=CARTESIAN_POINT('Ctrl Pts',(4.12504214775902,12.2,10.0046426137179));
#220227=CARTESIAN_POINT('Ctrl Pts',(4.12536636639683,12.2,10.0082362298622));
#220228=CARTESIAN_POINT('Ctrl Pts',(4.12568587198213,12.2,10.011845822455));
#220229=CARTESIAN_POINT('Ctrl Pts',(4.12600537761096,12.2,10.0154554155395));
#220230=CARTESIAN_POINT('Ctrl Pts',(4.12632016853646,12.2,10.019080983901));
#220231=CARTESIAN_POINT('Ctrl Pts',(4.12663014677526,12.2,10.0227224228228));
#220232=CARTESIAN_POINT('Ctrl Pts',(4.12694012497183,12.2,10.0263638612484));
#220233=CARTESIAN_POINT('Ctrl Pts',(4.12724528829049,12.2,10.0300211667268));
#220234=CARTESIAN_POINT('Ctrl Pts',(4.12754554044803,12.2,10.033694237442));
#220235=CARTESIAN_POINT('Ctrl Pts',(4.12784579264649,12.2,10.0373673086577));
#220236=CARTESIAN_POINT('Ctrl Pts',(4.12814113082482,12.2,10.0410561426972));
#220237=CARTESIAN_POINT('Ctrl Pts',(4.12843146050698,12.2,10.0447606345112));
#220238=CARTESIAN_POINT('Ctrl Pts',(4.12872179014959,12.2,10.0484651258205));
#220239=CARTESIAN_POINT('Ctrl Pts',(4.12900710847098,12.2,10.0521852753267));
#220240=CARTESIAN_POINT('Ctrl Pts',(4.12928732267081,12.2,10.0559209786308));
#220241=CARTESIAN_POINT('Ctrl Pts',(4.12956753690882,12.2,10.0596566824439));
#220242=CARTESIAN_POINT('Ctrl Pts',(4.12984264371201,12.2,10.0634079399884));
#220243=CARTESIAN_POINT('Ctrl Pts',(4.13011255128348,12.2,10.0671746477108));
#220244=CARTESIAN_POINT('Ctrl Pts',(4.13038245881818,12.2,10.0709413549201));
#220245=CARTESIAN_POINT('Ctrl Pts',(4.13064716516154,12.2,10.074723511891));
#220246=CARTESIAN_POINT('Ctrl Pts',(4.13090657747422,12.2,10.0785210159124));
#220247=CARTESIAN_POINT('Ctrl Pts',(4.13116598982223,12.2,10.0823185204511));
#220248=CARTESIAN_POINT('Ctrl Pts',(4.13142010693919,12.2,10.0861313724218));
#220249=CARTESIAN_POINT('Ctrl Pts',(4.1316688380083,12.2,10.0899594682416));
#220250=CARTESIAN_POINT('Ctrl Pts',(4.13191756907742,12.2,10.0937875640614));
#220251=CARTESIAN_POINT('Ctrl Pts',(4.13216091357368,12.2,10.0976309054384));
#220252=CARTESIAN_POINT('Ctrl Pts',(4.13239878053052,12.2,10.1014893893725));
#220253=CARTESIAN_POINT('Ctrl Pts',(4.13263664745496,12.2,10.1053478727808));
#220254=CARTESIAN_POINT('Ctrl Pts',(4.13286903463675,12.2,10.1092214997754));
#220255=CARTESIAN_POINT('Ctrl Pts',(4.13309585500814,12.2,10.1131101690306));
#220256=CARTESIAN_POINT('Ctrl Pts',(4.13332267541044,12.2,10.1169988388157));
#220257=CARTESIAN_POINT('Ctrl Pts',(4.13354392838237,12.2,10.1209025507894));
#220258=CARTESIAN_POINT('Ctrl Pts',(4.13375952356021,12.2,10.1248212046156));
#220259=CARTESIAN_POINT('Ctrl Pts',(4.13397511870868,12.2,10.1287398579079));
#220260=CARTESIAN_POINT('Ctrl Pts',(4.1341850578162,12.2,10.1326734524482));
#220261=CARTESIAN_POINT('Ctrl Pts',(4.13438925146655,12.2,10.1366218904023));
#220262=CARTESIAN_POINT('Ctrl Pts',(4.13459344514473,12.2,10.1405703288943));
#220263=CARTESIAN_POINT('Ctrl Pts',(4.13479189309994,12.2,10.1445336099077));
#220264=CARTESIAN_POINT('Ctrl Pts',(4.13498451028622,12.2,10.1485116346023));
#220265=CARTESIAN_POINT('Ctrl Pts',(4.13517712744625,12.2,10.1524896587548));
#220266=CARTESIAN_POINT('Ctrl Pts',(4.13536391402175,12.2,10.1564824252816));
#220267=CARTESIAN_POINT('Ctrl Pts',(4.13554478245179,12.2,10.1604898378975));
#220268=CARTESIAN_POINT('Ctrl Pts',(4.13577086800783,12.2,10.1654991040767));
#220269=CARTESIAN_POINT('Ctrl Pts',(4.13598770815807,12.2,10.1705312536262));
#220270=CARTESIAN_POINT('Ctrl Pts',(4.13619513781135,12.2,10.1755860949445));
#220271=CARTESIAN_POINT('Ctrl Pts',(4.13640256746461,12.2,10.1806409362627));
#220272=CARTESIAN_POINT('Ctrl Pts',(4.13660058633153,12.2,10.1857184699899));
#220273=CARTESIAN_POINT('Ctrl Pts',(4.13678903272092,12.2,10.1908185071415));
#220274=CARTESIAN_POINT('Ctrl Pts',(4.13693978984065,12.2,10.1948985370852));
#220275=CARTESIAN_POINT('Ctrl Pts',(4.13708442016443,12.2,10.1989929704685));
#220276=CARTESIAN_POINT('Ctrl Pts',(4.13722284201169,12.2,10.2031017086212));
#220277=CARTESIAN_POINT('Ctrl Pts',(4.13736126384008,12.2,10.2072104462141));
#220278=CARTESIAN_POINT('Ctrl Pts',(4.13749347726061,12.2,10.2113334899177));
#220279=CARTESIAN_POINT('Ctrl Pts',(4.13761940047295,12.2,10.2154707439118));
#220280=CARTESIAN_POINT('Ctrl Pts',(4.13777680450124,12.2,10.2206423118273));
#220281=CARTESIAN_POINT('Ctrl Pts',(4.13792438204039,12.2,10.2258360833379));
#220282=CARTESIAN_POINT('Ctrl Pts',(4.13806197599924,12.2,10.2310518736839));
#220283=CARTESIAN_POINT('Ctrl Pts',(4.13817205117233,12.2,10.2352245061882));
#220284=CARTESIAN_POINT('Ctrl Pts',(4.13827573674334,12.2,10.2394112302085));
#220285=CARTESIAN_POINT('Ctrl Pts',(4.13837295453071,12.2,10.2436119510929));
#220286=CARTESIAN_POINT('Ctrl Pts',(4.13847017230483,12.2,10.247812671405));
#220287=CARTESIAN_POINT('Ctrl Pts',(4.13856092142448,12.2,10.2520273907232));
#220288=CARTESIAN_POINT('Ctrl Pts',(4.13864512525136,12.2,10.2562560121544));
#220289=CARTESIAN_POINT('Ctrl Pts',(4.13872932908971,12.2,10.2604846341617));
#220290=CARTESIAN_POINT('Ctrl Pts',(4.13880698679672,12.2,10.2647271612513));
#220291=CARTESIAN_POINT('Ctrl Pts',(4.13887802202238,12.2,10.268983497873));
#220292=CARTESIAN_POINT('Ctrl Pts',(4.13894905723836,12.2,10.2732398339148));
#220293=CARTESIAN_POINT('Ctrl Pts',(4.13901346866503,12.2,10.2775099805213));
#220294=CARTESIAN_POINT('Ctrl Pts',(4.13907118244156,12.2,10.2817938448284));
#220295=CARTESIAN_POINT('Ctrl Pts',(4.13912889622595,12.2,10.2860777097191));
#220296=CARTESIAN_POINT('Ctrl Pts',(4.13917991115988,12.2,10.2903752923306));
#220297=CARTESIAN_POINT('Ctrl Pts',(4.13922415299519,12.2,10.2946865008442));
#220298=CARTESIAN_POINT('Ctrl Pts',(4.13926839482446,12.2,10.2989977087704));
#220299=CARTESIAN_POINT('Ctrl Pts',(4.13930586282732,12.2,10.3033225425717));
#220300=CARTESIAN_POINT('Ctrl Pts',(4.13933648276996,12.2,10.3076609100489));
#220301=CARTESIAN_POINT('Ctrl Pts',(4.13936710271677,12.2,10.3119992781173));
#220302=CARTESIAN_POINT('Ctrl Pts',(4.13939087517956,12.2,10.3163511809951));
#220303=CARTESIAN_POINT('Ctrl Pts',(4.13940772645831,12.2,10.3207165262529));
#220304=CARTESIAN_POINT('Ctrl Pts',(4.13942457773477,12.2,10.3250818709159));
#220305=CARTESIAN_POINT('Ctrl Pts',(4.13943450893234,12.2,10.3294606582283));
#220306=CARTESIAN_POINT('Ctrl Pts',(4.13943744626615,12.2,10.3338527982568));
#220307=CARTESIAN_POINT('Ctrl Pts',(4.13944038360036,12.2,10.3382449388837));
#220308=CARTESIAN_POINT('Ctrl Pts',(4.13943632774502,12.2,10.3426504317452));
#220309=CARTESIAN_POINT('Ctrl Pts',(4.13942520696664,12.2,10.3470691870416));
#220310=CARTESIAN_POINT('Ctrl Pts',(4.13941130599442,12.2,10.3525926308611));
#220311=CARTESIAN_POINT('Ctrl Pts',(4.13938636682792,12.2,10.3581367976721));
#220312=CARTESIAN_POINT('Ctrl Pts',(4.13935025092495,12.2,10.363701510753));
#220313=CARTESIAN_POINT('Ctrl Pts',(4.13932135820494,12.2,10.3681532808538));
#220314=CARTESIAN_POINT('Ctrl Pts',(4.13928531276943,12.2,10.3726182011825));
#220315=CARTESIAN_POINT('Ctrl Pts',(4.13924204477371,12.2,10.3770961837595));
#220316=CARTESIAN_POINT('Ctrl Pts',(4.13920959376955,12.2,10.3804546714548));
#220317=CARTESIAN_POINT('Ctrl Pts',(4.13917308026424,12.2,10.383820504994));
#220318=CARTESIAN_POINT('Ctrl Pts',(4.13913247521612,12.2,10.387193648777));
#220319=CARTESIAN_POINT('Ctrl Pts',(4.13909187017537,12.2,10.3905667919471));
#220320=CARTESIAN_POINT('Ctrl Pts',(4.13904717384317,12.2,10.3939472448917));
#220321=CARTESIAN_POINT('Ctrl Pts',(4.13899835680292,12.2,10.3973349706027));
#220322=CARTESIAN_POINT('Ctrl Pts',(4.13893326741887,12.2,10.4018519380121));
#220323=CARTESIAN_POINT('Ctrl Pts',(4.13886085166389,12.2,10.4063818332531));
#220324=CARTESIAN_POINT('Ctrl Pts',(4.13878104477818,12.2,10.4109245701075));
#220325=CARTESIAN_POINT('Ctrl Pts',(4.1387012378816,12.2,10.4154673075809));
#220326=CARTESIAN_POINT('Ctrl Pts',(4.13861403689503,12.2,10.4200228854821));
#220327=CARTESIAN_POINT('Ctrl Pts',(4.1385193775005,12.2,10.4245912168985));
#220328=CARTESIAN_POINT('Ctrl Pts',(4.13844838296104,12.2,10.4280174651496));
#220329=CARTESIAN_POINT('Ctrl Pts',(4.13837319151376,12.2,10.4314508882416));
#220330=CARTESIAN_POINT('Ctrl Pts',(4.13829377701664,12.2,10.4348914474916));
#220331=CARTESIAN_POINT('Ctrl Pts',(4.13821436251953,12.2,10.4383320067416));
#220332=CARTESIAN_POINT('Ctrl Pts',(4.13813072518925,12.2,10.4417797029163));
#220333=CARTESIAN_POINT('Ctrl Pts',(4.13804283527615,12.2,10.4452345001235));
#220334=CARTESIAN_POINT('Ctrl Pts',(4.13795494536304,12.2,10.4486892973307));
#220335=CARTESIAN_POINT('Ctrl Pts',(4.13786280418607,12.2,10.4521511951157));
#220336=CARTESIAN_POINT('Ctrl Pts',(4.13776638422692,12.2,10.4556201570372));
#220337=CARTESIAN_POINT('Ctrl Pts',(4.13766996426777,12.2,10.4590891189587));
#220338=CARTESIAN_POINT('Ctrl Pts',(4.13756926675179,12.2,10.4625651457515));
#220339=CARTESIAN_POINT('Ctrl Pts',(4.13746426183953,12.2,10.466048199499));
#220340=CARTESIAN_POINT('Ctrl Pts',(4.13735925690819,12.2,10.4695312538792));
#220341=CARTESIAN_POINT('Ctrl Pts',(4.1372499469423,12.2,10.4730213366364));
#220342=CARTESIAN_POINT('Ctrl Pts',(4.13713630350853,12.2,10.4765184110206));
#220343=CARTESIAN_POINT('Ctrl Pts',(4.1370226600954,12.2,10.4800154847696));
#220344=CARTESIAN_POINT('Ctrl Pts',(4.1369046841325,12.2,10.4835195502931));
#220345=CARTESIAN_POINT('Ctrl Pts',(4.13678234826157,12.2,10.4870305710828));
#220346=CARTESIAN_POINT('Ctrl Pts',(4.13666001239063,12.2,10.4905415918725));
#220347=CARTESIAN_POINT('Ctrl Pts',(4.13653331812904,12.2,10.4940595694985));
#220348=CARTESIAN_POINT('Ctrl Pts',(4.13640223721652,12.2,10.4975844662615));
#220349=CARTESIAN_POINT('Ctrl Pts',(4.13622746267443,12.2,10.5022843283986));
#220350=CARTESIAN_POINT('Ctrl Pts',(4.13604489059251,12.2,10.5069964933205));
#220351=CARTESIAN_POINT('Ctrl Pts',(4.13585446049777,12.2,10.5117208747108));
#220352=CARTESIAN_POINT('Ctrl Pts',(4.13571163789428,12.2,10.5152641615582));
#220353=CARTESIAN_POINT('Ctrl Pts',(4.13556439383956,12.2,10.5188143207408));
#220354=CARTESIAN_POINT('Ctrl Pts',(4.13541270373357,12.2,10.5223713170504));
#220355=CARTESIAN_POINT('Ctrl Pts',(4.13521045030485,12.2,10.5271139777195));
#220356=CARTESIAN_POINT('Ctrl Pts',(4.13500029072993,12.2,10.5318687920092));
#220357=CARTESIAN_POINT('Ctrl Pts',(4.13478216602607,12.2,10.5366356761187));
#220358=CARTESIAN_POINT('Ctrl Pts',(4.13461857249073,12.2,10.5402108393632));
#220359=CARTESIAN_POINT('Ctrl Pts',(4.13445049713071,12.2,10.5437927921822));
#220360=CARTESIAN_POINT('Ctrl Pts',(4.13427791659593,12.2,10.5473814989676));
#220361=CARTESIAN_POINT('Ctrl Pts',(4.13410533602979,12.2,10.5509702064049));
#220362=CARTESIAN_POINT('Ctrl Pts',(4.13392824853739,12.2,10.5545656691775));
#220363=CARTESIAN_POINT('Ctrl Pts',(4.13374663092704,12.2,10.5581678505352));
#220364=CARTESIAN_POINT('Ctrl Pts',(4.13356501334969,12.2,10.5617700312386));
#220365=CARTESIAN_POINT('Ctrl Pts',(4.13337886303283,12.2,10.5653789302828));
#220366=CARTESIAN_POINT('Ctrl Pts',(4.13318815748803,12.2,10.5689945137079));
#220367=CARTESIAN_POINT('Ctrl Pts',(4.13293388343986,12.2,10.573815291389));
#220368=CARTESIAN_POINT('Ctrl Pts',(4.1326715094077,12.2,10.5786479524786));
#220369=CARTESIAN_POINT('Ctrl Pts',(4.13240097626368,12.2,10.5834924126374));
#220370=CARTESIAN_POINT('Ctrl Pts',(4.13219807639645,12.2,10.5871257579214));
#220371=CARTESIAN_POINT('Ctrl Pts',(4.13199058845455,12.2,10.5907657411383));
#220372=CARTESIAN_POINT('Ctrl Pts',(4.13177848604621,12.2,10.5944123269217));
#220373=CARTESIAN_POINT('Ctrl Pts',(4.13149568280942,12.2,10.599274441741));
#220374=CARTESIAN_POINT('Ctrl Pts',(4.13120467765636,12.2,10.6041482949203));
#220375=CARTESIAN_POINT('Ctrl Pts',(4.13090541374977,12.2,10.6090338049866));
#220376=CARTESIAN_POINT('Ctrl Pts',(4.13068096584022,12.2,10.6126979372035));
#220377=CARTESIAN_POINT('Ctrl Pts',(4.13045187237607,12.2,10.6163686266635));
#220378=CARTESIAN_POINT('Ctrl Pts',(4.13021810896685,12.2,10.6200458370049));
#220379=CARTESIAN_POINT('Ctrl Pts',(4.12998434555764,12.2,10.6237230473463));
#220380=CARTESIAN_POINT('Ctrl Pts',(4.12974591236715,12.2,10.6274067807825));
#220381=CARTESIAN_POINT('Ctrl Pts',(4.1295027850014,12.2,10.6310970010645));
#220382=CARTESIAN_POINT('Ctrl Pts',(4.12925965763564,12.2,10.6347872213465));
#220383=CARTESIAN_POINT('Ctrl Pts',(4.12901183772854,12.2,10.6384839297615));
#220384=CARTESIAN_POINT('Ctrl Pts',(4.12875930082169,12.2,10.642187092501));
#220385=CARTESIAN_POINT('Ctrl Pts',(4.12842258491532,12.2,10.6471246432688));
#220386=CARTESIAN_POINT('Ctrl Pts',(4.12807748452064,12.2,10.6520736684298));
#220387=CARTESIAN_POINT('Ctrl Pts',(4.12772394249973,12.2,10.6570340857783));
#220388=CARTESIAN_POINT('Ctrl Pts',(4.127370400527,12.2,10.661994502451));
#220389=CARTESIAN_POINT('Ctrl Pts',(4.12700841624328,12.2,10.6669663091354));
#220390=CARTESIAN_POINT('Ctrl Pts',(4.12663793455221,12.2,10.6719494258935));
#220391=CARTESIAN_POINT('Ctrl Pts',(4.12636007322082,12.2,10.6756867643108));
#220392=CARTESIAN_POINT('Ctrl Pts',(4.12607743316307,12.2,10.6794304647049));
#220393=CARTESIAN_POINT('Ctrl Pts',(4.12578999416231,12.2,10.6831804980841));
#220394=CARTESIAN_POINT('Ctrl Pts',(4.12550255521377,12.2,10.686930530782));
#220395=CARTESIAN_POINT('Ctrl Pts',(4.12521031630714,12.2,10.6906868959797));
#220396=CARTESIAN_POINT('Ctrl Pts',(4.12491325519252,12.2,10.6944495576769));
#220397=CARTESIAN_POINT('Ctrl Pts',(4.12451717372434,12.2,10.6994664397119));
#220398=CARTESIAN_POINT('Ctrl Pts',(4.12411251545434,12.2,10.7044945146189));
#220399=CARTESIAN_POINT('Ctrl Pts',(4.12369921830157,12.2,10.7095336875688));
#220400=CARTESIAN_POINT('Ctrl Pts',(4.12328592109248,12.2,10.7145728612053));
#220401=CARTESIAN_POINT('Ctrl Pts',(4.12286398257608,12.2,10.7196231273852));
#220402=CARTESIAN_POINT('Ctrl Pts',(4.12243337123359,12.2,10.7246844426642));
#220403=CARTESIAN_POINT('Ctrl Pts',(4.12211041275606,12.2,10.7284804287786));
#220404=CARTESIAN_POINT('Ctrl Pts',(4.12178257806039,12.2,10.7322826273081));
#220405=CARTESIAN_POINT('Ctrl Pts',(4.12144986799994,12.2,10.736091048));
#220406=CARTESIAN_POINT('Origin',(-5.66257110645729E-14,15.2,-1.77635683940025E-14));
#220407=CARTESIAN_POINT('',(2.64164356330595,15.2,10.0330625578962));
#220408=CARTESIAN_POINT('',(2.64164356330595,12.2,10.0330625578962));
#220409=CARTESIAN_POINT('',(2.64164356299994,15.2,10.033062558));
#220410=CARTESIAN_POINT('Origin',(-5.66257110645729E-14,12.2,-1.77635683940025E-14));
#220411=CARTESIAN_POINT('Origin',(-5.66257110645729E-14,15.2,-1.77635683940025E-14));
#220412=CARTESIAN_POINT('Origin',(-5.66257110645729E-14,15.2,-1.77635683940025E-14));
#220413=CARTESIAN_POINT('',(2.55159438999994,15.2,11.213356593));
#220414=CARTESIAN_POINT('',(2.17615954695741,15.2,11.2922242994459));
#220415=CARTESIAN_POINT('Origin',(-5.66257110645729E-14,15.2,-1.77635683940025E-14));
#220416=CARTESIAN_POINT('',(2.17615954695741,12.2,11.2922242994459));
#220417=CARTESIAN_POINT('',(2.17615954699994,15.2,11.2922243));
#220418=CARTESIAN_POINT('',(2.55159438999994,12.2,11.213356593));
#220419=CARTESIAN_POINT('Origin',(-5.66257110645729E-14,12.2,-1.77635683940025E-14));
#220420=CARTESIAN_POINT('',(2.55159438999994,15.2,11.213356593));
#220421=CARTESIAN_POINT('Ctrl Pts',(2.64164356399994,15.2,10.033062558));
#220422=CARTESIAN_POINT('Ctrl Pts',(2.64164356399994,11.6,10.033062558));
#220423=CARTESIAN_POINT('Ctrl Pts',(2.64167330399995,15.2,10.033234361));
#220424=CARTESIAN_POINT('Ctrl Pts',(2.64167330399995,11.6,10.033234361));
#220425=CARTESIAN_POINT('Ctrl Pts',(2.64173373799995,15.2,10.033583982));
#220426=CARTESIAN_POINT('Ctrl Pts',(2.64173373799995,11.6,10.033583982));
#220427=CARTESIAN_POINT('Ctrl Pts',(2.64182504799995,15.2,10.034113786));
#220428=CARTESIAN_POINT('Ctrl Pts',(2.64182504799995,11.6,10.034113786));
#220429=CARTESIAN_POINT('Ctrl Pts',(2.64194751799995,15.2,10.034827572));
#220430=CARTESIAN_POINT('Ctrl Pts',(2.64194751799995,11.6,10.034827572));
#220431=CARTESIAN_POINT('Ctrl Pts',(2.64210152599994,15.2,10.03573056));
#220432=CARTESIAN_POINT('Ctrl Pts',(2.64210152599994,11.6,10.03573056));
#220433=CARTESIAN_POINT('Ctrl Pts',(2.64225710799994,15.2,10.03664834));
#220434=CARTESIAN_POINT('Ctrl Pts',(2.64225710799994,11.6,10.03664834));
#220435=CARTESIAN_POINT('Ctrl Pts',(2.64241334999994,15.2,10.037575658));
#220436=CARTESIAN_POINT('Ctrl Pts',(2.64241334999994,11.6,10.037575658));
#220437=CARTESIAN_POINT('Ctrl Pts',(2.64257022899994,15.2,10.03851249));
#220438=CARTESIAN_POINT('Ctrl Pts',(2.64257022899994,11.6,10.03851249));
#220439=CARTESIAN_POINT('Ctrl Pts',(2.64272772399994,15.2,10.039458812));
#220440=CARTESIAN_POINT('Ctrl Pts',(2.64272772399994,11.6,10.039458812));
#220441=CARTESIAN_POINT('Ctrl Pts',(2.64288581299994,15.2,10.040414602));
#220442=CARTESIAN_POINT('Ctrl Pts',(2.64288581299994,11.6,10.040414602));
#220443=CARTESIAN_POINT('Ctrl Pts',(2.64304447199994,15.2,10.041379835));
#220444=CARTESIAN_POINT('Ctrl Pts',(2.64304447199994,11.6,10.041379835));
#220445=CARTESIAN_POINT('Ctrl Pts',(2.64320368099995,15.2,10.04235449));
#220446=CARTESIAN_POINT('Ctrl Pts',(2.64320368099995,11.6,10.04235449));
#220447=CARTESIAN_POINT('Ctrl Pts',(2.64336341799994,15.2,10.043338541));
#220448=CARTESIAN_POINT('Ctrl Pts',(2.64336341799994,11.6,10.043338541));
#220449=CARTESIAN_POINT('Ctrl Pts',(2.64352365999994,15.2,10.044331969));
#220450=CARTESIAN_POINT('Ctrl Pts',(2.64352365999994,11.6,10.044331969));
#220451=CARTESIAN_POINT('Ctrl Pts',(2.64368438699994,15.2,10.045334747));
#220452=CARTESIAN_POINT('Ctrl Pts',(2.64368438699994,11.6,10.045334747));
#220453=CARTESIAN_POINT('Ctrl Pts',(2.64384557599994,15.2,10.046346855));
#220454=CARTESIAN_POINT('Ctrl Pts',(2.64384557599994,11.6,10.046346855));
#220455=CARTESIAN_POINT('Ctrl Pts',(2.64400720799994,15.2,10.047368269));
#220456=CARTESIAN_POINT('Ctrl Pts',(2.64400720799994,11.6,10.047368269));
#220457=CARTESIAN_POINT('Ctrl Pts',(2.64416925899994,15.2,10.048398967));
#220458=CARTESIAN_POINT('Ctrl Pts',(2.64416925899994,11.6,10.048398967));
#220459=CARTESIAN_POINT('Ctrl Pts',(2.64433170999995,15.2,10.049438926));
#220460=CARTESIAN_POINT('Ctrl Pts',(2.64433170999995,11.6,10.049438926));
#220461=CARTESIAN_POINT('Ctrl Pts',(2.64449453899994,15.2,10.050488124));
#220462=CARTESIAN_POINT('Ctrl Pts',(2.64449453899994,11.6,10.050488124));
#220463=CARTESIAN_POINT('Ctrl Pts',(2.64465772599995,15.2,10.051546539));
#220464=CARTESIAN_POINT('Ctrl Pts',(2.64465772599995,11.6,10.051546539));
#220465=CARTESIAN_POINT('Ctrl Pts',(2.64482124899994,15.2,10.052614149));
#220466=CARTESIAN_POINT('Ctrl Pts',(2.64482124899994,11.6,10.052614149));
#220467=CARTESIAN_POINT('Ctrl Pts',(2.64498508799994,15.2,10.053690931));
#220468=CARTESIAN_POINT('Ctrl Pts',(2.64498508799994,11.6,10.053690931));
#220469=CARTESIAN_POINT('Ctrl Pts',(2.64514922199994,15.2,10.054776862));
#220470=CARTESIAN_POINT('Ctrl Pts',(2.64514922199994,11.6,10.054776862));
#220471=CARTESIAN_POINT('Ctrl Pts',(2.64531363099994,15.2,10.055871924));
#220472=CARTESIAN_POINT('Ctrl Pts',(2.64531363099994,11.6,10.055871924));
#220473=CARTESIAN_POINT('Ctrl Pts',(2.64547829399994,15.2,10.056976092));
#220474=CARTESIAN_POINT('Ctrl Pts',(2.64547829399994,11.6,10.056976092));
#220475=CARTESIAN_POINT('Ctrl Pts',(2.64564319299994,15.2,10.058089345));
#220476=CARTESIAN_POINT('Ctrl Pts',(2.64564319299994,11.6,10.058089345));
#220477=CARTESIAN_POINT('Ctrl Pts',(2.64580830599995,15.2,10.059211661));
#220478=CARTESIAN_POINT('Ctrl Pts',(2.64580830599995,11.6,10.059211661));
#220479=CARTESIAN_POINT('Ctrl Pts',(2.64597361199994,15.2,10.060343019));
#220480=CARTESIAN_POINT('Ctrl Pts',(2.64597361199994,11.6,10.060343019));
#220481=CARTESIAN_POINT('Ctrl Pts',(2.64613909299994,15.2,10.061483398));
#220482=CARTESIAN_POINT('Ctrl Pts',(2.64613909299994,11.6,10.061483398));
#220483=CARTESIAN_POINT('Ctrl Pts',(2.64630472899994,15.2,10.062632776));
#220484=CARTESIAN_POINT('Ctrl Pts',(2.64630472899994,11.6,10.062632776));
#220485=CARTESIAN_POINT('Ctrl Pts',(2.64647049899994,15.2,10.063791132));
#220486=CARTESIAN_POINT('Ctrl Pts',(2.64647049899994,11.6,10.063791132));
#220487=CARTESIAN_POINT('Ctrl Pts',(2.64663638299994,15.2,10.064958444));
#220488=CARTESIAN_POINT('Ctrl Pts',(2.64663638299994,11.6,10.064958444));
#220489=CARTESIAN_POINT('Ctrl Pts',(2.64680236499995,15.2,10.066134693));
#220490=CARTESIAN_POINT('Ctrl Pts',(2.64680236499995,11.6,10.066134693));
#220491=CARTESIAN_POINT('Ctrl Pts',(2.64696842099994,15.2,10.067319856));
#220492=CARTESIAN_POINT('Ctrl Pts',(2.64696842099994,11.6,10.067319856));
#220493=CARTESIAN_POINT('Ctrl Pts',(2.64713453499994,15.2,10.068513912));
#220494=CARTESIAN_POINT('Ctrl Pts',(2.64713453499994,11.6,10.068513912));
#220495=CARTESIAN_POINT('Ctrl Pts',(2.64730068699994,15.2,10.069716842));
#220496=CARTESIAN_POINT('Ctrl Pts',(2.64730068699994,11.6,10.069716842));
#220497=CARTESIAN_POINT('Ctrl Pts',(2.64746685599994,15.2,10.070928625));
#220498=CARTESIAN_POINT('Ctrl Pts',(2.64746685599994,11.6,10.070928625));
#220499=CARTESIAN_POINT('Ctrl Pts',(2.64763302599994,15.2,10.072149238));
#220500=CARTESIAN_POINT('Ctrl Pts',(2.64763302599994,11.6,10.072149238));
#220501=CARTESIAN_POINT('Ctrl Pts',(2.64779917599994,15.2,10.073378662));
#220502=CARTESIAN_POINT('Ctrl Pts',(2.64779917599994,11.6,10.073378662));
#220503=CARTESIAN_POINT('Ctrl Pts',(2.64796528699994,15.2,10.074616878));
#220504=CARTESIAN_POINT('Ctrl Pts',(2.64796528699994,11.6,10.074616878));
#220505=CARTESIAN_POINT('Ctrl Pts',(2.64813134299994,15.2,10.075863863));
#220506=CARTESIAN_POINT('Ctrl Pts',(2.64813134299994,11.6,10.075863863));
#220507=CARTESIAN_POINT('Ctrl Pts',(2.64829732199995,15.2,10.077119598));
#220508=CARTESIAN_POINT('Ctrl Pts',(2.64829732199995,11.6,10.077119598));
#220509=CARTESIAN_POINT('Ctrl Pts',(2.64846320599994,15.2,10.078384063));
#220510=CARTESIAN_POINT('Ctrl Pts',(2.64846320599994,11.6,10.078384063));
#220511=CARTESIAN_POINT('Ctrl Pts',(2.64862897799994,15.2,10.079657238));
#220512=CARTESIAN_POINT('Ctrl Pts',(2.64862897799994,11.6,10.079657238));
#220513=CARTESIAN_POINT('Ctrl Pts',(2.64879461899994,15.2,10.080939101));
#220514=CARTESIAN_POINT('Ctrl Pts',(2.64879461899994,11.6,10.080939101));
#220515=CARTESIAN_POINT('Ctrl Pts',(2.64896010999994,15.2,10.082229634));
#220516=CARTESIAN_POINT('Ctrl Pts',(2.64896010999994,11.6,10.082229634));
#220517=CARTESIAN_POINT('Ctrl Pts',(2.64912543499995,15.2,10.083528816));
#220518=CARTESIAN_POINT('Ctrl Pts',(2.64912543499995,11.6,10.083528816));
#220519=CARTESIAN_POINT('Ctrl Pts',(2.64929057299994,15.2,10.084836628));
#220520=CARTESIAN_POINT('Ctrl Pts',(2.64929057299994,11.6,10.084836628));
#220521=CARTESIAN_POINT('Ctrl Pts',(2.64945550799994,15.2,10.08615305));
#220522=CARTESIAN_POINT('Ctrl Pts',(2.64945550799994,11.6,10.08615305));
#220523=CARTESIAN_POINT('Ctrl Pts',(2.64962022199994,15.2,10.087478062));
#220524=CARTESIAN_POINT('Ctrl Pts',(2.64962022199994,11.6,10.087478062));
#220525=CARTESIAN_POINT('Ctrl Pts',(2.64978469499995,15.2,10.088811644));
#220526=CARTESIAN_POINT('Ctrl Pts',(2.64978469499995,11.6,10.088811644));
#220527=CARTESIAN_POINT('Ctrl Pts',(2.64994891199994,15.2,10.090153777));
#220528=CARTESIAN_POINT('Ctrl Pts',(2.64994891199994,11.6,10.090153777));
#220529=CARTESIAN_POINT('Ctrl Pts',(2.65011285399994,15.2,10.091504443));
#220530=CARTESIAN_POINT('Ctrl Pts',(2.65011285399994,11.6,10.091504443));
#220531=CARTESIAN_POINT('Ctrl Pts',(2.65027650299994,15.2,10.09286362));
#220532=CARTESIAN_POINT('Ctrl Pts',(2.65027650299994,11.6,10.09286362));
#220533=CARTESIAN_POINT('Ctrl Pts',(2.65043984299994,15.2,10.09423129));
#220534=CARTESIAN_POINT('Ctrl Pts',(2.65043984299994,11.6,10.09423129));
#220535=CARTESIAN_POINT('Ctrl Pts',(2.65060285499994,15.2,10.095607434));
#220536=CARTESIAN_POINT('Ctrl Pts',(2.65060285499994,11.6,10.095607434));
#220537=CARTESIAN_POINT('Ctrl Pts',(2.65076552299994,15.2,10.096992032));
#220538=CARTESIAN_POINT('Ctrl Pts',(2.65076552299994,11.6,10.096992032));
#220539=CARTESIAN_POINT('Ctrl Pts',(2.65092782799994,15.2,10.098385066));
#220540=CARTESIAN_POINT('Ctrl Pts',(2.65092782799994,11.6,10.098385066));
#220541=CARTESIAN_POINT('Ctrl Pts',(2.65108975499994,15.2,10.099786515));
#220542=CARTESIAN_POINT('Ctrl Pts',(2.65108975499994,11.6,10.099786515));
#220543=CARTESIAN_POINT('Ctrl Pts',(2.65125128499994,15.2,10.101196362));
#220544=CARTESIAN_POINT('Ctrl Pts',(2.65125128499994,11.6,10.101196362));
#220545=CARTESIAN_POINT('Ctrl Pts',(2.65141240299994,15.2,10.102614588));
#220546=CARTESIAN_POINT('Ctrl Pts',(2.65141240299994,11.6,10.102614588));
#220547=CARTESIAN_POINT('Ctrl Pts',(2.65157308999994,15.2,10.104041173));
#220548=CARTESIAN_POINT('Ctrl Pts',(2.65157308999994,11.6,10.104041173));
#220549=CARTESIAN_POINT('Ctrl Pts',(2.65173333099994,15.2,10.1054761));
#220550=CARTESIAN_POINT('Ctrl Pts',(2.65173333099994,11.6,10.1054761));
#220551=CARTESIAN_POINT('Ctrl Pts',(2.65189310699995,15.2,10.106919348));
#220552=CARTESIAN_POINT('Ctrl Pts',(2.65189310699995,11.6,10.106919348));
#220553=CARTESIAN_POINT('Ctrl Pts',(2.65205240399994,15.2,10.1083709));
#220554=CARTESIAN_POINT('Ctrl Pts',(2.65205240399994,11.6,10.1083709));
#220555=CARTESIAN_POINT('Ctrl Pts',(2.65221120299994,15.2,10.109830736));
#220556=CARTESIAN_POINT('Ctrl Pts',(2.65221120299994,11.6,10.109830736));
#220557=CARTESIAN_POINT('Ctrl Pts',(2.65236948999994,15.2,10.11129884));
#220558=CARTESIAN_POINT('Ctrl Pts',(2.65236948999994,11.6,10.11129884));
#220559=CARTESIAN_POINT('Ctrl Pts',(2.65252724599994,15.2,10.112775193));
#220560=CARTESIAN_POINT('Ctrl Pts',(2.65252724599994,11.6,10.112775193));
#220561=CARTESIAN_POINT('Ctrl Pts',(2.65268445599995,15.2,10.114259774));
#220562=CARTESIAN_POINT('Ctrl Pts',(2.65268445599995,11.6,10.114259774));
#220563=CARTESIAN_POINT('Ctrl Pts',(2.65284110299994,15.2,10.115752568));
#220564=CARTESIAN_POINT('Ctrl Pts',(2.65284110299994,11.6,10.115752568));
#220565=CARTESIAN_POINT('Ctrl Pts',(2.65299717299994,15.2,10.117253554));
#220566=CARTESIAN_POINT('Ctrl Pts',(2.65299717299994,11.6,10.117253554));
#220567=CARTESIAN_POINT('Ctrl Pts',(2.65315264599994,15.2,10.118762716));
#220568=CARTESIAN_POINT('Ctrl Pts',(2.65315264599994,11.6,10.118762716));
#220569=CARTESIAN_POINT('Ctrl Pts',(2.65330750999994,15.2,10.120280036));
#220570=CARTESIAN_POINT('Ctrl Pts',(2.65330750999994,11.6,10.120280036));
#220571=CARTESIAN_POINT('Ctrl Pts',(2.65346174599994,15.2,10.121805494));
#220572=CARTESIAN_POINT('Ctrl Pts',(2.65346174599994,11.6,10.121805494));
#220573=CARTESIAN_POINT('Ctrl Pts',(2.65361533899994,15.2,10.123339075));
#220574=CARTESIAN_POINT('Ctrl Pts',(2.65361533899994,11.6,10.123339075));
#220575=CARTESIAN_POINT('Ctrl Pts',(2.65376827399994,15.2,10.124880757));
#220576=CARTESIAN_POINT('Ctrl Pts',(2.65376827399994,11.6,10.124880757));
#220577=CARTESIAN_POINT('Ctrl Pts',(2.65392053399994,15.2,10.126430526));
#220578=CARTESIAN_POINT('Ctrl Pts',(2.65392053399994,11.6,10.126430526));
#220579=CARTESIAN_POINT('Ctrl Pts',(2.65407210499994,15.2,10.127988362));
#220580=CARTESIAN_POINT('Ctrl Pts',(2.65407210499994,11.6,10.127988362));
#220581=CARTESIAN_POINT('Ctrl Pts',(2.65422296899994,15.2,10.129554248));
#220582=CARTESIAN_POINT('Ctrl Pts',(2.65422296899994,11.6,10.129554248));
#220583=CARTESIAN_POINT('Ctrl Pts',(2.65437311199994,15.2,10.131128167));
#220584=CARTESIAN_POINT('Ctrl Pts',(2.65437311199994,11.6,10.131128167));
#220585=CARTESIAN_POINT('Ctrl Pts',(2.65452251799994,15.2,10.132710101));
#220586=CARTESIAN_POINT('Ctrl Pts',(2.65452251799994,11.6,10.132710101));
#220587=CARTESIAN_POINT('Ctrl Pts',(2.65467117299994,15.2,10.134300032));
#220588=CARTESIAN_POINT('Ctrl Pts',(2.65467117299994,11.6,10.134300032));
#220589=CARTESIAN_POINT('Ctrl Pts',(2.65481905899994,15.2,10.135897942));
#220590=CARTESIAN_POINT('Ctrl Pts',(2.65481905899994,11.6,10.135897942));
#220591=CARTESIAN_POINT('Ctrl Pts',(2.65496616299994,15.2,10.137503816));
#220592=CARTESIAN_POINT('Ctrl Pts',(2.65496616299994,11.6,10.137503816));
#220593=CARTESIAN_POINT('Ctrl Pts',(2.65511246899994,15.2,10.139117634));
#220594=CARTESIAN_POINT('Ctrl Pts',(2.65511246899994,11.6,10.139117634));
#220595=CARTESIAN_POINT('Ctrl Pts',(2.65525796099995,15.2,10.14073938));
#220596=CARTESIAN_POINT('Ctrl Pts',(2.65525796099995,11.6,10.14073938));
#220597=CARTESIAN_POINT('Ctrl Pts',(2.65540262499994,15.2,10.142369037));
#220598=CARTESIAN_POINT('Ctrl Pts',(2.65540262499994,11.6,10.142369037));
#220599=CARTESIAN_POINT('Ctrl Pts',(2.65554644699994,15.2,10.144006587));
#220600=CARTESIAN_POINT('Ctrl Pts',(2.65554644699994,11.6,10.144006587));
#220601=CARTESIAN_POINT('Ctrl Pts',(2.65568941099994,15.2,10.145652013));
#220602=CARTESIAN_POINT('Ctrl Pts',(2.65568941099994,11.6,10.145652013));
#220603=CARTESIAN_POINT('Ctrl Pts',(2.65583150099994,15.2,10.147305299));
#220604=CARTESIAN_POINT('Ctrl Pts',(2.65583150099994,11.6,10.147305299));
#220605=CARTESIAN_POINT('Ctrl Pts',(2.65597270299994,15.2,10.148966427));
#220606=CARTESIAN_POINT('Ctrl Pts',(2.65597270299994,11.6,10.148966427));
#220607=CARTESIAN_POINT('Ctrl Pts',(2.65611300299994,15.2,10.150635381));
#220608=CARTESIAN_POINT('Ctrl Pts',(2.65611300299994,11.6,10.150635381));
#220609=CARTESIAN_POINT('Ctrl Pts',(2.65625238599994,15.2,10.152312142));
#220610=CARTESIAN_POINT('Ctrl Pts',(2.65625238599994,11.6,10.152312142));
#220611=CARTESIAN_POINT('Ctrl Pts',(2.65639083699994,15.2,10.153996696));
#220612=CARTESIAN_POINT('Ctrl Pts',(2.65639083699994,11.6,10.153996696));
#220613=CARTESIAN_POINT('Ctrl Pts',(2.65652834299994,15.2,10.155689024));
#220614=CARTESIAN_POINT('Ctrl Pts',(2.65652834299994,11.6,10.155689024));
#220615=CARTESIAN_POINT('Ctrl Pts',(2.65666488599994,15.2,10.157389111));
#220616=CARTESIAN_POINT('Ctrl Pts',(2.65666488599994,11.6,10.157389111));
#220617=CARTESIAN_POINT('Ctrl Pts',(2.65680045599994,15.2,10.159096939));
#220618=CARTESIAN_POINT('Ctrl Pts',(2.65680045599994,11.6,10.159096939));
#220619=CARTESIAN_POINT('Ctrl Pts',(2.65693503499994,15.2,10.160812492));
#220620=CARTESIAN_POINT('Ctrl Pts',(2.65693503499994,11.6,10.160812492));
#220621=CARTESIAN_POINT('Ctrl Pts',(2.65706860999994,15.2,10.162535753));
#220622=CARTESIAN_POINT('Ctrl Pts',(2.65706860999994,11.6,10.162535753));
#220623=CARTESIAN_POINT('Ctrl Pts',(2.65720116799995,15.2,10.164266705));
#220624=CARTESIAN_POINT('Ctrl Pts',(2.65720116799995,11.6,10.164266705));
#220625=CARTESIAN_POINT('Ctrl Pts',(2.65733269399994,15.2,10.166005334));
#220626=CARTESIAN_POINT('Ctrl Pts',(2.65733269399994,11.6,10.166005334));
#220627=CARTESIAN_POINT('Ctrl Pts',(2.65746317299994,15.2,10.167751622));
#220628=CARTESIAN_POINT('Ctrl Pts',(2.65746317299994,11.6,10.167751622));
#220629=CARTESIAN_POINT('Ctrl Pts',(2.65759259199994,15.2,10.169505552));
#220630=CARTESIAN_POINT('Ctrl Pts',(2.65759259199994,11.6,10.169505552));
#220631=CARTESIAN_POINT('Ctrl Pts',(2.65772093699994,15.2,10.171267109));
#220632=CARTESIAN_POINT('Ctrl Pts',(2.65772093699994,11.6,10.171267109));
#220633=CARTESIAN_POINT('Ctrl Pts',(2.65784819299994,15.2,10.173036275));
#220634=CARTESIAN_POINT('Ctrl Pts',(2.65784819299994,11.6,10.173036275));
#220635=CARTESIAN_POINT('Ctrl Pts',(2.65797434799994,15.2,10.174813035));
#220636=CARTESIAN_POINT('Ctrl Pts',(2.65797434799994,11.6,10.174813035));
#220637=CARTESIAN_POINT('Ctrl Pts',(2.65809938699994,15.2,10.176597374));
#220638=CARTESIAN_POINT('Ctrl Pts',(2.65809938699994,11.6,10.176597374));
#220639=CARTESIAN_POINT('Ctrl Pts',(2.65822329599994,15.2,10.178389274));
#220640=CARTESIAN_POINT('Ctrl Pts',(2.65822329599994,11.6,10.178389274));
#220641=CARTESIAN_POINT('Ctrl Pts',(2.65834606299994,15.2,10.18018872));
#220642=CARTESIAN_POINT('Ctrl Pts',(2.65834606299994,11.6,10.18018872));
#220643=CARTESIAN_POINT('Ctrl Pts',(2.65846767199994,15.2,10.181995695));
#220644=CARTESIAN_POINT('Ctrl Pts',(2.65846767199994,11.6,10.181995695));
#220645=CARTESIAN_POINT('Ctrl Pts',(2.65858811199994,15.2,10.183810184));
#220646=CARTESIAN_POINT('Ctrl Pts',(2.65858811199994,11.6,10.183810184));
#220647=CARTESIAN_POINT('Ctrl Pts',(2.65870736599994,15.2,10.185632171));
#220648=CARTESIAN_POINT('Ctrl Pts',(2.65870736599994,11.6,10.185632171));
#220649=CARTESIAN_POINT('Ctrl Pts',(2.65882542499994,15.2,10.18746164));
#220650=CARTESIAN_POINT('Ctrl Pts',(2.65882542499994,11.6,10.18746164));
#220651=CARTESIAN_POINT('Ctrl Pts',(2.65894227299994,15.2,10.189298575));
#220652=CARTESIAN_POINT('Ctrl Pts',(2.65894227299994,11.6,10.189298575));
#220653=CARTESIAN_POINT('Ctrl Pts',(2.65905789599994,15.2,10.19114296));
#220654=CARTESIAN_POINT('Ctrl Pts',(2.65905789599994,11.6,10.19114296));
#220655=CARTESIAN_POINT('Ctrl Pts',(2.65917228199994,15.2,10.192994781));
#220656=CARTESIAN_POINT('Ctrl Pts',(2.65917228199994,11.6,10.192994781));
#220657=CARTESIAN_POINT('Ctrl Pts',(2.65928541899994,15.2,10.194854021));
#220658=CARTESIAN_POINT('Ctrl Pts',(2.65928541899994,11.6,10.194854021));
#220659=CARTESIAN_POINT('Ctrl Pts',(2.65939729099995,15.2,10.196720664));
#220660=CARTESIAN_POINT('Ctrl Pts',(2.65939729099995,11.6,10.196720664));
#220661=CARTESIAN_POINT('Ctrl Pts',(2.65950788599994,15.2,10.198594695));
#220662=CARTESIAN_POINT('Ctrl Pts',(2.65950788599994,11.6,10.198594695));
#220663=CARTESIAN_POINT('Ctrl Pts',(2.65961719199994,15.2,10.200476099));
#220664=CARTESIAN_POINT('Ctrl Pts',(2.65961719199994,11.6,10.200476099));
#220665=CARTESIAN_POINT('Ctrl Pts',(2.65972519499994,15.2,10.202364859));
#220666=CARTESIAN_POINT('Ctrl Pts',(2.65972519499994,11.6,10.202364859));
#220667=CARTESIAN_POINT('Ctrl Pts',(2.65983188299994,15.2,10.204260962));
#220668=CARTESIAN_POINT('Ctrl Pts',(2.65983188299994,11.6,10.204260962));
#220669=CARTESIAN_POINT('Ctrl Pts',(2.65993724399994,15.2,10.20616439));
#220670=CARTESIAN_POINT('Ctrl Pts',(2.65993724399994,11.6,10.20616439));
#220671=CARTESIAN_POINT('Ctrl Pts',(2.66004126099994,15.2,10.20807513));
#220672=CARTESIAN_POINT('Ctrl Pts',(2.66004126099994,11.6,10.20807513));
#220673=CARTESIAN_POINT('Ctrl Pts',(2.66014392499994,15.2,10.209993164));
#220674=CARTESIAN_POINT('Ctrl Pts',(2.66014392499994,11.6,10.209993164));
#220675=CARTESIAN_POINT('Ctrl Pts',(2.66024522199994,15.2,10.21191848));
#220676=CARTESIAN_POINT('Ctrl Pts',(2.66024522199994,11.6,10.21191848));
#220677=CARTESIAN_POINT('Ctrl Pts',(2.66034513999994,15.2,10.213851061));
#220678=CARTESIAN_POINT('Ctrl Pts',(2.66034513999994,11.6,10.213851061));
#220679=CARTESIAN_POINT('Ctrl Pts',(2.66044366599994,15.2,10.215790892));
#220680=CARTESIAN_POINT('Ctrl Pts',(2.66044366599994,11.6,10.215790892));
#220681=CARTESIAN_POINT('Ctrl Pts',(2.66054078599995,15.2,10.217737957));
#220682=CARTESIAN_POINT('Ctrl Pts',(2.66054078599995,11.6,10.217737957));
#220683=CARTESIAN_POINT('Ctrl Pts',(2.66063649099994,15.2,10.219692243));
#220684=CARTESIAN_POINT('Ctrl Pts',(2.66063649099994,11.6,10.219692243));
#220685=CARTESIAN_POINT('Ctrl Pts',(2.66073076499994,15.2,10.221653733));
#220686=CARTESIAN_POINT('Ctrl Pts',(2.66073076499994,11.6,10.221653733));
#220687=CARTESIAN_POINT('Ctrl Pts',(2.66082359799994,15.2,10.223622414));
#220688=CARTESIAN_POINT('Ctrl Pts',(2.66082359799994,11.6,10.223622414));
#220689=CARTESIAN_POINT('Ctrl Pts',(2.66091497699994,15.2,10.22559827));
#220690=CARTESIAN_POINT('Ctrl Pts',(2.66091497699994,11.6,10.22559827));
#220691=CARTESIAN_POINT('Ctrl Pts',(2.66100488899994,15.2,10.227581285));
#220692=CARTESIAN_POINT('Ctrl Pts',(2.66100488899994,11.6,10.227581285));
#220693=CARTESIAN_POINT('Ctrl Pts',(2.66109332099994,15.2,10.229571446));
#220694=CARTESIAN_POINT('Ctrl Pts',(2.66109332099994,11.6,10.229571446));
#220695=CARTESIAN_POINT('Ctrl Pts',(2.66118026299994,15.2,10.231568737));
#220696=CARTESIAN_POINT('Ctrl Pts',(2.66118026299994,11.6,10.231568737));
#220697=CARTESIAN_POINT('Ctrl Pts',(2.66126570199994,15.2,10.233573145));
#220698=CARTESIAN_POINT('Ctrl Pts',(2.66126570199994,11.6,10.233573145));
#220699=CARTESIAN_POINT('Ctrl Pts',(2.66134962599994,15.2,10.235584653));
#220700=CARTESIAN_POINT('Ctrl Pts',(2.66134962599994,11.6,10.235584653));
#220701=CARTESIAN_POINT('Ctrl Pts',(2.66143202199994,15.2,10.237603247));
#220702=CARTESIAN_POINT('Ctrl Pts',(2.66143202199994,11.6,10.237603247));
#220703=CARTESIAN_POINT('Ctrl Pts',(2.66151287899994,15.2,10.239628914));
#220704=CARTESIAN_POINT('Ctrl Pts',(2.66151287899994,11.6,10.239628914));
#220705=CARTESIAN_POINT('Ctrl Pts',(2.66159218399994,15.2,10.241661637));
#220706=CARTESIAN_POINT('Ctrl Pts',(2.66159218399994,11.6,10.241661637));
#220707=CARTESIAN_POINT('Ctrl Pts',(2.66166992699994,15.2,10.243701404));
#220708=CARTESIAN_POINT('Ctrl Pts',(2.66166992699994,11.6,10.243701404));
#220709=CARTESIAN_POINT('Ctrl Pts',(2.66174609499994,15.2,10.245748197));
#220710=CARTESIAN_POINT('Ctrl Pts',(2.66174609499994,11.6,10.245748197));
#220711=CARTESIAN_POINT('Ctrl Pts',(2.66182067499994,15.2,10.247802005));
#220712=CARTESIAN_POINT('Ctrl Pts',(2.66182067499994,11.6,10.247802005));
#220713=CARTESIAN_POINT('Ctrl Pts',(2.66189365799995,15.2,10.249862812));
#220714=CARTESIAN_POINT('Ctrl Pts',(2.66189365799995,11.6,10.249862812));
#220715=CARTESIAN_POINT('Ctrl Pts',(2.66196502999994,15.2,10.251930604));
#220716=CARTESIAN_POINT('Ctrl Pts',(2.66196502999994,11.6,10.251930604));
#220717=CARTESIAN_POINT('Ctrl Pts',(2.66203477999994,15.2,10.254005366));
#220718=CARTESIAN_POINT('Ctrl Pts',(2.66203477999994,11.6,10.254005366));
#220719=CARTESIAN_POINT('Ctrl Pts',(2.66210289699994,15.2,10.256087084));
#220720=CARTESIAN_POINT('Ctrl Pts',(2.66210289699994,11.6,10.256087084));
#220721=CARTESIAN_POINT('Ctrl Pts',(2.66216936799994,15.2,10.258175744));
#220722=CARTESIAN_POINT('Ctrl Pts',(2.66216936799994,11.6,10.258175744));
#220723=CARTESIAN_POINT('Ctrl Pts',(2.66223418299994,15.2,10.260271332));
#220724=CARTESIAN_POINT('Ctrl Pts',(2.66223418299994,11.6,10.260271332));
#220725=CARTESIAN_POINT('Ctrl Pts',(2.66229732999994,15.2,10.262373833));
#220726=CARTESIAN_POINT('Ctrl Pts',(2.66229732999994,11.6,10.262373833));
#220727=CARTESIAN_POINT('Ctrl Pts',(2.66235879699994,15.2,10.264483234));
#220728=CARTESIAN_POINT('Ctrl Pts',(2.66235879699994,11.6,10.264483234));
#220729=CARTESIAN_POINT('Ctrl Pts',(2.66241857399995,15.2,10.266599519));
#220730=CARTESIAN_POINT('Ctrl Pts',(2.66241857399995,11.6,10.266599519));
#220731=CARTESIAN_POINT('Ctrl Pts',(2.66247664799995,15.2,10.268722676));
#220732=CARTESIAN_POINT('Ctrl Pts',(2.66247664799995,11.6,10.268722676));
#220733=CARTESIAN_POINT('Ctrl Pts',(2.66253300899994,15.2,10.270852689));
#220734=CARTESIAN_POINT('Ctrl Pts',(2.66253300899994,11.6,10.270852689));
#220735=CARTESIAN_POINT('Ctrl Pts',(2.66258764499995,15.2,10.272989546));
#220736=CARTESIAN_POINT('Ctrl Pts',(2.66258764499995,11.6,10.272989546));
#220737=CARTESIAN_POINT('Ctrl Pts',(2.66264054499994,15.2,10.275133232));
#220738=CARTESIAN_POINT('Ctrl Pts',(2.66264054499994,11.6,10.275133232));
#220739=CARTESIAN_POINT('Ctrl Pts',(2.66269169899994,15.2,10.277283732));
#220740=CARTESIAN_POINT('Ctrl Pts',(2.66269169899994,11.6,10.277283732));
#220741=CARTESIAN_POINT('Ctrl Pts',(2.66274109399995,15.2,10.279441035));
#220742=CARTESIAN_POINT('Ctrl Pts',(2.66274109399995,11.6,10.279441035));
#220743=CARTESIAN_POINT('Ctrl Pts',(2.66278871999994,15.2,10.281605124));
#220744=CARTESIAN_POINT('Ctrl Pts',(2.66278871999994,11.6,10.281605124));
#220745=CARTESIAN_POINT('Ctrl Pts',(2.66283456499994,15.2,10.283775987));
#220746=CARTESIAN_POINT('Ctrl Pts',(2.66283456499994,11.6,10.283775987));
#220747=CARTESIAN_POINT('Ctrl Pts',(2.66287861899994,15.2,10.285953609));
#220748=CARTESIAN_POINT('Ctrl Pts',(2.66287861899994,11.6,10.285953609));
#220749=CARTESIAN_POINT('Ctrl Pts',(2.66292087099994,15.2,10.288137978));
#220750=CARTESIAN_POINT('Ctrl Pts',(2.66292087099994,11.6,10.288137978));
#220751=CARTESIAN_POINT('Ctrl Pts',(2.66296130999994,15.2,10.290329079));
#220752=CARTESIAN_POINT('Ctrl Pts',(2.66296130999994,11.6,10.290329079));
#220753=CARTESIAN_POINT('Ctrl Pts',(2.66299992499994,15.2,10.292526899));
#220754=CARTESIAN_POINT('Ctrl Pts',(2.66299992499994,11.6,10.292526899));
#220755=CARTESIAN_POINT('Ctrl Pts',(2.66303670499994,15.2,10.294731424));
#220756=CARTESIAN_POINT('Ctrl Pts',(2.66303670499994,11.6,10.294731424));
#220757=CARTESIAN_POINT('Ctrl Pts',(2.66307164099994,15.2,10.29694264));
#220758=CARTESIAN_POINT('Ctrl Pts',(2.66307164099994,11.6,10.29694264));
#220759=CARTESIAN_POINT('Ctrl Pts',(2.66310471899994,15.2,10.299160533));
#220760=CARTESIAN_POINT('Ctrl Pts',(2.66310471899994,11.6,10.299160533));
#220761=CARTESIAN_POINT('Ctrl Pts',(2.66313593099994,15.2,10.301385091));
#220762=CARTESIAN_POINT('Ctrl Pts',(2.66313593099994,11.6,10.301385091));
#220763=CARTESIAN_POINT('Ctrl Pts',(2.66316526499994,15.2,10.3036163));
#220764=CARTESIAN_POINT('Ctrl Pts',(2.66316526499994,11.6,10.3036163));
#220765=CARTESIAN_POINT('Ctrl Pts',(2.66319271099994,15.2,10.305854146));
#220766=CARTESIAN_POINT('Ctrl Pts',(2.66319271099994,11.6,10.305854146));
#220767=CARTESIAN_POINT('Ctrl Pts',(2.66321825799994,15.2,10.308098616));
#220768=CARTESIAN_POINT('Ctrl Pts',(2.66321825799994,11.6,10.308098616));
#220769=CARTESIAN_POINT('Ctrl Pts',(2.66324189699994,15.2,10.310349697));
#220770=CARTESIAN_POINT('Ctrl Pts',(2.66324189699994,11.6,10.310349697));
#220771=CARTESIAN_POINT('Ctrl Pts',(2.66326361499994,15.2,10.312607375));
#220772=CARTESIAN_POINT('Ctrl Pts',(2.66326361499994,11.6,10.312607375));
#220773=CARTESIAN_POINT('Ctrl Pts',(2.66328340399994,15.2,10.314871635));
#220774=CARTESIAN_POINT('Ctrl Pts',(2.66328340399994,11.6,10.314871635));
#220775=CARTESIAN_POINT('Ctrl Pts',(2.66330125199994,15.2,10.317142467));
#220776=CARTESIAN_POINT('Ctrl Pts',(2.66330125199994,11.6,10.317142467));
#220777=CARTESIAN_POINT('Ctrl Pts',(2.66331714899994,15.2,10.319419856));
#220778=CARTESIAN_POINT('Ctrl Pts',(2.66331714899994,11.6,10.319419856));
#220779=CARTESIAN_POINT('Ctrl Pts',(2.66333108599994,15.2,10.321703789));
#220780=CARTESIAN_POINT('Ctrl Pts',(2.66333108599994,11.6,10.321703789));
#220781=CARTESIAN_POINT('Ctrl Pts',(2.66334304999994,15.2,10.323994251));
#220782=CARTESIAN_POINT('Ctrl Pts',(2.66334304999994,11.6,10.323994251));
#220783=CARTESIAN_POINT('Ctrl Pts',(2.66335303299994,15.2,10.326291233));
#220784=CARTESIAN_POINT('Ctrl Pts',(2.66335303299994,11.6,10.326291233));
#220785=CARTESIAN_POINT('Ctrl Pts',(2.66336102399995,15.2,10.328594718));
#220786=CARTESIAN_POINT('Ctrl Pts',(2.66336102399995,11.6,10.328594718));
#220787=CARTESIAN_POINT('Ctrl Pts',(2.66336701299994,15.2,10.330904695));
#220788=CARTESIAN_POINT('Ctrl Pts',(2.66336701299994,11.6,10.330904695));
#220789=CARTESIAN_POINT('Ctrl Pts',(2.66337099099994,15.2,10.33322115));
#220790=CARTESIAN_POINT('Ctrl Pts',(2.66337099099994,11.6,10.33322115));
#220791=CARTESIAN_POINT('Ctrl Pts',(2.66337294499994,15.2,10.33554407));
#220792=CARTESIAN_POINT('Ctrl Pts',(2.66337294499994,11.6,10.33554407));
#220793=CARTESIAN_POINT('Ctrl Pts',(2.66337286799994,15.2,10.337873442));
#220794=CARTESIAN_POINT('Ctrl Pts',(2.66337286799994,11.6,10.337873442));
#220795=CARTESIAN_POINT('Ctrl Pts',(2.66337074899994,15.2,10.340209254));
#220796=CARTESIAN_POINT('Ctrl Pts',(2.66337074899994,11.6,10.340209254));
#220797=CARTESIAN_POINT('Ctrl Pts',(2.66336657799994,15.2,10.342551492));
#220798=CARTESIAN_POINT('Ctrl Pts',(2.66336657799994,11.6,10.342551492));
#220799=CARTESIAN_POINT('Ctrl Pts',(2.66336034299994,15.2,10.344900144));
#220800=CARTESIAN_POINT('Ctrl Pts',(2.66336034299994,11.6,10.344900144));
#220801=CARTESIAN_POINT('Ctrl Pts',(2.66335203699994,15.2,10.347255195));
#220802=CARTESIAN_POINT('Ctrl Pts',(2.66335203699994,11.6,10.347255195));
#220803=CARTESIAN_POINT('Ctrl Pts',(2.66334164999994,15.2,10.349616634));
#220804=CARTESIAN_POINT('Ctrl Pts',(2.66334164999994,11.6,10.349616634));
#220805=CARTESIAN_POINT('Ctrl Pts',(2.66332917099994,15.2,10.351984449));
#220806=CARTESIAN_POINT('Ctrl Pts',(2.66332917099994,11.6,10.351984449));
#220807=CARTESIAN_POINT('Ctrl Pts',(2.66331458999994,15.2,10.354358624));
#220808=CARTESIAN_POINT('Ctrl Pts',(2.66331458999994,11.6,10.354358624));
#220809=CARTESIAN_POINT('Ctrl Pts',(2.66329789899994,15.2,10.35673915));
#220810=CARTESIAN_POINT('Ctrl Pts',(2.66329789899994,11.6,10.35673915));
#220811=CARTESIAN_POINT('Ctrl Pts',(2.66327908599994,15.2,10.359126012));
#220812=CARTESIAN_POINT('Ctrl Pts',(2.66327908599994,11.6,10.359126012));
#220813=CARTESIAN_POINT('Ctrl Pts',(2.66325814399994,15.2,10.361519198));
#220814=CARTESIAN_POINT('Ctrl Pts',(2.66325814399994,11.6,10.361519198));
#220815=CARTESIAN_POINT('Ctrl Pts',(2.66323505999994,15.2,10.363918694));
#220816=CARTESIAN_POINT('Ctrl Pts',(2.66323505999994,11.6,10.363918694));
#220817=CARTESIAN_POINT('Ctrl Pts',(2.66320982799995,15.2,10.36632449));
#220818=CARTESIAN_POINT('Ctrl Pts',(2.66320982799995,11.6,10.36632449));
#220819=CARTESIAN_POINT('Ctrl Pts',(2.66318243599994,15.2,10.368736571));
#220820=CARTESIAN_POINT('Ctrl Pts',(2.66318243599994,11.6,10.368736571));
#220821=CARTESIAN_POINT('Ctrl Pts',(2.66315287499994,15.2,10.371154926));
#220822=CARTESIAN_POINT('Ctrl Pts',(2.66315287499994,11.6,10.371154926));
#220823=CARTESIAN_POINT('Ctrl Pts',(2.66312113599994,15.2,10.37357954));
#220824=CARTESIAN_POINT('Ctrl Pts',(2.66312113599994,11.6,10.37357954));
#220825=CARTESIAN_POINT('Ctrl Pts',(2.66308720999994,15.2,10.376010404));
#220826=CARTESIAN_POINT('Ctrl Pts',(2.66308720999994,11.6,10.376010404));
#220827=CARTESIAN_POINT('Ctrl Pts',(2.66305108599994,15.2,10.378447504));
#220828=CARTESIAN_POINT('Ctrl Pts',(2.66305108599994,11.6,10.378447504));
#220829=CARTESIAN_POINT('Ctrl Pts',(2.66301275499994,15.2,10.380890825));
#220830=CARTESIAN_POINT('Ctrl Pts',(2.66301275499994,11.6,10.380890825));
#220831=CARTESIAN_POINT('Ctrl Pts',(2.66297220899995,15.2,10.383340359));
#220832=CARTESIAN_POINT('Ctrl Pts',(2.66297220899995,11.6,10.383340359));
#220833=CARTESIAN_POINT('Ctrl Pts',(2.66292943799994,15.2,10.385796091));
#220834=CARTESIAN_POINT('Ctrl Pts',(2.66292943799994,11.6,10.385796091));
#220835=CARTESIAN_POINT('Ctrl Pts',(2.66288443199994,15.2,10.388258008));
#220836=CARTESIAN_POINT('Ctrl Pts',(2.66288443199994,11.6,10.388258008));
#220837=CARTESIAN_POINT('Ctrl Pts',(2.66283718399994,15.2,10.3907261));
#220838=CARTESIAN_POINT('Ctrl Pts',(2.66283718399994,11.6,10.3907261));
#220839=CARTESIAN_POINT('Ctrl Pts',(2.66278768199995,15.2,10.393200352));
#220840=CARTESIAN_POINT('Ctrl Pts',(2.66278768199995,11.6,10.393200352));
#220841=CARTESIAN_POINT('Ctrl Pts',(2.66273591799994,15.2,10.395680754));
#220842=CARTESIAN_POINT('Ctrl Pts',(2.66273591799994,11.6,10.395680754));
#220843=CARTESIAN_POINT('Ctrl Pts',(2.66268188299994,15.2,10.398167293));
#220844=CARTESIAN_POINT('Ctrl Pts',(2.66268188299994,11.6,10.398167293));
#220845=CARTESIAN_POINT('Ctrl Pts',(2.66262556799994,15.2,10.400659956));
#220846=CARTESIAN_POINT('Ctrl Pts',(2.66262556799994,11.6,10.400659956));
#220847=CARTESIAN_POINT('Ctrl Pts',(2.66256696299994,15.2,10.40315873));
#220848=CARTESIAN_POINT('Ctrl Pts',(2.66256696299994,11.6,10.40315873));
#220849=CARTESIAN_POINT('Ctrl Pts',(2.66250606099995,15.2,10.405663606));
#220850=CARTESIAN_POINT('Ctrl Pts',(2.66250606099995,11.6,10.405663606));
#220851=CARTESIAN_POINT('Ctrl Pts',(2.66244285099994,15.2,10.408174569));
#220852=CARTESIAN_POINT('Ctrl Pts',(2.66244285099994,11.6,10.408174569));
#220853=CARTESIAN_POINT('Ctrl Pts',(2.66237732499994,15.2,10.410691609));
#220854=CARTESIAN_POINT('Ctrl Pts',(2.66237732499994,11.6,10.410691609));
#220855=CARTESIAN_POINT('Ctrl Pts',(2.66230947199994,15.2,10.413214712));
#220856=CARTESIAN_POINT('Ctrl Pts',(2.66230947199994,11.6,10.413214712));
#220857=CARTESIAN_POINT('Ctrl Pts',(2.66223928699994,15.2,10.415743866));
#220858=CARTESIAN_POINT('Ctrl Pts',(2.66223928699994,11.6,10.415743866));
#220859=CARTESIAN_POINT('Ctrl Pts',(2.66216675899994,15.2,10.418279061));
#220860=CARTESIAN_POINT('Ctrl Pts',(2.66216675899994,11.6,10.418279061));
#220861=CARTESIAN_POINT('Ctrl Pts',(2.66209187899995,15.2,10.420820283));
#220862=CARTESIAN_POINT('Ctrl Pts',(2.66209187899995,11.6,10.420820283));
#220863=CARTESIAN_POINT('Ctrl Pts',(2.66201463799994,15.2,10.42336752));
#220864=CARTESIAN_POINT('Ctrl Pts',(2.66201463799994,11.6,10.42336752));
#220865=CARTESIAN_POINT('Ctrl Pts',(2.66193502799994,15.2,10.425920761));
#220866=CARTESIAN_POINT('Ctrl Pts',(2.66193502799994,11.6,10.425920761));
#220867=CARTESIAN_POINT('Ctrl Pts',(2.66185303999994,15.2,10.428479993));
#220868=CARTESIAN_POINT('Ctrl Pts',(2.66185303999994,11.6,10.428479993));
#220869=CARTESIAN_POINT('Ctrl Pts',(2.66176866499995,15.2,10.431045206));
#220870=CARTESIAN_POINT('Ctrl Pts',(2.66176866499995,11.6,10.431045206));
#220871=CARTESIAN_POINT('Ctrl Pts',(2.66168189399994,15.2,10.433616386));
#220872=CARTESIAN_POINT('Ctrl Pts',(2.66168189399994,11.6,10.433616386));
#220873=CARTESIAN_POINT('Ctrl Pts',(2.66159271899994,15.2,10.436193522));
#220874=CARTESIAN_POINT('Ctrl Pts',(2.66159271899994,11.6,10.436193522));
#220875=CARTESIAN_POINT('Ctrl Pts',(2.66150113199994,15.2,10.438776602));
#220876=CARTESIAN_POINT('Ctrl Pts',(2.66150113199994,11.6,10.438776602));
#220877=CARTESIAN_POINT('Ctrl Pts',(2.66140712299994,15.2,10.441365615));
#220878=CARTESIAN_POINT('Ctrl Pts',(2.66140712299994,11.6,10.441365615));
#220879=CARTESIAN_POINT('Ctrl Pts',(2.66131068499994,15.2,10.443960548));
#220880=CARTESIAN_POINT('Ctrl Pts',(2.66131068499994,11.6,10.443960548));
#220881=CARTESIAN_POINT('Ctrl Pts',(2.66121180899995,15.2,10.44656139));
#220882=CARTESIAN_POINT('Ctrl Pts',(2.66121180899995,11.6,10.44656139));
#220883=CARTESIAN_POINT('Ctrl Pts',(2.66111048499994,15.2,10.449168128));
#220884=CARTESIAN_POINT('Ctrl Pts',(2.66111048499994,11.6,10.449168128));
#220885=CARTESIAN_POINT('Ctrl Pts',(2.66100670699994,15.2,10.451780752));
#220886=CARTESIAN_POINT('Ctrl Pts',(2.66100670699994,11.6,10.451780752));
#220887=CARTESIAN_POINT('Ctrl Pts',(2.66090046499994,15.2,10.45439925));
#220888=CARTESIAN_POINT('Ctrl Pts',(2.66090046499994,11.6,10.45439925));
#220889=CARTESIAN_POINT('Ctrl Pts',(2.66079174899994,15.2,10.457023609));
#220890=CARTESIAN_POINT('Ctrl Pts',(2.66079174899994,11.6,10.457023609));
#220891=CARTESIAN_POINT('Ctrl Pts',(2.66068055499994,15.2,10.459653818));
#220892=CARTESIAN_POINT('Ctrl Pts',(2.66068055499994,11.6,10.459653818));
#220893=CARTESIAN_POINT('Ctrl Pts',(2.66056687099995,15.2,10.462289868));
#220894=CARTESIAN_POINT('Ctrl Pts',(2.66056687099995,11.6,10.462289868));
#220895=CARTESIAN_POINT('Ctrl Pts',(2.66045068999994,15.2,10.464931742));
#220896=CARTESIAN_POINT('Ctrl Pts',(2.66045068999994,11.6,10.464931742));
#220897=CARTESIAN_POINT('Ctrl Pts',(2.66033200499994,15.2,10.467579433));
#220898=CARTESIAN_POINT('Ctrl Pts',(2.66033200499994,11.6,10.467579433));
#220899=CARTESIAN_POINT('Ctrl Pts',(2.66021080499995,15.2,10.470232928));
#220900=CARTESIAN_POINT('Ctrl Pts',(2.66021080499995,11.6,10.470232928));
#220901=CARTESIAN_POINT('Ctrl Pts',(2.66008708299994,15.2,10.472892215));
#220902=CARTESIAN_POINT('Ctrl Pts',(2.66008708299994,11.6,10.472892215));
#220903=CARTESIAN_POINT('Ctrl Pts',(2.65996083199994,15.2,10.475557283));
#220904=CARTESIAN_POINT('Ctrl Pts',(2.65996083199994,11.6,10.475557283));
#220905=CARTESIAN_POINT('Ctrl Pts',(2.65983204199994,15.2,10.47822812));
#220906=CARTESIAN_POINT('Ctrl Pts',(2.65983204199994,11.6,10.47822812));
#220907=CARTESIAN_POINT('Ctrl Pts',(2.65970070699994,15.2,10.480904716));
#220908=CARTESIAN_POINT('Ctrl Pts',(2.65970070699994,11.6,10.480904716));
#220909=CARTESIAN_POINT('Ctrl Pts',(2.65956681699994,15.2,10.483587057));
#220910=CARTESIAN_POINT('Ctrl Pts',(2.65956681699994,11.6,10.483587057));
#220911=CARTESIAN_POINT('Ctrl Pts',(2.65943036399995,15.2,10.486275135));
#220912=CARTESIAN_POINT('Ctrl Pts',(2.65943036399995,11.6,10.486275135));
#220913=CARTESIAN_POINT('Ctrl Pts',(2.65929134199994,15.2,10.488968935));
#220914=CARTESIAN_POINT('Ctrl Pts',(2.65929134199994,11.6,10.488968935));
#220915=CARTESIAN_POINT('Ctrl Pts',(2.65914973999994,15.2,10.491668448));
#220916=CARTESIAN_POINT('Ctrl Pts',(2.65914973999994,11.6,10.491668448));
#220917=CARTESIAN_POINT('Ctrl Pts',(2.65900555199994,15.2,10.494373663));
#220918=CARTESIAN_POINT('Ctrl Pts',(2.65900555199994,11.6,10.494373663));
#220919=CARTESIAN_POINT('Ctrl Pts',(2.65885876999994,15.2,10.497084567));
#220920=CARTESIAN_POINT('Ctrl Pts',(2.65885876999994,11.6,10.497084567));
#220921=CARTESIAN_POINT('Ctrl Pts',(2.65870938599994,15.2,10.499801148));
#220922=CARTESIAN_POINT('Ctrl Pts',(2.65870938599994,11.6,10.499801148));
#220923=CARTESIAN_POINT('Ctrl Pts',(2.65855739099994,15.2,10.502523398));
#220924=CARTESIAN_POINT('Ctrl Pts',(2.65855739099994,11.6,10.502523398));
#220925=CARTESIAN_POINT('Ctrl Pts',(2.65840277899994,15.2,10.505251304));
#220926=CARTESIAN_POINT('Ctrl Pts',(2.65840277899994,11.6,10.505251304));
#220927=CARTESIAN_POINT('Ctrl Pts',(2.65824553999995,15.2,10.507984853));
#220928=CARTESIAN_POINT('Ctrl Pts',(2.65824553999995,11.6,10.507984853));
#220929=CARTESIAN_POINT('Ctrl Pts',(2.65808566799994,15.2,10.510724037));
#220930=CARTESIAN_POINT('Ctrl Pts',(2.65808566799994,11.6,10.510724037));
#220931=CARTESIAN_POINT('Ctrl Pts',(2.65792315399994,15.2,10.513468843));
#220932=CARTESIAN_POINT('Ctrl Pts',(2.65792315399994,11.6,10.513468843));
#220933=CARTESIAN_POINT('Ctrl Pts',(2.65775799099994,15.2,10.51621926));
#220934=CARTESIAN_POINT('Ctrl Pts',(2.65775799099994,11.6,10.51621926));
#220935=CARTESIAN_POINT('Ctrl Pts',(2.65759017099994,15.2,10.518975277));
#220936=CARTESIAN_POINT('Ctrl Pts',(2.65759017099994,11.6,10.518975277));
#220937=CARTESIAN_POINT('Ctrl Pts',(2.65741968699994,15.2,10.521736883));
#220938=CARTESIAN_POINT('Ctrl Pts',(2.65741968699994,11.6,10.521736883));
#220939=CARTESIAN_POINT('Ctrl Pts',(2.65724653099995,15.2,10.524504067));
#220940=CARTESIAN_POINT('Ctrl Pts',(2.65724653099995,11.6,10.524504067));
#220941=CARTESIAN_POINT('Ctrl Pts',(2.65707069399994,15.2,10.527276817));
#220942=CARTESIAN_POINT('Ctrl Pts',(2.65707069399994,11.6,10.527276817));
#220943=CARTESIAN_POINT('Ctrl Pts',(2.65689216999994,15.2,10.530055124));
#220944=CARTESIAN_POINT('Ctrl Pts',(2.65689216999994,11.6,10.530055124));
#220945=CARTESIAN_POINT('Ctrl Pts',(2.65671094999994,15.2,10.532838975));
#220946=CARTESIAN_POINT('Ctrl Pts',(2.65671094999994,11.6,10.532838975));
#220947=CARTESIAN_POINT('Ctrl Pts',(2.65652702799994,15.2,10.535628359));
#220948=CARTESIAN_POINT('Ctrl Pts',(2.65652702799994,11.6,10.535628359));
#220949=CARTESIAN_POINT('Ctrl Pts',(2.65634039499994,15.2,10.538423266));
#220950=CARTESIAN_POINT('Ctrl Pts',(2.65634039499994,11.6,10.538423266));
#220951=CARTESIAN_POINT('Ctrl Pts',(2.65615104499994,15.2,10.541223686));
#220952=CARTESIAN_POINT('Ctrl Pts',(2.65615104499994,11.6,10.541223686));
#220953=CARTESIAN_POINT('Ctrl Pts',(2.65595896999994,15.2,10.544029606));
#220954=CARTESIAN_POINT('Ctrl Pts',(2.65595896999994,11.6,10.544029606));
#220955=CARTESIAN_POINT('Ctrl Pts',(2.65576416199994,15.2,10.546841015));
#220956=CARTESIAN_POINT('Ctrl Pts',(2.65576416199994,11.6,10.546841015));
#220957=CARTESIAN_POINT('Ctrl Pts',(2.65556661299994,15.2,10.549657904));
#220958=CARTESIAN_POINT('Ctrl Pts',(2.65556661299994,11.6,10.549657904));
#220959=CARTESIAN_POINT('Ctrl Pts',(2.65536631799994,15.2,10.552480261));
#220960=CARTESIAN_POINT('Ctrl Pts',(2.65536631799994,11.6,10.552480261));
#220961=CARTESIAN_POINT('Ctrl Pts',(2.65516326699994,15.2,10.555308075));
#220962=CARTESIAN_POINT('Ctrl Pts',(2.65516326699994,11.6,10.555308075));
#220963=CARTESIAN_POINT('Ctrl Pts',(2.65495745399994,15.2,10.558141336));
#220964=CARTESIAN_POINT('Ctrl Pts',(2.65495745399994,11.6,10.558141336));
#220965=CARTESIAN_POINT('Ctrl Pts',(2.65474887199994,15.2,10.560980032));
#220966=CARTESIAN_POINT('Ctrl Pts',(2.65474887199994,11.6,10.560980032));
#220967=CARTESIAN_POINT('Ctrl Pts',(2.65453751199995,15.2,10.563824153));
#220968=CARTESIAN_POINT('Ctrl Pts',(2.65453751199995,11.6,10.563824153));
#220969=CARTESIAN_POINT('Ctrl Pts',(2.65432336899994,15.2,10.566673688));
#220970=CARTESIAN_POINT('Ctrl Pts',(2.65432336899994,11.6,10.566673688));
#220971=CARTESIAN_POINT('Ctrl Pts',(2.65410643399994,15.2,10.569528625));
#220972=CARTESIAN_POINT('Ctrl Pts',(2.65410643399994,11.6,10.569528625));
#220973=CARTESIAN_POINT('Ctrl Pts',(2.65388669999994,15.2,10.572388957));
#220974=CARTESIAN_POINT('Ctrl Pts',(2.65388669999994,11.6,10.572388957));
#220975=CARTESIAN_POINT('Ctrl Pts',(2.65366415999994,15.2,10.575254668));
#220976=CARTESIAN_POINT('Ctrl Pts',(2.65366415999994,11.6,10.575254668));
#220977=CARTESIAN_POINT('Ctrl Pts',(2.65343880799994,15.2,10.578125753));
#220978=CARTESIAN_POINT('Ctrl Pts',(2.65343880799994,11.6,10.578125753));
#220979=CARTESIAN_POINT('Ctrl Pts',(2.65321063499994,15.2,10.581002197));
#220980=CARTESIAN_POINT('Ctrl Pts',(2.65321063499994,11.6,10.581002197));
#220981=CARTESIAN_POINT('Ctrl Pts',(2.65297963499994,15.2,10.583883991));
#220982=CARTESIAN_POINT('Ctrl Pts',(2.65297963499994,11.6,10.583883991));
#220983=CARTESIAN_POINT('Ctrl Pts',(2.65274580099994,15.2,10.586771124));
#220984=CARTESIAN_POINT('Ctrl Pts',(2.65274580099994,11.6,10.586771124));
#220985=CARTESIAN_POINT('Ctrl Pts',(2.65250912499994,15.2,10.589663585));
#220986=CARTESIAN_POINT('Ctrl Pts',(2.65250912499994,11.6,10.589663585));
#220987=CARTESIAN_POINT('Ctrl Pts',(2.65226959999994,15.2,10.592561365));
#220988=CARTESIAN_POINT('Ctrl Pts',(2.65226959999994,11.6,10.592561365));
#220989=CARTESIAN_POINT('Ctrl Pts',(2.65202722099994,15.2,10.595464452));
#220990=CARTESIAN_POINT('Ctrl Pts',(2.65202722099994,11.6,10.595464452));
#220991=CARTESIAN_POINT('Ctrl Pts',(2.65178197899994,15.2,10.598372837));
#220992=CARTESIAN_POINT('Ctrl Pts',(2.65178197899994,11.6,10.598372837));
#220993=CARTESIAN_POINT('Ctrl Pts',(2.65153386699994,15.2,10.601286506));
#220994=CARTESIAN_POINT('Ctrl Pts',(2.65153386699994,11.6,10.601286506));
#220995=CARTESIAN_POINT('Ctrl Pts',(2.65128287799994,15.2,10.604205452));
#220996=CARTESIAN_POINT('Ctrl Pts',(2.65128287799994,11.6,10.604205452));
#220997=CARTESIAN_POINT('Ctrl Pts',(2.65102900699994,15.2,10.607129663));
#220998=CARTESIAN_POINT('Ctrl Pts',(2.65102900699994,11.6,10.607129663));
#220999=CARTESIAN_POINT('Ctrl Pts',(2.65077224499994,15.2,10.61005913));
#221000=CARTESIAN_POINT('Ctrl Pts',(2.65077224499994,11.6,10.61005913));
#221001=CARTESIAN_POINT('Ctrl Pts',(2.65051258499994,15.2,10.61299384));
#221002=CARTESIAN_POINT('Ctrl Pts',(2.65051258499994,11.6,10.61299384));
#221003=CARTESIAN_POINT('Ctrl Pts',(2.65025002199994,15.2,10.615933784));
#221004=CARTESIAN_POINT('Ctrl Pts',(2.65025002199994,11.6,10.615933784));
#221005=CARTESIAN_POINT('Ctrl Pts',(2.64998454799994,15.2,10.618878952));
#221006=CARTESIAN_POINT('Ctrl Pts',(2.64998454799994,11.6,10.618878952));
#221007=CARTESIAN_POINT('Ctrl Pts',(2.64971615599995,15.2,10.621829333));
#221008=CARTESIAN_POINT('Ctrl Pts',(2.64971615599995,11.6,10.621829333));
#221009=CARTESIAN_POINT('Ctrl Pts',(2.64944483999995,15.2,10.624784916));
#221010=CARTESIAN_POINT('Ctrl Pts',(2.64944483999995,11.6,10.624784916));
#221011=CARTESIAN_POINT('Ctrl Pts',(2.64917059199994,15.2,10.627745693));
#221012=CARTESIAN_POINT('Ctrl Pts',(2.64917059199994,11.6,10.627745693));
#221013=CARTESIAN_POINT('Ctrl Pts',(2.64889340699995,15.2,10.63071165));
#221014=CARTESIAN_POINT('Ctrl Pts',(2.64889340699995,11.6,10.63071165));
#221015=CARTESIAN_POINT('Ctrl Pts',(2.64861327699994,15.2,10.63368278));
#221016=CARTESIAN_POINT('Ctrl Pts',(2.64861327699994,11.6,10.63368278));
#221017=CARTESIAN_POINT('Ctrl Pts',(2.64833019499994,15.2,10.636659071));
#221018=CARTESIAN_POINT('Ctrl Pts',(2.64833019499994,11.6,10.636659071));
#221019=CARTESIAN_POINT('Ctrl Pts',(2.64804415599994,15.2,10.639640513));
#221020=CARTESIAN_POINT('Ctrl Pts',(2.64804415599994,11.6,10.639640513));
#221021=CARTESIAN_POINT('Ctrl Pts',(2.64775515099994,15.2,10.642627096));
#221022=CARTESIAN_POINT('Ctrl Pts',(2.64775515099994,11.6,10.642627096));
#221023=CARTESIAN_POINT('Ctrl Pts',(2.64746317599994,15.2,10.645618809));
#221024=CARTESIAN_POINT('Ctrl Pts',(2.64746317599994,11.6,10.645618809));
#221025=CARTESIAN_POINT('Ctrl Pts',(2.64716822299994,15.2,10.648615642));
#221026=CARTESIAN_POINT('Ctrl Pts',(2.64716822299994,11.6,10.648615642));
#221027=CARTESIAN_POINT('Ctrl Pts',(2.64687028499994,15.2,10.651617586));
#221028=CARTESIAN_POINT('Ctrl Pts',(2.64687028499994,11.6,10.651617586));
#221029=CARTESIAN_POINT('Ctrl Pts',(2.64656935599994,15.2,10.65462463));
#221030=CARTESIAN_POINT('Ctrl Pts',(2.64656935599994,11.6,10.65462463));
#221031=CARTESIAN_POINT('Ctrl Pts',(2.64626542899994,15.2,10.657636762));
#221032=CARTESIAN_POINT('Ctrl Pts',(2.64626542899994,11.6,10.657636762));
#221033=CARTESIAN_POINT('Ctrl Pts',(2.64595849899994,15.2,10.660653975));
#221034=CARTESIAN_POINT('Ctrl Pts',(2.64595849899994,11.6,10.660653975));
#221035=CARTESIAN_POINT('Ctrl Pts',(2.64564855699994,15.2,10.663676257));
#221036=CARTESIAN_POINT('Ctrl Pts',(2.64564855699994,11.6,10.663676257));
#221037=CARTESIAN_POINT('Ctrl Pts',(2.64533559999995,15.2,10.666703598));
#221038=CARTESIAN_POINT('Ctrl Pts',(2.64533559999995,11.6,10.666703598));
#221039=CARTESIAN_POINT('Ctrl Pts',(2.64501961799994,15.2,10.669735989));
#221040=CARTESIAN_POINT('Ctrl Pts',(2.64501961799994,11.6,10.669735989));
#221041=CARTESIAN_POINT('Ctrl Pts',(2.64470060599994,15.2,10.672773419));
#221042=CARTESIAN_POINT('Ctrl Pts',(2.64470060599994,11.6,10.672773419));
#221043=CARTESIAN_POINT('Ctrl Pts',(2.64437855799994,15.2,10.675815876));
#221044=CARTESIAN_POINT('Ctrl Pts',(2.64437855799994,11.6,10.675815876));
#221045=CARTESIAN_POINT('Ctrl Pts',(2.64405346699994,15.2,10.678863354));
#221046=CARTESIAN_POINT('Ctrl Pts',(2.64405346699994,11.6,10.678863354));
#221047=CARTESIAN_POINT('Ctrl Pts',(2.64372532799994,15.2,10.68191584));
#221048=CARTESIAN_POINT('Ctrl Pts',(2.64372532799994,11.6,10.68191584));
#221049=CARTESIAN_POINT('Ctrl Pts',(2.64339413299994,15.2,10.684973325));
#221050=CARTESIAN_POINT('Ctrl Pts',(2.64339413299994,11.6,10.684973325));
#221051=CARTESIAN_POINT('Ctrl Pts',(2.64305987599994,15.2,10.688035799));
#221052=CARTESIAN_POINT('Ctrl Pts',(2.64305987599994,11.6,10.688035799));
#221053=CARTESIAN_POINT('Ctrl Pts',(2.64272255199994,15.2,10.691103251));
#221054=CARTESIAN_POINT('Ctrl Pts',(2.64272255199994,11.6,10.691103251));
#221055=CARTESIAN_POINT('Ctrl Pts',(2.64238215299994,15.2,10.694175673));
#221056=CARTESIAN_POINT('Ctrl Pts',(2.64238215299994,11.6,10.694175673));
#221057=CARTESIAN_POINT('Ctrl Pts',(2.64203867399994,15.2,10.697253054));
#221058=CARTESIAN_POINT('Ctrl Pts',(2.64203867399994,11.6,10.697253054));
#221059=CARTESIAN_POINT('Ctrl Pts',(2.64169210799994,15.2,10.700335382));
#221060=CARTESIAN_POINT('Ctrl Pts',(2.64169210799994,11.6,10.700335382));
#221061=CARTESIAN_POINT('Ctrl Pts',(2.64134244799994,15.2,10.703422651));
#221062=CARTESIAN_POINT('Ctrl Pts',(2.64134244799994,11.6,10.703422651));
#221063=CARTESIAN_POINT('Ctrl Pts',(2.64098969099994,15.2,10.706514848));
#221064=CARTESIAN_POINT('Ctrl Pts',(2.64098969099994,11.6,10.706514848));
#221065=CARTESIAN_POINT('Ctrl Pts',(2.64063382699995,15.2,10.709611966));
#221066=CARTESIAN_POINT('Ctrl Pts',(2.64063382699995,11.6,10.709611966));
#221067=CARTESIAN_POINT('Ctrl Pts',(2.64027485199994,15.2,10.712713991));
#221068=CARTESIAN_POINT('Ctrl Pts',(2.64027485199994,11.6,10.712713991));
#221069=CARTESIAN_POINT('Ctrl Pts',(2.63991275999994,15.2,10.715820917));
#221070=CARTESIAN_POINT('Ctrl Pts',(2.63991275999994,11.6,10.715820917));
#221071=CARTESIAN_POINT('Ctrl Pts',(2.63954754299994,15.2,10.718932732));
#221072=CARTESIAN_POINT('Ctrl Pts',(2.63954754299994,11.6,10.718932732));
#221073=CARTESIAN_POINT('Ctrl Pts',(2.63917919799994,15.2,10.722049427));
#221074=CARTESIAN_POINT('Ctrl Pts',(2.63917919799994,11.6,10.722049427));
#221075=CARTESIAN_POINT('Ctrl Pts',(2.63880771699994,15.2,10.725170991));
#221076=CARTESIAN_POINT('Ctrl Pts',(2.63880771699994,11.6,10.725170991));
#221077=CARTESIAN_POINT('Ctrl Pts',(2.63843309399994,15.2,10.728297417));
#221078=CARTESIAN_POINT('Ctrl Pts',(2.63843309399994,11.6,10.728297417));
#221079=CARTESIAN_POINT('Ctrl Pts',(2.63805532199994,15.2,10.731428692));
#221080=CARTESIAN_POINT('Ctrl Pts',(2.63805532199994,11.6,10.731428692));
#221081=CARTESIAN_POINT('Ctrl Pts',(2.63767439799994,15.2,10.734564809));
#221082=CARTESIAN_POINT('Ctrl Pts',(2.63767439799994,11.6,10.734564809));
#221083=CARTESIAN_POINT('Ctrl Pts',(2.63729031299994,15.2,10.737705755));
#221084=CARTESIAN_POINT('Ctrl Pts',(2.63729031299994,11.6,10.737705755));
#221085=CARTESIAN_POINT('Ctrl Pts',(2.63690306199994,15.2,10.740851524));
#221086=CARTESIAN_POINT('Ctrl Pts',(2.63690306199994,11.6,10.740851524));
#221087=CARTESIAN_POINT('Ctrl Pts',(2.63651263999995,15.2,10.744002104));
#221088=CARTESIAN_POINT('Ctrl Pts',(2.63651263999995,11.6,10.744002104));
#221089=CARTESIAN_POINT('Ctrl Pts',(2.63611903999994,15.2,10.747157485));
#221090=CARTESIAN_POINT('Ctrl Pts',(2.63611903999994,11.6,10.747157485));
#221091=CARTESIAN_POINT('Ctrl Pts',(2.63572225699995,15.2,10.750317659));
#221092=CARTESIAN_POINT('Ctrl Pts',(2.63572225699995,11.6,10.750317659));
#221093=CARTESIAN_POINT('Ctrl Pts',(2.63532228399994,15.2,10.753482615));
#221094=CARTESIAN_POINT('Ctrl Pts',(2.63532228399994,11.6,10.753482615));
#221095=CARTESIAN_POINT('Ctrl Pts',(2.63491911699994,15.2,10.756652344));
#221096=CARTESIAN_POINT('Ctrl Pts',(2.63491911699994,11.6,10.756652344));
#221097=CARTESIAN_POINT('Ctrl Pts',(2.63451274799994,15.2,10.759826836));
#221098=CARTESIAN_POINT('Ctrl Pts',(2.63451274799994,11.6,10.759826836));
#221099=CARTESIAN_POINT('Ctrl Pts',(2.63410317099994,15.2,10.763006082));
#221100=CARTESIAN_POINT('Ctrl Pts',(2.63410317099994,11.6,10.763006082));
#221101=CARTESIAN_POINT('Ctrl Pts',(2.63369038199994,15.2,10.766190072));
#221102=CARTESIAN_POINT('Ctrl Pts',(2.63369038199994,11.6,10.766190072));
#221103=CARTESIAN_POINT('Ctrl Pts',(2.63327437499994,15.2,10.769378796));
#221104=CARTESIAN_POINT('Ctrl Pts',(2.63327437499994,11.6,10.769378796));
#221105=CARTESIAN_POINT('Ctrl Pts',(2.63285514299994,15.2,10.772572244));
#221106=CARTESIAN_POINT('Ctrl Pts',(2.63285514299994,11.6,10.772572244));
#221107=CARTESIAN_POINT('Ctrl Pts',(2.63243268299994,15.2,10.775770408));
#221108=CARTESIAN_POINT('Ctrl Pts',(2.63243268299994,11.6,10.775770408));
#221109=CARTESIAN_POINT('Ctrl Pts',(2.63200698499995,15.2,10.778973278));
#221110=CARTESIAN_POINT('Ctrl Pts',(2.63200698499995,11.6,10.778973278));
#221111=CARTESIAN_POINT('Ctrl Pts',(2.63157804599994,15.2,10.782180844));
#221112=CARTESIAN_POINT('Ctrl Pts',(2.63157804599994,11.6,10.782180844));
#221113=CARTESIAN_POINT('Ctrl Pts',(2.63114586099995,15.2,10.785393097));
#221114=CARTESIAN_POINT('Ctrl Pts',(2.63114586099995,11.6,10.785393097));
#221115=CARTESIAN_POINT('Ctrl Pts',(2.63071042299994,15.2,10.788610025));
#221116=CARTESIAN_POINT('Ctrl Pts',(2.63071042299994,11.6,10.788610025));
#221117=CARTESIAN_POINT('Ctrl Pts',(2.63027172599994,15.2,10.791831623));
#221118=CARTESIAN_POINT('Ctrl Pts',(2.63027172599994,11.6,10.791831623));
#221119=CARTESIAN_POINT('Ctrl Pts',(2.62982976499994,15.2,10.795057878));
#221120=CARTESIAN_POINT('Ctrl Pts',(2.62982976499994,11.6,10.795057878));
#221121=CARTESIAN_POINT('Ctrl Pts',(2.62938453499994,15.2,10.798288782));
#221122=CARTESIAN_POINT('Ctrl Pts',(2.62938453499994,11.6,10.798288782));
#221123=CARTESIAN_POINT('Ctrl Pts',(2.62893602899994,15.2,10.801524325));
#221124=CARTESIAN_POINT('Ctrl Pts',(2.62893602899994,11.6,10.801524325));
#221125=CARTESIAN_POINT('Ctrl Pts',(2.62848424199994,15.2,10.804764499));
#221126=CARTESIAN_POINT('Ctrl Pts',(2.62848424199994,11.6,10.804764499));
#221127=CARTESIAN_POINT('Ctrl Pts',(2.62802916999994,15.2,10.808009293));
#221128=CARTESIAN_POINT('Ctrl Pts',(2.62802916999994,11.6,10.808009293));
#221129=CARTESIAN_POINT('Ctrl Pts',(2.62757080599994,15.2,10.811258697));
#221130=CARTESIAN_POINT('Ctrl Pts',(2.62757080599994,11.6,10.811258697));
#221131=CARTESIAN_POINT('Ctrl Pts',(2.62710914299995,15.2,10.814512704));
#221132=CARTESIAN_POINT('Ctrl Pts',(2.62710914299995,11.6,10.814512704));
#221133=CARTESIAN_POINT('Ctrl Pts',(2.62664417899994,15.2,10.817771303));
#221134=CARTESIAN_POINT('Ctrl Pts',(2.62664417899994,11.6,10.817771303));
#221135=CARTESIAN_POINT('Ctrl Pts',(2.62617590599994,15.2,10.821034484));
#221136=CARTESIAN_POINT('Ctrl Pts',(2.62617590599994,11.6,10.821034484));
#221137=CARTESIAN_POINT('Ctrl Pts',(2.62570431899994,15.2,10.82430224));
#221138=CARTESIAN_POINT('Ctrl Pts',(2.62570431899994,11.6,10.82430224));
#221139=CARTESIAN_POINT('Ctrl Pts',(2.62522941199994,15.2,10.82757456));
#221140=CARTESIAN_POINT('Ctrl Pts',(2.62522941199994,11.6,10.82757456));
#221141=CARTESIAN_POINT('Ctrl Pts',(2.62475118199994,15.2,10.830851435));
#221142=CARTESIAN_POINT('Ctrl Pts',(2.62475118199994,11.6,10.830851435));
#221143=CARTESIAN_POINT('Ctrl Pts',(2.62426961999994,15.2,10.834132855));
#221144=CARTESIAN_POINT('Ctrl Pts',(2.62426961999994,11.6,10.834132855));
#221145=CARTESIAN_POINT('Ctrl Pts',(2.62378472399994,15.2,10.837418812));
#221146=CARTESIAN_POINT('Ctrl Pts',(2.62378472399994,11.6,10.837418812));
#221147=CARTESIAN_POINT('Ctrl Pts',(2.62329648699994,15.2,10.840709296));
#221148=CARTESIAN_POINT('Ctrl Pts',(2.62329648699994,11.6,10.840709296));
#221149=CARTESIAN_POINT('Ctrl Pts',(2.62280490399994,15.2,10.844004298));
#221150=CARTESIAN_POINT('Ctrl Pts',(2.62280490399994,11.6,10.844004298));
#221151=CARTESIAN_POINT('Ctrl Pts',(2.62230996799994,15.2,10.847303809));
#221152=CARTESIAN_POINT('Ctrl Pts',(2.62230996799994,11.6,10.847303809));
#221153=CARTESIAN_POINT('Ctrl Pts',(2.62181167599994,15.2,10.850607819));
#221154=CARTESIAN_POINT('Ctrl Pts',(2.62181167599994,11.6,10.850607819));
#221155=CARTESIAN_POINT('Ctrl Pts',(2.62131002299994,15.2,10.85391632));
#221156=CARTESIAN_POINT('Ctrl Pts',(2.62131002299994,11.6,10.85391632));
#221157=CARTESIAN_POINT('Ctrl Pts',(2.62080500299994,15.2,10.857229301));
#221158=CARTESIAN_POINT('Ctrl Pts',(2.62080500299994,11.6,10.857229301));
#221159=CARTESIAN_POINT('Ctrl Pts',(2.62029660899994,15.2,10.860546755));
#221160=CARTESIAN_POINT('Ctrl Pts',(2.62029660899994,11.6,10.860546755));
#221161=CARTESIAN_POINT('Ctrl Pts',(2.61978483699994,15.2,10.86386867));
#221162=CARTESIAN_POINT('Ctrl Pts',(2.61978483699994,11.6,10.86386867));
#221163=CARTESIAN_POINT('Ctrl Pts',(2.61926968199994,15.2,10.86719504));
#221164=CARTESIAN_POINT('Ctrl Pts',(2.61926968199994,11.6,10.86719504));
#221165=CARTESIAN_POINT('Ctrl Pts',(2.61875113899994,15.2,10.870525854));
#221166=CARTESIAN_POINT('Ctrl Pts',(2.61875113899994,11.6,10.870525854));
#221167=CARTESIAN_POINT('Ctrl Pts',(2.61822920199994,15.2,10.873861104));
#221168=CARTESIAN_POINT('Ctrl Pts',(2.61822920199994,11.6,10.873861104));
#221169=CARTESIAN_POINT('Ctrl Pts',(2.61770386699994,15.2,10.877200779));
#221170=CARTESIAN_POINT('Ctrl Pts',(2.61770386699994,11.6,10.877200779));
#221171=CARTESIAN_POINT('Ctrl Pts',(2.61717512799994,15.2,10.880544872));
#221172=CARTESIAN_POINT('Ctrl Pts',(2.61717512799994,11.6,10.880544872));
#221173=CARTESIAN_POINT('Ctrl Pts',(2.61664297999994,15.2,10.883893373));
#221174=CARTESIAN_POINT('Ctrl Pts',(2.61664297999994,11.6,10.883893373));
#221175=CARTESIAN_POINT('Ctrl Pts',(2.61610741899994,15.2,10.887246272));
#221176=CARTESIAN_POINT('Ctrl Pts',(2.61610741899994,11.6,10.887246272));
#221177=CARTESIAN_POINT('Ctrl Pts',(2.61556843699994,15.2,10.890603562));
#221178=CARTESIAN_POINT('Ctrl Pts',(2.61556843699994,11.6,10.890603562));
#221179=CARTESIAN_POINT('Ctrl Pts',(2.61502603099995,15.2,10.893965232));
#221180=CARTESIAN_POINT('Ctrl Pts',(2.61502603099995,11.6,10.893965232));
#221181=CARTESIAN_POINT('Ctrl Pts',(2.61448019699994,15.2,10.897331274));
#221182=CARTESIAN_POINT('Ctrl Pts',(2.61448019699994,11.6,10.897331274));
#221183=CARTESIAN_POINT('Ctrl Pts',(2.61393092799994,15.2,10.900701679));
#221184=CARTESIAN_POINT('Ctrl Pts',(2.61393092799994,11.6,10.900701679));
#221185=CARTESIAN_POINT('Ctrl Pts',(2.61337821899994,15.2,10.904076437));
#221186=CARTESIAN_POINT('Ctrl Pts',(2.61337821899994,11.6,10.904076437));
#221187=CARTESIAN_POINT('Ctrl Pts',(2.61282206599994,15.2,10.907455542));
#221188=CARTESIAN_POINT('Ctrl Pts',(2.61282206599994,11.6,10.907455542));
#221189=CARTESIAN_POINT('Ctrl Pts',(2.61226246399994,15.2,10.910838981));
#221190=CARTESIAN_POINT('Ctrl Pts',(2.61226246399994,11.6,10.910838981));
#221191=CARTESIAN_POINT('Ctrl Pts',(2.61169940699994,15.2,10.914226746));
#221192=CARTESIAN_POINT('Ctrl Pts',(2.61169940699994,11.6,10.914226746));
#221193=CARTESIAN_POINT('Ctrl Pts',(2.61113289099994,15.2,10.917618831));
#221194=CARTESIAN_POINT('Ctrl Pts',(2.61113289099994,11.6,10.917618831));
#221195=CARTESIAN_POINT('Ctrl Pts',(2.61056290999994,15.2,10.921015224));
#221196=CARTESIAN_POINT('Ctrl Pts',(2.61056290999994,11.6,10.921015224));
#221197=CARTESIAN_POINT('Ctrl Pts',(2.60998946099994,15.2,10.924415916));
#221198=CARTESIAN_POINT('Ctrl Pts',(2.60998946099994,11.6,10.924415916));
#221199=CARTESIAN_POINT('Ctrl Pts',(2.60941253699994,15.2,10.9278209));
#221200=CARTESIAN_POINT('Ctrl Pts',(2.60941253699994,11.6,10.9278209));
#221201=CARTESIAN_POINT('Ctrl Pts',(2.60883213299994,15.2,10.931230167));
#221202=CARTESIAN_POINT('Ctrl Pts',(2.60883213299994,11.6,10.931230167));
#221203=CARTESIAN_POINT('Ctrl Pts',(2.60824824599994,15.2,10.934643706));
#221204=CARTESIAN_POINT('Ctrl Pts',(2.60824824599994,11.6,10.934643706));
#221205=CARTESIAN_POINT('Ctrl Pts',(2.60766086999995,15.2,10.93806151));
#221206=CARTESIAN_POINT('Ctrl Pts',(2.60766086999995,11.6,10.93806151));
#221207=CARTESIAN_POINT('Ctrl Pts',(2.60706999999994,15.2,10.941483569));
#221208=CARTESIAN_POINT('Ctrl Pts',(2.60706999999994,11.6,10.941483569));
#221209=CARTESIAN_POINT('Ctrl Pts',(2.60647563299994,15.2,10.944909876));
#221210=CARTESIAN_POINT('Ctrl Pts',(2.60647563299994,11.6,10.944909876));
#221211=CARTESIAN_POINT('Ctrl Pts',(2.60587776199994,15.2,10.94834042));
#221212=CARTESIAN_POINT('Ctrl Pts',(2.60587776199994,11.6,10.94834042));
#221213=CARTESIAN_POINT('Ctrl Pts',(2.60527638099994,15.2,10.951775193));
#221214=CARTESIAN_POINT('Ctrl Pts',(2.60527638099994,11.6,10.951775193));
#221215=CARTESIAN_POINT('Ctrl Pts',(2.60467148899994,15.2,10.955214187));
#221216=CARTESIAN_POINT('Ctrl Pts',(2.60467148899994,11.6,10.955214187));
#221217=CARTESIAN_POINT('Ctrl Pts',(2.60406307899995,15.2,10.958657392));
#221218=CARTESIAN_POINT('Ctrl Pts',(2.60406307899995,11.6,10.958657392));
#221219=CARTESIAN_POINT('Ctrl Pts',(2.60345114599994,15.2,10.9621048));
#221220=CARTESIAN_POINT('Ctrl Pts',(2.60345114599994,11.6,10.9621048));
#221221=CARTESIAN_POINT('Ctrl Pts',(2.60283568599994,15.2,10.965556401));
#221222=CARTESIAN_POINT('Ctrl Pts',(2.60283568599994,11.6,10.965556401));
#221223=CARTESIAN_POINT('Ctrl Pts',(2.60221669299994,15.2,10.969012187));
#221224=CARTESIAN_POINT('Ctrl Pts',(2.60221669299994,11.6,10.969012187));
#221225=CARTESIAN_POINT('Ctrl Pts',(2.60159416499994,15.2,10.972472151));
#221226=CARTESIAN_POINT('Ctrl Pts',(2.60159416499994,11.6,10.972472151));
#221227=CARTESIAN_POINT('Ctrl Pts',(2.60096809499994,15.2,10.975936282));
#221228=CARTESIAN_POINT('Ctrl Pts',(2.60096809499994,11.6,10.975936282));
#221229=CARTESIAN_POINT('Ctrl Pts',(2.60033847899994,15.2,10.979404571));
#221230=CARTESIAN_POINT('Ctrl Pts',(2.60033847899994,11.6,10.979404571));
#221231=CARTESIAN_POINT('Ctrl Pts',(2.59970531199994,15.2,10.982877011));
#221232=CARTESIAN_POINT('Ctrl Pts',(2.59970531199994,11.6,10.982877011));
#221233=CARTESIAN_POINT('Ctrl Pts',(2.59906858999994,15.2,10.986353591));
#221234=CARTESIAN_POINT('Ctrl Pts',(2.59906858999994,11.6,10.986353591));
#221235=CARTESIAN_POINT('Ctrl Pts',(2.59842830799994,15.2,10.989834306));
#221236=CARTESIAN_POINT('Ctrl Pts',(2.59842830799994,11.6,10.989834306));
#221237=CARTESIAN_POINT('Ctrl Pts',(2.59778446099994,15.2,10.993319144));
#221238=CARTESIAN_POINT('Ctrl Pts',(2.59778446099994,11.6,10.993319144));
#221239=CARTESIAN_POINT('Ctrl Pts',(2.59713704599994,15.2,10.996808097));
#221240=CARTESIAN_POINT('Ctrl Pts',(2.59713704599994,11.6,10.996808097));
#221241=CARTESIAN_POINT('Ctrl Pts',(2.59648605699994,15.2,11.000301157));
#221242=CARTESIAN_POINT('Ctrl Pts',(2.59648605699994,11.6,11.000301157));
#221243=CARTESIAN_POINT('Ctrl Pts',(2.59583148899994,15.2,11.003798316));
#221244=CARTESIAN_POINT('Ctrl Pts',(2.59583148899994,11.6,11.003798316));
#221245=CARTESIAN_POINT('Ctrl Pts',(2.59517333799994,15.2,11.007299564));
#221246=CARTESIAN_POINT('Ctrl Pts',(2.59517333799994,11.6,11.007299564));
#221247=CARTESIAN_POINT('Ctrl Pts',(2.59451159899994,15.2,11.010804893));
#221248=CARTESIAN_POINT('Ctrl Pts',(2.59451159899994,11.6,11.010804893));
#221249=CARTESIAN_POINT('Ctrl Pts',(2.59384626999994,15.2,11.014314294));
#221250=CARTESIAN_POINT('Ctrl Pts',(2.59384626999994,11.6,11.014314294));
#221251=CARTESIAN_POINT('Ctrl Pts',(2.59317734299994,15.2,11.017827759));
#221252=CARTESIAN_POINT('Ctrl Pts',(2.59317734299994,11.6,11.017827759));
#221253=CARTESIAN_POINT('Ctrl Pts',(2.59250481599994,15.2,11.021345279));
#221254=CARTESIAN_POINT('Ctrl Pts',(2.59250481599994,11.6,11.021345279));
#221255=CARTESIAN_POINT('Ctrl Pts',(2.59182868199994,15.2,11.024866846));
#221256=CARTESIAN_POINT('Ctrl Pts',(2.59182868199994,11.6,11.024866846));
#221257=CARTESIAN_POINT('Ctrl Pts',(2.59114893999994,15.2,11.02839245));
#221258=CARTESIAN_POINT('Ctrl Pts',(2.59114893999994,11.6,11.02839245));
#221259=CARTESIAN_POINT('Ctrl Pts',(2.59046558299994,15.2,11.031922084));
#221260=CARTESIAN_POINT('Ctrl Pts',(2.59046558299994,11.6,11.031922084));
#221261=CARTESIAN_POINT('Ctrl Pts',(2.58977860699994,15.2,11.035455739));
#221262=CARTESIAN_POINT('Ctrl Pts',(2.58977860699994,11.6,11.035455739));
#221263=CARTESIAN_POINT('Ctrl Pts',(2.58908800699994,15.2,11.038993406));
#221264=CARTESIAN_POINT('Ctrl Pts',(2.58908800699994,11.6,11.038993406));
#221265=CARTESIAN_POINT('Ctrl Pts',(2.58839378099994,15.2,11.042535078));
#221266=CARTESIAN_POINT('Ctrl Pts',(2.58839378099994,11.6,11.042535078));
#221267=CARTESIAN_POINT('Ctrl Pts',(2.58769592199994,15.2,11.046080744));
#221268=CARTESIAN_POINT('Ctrl Pts',(2.58769592199994,11.6,11.046080744));
#221269=CARTESIAN_POINT('Ctrl Pts',(2.58699442799994,15.2,11.049630398));
#221270=CARTESIAN_POINT('Ctrl Pts',(2.58699442799994,11.6,11.049630398));
#221271=CARTESIAN_POINT('Ctrl Pts',(2.58628929199994,15.2,11.05318403));
#221272=CARTESIAN_POINT('Ctrl Pts',(2.58628929199994,11.6,11.05318403));
#221273=CARTESIAN_POINT('Ctrl Pts',(2.58558051099994,15.2,11.056741632));
#221274=CARTESIAN_POINT('Ctrl Pts',(2.58558051099994,11.6,11.056741632));
#221275=CARTESIAN_POINT('Ctrl Pts',(2.58486808099994,15.2,11.060303195));
#221276=CARTESIAN_POINT('Ctrl Pts',(2.58486808099994,11.6,11.060303195));
#221277=CARTESIAN_POINT('Ctrl Pts',(2.58415199599995,15.2,11.06386871));
#221278=CARTESIAN_POINT('Ctrl Pts',(2.58415199599995,11.6,11.06386871));
#221279=CARTESIAN_POINT('Ctrl Pts',(2.58343225499994,15.2,11.067438172));
#221280=CARTESIAN_POINT('Ctrl Pts',(2.58343225499994,11.6,11.067438172));
#221281=CARTESIAN_POINT('Ctrl Pts',(2.58270885099994,15.2,11.071011569));
#221282=CARTESIAN_POINT('Ctrl Pts',(2.58270885099994,11.6,11.071011569));
#221283=CARTESIAN_POINT('Ctrl Pts',(2.58198177999994,15.2,11.074588894));
#221284=CARTESIAN_POINT('Ctrl Pts',(2.58198177999994,11.6,11.074588894));
#221285=CARTESIAN_POINT('Ctrl Pts',(2.58125103799994,15.2,11.078170138));
#221286=CARTESIAN_POINT('Ctrl Pts',(2.58125103799994,11.6,11.078170138));
#221287=CARTESIAN_POINT('Ctrl Pts',(2.58051662099994,15.2,11.081755293));
#221288=CARTESIAN_POINT('Ctrl Pts',(2.58051662099994,11.6,11.081755293));
#221289=CARTESIAN_POINT('Ctrl Pts',(2.57977852499994,15.2,11.085344351));
#221290=CARTESIAN_POINT('Ctrl Pts',(2.57977852499994,11.6,11.085344351));
#221291=CARTESIAN_POINT('Ctrl Pts',(2.57903674499994,15.2,11.088937303));
#221292=CARTESIAN_POINT('Ctrl Pts',(2.57903674499994,11.6,11.088937303));
#221293=CARTESIAN_POINT('Ctrl Pts',(2.57829127799994,15.2,11.092534141));
#221294=CARTESIAN_POINT('Ctrl Pts',(2.57829127799994,11.6,11.092534141));
#221295=CARTESIAN_POINT('Ctrl Pts',(2.57754211899994,15.2,11.096134856));
#221296=CARTESIAN_POINT('Ctrl Pts',(2.57754211899994,11.6,11.096134856));
#221297=CARTESIAN_POINT('Ctrl Pts',(2.57678926299994,15.2,11.09973944));
#221298=CARTESIAN_POINT('Ctrl Pts',(2.57678926299994,11.6,11.09973944));
#221299=CARTESIAN_POINT('Ctrl Pts',(2.57603270799994,15.2,11.103347886));
#221300=CARTESIAN_POINT('Ctrl Pts',(2.57603270799994,11.6,11.103347886));
#221301=CARTESIAN_POINT('Ctrl Pts',(2.57527244699994,15.2,11.106960183));
#221302=CARTESIAN_POINT('Ctrl Pts',(2.57527244699994,11.6,11.106960183));
#221303=CARTESIAN_POINT('Ctrl Pts',(2.57450847899994,15.2,11.110576325));
#221304=CARTESIAN_POINT('Ctrl Pts',(2.57450847899994,11.6,11.110576325));
#221305=CARTESIAN_POINT('Ctrl Pts',(2.57374079699995,15.2,11.114196302));
#221306=CARTESIAN_POINT('Ctrl Pts',(2.57374079699995,11.6,11.114196302));
#221307=CARTESIAN_POINT('Ctrl Pts',(2.57296939999994,15.2,11.117820108));
#221308=CARTESIAN_POINT('Ctrl Pts',(2.57296939999994,11.6,11.117820108));
#221309=CARTESIAN_POINT('Ctrl Pts',(2.57219427999994,15.2,11.121447733));
#221310=CARTESIAN_POINT('Ctrl Pts',(2.57219427999994,11.6,11.121447733));
#221311=CARTESIAN_POINT('Ctrl Pts',(2.57141543699994,15.2,11.125079169));
#221312=CARTESIAN_POINT('Ctrl Pts',(2.57141543699994,11.6,11.125079169));
#221313=CARTESIAN_POINT('Ctrl Pts',(2.57063286499994,15.2,11.128714409));
#221314=CARTESIAN_POINT('Ctrl Pts',(2.57063286499994,11.6,11.128714409));
#221315=CARTESIAN_POINT('Ctrl Pts',(2.56984655899994,15.2,11.132353445));
#221316=CARTESIAN_POINT('Ctrl Pts',(2.56984655899994,11.6,11.132353445));
#221317=CARTESIAN_POINT('Ctrl Pts',(2.56905651699994,15.2,11.135996265));
#221318=CARTESIAN_POINT('Ctrl Pts',(2.56905651699994,11.6,11.135996265));
#221319=CARTESIAN_POINT('Ctrl Pts',(2.56826273399994,15.2,11.139642864));
#221320=CARTESIAN_POINT('Ctrl Pts',(2.56826273399994,11.6,11.139642864));
#221321=CARTESIAN_POINT('Ctrl Pts',(2.56746520399994,15.2,11.143293232));
#221322=CARTESIAN_POINT('Ctrl Pts',(2.56746520399994,11.6,11.143293232));
#221323=CARTESIAN_POINT('Ctrl Pts',(2.56666392499994,15.2,11.146947362));
#221324=CARTESIAN_POINT('Ctrl Pts',(2.56666392499994,11.6,11.146947362));
#221325=CARTESIAN_POINT('Ctrl Pts',(2.56585889299994,15.2,11.150605243));
#221326=CARTESIAN_POINT('Ctrl Pts',(2.56585889299994,11.6,11.150605243));
#221327=CARTESIAN_POINT('Ctrl Pts',(2.56505010399994,15.2,11.15426687));
#221328=CARTESIAN_POINT('Ctrl Pts',(2.56505010399994,11.6,11.15426687));
#221329=CARTESIAN_POINT('Ctrl Pts',(2.56423755299994,15.2,11.157932235));
#221330=CARTESIAN_POINT('Ctrl Pts',(2.56423755299994,11.6,11.157932235));
#221331=CARTESIAN_POINT('Ctrl Pts',(2.56342123799994,15.2,11.161601329));
#221332=CARTESIAN_POINT('Ctrl Pts',(2.56342123799994,11.6,11.161601329));
#221333=CARTESIAN_POINT('Ctrl Pts',(2.56260115599994,15.2,11.165274147));
#221334=CARTESIAN_POINT('Ctrl Pts',(2.56260115599994,11.6,11.165274147));
#221335=CARTESIAN_POINT('Ctrl Pts',(2.56177730199994,15.2,11.168950679));
#221336=CARTESIAN_POINT('Ctrl Pts',(2.56177730199994,11.6,11.168950679));
#221337=CARTESIAN_POINT('Ctrl Pts',(2.56094967199994,15.2,11.172630919));
#221338=CARTESIAN_POINT('Ctrl Pts',(2.56094967199994,11.6,11.172630919));
#221339=CARTESIAN_POINT('Ctrl Pts',(2.56011826199994,15.2,11.176314857));
#221340=CARTESIAN_POINT('Ctrl Pts',(2.56011826199994,11.6,11.176314857));
#221341=CARTESIAN_POINT('Ctrl Pts',(2.55928306599994,15.2,11.18000248));
#221342=CARTESIAN_POINT('Ctrl Pts',(2.55928306599994,11.6,11.18000248));
#221343=CARTESIAN_POINT('Ctrl Pts',(2.55844408099994,15.2,11.183693782));
#221344=CARTESIAN_POINT('Ctrl Pts',(2.55844408099994,11.6,11.183693782));
#221345=CARTESIAN_POINT('Ctrl Pts',(2.55760130099994,15.2,11.18738875));
#221346=CARTESIAN_POINT('Ctrl Pts',(2.55760130099994,11.6,11.18738875));
#221347=CARTESIAN_POINT('Ctrl Pts',(2.55675472199994,15.2,11.191087377));
#221348=CARTESIAN_POINT('Ctrl Pts',(2.55675472199994,11.6,11.191087377));
#221349=CARTESIAN_POINT('Ctrl Pts',(2.55590434099994,15.2,11.194789655));
#221350=CARTESIAN_POINT('Ctrl Pts',(2.55590434099994,11.6,11.194789655));
#221351=CARTESIAN_POINT('Ctrl Pts',(2.55505015499994,15.2,11.19849558));
#221352=CARTESIAN_POINT('Ctrl Pts',(2.55505015499994,11.6,11.19849558));
#221353=CARTESIAN_POINT('Ctrl Pts',(2.55419216299994,15.2,11.202205147));
#221354=CARTESIAN_POINT('Ctrl Pts',(2.55419216299994,11.6,11.202205147));
#221355=CARTESIAN_POINT('Ctrl Pts',(2.55333036399994,15.2,11.205918353));
#221356=CARTESIAN_POINT('Ctrl Pts',(2.55333036399994,11.6,11.205918353));
#221357=CARTESIAN_POINT('Ctrl Pts',(2.55263787799994,15.2,11.20889183));
#221358=CARTESIAN_POINT('Ctrl Pts',(2.55263787799994,11.6,11.20889183));
#221359=CARTESIAN_POINT('Ctrl Pts',(2.55211680099994,15.2,11.211123574));
#221360=CARTESIAN_POINT('Ctrl Pts',(2.55211680099994,11.6,11.211123574));
#221361=CARTESIAN_POINT('Ctrl Pts',(2.55176865299994,15.2,11.212612132));
#221362=CARTESIAN_POINT('Ctrl Pts',(2.55176865299994,11.6,11.212612132));
#221363=CARTESIAN_POINT('Ctrl Pts',(2.55159438999994,15.2,11.213356593));
#221364=CARTESIAN_POINT('Ctrl Pts',(2.55159438999994,11.6,11.213356593));
#221365=CARTESIAN_POINT('Ctrl Pts',(2.64164356399994,15.2,10.033062558));
#221366=CARTESIAN_POINT('Ctrl Pts',(2.64194831228518,15.2,10.0348230378133));
#221367=CARTESIAN_POINT('Ctrl Pts',(2.64225752130084,15.2,10.0366407499629));
#221368=CARTESIAN_POINT('Ctrl Pts',(2.64257038295734,15.2,10.0385148623113));
#221369=CARTESIAN_POINT('Ctrl Pts',(2.6428847533909,15.2,10.0403980125768));
#221370=CARTESIAN_POINT('Ctrl Pts',(2.64320281580563,15.2,10.0423381044564));
#221371=CARTESIAN_POINT('Ctrl Pts',(2.643523781256,15.2,10.0443343067515));
#221372=CARTESIAN_POINT('Ctrl Pts',(2.6438447466772,15.2,10.0463305088653));
#221373=CARTESIAN_POINT('Ctrl Pts',(2.64416861599511,15.2,10.0483828189931));
#221374=CARTESIAN_POINT('Ctrl Pts',(2.64449462848328,15.2,10.0504904282499));
#221375=CARTESIAN_POINT('Ctrl Pts',(2.64482064097144,15.2,10.0525980375067));
#221376=CARTESIAN_POINT('Ctrl Pts',(2.64514879426365,15.2,10.0547609455835));
#221377=CARTESIAN_POINT('Ctrl Pts',(2.64547835293473,15.2,10.0569783630272));
#221378=CARTESIAN_POINT('Ctrl Pts',(2.64580791163574,15.2,10.0591957806723));
#221379=CARTESIAN_POINT('Ctrl Pts',(2.6461388765513,15.2,10.0614677065646));
#221380=CARTESIAN_POINT('Ctrl Pts',(2.64647052756943,15.2,10.0637933712784));
#221381=CARTESIAN_POINT('Ctrl Pts',(2.64680217855742,15.2,10.0661190357809));
#221382=CARTESIAN_POINT('Ctrl Pts',(2.64713452030233,15.2,10.0684984401115));
#221383=CARTESIAN_POINT('Ctrl Pts',(2.64746685620843,15.2,10.0709308325343));
#221384=CARTESIAN_POINT('Ctrl Pts',(2.64779919211453,15.2,10.0733632249571));
#221385=CARTESIAN_POINT('Ctrl Pts',(2.64813152497723,15.2,10.0758486039396));
#221386=CARTESIAN_POINT('Ctrl Pts',(2.6484631779652,15.2,10.0783862403452));
#221387=CARTESIAN_POINT('Ctrl Pts',(2.6487948309833,15.2,10.0809238769812));
#221388=CARTESIAN_POINT('Ctrl Pts',(2.64912580691801,15.2,10.0835137669737));
#221389=CARTESIAN_POINT('Ctrl Pts',(2.64945545276921,15.2,10.0861551977878));
#221390=CARTESIAN_POINT('Ctrl Pts',(2.64978509859048,15.2,10.088796628362));
#221391=CARTESIAN_POINT('Ctrl Pts',(2.65011341197134,15.2,10.0914895979888));
#221392=CARTESIAN_POINT('Ctrl Pts',(2.65043976104272,15.2,10.0942334086413));
#221393=CARTESIAN_POINT('Ctrl Pts',(2.65076611011411,15.2,10.0969772192938));
#221394=CARTESIAN_POINT('Ctrl Pts',(2.65109049311065,15.2,10.0997718698089));
#221395=CARTESIAN_POINT('Ctrl Pts',(2.65141229526573,15.2,10.1026166776201));
#221396=CARTESIAN_POINT('Ctrl Pts',(2.65173409742082,15.2,10.1054614854312));
#221397=CARTESIAN_POINT('Ctrl Pts',(2.65205331709344,15.2,10.108356448356));
#221398=CARTESIAN_POINT('Ctrl Pts',(2.65236935724883,15.2,10.1113009019123));
#221399=CARTESIAN_POINT('Ctrl Pts',(2.65268539743294,15.2,10.1142453557361));
#221400=CARTESIAN_POINT('Ctrl Pts',(2.65299825586676,15.2,10.1172392954563));
#221401=CARTESIAN_POINT('Ctrl Pts',(2.65330735305012,15.2,10.1202820707076));
#221402=CARTESIAN_POINT('Ctrl Pts',(2.65366796638857,15.2,10.1238319747529));
#221403=CARTESIAN_POINT('Ctrl Pts',(2.65402345683872,15.2,10.1274483456391));
#221404=CARTESIAN_POINT('Ctrl Pts',(2.65437292773397,15.2,10.1311301704059));
#221405=CARTESIAN_POINT('Ctrl Pts',(2.65472239865642,15.2,10.1348119954594));
#221406=CARTESIAN_POINT('Ctrl Pts',(2.65506585037871,15.2,10.1385592719262));
#221407=CARTESIAN_POINT('Ctrl Pts',(2.65540241446754,15.2,10.1423710100804));
#221408=CARTESIAN_POINT('Ctrl Pts',(2.65569089798348,15.2,10.1456382143397));
#221409=CARTESIAN_POINT('Ctrl Pts',(2.65597432136547,15.2,10.1489527781383));
#221410=CARTESIAN_POINT('Ctrl Pts',(2.6562521530469,15.2,10.1523140905746));
#221411=CARTESIAN_POINT('Ctrl Pts',(2.6565299847031,15.2,10.1556754027057));
#221412=CARTESIAN_POINT('Ctrl Pts',(2.65680222509103,15.2,10.1590834656702));
#221413=CARTESIAN_POINT('Ctrl Pts',(2.65706835574777,15.2,10.1625376759633));
#221414=CARTESIAN_POINT('Ctrl Pts',(2.6573344864045,15.2,10.1659918862565));
#221415=CARTESIAN_POINT('Ctrl Pts',(2.65759450897003,15.2,10.1694922499377));
#221416=CARTESIAN_POINT('Ctrl Pts',(2.65784791771112,15.2,10.1730381733068));
#221417=CARTESIAN_POINT('Ctrl Pts',(2.6581013264522,15.2,10.176584096676));
#221418=CARTESIAN_POINT('Ctrl Pts',(2.65834812371539,15.2,10.1801755849054));
#221419=CARTESIAN_POINT('Ctrl Pts',(2.65858781554049,15.2,10.1838120581035));
#221420=CARTESIAN_POINT('Ctrl Pts',(2.65886745601764,15.2,10.1880546103882));
#221421=CARTESIAN_POINT('Ctrl Pts',(2.65913742923337,15.2,10.1923583939805));
#221422=CARTESIAN_POINT('Ctrl Pts',(2.6593969717378,15.2,10.1967225107962));
#221423=CARTESIAN_POINT('Ctrl Pts',(2.65961943673005,15.2,10.2004631821584));
#221424=CARTESIAN_POINT('Ctrl Pts',(2.65983424360939,15.2,10.2042481817746));
#221425=CARTESIAN_POINT('Ctrl Pts',(2.66004092268576,15.2,10.2080769531326));
#221426=CARTESIAN_POINT('Ctrl Pts',(2.66024760178091,15.2,10.2119057248383));
#221427=CARTESIAN_POINT('Ctrl Pts',(2.66044615646696,15.2,10.2157782705315));
#221428=CARTESIAN_POINT('Ctrl Pts',(2.66063613331028,15.2,10.2196940442468));
#221429=CARTESIAN_POINT('Ctrl Pts',(2.66085777293492,15.2,10.2242624463811));
#221430=CARTESIAN_POINT('Ctrl Pts',(2.66106773549864,15.2,10.2288896875629));
#221431=CARTESIAN_POINT('Ctrl Pts',(2.66126532322316,15.2,10.2335749195872));
#221432=CARTESIAN_POINT('Ctrl Pts',(2.6614064573209,15.2,10.2369215140987));
#221433=CARTESIAN_POINT('Ctrl Pts',(2.66154127587154,15.2,10.2402976954625));
#221434=CARTESIAN_POINT('Ctrl Pts',(2.66166953323318,15.2,10.2437031601128));
#221435=CARTESIAN_POINT('Ctrl Pts',(2.66182344207555,15.2,10.247789717916));
#221436=CARTESIAN_POINT('Ctrl Pts',(2.66196789944114,15.2,10.2519184437987));
#221437=CARTESIAN_POINT('Ctrl Pts',(2.66210248553796,15.2,10.2560888199035));
#221438=CARTESIAN_POINT('Ctrl Pts',(2.66221464061253,15.2,10.2595641331347));
#221439=CARTESIAN_POINT('Ctrl Pts',(2.66231994071894,15.2,10.2630683710375));
#221440=CARTESIAN_POINT('Ctrl Pts',(2.66241814828781,15.2,10.2666012374287));
#221441=CARTESIAN_POINT('Ctrl Pts',(2.66251635585667,15.2,10.2701341038199));
#221442=CARTESIAN_POINT('Ctrl Pts',(2.66260747005041,15.2,10.2736955992783));
#221443=CARTESIAN_POINT('Ctrl Pts',(2.66269125928592,15.2,10.2772854331695));
#221444=CARTESIAN_POINT('Ctrl Pts',(2.6627750485123,15.2,10.2808752666694));
#221445=CARTESIAN_POINT('Ctrl Pts',(2.66285151010895,15.2,10.2844934378839));
#221446=CARTESIAN_POINT('Ctrl Pts',(2.66292041774095,15.2,10.2881396605397));
#221447=CARTESIAN_POINT('Ctrl Pts',(2.66298932538046,15.2,10.2917858835929));
#221448=CARTESIAN_POINT('Ctrl Pts',(2.66305067884788,15.2,10.2954601580569));
#221449=CARTESIAN_POINT('Ctrl Pts',(2.66310425245962,15.2,10.299162198749));
#221450=CARTESIAN_POINT('Ctrl Pts',(2.66315782607137,15.2,10.3028642394412));
#221451=CARTESIAN_POINT('Ctrl Pts',(2.6632036207431,15.2,10.306594048467));
#221452=CARTESIAN_POINT('Ctrl Pts',(2.66324141678721,15.2,10.3103513458055));
#221453=CARTESIAN_POINT('Ctrl Pts',(2.66328677204262,15.2,10.3148601028575));
#221454=CARTESIAN_POINT('Ctrl Pts',(2.6633206093103,15.2,10.3194084393473));
#221455=CARTESIAN_POINT('Ctrl Pts',(2.66334255472735,15.2,10.3239958814333));
#221456=CARTESIAN_POINT('Ctrl Pts',(2.6633608425739,15.2,10.32781874963));
#221457=CARTESIAN_POINT('Ctrl Pts',(2.66337087430086,15.2,10.3316687752493));
#221458=CARTESIAN_POINT('Ctrl Pts',(2.66337243721683,15.2,10.3355456835154));
#221459=CARTESIAN_POINT('Ctrl Pts',(2.66337400013264,15.2,10.3394225913589));
#221460=CARTESIAN_POINT('Ctrl Pts',(2.66336709569959,15.2,10.3433263851719));
#221461=CARTESIAN_POINT('Ctrl Pts',(2.66335151674367,15.2,10.3472567914775));
#221462=CARTESIAN_POINT('Ctrl Pts',(2.66333593778604,15.2,10.3511871982115));
#221463=CARTESIAN_POINT('Ctrl Pts',(2.66331168425913,15.2,10.3551442209366));
#221464=CARTESIAN_POINT('Ctrl Pts',(2.6632785537043,15.2,10.3591275924622));
#221465=CARTESIAN_POINT('Ctrl Pts',(2.66323879703633,15.2,10.3639076385535));
#221466=CARTESIAN_POINT('Ctrl Pts',(2.66318625590048,15.2,10.3687256263734));
#221467=CARTESIAN_POINT('Ctrl Pts',(2.66312058922967,15.2,10.373581102723));
#221468=CARTESIAN_POINT('Ctrl Pts',(2.66305492256482,15.2,10.3784365786316));
#221469=CARTESIAN_POINT('Ctrl Pts',(2.66297612703871,15.2,10.3833295449462));
#221470=CARTESIAN_POINT('Ctrl Pts',(2.66288387145834,15.2,10.388259551706));
#221471=CARTESIAN_POINT('Ctrl Pts',(2.66279161587797,15.2,10.3931895584659));
#221472=CARTESIAN_POINT('Ctrl Pts',(2.66268589722438,15.2,10.3981566070889));
#221473=CARTESIAN_POINT('Ctrl Pts',(2.66256638872966,15.2,10.4031602549045));
#221474=CARTESIAN_POINT('Ctrl Pts',(2.66248671639261,15.2,10.406496020418));
#221475=CARTESIAN_POINT('Ctrl Pts',(2.66240091517758,15.2,10.4098480544589));
#221476=CARTESIAN_POINT('Ctrl Pts',(2.6623088889499,15.2,10.4132162247689));
#221477=CARTESIAN_POINT('Ctrl Pts',(2.66214784305774,15.2,10.4191105225819));
#221478=CARTESIAN_POINT('Ctrl Pts',(2.66196773798001,15.2,10.4250542421692));
#221479=CARTESIAN_POINT('Ctrl Pts',(2.66176806598964,15.2,10.4310466983348));
#221480=CARTESIAN_POINT('Ctrl Pts',(2.66159691857822,15.2,10.4361830890673));
#221481=CARTESIAN_POINT('Ctrl Pts',(2.66141139836021,15.2,10.4413552861094));
#221482=CARTESIAN_POINT('Ctrl Pts',(2.66121119703321,15.2,10.4465628640273));
#221483=CARTESIAN_POINT('Ctrl Pts',(2.66101099570621,15.2,10.4517704419452));
#221484=CARTESIAN_POINT('Ctrl Pts',(2.6607961129201,15.2,10.4570134019889));
#221485=CARTESIAN_POINT('Ctrl Pts',(2.66056624676244,15.2,10.4622913237957));
#221486=CARTESIAN_POINT('Ctrl Pts',(2.66037469162409,15.2,10.4666895921279));
#221487=CARTESIAN_POINT('Ctrl Pts',(2.66017273257437,15.2,10.4711121390049));
#221488=CARTESIAN_POINT('Ctrl Pts',(2.65996019729714,15.2,10.4755587249759));
#221489=CARTESIAN_POINT('Ctrl Pts',(2.6597901690661,15.2,10.4791159939466));
#221490=CARTESIAN_POINT('Ctrl Pts',(2.65961337264584,15.2,10.4826886483612));
#221491=CARTESIAN_POINT('Ctrl Pts',(2.65942972168162,15.2,10.4862765660707));
#221492=CARTESIAN_POINT('Ctrl Pts',(2.65920015798885,15.2,10.490761462963));
#221493=CARTESIAN_POINT('Ctrl Pts',(2.65895988345134,15.2,10.4952702080909));
#221494=CARTESIAN_POINT('Ctrl Pts',(2.65870873324212,15.2,10.4998025658011));
#221495=CARTESIAN_POINT('Ctrl Pts',(2.65850781309116,15.2,10.5034284516729));
#221496=CARTESIAN_POINT('Ctrl Pts',(2.658299932405,15.2,10.5070694505177));
#221497=CARTESIAN_POINT('Ctrl Pts',(2.65808500753414,15.2,10.5107254422179));
#221498=CARTESIAN_POINT('Ctrl Pts',(2.65787008263399,15.2,10.5143814344162));
#221499=CARTESIAN_POINT('Ctrl Pts',(2.65764811326068,15.2,10.518052418918));
#221500=CARTESIAN_POINT('Ctrl Pts',(2.65741901895836,15.2,10.5217382780265));
#221501=CARTESIAN_POINT('Ctrl Pts',(2.65713265109606,15.2,10.5263456016611));
#221502=CARTESIAN_POINT('Ctrl Pts',(2.6568351471105,15.2,10.5309761659123));
#221503=CARTESIAN_POINT('Ctrl Pts',(2.65652635023458,15.2,10.5356297403586));
#221504=CARTESIAN_POINT('Ctrl Pts',(2.65627931275404,15.2,10.5393525996113));
#221505=CARTESIAN_POINT('Ctrl Pts',(2.65602504882998,15.2,10.543090187476));
#221506=CARTESIAN_POINT('Ctrl Pts',(2.65576347679629,15.2,10.5468423846683));
#221507=CARTESIAN_POINT('Ctrl Pts',(2.65550190472695,15.2,10.5505945823719));
#221508=CARTESIAN_POINT('Ctrl Pts',(2.6552330259449,15.2,10.5543613914746));
#221509=CARTESIAN_POINT('Ctrl Pts',(2.65495676169318,15.2,10.5581426953154));
#221510=CARTESIAN_POINT('Ctrl Pts',(2.65468049747909,15.2,10.5619239986409));
#221511=CARTESIAN_POINT('Ctrl Pts',(2.65439684769386,15.2,10.5657197956204));
#221512=CARTESIAN_POINT('Ctrl Pts',(2.6541057342737,15.2,10.5695299733636));
#221513=CARTESIAN_POINT('Ctrl Pts',(2.65374184246875,15.2,10.5742926959319));
#221514=CARTESIAN_POINT('Ctrl Pts',(2.65336628922462,15.2,10.5790778877979));
#221515=CARTESIAN_POINT('Ctrl Pts',(2.6529789265169,15.2,10.5838853254357));
#221516=CARTESIAN_POINT('Ctrl Pts',(2.65266903633384,15.2,10.5877312757555));
#221517=CARTESIAN_POINT('Ctrl Pts',(2.6523515868096,15.2,10.5915914632257));
#221518=CARTESIAN_POINT('Ctrl Pts',(2.65202650521943,15.2,10.5954657770205));
#221519=CARTESIAN_POINT('Ctrl Pts',(2.65162015325385,15.2,10.6003086690001));
#221520=CARTESIAN_POINT('Ctrl Pts',(2.65120187296133,15.2,10.6051736287818));
#221521=CARTESIAN_POINT('Ctrl Pts',(2.65077152046035,15.2,10.6100604414225));
#221522=CARTESIAN_POINT('Ctrl Pts',(2.6504272384877,15.2,10.6139698912154));
#221523=CARTESIAN_POINT('Ctrl Pts',(2.65007523109384,15.2,10.6178933252482));
#221524=CARTESIAN_POINT('Ctrl Pts',(2.64971542501265,15.2,10.6218306332032));
#221525=CARTESIAN_POINT('Ctrl Pts',(2.64935561888244,15.2,10.6257679416947));
#221526=CARTESIAN_POINT('Ctrl Pts',(2.64898801433535,15.2,10.6297191243156));
#221527=CARTESIAN_POINT('Ctrl Pts',(2.64861253896211,15.2,10.633684070842));
#221528=CARTESIAN_POINT('Ctrl Pts',(2.64823706364004,15.2,10.6376490168282));
#221529=CARTESIAN_POINT('Ctrl Pts',(2.64785371767437,15.2,10.6416277260649));
#221530=CARTESIAN_POINT('Ctrl Pts',(2.64746243154022,15.2,10.645620088682));
#221531=CARTESIAN_POINT('Ctrl Pts',(2.64707114535275,15.2,10.6496124518431));
#221532=CARTESIAN_POINT('Ctrl Pts',(2.64667191698377,15.2,10.6536184700392));
#221533=CARTESIAN_POINT('Ctrl Pts',(2.64626467818327,15.2,10.657638032537));
#221534=CARTESIAN_POINT('Ctrl Pts',(2.64585743943827,15.2,10.6616575944871));
#221535=CARTESIAN_POINT('Ctrl Pts',(2.64544219046987,15.2,10.6656907023566));
#221536=CARTESIAN_POINT('Ctrl Pts',(2.64501886056085,15.2,10.66973724808));
#221537=CARTESIAN_POINT('Ctrl Pts',(2.64448969813133,15.2,10.6747954306477));
#221538=CARTESIAN_POINT('Ctrl Pts',(2.64394791169668,15.2,10.6798746070213));
#221539=CARTESIAN_POINT('Ctrl Pts',(2.64339336757264,15.2,10.6849745716497));
#221540=CARTESIAN_POINT('Ctrl Pts',(2.64294973224923,15.2,10.6890545435747));
#221541=CARTESIAN_POINT('Ctrl Pts',(2.64249793301568,15.2,10.6931478192444));
#221542=CARTESIAN_POINT('Ctrl Pts',(2.64203790221229,15.2,10.6972542911358));
#221543=CARTESIAN_POINT('Ctrl Pts',(2.64157787147158,15.2,10.7013607624676));
#221544=CARTESIAN_POINT('Ctrl Pts',(2.6411096091603,15.2,10.7054804315912));
#221545=CARTESIAN_POINT('Ctrl Pts',(2.64063304931123,15.2,10.7096131921409));
#221546=CARTESIAN_POINT('Ctrl Pts',(2.63979906949417,15.2,10.7168455238067));
#221547=CARTESIAN_POINT('Ctrl Pts',(2.63893968046807,15.2,10.7241179469112));
#221548=CARTESIAN_POINT('Ctrl Pts',(2.63805453395032,15.2,10.7314299024471));
#221549=CARTESIAN_POINT('Ctrl Pts',(2.63716938743256,15.2,10.738741857983));
#221550=CARTESIAN_POINT('Ctrl Pts',(2.63625848327169,15.2,10.7460933444843));
#221551=CARTESIAN_POINT('Ctrl Pts',(2.63532148542279,15.2,10.753483808587));
#221552=CARTESIAN_POINT('Ctrl Pts',(2.63438448764684,15.2,10.7608742721142));
#221553=CARTESIAN_POINT('Ctrl Pts',(2.63342139251814,15.2,10.7683037132141));
#221554=CARTESIAN_POINT('Ctrl Pts',(2.63243187365076,15.2,10.7757715838022));
#221555=CARTESIAN_POINT('Ctrl Pts',(2.63144235470634,15.2,10.7832394549718));
#221556=CARTESIAN_POINT('Ctrl Pts',(2.63042640924717,15.2,10.7907457548816));
#221557=CARTESIAN_POINT('Ctrl Pts',(2.62938371606527,15.2,10.7982899414143));
#221558=CARTESIAN_POINT('Ctrl Pts',(2.6284899790986,15.2,10.8047563866781));
#221559=CARTESIAN_POINT('Ctrl Pts',(2.62757658992477,15.2,10.8112506694695));
#221560=CARTESIAN_POINT('Ctrl Pts',(2.6266433518767,15.2,10.8177724478141));
#221561=CARTESIAN_POINT('Ctrl Pts',(2.62571011374384,15.2,10.824294226751));
#221562=CARTESIAN_POINT('Ctrl Pts',(2.62475702276745,15.2,10.8308435043405));
#221563=CARTESIAN_POINT('Ctrl Pts',(2.62378388871353,15.2,10.8374199441168));
#221564=CARTESIAN_POINT('Ctrl Pts',(2.62313513276597,15.2,10.8418042367037));
#221565=CARTESIAN_POINT('Ctrl Pts',(2.62247746642747,15.2,10.8462006016154));
#221566=CARTESIAN_POINT('Ctrl Pts',(2.62181083583833,15.2,10.8506089410853));
#221567=CARTESIAN_POINT('Ctrl Pts',(2.62131086287377,15.2,10.8539151958379));
#221568=CARTESIAN_POINT('Ctrl Pts',(2.62080584795862,15.2,10.8572281859478));
#221569=CARTESIAN_POINT('Ctrl Pts',(2.62029576460284,15.2,10.8605478695762));
#221570=CARTESIAN_POINT('Ctrl Pts',(2.6197856811544,15.2,10.8638675538078));
#221571=CARTESIAN_POINT('Ctrl Pts',(2.6192705308962,15.2,10.8671939320079));
#221572=CARTESIAN_POINT('Ctrl Pts',(2.61875029040323,15.2,10.8705269637016));
#221573=CARTESIAN_POINT('Ctrl Pts',(2.61788322304095,15.2,10.876082015717));
#221574=CARTESIAN_POINT('Ctrl Pts',(2.61700201693956,15.2,10.8816555475299));
#221575=CARTESIAN_POINT('Ctrl Pts',(2.61610656367452,15.2,10.887247370448));
#221576=CARTESIAN_POINT('Ctrl Pts',(2.61556929173501,15.2,10.890602464077));
#221577=CARTESIAN_POINT('Ctrl Pts',(2.61502689016871,15.2,10.8939641426383));
#221578=CARTESIAN_POINT('Ctrl Pts',(2.61447933816066,15.2,10.8973323653933));
#221579=CARTESIAN_POINT('Ctrl Pts',(2.6139317861526,15.2,10.9007005881484));
#221580=CARTESIAN_POINT('Ctrl Pts',(2.61337908161927,15.2,10.9040753549076));
#221581=CARTESIAN_POINT('Ctrl Pts',(2.61282120368075,15.2,10.9074566259103));
#221582=CARTESIAN_POINT('Ctrl Pts',(2.61226332574224,15.2,10.910837896913));
#221583=CARTESIAN_POINT('Ctrl Pts',(2.61170027362933,15.2,10.9142256700233));
#221584=CARTESIAN_POINT('Ctrl Pts',(2.61113202477498,15.2,10.9176199080249));
#221585=CARTESIAN_POINT('Ctrl Pts',(2.61037435956703,15.2,10.9221455591049));
#221586=CARTESIAN_POINT('Ctrl Pts',(2.60960745664132,15.2,10.9266826991946));
#221587=CARTESIAN_POINT('Ctrl Pts',(2.60883126209807,15.2,10.931231235777));
#221588=CARTESIAN_POINT('Ctrl Pts',(2.6082491162435,15.2,10.9346426379039));
#221589=CARTESIAN_POINT('Ctrl Pts',(2.60766174452729,15.2,10.9380604493318));
#221590=CARTESIAN_POINT('Ctrl Pts',(2.60706912560194,15.2,10.9414846316292));
#221591=CARTESIAN_POINT('Ctrl Pts',(2.60647650667659,15.2,10.9449088139266));
#221592=CARTESIAN_POINT('Ctrl Pts',(2.60587863994603,15.2,10.9483393659823));
#221593=CARTESIAN_POINT('Ctrl Pts',(2.60527550313415,15.2,10.951776248608));
#221594=CARTESIAN_POINT('Ctrl Pts',(2.60447132075484,15.2,10.9563587585675));
#221595=CARTESIAN_POINT('Ctrl Pts',(2.60365777196074,15.2,10.9609525230496));
#221596=CARTESIAN_POINT('Ctrl Pts',(2.60283480291787,15.2,10.9655574465054));
#221597=CARTESIAN_POINT('Ctrl Pts',(2.60221757599555,15.2,10.9690111398815));
#221598=CARTESIAN_POINT('Ctrl Pts',(2.60159505182174,15.2,10.9724711124344));
#221599=CARTESIAN_POINT('Ctrl Pts',(2.60096720835477,15.2,10.9759373222722));
#221600=CARTESIAN_POINT('Ctrl Pts',(2.60033936500187,15.2,10.9794035314804));
#221601=CARTESIAN_POINT('Ctrl Pts',(2.59970620230238,15.2,10.9828759785249));
#221602=CARTESIAN_POINT('Ctrl Pts',(2.59906769987639,15.2,10.9863546253647));
#221603=CARTESIAN_POINT('Ctrl Pts',(2.5984291974504,15.2,10.9898332722045));
#221604=CARTESIAN_POINT('Ctrl Pts',(2.59778535487268,15.2,10.9933181184235));
#221605=CARTESIAN_POINT('Ctrl Pts',(2.59713615243746,15.2,10.9968091241306));
#221606=CARTESIAN_POINT('Ctrl Pts',(2.59627054922982,15.2,11.0014637981952));
#221607=CARTESIAN_POINT('Ctrl Pts',(2.59539541407688,15.2,11.0061294249049));
#221608=CARTESIAN_POINT('Ctrl Pts',(2.59451070159463,15.2,11.0108059102437));
#221609=CARTESIAN_POINT('Ctrl Pts',(2.59362598899183,15.2,11.0154823962197));
#221610=CARTESIAN_POINT('Ctrl Pts',(2.59273169777704,15.2,11.0201697419633));
#221611=CARTESIAN_POINT('Ctrl Pts',(2.59182777994998,15.2,11.024867855275));
#221612=CARTESIAN_POINT('Ctrl Pts',(2.59114984164126,15.2,11.0283914399387));
#221613=CARTESIAN_POINT('Ctrl Pts',(2.59046648936613,15.2,11.031921081427));
#221614=CARTESIAN_POINT('Ctrl Pts',(2.58977770109997,15.2,11.0354567416313));
#221615=CARTESIAN_POINT('Ctrl Pts',(2.58885931666166,15.2,11.0401709556653));
#221616=CARTESIAN_POINT('Ctrl Pts',(2.58793127138487,15.2,11.0448958697083));
#221617=CARTESIAN_POINT('Ctrl Pts',(2.58699351739719,15.2,11.0496313932038));
#221618=CARTESIAN_POINT('Ctrl Pts',(2.58629020197032,15.2,11.0531830355029));
#221619=CARTESIAN_POINT('Ctrl Pts',(2.5855814249799,15.2,11.0567406451341));
#221620=CARTESIAN_POINT('Ctrl Pts',(2.5848671672137,15.2,11.0603041834218));
#221621=CARTESIAN_POINT('Ctrl Pts',(2.58415290944751,15.2,11.0638677217095));
#221622=CARTESIAN_POINT('Ctrl Pts',(2.58343317205698,15.2,11.0674371907798));
#221623=CARTESIAN_POINT('Ctrl Pts',(2.58270793424998,15.2,11.0710125509833));
#221624=CARTESIAN_POINT('Ctrl Pts',(2.58198269644299,15.2,11.0745879111868));
#221625=CARTESIAN_POINT('Ctrl Pts',(2.58125195816958,15.2,11.0781691626899));
#221626=CARTESIAN_POINT('Ctrl Pts',(2.58051570132181,15.2,11.0817562683507));
#221627=CARTESIAN_POINT('Ctrl Pts',(2.57977944447404,15.2,11.0853433740115));
#221628=CARTESIAN_POINT('Ctrl Pts',(2.57903766857072,15.2,11.088936333722));
#221629=CARTESIAN_POINT('Ctrl Pts',(2.57829035514452,15.2,11.0925351095621));
#221630=CARTESIAN_POINT('Ctrl Pts',(2.5772939371524,15.2,11.0973334777846));
#221631=CARTESIAN_POINT('Ctrl Pts',(2.57628767328396,15.2,11.1021421859029));
#221632=CARTESIAN_POINT('Ctrl Pts',(2.57527152011682,15.2,11.1069611446107));
#221633=CARTESIAN_POINT('Ctrl Pts',(2.57450940531068,15.2,11.1105753633132));
#221634=CARTESIAN_POINT('Ctrl Pts',(2.57374172812189,15.2,11.1141953481483));
#221635=CARTESIAN_POINT('Ctrl Pts',(2.57296846931665,15.2,11.1178210627666));
#221636=CARTESIAN_POINT('Ctrl Pts',(2.57167970459443,15.2,11.1238639206833));
#221637=CARTESIAN_POINT('Ctrl Pts',(2.57037543667752,15.2,11.1299226948923));
#221638=CARTESIAN_POINT('Ctrl Pts',(2.56905558174093,15.2,11.1359972097116));
#221639=CARTESIAN_POINT('Ctrl Pts',(2.56826366880775,15.2,11.1396419184707));
#221640=CARTESIAN_POINT('Ctrl Pts',(2.56746614255848,15.2,11.1432922950796));
#221641=CARTESIAN_POINT('Ctrl Pts',(2.56666298675071,15.2,11.1469482997966));
#221642=CARTESIAN_POINT('Ctrl Pts',(2.56585983094294,15.2,11.1506043045137));
#221643=CARTESIAN_POINT('Ctrl Pts',(2.56505104525857,15.2,11.1542659381007));
#221644=CARTESIAN_POINT('Ctrl Pts',(2.56423661208033,15.2,11.1579331668836));
#221645=CARTESIAN_POINT('Ctrl Pts',(2.56315070107737,15.2,11.162822805705));
#221646=CARTESIAN_POINT('Ctrl Pts',(2.56205475417597,15.2,11.1677223928859));
#221647=CARTESIAN_POINT('Ctrl Pts',(2.56094872689281,15.2,11.1726318438764));
#221648=CARTESIAN_POINT('Ctrl Pts',(2.56011920650578,15.2,11.1763139317848));
#221649=CARTESIAN_POINT('Ctrl Pts',(2.55928401515584,15.2,11.180001564504));
#221650=CARTESIAN_POINT('Ctrl Pts',(2.55844313226588,15.2,11.1836946985533));
#221651=CARTESIAN_POINT('Ctrl Pts',(2.55760224937592,15.2,11.1873878326026));
#221652=CARTESIAN_POINT('Ctrl Pts',(2.55675567340697,15.2,11.1910864657311));
#221653=CARTESIAN_POINT('Ctrl Pts',(2.55590338976742,15.2,11.1947905667382));
#221654=CARTESIAN_POINT('Ctrl Pts',(2.55448291698325,15.2,11.2009640686412));
#221655=CARTESIAN_POINT('Ctrl Pts',(2.55304658198318,15.2,11.2071527499809));
#221656=CARTESIAN_POINT('Ctrl Pts',(2.55159438999994,15.2,11.213356593));
#221657=CARTESIAN_POINT('Ctrl Pts',(2.64164356399994,12.2,10.033062558));
#221658=CARTESIAN_POINT('Ctrl Pts',(2.64194831228518,12.2,10.0348230378133));
#221659=CARTESIAN_POINT('Ctrl Pts',(2.64225752130084,12.2,10.0366407499629));
#221660=CARTESIAN_POINT('Ctrl Pts',(2.64257038295734,12.2,10.0385148623113));
#221661=CARTESIAN_POINT('Ctrl Pts',(2.6428847533909,12.2,10.0403980125768));
#221662=CARTESIAN_POINT('Ctrl Pts',(2.64320281580563,12.2,10.0423381044564));
#221663=CARTESIAN_POINT('Ctrl Pts',(2.643523781256,12.2,10.0443343067515));
#221664=CARTESIAN_POINT('Ctrl Pts',(2.6438447466772,12.2,10.0463305088653));
#221665=CARTESIAN_POINT('Ctrl Pts',(2.64416861599511,12.2,10.0483828189931));
#221666=CARTESIAN_POINT('Ctrl Pts',(2.64449462848328,12.2,10.0504904282499));
#221667=CARTESIAN_POINT('Ctrl Pts',(2.64482064097144,12.2,10.0525980375067));
#221668=CARTESIAN_POINT('Ctrl Pts',(2.64514879426365,12.2,10.0547609455835));
#221669=CARTESIAN_POINT('Ctrl Pts',(2.64547835293473,12.2,10.0569783630272));
#221670=CARTESIAN_POINT('Ctrl Pts',(2.64580791163574,12.2,10.0591957806723));
#221671=CARTESIAN_POINT('Ctrl Pts',(2.6461388765513,12.2,10.0614677065646));
#221672=CARTESIAN_POINT('Ctrl Pts',(2.64647052756943,12.2,10.0637933712784));
#221673=CARTESIAN_POINT('Ctrl Pts',(2.64680217855742,12.2,10.0661190357809));
#221674=CARTESIAN_POINT('Ctrl Pts',(2.64713452030233,12.2,10.0684984401115));
#221675=CARTESIAN_POINT('Ctrl Pts',(2.64746685620843,12.2,10.0709308325343));
#221676=CARTESIAN_POINT('Ctrl Pts',(2.64779919211453,12.2,10.0733632249571));
#221677=CARTESIAN_POINT('Ctrl Pts',(2.64813152497723,12.2,10.0758486039396));
#221678=CARTESIAN_POINT('Ctrl Pts',(2.6484631779652,12.2,10.0783862403452));
#221679=CARTESIAN_POINT('Ctrl Pts',(2.6487948309833,12.2,10.0809238769812));
#221680=CARTESIAN_POINT('Ctrl Pts',(2.64912580691801,12.2,10.0835137669737));
#221681=CARTESIAN_POINT('Ctrl Pts',(2.64945545276921,12.2,10.0861551977878));
#221682=CARTESIAN_POINT('Ctrl Pts',(2.64978509859048,12.2,10.088796628362));
#221683=CARTESIAN_POINT('Ctrl Pts',(2.65011341197134,12.2,10.0914895979888));
#221684=CARTESIAN_POINT('Ctrl Pts',(2.65043976104272,12.2,10.0942334086413));
#221685=CARTESIAN_POINT('Ctrl Pts',(2.65076611011411,12.2,10.0969772192938));
#221686=CARTESIAN_POINT('Ctrl Pts',(2.65109049311065,12.2,10.0997718698089));
#221687=CARTESIAN_POINT('Ctrl Pts',(2.65141229526573,12.2,10.1026166776201));
#221688=CARTESIAN_POINT('Ctrl Pts',(2.65173409742082,12.2,10.1054614854312));
#221689=CARTESIAN_POINT('Ctrl Pts',(2.65205331709344,12.2,10.108356448356));
#221690=CARTESIAN_POINT('Ctrl Pts',(2.65236935724883,12.2,10.1113009019123));
#221691=CARTESIAN_POINT('Ctrl Pts',(2.65268539743294,12.2,10.1142453557361));
#221692=CARTESIAN_POINT('Ctrl Pts',(2.65299825586676,12.2,10.1172392954563));
#221693=CARTESIAN_POINT('Ctrl Pts',(2.65330735305012,12.2,10.1202820707076));
#221694=CARTESIAN_POINT('Ctrl Pts',(2.65366796638857,12.2,10.1238319747529));
#221695=CARTESIAN_POINT('Ctrl Pts',(2.65402345683872,12.2,10.1274483456391));
#221696=CARTESIAN_POINT('Ctrl Pts',(2.65437292773397,12.2,10.1311301704059));
#221697=CARTESIAN_POINT('Ctrl Pts',(2.65472239865642,12.2,10.1348119954594));
#221698=CARTESIAN_POINT('Ctrl Pts',(2.65506585037871,12.2,10.1385592719262));
#221699=CARTESIAN_POINT('Ctrl Pts',(2.65540241446754,12.2,10.1423710100804));
#221700=CARTESIAN_POINT('Ctrl Pts',(2.65569089798348,12.2,10.1456382143397));
#221701=CARTESIAN_POINT('Ctrl Pts',(2.65597432136547,12.2,10.1489527781383));
#221702=CARTESIAN_POINT('Ctrl Pts',(2.6562521530469,12.2,10.1523140905746));
#221703=CARTESIAN_POINT('Ctrl Pts',(2.65652998470309,12.2,10.1556754027057));
#221704=CARTESIAN_POINT('Ctrl Pts',(2.65680222509103,12.2,10.1590834656702));
#221705=CARTESIAN_POINT('Ctrl Pts',(2.65706835574777,12.2,10.1625376759633));
#221706=CARTESIAN_POINT('Ctrl Pts',(2.6573344864045,12.2,10.1659918862565));
#221707=CARTESIAN_POINT('Ctrl Pts',(2.65759450897003,12.2,10.1694922499377));
#221708=CARTESIAN_POINT('Ctrl Pts',(2.65784791771112,12.2,10.1730381733068));
#221709=CARTESIAN_POINT('Ctrl Pts',(2.6581013264522,12.2,10.176584096676));
#221710=CARTESIAN_POINT('Ctrl Pts',(2.65834812371539,12.2,10.1801755849054));
#221711=CARTESIAN_POINT('Ctrl Pts',(2.6585878155405,12.2,10.1838120581035));
#221712=CARTESIAN_POINT('Ctrl Pts',(2.65882750738738,12.2,10.187448531632));
#221713=CARTESIAN_POINT('Ctrl Pts',(2.65906009611692,12.2,10.1911299913398));
#221714=CARTESIAN_POINT('Ctrl Pts',(2.65928510279552,12.2,10.1948558719615));
#221715=CARTESIAN_POINT('Ctrl Pts',(2.65951010945368,12.2,10.1985817522447));
#221716=CARTESIAN_POINT('Ctrl Pts',(2.65972753223983,12.2,10.2023520526612));
#221717=CARTESIAN_POINT('Ctrl Pts',(2.65993690806653,12.2,10.2061662179565));
#221718=CARTESIAN_POINT('Ctrl Pts',(2.66014628389323,12.2,10.2099803832518));
#221719=CARTESIAN_POINT('Ctrl Pts',(2.66034760926037,12.2,10.213838413436));
#221720=CARTESIAN_POINT('Ctrl Pts',(2.66054043217061,12.2,10.2177397617913));
#221721=CARTESIAN_POINT('Ctrl Pts',(2.66073325509836,12.2,10.221641110501));
#221722=CARTESIAN_POINT('Ctrl Pts',(2.66091757639077,12.2,10.2255857789084));
#221723=CARTESIAN_POINT('Ctrl Pts',(2.6610929484919,12.2,10.2295732289107));
#221724=CARTESIAN_POINT('Ctrl Pts',(2.66123909190155,12.2,10.2328961037316));
#221725=CARTESIAN_POINT('Ctrl Pts',(2.66137902430683,12.2,10.2362486888288));
#221726=CARTESIAN_POINT('Ctrl Pts',(2.66151249104242,12.2,10.239630678484));
#221727=CARTESIAN_POINT('Ctrl Pts',(2.66164595777799,12.2,10.2430126681391));
#221728=CARTESIAN_POINT('Ctrl Pts',(2.66177296119402,12.2,10.2464240615365));
#221729=CARTESIAN_POINT('Ctrl Pts',(2.66189325529069,12.2,10.2498645586916));
#221730=CARTESIAN_POINT('Ctrl Pts',(2.66203760820146,12.2,10.2539931551278));
#221731=CARTESIAN_POINT('Ctrl Pts',(2.66217229786168,12.2,10.2581636587725));
#221732=CARTESIAN_POINT('Ctrl Pts',(2.66229691002338,12.2,10.2623755582046));
#221733=CARTESIAN_POINT('Ctrl Pts',(2.66240075349523,12.2,10.2658854745256));
#221734=CARTESIAN_POINT('Ctrl Pts',(2.66249759913949,12.2,10.2694241363985));
#221735=CARTESIAN_POINT('Ctrl Pts',(2.66258721101411,12.2,10.2729912534834));
#221736=CARTESIAN_POINT('Ctrl Pts',(2.66267682288873,12.2,10.2765583705682));
#221737=CARTESIAN_POINT('Ctrl Pts',(2.66275920287207,12.2,10.2801539413877));
#221738=CARTESIAN_POINT('Ctrl Pts',(2.6628341172503,12.2,10.2837776771957));
#221739=CARTESIAN_POINT('Ctrl Pts',(2.66290903162853,12.2,10.2874014130037));
#221740=CARTESIAN_POINT('Ctrl Pts',(2.66297648223063,12.2,10.2910533150067));
#221741=CARTESIAN_POINT('Ctrl Pts',(2.66303624396611,12.2,10.2947330972312));
#221742=CARTESIAN_POINT('Ctrl Pts',(2.66310795804609,12.2,10.2991488357403));
#221743=CARTESIAN_POINT('Ctrl Pts',(2.66316859680157,12.2,10.3036047201364));
#221744=CARTESIAN_POINT('Ctrl Pts',(2.66321778096665,12.2,10.3081002687436));
#221745=CARTESIAN_POINT('Ctrl Pts',(2.66325876777237,12.2,10.3118465593857));
#221746=CARTESIAN_POINT('Ctrl Pts',(2.66329179882974,12.2,10.3156203925083));
#221747=CARTESIAN_POINT('Ctrl Pts',(2.66331665896821,12.2,10.319421492232));
#221748=CARTESIAN_POINT('Ctrl Pts',(2.66334151910667,12.2,10.3232225919557));
#221749=CARTESIAN_POINT('Ctrl Pts',(2.66335820591201,12.2,10.3270509566341));
#221750=CARTESIAN_POINT('Ctrl Pts',(2.66336651021712,12.2,10.3309063147606));
#221751=CARTESIAN_POINT('Ctrl Pts',(2.66337813624356,12.2,10.3363038158013));
#221752=CARTESIAN_POINT('Ctrl Pts',(2.66337332728298,12.2,10.3417542223926));
#221753=CARTESIAN_POINT('Ctrl Pts',(2.66335151674367,12.2,10.3472567914775));
#221754=CARTESIAN_POINT('Ctrl Pts',(2.66333593778604,12.2,10.3511871982115));
#221755=CARTESIAN_POINT('Ctrl Pts',(2.66331168425913,12.2,10.3551442209366));
#221756=CARTESIAN_POINT('Ctrl Pts',(2.6632785537043,12.2,10.3591275924622));
#221757=CARTESIAN_POINT('Ctrl Pts',(2.66323879703633,12.2,10.3639076385535));
#221758=CARTESIAN_POINT('Ctrl Pts',(2.66318625590048,12.2,10.3687256263734));
#221759=CARTESIAN_POINT('Ctrl Pts',(2.66312058922967,12.2,10.373581102723));
#221760=CARTESIAN_POINT('Ctrl Pts',(2.66305492256482,12.2,10.3784365786316));
#221761=CARTESIAN_POINT('Ctrl Pts',(2.66297612703871,12.2,10.3833295449462));
#221762=CARTESIAN_POINT('Ctrl Pts',(2.66288387145834,12.2,10.388259551706));
#221763=CARTESIAN_POINT('Ctrl Pts',(2.66280699180524,12.2,10.3923678908218));
#221764=CARTESIAN_POINT('Ctrl Pts',(2.66272076337219,12.2,10.3965019544776));
#221765=CARTESIAN_POINT('Ctrl Pts',(2.66262499552497,12.2,10.4006614837833));
#221766=CARTESIAN_POINT('Ctrl Pts',(2.66254838124302,12.2,10.4039891074091));
#221767=CARTESIAN_POINT('Ctrl Pts',(2.66246566351313,12.2,10.4073330312423));
#221768=CARTESIAN_POINT('Ctrl Pts',(2.66237674328543,12.2,10.410693125316));
#221769=CARTESIAN_POINT('Ctrl Pts',(2.66228782306984,12.2,10.4140532189319));
#221770=CARTESIAN_POINT('Ctrl Pts',(2.66219270369496,12.2,10.4174294822957));
#221771=CARTESIAN_POINT('Ctrl Pts',(2.66209128875837,12.2,10.4208217867559));
#221772=CARTESIAN_POINT('Ctrl Pts',(2.66198987380796,12.2,10.4242140916783));
#221773=CARTESIAN_POINT('Ctrl Pts',(2.66188216427429,12.2,10.4276224375355));
#221774=CARTESIAN_POINT('Ctrl Pts',(2.66176806598964,12.2,10.4310466983348));
#221775=CARTESIAN_POINT('Ctrl Pts',(2.66165396772054,12.2,10.4344709586676));
#221776=CARTESIAN_POINT('Ctrl Pts',(2.66153348128837,12.2,10.4379111323511));
#221777=CARTESIAN_POINT('Ctrl Pts',(2.66140651574362,12.2,10.4413670947342));
#221778=CARTESIAN_POINT('Ctrl Pts',(2.66124780879971,12.2,10.4456870480662));
#221779=CARTESIAN_POINT('Ctrl Pts',(2.66107897918974,12.2,10.450031669411));
#221780=CARTESIAN_POINT('Ctrl Pts',(2.66089984655007,12.2,10.4544007152642));
#221781=CARTESIAN_POINT('Ctrl Pts',(2.66075654043052,12.2,10.4578959521373));
#221782=CARTESIAN_POINT('Ctrl Pts',(2.66060664228359,12.2,10.4614068210272));
#221783=CARTESIAN_POINT('Ctrl Pts',(2.66045006394103,12.2,10.4649331967765));
#221784=CARTESIAN_POINT('Ctrl Pts',(2.66029348561982,12.2,10.4684595720453));
#221785=CARTESIAN_POINT('Ctrl Pts',(2.66013022550502,12.2,10.4720014564899));
#221786=CARTESIAN_POINT('Ctrl Pts',(2.65996019729714,12.2,10.4755587249759));
#221787=CARTESIAN_POINT('Ctrl Pts',(2.65979016906609,12.2,10.4791159939466));
#221788=CARTESIAN_POINT('Ctrl Pts',(2.65961337264584,12.2,10.4826886483612));
#221789=CARTESIAN_POINT('Ctrl Pts',(2.65942972168162,12.2,10.4862765660706));
#221790=CARTESIAN_POINT('Ctrl Pts',(2.65924607074242,12.2,10.4898644832912));
#221791=CARTESIAN_POINT('Ctrl Pts',(2.65905556443556,12.2,10.4934676640622));
#221792=CARTESIAN_POINT('Ctrl Pts',(2.65885811950771,12.2,10.4970859859876));
#221793=CARTESIAN_POINT('Ctrl Pts',(2.65866067455296,12.2,10.500704308406));
#221794=CARTESIAN_POINT('Ctrl Pts',(2.65845628988627,12.2,10.5043377743068));
#221795=CARTESIAN_POINT('Ctrl Pts',(2.65824488170762,12.2,10.5079862620067));
#221796=CARTESIAN_POINT('Ctrl Pts',(2.65803347355778,12.2,10.5116347492095));
#221797=CARTESIAN_POINT('Ctrl Pts',(2.65781504184987,12.2,10.5152982597234));
#221798=CARTESIAN_POINT('Ctrl Pts',(2.65758950502433,12.2,10.5189766737163));
#221799=CARTESIAN_POINT('Ctrl Pts',(2.65736396816805,12.2,10.5226550882103));
#221800=CARTESIAN_POINT('Ctrl Pts',(2.65713132618551,12.2,10.5263484061167));
#221801=CARTESIAN_POINT('Ctrl Pts',(2.6568914960053,12.2,10.5300565103199));
#221802=CARTESIAN_POINT('Ctrl Pts',(2.65665166585776,12.2,10.5337646140178));
#221803=CARTESIAN_POINT('Ctrl Pts',(2.65640464799223,12.2,10.5374875020459));
#221804=CARTESIAN_POINT('Ctrl Pts',(2.65615036379154,12.2,10.5412250604055));
#221805=CARTESIAN_POINT('Ctrl Pts',(2.65589607955621,12.2,10.5449626192743));
#221806=CARTESIAN_POINT('Ctrl Pts',(2.65563452727124,12.2,10.5487148455384));
#221807=CARTESIAN_POINT('Ctrl Pts',(2.65536562903312,12.2,10.5524816252608));
#221808=CARTESIAN_POINT('Ctrl Pts',(2.65509673083164,12.2,10.55624840447));
#221809=CARTESIAN_POINT('Ctrl Pts',(2.65482048568351,12.2,10.5600297367939));
#221810=CARTESIAN_POINT('Ctrl Pts',(2.65453681626302,12.2,10.563825505871));
#221811=CARTESIAN_POINT('Ctrl Pts',(2.65425314680387,12.2,10.5676212754653));
#221812=CARTESIAN_POINT('Ctrl Pts',(2.65396205249125,12.2,10.5714314816526));
#221813=CARTESIAN_POINT('Ctrl Pts',(2.65366345697498,12.2,10.5752560114166));
#221814=CARTESIAN_POINT('Ctrl Pts',(2.6533648614587,12.2,10.5790805411806));
#221815=CARTESIAN_POINT('Ctrl Pts',(2.65305876464155,12.2,10.5829193948796));
#221816=CARTESIAN_POINT('Ctrl Pts',(2.65274509045702,12.2,10.5867724566466));
#221817=CARTESIAN_POINT('Ctrl Pts',(2.65235299779045,12.2,10.5915887830678));
#221818=CARTESIAN_POINT('Ctrl Pts',(2.65194906610805,12.2,10.5964273139236));
#221819=CARTESIAN_POINT('Ctrl Pts',(2.65153314782104,12.2,10.6012878245725));
#221820=CARTESIAN_POINT('Ctrl Pts',(2.65120041313703,12.2,10.6051762337274));
#221821=CARTESIAN_POINT('Ctrl Pts',(2.65086000863283,12.2,10.6090787133337));
#221822=CARTESIAN_POINT('Ctrl Pts',(2.65051185922498,12.2,10.6129951484916));
#221823=CARTESIAN_POINT('Ctrl Pts',(2.65016370981712,12.2,10.6169115836495));
#221824=CARTESIAN_POINT('Ctrl Pts',(2.64980781704169,12.2,10.6208419761006));
#221825=CARTESIAN_POINT('Ctrl Pts',(2.6494441069655,12.2,10.6247862150948));
#221826=CARTESIAN_POINT('Ctrl Pts',(2.64908039693888,12.2,10.6287304535517));
#221827=CARTESIAN_POINT('Ctrl Pts',(2.64870887046536,12.2,10.632688538165));
#221828=CARTESIAN_POINT('Ctrl Pts',(2.6483294557169,12.2,10.6366603587472));
#221829=CARTESIAN_POINT('Ctrl Pts',(2.64795004091675,12.2,10.6406321798705));
#221830=CARTESIAN_POINT('Ctrl Pts',(2.64756273810492,12.2,10.6446177366123));
#221831=CARTESIAN_POINT('Ctrl Pts',(2.64716747669368,12.2,10.6486169203871));
#221832=CARTESIAN_POINT('Ctrl Pts',(2.64677221533629,12.2,10.6526161036171));
#221833=CARTESIAN_POINT('Ctrl Pts',(2.64636899471604,12.2,10.6566289134899));
#221834=CARTESIAN_POINT('Ctrl Pts',(2.64595774608352,12.2,10.6606552419376));
#221835=CARTESIAN_POINT('Ctrl Pts',(2.64554649739497,12.2,10.6646815709339));
#221836=CARTESIAN_POINT('Ctrl Pts',(2.64512722103601,12.2,10.6687214189096));
#221837=CARTESIAN_POINT('Ctrl Pts',(2.64469984695663,12.2,10.6727746761314));
#221838=CARTESIAN_POINT('Ctrl Pts',(2.64427247293547,12.2,10.676827932801));
#221839=CARTESIAN_POINT('Ctrl Pts',(2.64383700283561,12.2,10.6808946002805));
#221840=CARTESIAN_POINT('Ctrl Pts',(2.64339336757264,12.2,10.6849745716497));
#221841=CARTESIAN_POINT('Ctrl Pts',(2.64294973224923,12.2,10.6890545435747));
#221842=CARTESIAN_POINT('Ctrl Pts',(2.64249793301568,12.2,10.6931478192444));
#221843=CARTESIAN_POINT('Ctrl Pts',(2.64203790221229,12.2,10.6972542911358));
#221844=CARTESIAN_POINT('Ctrl Pts',(2.64157787147158,12.2,10.7013607624676));
#221845=CARTESIAN_POINT('Ctrl Pts',(2.6411096091603,12.2,10.7054804315912));
#221846=CARTESIAN_POINT('Ctrl Pts',(2.64063304931123,12.2,10.7096131921409));
#221847=CARTESIAN_POINT('Ctrl Pts',(2.64015648939721,12.2,10.7137459532536));
#221848=CARTESIAN_POINT('Ctrl Pts',(2.63967163215657,12.2,10.7178918057072));
#221849=CARTESIAN_POINT('Ctrl Pts',(2.63917841401631,12.2,10.7220506442861));
#221850=CARTESIAN_POINT('Ctrl Pts',(2.63868519594325,12.2,10.7262094822984));
#221851=CARTESIAN_POINT('Ctrl Pts',(2.63818361460192,12.2,10.7303813083564));
#221852=CARTESIAN_POINT('Ctrl Pts',(2.63767360786669,12.2,10.7345660156241));
#221853=CARTESIAN_POINT('Ctrl Pts',(2.63716360106198,12.2,10.7387507234619));
#221854=CARTESIAN_POINT('Ctrl Pts',(2.6366451669287,12.2,10.742948314051));
#221855=CARTESIAN_POINT('Ctrl Pts',(2.63611824423331,12.2,10.7471586832249));
#221856=CARTESIAN_POINT('Ctrl Pts',(2.63559132153793,12.2,10.7513690523989));
#221857=CARTESIAN_POINT('Ctrl Pts',(2.63505591051378,12.2,10.7555922006743));
#221858=CARTESIAN_POINT('Ctrl Pts',(2.6345119459277,12.2,10.7598280251842));
#221859=CARTESIAN_POINT('Ctrl Pts',(2.63383199030629,12.2,10.7651228049559));
#221860=CARTESIAN_POINT('Ctrl Pts',(2.63313867280872,12.2,10.7704373907742));
#221861=CARTESIAN_POINT('Ctrl Pts',(2.63243187365076,12.2,10.7757715838022));
#221862=CARTESIAN_POINT('Ctrl Pts',(2.63186643423193,12.2,10.7800389389224));
#221863=CARTESIAN_POINT('Ctrl Pts',(2.63129236556785,12.2,10.7843188425327));
#221864=CARTESIAN_POINT('Ctrl Pts',(2.63070960825831,12.2,10.7886111924333));
#221865=CARTESIAN_POINT('Ctrl Pts',(2.63012685094879,12.2,10.7929035423338));
#221866=CARTESIAN_POINT('Ctrl Pts',(2.62953540452712,12.2,10.7972083395831));
#221867=CARTESIAN_POINT('Ctrl Pts',(2.62893520866017,12.2,10.8015254834308));
#221868=CARTESIAN_POINT('Ctrl Pts',(2.628335012875,12.2,10.8058426266903));
#221869=CARTESIAN_POINT('Ctrl Pts',(2.62772606954156,12.2,10.8101721161739));
#221870=CARTESIAN_POINT('Ctrl Pts',(2.6271083177004,12.2,10.8145138520053));
#221871=CARTESIAN_POINT('Ctrl Pts',(2.62649056577506,12.2,10.8188555884283));
#221872=CARTESIAN_POINT('Ctrl Pts',(2.62586400646495,12.2,10.8232095702718));
#221873=CARTESIAN_POINT('Ctrl Pts',(2.62522858109608,12.2,10.8275756994555));
#221874=CARTESIAN_POINT('Ctrl Pts',(2.62459315581379,12.2,10.8319418280442));
#221875=CARTESIAN_POINT('Ctrl Pts',(2.62394886448265,12.2,10.8363201025008));
#221876=CARTESIAN_POINT('Ctrl Pts',(2.62329565053663,12.2,10.8407104251411));
#221877=CARTESIAN_POINT('Ctrl Pts',(2.62280574005486,12.2,10.8440031672709));
#221878=CARTESIAN_POINT('Ctrl Pts',(2.62231080880289,12.2,10.8473026863327));
#221879=CARTESIAN_POINT('Ctrl Pts',(2.62181083583833,12.2,10.8506089410853));
#221880=CARTESIAN_POINT('Ctrl Pts',(2.62131086287377,12.2,10.8539151958379));
#221881=CARTESIAN_POINT('Ctrl Pts',(2.62080584795862,12.2,10.8572281859478));
#221882=CARTESIAN_POINT('Ctrl Pts',(2.62029576460284,12.2,10.8605478695762));
#221883=CARTESIAN_POINT('Ctrl Pts',(2.6197856811544,12.2,10.8638675538078));
#221884=CARTESIAN_POINT('Ctrl Pts',(2.6192705308962,12.2,10.8671939320079));
#221885=CARTESIAN_POINT('Ctrl Pts',(2.61875029040323,12.2,10.8705269637016));
#221886=CARTESIAN_POINT('Ctrl Pts',(2.61823005000476,12.2,10.8738599947897));
#221887=CARTESIAN_POINT('Ctrl Pts',(2.61770471955658,12.2,10.8771996783191));
#221888=CARTESIAN_POINT('Ctrl Pts',(2.61717427570041,12.2,10.8805459743648));
#221889=CARTESIAN_POINT('Ctrl Pts',(2.61664383184423,12.2,10.8838922704105));
#221890=CARTESIAN_POINT('Ctrl Pts',(2.61610827526565,12.2,10.8872451779264));
#221891=CARTESIAN_POINT('Ctrl Pts',(2.61556758099115,12.2,10.890604657028));
#221892=CARTESIAN_POINT('Ctrl Pts',(2.61484665532456,12.2,10.8950839622933));
#221893=CARTESIAN_POINT('Ctrl Pts',(2.61411659988447,12.2,10.8995749490469));
#221894=CARTESIAN_POINT('Ctrl Pts',(2.61337735811251,12.2,10.9040775229554));
#221895=CARTESIAN_POINT('Ctrl Pts',(2.61282292665763,12.2,10.9074544541537));
#221896=CARTESIAN_POINT('Ctrl Pts',(2.61226332910964,12.2,10.9108379019454));
#221897=CARTESIAN_POINT('Ctrl Pts',(2.61169854211018,12.2,10.914227826689));
#221898=CARTESIAN_POINT('Ctrl Pts',(2.61094549294858,12.2,10.9187477253207));
#221899=CARTESIAN_POINT('Ctrl Pts',(2.6101832194604,12.2,10.9232791378452));
#221900=CARTESIAN_POINT('Ctrl Pts',(2.60941166707963,12.2,10.927821970362));
#221901=CARTESIAN_POINT('Ctrl Pts',(2.60883300276778,12.2,10.9312290949044));
#221902=CARTESIAN_POINT('Ctrl Pts',(2.60824911997133,12.2,10.9346426422758));
#221903=CARTESIAN_POINT('Ctrl Pts',(2.60765999663058,12.2,10.9380625731133));
#221904=CARTESIAN_POINT('Ctrl Pts',(2.60707087328983,12.2,10.9414825039508));
#221905=CARTESIAN_POINT('Ctrl Pts',(2.60647651094153,12.2,10.9449088187939));
#221906=CARTESIAN_POINT('Ctrl Pts',(2.60587688467236,12.2,10.9483414765016));
#221907=CARTESIAN_POINT('Ctrl Pts',(2.60527725829426,12.2,10.951774134833));
#221908=CARTESIAN_POINT('Ctrl Pts',(2.60467237008969,12.2,10.9552131372328));
#221909=CARTESIAN_POINT('Ctrl Pts',(2.60406219812529,12.2,10.9586584434844));
#221910=CARTESIAN_POINT('Ctrl Pts',(2.60345202627174,12.2,10.96210374911));
#221911=CARTESIAN_POINT('Ctrl Pts',(2.60283656999347,12.2,10.9655553577187));
#221912=CARTESIAN_POINT('Ctrl Pts',(2.60221580914056,12.2,10.9690132318436));
#221913=CARTESIAN_POINT('Ctrl Pts',(2.60138812804095,12.2,10.9736237304674));
#221914=CARTESIAN_POINT('Ctrl Pts',(2.60055101650336,12.2,10.9782453664149));
#221915=CARTESIAN_POINT('Ctrl Pts',(2.59970442336445,12.2,10.9828780453778));
#221916=CARTESIAN_POINT('Ctrl Pts',(2.59906947848142,12.2,10.9863525547577));
#221917=CARTESIAN_POINT('Ctrl Pts',(2.59842920046654,12.2,10.989833277284));
#221918=CARTESIAN_POINT('Ctrl Pts',(2.59778356911573,12.2,10.9933201719898));
#221919=CARTESIAN_POINT('Ctrl Pts',(2.59713793764762,12.2,10.9968070673291));
#221920=CARTESIAN_POINT('Ctrl Pts',(2.59648695306968,12.2,11.0003001357701));
#221921=CARTESIAN_POINT('Ctrl Pts',(2.59583059309856,12.2,11.0037993390295));
#221922=CARTESIAN_POINT('Ctrl Pts',(2.59495544666912,12.2,11.0084649423158));
#221923=CARTESIAN_POINT('Ctrl Pts',(2.59407074612426,12.2,11.0131414503702));
#221924=CARTESIAN_POINT('Ctrl Pts',(2.59317644303133,12.2,11.0178287723752));
#221925=CARTESIAN_POINT('Ctrl Pts',(2.59250571568118,12.2,11.0213442640386));
#221926=CARTESIAN_POINT('Ctrl Pts',(2.59182958635638,12.2,11.0248658385099));
#221927=CARTESIAN_POINT('Ctrl Pts',(2.59114803642356,12.2,11.0283934567143));
#221928=CARTESIAN_POINT('Ctrl Pts',(2.59046648636691,12.2,11.0319210755594));
#221929=CARTESIAN_POINT('Ctrl Pts',(2.58977951378373,12.2,11.035454738723));
#221930=CARTESIAN_POINT('Ctrl Pts',(2.58908710030737,12.2,11.0389944079883));
#221931=CARTESIAN_POINT('Ctrl Pts',(2.58839468695679,12.2,11.0425340766104));
#221932=CARTESIAN_POINT('Ctrl Pts',(2.58769683282407,12.2,11.0460797509048));
#221933=CARTESIAN_POINT('Ctrl Pts',(2.58699351739719,12.2,11.0496313932038));
#221934=CARTESIAN_POINT('Ctrl Pts',(2.58605576353728,12.2,11.0543669160541));
#221935=CARTESIAN_POINT('Ctrl Pts',(2.58510829972704,12.2,11.0591130463035));
#221936=CARTESIAN_POINT('Ctrl Pts',(2.58415108202815,12.2,11.0638696963028));
#221937=CARTESIAN_POINT('Ctrl Pts',(2.58343316872137,12.2,11.0674371839644));
#221938=CARTESIAN_POINT('Ctrl Pts',(2.58270976921498,12.2,11.0710105893172));
#221939=CARTESIAN_POINT('Ctrl Pts',(2.58198086240888,12.2,11.074589872978));
#221940=CARTESIAN_POINT('Ctrl Pts',(2.58125195547036,12.2,11.078169157289));
#221941=CARTESIAN_POINT('Ctrl Pts',(2.58051754229697,12.2,11.0817543204768));
#221942=CARTESIAN_POINT('Ctrl Pts',(2.57977760385534,12.2,11.0853453252911));
#221943=CARTESIAN_POINT('Ctrl Pts',(2.57879101949055,12.2,11.090133330623));
#221944=CARTESIAN_POINT('Ctrl Pts',(2.57779461263128,12.2,11.094931720168));
#221945=CARTESIAN_POINT('Ctrl Pts',(2.576788338209,12.2,11.0997404054634));
#221946=CARTESIAN_POINT('Ctrl Pts',(2.57603363235801,12.2,11.1033469195987));
#221947=CARTESIAN_POINT('Ctrl Pts',(2.57527337593838,12.2,11.1069592246876));
#221948=CARTESIAN_POINT('Ctrl Pts',(2.57450755063337,12.2,11.110577283389));
#221949=CARTESIAN_POINT('Ctrl Pts',(2.57374172532834,12.2,11.1141953420904));
#221950=CARTESIAN_POINT('Ctrl Pts',(2.57297033109037,12.2,11.1178191552247));
#221951=CARTESIAN_POINT('Ctrl Pts',(2.57219334936936,12.2,11.121448684967));
#221952=CARTESIAN_POINT('Ctrl Pts',(2.57115737364725,12.2,11.1262880583964));
#221953=CARTESIAN_POINT('Ctrl Pts',(2.57011146574774,12.2,11.1311375975913));
#221954=CARTESIAN_POINT('Ctrl Pts',(2.56905558174093,12.2,11.1359972097116));
#221955=CARTESIAN_POINT('Ctrl Pts',(2.56826366880775,12.2,11.1396419184707));
#221956=CARTESIAN_POINT('Ctrl Pts',(2.56746614255848,12.2,11.1432922950796));
#221957=CARTESIAN_POINT('Ctrl Pts',(2.56666298675071,12.2,11.1469482997966));
#221958=CARTESIAN_POINT('Ctrl Pts',(2.56585983094294,12.2,11.1506043045137));
#221959=CARTESIAN_POINT('Ctrl Pts',(2.56505104525857,12.2,11.1542659381007));
#221960=CARTESIAN_POINT('Ctrl Pts',(2.56423661208033,12.2,11.1579331668836));
#221961=CARTESIAN_POINT('Ctrl Pts',(2.56342217890209,12.2,11.1616003956665));
#221962=CARTESIAN_POINT('Ctrl Pts',(2.56260210048255,12.2,11.1652732199658));
#221963=CARTESIAN_POINT('Ctrl Pts',(2.56177635817999,12.2,11.1689516051647));
#221964=CARTESIAN_POINT('Ctrl Pts',(2.56095061572743,12.2,11.1726299910319));
#221965=CARTESIAN_POINT('Ctrl Pts',(2.56011920953992,12.2,11.1763139382507));
#221966=CARTESIAN_POINT('Ctrl Pts',(2.55928211854249,12.2,11.1800034004959));
#221967=CARTESIAN_POINT('Ctrl Pts',(2.55844502769714,12.2,11.183692862071));
#221968=CARTESIAN_POINT('Ctrl Pts',(2.55760225159798,12.2,11.1873878384482));
#221969=CARTESIAN_POINT('Ctrl Pts',(2.55675377133577,12.2,11.1910882904993));
#221970=CARTESIAN_POINT('Ctrl Pts',(2.55590529107355,12.2,11.1947887425503));
#221971=CARTESIAN_POINT('Ctrl Pts',(2.55505110672384,12.2,11.198494670904));
#221972=CARTESIAN_POINT('Ctrl Pts',(2.55419121115239,12.2,11.2022060571883));
#221973=CARTESIAN_POINT('Ctrl Pts',(2.55333131558093,12.2,11.2059174434726));
#221974=CARTESIAN_POINT('Ctrl Pts',(2.55246570515823,12.2,11.2096342873238));
#221975=CARTESIAN_POINT('Ctrl Pts',(2.55159438999994,12.2,11.213356593));
#221976=CARTESIAN_POINT('Ctrl Pts',(2.17615954699994,15.2,11.292224299));
#221977=CARTESIAN_POINT('Ctrl Pts',(2.17615954699994,11.6,11.292224299));
#221978=CARTESIAN_POINT('Ctrl Pts',(2.17570045499994,15.2,11.291612888));
#221979=CARTESIAN_POINT('Ctrl Pts',(2.17570045499994,11.6,11.291612888));
#221980=CARTESIAN_POINT('Ctrl Pts',(2.17478276499994,15.2,11.290390245));
#221981=CARTESIAN_POINT('Ctrl Pts',(2.17478276499994,11.6,11.290390245));
#221982=CARTESIAN_POINT('Ctrl Pts',(2.17340771699994,15.2,11.28855682));
#221983=CARTESIAN_POINT('Ctrl Pts',(2.17340771699994,11.6,11.28855682));
#221984=CARTESIAN_POINT('Ctrl Pts',(2.17157728799994,15.2,11.286113333));
#221985=CARTESIAN_POINT('Ctrl Pts',(2.17157728799994,11.6,11.286113333));
#221986=CARTESIAN_POINT('Ctrl Pts',(2.16929420199994,15.2,11.283060774));
#221987=CARTESIAN_POINT('Ctrl Pts',(2.16929420199994,11.6,11.283060774));
#221988=CARTESIAN_POINT('Ctrl Pts',(2.16701606599994,15.2,11.280010014));
#221989=CARTESIAN_POINT('Ctrl Pts',(2.16701606599994,11.6,11.280010014));
#221990=CARTESIAN_POINT('Ctrl Pts',(2.16474288099994,15.2,11.276961058));
#221991=CARTESIAN_POINT('Ctrl Pts',(2.16474288099994,11.6,11.276961058));
#221992=CARTESIAN_POINT('Ctrl Pts',(2.16247464499994,15.2,11.273913908));
#221993=CARTESIAN_POINT('Ctrl Pts',(2.16247464499994,11.6,11.273913908));
#221994=CARTESIAN_POINT('Ctrl Pts',(2.16021135899994,15.2,11.270868571));
#221995=CARTESIAN_POINT('Ctrl Pts',(2.16021135899994,11.6,11.270868571));
#221996=CARTESIAN_POINT('Ctrl Pts',(2.15795302399994,15.2,11.267825055));
#221997=CARTESIAN_POINT('Ctrl Pts',(2.15795302399994,11.6,11.267825055));
#221998=CARTESIAN_POINT('Ctrl Pts',(2.15569963799994,15.2,11.264783368));
#221999=CARTESIAN_POINT('Ctrl Pts',(2.15569963799994,11.6,11.264783368));
#222000=CARTESIAN_POINT('Ctrl Pts',(2.15345120199994,15.2,11.261743524));
#222001=CARTESIAN_POINT('Ctrl Pts',(2.15345120199994,11.6,11.261743524));
#222002=CARTESIAN_POINT('Ctrl Pts',(2.15120771399994,15.2,11.258705532));
#222003=CARTESIAN_POINT('Ctrl Pts',(2.15120771399994,11.6,11.258705532));
#222004=CARTESIAN_POINT('Ctrl Pts',(2.14896917399995,15.2,11.255669403));
#222005=CARTESIAN_POINT('Ctrl Pts',(2.14896917399995,11.6,11.255669403));
#222006=CARTESIAN_POINT('Ctrl Pts',(2.14673558299994,15.2,11.252635149));
#222007=CARTESIAN_POINT('Ctrl Pts',(2.14673558299994,11.6,11.252635149));
#222008=CARTESIAN_POINT('Ctrl Pts',(2.14450693999995,15.2,11.249602778));
#222009=CARTESIAN_POINT('Ctrl Pts',(2.14450693999995,11.6,11.249602778));
#222010=CARTESIAN_POINT('Ctrl Pts',(2.14228324299994,15.2,11.246572299));
#222011=CARTESIAN_POINT('Ctrl Pts',(2.14228324299994,11.6,11.246572299));
#222012=CARTESIAN_POINT('Ctrl Pts',(2.14006449499994,15.2,11.243543721));
#222013=CARTESIAN_POINT('Ctrl Pts',(2.14006449499994,11.6,11.243543721));
#222014=CARTESIAN_POINT('Ctrl Pts',(2.13785069299994,15.2,11.24051705));
#222015=CARTESIAN_POINT('Ctrl Pts',(2.13785069299994,11.6,11.24051705));
#222016=CARTESIAN_POINT('Ctrl Pts',(2.13564183699994,15.2,11.237492297));
#222017=CARTESIAN_POINT('Ctrl Pts',(2.13564183699994,11.6,11.237492297));
#222018=CARTESIAN_POINT('Ctrl Pts',(2.13343792799995,15.2,11.234469469));
#222019=CARTESIAN_POINT('Ctrl Pts',(2.13343792799995,11.6,11.234469469));
#222020=CARTESIAN_POINT('Ctrl Pts',(2.13123896499994,15.2,11.231448575));
#222021=CARTESIAN_POINT('Ctrl Pts',(2.13123896499994,11.6,11.231448575));
#222022=CARTESIAN_POINT('Ctrl Pts',(2.12904494799994,15.2,11.228429624));
#222023=CARTESIAN_POINT('Ctrl Pts',(2.12904494799994,11.6,11.228429624));
#222024=CARTESIAN_POINT('Ctrl Pts',(2.12685587499994,15.2,11.225412627));
#222025=CARTESIAN_POINT('Ctrl Pts',(2.12685587499994,11.6,11.225412627));
#222026=CARTESIAN_POINT('Ctrl Pts',(2.12467174699994,15.2,11.222397591));
#222027=CARTESIAN_POINT('Ctrl Pts',(2.12467174699994,11.6,11.222397591));
#222028=CARTESIAN_POINT('Ctrl Pts',(2.12249256499994,15.2,11.219384528));
#222029=CARTESIAN_POINT('Ctrl Pts',(2.12249256499994,11.6,11.219384528));
#222030=CARTESIAN_POINT('Ctrl Pts',(2.12031832399994,15.2,11.216373447));
#222031=CARTESIAN_POINT('Ctrl Pts',(2.12031832399994,11.6,11.216373447));
#222032=CARTESIAN_POINT('Ctrl Pts',(2.11814902899994,15.2,11.213364355));
#222033=CARTESIAN_POINT('Ctrl Pts',(2.11814902899994,11.6,11.213364355));
#222034=CARTESIAN_POINT('Ctrl Pts',(2.11598467599994,15.2,11.210357263));
#222035=CARTESIAN_POINT('Ctrl Pts',(2.11598467599994,11.6,11.210357263));
#222036=CARTESIAN_POINT('Ctrl Pts',(2.11382526699994,15.2,11.207352181));
#222037=CARTESIAN_POINT('Ctrl Pts',(2.11382526699994,11.6,11.207352181));
#222038=CARTESIAN_POINT('Ctrl Pts',(2.11167079899994,15.2,11.204349116));
#222039=CARTESIAN_POINT('Ctrl Pts',(2.11167079899994,11.6,11.204349116));
#222040=CARTESIAN_POINT('Ctrl Pts',(2.10952127399994,15.2,11.201348078));
#222041=CARTESIAN_POINT('Ctrl Pts',(2.10952127399994,11.6,11.201348078));
#222042=CARTESIAN_POINT('Ctrl Pts',(2.10737668999994,15.2,11.198349076));
#222043=CARTESIAN_POINT('Ctrl Pts',(2.10737668999994,11.6,11.198349076));
#222044=CARTESIAN_POINT('Ctrl Pts',(2.10523704699995,15.2,11.19535212));
#222045=CARTESIAN_POINT('Ctrl Pts',(2.10523704699995,11.6,11.19535212));
#222046=CARTESIAN_POINT('Ctrl Pts',(2.10310234499994,15.2,11.192357218));
#222047=CARTESIAN_POINT('Ctrl Pts',(2.10310234499994,11.6,11.192357218));
#222048=CARTESIAN_POINT('Ctrl Pts',(2.10097258199994,15.2,11.189364381));
#222049=CARTESIAN_POINT('Ctrl Pts',(2.10097258199994,11.6,11.189364381));
#222050=CARTESIAN_POINT('Ctrl Pts',(2.09884775899994,15.2,11.186373617));
#222051=CARTESIAN_POINT('Ctrl Pts',(2.09884775899994,11.6,11.186373617));
#222052=CARTESIAN_POINT('Ctrl Pts',(2.09672787599994,15.2,11.183384935));
#222053=CARTESIAN_POINT('Ctrl Pts',(2.09672787599994,11.6,11.183384935));
#222054=CARTESIAN_POINT('Ctrl Pts',(2.09461293099994,15.2,11.180398346));
#222055=CARTESIAN_POINT('Ctrl Pts',(2.09461293099994,11.6,11.180398346));
#222056=CARTESIAN_POINT('Ctrl Pts',(2.09250292399994,15.2,11.177413859));
#222057=CARTESIAN_POINT('Ctrl Pts',(2.09250292399994,11.6,11.177413859));
#222058=CARTESIAN_POINT('Ctrl Pts',(2.09039785499994,15.2,11.174431483));
#222059=CARTESIAN_POINT('Ctrl Pts',(2.09039785499994,11.6,11.174431483));
#222060=CARTESIAN_POINT('Ctrl Pts',(2.08829772299994,15.2,11.171451227));
#222061=CARTESIAN_POINT('Ctrl Pts',(2.08829772299994,11.6,11.171451227));
#222062=CARTESIAN_POINT('Ctrl Pts',(2.08620252699994,15.2,11.168473101));
#222063=CARTESIAN_POINT('Ctrl Pts',(2.08620252699994,11.6,11.168473101));
#222064=CARTESIAN_POINT('Ctrl Pts',(2.08411226699994,15.2,11.165497114));
#222065=CARTESIAN_POINT('Ctrl Pts',(2.08411226699994,11.6,11.165497114));
#222066=CARTESIAN_POINT('Ctrl Pts',(2.08202694399994,15.2,11.162523276));
#222067=CARTESIAN_POINT('Ctrl Pts',(2.08202694399994,11.6,11.162523276));
#222068=CARTESIAN_POINT('Ctrl Pts',(2.07994655499994,15.2,11.159551596));
#222069=CARTESIAN_POINT('Ctrl Pts',(2.07994655499994,11.6,11.159551596));
#222070=CARTESIAN_POINT('Ctrl Pts',(2.07787109999995,15.2,11.156582083));
#222071=CARTESIAN_POINT('Ctrl Pts',(2.07787109999995,11.6,11.156582083));
#222072=CARTESIAN_POINT('Ctrl Pts',(2.07580057999994,15.2,11.153614749));
#222073=CARTESIAN_POINT('Ctrl Pts',(2.07580057999994,11.6,11.153614749));
#222074=CARTESIAN_POINT('Ctrl Pts',(2.07373499199994,15.2,11.1506496));
#222075=CARTESIAN_POINT('Ctrl Pts',(2.07373499199994,11.6,11.1506496));
#222076=CARTESIAN_POINT('Ctrl Pts',(2.07167433699994,15.2,11.147686647));
#222077=CARTESIAN_POINT('Ctrl Pts',(2.07167433699994,11.6,11.147686647));
#222078=CARTESIAN_POINT('Ctrl Pts',(2.06961861499994,15.2,11.144725901));
#222079=CARTESIAN_POINT('Ctrl Pts',(2.06961861499994,11.6,11.144725901));
#222080=CARTESIAN_POINT('Ctrl Pts',(2.06756782299994,15.2,11.14176737));
#222081=CARTESIAN_POINT('Ctrl Pts',(2.06756782299994,11.6,11.14176737));
#222082=CARTESIAN_POINT('Ctrl Pts',(2.06552196199994,15.2,11.138811063));
#222083=CARTESIAN_POINT('Ctrl Pts',(2.06552196199994,11.6,11.138811063));
#222084=CARTESIAN_POINT('Ctrl Pts',(2.06348103199994,15.2,11.13585699));
#222085=CARTESIAN_POINT('Ctrl Pts',(2.06348103199994,11.6,11.13585699));
#222086=CARTESIAN_POINT('Ctrl Pts',(2.06144503099994,15.2,11.132905163));
#222087=CARTESIAN_POINT('Ctrl Pts',(2.06144503099994,11.6,11.132905163));
#222088=CARTESIAN_POINT('Ctrl Pts',(2.05941395899994,15.2,11.129955588));
#222089=CARTESIAN_POINT('Ctrl Pts',(2.05941395899994,11.6,11.129955588));
#222090=CARTESIAN_POINT('Ctrl Pts',(2.05738781599994,15.2,11.127008278));
#222091=CARTESIAN_POINT('Ctrl Pts',(2.05738781599994,11.6,11.127008278));
#222092=CARTESIAN_POINT('Ctrl Pts',(2.05536659999995,15.2,11.12406324));
#222093=CARTESIAN_POINT('Ctrl Pts',(2.05536659999995,11.6,11.12406324));
#222094=CARTESIAN_POINT('Ctrl Pts',(2.05335030999994,15.2,11.121120485));
#222095=CARTESIAN_POINT('Ctrl Pts',(2.05335030999994,11.6,11.121120485));
#222096=CARTESIAN_POINT('Ctrl Pts',(2.05133894799994,15.2,11.118180022));
#222097=CARTESIAN_POINT('Ctrl Pts',(2.05133894799994,11.6,11.118180022));
#222098=CARTESIAN_POINT('Ctrl Pts',(2.04933251099995,15.2,11.115241863));
#222099=CARTESIAN_POINT('Ctrl Pts',(2.04933251099995,11.6,11.115241863));
#222100=CARTESIAN_POINT('Ctrl Pts',(2.04733099799994,15.2,11.112306014));
#222101=CARTESIAN_POINT('Ctrl Pts',(2.04733099799994,11.6,11.112306014));
#222102=CARTESIAN_POINT('Ctrl Pts',(2.04533441099994,15.2,11.109372487));
#222103=CARTESIAN_POINT('Ctrl Pts',(2.04533441099994,11.6,11.109372487));
#222104=CARTESIAN_POINT('Ctrl Pts',(2.04334274699994,15.2,11.106441291));
#222105=CARTESIAN_POINT('Ctrl Pts',(2.04334274699994,11.6,11.106441291));
#222106=CARTESIAN_POINT('Ctrl Pts',(2.04135600499994,15.2,11.103512437));
#222107=CARTESIAN_POINT('Ctrl Pts',(2.04135600499994,11.6,11.103512437));
#222108=CARTESIAN_POINT('Ctrl Pts',(2.03937418399994,15.2,11.100585934));
#222109=CARTESIAN_POINT('Ctrl Pts',(2.03937418399994,11.6,11.100585934));
#222110=CARTESIAN_POINT('Ctrl Pts',(2.03739728499994,15.2,11.097661791));
#222111=CARTESIAN_POINT('Ctrl Pts',(2.03739728499994,11.6,11.097661791));
#222112=CARTESIAN_POINT('Ctrl Pts',(2.03542530699994,15.2,11.094740019));
#222113=CARTESIAN_POINT('Ctrl Pts',(2.03542530699994,11.6,11.094740019));
#222114=CARTESIAN_POINT('Ctrl Pts',(2.03345824999994,15.2,11.091820628));
#222115=CARTESIAN_POINT('Ctrl Pts',(2.03345824999994,11.6,11.091820628));
#222116=CARTESIAN_POINT('Ctrl Pts',(2.03149610999994,15.2,11.088903627));
#222117=CARTESIAN_POINT('Ctrl Pts',(2.03149610999994,11.6,11.088903627));
#222118=CARTESIAN_POINT('Ctrl Pts',(2.02953888899994,15.2,11.085989026));
#222119=CARTESIAN_POINT('Ctrl Pts',(2.02953888899994,11.6,11.085989026));
#222120=CARTESIAN_POINT('Ctrl Pts',(2.02758658499994,15.2,11.083076836));
#222121=CARTESIAN_POINT('Ctrl Pts',(2.02758658499994,11.6,11.083076836));
#222122=CARTESIAN_POINT('Ctrl Pts',(2.02563919799994,15.2,11.080167065));
#222123=CARTESIAN_POINT('Ctrl Pts',(2.02563919799994,11.6,11.080167065));
#222124=CARTESIAN_POINT('Ctrl Pts',(2.02369672699994,15.2,11.077259725));
#222125=CARTESIAN_POINT('Ctrl Pts',(2.02369672699994,11.6,11.077259725));
#222126=CARTESIAN_POINT('Ctrl Pts',(2.02175917099995,15.2,11.074354824));
#222127=CARTESIAN_POINT('Ctrl Pts',(2.02175917099995,11.6,11.074354824));
#222128=CARTESIAN_POINT('Ctrl Pts',(2.01982652899994,15.2,11.071452374));
#222129=CARTESIAN_POINT('Ctrl Pts',(2.01982652899994,11.6,11.071452374));
#222130=CARTESIAN_POINT('Ctrl Pts',(2.01789879999994,15.2,11.068552383));
#222131=CARTESIAN_POINT('Ctrl Pts',(2.01789879999994,11.6,11.068552383));
#222132=CARTESIAN_POINT('Ctrl Pts',(2.01597598299994,15.2,11.065654862));
#222133=CARTESIAN_POINT('Ctrl Pts',(2.01597598299994,11.6,11.065654862));
#222134=CARTESIAN_POINT('Ctrl Pts',(2.01405807799994,15.2,11.062759822));
#222135=CARTESIAN_POINT('Ctrl Pts',(2.01405807799994,11.6,11.062759822));
#222136=CARTESIAN_POINT('Ctrl Pts',(2.01214508399994,15.2,11.059867271));
#222137=CARTESIAN_POINT('Ctrl Pts',(2.01214508399994,11.6,11.059867271));
#222138=CARTESIAN_POINT('Ctrl Pts',(2.01023699999994,15.2,11.056977221));
#222139=CARTESIAN_POINT('Ctrl Pts',(2.01023699999994,11.6,11.056977221));
#222140=CARTESIAN_POINT('Ctrl Pts',(2.00833382599995,15.2,11.054089681));
#222141=CARTESIAN_POINT('Ctrl Pts',(2.00833382599995,11.6,11.054089681));
#222142=CARTESIAN_POINT('Ctrl Pts',(2.00643555799994,15.2,11.051204661));
#222143=CARTESIAN_POINT('Ctrl Pts',(2.00643555799994,11.6,11.051204661));
#222144=CARTESIAN_POINT('Ctrl Pts',(2.00454219899994,15.2,11.048322171));
#222145=CARTESIAN_POINT('Ctrl Pts',(2.00454219899994,11.6,11.048322171));
#222146=CARTESIAN_POINT('Ctrl Pts',(2.00265374499994,15.2,11.045442222));
#222147=CARTESIAN_POINT('Ctrl Pts',(2.00265374499994,11.6,11.045442222));
#222148=CARTESIAN_POINT('Ctrl Pts',(2.00077019699994,15.2,11.042564824));
#222149=CARTESIAN_POINT('Ctrl Pts',(2.00077019699994,11.6,11.042564824));
#222150=CARTESIAN_POINT('Ctrl Pts',(1.99889155299994,15.2,11.039689986));
#222151=CARTESIAN_POINT('Ctrl Pts',(1.99889155299994,11.6,11.039689986));
#222152=CARTESIAN_POINT('Ctrl Pts',(1.99701781299994,15.2,11.036817721));
#222153=CARTESIAN_POINT('Ctrl Pts',(1.99701781299994,11.6,11.036817721));
#222154=CARTESIAN_POINT('Ctrl Pts',(1.99514897499994,15.2,11.033948035));
#222155=CARTESIAN_POINT('Ctrl Pts',(1.99514897499994,11.6,11.033948035));
#222156=CARTESIAN_POINT('Ctrl Pts',(1.99328503899994,15.2,11.031080942));
#222157=CARTESIAN_POINT('Ctrl Pts',(1.99328503899994,11.6,11.031080942));
#222158=CARTESIAN_POINT('Ctrl Pts',(1.99142600299994,15.2,11.02821645));
#222159=CARTESIAN_POINT('Ctrl Pts',(1.99142600299994,11.6,11.02821645));
#222160=CARTESIAN_POINT('Ctrl Pts',(1.98957186799994,15.2,11.025354571));
#222161=CARTESIAN_POINT('Ctrl Pts',(1.98957186799994,11.6,11.025354571));
#222162=CARTESIAN_POINT('Ctrl Pts',(1.98772262899995,15.2,11.022495314));
#222163=CARTESIAN_POINT('Ctrl Pts',(1.98772262899995,11.6,11.022495314));
#222164=CARTESIAN_POINT('Ctrl Pts',(1.98587828999994,15.2,11.019638689));
#222165=CARTESIAN_POINT('Ctrl Pts',(1.98587828999994,11.6,11.019638689));
#222166=CARTESIAN_POINT('Ctrl Pts',(1.98403884699994,15.2,11.016784707));
#222167=CARTESIAN_POINT('Ctrl Pts',(1.98403884699994,11.6,11.016784707));
#222168=CARTESIAN_POINT('Ctrl Pts',(1.98220429799994,15.2,11.01393338));
#222169=CARTESIAN_POINT('Ctrl Pts',(1.98220429799994,11.6,11.01393338));
#222170=CARTESIAN_POINT('Ctrl Pts',(1.98037464499994,15.2,11.011084715));
#222171=CARTESIAN_POINT('Ctrl Pts',(1.98037464499994,11.6,11.011084715));
#222172=CARTESIAN_POINT('Ctrl Pts',(1.97854988599994,15.2,11.008238724));
#222173=CARTESIAN_POINT('Ctrl Pts',(1.97854988599994,11.6,11.008238724));
#222174=CARTESIAN_POINT('Ctrl Pts',(1.97673001799994,15.2,11.005395419));
#222175=CARTESIAN_POINT('Ctrl Pts',(1.97673001799994,11.6,11.005395419));
#222176=CARTESIAN_POINT('Ctrl Pts',(1.97491504199994,15.2,11.002554807));
#222177=CARTESIAN_POINT('Ctrl Pts',(1.97491504199994,11.6,11.002554807));
#222178=CARTESIAN_POINT('Ctrl Pts',(1.97310495599994,15.2,10.999716902));
#222179=CARTESIAN_POINT('Ctrl Pts',(1.97310495599994,11.6,10.999716902));
#222180=CARTESIAN_POINT('Ctrl Pts',(1.97129975999994,15.2,10.996881711));
#222181=CARTESIAN_POINT('Ctrl Pts',(1.97129975999994,11.6,10.996881711));
#222182=CARTESIAN_POINT('Ctrl Pts',(1.96949945099994,15.2,10.994049248));
#222183=CARTESIAN_POINT('Ctrl Pts',(1.96949945099994,11.6,10.994049248));
#222184=CARTESIAN_POINT('Ctrl Pts',(1.96770402899994,15.2,10.991219521));
#222185=CARTESIAN_POINT('Ctrl Pts',(1.96770402899994,11.6,10.991219521));
#222186=CARTESIAN_POINT('Ctrl Pts',(1.96591349399994,15.2,10.988392541));
#222187=CARTESIAN_POINT('Ctrl Pts',(1.96591349399994,11.6,10.988392541));
#222188=CARTESIAN_POINT('Ctrl Pts',(1.96412784199994,15.2,10.98556832));
#222189=CARTESIAN_POINT('Ctrl Pts',(1.96412784199994,11.6,10.98556832));
#222190=CARTESIAN_POINT('Ctrl Pts',(1.96234707499994,15.2,10.982746866));
#222191=CARTESIAN_POINT('Ctrl Pts',(1.96234707499994,11.6,10.982746866));
#222192=CARTESIAN_POINT('Ctrl Pts',(1.96057118999994,15.2,10.979928192));
#222193=CARTESIAN_POINT('Ctrl Pts',(1.96057118999994,11.6,10.979928192));
#222194=CARTESIAN_POINT('Ctrl Pts',(1.95880018599994,15.2,10.977112307));
#222195=CARTESIAN_POINT('Ctrl Pts',(1.95880018599994,11.6,10.977112307));
#222196=CARTESIAN_POINT('Ctrl Pts',(1.95703406199994,15.2,10.974299224));
#222197=CARTESIAN_POINT('Ctrl Pts',(1.95703406199994,11.6,10.974299224));
#222198=CARTESIAN_POINT('Ctrl Pts',(1.95527281699994,15.2,10.971488949));
#222199=CARTESIAN_POINT('Ctrl Pts',(1.95527281699994,11.6,10.971488949));
#222200=CARTESIAN_POINT('Ctrl Pts',(1.95351644999994,15.2,10.968681497));
#222201=CARTESIAN_POINT('Ctrl Pts',(1.95351644999994,11.6,10.968681497));
#222202=CARTESIAN_POINT('Ctrl Pts',(1.95176495899994,15.2,10.965876878));
#222203=CARTESIAN_POINT('Ctrl Pts',(1.95176495899994,11.6,10.965876878));
#222204=CARTESIAN_POINT('Ctrl Pts',(1.95001834399994,15.2,10.9630751));
#222205=CARTESIAN_POINT('Ctrl Pts',(1.95001834399994,11.6,10.9630751));
#222206=CARTESIAN_POINT('Ctrl Pts',(1.94827660299994,15.2,10.960276177));
#222207=CARTESIAN_POINT('Ctrl Pts',(1.94827660299994,11.6,10.960276177));
#222208=CARTESIAN_POINT('Ctrl Pts',(1.94653973299994,15.2,10.957480118));
#222209=CARTESIAN_POINT('Ctrl Pts',(1.94653973299994,11.6,10.957480118));
#222210=CARTESIAN_POINT('Ctrl Pts',(1.94480773699994,15.2,10.954686935));
#222211=CARTESIAN_POINT('Ctrl Pts',(1.94480773699994,11.6,10.954686935));
#222212=CARTESIAN_POINT('Ctrl Pts',(1.94308060999994,15.2,10.951896637));
#222213=CARTESIAN_POINT('Ctrl Pts',(1.94308060999994,11.6,10.951896637));
#222214=CARTESIAN_POINT('Ctrl Pts',(1.94135835199994,15.2,10.949109235));
#222215=CARTESIAN_POINT('Ctrl Pts',(1.94135835199994,11.6,10.949109235));
#222216=CARTESIAN_POINT('Ctrl Pts',(1.93964096199994,15.2,10.946324741));
#222217=CARTESIAN_POINT('Ctrl Pts',(1.93964096199994,11.6,10.946324741));
#222218=CARTESIAN_POINT('Ctrl Pts',(1.93792843899994,15.2,10.943543166));
#222219=CARTESIAN_POINT('Ctrl Pts',(1.93792843899994,11.6,10.943543166));
#222220=CARTESIAN_POINT('Ctrl Pts',(1.93622078099994,15.2,10.94076452));
#222221=CARTESIAN_POINT('Ctrl Pts',(1.93622078099994,11.6,10.94076452));
#222222=CARTESIAN_POINT('Ctrl Pts',(1.93451798599994,15.2,10.937988814));
#222223=CARTESIAN_POINT('Ctrl Pts',(1.93451798599994,11.6,10.937988814));
#222224=CARTESIAN_POINT('Ctrl Pts',(1.93282005399994,15.2,10.935216059));
#222225=CARTESIAN_POINT('Ctrl Pts',(1.93282005399994,11.6,10.935216059));
#222226=CARTESIAN_POINT('Ctrl Pts',(1.93112698299994,15.2,10.932446265));
#222227=CARTESIAN_POINT('Ctrl Pts',(1.93112698299994,11.6,10.932446265));
#222228=CARTESIAN_POINT('Ctrl Pts',(1.92943877199994,15.2,10.929679446));
#222229=CARTESIAN_POINT('Ctrl Pts',(1.92943877199994,11.6,10.929679446));
#222230=CARTESIAN_POINT('Ctrl Pts',(1.92775541899994,15.2,10.92691561));
#222231=CARTESIAN_POINT('Ctrl Pts',(1.92775541899994,11.6,10.92691561));
#222232=CARTESIAN_POINT('Ctrl Pts',(1.92607692399994,15.2,10.924154768));
#222233=CARTESIAN_POINT('Ctrl Pts',(1.92607692399994,11.6,10.924154768));
#222234=CARTESIAN_POINT('Ctrl Pts',(1.92440328299994,15.2,10.921396933));
#222235=CARTESIAN_POINT('Ctrl Pts',(1.92440328299994,11.6,10.921396933));
#222236=CARTESIAN_POINT('Ctrl Pts',(1.92273449799994,15.2,10.918642115));
#222237=CARTESIAN_POINT('Ctrl Pts',(1.92273449799994,11.6,10.918642115));
#222238=CARTESIAN_POINT('Ctrl Pts',(1.92107056499994,15.2,10.915890325));
#222239=CARTESIAN_POINT('Ctrl Pts',(1.92107056499994,11.6,10.915890325));
#222240=CARTESIAN_POINT('Ctrl Pts',(1.91941148399994,15.2,10.913141574));
#222241=CARTESIAN_POINT('Ctrl Pts',(1.91941148399994,11.6,10.913141574));
#222242=CARTESIAN_POINT('Ctrl Pts',(1.91775725299994,15.2,10.910395872));
#222243=CARTESIAN_POINT('Ctrl Pts',(1.91775725299994,11.6,10.910395872));
#222244=CARTESIAN_POINT('Ctrl Pts',(1.91610786999994,15.2,10.907653233));
#222245=CARTESIAN_POINT('Ctrl Pts',(1.91610786999994,11.6,10.907653233));
#222246=CARTESIAN_POINT('Ctrl Pts',(1.91446333499994,15.2,10.904913665));
#222247=CARTESIAN_POINT('Ctrl Pts',(1.91446333499994,11.6,10.904913665));
#222248=CARTESIAN_POINT('Ctrl Pts',(1.91282364499994,15.2,10.902177181));
#222249=CARTESIAN_POINT('Ctrl Pts',(1.91282364499994,11.6,10.902177181));
#222250=CARTESIAN_POINT('Ctrl Pts',(1.91118879899994,15.2,10.899443792));
#222251=CARTESIAN_POINT('Ctrl Pts',(1.91118879899994,11.6,10.899443792));
#222252=CARTESIAN_POINT('Ctrl Pts',(1.90955879599994,15.2,10.896713509));
#222253=CARTESIAN_POINT('Ctrl Pts',(1.90955879599994,11.6,10.896713509));
#222254=CARTESIAN_POINT('Ctrl Pts',(1.90793363299994,15.2,10.893986344));
#222255=CARTESIAN_POINT('Ctrl Pts',(1.90793363299994,11.6,10.893986344));
#222256=CARTESIAN_POINT('Ctrl Pts',(1.90631331099994,15.2,10.891262308));
#222257=CARTESIAN_POINT('Ctrl Pts',(1.90631331099994,11.6,10.891262308));
#222258=CARTESIAN_POINT('Ctrl Pts',(1.90469782699994,15.2,10.88854141));
#222259=CARTESIAN_POINT('Ctrl Pts',(1.90469782699994,11.6,10.88854141));
#222260=CARTESIAN_POINT('Ctrl Pts',(1.90308717899994,15.2,10.885823664));
#222261=CARTESIAN_POINT('Ctrl Pts',(1.90308717899994,11.6,10.885823664));
#222262=CARTESIAN_POINT('Ctrl Pts',(1.90148136699994,15.2,10.883109081));
#222263=CARTESIAN_POINT('Ctrl Pts',(1.90148136699994,11.6,10.883109081));
#222264=CARTESIAN_POINT('Ctrl Pts',(1.89988038799994,15.2,10.88039767));
#222265=CARTESIAN_POINT('Ctrl Pts',(1.89988038799994,11.6,10.88039767));
#222266=CARTESIAN_POINT('Ctrl Pts',(1.89828424099994,15.2,10.877689446));
#222267=CARTESIAN_POINT('Ctrl Pts',(1.89828424099994,11.6,10.877689446));
#222268=CARTESIAN_POINT('Ctrl Pts',(1.89669292499994,15.2,10.874984418));
#222269=CARTESIAN_POINT('Ctrl Pts',(1.89669292499994,11.6,10.874984418));
#222270=CARTESIAN_POINT('Ctrl Pts',(1.89510643699994,15.2,10.872282598));
#222271=CARTESIAN_POINT('Ctrl Pts',(1.89510643699994,11.6,10.872282598));
#222272=CARTESIAN_POINT('Ctrl Pts',(1.89352477599994,15.2,10.869583997));
#222273=CARTESIAN_POINT('Ctrl Pts',(1.89352477599994,11.6,10.869583997));
#222274=CARTESIAN_POINT('Ctrl Pts',(1.89194794099994,15.2,10.866888628));
#222275=CARTESIAN_POINT('Ctrl Pts',(1.89194794099994,11.6,10.866888628));
#222276=CARTESIAN_POINT('Ctrl Pts',(1.89037592899994,15.2,10.8641965));
#222277=CARTESIAN_POINT('Ctrl Pts',(1.89037592899994,11.6,10.8641965));
#222278=CARTESIAN_POINT('Ctrl Pts',(1.88880873999994,15.2,10.861507627));
#222279=CARTESIAN_POINT('Ctrl Pts',(1.88880873999994,11.6,10.861507627));
#222280=CARTESIAN_POINT('Ctrl Pts',(1.88724637099994,15.2,10.858822018));
#222281=CARTESIAN_POINT('Ctrl Pts',(1.88724637099994,11.6,10.858822018));
#222282=CARTESIAN_POINT('Ctrl Pts',(1.88568882099994,15.2,10.856139687));
#222283=CARTESIAN_POINT('Ctrl Pts',(1.88568882099994,11.6,10.856139687));
#222284=CARTESIAN_POINT('Ctrl Pts',(1.88413608799994,15.2,10.853460645));
#222285=CARTESIAN_POINT('Ctrl Pts',(1.88413608799994,11.6,10.853460645));
#222286=CARTESIAN_POINT('Ctrl Pts',(1.88258817099994,15.2,10.850784902));
#222287=CARTESIAN_POINT('Ctrl Pts',(1.88258817099994,11.6,10.850784902));
#222288=CARTESIAN_POINT('Ctrl Pts',(1.88104506799994,15.2,10.848112472));
#222289=CARTESIAN_POINT('Ctrl Pts',(1.88104506799994,11.6,10.848112472));
#222290=CARTESIAN_POINT('Ctrl Pts',(1.87950677599994,15.2,10.845443365));
#222291=CARTESIAN_POINT('Ctrl Pts',(1.87950677599994,11.6,10.845443365));
#222292=CARTESIAN_POINT('Ctrl Pts',(1.87797329499995,15.2,10.842777593));
#222293=CARTESIAN_POINT('Ctrl Pts',(1.87797329499995,11.6,10.842777593));
#222294=CARTESIAN_POINT('Ctrl Pts',(1.87644462199994,15.2,10.840115168));
#222295=CARTESIAN_POINT('Ctrl Pts',(1.87644462199994,11.6,10.840115168));
#222296=CARTESIAN_POINT('Ctrl Pts',(1.87492075599994,15.2,10.837456102));
#222297=CARTESIAN_POINT('Ctrl Pts',(1.87492075599994,11.6,10.837456102));
#222298=CARTESIAN_POINT('Ctrl Pts',(1.87340169499994,15.2,10.834800405));
#222299=CARTESIAN_POINT('Ctrl Pts',(1.87340169499994,11.6,10.834800405));
#222300=CARTESIAN_POINT('Ctrl Pts',(1.87188743799994,15.2,10.832148092));
#222301=CARTESIAN_POINT('Ctrl Pts',(1.87188743799994,11.6,10.832148092));
#222302=CARTESIAN_POINT('Ctrl Pts',(1.87037798199994,15.2,10.829499171));
#222303=CARTESIAN_POINT('Ctrl Pts',(1.87037798199994,11.6,10.829499171));
#222304=CARTESIAN_POINT('Ctrl Pts',(1.86887332499994,15.2,10.826853657));
#222305=CARTESIAN_POINT('Ctrl Pts',(1.86887332499994,11.6,10.826853657));
#222306=CARTESIAN_POINT('Ctrl Pts',(1.86737346599994,15.2,10.82421156));
#222307=CARTESIAN_POINT('Ctrl Pts',(1.86737346599994,11.6,10.82421156));
#222308=CARTESIAN_POINT('Ctrl Pts',(1.86587840299994,15.2,10.821572892));
#222309=CARTESIAN_POINT('Ctrl Pts',(1.86587840299994,11.6,10.821572892));
#222310=CARTESIAN_POINT('Ctrl Pts',(1.86438813399994,15.2,10.818937667));
#222311=CARTESIAN_POINT('Ctrl Pts',(1.86438813399994,11.6,10.818937667));
#222312=CARTESIAN_POINT('Ctrl Pts',(1.86290265699994,15.2,10.816305893));
#222313=CARTESIAN_POINT('Ctrl Pts',(1.86290265699994,11.6,10.816305893));
#222314=CARTESIAN_POINT('Ctrl Pts',(1.86142197099994,15.2,10.813677587));
#222315=CARTESIAN_POINT('Ctrl Pts',(1.86142197099994,11.6,10.813677587));
#222316=CARTESIAN_POINT('Ctrl Pts',(1.85994607299994,15.2,10.811052756));
#222317=CARTESIAN_POINT('Ctrl Pts',(1.85994607299994,11.6,10.811052756));
#222318=CARTESIAN_POINT('Ctrl Pts',(1.85847496099994,15.2,10.808431415));
#222319=CARTESIAN_POINT('Ctrl Pts',(1.85847496099994,11.6,10.808431415));
#222320=CARTESIAN_POINT('Ctrl Pts',(1.85700863399994,15.2,10.805813575));
#222321=CARTESIAN_POINT('Ctrl Pts',(1.85700863399994,11.6,10.805813575));
#222322=CARTESIAN_POINT('Ctrl Pts',(1.85554708999994,15.2,10.803199249));
#222323=CARTESIAN_POINT('Ctrl Pts',(1.85554708999994,11.6,10.803199249));
#222324=CARTESIAN_POINT('Ctrl Pts',(1.85409032699994,15.2,10.800588447));
#222325=CARTESIAN_POINT('Ctrl Pts',(1.85409032699994,11.6,10.800588447));
#222326=CARTESIAN_POINT('Ctrl Pts',(1.85263834199994,15.2,10.797981184));
#222327=CARTESIAN_POINT('Ctrl Pts',(1.85263834199994,11.6,10.797981184));
#222328=CARTESIAN_POINT('Ctrl Pts',(1.85119113399994,15.2,10.79537747));
#222329=CARTESIAN_POINT('Ctrl Pts',(1.85119113399994,11.6,10.79537747));
#222330=CARTESIAN_POINT('Ctrl Pts',(1.84974869999994,15.2,10.792777317));
#222331=CARTESIAN_POINT('Ctrl Pts',(1.84974869999994,11.6,10.792777317));
#222332=CARTESIAN_POINT('Ctrl Pts',(1.84831103999994,15.2,10.790180739));
#222333=CARTESIAN_POINT('Ctrl Pts',(1.84831103999994,11.6,10.790180739));
#222334=CARTESIAN_POINT('Ctrl Pts',(1.84687814999994,15.2,10.787587747));
#222335=CARTESIAN_POINT('Ctrl Pts',(1.84687814999994,11.6,10.787587747));
#222336=CARTESIAN_POINT('Ctrl Pts',(1.84545002899994,15.2,10.784998353));
#222337=CARTESIAN_POINT('Ctrl Pts',(1.84545002899994,11.6,10.784998353));
#222338=CARTESIAN_POINT('Ctrl Pts',(1.84402667499994,15.2,10.78241257));
#222339=CARTESIAN_POINT('Ctrl Pts',(1.84402667499994,11.6,10.78241257));
#222340=CARTESIAN_POINT('Ctrl Pts',(1.84260808499994,15.2,10.77983041));
#222341=CARTESIAN_POINT('Ctrl Pts',(1.84260808499994,11.6,10.77983041));
#222342=CARTESIAN_POINT('Ctrl Pts',(1.84119425799994,15.2,10.777251886));
#222343=CARTESIAN_POINT('Ctrl Pts',(1.84119425799994,11.6,10.777251886));
#222344=CARTESIAN_POINT('Ctrl Pts',(1.83978518999994,15.2,10.774677008));
#222345=CARTESIAN_POINT('Ctrl Pts',(1.83978518999994,11.6,10.774677008));
#222346=CARTESIAN_POINT('Ctrl Pts',(1.83838088199994,15.2,10.772105791));
#222347=CARTESIAN_POINT('Ctrl Pts',(1.83838088199994,11.6,10.772105791));
#222348=CARTESIAN_POINT('Ctrl Pts',(1.83698132999994,15.2,10.769538246));
#222349=CARTESIAN_POINT('Ctrl Pts',(1.83698132999994,11.6,10.769538246));
#222350=CARTESIAN_POINT('Ctrl Pts',(1.83558653199994,15.2,10.766974385));
#222351=CARTESIAN_POINT('Ctrl Pts',(1.83558653199994,11.6,10.766974385));
#222352=CARTESIAN_POINT('Ctrl Pts',(1.83419648599994,15.2,10.764414223));
#222353=CARTESIAN_POINT('Ctrl Pts',(1.83419648599994,11.6,10.764414223));
#222354=CARTESIAN_POINT('Ctrl Pts',(1.83281118899994,15.2,10.761857769));
#222355=CARTESIAN_POINT('Ctrl Pts',(1.83281118899994,11.6,10.761857769));
#222356=CARTESIAN_POINT('Ctrl Pts',(1.83143063899994,15.2,10.759305039));
#222357=CARTESIAN_POINT('Ctrl Pts',(1.83143063899994,11.6,10.759305039));
#222358=CARTESIAN_POINT('Ctrl Pts',(1.83005483599994,15.2,10.756756044));
#222359=CARTESIAN_POINT('Ctrl Pts',(1.83005483599994,11.6,10.756756044));
#222360=CARTESIAN_POINT('Ctrl Pts',(1.82868377599994,15.2,10.754210794));
#222361=CARTESIAN_POINT('Ctrl Pts',(1.82868377599994,11.6,10.754210794));
#222362=CARTESIAN_POINT('Ctrl Pts',(1.82731745699994,15.2,10.751669306));
#222363=CARTESIAN_POINT('Ctrl Pts',(1.82731745699994,11.6,10.751669306));
#222364=CARTESIAN_POINT('Ctrl Pts',(1.82595587499994,15.2,10.74913159));
#222365=CARTESIAN_POINT('Ctrl Pts',(1.82595587499994,11.6,10.74913159));
#222366=CARTESIAN_POINT('Ctrl Pts',(1.82459903099994,15.2,10.746597659));
#222367=CARTESIAN_POINT('Ctrl Pts',(1.82459903099994,11.6,10.746597659));
#222368=CARTESIAN_POINT('Ctrl Pts',(1.82324692099994,15.2,10.744067525));
#222369=CARTESIAN_POINT('Ctrl Pts',(1.82324692099994,11.6,10.744067525));
#222370=CARTESIAN_POINT('Ctrl Pts',(1.82189954399994,15.2,10.741541203));
#222371=CARTESIAN_POINT('Ctrl Pts',(1.82189954399994,11.6,10.741541203));
#222372=CARTESIAN_POINT('Ctrl Pts',(1.82055689499994,15.2,10.739018704));
#222373=CARTESIAN_POINT('Ctrl Pts',(1.82055689499994,11.6,10.739018704));
#222374=CARTESIAN_POINT('Ctrl Pts',(1.81921897399994,15.2,10.736500041));
#222375=CARTESIAN_POINT('Ctrl Pts',(1.81921897399994,11.6,10.736500041));
#222376=CARTESIAN_POINT('Ctrl Pts',(1.81788577799994,15.2,10.733985226));
#222377=CARTESIAN_POINT('Ctrl Pts',(1.81788577799994,11.6,10.733985226));
#222378=CARTESIAN_POINT('Ctrl Pts',(1.81655730499994,15.2,10.731474274));
#222379=CARTESIAN_POINT('Ctrl Pts',(1.81655730499994,11.6,10.731474274));
#222380=CARTESIAN_POINT('Ctrl Pts',(1.81523355199994,15.2,10.728967196));
#222381=CARTESIAN_POINT('Ctrl Pts',(1.81523355199994,11.6,10.728967196));
#222382=CARTESIAN_POINT('Ctrl Pts',(1.81391451699994,15.2,10.726464006));
#222383=CARTESIAN_POINT('Ctrl Pts',(1.81391451699994,11.6,10.726464006));
#222384=CARTESIAN_POINT('Ctrl Pts',(1.81260019699994,15.2,10.723964716));
#222385=CARTESIAN_POINT('Ctrl Pts',(1.81260019699994,11.6,10.723964716));
#222386=CARTESIAN_POINT('Ctrl Pts',(1.81129059099994,15.2,10.721469338));
#222387=CARTESIAN_POINT('Ctrl Pts',(1.81129059099994,11.6,10.721469338));
#222388=CARTESIAN_POINT('Ctrl Pts',(1.80998569499994,15.2,10.718977888));
#222389=CARTESIAN_POINT('Ctrl Pts',(1.80998569499994,11.6,10.718977888));
#222390=CARTESIAN_POINT('Ctrl Pts',(1.80868550699994,15.2,10.716490376));
#222391=CARTESIAN_POINT('Ctrl Pts',(1.80868550699994,11.6,10.716490376));
#222392=CARTESIAN_POINT('Ctrl Pts',(1.80739002699994,15.2,10.714006816));
#222393=CARTESIAN_POINT('Ctrl Pts',(1.80739002699994,11.6,10.714006816));
#222394=CARTESIAN_POINT('Ctrl Pts',(1.80609924799994,15.2,10.711527222));
#222395=CARTESIAN_POINT('Ctrl Pts',(1.80609924799994,11.6,10.711527222));
#222396=CARTESIAN_POINT('Ctrl Pts',(1.80481317199994,15.2,10.709051607));
#222397=CARTESIAN_POINT('Ctrl Pts',(1.80481317199994,11.6,10.709051607));
#222398=CARTESIAN_POINT('Ctrl Pts',(1.80353179199994,15.2,10.706579983));
#222399=CARTESIAN_POINT('Ctrl Pts',(1.80353179199994,11.6,10.706579983));
#222400=CARTESIAN_POINT('Ctrl Pts',(1.80225510999994,15.2,10.704112364));
#222401=CARTESIAN_POINT('Ctrl Pts',(1.80225510999994,11.6,10.704112364));
#222402=CARTESIAN_POINT('Ctrl Pts',(1.80098311999994,15.2,10.701648763));
#222403=CARTESIAN_POINT('Ctrl Pts',(1.80098311999994,11.6,10.701648763));
#222404=CARTESIAN_POINT('Ctrl Pts',(1.79971582199994,15.2,10.699189192));
#222405=CARTESIAN_POINT('Ctrl Pts',(1.79971582199994,11.6,10.699189192));
#222406=CARTESIAN_POINT('Ctrl Pts',(1.79845321199994,15.2,10.696733665));
#222407=CARTESIAN_POINT('Ctrl Pts',(1.79845321199994,11.6,10.696733665));
#222408=CARTESIAN_POINT('Ctrl Pts',(1.79719528699994,15.2,10.694282197));
#222409=CARTESIAN_POINT('Ctrl Pts',(1.79719528699994,11.6,10.694282197));
#222410=CARTESIAN_POINT('Ctrl Pts',(1.79594204599994,15.2,10.691834799));
#222411=CARTESIAN_POINT('Ctrl Pts',(1.79594204599994,11.6,10.691834799));
#222412=CARTESIAN_POINT('Ctrl Pts',(1.79469348599994,15.2,10.689391486));
#222413=CARTESIAN_POINT('Ctrl Pts',(1.79469348599994,11.6,10.689391486));
#222414=CARTESIAN_POINT('Ctrl Pts',(1.79344960199994,15.2,10.68695227));
#222415=CARTESIAN_POINT('Ctrl Pts',(1.79344960199994,11.6,10.68695227));
#222416=CARTESIAN_POINT('Ctrl Pts',(1.79221039399994,15.2,10.684517164));
#222417=CARTESIAN_POINT('Ctrl Pts',(1.79221039399994,11.6,10.684517164));
#222418=CARTESIAN_POINT('Ctrl Pts',(1.79097585899994,15.2,10.682086184));
#222419=CARTESIAN_POINT('Ctrl Pts',(1.79097585899994,11.6,10.682086184));
#222420=CARTESIAN_POINT('Ctrl Pts',(1.78974599399994,15.2,10.679659341));
#222421=CARTESIAN_POINT('Ctrl Pts',(1.78974599399994,11.6,10.679659341));
#222422=CARTESIAN_POINT('Ctrl Pts',(1.78852079599994,15.2,10.677236649));
#222423=CARTESIAN_POINT('Ctrl Pts',(1.78852079599994,11.6,10.677236649));
#222424=CARTESIAN_POINT('Ctrl Pts',(1.78730026299994,15.2,10.674818122));
#222425=CARTESIAN_POINT('Ctrl Pts',(1.78730026299994,11.6,10.674818122));
#222426=CARTESIAN_POINT('Ctrl Pts',(1.78608439099994,15.2,10.672403774));
#222427=CARTESIAN_POINT('Ctrl Pts',(1.78608439099994,11.6,10.672403774));
#222428=CARTESIAN_POINT('Ctrl Pts',(1.78487317799994,15.2,10.669993618));
#222429=CARTESIAN_POINT('Ctrl Pts',(1.78487317799994,11.6,10.669993618));
#222430=CARTESIAN_POINT('Ctrl Pts',(1.78366662199994,15.2,10.667587667));
#222431=CARTESIAN_POINT('Ctrl Pts',(1.78366662199994,11.6,10.667587667));
#222432=CARTESIAN_POINT('Ctrl Pts',(1.78246471799994,15.2,10.665185936));
#222433=CARTESIAN_POINT('Ctrl Pts',(1.78246471799994,11.6,10.665185936));
#222434=CARTESIAN_POINT('Ctrl Pts',(1.78126746699994,15.2,10.662788437));
#222435=CARTESIAN_POINT('Ctrl Pts',(1.78126746699994,11.6,10.662788437));
#222436=CARTESIAN_POINT('Ctrl Pts',(1.78007486299994,15.2,10.660395185));
#222437=CARTESIAN_POINT('Ctrl Pts',(1.78007486299994,11.6,10.660395185));
#222438=CARTESIAN_POINT('Ctrl Pts',(1.77888690299994,15.2,10.658006193));
#222439=CARTESIAN_POINT('Ctrl Pts',(1.77888690299994,11.6,10.658006193));
#222440=CARTESIAN_POINT('Ctrl Pts',(1.77770358699994,15.2,10.655621476));
#222441=CARTESIAN_POINT('Ctrl Pts',(1.77770358699994,11.6,10.655621476));
#222442=CARTESIAN_POINT('Ctrl Pts',(1.77652490899994,15.2,10.653241047));
#222443=CARTESIAN_POINT('Ctrl Pts',(1.77652490899994,11.6,10.653241047));
#222444=CARTESIAN_POINT('Ctrl Pts',(1.77535086799994,15.2,10.650864921));
#222445=CARTESIAN_POINT('Ctrl Pts',(1.77535086799994,11.6,10.650864921));
#222446=CARTESIAN_POINT('Ctrl Pts',(1.77418146099994,15.2,10.648493109));
#222447=CARTESIAN_POINT('Ctrl Pts',(1.77418146099994,11.6,10.648493109));
#222448=CARTESIAN_POINT('Ctrl Pts',(1.77301668399994,15.2,10.646125627));
#222449=CARTESIAN_POINT('Ctrl Pts',(1.77301668399994,11.6,10.646125627));
#222450=CARTESIAN_POINT('Ctrl Pts',(1.77185653499994,15.2,10.643762489));
#222451=CARTESIAN_POINT('Ctrl Pts',(1.77185653499994,11.6,10.643762489));
#222452=CARTESIAN_POINT('Ctrl Pts',(1.77070101099994,15.2,10.641403709));
#222453=CARTESIAN_POINT('Ctrl Pts',(1.77070101099994,11.6,10.641403709));
#222454=CARTESIAN_POINT('Ctrl Pts',(1.76955010899994,15.2,10.6390493));
#222455=CARTESIAN_POINT('Ctrl Pts',(1.76955010899994,11.6,10.6390493));
#222456=CARTESIAN_POINT('Ctrl Pts',(1.76840382499994,15.2,10.636699276));
#222457=CARTESIAN_POINT('Ctrl Pts',(1.76840382499994,11.6,10.636699276));
#222458=CARTESIAN_POINT('Ctrl Pts',(1.76726215699994,15.2,10.634353653));
#222459=CARTESIAN_POINT('Ctrl Pts',(1.76726215699994,11.6,10.634353653));
#222460=CARTESIAN_POINT('Ctrl Pts',(1.76612510299994,15.2,10.632012444));
#222461=CARTESIAN_POINT('Ctrl Pts',(1.76612510299994,11.6,10.632012444));
#222462=CARTESIAN_POINT('Ctrl Pts',(1.76499265799994,15.2,10.629675662));
#222463=CARTESIAN_POINT('Ctrl Pts',(1.76499265799994,11.6,10.629675662));
#222464=CARTESIAN_POINT('Ctrl Pts',(1.76386481999994,15.2,10.627343324));
#222465=CARTESIAN_POINT('Ctrl Pts',(1.76386481999994,11.6,10.627343324));
#222466=CARTESIAN_POINT('Ctrl Pts',(1.76274158499994,15.2,10.625015441));
#222467=CARTESIAN_POINT('Ctrl Pts',(1.76274158499994,11.6,10.625015441));
#222468=CARTESIAN_POINT('Ctrl Pts',(1.76162295199994,15.2,10.62269203));
#222469=CARTESIAN_POINT('Ctrl Pts',(1.76162295199994,11.6,10.62269203));
#222470=CARTESIAN_POINT('Ctrl Pts',(1.76050891399994,15.2,10.620373104));
#222471=CARTESIAN_POINT('Ctrl Pts',(1.76050891399994,11.6,10.620373104));
#222472=CARTESIAN_POINT('Ctrl Pts',(1.75939947199994,15.2,10.618058677));
#222473=CARTESIAN_POINT('Ctrl Pts',(1.75939947199994,11.6,10.618058677));
#222474=CARTESIAN_POINT('Ctrl Pts',(1.75829462199994,15.2,10.615748764));
#222475=CARTESIAN_POINT('Ctrl Pts',(1.75829462199994,11.6,10.615748764));
#222476=CARTESIAN_POINT('Ctrl Pts',(1.75719435899994,15.2,10.61344338));
#222477=CARTESIAN_POINT('Ctrl Pts',(1.75719435899994,11.6,10.61344338));
#222478=CARTESIAN_POINT('Ctrl Pts',(1.75609867999994,15.2,10.611142538));
#222479=CARTESIAN_POINT('Ctrl Pts',(1.75609867999994,11.6,10.611142538));
#222480=CARTESIAN_POINT('Ctrl Pts',(1.75500758399994,15.2,10.608846253));
#222481=CARTESIAN_POINT('Ctrl Pts',(1.75500758399994,11.6,10.608846253));
#222482=CARTESIAN_POINT('Ctrl Pts',(1.75392106599994,15.2,10.606554541));
#222483=CARTESIAN_POINT('Ctrl Pts',(1.75392106599994,11.6,10.606554541));
#222484=CARTESIAN_POINT('Ctrl Pts',(1.75283912199994,15.2,10.604267413));
#222485=CARTESIAN_POINT('Ctrl Pts',(1.75283912199994,11.6,10.604267413));
#222486=CARTESIAN_POINT('Ctrl Pts',(1.75176175099994,15.2,10.601984888));
#222487=CARTESIAN_POINT('Ctrl Pts',(1.75176175099994,11.6,10.601984888));
#222488=CARTESIAN_POINT('Ctrl Pts',(1.75068894799994,15.2,10.599706978));
#222489=CARTESIAN_POINT('Ctrl Pts',(1.75068894799994,11.6,10.599706978));
#222490=CARTESIAN_POINT('Ctrl Pts',(1.74962071199994,15.2,10.597433698));
#222491=CARTESIAN_POINT('Ctrl Pts',(1.74962071199994,11.6,10.597433698));
#222492=CARTESIAN_POINT('Ctrl Pts',(1.74855703599994,15.2,10.595165063));
#222493=CARTESIAN_POINT('Ctrl Pts',(1.74855703599994,11.6,10.595165063));
#222494=CARTESIAN_POINT('Ctrl Pts',(1.74749791799994,15.2,10.592901088));
#222495=CARTESIAN_POINT('Ctrl Pts',(1.74749791799994,11.6,10.592901088));
#222496=CARTESIAN_POINT('Ctrl Pts',(1.74644335699994,15.2,10.590641787));
#222497=CARTESIAN_POINT('Ctrl Pts',(1.74644335699994,11.6,10.590641787));
#222498=CARTESIAN_POINT('Ctrl Pts',(1.74539334699994,15.2,10.588387175));
#222499=CARTESIAN_POINT('Ctrl Pts',(1.74539334699994,11.6,10.588387175));
#222500=CARTESIAN_POINT('Ctrl Pts',(1.74434788599994,15.2,10.586137268));
#222501=CARTESIAN_POINT('Ctrl Pts',(1.74434788599994,11.6,10.586137268));
#222502=CARTESIAN_POINT('Ctrl Pts',(1.74330696999994,15.2,10.583892079));
#222503=CARTESIAN_POINT('Ctrl Pts',(1.74330696999994,11.6,10.583892079));
#222504=CARTESIAN_POINT('Ctrl Pts',(1.74227059499994,15.2,10.581651625));
#222505=CARTESIAN_POINT('Ctrl Pts',(1.74227059499994,11.6,10.581651625));
#222506=CARTESIAN_POINT('Ctrl Pts',(1.74123875899994,15.2,10.57941592));
#222507=CARTESIAN_POINT('Ctrl Pts',(1.74123875899994,11.6,10.57941592));
#222508=CARTESIAN_POINT('Ctrl Pts',(1.74021145699994,15.2,10.577184979));
#222509=CARTESIAN_POINT('Ctrl Pts',(1.74021145699994,11.6,10.577184979));
#222510=CARTESIAN_POINT('Ctrl Pts',(1.73918868599995,15.2,10.574958817));
#222511=CARTESIAN_POINT('Ctrl Pts',(1.73918868599995,11.6,10.574958817));
#222512=CARTESIAN_POINT('Ctrl Pts',(1.73817044299994,15.2,10.572737449));
#222513=CARTESIAN_POINT('Ctrl Pts',(1.73817044299994,11.6,10.572737449));
#222514=CARTESIAN_POINT('Ctrl Pts',(1.73715672399994,15.2,10.570520891));
#222515=CARTESIAN_POINT('Ctrl Pts',(1.73715672399994,11.6,10.570520891));
#222516=CARTESIAN_POINT('Ctrl Pts',(1.73614752599994,15.2,10.568309157));
#222517=CARTESIAN_POINT('Ctrl Pts',(1.73614752599994,11.6,10.568309157));
#222518=CARTESIAN_POINT('Ctrl Pts',(1.73514284399995,15.2,10.566102263));
#222519=CARTESIAN_POINT('Ctrl Pts',(1.73514284399995,11.6,10.566102263));
#222520=CARTESIAN_POINT('Ctrl Pts',(1.73414267599994,15.2,10.563900224));
#222521=CARTESIAN_POINT('Ctrl Pts',(1.73414267599994,11.6,10.563900224));
#222522=CARTESIAN_POINT('Ctrl Pts',(1.73314701799994,15.2,10.561703055));
#222523=CARTESIAN_POINT('Ctrl Pts',(1.73314701799994,11.6,10.561703055));
#222524=CARTESIAN_POINT('Ctrl Pts',(1.73215586599994,15.2,10.559510772));
#222525=CARTESIAN_POINT('Ctrl Pts',(1.73215586599994,11.6,10.559510772));
#222526=CARTESIAN_POINT('Ctrl Pts',(1.73116921499994,15.2,10.557323391));
#222527=CARTESIAN_POINT('Ctrl Pts',(1.73116921499994,11.6,10.557323391));
#222528=CARTESIAN_POINT('Ctrl Pts',(1.73018706399994,15.2,10.555140925));
#222529=CARTESIAN_POINT('Ctrl Pts',(1.73018706399994,11.6,10.555140925));
#222530=CARTESIAN_POINT('Ctrl Pts',(1.72920940799994,15.2,10.552963392));
#222531=CARTESIAN_POINT('Ctrl Pts',(1.72920940799994,11.6,10.552963392));
#222532=CARTESIAN_POINT('Ctrl Pts',(1.72823624299994,15.2,10.550790806));
#222533=CARTESIAN_POINT('Ctrl Pts',(1.72823624299994,11.6,10.550790806));
#222534=CARTESIAN_POINT('Ctrl Pts',(1.72726756499994,15.2,10.548623183));
#222535=CARTESIAN_POINT('Ctrl Pts',(1.72726756499994,11.6,10.548623183));
#222536=CARTESIAN_POINT('Ctrl Pts',(1.72630337199994,15.2,10.546460539));
#222537=CARTESIAN_POINT('Ctrl Pts',(1.72630337199994,11.6,10.546460539));
#222538=CARTESIAN_POINT('Ctrl Pts',(1.72534365799994,15.2,10.544302888));
#222539=CARTESIAN_POINT('Ctrl Pts',(1.72534365799994,11.6,10.544302888));
#222540=CARTESIAN_POINT('Ctrl Pts',(1.72438841999994,15.2,10.542150249));
#222541=CARTESIAN_POINT('Ctrl Pts',(1.72438841999994,11.6,10.542150249));
#222542=CARTESIAN_POINT('Ctrl Pts',(1.72343765399994,15.2,10.540002635));
#222543=CARTESIAN_POINT('Ctrl Pts',(1.72343765399994,11.6,10.540002635));
#222544=CARTESIAN_POINT('Ctrl Pts',(1.72249135799994,15.2,10.537860062));
#222545=CARTESIAN_POINT('Ctrl Pts',(1.72249135799994,11.6,10.537860062));
#222546=CARTESIAN_POINT('Ctrl Pts',(1.72154952499994,15.2,10.535722546));
#222547=CARTESIAN_POINT('Ctrl Pts',(1.72154952499994,11.6,10.535722546));
#222548=CARTESIAN_POINT('Ctrl Pts',(1.72061215299994,15.2,10.533590105));
#222549=CARTESIAN_POINT('Ctrl Pts',(1.72061215299994,11.6,10.533590105));
#222550=CARTESIAN_POINT('Ctrl Pts',(1.71967923699994,15.2,10.531462751));
#222551=CARTESIAN_POINT('Ctrl Pts',(1.71967923699994,11.6,10.531462751));
#222552=CARTESIAN_POINT('Ctrl Pts',(1.71875077499994,15.2,10.529340503));
#222553=CARTESIAN_POINT('Ctrl Pts',(1.71875077499994,11.6,10.529340503));
#222554=CARTESIAN_POINT('Ctrl Pts',(1.71782676099994,15.2,10.527223377));
#222555=CARTESIAN_POINT('Ctrl Pts',(1.71782676099994,11.6,10.527223377));
#222556=CARTESIAN_POINT('Ctrl Pts',(1.71690719199994,15.2,10.525111386));
#222557=CARTESIAN_POINT('Ctrl Pts',(1.71690719199994,11.6,10.525111386));
#222558=CARTESIAN_POINT('Ctrl Pts',(1.71599206399994,15.2,10.52300455));
#222559=CARTESIAN_POINT('Ctrl Pts',(1.71599206399994,11.6,10.52300455));
#222560=CARTESIAN_POINT('Ctrl Pts',(1.71508137199994,15.2,10.520902882));
#222561=CARTESIAN_POINT('Ctrl Pts',(1.71508137199994,11.6,10.520902882));
#222562=CARTESIAN_POINT('Ctrl Pts',(1.71417511299994,15.2,10.5188064));
#222563=CARTESIAN_POINT('Ctrl Pts',(1.71417511299994,11.6,10.5188064));
#222564=CARTESIAN_POINT('Ctrl Pts',(1.71327328299994,15.2,10.516715119));
#222565=CARTESIAN_POINT('Ctrl Pts',(1.71327328299994,11.6,10.516715119));
#222566=CARTESIAN_POINT('Ctrl Pts',(1.71237587599994,15.2,10.514629057));
#222567=CARTESIAN_POINT('Ctrl Pts',(1.71237587599994,11.6,10.514629057));
#222568=CARTESIAN_POINT('Ctrl Pts',(1.71148289099994,15.2,10.512548229));
#222569=CARTESIAN_POINT('Ctrl Pts',(1.71148289099994,11.6,10.512548229));
#222570=CARTESIAN_POINT('Ctrl Pts',(1.71059432099994,15.2,10.51047265));
#222571=CARTESIAN_POINT('Ctrl Pts',(1.71059432099994,11.6,10.51047265));
#222572=CARTESIAN_POINT('Ctrl Pts',(1.70971016399994,15.2,10.50840234));
#222573=CARTESIAN_POINT('Ctrl Pts',(1.70971016399994,11.6,10.50840234));
#222574=CARTESIAN_POINT('Ctrl Pts',(1.70883041399994,15.2,10.506337312));
#222575=CARTESIAN_POINT('Ctrl Pts',(1.70883041399994,11.6,10.506337312));
#222576=CARTESIAN_POINT('Ctrl Pts',(1.70795506799994,15.2,10.504277585));
#222577=CARTESIAN_POINT('Ctrl Pts',(1.70795506799994,11.6,10.504277585));
#222578=CARTESIAN_POINT('Ctrl Pts',(1.70708411999994,15.2,10.502223173));
#222579=CARTESIAN_POINT('Ctrl Pts',(1.70708411999994,11.6,10.502223173));
#222580=CARTESIAN_POINT('Ctrl Pts',(1.70621756899994,15.2,10.500174096));
#222581=CARTESIAN_POINT('Ctrl Pts',(1.70621756899994,11.6,10.500174096));
#222582=CARTESIAN_POINT('Ctrl Pts',(1.70535540699994,15.2,10.498130368));
#222583=CARTESIAN_POINT('Ctrl Pts',(1.70535540699994,11.6,10.498130368));
#222584=CARTESIAN_POINT('Ctrl Pts',(1.70449763199994,15.2,10.496092007));
#222585=CARTESIAN_POINT('Ctrl Pts',(1.70449763199994,11.6,10.496092007));
#222586=CARTESIAN_POINT('Ctrl Pts',(1.70364423799994,15.2,10.494059028));
#222587=CARTESIAN_POINT('Ctrl Pts',(1.70364423799994,11.6,10.494059028));
#222588=CARTESIAN_POINT('Ctrl Pts',(1.70279522299994,15.2,10.492031449));
#222589=CARTESIAN_POINT('Ctrl Pts',(1.70279522299994,11.6,10.492031449));
#222590=CARTESIAN_POINT('Ctrl Pts',(1.70195057999994,15.2,10.490009287));
#222591=CARTESIAN_POINT('Ctrl Pts',(1.70195057999994,11.6,10.490009287));
#222592=CARTESIAN_POINT('Ctrl Pts',(1.70111030699994,15.2,10.487992559));
#222593=CARTESIAN_POINT('Ctrl Pts',(1.70111030699994,11.6,10.487992559));
#222594=CARTESIAN_POINT('Ctrl Pts',(1.70027439799994,15.2,10.485981282));
#222595=CARTESIAN_POINT('Ctrl Pts',(1.70027439799994,11.6,10.485981282));
#222596=CARTESIAN_POINT('Ctrl Pts',(1.69944284799994,15.2,10.483975472));
#222597=CARTESIAN_POINT('Ctrl Pts',(1.69944284799994,11.6,10.483975472));
#222598=CARTESIAN_POINT('Ctrl Pts',(1.69861565399994,15.2,10.481975147));
#222599=CARTESIAN_POINT('Ctrl Pts',(1.69861565399994,11.6,10.481975147));
#222600=CARTESIAN_POINT('Ctrl Pts',(1.69779281099994,15.2,10.479980323));
#222601=CARTESIAN_POINT('Ctrl Pts',(1.69779281099994,11.6,10.479980323));
#222602=CARTESIAN_POINT('Ctrl Pts',(1.69697431399994,15.2,10.477991018));
#222603=CARTESIAN_POINT('Ctrl Pts',(1.69697431399994,11.6,10.477991018));
#222604=CARTESIAN_POINT('Ctrl Pts',(1.69616015899994,15.2,10.47600725));
#222605=CARTESIAN_POINT('Ctrl Pts',(1.69616015899994,11.6,10.47600725));
#222606=CARTESIAN_POINT('Ctrl Pts',(1.69535033999994,15.2,10.474029035));
#222607=CARTESIAN_POINT('Ctrl Pts',(1.69535033999994,11.6,10.474029035));
#222608=CARTESIAN_POINT('Ctrl Pts',(1.69454485499994,15.2,10.472056389));
#222609=CARTESIAN_POINT('Ctrl Pts',(1.69454485499994,11.6,10.472056389));
#222610=CARTESIAN_POINT('Ctrl Pts',(1.69374369599994,15.2,10.470089333));
#222611=CARTESIAN_POINT('Ctrl Pts',(1.69374369599994,11.6,10.470089333));
#222612=CARTESIAN_POINT('Ctrl Pts',(1.69294686199994,15.2,10.468127882));
#222613=CARTESIAN_POINT('Ctrl Pts',(1.69294686199994,11.6,10.468127882));
#222614=CARTESIAN_POINT('Ctrl Pts',(1.69215434499994,15.2,10.466172053));
#222615=CARTESIAN_POINT('Ctrl Pts',(1.69215434499994,11.6,10.466172053));
#222616=CARTESIAN_POINT('Ctrl Pts',(1.69136614299994,15.2,10.464221864));
#222617=CARTESIAN_POINT('Ctrl Pts',(1.69136614299994,11.6,10.464221864));
#222618=CARTESIAN_POINT('Ctrl Pts',(1.69058224899994,15.2,10.462277333));
#222619=CARTESIAN_POINT('Ctrl Pts',(1.69058224899994,11.6,10.462277333));
#222620=CARTESIAN_POINT('Ctrl Pts',(1.68980265899994,15.2,10.460338478));
#222621=CARTESIAN_POINT('Ctrl Pts',(1.68980265899994,11.6,10.460338478));
#222622=CARTESIAN_POINT('Ctrl Pts',(1.68902736899994,15.2,10.458405317));
#222623=CARTESIAN_POINT('Ctrl Pts',(1.68902736899994,11.6,10.458405317));
#222624=CARTESIAN_POINT('Ctrl Pts',(1.68825637199994,15.2,10.456477865));
#222625=CARTESIAN_POINT('Ctrl Pts',(1.68825637199994,11.6,10.456477865));
#222626=CARTESIAN_POINT('Ctrl Pts',(1.68748966599994,15.2,10.454556143));
#222627=CARTESIAN_POINT('Ctrl Pts',(1.68748966599994,11.6,10.454556143));
#222628=CARTESIAN_POINT('Ctrl Pts',(1.68672724499994,15.2,10.452640167));
#222629=CARTESIAN_POINT('Ctrl Pts',(1.68672724499994,11.6,10.452640167));
#222630=CARTESIAN_POINT('Ctrl Pts',(1.68596910199994,15.2,10.450729955));
#222631=CARTESIAN_POINT('Ctrl Pts',(1.68596910199994,11.6,10.450729955));
#222632=CARTESIAN_POINT('Ctrl Pts',(1.68521523599995,15.2,10.448825525));
#222633=CARTESIAN_POINT('Ctrl Pts',(1.68521523599995,11.6,10.448825525));
#222634=CARTESIAN_POINT('Ctrl Pts',(1.68446563799994,15.2,10.446926895));
#222635=CARTESIAN_POINT('Ctrl Pts',(1.68446563799994,11.6,10.446926895));
#222636=CARTESIAN_POINT('Ctrl Pts',(1.68372030499994,15.2,10.445034085));
#222637=CARTESIAN_POINT('Ctrl Pts',(1.68372030499994,11.6,10.445034085));
#222638=CARTESIAN_POINT('Ctrl Pts',(1.68297923299994,15.2,10.44314711));
#222639=CARTESIAN_POINT('Ctrl Pts',(1.68297923299994,11.6,10.44314711));
#222640=CARTESIAN_POINT('Ctrl Pts',(1.68224241499994,15.2,10.44126599));
#222641=CARTESIAN_POINT('Ctrl Pts',(1.68224241499994,11.6,10.44126599));
#222642=CARTESIAN_POINT('Ctrl Pts',(1.68150984699994,15.2,10.439390743));
#222643=CARTESIAN_POINT('Ctrl Pts',(1.68150984699994,11.6,10.439390743));
#222644=CARTESIAN_POINT('Ctrl Pts',(1.68078152299994,15.2,10.437521387));
#222645=CARTESIAN_POINT('Ctrl Pts',(1.68078152299994,11.6,10.437521387));
#222646=CARTESIAN_POINT('Ctrl Pts',(1.68005743899994,15.2,10.43565794));
#222647=CARTESIAN_POINT('Ctrl Pts',(1.68005743899994,11.6,10.43565794));
#222648=CARTESIAN_POINT('Ctrl Pts',(1.67933758799994,15.2,10.433800421));
#222649=CARTESIAN_POINT('Ctrl Pts',(1.67933758799994,11.6,10.433800421));
#222650=CARTESIAN_POINT('Ctrl Pts',(1.67862196699994,15.2,10.431948848));
#222651=CARTESIAN_POINT('Ctrl Pts',(1.67862196699994,11.6,10.431948848));
#222652=CARTESIAN_POINT('Ctrl Pts',(1.67791056899994,15.2,10.43010324));
#222653=CARTESIAN_POINT('Ctrl Pts',(1.67791056899994,11.6,10.43010324));
#222654=CARTESIAN_POINT('Ctrl Pts',(1.67720338999994,15.2,10.428263616));
#222655=CARTESIAN_POINT('Ctrl Pts',(1.67720338999994,11.6,10.428263616));
#222656=CARTESIAN_POINT('Ctrl Pts',(1.67650042399994,15.2,10.426429993));
#222657=CARTESIAN_POINT('Ctrl Pts',(1.67650042399994,11.6,10.426429993));
#222658=CARTESIAN_POINT('Ctrl Pts',(1.67580166599994,15.2,10.424602391));
#222659=CARTESIAN_POINT('Ctrl Pts',(1.67580166599994,11.6,10.424602391));
#222660=CARTESIAN_POINT('Ctrl Pts',(1.67510710999994,15.2,10.422780829));
#222661=CARTESIAN_POINT('Ctrl Pts',(1.67510710999994,11.6,10.422780829));
#222662=CARTESIAN_POINT('Ctrl Pts',(1.67441675199994,15.2,10.420965325));
#222663=CARTESIAN_POINT('Ctrl Pts',(1.67441675199994,11.6,10.420965325));
#222664=CARTESIAN_POINT('Ctrl Pts',(1.67373058499994,15.2,10.419155898));
#222665=CARTESIAN_POINT('Ctrl Pts',(1.67373058499994,11.6,10.419155898));
#222666=CARTESIAN_POINT('Ctrl Pts',(1.67304860399994,15.2,10.417352566));
#222667=CARTESIAN_POINT('Ctrl Pts',(1.67304860399994,11.6,10.417352566));
#222668=CARTESIAN_POINT('Ctrl Pts',(1.67237080499994,15.2,10.41555535));
#222669=CARTESIAN_POINT('Ctrl Pts',(1.67237080499994,11.6,10.41555535));
#222670=CARTESIAN_POINT('Ctrl Pts',(1.67169717899994,15.2,10.413764268));
#222671=CARTESIAN_POINT('Ctrl Pts',(1.67169717899994,11.6,10.413764268));
#222672=CARTESIAN_POINT('Ctrl Pts',(1.67102772499994,15.2,10.41197934));
#222673=CARTESIAN_POINT('Ctrl Pts',(1.67102772499994,11.6,10.41197934));
#222674=CARTESIAN_POINT('Ctrl Pts',(1.67036243399994,15.2,10.410200583));
#222675=CARTESIAN_POINT('Ctrl Pts',(1.67036243399994,11.6,10.410200583));
#222676=CARTESIAN_POINT('Ctrl Pts',(1.66970130199994,15.2,10.408428019));
#222677=CARTESIAN_POINT('Ctrl Pts',(1.66970130199994,11.6,10.408428019));
#222678=CARTESIAN_POINT('Ctrl Pts',(1.66904432199994,15.2,10.406661665));
#222679=CARTESIAN_POINT('Ctrl Pts',(1.66904432199994,11.6,10.406661665));
#222680=CARTESIAN_POINT('Ctrl Pts',(1.66839148999994,15.2,10.404901541));
#222681=CARTESIAN_POINT('Ctrl Pts',(1.66839148999994,11.6,10.404901541));
#222682=CARTESIAN_POINT('Ctrl Pts',(1.66774279899994,15.2,10.403147668));
#222683=CARTESIAN_POINT('Ctrl Pts',(1.66774279899994,11.6,10.403147668));
#222684=CARTESIAN_POINT('Ctrl Pts',(1.66709824499994,15.2,10.401400063));
#222685=CARTESIAN_POINT('Ctrl Pts',(1.66709824499994,11.6,10.401400063));
#222686=CARTESIAN_POINT('Ctrl Pts',(1.66645781999994,15.2,10.399658748));
#222687=CARTESIAN_POINT('Ctrl Pts',(1.66645781999994,11.6,10.399658748));
#222688=CARTESIAN_POINT('Ctrl Pts',(1.66582151999994,15.2,10.397923741));
#222689=CARTESIAN_POINT('Ctrl Pts',(1.66582151999994,11.6,10.397923741));
#222690=CARTESIAN_POINT('Ctrl Pts',(1.66518933799994,15.2,10.396195062));
#222691=CARTESIAN_POINT('Ctrl Pts',(1.66518933799994,11.6,10.396195062));
#222692=CARTESIAN_POINT('Ctrl Pts',(1.66456126799994,15.2,10.394472732));
#222693=CARTESIAN_POINT('Ctrl Pts',(1.66456126799994,11.6,10.394472732));
#222694=CARTESIAN_POINT('Ctrl Pts',(1.66393730499994,15.2,10.392756769));
#222695=CARTESIAN_POINT('Ctrl Pts',(1.66393730499994,11.6,10.392756769));
#222696=CARTESIAN_POINT('Ctrl Pts',(1.66331744299994,15.2,10.391047193));
#222697=CARTESIAN_POINT('Ctrl Pts',(1.66331744299994,11.6,10.391047193));
#222698=CARTESIAN_POINT('Ctrl Pts',(1.66270167599994,15.2,10.389344026));
#222699=CARTESIAN_POINT('Ctrl Pts',(1.66270167599994,11.6,10.389344026));
#222700=CARTESIAN_POINT('Ctrl Pts',(1.66208999699994,15.2,10.387647286));
#222701=CARTESIAN_POINT('Ctrl Pts',(1.66208999699994,11.6,10.387647286));
#222702=CARTESIAN_POINT('Ctrl Pts',(1.66148240099994,15.2,10.385956994));
#222703=CARTESIAN_POINT('Ctrl Pts',(1.66148240099994,11.6,10.385956994));
#222704=CARTESIAN_POINT('Ctrl Pts',(1.66087888199994,15.2,10.384273171));
#222705=CARTESIAN_POINT('Ctrl Pts',(1.66087888199994,11.6,10.384273171));
#222706=CARTESIAN_POINT('Ctrl Pts',(1.66027943499994,15.2,10.382595835));
#222707=CARTESIAN_POINT('Ctrl Pts',(1.66027943499994,11.6,10.382595835));
#222708=CARTESIAN_POINT('Ctrl Pts',(1.65968404999994,15.2,10.380925008));
#222709=CARTESIAN_POINT('Ctrl Pts',(1.65968404999994,11.6,10.380925008));
#222710=CARTESIAN_POINT('Ctrl Pts',(1.65909272599994,15.2,10.37926071));
#222711=CARTESIAN_POINT('Ctrl Pts',(1.65909272599994,11.6,10.37926071));
#222712=CARTESIAN_POINT('Ctrl Pts',(1.65850545199994,15.2,10.377602961));
#222713=CARTESIAN_POINT('Ctrl Pts',(1.65850545199994,11.6,10.377602961));
#222714=CARTESIAN_POINT('Ctrl Pts',(1.65792222399994,15.2,10.375951783));
#222715=CARTESIAN_POINT('Ctrl Pts',(1.65792222399994,11.6,10.375951783));
#222716=CARTESIAN_POINT('Ctrl Pts',(1.65734303699994,15.2,10.374307195));
#222717=CARTESIAN_POINT('Ctrl Pts',(1.65734303699994,11.6,10.374307195));
#222718=CARTESIAN_POINT('Ctrl Pts',(1.65676788199994,15.2,10.372669218));
#222719=CARTESIAN_POINT('Ctrl Pts',(1.65676788199994,11.6,10.372669218));
#222720=CARTESIAN_POINT('Ctrl Pts',(1.65619675499994,15.2,10.371037874));
#222721=CARTESIAN_POINT('Ctrl Pts',(1.65619675499994,11.6,10.371037874));
#222722=CARTESIAN_POINT('Ctrl Pts',(1.65562964799994,15.2,10.369413182));
#222723=CARTESIAN_POINT('Ctrl Pts',(1.65562964799994,11.6,10.369413182));
#222724=CARTESIAN_POINT('Ctrl Pts',(1.65506655599994,15.2,10.367795164));
#222725=CARTESIAN_POINT('Ctrl Pts',(1.65506655599994,11.6,10.367795164));
#222726=CARTESIAN_POINT('Ctrl Pts',(1.65450747099994,15.2,10.366183841));
#222727=CARTESIAN_POINT('Ctrl Pts',(1.65450747099994,11.6,10.366183841));
#222728=CARTESIAN_POINT('Ctrl Pts',(1.65395238799994,15.2,10.364579233));
#222729=CARTESIAN_POINT('Ctrl Pts',(1.65395238799994,11.6,10.364579233));
#222730=CARTESIAN_POINT('Ctrl Pts',(1.65340129899994,15.2,10.362981363));
#222731=CARTESIAN_POINT('Ctrl Pts',(1.65340129899994,11.6,10.362981363));
#222732=CARTESIAN_POINT('Ctrl Pts',(1.65285419799994,15.2,10.36139025));
#222733=CARTESIAN_POINT('Ctrl Pts',(1.65285419799994,11.6,10.36139025));
#222734=CARTESIAN_POINT('Ctrl Pts',(1.65231107899994,15.2,10.359805917));
#222735=CARTESIAN_POINT('Ctrl Pts',(1.65231107899994,11.6,10.359805917));
#222736=CARTESIAN_POINT('Ctrl Pts',(1.65177193599994,15.2,10.358228384));
#222737=CARTESIAN_POINT('Ctrl Pts',(1.65177193599994,11.6,10.358228384));
#222738=CARTESIAN_POINT('Ctrl Pts',(1.65123676099994,15.2,10.356657674));
#222739=CARTESIAN_POINT('Ctrl Pts',(1.65123676099994,11.6,10.356657674));
#222740=CARTESIAN_POINT('Ctrl Pts',(1.65070554599994,15.2,10.355093807));
#222741=CARTESIAN_POINT('Ctrl Pts',(1.65070554599994,11.6,10.355093807));
#222742=CARTESIAN_POINT('Ctrl Pts',(1.65017828699994,15.2,10.353536806));
#222743=CARTESIAN_POINT('Ctrl Pts',(1.65017828699994,11.6,10.353536806));
#222744=CARTESIAN_POINT('Ctrl Pts',(1.64965497699994,15.2,10.351986692));
#222745=CARTESIAN_POINT('Ctrl Pts',(1.64965497699994,11.6,10.351986692));
#222746=CARTESIAN_POINT('Ctrl Pts',(1.64913560699994,15.2,10.350443486));
#222747=CARTESIAN_POINT('Ctrl Pts',(1.64913560699994,11.6,10.350443486));
#222748=CARTESIAN_POINT('Ctrl Pts',(1.64862017199994,15.2,10.348907211));
#222749=CARTESIAN_POINT('Ctrl Pts',(1.64862017199994,11.6,10.348907211));
#222750=CARTESIAN_POINT('Ctrl Pts',(1.64810866499994,15.2,10.347377888));
#222751=CARTESIAN_POINT('Ctrl Pts',(1.64810866499994,11.6,10.347377888));
#222752=CARTESIAN_POINT('Ctrl Pts',(1.64760107699994,15.2,10.34585554));
#222753=CARTESIAN_POINT('Ctrl Pts',(1.64760107699994,11.6,10.34585554));
#222754=CARTESIAN_POINT('Ctrl Pts',(1.64709740399994,15.2,10.344340188));
#222755=CARTESIAN_POINT('Ctrl Pts',(1.64709740399994,11.6,10.344340188));
#222756=CARTESIAN_POINT('Ctrl Pts',(1.64659763699994,15.2,10.342831855));
#222757=CARTESIAN_POINT('Ctrl Pts',(1.64659763699994,11.6,10.342831855));
#222758=CARTESIAN_POINT('Ctrl Pts',(1.64610176899994,15.2,10.341330562));
#222759=CARTESIAN_POINT('Ctrl Pts',(1.64610176899994,11.6,10.341330562));
#222760=CARTESIAN_POINT('Ctrl Pts',(1.64560979399994,15.2,10.339836333));
#222761=CARTESIAN_POINT('Ctrl Pts',(1.64560979399994,11.6,10.339836333));
#222762=CARTESIAN_POINT('Ctrl Pts',(1.64512170499994,15.2,10.33834919));
#222763=CARTESIAN_POINT('Ctrl Pts',(1.64512170499994,11.6,10.33834919));
#222764=CARTESIAN_POINT('Ctrl Pts',(1.64463749299994,15.2,10.336869155));
#222765=CARTESIAN_POINT('Ctrl Pts',(1.64463749299994,11.6,10.336869155));
#222766=CARTESIAN_POINT('Ctrl Pts',(1.64415715199994,15.2,10.335396249));
#222767=CARTESIAN_POINT('Ctrl Pts',(1.64415715199994,11.6,10.335396249));
#222768=CARTESIAN_POINT('Ctrl Pts',(1.64368067599994,15.2,10.333930498));
#222769=CARTESIAN_POINT('Ctrl Pts',(1.64368067599994,11.6,10.333930498));
#222770=CARTESIAN_POINT('Ctrl Pts',(1.64320805499994,15.2,10.332471923));
#222771=CARTESIAN_POINT('Ctrl Pts',(1.64320805499994,11.6,10.332471923));
#222772=CARTESIAN_POINT('Ctrl Pts',(1.64273928299994,15.2,10.331020546));
#222773=CARTESIAN_POINT('Ctrl Pts',(1.64273928299994,11.6,10.331020546));
#222774=CARTESIAN_POINT('Ctrl Pts',(1.64227435299994,15.2,10.329576392));
#222775=CARTESIAN_POINT('Ctrl Pts',(1.64227435299994,11.6,10.329576392));
#222776=CARTESIAN_POINT('Ctrl Pts',(1.64181325799994,15.2,10.328139482));
#222777=CARTESIAN_POINT('Ctrl Pts',(1.64181325799994,11.6,10.328139482));
#222778=CARTESIAN_POINT('Ctrl Pts',(1.64135598799994,15.2,10.32670984));
#222779=CARTESIAN_POINT('Ctrl Pts',(1.64135598799994,11.6,10.32670984));
#222780=CARTESIAN_POINT('Ctrl Pts',(1.64090253799994,15.2,10.32528749));
#222781=CARTESIAN_POINT('Ctrl Pts',(1.64090253799994,11.6,10.32528749));
#222782=CARTESIAN_POINT('Ctrl Pts',(1.64045289999994,15.2,10.323872453));
#222783=CARTESIAN_POINT('Ctrl Pts',(1.64045289999994,11.6,10.323872453));
#222784=CARTESIAN_POINT('Ctrl Pts',(1.64000706499994,15.2,10.322464755));
#222785=CARTESIAN_POINT('Ctrl Pts',(1.64000706499994,11.6,10.322464755));
#222786=CARTESIAN_POINT('Ctrl Pts',(1.63956502699994,15.2,10.321064418));
#222787=CARTESIAN_POINT('Ctrl Pts',(1.63956502699994,11.6,10.321064418));
#222788=CARTESIAN_POINT('Ctrl Pts',(1.63912677699994,15.2,10.319671465));
#222789=CARTESIAN_POINT('Ctrl Pts',(1.63912677699994,11.6,10.319671465));
#222790=CARTESIAN_POINT('Ctrl Pts',(1.63869230999994,15.2,10.318285922));
#222791=CARTESIAN_POINT('Ctrl Pts',(1.63869230999994,11.6,10.318285922));
#222792=CARTESIAN_POINT('Ctrl Pts',(1.63826161399994,15.2,10.31690781));
#222793=CARTESIAN_POINT('Ctrl Pts',(1.63826161399994,11.6,10.31690781));
#222794=CARTESIAN_POINT('Ctrl Pts',(1.63783468399994,15.2,10.315537154));
#222795=CARTESIAN_POINT('Ctrl Pts',(1.63783468399994,11.6,10.315537154));
#222796=CARTESIAN_POINT('Ctrl Pts',(1.63741151199994,15.2,10.314173979));
#222797=CARTESIAN_POINT('Ctrl Pts',(1.63741151199994,11.6,10.314173979));
#222798=CARTESIAN_POINT('Ctrl Pts',(1.63699208899994,15.2,10.312818307));
#222799=CARTESIAN_POINT('Ctrl Pts',(1.63699208899994,11.6,10.312818307));
#222800=CARTESIAN_POINT('Ctrl Pts',(1.63657640799994,15.2,10.311470163));
#222801=CARTESIAN_POINT('Ctrl Pts',(1.63657640799994,11.6,10.311470163));
#222802=CARTESIAN_POINT('Ctrl Pts',(1.63616445999994,15.2,10.310129573));
#222803=CARTESIAN_POINT('Ctrl Pts',(1.63616445999994,11.6,10.310129573));
#222804=CARTESIAN_POINT('Ctrl Pts',(1.63575623799994,15.2,10.308796559));
#222805=CARTESIAN_POINT('Ctrl Pts',(1.63575623799994,11.6,10.308796559));
#222806=CARTESIAN_POINT('Ctrl Pts',(1.63535173399994,15.2,10.307471145));
#222807=CARTESIAN_POINT('Ctrl Pts',(1.63535173399994,11.6,10.307471145));
#222808=CARTESIAN_POINT('Ctrl Pts',(1.63495093799994,15.2,10.306153357));
#222809=CARTESIAN_POINT('Ctrl Pts',(1.63495093799994,11.6,10.306153357));
#222810=CARTESIAN_POINT('Ctrl Pts',(1.63455384399994,15.2,10.30484322));
#222811=CARTESIAN_POINT('Ctrl Pts',(1.63455384399994,11.6,10.30484322));
#222812=CARTESIAN_POINT('Ctrl Pts',(1.63416044299994,15.2,10.303540758));
#222813=CARTESIAN_POINT('Ctrl Pts',(1.63416044299994,11.6,10.303540758));
#222814=CARTESIAN_POINT('Ctrl Pts',(1.63377072599994,15.2,10.302245995));
#222815=CARTESIAN_POINT('Ctrl Pts',(1.63377072599994,11.6,10.302245995));
#222816=CARTESIAN_POINT('Ctrl Pts',(1.63338468399994,15.2,10.300958957));
#222817=CARTESIAN_POINT('Ctrl Pts',(1.63338468399994,11.6,10.300958957));
#222818=CARTESIAN_POINT('Ctrl Pts',(1.63300231199994,15.2,10.299679669));
#222819=CARTESIAN_POINT('Ctrl Pts',(1.63300231199994,11.6,10.299679669));
#222820=CARTESIAN_POINT('Ctrl Pts',(1.63262359899994,15.2,10.298408156));
#222821=CARTESIAN_POINT('Ctrl Pts',(1.63262359899994,11.6,10.298408156));
#222822=CARTESIAN_POINT('Ctrl Pts',(1.63224853599994,15.2,10.297144443));
#222823=CARTESIAN_POINT('Ctrl Pts',(1.63224853599994,11.6,10.297144443));
#222824=CARTESIAN_POINT('Ctrl Pts',(1.63187711599994,15.2,10.295888555));
#222825=CARTESIAN_POINT('Ctrl Pts',(1.63187711599994,11.6,10.295888555));
#222826=CARTESIAN_POINT('Ctrl Pts',(1.63150932899994,15.2,10.294640518));
#222827=CARTESIAN_POINT('Ctrl Pts',(1.63150932899994,11.6,10.294640518));
#222828=CARTESIAN_POINT('Ctrl Pts',(1.63114516899994,15.2,10.293400358));
#222829=CARTESIAN_POINT('Ctrl Pts',(1.63114516899994,11.6,10.293400358));
#222830=CARTESIAN_POINT('Ctrl Pts',(1.63078462299994,15.2,10.292168099));
#222831=CARTESIAN_POINT('Ctrl Pts',(1.63078462299994,11.6,10.292168099));
#222832=CARTESIAN_POINT('Ctrl Pts',(1.63042768599994,15.2,10.290943769));
#222833=CARTESIAN_POINT('Ctrl Pts',(1.63042768599994,11.6,10.290943769));
#222834=CARTESIAN_POINT('Ctrl Pts',(1.63007434799994,15.2,10.289727393));
#222835=CARTESIAN_POINT('Ctrl Pts',(1.63007434799994,11.6,10.289727393));
#222836=CARTESIAN_POINT('Ctrl Pts',(1.62972459999994,15.2,10.288518995));
#222837=CARTESIAN_POINT('Ctrl Pts',(1.62972459999994,11.6,10.288518995));
#222838=CARTESIAN_POINT('Ctrl Pts',(1.62937843299995,15.2,10.287318605));
#222839=CARTESIAN_POINT('Ctrl Pts',(1.62937843299995,11.6,10.287318605));
#222840=CARTESIAN_POINT('Ctrl Pts',(1.62903583799994,15.2,10.286126245));
#222841=CARTESIAN_POINT('Ctrl Pts',(1.62903583799994,11.6,10.286126245));
#222842=CARTESIAN_POINT('Ctrl Pts',(1.62869680599994,15.2,10.284941946));
#222843=CARTESIAN_POINT('Ctrl Pts',(1.62869680599994,11.6,10.284941946));
#222844=CARTESIAN_POINT('Ctrl Pts',(1.62836132899994,15.2,10.28376573));
#222845=CARTESIAN_POINT('Ctrl Pts',(1.62836132899994,11.6,10.28376573));
#222846=CARTESIAN_POINT('Ctrl Pts',(1.62802939799994,15.2,10.282597626));
#222847=CARTESIAN_POINT('Ctrl Pts',(1.62802939799994,11.6,10.282597626));
#222848=CARTESIAN_POINT('Ctrl Pts',(1.62770099999994,15.2,10.28143766));
#222849=CARTESIAN_POINT('Ctrl Pts',(1.62770099999994,11.6,10.28143766));
#222850=CARTESIAN_POINT('Ctrl Pts',(1.62737613099994,15.2,10.280285859));
#222851=CARTESIAN_POINT('Ctrl Pts',(1.62737613099994,11.6,10.280285859));
#222852=CARTESIAN_POINT('Ctrl Pts',(1.62705477799994,15.2,10.279142249));
#222853=CARTESIAN_POINT('Ctrl Pts',(1.62705477799994,11.6,10.279142249));
#222854=CARTESIAN_POINT('Ctrl Pts',(1.62673693399994,15.2,10.278006859));
#222855=CARTESIAN_POINT('Ctrl Pts',(1.62673693399994,11.6,10.278006859));
#222856=CARTESIAN_POINT('Ctrl Pts',(1.62642258799994,15.2,10.276879714));
#222857=CARTESIAN_POINT('Ctrl Pts',(1.62642258799994,11.6,10.276879714));
#222858=CARTESIAN_POINT('Ctrl Pts',(1.62611173199994,15.2,10.275760843));
#222859=CARTESIAN_POINT('Ctrl Pts',(1.62611173199994,11.6,10.275760843));
#222860=CARTESIAN_POINT('Ctrl Pts',(1.62580435499994,15.2,10.274650272));
#222861=CARTESIAN_POINT('Ctrl Pts',(1.62580435499994,11.6,10.274650272));
#222862=CARTESIAN_POINT('Ctrl Pts',(1.62550044799994,15.2,10.27354803));
#222863=CARTESIAN_POINT('Ctrl Pts',(1.62550044799994,11.6,10.27354803));
#222864=CARTESIAN_POINT('Ctrl Pts',(1.62520000299994,15.2,10.272454143));
#222865=CARTESIAN_POINT('Ctrl Pts',(1.62520000299994,11.6,10.272454143));
#222866=CARTESIAN_POINT('Ctrl Pts',(1.62490300799994,15.2,10.27136864));
#222867=CARTESIAN_POINT('Ctrl Pts',(1.62490300799994,11.6,10.27136864));
#222868=CARTESIAN_POINT('Ctrl Pts',(1.62460945299994,15.2,10.270291547));
#222869=CARTESIAN_POINT('Ctrl Pts',(1.62460945299994,11.6,10.270291547));
#222870=CARTESIAN_POINT('Ctrl Pts',(1.62431932999994,15.2,10.269222896));
#222871=CARTESIAN_POINT('Ctrl Pts',(1.62431932999994,11.6,10.269222896));
#222872=CARTESIAN_POINT('Ctrl Pts',(1.62403262999994,15.2,10.268162711));
#222873=CARTESIAN_POINT('Ctrl Pts',(1.62403262999994,11.6,10.268162711));
#222874=CARTESIAN_POINT('Ctrl Pts',(1.62374933999994,15.2,10.267111022));
#222875=CARTESIAN_POINT('Ctrl Pts',(1.62374933999994,11.6,10.267111022));
#222876=CARTESIAN_POINT('Ctrl Pts',(1.62346945199994,15.2,10.266067857));
#222877=CARTESIAN_POINT('Ctrl Pts',(1.62346945199994,11.6,10.266067857));
#222878=CARTESIAN_POINT('Ctrl Pts',(1.62319295499994,15.2,10.265033245));
#222879=CARTESIAN_POINT('Ctrl Pts',(1.62319295499994,11.6,10.265033245));
#222880=CARTESIAN_POINT('Ctrl Pts',(1.62291983999994,15.2,10.264007215));
#222881=CARTESIAN_POINT('Ctrl Pts',(1.62291983999994,11.6,10.264007215));
#222882=CARTESIAN_POINT('Ctrl Pts',(1.62265009699994,15.2,10.262989795));
#222883=CARTESIAN_POINT('Ctrl Pts',(1.62265009699994,11.6,10.262989795));
#222884=CARTESIAN_POINT('Ctrl Pts',(1.62238371499994,15.2,10.261981014));
#222885=CARTESIAN_POINT('Ctrl Pts',(1.62238371499994,11.6,10.261981014));
#222886=CARTESIAN_POINT('Ctrl Pts',(1.62212068299994,15.2,10.2609809));
#222887=CARTESIAN_POINT('Ctrl Pts',(1.62212068299994,11.6,10.2609809));
#222888=CARTESIAN_POINT('Ctrl Pts',(1.62186099299995,15.2,10.259989485));
#222889=CARTESIAN_POINT('Ctrl Pts',(1.62186099299995,11.6,10.259989485));
#222890=CARTESIAN_POINT('Ctrl Pts',(1.62160463199994,15.2,10.259006796));
#222891=CARTESIAN_POINT('Ctrl Pts',(1.62160463199994,11.6,10.259006796));
#222892=CARTESIAN_POINT('Ctrl Pts',(1.62135158999994,15.2,10.258032864));
#222893=CARTESIAN_POINT('Ctrl Pts',(1.62135158999994,11.6,10.258032864));
#222894=CARTESIAN_POINT('Ctrl Pts',(1.62110185799994,15.2,10.257067718));
#222895=CARTESIAN_POINT('Ctrl Pts',(1.62110185799994,11.6,10.257067718));
#222896=CARTESIAN_POINT('Ctrl Pts',(1.62085542399994,15.2,10.256111387));
#222897=CARTESIAN_POINT('Ctrl Pts',(1.62085542399994,11.6,10.256111387));
#222898=CARTESIAN_POINT('Ctrl Pts',(1.62061227799994,15.2,10.2551639));
#222899=CARTESIAN_POINT('Ctrl Pts',(1.62061227799994,11.6,10.2551639));
#222900=CARTESIAN_POINT('Ctrl Pts',(1.62037240999994,15.2,10.25422529));
#222901=CARTESIAN_POINT('Ctrl Pts',(1.62037240999994,11.6,10.25422529));
#222902=CARTESIAN_POINT('Ctrl Pts',(1.62013580699994,15.2,10.253295587));
#222903=CARTESIAN_POINT('Ctrl Pts',(1.62013580699994,11.6,10.253295587));
#222904=CARTESIAN_POINT('Ctrl Pts',(1.61990245999994,15.2,10.252374818));
#222905=CARTESIAN_POINT('Ctrl Pts',(1.61990245999994,11.6,10.252374818));
#222906=CARTESIAN_POINT('Ctrl Pts',(1.61967235799994,15.2,10.251463016));
#222907=CARTESIAN_POINT('Ctrl Pts',(1.61967235799994,11.6,10.251463016));
#222908=CARTESIAN_POINT('Ctrl Pts',(1.61944548799994,15.2,10.250560211));
#222909=CARTESIAN_POINT('Ctrl Pts',(1.61944548799994,11.6,10.250560211));
#222910=CARTESIAN_POINT('Ctrl Pts',(1.61922312999994,15.2,10.249671582));
#222911=CARTESIAN_POINT('Ctrl Pts',(1.61922312999994,11.6,10.249671582));
#222912=CARTESIAN_POINT('Ctrl Pts',(1.61904803299994,15.2,10.248968852));
#222913=CARTESIAN_POINT('Ctrl Pts',(1.61904803299994,11.6,10.248968852));
#222914=CARTESIAN_POINT('Ctrl Pts',(1.61891843999994,15.2,10.248447089));
#222915=CARTESIAN_POINT('Ctrl Pts',(1.61891843999994,11.6,10.248447089));
#222916=CARTESIAN_POINT('Ctrl Pts',(1.61883308399994,15.2,10.248102704));
#222917=CARTESIAN_POINT('Ctrl Pts',(1.61883308399994,11.6,10.248102704));
#222918=CARTESIAN_POINT('Ctrl Pts',(1.61879117999994,15.2,10.247933457));
#222919=CARTESIAN_POINT('Ctrl Pts',(1.61879117999994,11.6,10.247933457));
#222920=CARTESIAN_POINT('',(1.61879117999994,12.2,10.247933456));
#222921=CARTESIAN_POINT('',(1.61879117999994,15.2,10.247933456));
#222922=CARTESIAN_POINT('',(1.61879117999994,12.2,10.247933456));
#222923=CARTESIAN_POINT('Ctrl Pts',(2.17615954699994,12.2,11.292224299));
#222924=CARTESIAN_POINT('Ctrl Pts',(2.17309893155329,12.2,11.2881482228521));
#222925=CARTESIAN_POINT('Ctrl Pts',(2.17005151744838,12.2,11.2840769414757));
#222926=CARTESIAN_POINT('Ctrl Pts',(2.1670173032288,12.2,11.2800104643101));
#222927=CARTESIAN_POINT('Ctrl Pts',(2.16474164277082,12.2,11.2769606067129));
#222928=CARTESIAN_POINT('Ctrl Pts',(2.16247340685917,12.2,11.2739134515355));
#222929=CARTESIAN_POINT('Ctrl Pts',(2.16021259628755,12.2,11.270869025661));
#222930=CARTESIAN_POINT('Ctrl Pts',(2.15795178571594,12.2,11.2678245997865));
#222931=CARTESIAN_POINT('Ctrl Pts',(2.15569840077296,12.2,11.2647829037414));
#222932=CARTESIAN_POINT('Ctrl Pts',(2.15345243877187,12.2,11.2617439866854));
#222933=CARTESIAN_POINT('Ctrl Pts',(2.15120647677078,12.2,11.2587050696294));
#222934=CARTESIAN_POINT('Ctrl Pts',(2.14896793703549,12.2,11.2556689314398));
#222935=CARTESIAN_POINT('Ctrl Pts',(2.14673681999156,12.2,11.2526356197583));
#222936=CARTESIAN_POINT('Ctrl Pts',(2.14450570294763,12.2,11.2496023080769));
#222937=CARTESIAN_POINT('Ctrl Pts',(2.14228200681172,12.2,11.2465718218036));
#222938=CARTESIAN_POINT('Ctrl Pts',(2.14006573176659,12.2,11.2435441981217));
#222939=CARTESIAN_POINT('Ctrl Pts',(2.13784945672146,12.2,11.2405165744398));
#222940=CARTESIAN_POINT('Ctrl Pts',(2.13564060100672,12.2,11.2374918133761));
#222941=CARTESIAN_POINT('Ctrl Pts',(2.13343916493422,12.2,11.2344699530847));
#222942=CARTESIAN_POINT('Ctrl Pts',(2.13123772886173,12.2,11.2314480927932));
#222943=CARTESIAN_POINT('Ctrl Pts',(2.12904371206482,12.2,11.2284291335483));
#222944=CARTESIAN_POINT('Ctrl Pts',(2.12685711172657,12.2,11.2254131179491));
#222945=CARTESIAN_POINT('Ctrl Pts',(2.12467051099109,12.2,11.222397101802));
#222946=CARTESIAN_POINT('Ctrl Pts',(2.12249132822439,12.2,11.2193840298141));
#222947=CARTESIAN_POINT('Ctrl Pts',(2.12031955995146,12.2,11.2163739436271));
#222948=CARTESIAN_POINT('Ctrl Pts',(2.11814779207307,12.2,11.2133638579869));
#222949=CARTESIAN_POINT('Ctrl Pts',(2.11598344051922,12.2,11.2103567576298));
#222950=CARTESIAN_POINT('Ctrl Pts',(2.11382650205658,12.2,11.2073526849476));
#222951=CARTESIAN_POINT('Ctrl Pts',(2.11166956359395,12.2,11.2043486122654));
#222952=CARTESIAN_POINT('Ctrl Pts',(2.10952003867981,12.2,11.2013475656353));
#222953=CARTESIAN_POINT('Ctrl Pts',(2.10737792524795,12.2,11.1983495874806));
#222954=CARTESIAN_POINT('Ctrl Pts',(2.10523581181609,12.2,11.1953516093259));
#222955=CARTESIAN_POINT('Ctrl Pts',(2.10310110988422,12.2,11.1923566989576));
#222956=CARTESIAN_POINT('Ctrl Pts',(2.1009738169935,12.2,11.189364899261));
#222957=CARTESIAN_POINT('Ctrl Pts',(2.09884652410277,12.2,11.1863730995645));
#222958=CARTESIAN_POINT('Ctrl Pts',(2.09672664165414,12.2,11.1833844089672));
#222959=CARTESIAN_POINT('Ctrl Pts',(2.09461416573028,12.2,11.1803988718254));
#222960=CARTESIAN_POINT('Ctrl Pts',(2.09250168980641,12.2,11.1774133346837));
#222961=CARTESIAN_POINT('Ctrl Pts',(2.090396621432,12.2,11.1744309502416));
#222962=CARTESIAN_POINT('Ctrl Pts',(2.08829895746552,12.2,11.1714517601411));
#222963=CARTESIAN_POINT('Ctrl Pts',(2.08620129311796,12.2,11.1684725694993));
#222964=CARTESIAN_POINT('Ctrl Pts',(2.08411103349752,12.2,11.1654965735335));
#222965=CARTESIAN_POINT('Ctrl Pts',(2.08202817707084,12.2,11.1625238148519));
#222966=CARTESIAN_POINT('Ctrl Pts',(2.07994532102253,12.2,11.1595510567104));
#222967=CARTESIAN_POINT('Ctrl Pts',(2.07786986674384,12.2,11.1565815355495));
#222968=CARTESIAN_POINT('Ctrl Pts',(2.07580181263318,12.2,11.1536152947178));
#222969=CARTESIAN_POINT('Ctrl Pts',(2.07373375852252,12.2,11.1506490538861));
#222970=CARTESIAN_POINT('Ctrl Pts',(2.07167310431762,12.2,11.1476860921196));
#222971=CARTESIAN_POINT('Ctrl Pts',(2.06961984730955,12.2,11.1447264544358));
#222972=CARTESIAN_POINT('Ctrl Pts',(2.06756659030147,12.2,11.1417668167519));
#222973=CARTESIAN_POINT('Ctrl Pts',(2.06552072977582,12.2,11.1388105005927));
#222974=CARTESIAN_POINT('Ctrl Pts',(2.06348226426655,12.2,11.13585755145));
#222975=CARTESIAN_POINT('Ctrl Pts',(2.06144379875728,12.2,11.1329046023072));
#222976=CARTESIAN_POINT('Ctrl Pts',(2.05941272753107,12.2,11.1299550194978));
#222977=CARTESIAN_POINT('Ctrl Pts',(2.05738904797893,12.2,11.1270088463545));
#222978=CARTESIAN_POINT('Ctrl Pts',(2.05536536842678,12.2,11.1240626732112));
#222979=CARTESIAN_POINT('Ctrl Pts',(2.05334907929919,12.2,11.1211199087344));
#222980=CARTESIAN_POINT('Ctrl Pts',(2.05134017970451,12.2,11.1181805985907));
#222981=CARTESIAN_POINT('Ctrl Pts',(2.04933127974487,12.2,11.1152412879131));
#222982=CARTESIAN_POINT('Ctrl Pts',(2.04732976728732,12.2,11.1123054302197));
#222983=CARTESIAN_POINT('Ctrl Pts',(2.04533564133185,12.2,11.1093730691274));
#222984=CARTESIAN_POINT('Ctrl Pts',(2.04334151573865,12.2,11.1064407085677));
#222985=CARTESIAN_POINT('Ctrl Pts',(2.04135477412644,12.2,11.1035118456568));
#222986=CARTESIAN_POINT('Ctrl Pts',(2.03937541410034,12.2,11.1005865234507));
#222987=CARTESIAN_POINT('Ctrl Pts',(2.03739605407425,12.2,11.0976612012446));
#222988=CARTESIAN_POINT('Ctrl Pts',(2.03542407759717,12.2,11.0947394202922));
#222989=CARTESIAN_POINT('Ctrl Pts',(2.03345947908588,12.2,11.0918212251903));
#222990=CARTESIAN_POINT('Ctrl Pts',(2.03149488057459,12.2,11.0889030300883));
#222991=CARTESIAN_POINT('Ctrl Pts',(2.02953765971237,12.2,11.0859884203442));
#222992=CARTESIAN_POINT('Ctrl Pts',(2.02758781424156,12.2,11.0830774407833));
#222993=CARTESIAN_POINT('Ctrl Pts',(2.02563796877075,12.2,11.0801664612224));
#222994=CARTESIAN_POINT('Ctrl Pts',(2.02369549872463,12.2,11.0772591115947));
#222995=CARTESIAN_POINT('Ctrl Pts',(2.02176039971094,12.2,11.0743554370332));
#222996=CARTESIAN_POINT('Ctrl Pts',(2.01982530069725,12.2,11.0714517624717));
#222997=CARTESIAN_POINT('Ctrl Pts',(2.01789757243184,12.2,11.0685517625335));
#222998=CARTESIAN_POINT('Ctrl Pts',(2.01597721136318,12.2,11.0656554827854));
#222999=CARTESIAN_POINT('Ctrl Pts',(2.01405685029451,12.2,11.0627592030372));
#223000=CARTESIAN_POINT('Ctrl Pts',(2.01214385698044,12.2,11.059866643242));
#223001=CARTESIAN_POINT('Ctrl Pts',(2.01023822788199,12.2,11.0569778491381));
#223002=CARTESIAN_POINT('Ctrl Pts',(2.00833259843735,12.2,11.0540890545093));
#223003=CARTESIAN_POINT('Ctrl Pts',(2.00643433177815,12.2,11.0512040246567));
#223004=CARTESIAN_POINT('Ctrl Pts',(2.00454342487935,12.2,11.0483228056135));
#223005=CARTESIAN_POINT('Ctrl Pts',(2.00202221625347,12.2,11.044481181095));
#223006=CARTESIAN_POINT('Ctrl Pts',(1.99951409062867,12.2,11.0406463320394));
#223007=CARTESIAN_POINT('Ctrl Pts',(1.99701903872065,12.2,11.0368183661296));
#223008=CARTESIAN_POINT('Ctrl Pts',(1.99514774970465,12.2,11.0339473915669));
#223009=CARTESIAN_POINT('Ctrl Pts',(1.99328381425198,12.2,11.0310802884434));
#223010=CARTESIAN_POINT('Ctrl Pts',(1.99142722855917,12.2,11.0282171037789));
#223011=CARTESIAN_POINT('Ctrl Pts',(1.98957064286635,12.2,11.0253539191145));
#223012=CARTESIAN_POINT('Ctrl Pts',(1.98772140560218,12.2,11.0224946528192));
#223013=CARTESIAN_POINT('Ctrl Pts',(1.9858795144181,12.2,11.0196393503808));
#223014=CARTESIAN_POINT('Ctrl Pts',(1.98403762289942,12.2,11.0167840474236));
#223015=CARTESIAN_POINT('Ctrl Pts',(1.98220307456614,12.2,11.0139327102925));
#223016=CARTESIAN_POINT('Ctrl Pts',(1.98037586809323,12.2,11.0110853828792));
#223017=CARTESIAN_POINT('Ctrl Pts',(1.97793959334926,12.2,11.0072889471903));
#223018=CARTESIAN_POINT('Ctrl Pts',(1.97551636664254,12.2,11.0034996433922));
#223019=CARTESIAN_POINT('Ctrl Pts',(1.97310617867204,12.2,10.9997175808675));
#223020=CARTESIAN_POINT('Ctrl Pts',(1.97129853761207,12.2,10.9968810338452));
#223021=CARTESIAN_POINT('Ctrl Pts',(1.96949822975547,12.2,10.9940485608862));
#223022=CARTESIAN_POINT('Ctrl Pts',(1.96770525106353,12.2,10.9912202083055));
#223023=CARTESIAN_POINT('Ctrl Pts',(1.96591227237159,12.2,10.9883918557249));
#223024=CARTESIAN_POINT('Ctrl Pts',(1.96412662200731,12.2,10.9855676245629));
#223025=CARTESIAN_POINT('Ctrl Pts',(1.96234829590424,12.2,10.9827475615814));
#223026=CARTESIAN_POINT('Ctrl Pts',(1.95997719421811,12.2,10.9789874772646));
#223027=CARTESIAN_POINT('Ctrl Pts',(1.95761911145266,12.2,10.9752348048568));
#223028=CARTESIAN_POINT('Ctrl Pts',(1.95527403649156,12.2,10.9714896547083));
#223029=CARTESIAN_POINT('Ctrl Pts',(1.95292896153046,12.2,10.9677445045598));
#223030=CARTESIAN_POINT('Ctrl Pts',(1.95059689454579,12.2,10.9640068794509));
#223031=CARTESIAN_POINT('Ctrl Pts',(1.94827782042073,12.2,10.9602768924151));
#223032=CARTESIAN_POINT('Ctrl Pts',(1.94479920954912,12.2,10.9546819123696));
#223033=CARTESIAN_POINT('Ctrl Pts',(1.9413498362714,12.2,10.9491041170025));
#223034=CARTESIAN_POINT('Ctrl Pts',(1.93792965506362,12.2,10.9435438979553));
#223035=CARTESIAN_POINT('Ctrl Pts',(1.93564953436199,12.2,10.9398370854256));
#223036=CARTESIAN_POINT('Ctrl Pts',(1.93338238634383,12.2,10.9361380831136));
#223037=CARTESIAN_POINT('Ctrl Pts',(1.93112819836012,12.2,10.9324470093034));
#223038=CARTESIAN_POINT('Ctrl Pts',(1.92887401006929,12.2,10.9287559349904));
#223039=CARTESIAN_POINT('Ctrl Pts',(1.92663278119101,12.2,10.9250727883061));
#223040=CARTESIAN_POINT('Ctrl Pts',(1.92440449694838,12.2,10.9213976872558));
#223041=CARTESIAN_POINT('Ctrl Pts',(1.92217621300935,12.2,10.9177225867062));
#223042=CARTESIAN_POINT('Ctrl Pts',(1.9199608746424,12.2,10.9140555307777));
#223043=CARTESIAN_POINT('Ctrl Pts',(1.91775846537666,12.2,10.9103966382982));
#223044=CARTESIAN_POINT('Ctrl Pts',(1.91555605581084,12.2,10.9067377453201));
#223045=CARTESIAN_POINT('Ctrl Pts',(1.91336657607407,12.2,10.903087015429));
#223046=CARTESIAN_POINT('Ctrl Pts',(1.91119000973322,12.2,10.8994445685083));
#223047=CARTESIAN_POINT('Ctrl Pts',(1.90901344339237,12.2,10.8958021215875));
#223048=CARTESIAN_POINT('Ctrl Pts',(1.9068497905586,12.2,10.8921679588567));
#223049=CARTESIAN_POINT('Ctrl Pts',(1.90469903566491,12.2,10.8885421973821));
#223050=CARTESIAN_POINT('Ctrl Pts',(1.90254828106427,12.2,10.8849164364016));
#223051=CARTESIAN_POINT('Ctrl Pts',(1.9004104241262,12.2,10.8812990782488));
#223052=CARTESIAN_POINT('Ctrl Pts',(1.89828544873468,12.2,10.8776902450274));
#223053=CARTESIAN_POINT('Ctrl Pts',(1.89616047305363,12.2,10.8740814113143));
#223054=CARTESIAN_POINT('Ctrl Pts',(1.89404837804477,12.2,10.8704811012881));
#223055=CARTESIAN_POINT('Ctrl Pts',(1.89194914643168,12.2,10.8668894377044));
#223056=CARTESIAN_POINT('Ctrl Pts',(1.88984991510461,12.2,10.86329777461));
#223057=CARTESIAN_POINT('Ctrl Pts',(1.88776354742586,12.2,10.8597147567423));
#223058=CARTESIAN_POINT('Ctrl Pts',(1.88569002542786,12.2,10.8561405095339));
#223059=CARTESIAN_POINT('Ctrl Pts',(1.88361650314734,12.2,10.8525662618385));
#223060=CARTESIAN_POINT('Ctrl Pts',(1.88155582747394,12.2,10.8490007832713));
#223061=CARTESIAN_POINT('Ctrl Pts',(1.87950797842781,12.2,10.8454441982339));
#223062=CARTESIAN_POINT('Ctrl Pts',(1.8774601296607,12.2,10.8418876136811));
#223063=CARTESIAN_POINT('Ctrl Pts',(1.87542510820642,12.2,10.8383399229979));
#223064=CARTESIAN_POINT('Ctrl Pts',(1.87340289614866,12.2,10.834801251231));
#223065=CARTESIAN_POINT('Ctrl Pts',(1.87138068381538,12.2,10.8312625789819));
#223066=CARTESIAN_POINT('Ctrl Pts',(1.86937127983366,12.2,10.8277329257257));
#223067=CARTESIAN_POINT('Ctrl Pts',(1.8673746648368,12.2,10.8242124169789));
#223068=CARTESIAN_POINT('Ctrl Pts',(1.86537805011197,12.2,10.8206919087118));
#223069=CARTESIAN_POINT('Ctrl Pts',(1.86339422444842,12.2,10.8171805462149));
#223070=CARTESIAN_POINT('Ctrl Pts',(1.8614231683305,12.2,10.8136784563892));
#223071=CARTESIAN_POINT('Ctrl Pts',(1.85945211194402,12.2,10.8101763660863));
#223072=CARTESIAN_POINT('Ctrl Pts',(1.85749382363286,12.2,10.8066835475227));
#223073=CARTESIAN_POINT('Ctrl Pts',(1.85554828524024,12.2,10.8032001300392));
#223074=CARTESIAN_POINT('Ctrl Pts',(1.85360274711269,12.2,10.7997167130304));
#223075=CARTESIAN_POINT('Ctrl Pts',(1.85166995651375,12.2,10.7962426969536));
#223076=CARTESIAN_POINT('Ctrl Pts',(1.8497498937805,12.2,10.7927782112914));
#223077=CARTESIAN_POINT('Ctrl Pts',(1.84782983078564,12.2,10.7893137251571));
#223078=CARTESIAN_POINT('Ctrl Pts',(1.84592249567537,12.2,10.7858587698905));
#223079=CARTESIAN_POINT('Ctrl Pts',(1.84402786601656,12.2,10.7824134757583));
#223080=CARTESIAN_POINT('Ctrl Pts',(1.84213323635775,12.2,10.7789681816261));
#223081=CARTESIAN_POINT('Ctrl Pts',(1.84025131114487,12.2,10.7755325486895));
#223082=CARTESIAN_POINT('Ctrl Pts',(1.83838207071094,12.2,10.7721067084482));
#223083=CARTESIAN_POINT('Ctrl Pts',(1.8365128305317,12.2,10.7686808686736));
#223084=CARTESIAN_POINT('Ctrl Pts',(1.83465627373659,12.2,10.7652648208643));
#223085=CARTESIAN_POINT('Ctrl Pts',(1.83281237576783,12.2,10.7618586999606));
#223086=CARTESIAN_POINT('Ctrl Pts',(1.83096847754783,12.2,10.7584525785929));
#223087=CARTESIAN_POINT('Ctrl Pts',(1.82913724192538,12.2,10.7550563833771));
#223088=CARTESIAN_POINT('Ctrl Pts',(1.82731864099423,12.2,10.7516702484713));
#223089=CARTESIAN_POINT('Ctrl Pts',(1.82550004031086,12.2,10.7482841140269));
#223090=CARTESIAN_POINT('Ctrl Pts',(1.82369407698697,12.2,10.7449080381008));
#223091=CARTESIAN_POINT('Ctrl Pts',(1.82190072618828,12.2,10.7415421590419));
#223092=CARTESIAN_POINT('Ctrl Pts',(1.82010737514524,12.2,10.7381762795244));
#223093=CARTESIAN_POINT('Ctrl Pts',(1.81832663587978,12.2,10.7348205943326));
#223094=CARTESIAN_POINT('Ctrl Pts',(1.81655848475172,12.2,10.7314752420396));
#223095=CARTESIAN_POINT('Ctrl Pts',(1.81479033386458,12.2,10.7281298902024));
#223096=CARTESIAN_POINT('Ctrl Pts',(1.81303477018419,12.2,10.7247948705063));
#223097=CARTESIAN_POINT('Ctrl Pts',(1.81129176865916,12.2,10.7214703202218));
#223098=CARTESIAN_POINT('Ctrl Pts',(1.80954876689666,12.2,10.7181457694843));
#223099=CARTESIAN_POINT('Ctrl Pts',(1.80781832723848,12.2,10.7148316879288));
#223100=CARTESIAN_POINT('Ctrl Pts',(1.80610042353458,12.2,10.7115282164717));
#223101=CARTESIAN_POINT('Ctrl Pts',(1.80438252006474,12.2,10.7082247454647));
#223102=CARTESIAN_POINT('Ctrl Pts',(1.80267715204844,12.2,10.7049318841117));
#223103=CARTESIAN_POINT('Ctrl Pts',(1.80098429321228,12.2,10.7016497709929));
#223104=CARTESIAN_POINT('Ctrl Pts',(1.79929143414546,12.2,10.6983676574269));
#223105=CARTESIAN_POINT('Ctrl Pts',(1.79761108396485,12.2,10.6950962926355));
#223106=CARTESIAN_POINT('Ctrl Pts',(1.795943216097,12.2,10.6918358199585));
#223107=CARTESIAN_POINT('Ctrl Pts',(1.7942753484564,12.2,10.6885753477258));
#223108=CARTESIAN_POINT('Ctrl Pts',(1.79261996030214,12.2,10.6853257658186));
#223109=CARTESIAN_POINT('Ctrl Pts',(1.79097702676852,12.2,10.6820872188045));
#223110=CARTESIAN_POINT('Ctrl Pts',(1.78933409301105,12.2,10.6788486713491));
#223111=CARTESIAN_POINT('Ctrl Pts',(1.78770361273316,12.2,10.6756211567431));
#223112=CARTESIAN_POINT('Ctrl Pts',(1.7860855557488,12.2,10.6724048219978));
#223113=CARTESIAN_POINT('Ctrl Pts',(1.7844674989849,12.2,10.6691884876906));
#223114=CARTESIAN_POINT('Ctrl Pts',(1.78286186607308,12.2,10.66598333144));
#223115=CARTESIAN_POINT('Ctrl Pts',(1.7812686290354,12.2,10.6627894992555));
#223116=CARTESIAN_POINT('Ctrl Pts',(1.77967539178064,12.2,10.6595956666358));
#223117=CARTESIAN_POINT('Ctrl Pts',(1.77809454787428,12.2,10.6564131581117));
#223118=CARTESIAN_POINT('Ctrl Pts',(1.77652606823323,12.2,10.6532421227166));
#223119=CARTESIAN_POINT('Ctrl Pts',(1.77495758859218,12.2,10.6500710873215));
#223120=CARTESIAN_POINT('Ctrl Pts',(1.77340147341368,12.2,10.6469115219806));
#223121=CARTESIAN_POINT('Ctrl Pts',(1.7718576909975,12.2,10.6437635779769));
#223122=CARTESIAN_POINT('Ctrl Pts',(1.77031390879166,12.2,10.6406156344022));
#223123=CARTESIAN_POINT('Ctrl Pts',(1.76878245874758,12.2,10.6374793094831));
#223124=CARTESIAN_POINT('Ctrl Pts',(1.76726331047594,12.2,10.6343547565021));
#223125=CARTESIAN_POINT('Ctrl Pts',(1.76574416199731,12.2,10.6312302030953));
#223126=CARTESIAN_POINT('Ctrl Pts',(1.76423731439687,12.2,10.6281174196274));
#223127=CARTESIAN_POINT('Ctrl Pts',(1.76274273520554,12.2,10.6250165584596));
#223128=CARTESIAN_POINT('Ctrl Pts',(1.76124815621784,12.2,10.6219156977143));
#223129=CARTESIAN_POINT('Ctrl Pts',(1.75976584454525,12.2,10.6188267593453));
#223130=CARTESIAN_POINT('Ctrl Pts',(1.75829576888686,12.2,10.6157498964849));
#223131=CARTESIAN_POINT('Ctrl Pts',(1.75682569302816,12.2,10.6126730332053));
#223132=CARTESIAN_POINT('Ctrl Pts',(1.75536785107626,12.2,10.6096082452749));
#223133=CARTESIAN_POINT('Ctrl Pts',(1.75392220931519,12.2,10.6065556866237));
#223134=CARTESIAN_POINT('Ctrl Pts',(1.7524765677511,12.2,10.6035031283885));
#223135=CARTESIAN_POINT('Ctrl Pts',(1.75104312720914,12.2,10.6004628009175));
#223136=CARTESIAN_POINT('Ctrl Pts',(1.74962185215787,12.2,10.5974348594976));
#223137=CARTESIAN_POINT('Ctrl Pts',(1.74784525819854,12.2,10.5936499324133));
#223138=CARTESIAN_POINT('Ctrl Pts',(1.74608767042026,12.2,10.5898843590294));
#223139=CARTESIAN_POINT('Ctrl Pts',(1.74434902236372,12.2,10.5861384477784));
#223140=CARTESIAN_POINT('Ctrl Pts',(1.74261037430718,12.2,10.5823925365274));
#223141=CARTESIAN_POINT('Ctrl Pts',(1.74089066348638,12.2,10.5786662883744));
#223142=CARTESIAN_POINT('Ctrl Pts',(1.73918981799249,12.2,10.5749600155103));
#223143=CARTESIAN_POINT('Ctrl Pts',(1.73748897249861,12.2,10.5712537426462));
#223144=CARTESIAN_POINT('Ctrl Pts',(1.73580699238881,12.2,10.5675674460222));
#223145=CARTESIAN_POINT('Ctrl Pts',(1.73414380349989,12.2,10.5639014415083));
#223146=CARTESIAN_POINT('Ctrl Pts',(1.73248061461097,12.2,10.5602354369943));
#223147=CARTESIAN_POINT('Ctrl Pts',(1.73083621547212,12.2,10.5565897258499));
#223148=CARTESIAN_POINT('Ctrl Pts',(1.7292105307499,12.2,10.5529646287666));
#223149=CARTESIAN_POINT('Ctrl Pts',(1.72758484602768,12.2,10.5493395316833));
#223150=CARTESIAN_POINT('Ctrl Pts',(1.7259778751062,12.2,10.545735047442));
#223151=CARTESIAN_POINT('Ctrl Pts',(1.7243895380157,12.2,10.542151505273));
#223152=CARTESIAN_POINT('Ctrl Pts',(1.7228012009252,12.2,10.538567963104));
#223153=CARTESIAN_POINT('Ctrl Pts',(1.72123149925315,12.2,10.5350053598118));
#223154=CARTESIAN_POINT('Ctrl Pts',(1.71968035036523,12.2,10.5314640272435));
#223155=CARTESIAN_POINT('Ctrl Pts',(1.71812920147731,12.2,10.5279226946751));
#223156=CARTESIAN_POINT('Ctrl Pts',(1.71659660646114,12.2,10.5244026342868));
#223157=CARTESIAN_POINT('Ctrl Pts',(1.71508248014265,12.2,10.5209041782463));
#223158=CARTESIAN_POINT('Ctrl Pts',(1.71356835382416,12.2,10.5174057222057));
#223159=CARTESIAN_POINT('Ctrl Pts',(1.71207269717323,12.2,10.51392887217));
#223160=CARTESIAN_POINT('Ctrl Pts',(1.71059542404514,12.2,10.5104739667906));
#223161=CARTESIAN_POINT('Ctrl Pts',(1.70911815091704,12.2,10.5070190614112));
#223162=CARTESIAN_POINT('Ctrl Pts',(1.70765926097109,12.2,10.5035861014465));
#223163=CARTESIAN_POINT('Ctrl Pts',(1.70621866611147,12.2,10.5001754328372));
#223164=CARTESIAN_POINT('Ctrl Pts',(1.70477807125186,12.2,10.4967647642279));
#223165=CARTESIAN_POINT('Ctrl Pts',(1.70335576950365,12.2,10.4933763843634));
#223166=CARTESIAN_POINT('Ctrl Pts',(1.70195167228292,12.2,10.4900106450597));
#223167=CARTESIAN_POINT('Ctrl Pts',(1.70054757521522,12.2,10.4866449061229));
#223168=CARTESIAN_POINT('Ctrl Pts',(1.69916168149787,12.2,10.4833018078242));
#223169=CARTESIAN_POINT('Ctrl Pts',(1.69779389768714,12.2,10.4799817031842));
#223170=CARTESIAN_POINT('Ctrl Pts',(1.69642611372733,12.2,10.4766615981823));
#223171=CARTESIAN_POINT('Ctrl Pts',(1.69507643882556,12.2,10.4733644883078));
#223172=CARTESIAN_POINT('Ctrl Pts',(1.69374477736575,12.2,10.4700907346948));
#223173=CARTESIAN_POINT('Ctrl Pts',(1.69241311590595,12.2,10.4668169810818));
#223174=CARTESIAN_POINT('Ctrl Pts',(1.69109946828857,12.2,10.4635665797207));
#223175=CARTESIAN_POINT('Ctrl Pts',(1.68980373412538,12.2,10.4603399018496));
#223176=CARTESIAN_POINT('Ctrl Pts',(1.6885079999622,12.2,10.4571132239785));
#223177=CARTESIAN_POINT('Ctrl Pts',(1.68723017946111,12.2,10.4539102665425));
#223178=CARTESIAN_POINT('Ctrl Pts',(1.68597017126575,12.2,10.450731400708));
#223179=CARTESIAN_POINT('Ctrl Pts',(1.68471016307039,12.2,10.4475525348734));
#223180=CARTESIAN_POINT('Ctrl Pts',(1.68346796659213,12.2,10.4443977617894));
#223181=CARTESIAN_POINT('Ctrl Pts',(1.68224347756342,12.2,10.4412674584548));
#223182=CARTESIAN_POINT('Ctrl Pts',(1.68077409078236,12.2,10.4375110945897));
#223183=CARTESIAN_POINT('Ctrl Pts',(1.67933020167139,12.2,10.4337899652535));
#223184=CARTESIAN_POINT('Ctrl Pts',(1.67791162388786,12.2,10.430104736385));
#223185=CARTESIAN_POINT('Ctrl Pts',(1.67649304597548,12.2,10.4264195071816));
#223186=CARTESIAN_POINT('Ctrl Pts',(1.67509978025723,12.2,10.4227701775234));
#223187=CARTESIAN_POINT('Ctrl Pts',(1.67373163143378,12.2,10.4191574215782));
#223188=CARTESIAN_POINT('Ctrl Pts',(1.6723634827346,12.2,10.4155446659611));
#223189=CARTESIAN_POINT('Ctrl Pts',(1.67102045290033,12.2,10.4119684863308));
#223190=CARTESIAN_POINT('Ctrl Pts',(1.66970234002549,12.2,10.4084295715265));
#223191=CARTESIAN_POINT('Ctrl Pts',(1.66838422715066,12.2,10.4048906567222));
#223192=CARTESIAN_POINT('Ctrl Pts',(1.66709103268544,12.2,10.4013890058459));
#223193=CARTESIAN_POINT('Ctrl Pts',(1.6658225496465,12.2,10.3979253233858));
#223194=CARTESIAN_POINT('Ctrl Pts',(1.66455406649235,12.2,10.3944616406111));
#223195=CARTESIAN_POINT('Ctrl Pts',(1.66331029366625,12.2,10.3910359265238));
#223196=CARTESIAN_POINT('Ctrl Pts',(1.66209101762368,12.2,10.3876488976724));
#223197=CARTESIAN_POINT('Ctrl Pts',(1.66087174169186,12.2,10.3842618691286));
#223198=CARTESIAN_POINT('Ctrl Pts',(1.65967696619903,12.2,10.380913527188));
#223199=CARTESIAN_POINT('Ctrl Pts',(1.65850646349157,12.2,10.3776046037249));
#223200=CARTESIAN_POINT('Ctrl Pts',(1.65733596078412,12.2,10.3742956802619));
#223201=CARTESIAN_POINT('Ctrl Pts',(1.65618973598353,12.2,10.3710261756837));
#223202=CARTESIAN_POINT('Ctrl Pts',(1.65506755788352,12.2,10.3677968380541));
#223203=CARTESIAN_POINT('Ctrl Pts',(1.65394537968158,12.2,10.3645675001311));
#223204=CARTESIAN_POINT('Ctrl Pts',(1.65284724727307,12.2,10.3613783289672));
#223205=CARTESIAN_POINT('Ctrl Pts',(1.65177292788281,12.2,10.3582300893818));
#223206=CARTESIAN_POINT('Ctrl Pts',(1.65069860859013,12.2,10.3550818500823));
#223207=CARTESIAN_POINT('Ctrl Pts',(1.64964809727928,12.2,10.3519745432386));
#223208=CARTESIAN_POINT('Ctrl Pts',(1.64862115398323,12.2,10.3489089490166));
#223209=CARTESIAN_POINT('Ctrl Pts',(1.64759421068719,12.2,10.3458433547945));
#223210=CARTESIAN_POINT('Ctrl Pts',(1.64659083092614,12.2,10.3428194731649));
#223211=CARTESIAN_POINT('Ctrl Pts',(1.6456107655781,12.2,10.3398381047884));
#223212=CARTESIAN_POINT('Ctrl Pts',(1.64463070014104,12.2,10.3368567361412));
#223213=CARTESIAN_POINT('Ctrl Pts',(1.64367394661412,12.2,10.3339178787225));
#223214=CARTESIAN_POINT('Ctrl Pts',(1.64274024339814,12.2,10.331022351401));
#223215=CARTESIAN_POINT('Ctrl Pts',(1.64180654026696,12.2,10.3281268243424));
#223216=CARTESIAN_POINT('Ctrl Pts',(1.64089588844622,12.2,10.3252746264176));
#223217=CARTESIAN_POINT('Ctrl Pts',(1.6400080142245,12.2,10.322466595257));
#223218=CARTESIAN_POINT('Ctrl Pts',(1.63912014000279,12.2,10.3196585640964));
#223219=CARTESIAN_POINT('Ctrl Pts',(1.63825504561629,12.2,10.3168946979098));
#223220=CARTESIAN_POINT('Ctrl Pts',(1.63741244931259,12.2,10.3141758549233));
#223221=CARTESIAN_POINT('Ctrl Pts',(1.63656985293235,12.2,10.3114570116898));
#223222=CARTESIAN_POINT('Ctrl Pts',(1.6357497546799,12.2,10.3087831905119));
#223223=CARTESIAN_POINT('Ctrl Pts',(1.63495186338794,12.2,10.3061552694551));
#223224=CARTESIAN_POINT('Ctrl Pts',(1.63415397216845,12.2,10.3035273486371));
#223225=CARTESIAN_POINT('Ctrl Pts',(1.63337828878057,12.2,10.3009453276011));
#223226=CARTESIAN_POINT('Ctrl Pts',(1.63262451147558,12.2,10.2984101058619));
#223227=CARTESIAN_POINT('Ctrl Pts',(1.6318707341706,12.2,10.2958748841228));
#223228=CARTESIAN_POINT('Ctrl Pts',(1.63113886235551,12.2,10.2933864594548));
#223229=CARTESIAN_POINT('Ctrl Pts',(1.63042858579704,12.2,10.2909457576248));
#223230=CARTESIAN_POINT('Ctrl Pts',(1.62971830923857,12.2,10.2885050557947));
#223231=CARTESIAN_POINT('Ctrl Pts',(1.62902962534985,12.2,10.2861120735653));
#223232=CARTESIAN_POINT('Ctrl Pts',(1.62836221553933,12.2,10.2837677582304));
#223233=CARTESIAN_POINT('Ctrl Pts',(1.62769480566818,12.2,10.2814234426827));
#223234=CARTESIAN_POINT('Ctrl Pts',(1.62704866405742,12.2,10.2791277938896));
#223235=CARTESIAN_POINT('Ctrl Pts',(1.62642346044092,12.2,10.2768817823527));
#223236=CARTESIAN_POINT('Ctrl Pts',(1.62569405630686,12.2,10.2742614358656));
#223237=CARTESIAN_POINT('Ctrl Pts',(1.62499314804473,12.2,10.2717086493813));
#223238=CARTESIAN_POINT('Ctrl Pts',(1.62432018577945,12.2,10.2692250127819));
#223239=CARTESIAN_POINT('Ctrl Pts',(1.62374336091328,12.2,10.2670961811625));
#223240=CARTESIAN_POINT('Ctrl Pts',(1.62318706408245,12.2,10.2650181509895));
#223241=CARTESIAN_POINT('Ctrl Pts',(1.62265093722078,12.2,10.2629919546313));
#223242=CARTESIAN_POINT('Ctrl Pts',(1.6221148104078,12.2,10.2609657584572));
#223243=CARTESIAN_POINT('Ctrl Pts',(1.62159885033441,12.2,10.2589913938565));
#223244=CARTESIAN_POINT('Ctrl Pts',(1.6211026825168,12.2,10.2570699217508));
#223245=CARTESIAN_POINT('Ctrl Pts',(1.62027811736746,12.2,10.2538766897886));
#223246=CARTESIAN_POINT('Ctrl Pts',(1.61950821818824,12.2,10.2508295185277));
#223247=CARTESIAN_POINT('Ctrl Pts',(1.61879117999994,12.2,10.247933457));
#223248=CARTESIAN_POINT('Ctrl Pts',(1.61879117999994,15.2,10.247933457));
#223249=CARTESIAN_POINT('Ctrl Pts',(1.61922057460978,15.2,10.2496677484646));
#223250=CARTESIAN_POINT('Ctrl Pts',(1.61966892470867,15.2,10.2514562343097));
#223251=CARTESIAN_POINT('Ctrl Pts',(1.62013662093202,15.2,10.2532978203482));
#223252=CARTESIAN_POINT('Ctrl Pts',(1.62060657262298,15.2,10.2551482874454));
#223253=CARTESIAN_POINT('Ctrl Pts',(1.62109605716988,15.2,10.2570523692153));
#223254=CARTESIAN_POINT('Ctrl Pts',(1.62160546180757,15.2,10.2590089854226));
#223255=CARTESIAN_POINT('Ctrl Pts',(1.62211486639899,15.2,10.2609656014523));
#223256=CARTESIAN_POINT('Ctrl Pts',(1.62264418692822,15.2,10.2629747533165));
#223257=CARTESIAN_POINT('Ctrl Pts',(1.62319380049157,15.2,10.2650353904916));
#223258=CARTESIAN_POINT('Ctrl Pts',(1.62374341405492,15.2,10.2670960276667));
#223259=CARTESIAN_POINT('Ctrl Pts',(1.62431331645265,15.2,10.2692081511476));
#223260=CARTESIAN_POINT('Ctrl Pts',(1.6249038679595,15.2,10.2713707423408));
#223261=CARTESIAN_POINT('Ctrl Pts',(1.62549441951999,15.2,10.2735333337305));
#223262=CARTESIAN_POINT('Ctrl Pts',(1.62610561697461,15.2,10.2757463899032));
#223263=CARTESIAN_POINT('Ctrl Pts',(1.62673780859382,15.2,10.2780089205299));
#223264=CARTESIAN_POINT('Ctrl Pts',(1.62737000015561,15.2,10.280271450951));
#223265=CARTESIAN_POINT('Ctrl Pts',(1.62802318434661,15.2,10.2825834561342));
#223266=CARTESIAN_POINT('Ctrl Pts',(1.62869769474188,15.2,10.2849439668093));
#223267=CARTESIAN_POINT('Ctrl Pts',(1.62937220513716,15.2,10.2873044774844));
#223268=CARTESIAN_POINT('Ctrl Pts',(1.63006804094624,15.2,10.2897134965992));
#223269=CARTESIAN_POINT('Ctrl Pts',(1.63078552516923,15.2,10.2921700810912));
#223270=CARTESIAN_POINT('Ctrl Pts',(1.63150300945739,15.2,10.2946266658064));
#223271=CARTESIAN_POINT('Ctrl Pts',(1.63224214013989,15.2,10.2971308160524));
#223272=CARTESIAN_POINT('Ctrl Pts',(1.63300322684954,15.2,10.299681613028));
#223273=CARTESIAN_POINT('Ctrl Pts',(1.63376431349005,15.2,10.3022324097718));
#223274=CARTESIAN_POINT('Ctrl Pts',(1.63454735977218,15.2,10.3048298539799));
#223275=CARTESIAN_POINT('Ctrl Pts',(1.63535266107722,15.2,10.3074730516358));
#223276=CARTESIAN_POINT('Ctrl Pts',(1.63629217931521,15.2,10.3105567823945));
#223277=CARTESIAN_POINT('Ctrl Pts',(1.63726199062046,15.2,10.3137027831072));
#223278=CARTESIAN_POINT('Ctrl Pts',(1.63826255556839,15.2,10.3169096742995));
#223279=CARTESIAN_POINT('Ctrl Pts',(1.6391201826221,15.2,10.319658438036));
#223280=CARTESIAN_POINT('Ctrl Pts',(1.64000040165602,15.2,10.3224519354642));
#223281=CARTESIAN_POINT('Ctrl Pts',(1.64090349104089,15.2,10.3252893184464));
#223282=CARTESIAN_POINT('Ctrl Pts',(1.64210761024805,15.2,10.3290724958419));
#223283=CARTESIAN_POINT('Ctrl Pts',(1.64335238876196,15.2,10.3329336878841));
#223284=CARTESIAN_POINT('Ctrl Pts',(1.64463846075034,15.2,10.3368709372929));
#223285=CARTESIAN_POINT('Ctrl Pts',(1.64560301471972,15.2,10.3398238742825));
#223286=CARTESIAN_POINT('Ctrl Pts',(1.64659079360766,15.2,10.3428195926301));
#223287=CARTESIAN_POINT('Ctrl Pts',(1.64760205565322,15.2,10.3458572888512));
#223288=CARTESIAN_POINT('Ctrl Pts',(1.64861331779063,15.2,10.3488949853482));
#223289=CARTESIAN_POINT('Ctrl Pts',(1.64964806011433,15.2,10.3519746593173));
#223290=CARTESIAN_POINT('Ctrl Pts',(1.65070653509028,15.2,10.3550955238234));
#223291=CARTESIAN_POINT('Ctrl Pts',(1.65176500997008,15.2,10.3582163880461));
#223292=CARTESIAN_POINT('Ctrl Pts',(1.65284721338551,15.2,10.3613784430697));
#223293=CARTESIAN_POINT('Ctrl Pts',(1.65395338651708,15.2,10.364580917468));
#223294=CARTESIAN_POINT('Ctrl Pts',(1.65524392190422,15.2,10.3683171377934));
#223295=CARTESIAN_POINT('Ctrl Pts',(1.65656708212579,15.2,10.3721083743684));
#223296=CARTESIAN_POINT('Ctrl Pts',(1.65792323434328,15.2,10.3759534308758));
#223297=CARTESIAN_POINT('Ctrl Pts',(1.65908565046937,15.2,10.3792491934255));
#223298=CARTESIAN_POINT('Ctrl Pts',(1.66027230438057,15.2,10.3825844995836));
#223299=CARTESIAN_POINT('Ctrl Pts',(1.66148342025879,15.2,10.3859586112265));
#223300=CARTESIAN_POINT('Ctrl Pts',(1.66269453613701,15.2,10.3893327228693));
#223301=CARTESIAN_POINT('Ctrl Pts',(1.66393011306989,15.2,10.3927456434142));
#223302=CARTESIAN_POINT('Ctrl Pts',(1.66519036593965,15.2,10.396196649037));
#223303=CARTESIAN_POINT('Ctrl Pts',(1.66645061892389,15.2,10.3996476549733));
#223304=CARTESIAN_POINT('Ctrl Pts',(1.66773554612792,15.2,10.4031367481145));
#223305=CARTESIAN_POINT('Ctrl Pts',(1.66904535911768,15.2,10.4066632228927));
#223306=CARTESIAN_POINT('Ctrl Pts',(1.67035517198846,15.2,10.4101896973504));
#223307=CARTESIAN_POINT('Ctrl Pts',(1.67168986849743,15.2,10.4137535505506));
#223308=CARTESIAN_POINT('Ctrl Pts',(1.67304964953245,15.2,10.4173540951713));
#223309=CARTESIAN_POINT('Ctrl Pts',(1.67440943056746,15.2,10.420954639792));
#223310=CARTESIAN_POINT('Ctrl Pts',(1.67579429731715,15.2,10.4245918722932));
#223311=CARTESIAN_POINT('Ctrl Pts',(1.67720444318149,15.2,10.4282651160749));
#223312=CARTESIAN_POINT('Ctrl Pts',(1.67861458904582,15.2,10.4319383598565));
#223313=CARTESIAN_POINT('Ctrl Pts',(1.68005001507881,15.2,10.4356476154802));
#223314=CARTESIAN_POINT('Ctrl Pts',(1.68151090785734,15.2,10.4393922153418));
#223315=CARTESIAN_POINT('Ctrl Pts',(1.68272831855034,15.2,10.4425127153398));
#223316=CARTESIAN_POINT('Ctrl Pts',(1.68396341538748,15.2,10.4456577605763));
#223317=CARTESIAN_POINT('Ctrl Pts',(1.68521630288603,15.2,10.4488269746021));
#223318=CARTESIAN_POINT('Ctrl Pts',(1.68646919038459,15.2,10.4519961886279));
#223319=CARTESIAN_POINT('Ctrl Pts',(1.6877398689539,15.2,10.4551895687675));
#223320=CARTESIAN_POINT('Ctrl Pts',(1.68902844214205,15.2,10.4584067439265));
#223321=CARTESIAN_POINT('Ctrl Pts',(1.69031701533019,15.2,10.4616239190857));
#223322=CARTESIAN_POINT('Ctrl Pts',(1.69162348135319,15.2,10.4648648897266));
#223323=CARTESIAN_POINT('Ctrl Pts',(1.69294794121339,15.2,10.4681292872949));
#223324=CARTESIAN_POINT('Ctrl Pts',(1.69427240107359,15.2,10.4713936848632));
#223325=CARTESIAN_POINT('Ctrl Pts',(1.69561485536754,15.2,10.4746815102126));
#223326=CARTESIAN_POINT('Ctrl Pts',(1.69697539939436,15.2,10.4779924020169));
#223327=CARTESIAN_POINT('Ctrl Pts',(1.69860805216722,15.2,10.4819654720377));
#223328=CARTESIAN_POINT('Ctrl Pts',(1.70026675567926,15.2,10.485971758042));
#223329=CARTESIAN_POINT('Ctrl Pts',(1.70195167228292,15.2,10.4900106450597));
#223330=CARTESIAN_POINT('Ctrl Pts',(1.70335576950365,15.2,10.4933763843634));
#223331=CARTESIAN_POINT('Ctrl Pts',(1.70477807125186,15.2,10.4967647642279));
#223332=CARTESIAN_POINT('Ctrl Pts',(1.70621866611148,15.2,10.5001754328372));
#223333=CARTESIAN_POINT('Ctrl Pts',(1.70765926097109,15.2,10.5035861014465));
#223334=CARTESIAN_POINT('Ctrl Pts',(1.70911815091707,15.2,10.5070190614112));
#223335=CARTESIAN_POINT('Ctrl Pts',(1.71059542404514,15.2,10.5104739667906));
#223336=CARTESIAN_POINT('Ctrl Pts',(1.71207269717321,15.2,10.51392887217));
#223337=CARTESIAN_POINT('Ctrl Pts',(1.71356835382412,15.2,10.5174057222056));
#223338=CARTESIAN_POINT('Ctrl Pts',(1.71508248014265,15.2,10.5209041782463));
#223339=CARTESIAN_POINT('Ctrl Pts',(1.71659660646118,15.2,10.5244026342869));
#223340=CARTESIAN_POINT('Ctrl Pts',(1.71812920147731,15.2,10.5279226946751));
#223341=CARTESIAN_POINT('Ctrl Pts',(1.71968035036523,15.2,10.5314640272435));
#223342=CARTESIAN_POINT('Ctrl Pts',(1.7215417289631,15.2,10.535713626171));
#223343=CARTESIAN_POINT('Ctrl Pts',(1.7234298242709,15.2,10.5399938533054));
#223344=CARTESIAN_POINT('Ctrl Pts',(1.72534477678284,15.2,10.5443041404801));
#223345=CARTESIAN_POINT('Ctrl Pts',(1.72694057060076,15.2,10.5478960465895));
#223346=CARTESIAN_POINT('Ctrl Pts',(1.72855501442117,15.2,10.5515088274653));
#223347=CARTESIAN_POINT('Ctrl Pts',(1.73018818754462,15.2,10.5551421577414));
#223348=CARTESIAN_POINT('Ctrl Pts',(1.73182136066807,15.2,10.5587754880174));
#223349=CARTESIAN_POINT('Ctrl Pts',(1.73347326351627,15.2,10.5624293675211));
#223350=CARTESIAN_POINT('Ctrl Pts',(1.7351439722647,15.2,10.5661034762694));
#223351=CARTESIAN_POINT('Ctrl Pts',(1.73681468101314,15.2,10.5697775850177));
#223352=CARTESIAN_POINT('Ctrl Pts',(1.73850419488427,15.2,10.573471922718));
#223353=CARTESIAN_POINT('Ctrl Pts',(1.74021258955164,15.2,10.5771861733188));
#223354=CARTESIAN_POINT('Ctrl Pts',(1.7422626632642,15.2,10.5816432742827));
#223355=CARTESIAN_POINT('Ctrl Pts',(1.74433992322938,15.2,10.5861290490857));
#223356=CARTESIAN_POINT('Ctrl Pts',(1.74644449501264,15.2,10.5906429597503));
#223357=CARTESIAN_POINT('Ctrl Pts',(1.74784754267698,15.2,10.5936522331167));
#223358=CARTESIAN_POINT('Ctrl Pts',(1.74926272992304,15.2,10.5966740105009));
#223359=CARTESIAN_POINT('Ctrl Pts',(1.75069008958332,15.2,10.599708135252));
#223360=CARTESIAN_POINT('Ctrl Pts',(1.75211744943807,15.2,10.6027422604165));
#223361=CARTESIAN_POINT('Ctrl Pts',(1.75355698539958,15.2,10.605788733165));
#223362=CARTESIAN_POINT('Ctrl Pts',(1.75500872871896,15.2,10.6088473966522));
#223363=CARTESIAN_POINT('Ctrl Pts',(1.75646047184052,15.2,10.6119060597227));
#223364=CARTESIAN_POINT('Ctrl Pts',(1.7579244248258,15.2,10.6149769138342));
#223365=CARTESIAN_POINT('Ctrl Pts',(1.75940061987099,15.2,10.618059805248));
#223366=CARTESIAN_POINT('Ctrl Pts',(1.76087681511732,15.2,10.6211426970819));
#223367=CARTESIAN_POINT('Ctrl Pts',(1.76236525520398,15.2,10.6242376254395));
#223368=CARTESIAN_POINT('Ctrl Pts',(1.7638659708977,15.2,10.627344438054));
#223369=CARTESIAN_POINT('Ctrl Pts',(1.7657418654126,15.2,10.6312279536106));
#223370=CARTESIAN_POINT('Ctrl Pts',(1.76763694155852,15.2,10.6351300377746));
#223371=CARTESIAN_POINT('Ctrl Pts',(1.76955126373886,15.2,10.6390503967218));
#223372=CARTESIAN_POINT('Ctrl Pts',(1.77108272135793,15.2,10.6421866836231));
#223373=CARTESIAN_POINT('Ctrl Pts',(1.77262649551749,15.2,10.6453346638175));
#223374=CARTESIAN_POINT('Ctrl Pts',(1.77418261838946,15.2,10.6484941912251));
#223375=CARTESIAN_POINT('Ctrl Pts',(1.77573874147345,15.2,10.6516537190632));
#223376=CARTESIAN_POINT('Ctrl Pts',(1.77730721299229,15.2,10.6548247907083));
#223377=CARTESIAN_POINT('Ctrl Pts',(1.77888806407925,15.2,10.6580072619936));
#223378=CARTESIAN_POINT('Ctrl Pts',(1.78086412783026,15.2,10.6619853508834));
#223379=CARTESIAN_POINT('Ctrl Pts',(1.78285953437075,15.2,10.6659812489754));
#223380=CARTESIAN_POINT('Ctrl Pts',(1.78487434245885,15.2,10.6699946697326));
#223381=CARTESIAN_POINT('Ctrl Pts',(1.78648618879755,15.2,10.6732054060759));
#223382=CARTESIAN_POINT('Ctrl Pts',(1.78811045181469,15.2,10.6764273569729));
#223383=CARTESIAN_POINT('Ctrl Pts',(1.78974716062455,15.2,10.6796603784858));
#223384=CARTESIAN_POINT('Ctrl Pts',(1.79138386965741,15.2,10.6828934004391));
#223385=CARTESIAN_POINT('Ctrl Pts',(1.79303302547503,15.2,10.6861374924019));
#223386=CARTESIAN_POINT('Ctrl Pts',(1.79469465517752,15.2,10.6893925105245));
#223387=CARTESIAN_POINT('Ctrl Pts',(1.79760250681729,15.2,10.6950887915737));
#223388=CARTESIAN_POINT('Ctrl Pts',(1.80054856028695,15.2,10.7008185365223));
#223389=CARTESIAN_POINT('Ctrl Pts',(1.80353296615441,15.2,10.7065809837032));
#223390=CARTESIAN_POINT('Ctrl Pts',(1.80566468476394,15.2,10.7106970176603));
#223391=CARTESIAN_POINT('Ctrl Pts',(1.80781596826203,15.2,10.7148297386586));
#223392=CARTESIAN_POINT('Ctrl Pts',(1.80998687173261,15.2,10.7189788719906));
#223393=CARTESIAN_POINT('Ctrl Pts',(1.81172359460372,15.2,10.722298178837));
#223394=CARTESIAN_POINT('Ctrl Pts',(1.81347287244424,15.2,10.7256279905661));
#223395=CARTESIAN_POINT('Ctrl Pts',(1.81523473149277,15.2,10.7289681679856));
#223396=CARTESIAN_POINT('Ctrl Pts',(1.81699659030124,15.2,10.7323083449499));
#223397=CARTESIAN_POINT('Ctrl Pts',(1.81877102999677,15.2,10.7356588894401));
#223398=CARTESIAN_POINT('Ctrl Pts',(1.82055807668272,15.2,10.7390196624421));
#223399=CARTESIAN_POINT('Ctrl Pts',(1.82279188522277,15.2,10.743220629038));
#223400=CARTESIAN_POINT('Ctrl Pts',(1.82504538995417,15.2,10.7474375800698));
#223401=CARTESIAN_POINT('Ctrl Pts',(1.82731864099423,15.2,10.7516702484713));
#223402=CARTESIAN_POINT('Ctrl Pts',(1.82959189203429,15.2,10.7559029168728));
#223403=CARTESIAN_POINT('Ctrl Pts',(1.83188488669511,15.2,10.7601513044209));
#223404=CARTESIAN_POINT('Ctrl Pts',(1.83419767298982,15.2,10.7644151495634));
#223405=CARTESIAN_POINT('Ctrl Pts',(1.83651045928452,15.2,10.7686789947058));
#223406=CARTESIAN_POINT('Ctrl Pts',(1.83884303493055,15.2,10.7729582973311));
#223407=CARTESIAN_POINT('Ctrl Pts',(1.84119544763783,15.2,10.7772527972608));
#223408=CARTESIAN_POINT('Ctrl Pts',(1.84354786034511,15.2,10.7815472971906));
#223409=CARTESIAN_POINT('Ctrl Pts',(1.84592010702239,15.2,10.7858569951569));
#223410=CARTESIAN_POINT('Ctrl Pts',(1.84831223236857,15.2,10.7901816352255));
#223411=CARTESIAN_POINT('Ctrl Pts',(1.85022593274982,15.2,10.793641347469));
#223412=CARTESIAN_POINT('Ctrl Pts',(1.85215235603877,15.2,10.7971106232378));
#223413=CARTESIAN_POINT('Ctrl Pts',(1.85409152179802,15.2,10.8005893322131));
#223414=CARTESIAN_POINT('Ctrl Pts',(1.85603068729305,15.2,10.8040680407145));
#223415=CARTESIAN_POINT('Ctrl Pts',(1.85798259600919,15.2,10.8075561819118));
#223416=CARTESIAN_POINT('Ctrl Pts',(1.85994726934773,15.2,10.8110536281808));
#223417=CARTESIAN_POINT('Ctrl Pts',(1.86289427975707,15.2,10.8162997982991));
#223418=CARTESIAN_POINT('Ctrl Pts',(1.86587000840336,15.2,10.8215669023867));
#223419=CARTESIAN_POINT('Ctrl Pts',(1.86887452481906,15.2,10.826854511843));
#223420=CARTESIAN_POINT('Ctrl Pts',(1.87087753548994,15.2,10.8303795843335));
#223421=CARTESIAN_POINT('Ctrl Pts',(1.87289333909252,15.2,10.8339137703478));
#223422=CARTESIAN_POINT('Ctrl Pts',(1.8749219570925,15.2,10.837456944002));
#223423=CARTESIAN_POINT('Ctrl Pts',(1.87745772979979,15.2,10.8418859114318));
#223424=CARTESIAN_POINT('Ctrl Pts',(1.88001352413129,15.2,10.8463289210273));
#223425=CARTESIAN_POINT('Ctrl Pts',(1.88258937449016,15.2,10.8507857302142));
#223426=CARTESIAN_POINT('Ctrl Pts',(1.88465005488956,15.2,10.854351177758));
#223427=CARTESIAN_POINT('Ctrl Pts',(1.88672357302046,15.2,10.8579254567091));
#223428=CARTESIAN_POINT('Ctrl Pts',(1.88880994535769,15.2,10.8615084436274));
#223429=CARTESIAN_POINT('Ctrl Pts',(1.89141791063708,15.2,10.8659871770313));
#223430=CARTESIAN_POINT('Ctrl Pts',(1.89404596208352,15.2,10.8704795155104));
#223431=CARTESIAN_POINT('Ctrl Pts',(1.89669413236295,15.2,10.874985220581));
#223432=CARTESIAN_POINT('Ctrl Pts',(1.8988126684133,15.2,10.8785897843427));
#223433=CARTESIAN_POINT('Ctrl Pts',(1.90094408130573,15.2,10.8822029034549));
#223434=CARTESIAN_POINT('Ctrl Pts',(1.90308838797343,15.2,10.8858244547308));
#223435=CARTESIAN_POINT('Ctrl Pts',(1.9052326949333,15.2,10.8894460065001));
#223436=CARTESIAN_POINT('Ctrl Pts',(1.9073898954907,15.2,10.8930759914985));
#223437=CARTESIAN_POINT('Ctrl Pts',(1.90956000638805,15.2,10.8967142890865));
#223438=CARTESIAN_POINT('Ctrl Pts',(1.91173011698973,15.2,10.9003525861788));
#223439=CARTESIAN_POINT('Ctrl Pts',(1.91391313647585,15.2,10.9039991972922));
#223440=CARTESIAN_POINT('Ctrl Pts',(1.9161090817955,15.2,10.9076540004929));
#223441=CARTESIAN_POINT('Ctrl Pts',(1.91885401366945,15.2,10.9122225048673));
#223442=CARTESIAN_POINT('Ctrl Pts',(1.92161914179689,15.2,10.9168038111933));
#223443=CARTESIAN_POINT('Ctrl Pts',(1.92440449694837,15.2,10.9213976872558));
#223444=CARTESIAN_POINT('Ctrl Pts',(1.92718985209986,15.2,10.9259915633183));
#223445=CARTESIAN_POINT('Ctrl Pts',(1.92999543321655,15.2,10.9305980101166));
#223446=CARTESIAN_POINT('Ctrl Pts',(1.93282126925822,15.2,10.9352167992833));
#223447=CARTESIAN_POINT('Ctrl Pts',(1.93621227238501,15.2,10.9407593460819));
#223448=CARTESIAN_POINT('Ctrl Pts',(1.9396324417793,15.2,10.9463196623104));
#223449=CARTESIAN_POINT('Ctrl Pts',(1.94308182690795,15.2,10.9518973604688));
#223450=CARTESIAN_POINT('Ctrl Pts',(1.94538141720259,15.2,10.9556158262454));
#223451=CARTESIAN_POINT('Ctrl Pts',(1.94769399160979,15.2,10.9593420144208));
#223452=CARTESIAN_POINT('Ctrl Pts',(1.9500195626818,15.2,10.9630758140136));
#223453=CARTESIAN_POINT('Ctrl Pts',(1.95292652636337,15.2,10.9677430632503));
#223454=CARTESIAN_POINT('Ctrl Pts',(1.95585379938614,15.2,10.9724222024006));
#223455=CARTESIAN_POINT('Ctrl Pts',(1.95880140619279,15.2,10.9771130077485));
#223456=CARTESIAN_POINT('Ctrl Pts',(1.96115949144534,15.2,10.98086565172));
#223457=CARTESIAN_POINT('Ctrl Pts',(1.96353058975313,15.2,10.9846257640681));
#223458=CARTESIAN_POINT('Ctrl Pts',(1.96591471445402,15.2,10.98839323017));
#223459=CARTESIAN_POINT('Ctrl Pts',(1.96770280806089,15.2,10.9912188298747));
#223460=CARTESIAN_POINT('Ctrl Pts',(1.9694982288234,15.2,10.9940485663524));
#223461=CARTESIAN_POINT('Ctrl Pts',(1.97130098138189,15.2,10.9968823923322));
#223462=CARTESIAN_POINT('Ctrl Pts',(1.9737046516782,15.2,11.0006608273151));
#223463=CARTESIAN_POINT('Ctrl Pts',(1.97612135720634,15.2,11.0044465323071));
#223464=CARTESIAN_POINT('Ctrl Pts',(1.97855110878322,15.2,11.0082393954583));
#223465=CARTESIAN_POINT('Ctrl Pts',(1.98037342230036,15.2,11.0110840425633));
#223466=CARTESIAN_POINT('Ctrl Pts',(1.98220307440052,15.2,11.0139327167931));
#223467=CARTESIAN_POINT('Ctrl Pts',(1.98404007033311,15.2,11.0167853703974));
#223468=CARTESIAN_POINT('Ctrl Pts',(1.98587706626569,15.2,11.0196380240017));
#223469=CARTESIAN_POINT('Ctrl Pts',(1.98772140465066,15.2,11.022494658708));
#223470=CARTESIAN_POINT('Ctrl Pts',(1.98957309171671,15.2,11.0253552259549));
#223471=CARTESIAN_POINT('Ctrl Pts',(1.99142477878276,15.2,11.0282157932017));
#223472=CARTESIAN_POINT('Ctrl Pts',(1.99328381306184,15.2,11.0310802940961));
#223473=CARTESIAN_POINT('Ctrl Pts',(1.99515020007635,15.2,11.0339486825746));
#223474=CARTESIAN_POINT('Ctrl Pts',(1.99763871632174,15.2,11.0377732008935));
#223475=CARTESIAN_POINT('Ctrl Pts',(2.00014030328227,15.2,11.0416046292546));
#223476=CARTESIAN_POINT('Ctrl Pts',(2.00265497147489,15.2,11.0454428597416));
#223477=CARTESIAN_POINT('Ctrl Pts',(2.00454097244804,15.2,11.0483215323454));
#223478=CARTESIAN_POINT('Ctrl Pts',(2.00643433137921,15.2,11.051204031624));
#223479=CARTESIAN_POINT('Ctrl Pts',(2.00833505235117,15.2,11.0540903106854));
#223480=CARTESIAN_POINT('Ctrl Pts',(2.01023577332312,15.2,11.0569765897469));
#223481=CARTESIAN_POINT('Ctrl Pts',(2.01214385577079,15.2,11.0598666490178));
#223482=CARTESIAN_POINT('Ctrl Pts',(2.01405930537938,15.2,11.0627604437235));
#223483=CARTESIAN_POINT('Ctrl Pts',(2.01597475498796,15.2,11.0656542384291));
#223484=CARTESIAN_POINT('Ctrl Pts',(2.01789757131692,15.2,11.0685517685401));
#223485=CARTESIAN_POINT('Ctrl Pts',(2.01982775682912,15.2,11.0714529881425));
#223486=CARTESIAN_POINT('Ctrl Pts',(2.02175794269196,15.2,11.074354208272));
#223487=CARTESIAN_POINT('Ctrl Pts',(2.02369549805691,15.2,11.0772591182608));
#223488=CARTESIAN_POINT('Ctrl Pts',(2.0256404274239,15.2,11.0801676733507));
#223489=CARTESIAN_POINT('Ctrl Pts',(2.02758535643756,15.2,11.0830762279122));
#223490=CARTESIAN_POINT('Ctrl Pts',(2.02953765950087,15.2,11.0859884273068));
#223491=CARTESIAN_POINT('Ctrl Pts',(2.03149733993029,15.2,11.0889042273262));
#223492=CARTESIAN_POINT('Ctrl Pts',(2.03345702035971,15.2,11.0918200273455));
#223493=CARTESIAN_POINT('Ctrl Pts',(2.03542407678109,15.2,11.0947394272122));
#223494=CARTESIAN_POINT('Ctrl Pts',(2.03739851526002,15.2,11.0976623837443));
#223495=CARTESIAN_POINT('Ctrl Pts',(2.04003109977905,15.2,11.1015596589434));
#223496=CARTESIAN_POINT('Ctrl Pts',(2.04267680732835,15.2,11.1054632552255));
#223497=CARTESIAN_POINT('Ctrl Pts',(2.04533564133184,15.2,11.1093730691274));
#223498=CARTESIAN_POINT('Ctrl Pts',(2.0473297672873,15.2,11.1123054302197));
#223499=CARTESIAN_POINT('Ctrl Pts',(2.04933127974491,15.2,11.1152412879131));
#223500=CARTESIAN_POINT('Ctrl Pts',(2.05134017970451,15.2,11.1181805985907));
#223501=CARTESIAN_POINT('Ctrl Pts',(2.05468834581724,15.2,11.1230794490081));
#223502=CARTESIAN_POINT('Ctrl Pts',(2.05805703619151,15.2,11.1279878930202));
#223503=CARTESIAN_POINT('Ctrl Pts',(2.06144626369321,15.2,11.1329057267015));
#223504=CARTESIAN_POINT('Ctrl Pts',(2.06347980012034,15.2,11.1358564268031));
#223505=CARTESIAN_POINT('Ctrl Pts',(2.06552072958039,15.2,11.1388105082295));
#223506=CARTESIAN_POINT('Ctrl Pts',(2.06756905596495,15.2,11.1417679263307));
#223507=CARTESIAN_POINT('Ctrl Pts',(2.06961738234951,15.2,11.1447253444319));
#223508=CARTESIAN_POINT('Ctrl Pts',(2.07167310385066,15.2,11.1476860990135));
#223509=CARTESIAN_POINT('Ctrl Pts',(2.07373622524344,15.2,11.1506501490027));
#223510=CARTESIAN_POINT('Ctrl Pts',(2.07648705364221,15.2,11.1546022154753));
#223511=CARTESIAN_POINT('Ctrl Pts',(2.07925103579924,15.2,11.1585601375099));
#223512=CARTESIAN_POINT('Ctrl Pts',(2.08202817707083,15.2,11.1625238148519));
#223513=CARTESIAN_POINT('Ctrl Pts',(2.08480531872081,15.2,11.1664874927339));
#223514=CARTESIAN_POINT('Ctrl Pts',(2.08759562165266,15.2,11.1704569258472));
#223515=CARTESIAN_POINT('Ctrl Pts',(2.09039908924989,15.2,11.1744320130083));
#223516=CARTESIAN_POINT('Ctrl Pts',(2.09250168975683,15.2,11.1774133281083));
#223517=CARTESIAN_POINT('Ctrl Pts',(2.09461169628014,15.2,11.1803978233499));
#223518=CARTESIAN_POINT('Ctrl Pts',(2.09672911028588,15.2,11.1833854579077));
#223519=CARTESIAN_POINT('Ctrl Pts',(2.09955232921665,15.2,11.1873689710133));
#223520=CARTESIAN_POINT('Ctrl Pts',(2.10238871890352,15.2,11.1913580627424));
#223521=CARTESIAN_POINT('Ctrl Pts',(2.1052382826468,15.2,11.1953526341046));
#223522=CARTESIAN_POINT('Ctrl Pts',(2.10880023713176,15.2,11.2003458480353));
#223523=CARTESIAN_POINT('Ctrl Pts',(2.11238277735841,15.2,11.2053476223102));
#223524=CARTESIAN_POINT('Ctrl Pts',(2.11598591242953,15.2,11.2103577661303));
#223525=CARTESIAN_POINT('Ctrl Pts',(2.11814779339365,15.2,11.2133638523132));
#223526=CARTESIAN_POINT('Ctrl Pts',(2.12031708914906,15.2,11.2163729525875));
#223527=CARTESIAN_POINT('Ctrl Pts',(2.12249380057062,15.2,11.2193850238117));
#223528=CARTESIAN_POINT('Ctrl Pts',(2.12467051199217,15.2,11.2223970950358));
#223529=CARTESIAN_POINT('Ctrl Pts',(2.12685463905486,15.2,11.2254121393153));
#223530=CARTESIAN_POINT('Ctrl Pts',(2.12904618402689,15.2,11.2284301124694));
#223531=CARTESIAN_POINT('Ctrl Pts',(2.13196824385688,15.2,11.232454076492));
#223532=CARTESIAN_POINT('Ctrl Pts',(2.13490349065741,15.2,11.2364832474706));
#223533=CARTESIAN_POINT('Ctrl Pts',(2.13785192902616,15.2,11.240517528807));
#223534=CARTESIAN_POINT('Ctrl Pts',(2.14006325830488,15.2,11.2435432404964));
#223535=CARTESIAN_POINT('Ctrl Pts',(2.14228200674397,15.2,11.2465718269698));
#223536=CARTESIAN_POINT('Ctrl Pts',(2.14450817702687,15.2,11.2496032516608));
#223537=CARTESIAN_POINT('Ctrl Pts',(2.14673434690535,15.2,11.2526346758011));
#223538=CARTESIAN_POINT('Ctrl Pts',(2.14896793737503,15.2,11.2556689386578));
#223539=CARTESIAN_POINT('Ctrl Pts',(2.15120895125263,15.2,11.2587059980894));
#223540=CARTESIAN_POINT('Ctrl Pts',(2.15344996513022,15.2,11.261743057521));
#223541=CARTESIAN_POINT('Ctrl Pts',(2.15569840080699,15.2,11.2647829118161));
#223542=CARTESIAN_POINT('Ctrl Pts',(2.15795426127694,15.2,11.2678255123027));
#223543=CARTESIAN_POINT('Ctrl Pts',(2.16021012174689,15.2,11.2708681127893));
#223544=CARTESIAN_POINT('Ctrl Pts',(2.16247340780339,15.2,11.2739134570108));
#223545=CARTESIAN_POINT('Ctrl Pts',(2.16474411827283,15.2,11.2769615095389));
#223546=CARTESIAN_POINT('Ctrl Pts',(2.16852863585938,15.2,11.2820415972702));
#223547=CARTESIAN_POINT('Ctrl Pts',(2.17233377790013,15.2,11.2871292040928));
#223548=CARTESIAN_POINT('Ctrl Pts',(2.17615954699994,15.2,11.292224299));
#223549=CARTESIAN_POINT('Origin',(-5.66257110645729E-14,15.2,-1.77635683940025E-14));
#223550=CARTESIAN_POINT('',(1.18690176598713,15.2,10.306885524222));
#223551=CARTESIAN_POINT('',(1.18690176598713,12.2,10.306885524222));
#223552=CARTESIAN_POINT('',(1.18690176599994,15.2,10.306885524));
#223553=CARTESIAN_POINT('Origin',(-5.66257110645729E-14,12.2,-1.77635683940025E-14));
#223554=CARTESIAN_POINT('Origin',(-5.66257110645729E-14,15.2,-1.77635683940025E-14));
#223555=CARTESIAN_POINT('Origin',(-5.66257110645729E-14,15.2,-1.77635683940025E-14));
#223556=CARTESIAN_POINT('',(0.929795807999944,15.2,11.462350534));
#223557=CARTESIAN_POINT('',(0.546958305999944,15.2,11.486985532));
#223558=CARTESIAN_POINT('Origin',(-5.66257110645729E-14,15.2,-1.77635683940025E-14));
#223559=CARTESIAN_POINT('',(0.546958305999944,12.2,11.486985532));
#223560=CARTESIAN_POINT('',(0.546958305999944,15.2,11.486985532));
#223561=CARTESIAN_POINT('',(0.929795807999944,12.2,11.462350534));
#223562=CARTESIAN_POINT('Origin',(-5.66257110645729E-14,12.2,-1.77635683940025E-14));
#223563=CARTESIAN_POINT('',(0.929795807999944,15.2,11.462350534));
#223564=CARTESIAN_POINT('Ctrl Pts',(0.546958305999944,15.2,11.486985532));
#223565=CARTESIAN_POINT('Ctrl Pts',(0.546958305999944,11.6,11.486985532));
#223566=CARTESIAN_POINT('Ctrl Pts',(0.546590898999945,15.2,11.486315008));
#223567=CARTESIAN_POINT('Ctrl Pts',(0.546590898999945,11.6,11.486315008));
#223568=CARTESIAN_POINT('Ctrl Pts',(0.545856550999945,15.2,11.484974209));
#223569=CARTESIAN_POINT('Ctrl Pts',(0.545856550999945,11.6,11.484974209));
#223570=CARTESIAN_POINT('Ctrl Pts',(0.544756420999944,15.2,11.482963756));
#223571=CARTESIAN_POINT('Ctrl Pts',(0.544756420999944,11.6,11.482963756));
#223572=CARTESIAN_POINT('Ctrl Pts',(0.543292368999944,15.2,11.480284644));
#223573=CARTESIAN_POINT('Ctrl Pts',(0.543292368999944,11.6,11.480284644));
#223574=CARTESIAN_POINT('Ctrl Pts',(0.541466945999944,15.2,11.476938237));
#223575=CARTESIAN_POINT('Ctrl Pts',(0.541466945999944,11.6,11.476938237));
#223576=CARTESIAN_POINT('Ctrl Pts',(0.539646165999944,15.2,11.473594318));
#223577=CARTESIAN_POINT('Ctrl Pts',(0.539646165999944,11.6,11.473594318));
#223578=CARTESIAN_POINT('Ctrl Pts',(0.537830029999945,15.2,11.470252887));
#223579=CARTESIAN_POINT('Ctrl Pts',(0.537830029999945,11.6,11.470252887));
#223580=CARTESIAN_POINT('Ctrl Pts',(0.536018536999944,15.2,11.466913949));
#223581=CARTESIAN_POINT('Ctrl Pts',(0.536018536999944,11.6,11.466913949));
#223582=CARTESIAN_POINT('Ctrl Pts',(0.534211683999944,15.2,11.46357751));
#223583=CARTESIAN_POINT('Ctrl Pts',(0.534211683999944,11.6,11.46357751));
#223584=CARTESIAN_POINT('Ctrl Pts',(0.532409473999944,15.2,11.460243578));
#223585=CARTESIAN_POINT('Ctrl Pts',(0.532409473999944,11.6,11.460243578));
#223586=CARTESIAN_POINT('Ctrl Pts',(0.530611901999943,15.2,11.456912161));
#223587=CARTESIAN_POINT('Ctrl Pts',(0.530611901999943,11.6,11.456912161));
#223588=CARTESIAN_POINT('Ctrl Pts',(0.528818964999944,15.2,11.453583273));
#223589=CARTESIAN_POINT('Ctrl Pts',(0.528818964999944,11.6,11.453583273));
#223590=CARTESIAN_POINT('Ctrl Pts',(0.527030663999944,15.2,11.450256921));
#223591=CARTESIAN_POINT('Ctrl Pts',(0.527030663999944,11.6,11.450256921));
#223592=CARTESIAN_POINT('Ctrl Pts',(0.525246995999944,15.2,11.446933119));
#223593=CARTESIAN_POINT('Ctrl Pts',(0.525246995999944,11.6,11.446933119));
#223594=CARTESIAN_POINT('Ctrl Pts',(0.523467958999944,15.2,11.443611876));
#223595=CARTESIAN_POINT('Ctrl Pts',(0.523467958999944,11.6,11.443611876));
#223596=CARTESIAN_POINT('Ctrl Pts',(0.521693550999944,15.2,11.440293201));
#223597=CARTESIAN_POINT('Ctrl Pts',(0.521693550999944,11.6,11.440293201));
#223598=CARTESIAN_POINT('Ctrl Pts',(0.519923770999945,15.2,11.436977102));
#223599=CARTESIAN_POINT('Ctrl Pts',(0.519923770999945,11.6,11.436977102));
#223600=CARTESIAN_POINT('Ctrl Pts',(0.518158616999944,15.2,11.43366359));
#223601=CARTESIAN_POINT('Ctrl Pts',(0.518158616999944,11.6,11.43366359));
#223602=CARTESIAN_POINT('Ctrl Pts',(0.516398088999944,15.2,11.43035267));
#223603=CARTESIAN_POINT('Ctrl Pts',(0.516398088999944,11.6,11.43035267));
#223604=CARTESIAN_POINT('Ctrl Pts',(0.514642183999944,15.2,11.427044351));
#223605=CARTESIAN_POINT('Ctrl Pts',(0.514642183999944,11.6,11.427044351));
#223606=CARTESIAN_POINT('Ctrl Pts',(0.512890899999944,15.2,11.423738642));
#223607=CARTESIAN_POINT('Ctrl Pts',(0.512890899999944,11.6,11.423738642));
#223608=CARTESIAN_POINT('Ctrl Pts',(0.511144237999944,15.2,11.420435552));
#223609=CARTESIAN_POINT('Ctrl Pts',(0.511144237999944,11.6,11.420435552));
#223610=CARTESIAN_POINT('Ctrl Pts',(0.509402193999944,15.2,11.417135088));
#223611=CARTESIAN_POINT('Ctrl Pts',(0.509402193999944,11.6,11.417135088));
#223612=CARTESIAN_POINT('Ctrl Pts',(0.507664765999943,15.2,11.413837262));
#223613=CARTESIAN_POINT('Ctrl Pts',(0.507664765999943,11.6,11.413837262));
#223614=CARTESIAN_POINT('Ctrl Pts',(0.505931953999944,15.2,11.410542081));
#223615=CARTESIAN_POINT('Ctrl Pts',(0.505931953999944,11.6,11.410542081));
#223616=CARTESIAN_POINT('Ctrl Pts',(0.504203755999945,15.2,11.407249557));
#223617=CARTESIAN_POINT('Ctrl Pts',(0.504203755999945,11.6,11.407249557));
#223618=CARTESIAN_POINT('Ctrl Pts',(0.502480167999945,15.2,11.403959697));
#223619=CARTESIAN_POINT('Ctrl Pts',(0.502480167999945,11.6,11.403959697));
#223620=CARTESIAN_POINT('Ctrl Pts',(0.500761191999944,15.2,11.400672511));
#223621=CARTESIAN_POINT('Ctrl Pts',(0.500761191999944,11.6,11.400672511));
#223622=CARTESIAN_POINT('Ctrl Pts',(0.499046822999943,15.2,11.397388008));
#223623=CARTESIAN_POINT('Ctrl Pts',(0.499046822999943,11.6,11.397388008));
#223624=CARTESIAN_POINT('Ctrl Pts',(0.497337059999945,15.2,11.394106196));
#223625=CARTESIAN_POINT('Ctrl Pts',(0.497337059999945,11.6,11.394106196));
#223626=CARTESIAN_POINT('Ctrl Pts',(0.495631902999945,15.2,11.390827085));
#223627=CARTESIAN_POINT('Ctrl Pts',(0.495631902999945,11.6,11.390827085));
#223628=CARTESIAN_POINT('Ctrl Pts',(0.493931348999944,15.2,11.387550685));
#223629=CARTESIAN_POINT('Ctrl Pts',(0.493931348999944,11.6,11.387550685));
#223630=CARTESIAN_POINT('Ctrl Pts',(0.492235395999945,15.2,11.384277002));
#223631=CARTESIAN_POINT('Ctrl Pts',(0.492235395999945,11.6,11.384277002));
#223632=CARTESIAN_POINT('Ctrl Pts',(0.490544042999945,15.2,11.381006048));
#223633=CARTESIAN_POINT('Ctrl Pts',(0.490544042999945,11.6,11.381006048));
#223634=CARTESIAN_POINT('Ctrl Pts',(0.488857286999943,15.2,11.37773783));
#223635=CARTESIAN_POINT('Ctrl Pts',(0.488857286999943,11.6,11.37773783));
#223636=CARTESIAN_POINT('Ctrl Pts',(0.487175127999944,15.2,11.374472358));
#223637=CARTESIAN_POINT('Ctrl Pts',(0.487175127999944,11.6,11.374472358));
#223638=CARTESIAN_POINT('Ctrl Pts',(0.485497562999945,15.2,11.371209642));
#223639=CARTESIAN_POINT('Ctrl Pts',(0.485497562999945,11.6,11.371209642));
#223640=CARTESIAN_POINT('Ctrl Pts',(0.483824590999945,15.2,11.36794969));
#223641=CARTESIAN_POINT('Ctrl Pts',(0.483824590999945,11.6,11.36794969));
#223642=CARTESIAN_POINT('Ctrl Pts',(0.482156208999944,15.2,11.364692512));
#223643=CARTESIAN_POINT('Ctrl Pts',(0.482156208999944,11.6,11.364692512));
#223644=CARTESIAN_POINT('Ctrl Pts',(0.480492415999944,15.2,11.361438117));
#223645=CARTESIAN_POINT('Ctrl Pts',(0.480492415999944,11.6,11.361438117));
#223646=CARTESIAN_POINT('Ctrl Pts',(0.478833209999945,15.2,11.358186515));
#223647=CARTESIAN_POINT('Ctrl Pts',(0.478833209999945,11.6,11.358186515));
#223648=CARTESIAN_POINT('Ctrl Pts',(0.477178588999945,15.2,11.354937714));
#223649=CARTESIAN_POINT('Ctrl Pts',(0.477178588999945,11.6,11.354937714));
#223650=CARTESIAN_POINT('Ctrl Pts',(0.475528549999943,15.2,11.351691724));
#223651=CARTESIAN_POINT('Ctrl Pts',(0.475528549999943,11.6,11.351691724));
#223652=CARTESIAN_POINT('Ctrl Pts',(0.473883093999945,15.2,11.348448553));
#223653=CARTESIAN_POINT('Ctrl Pts',(0.473883093999945,11.6,11.348448553));
#223654=CARTESIAN_POINT('Ctrl Pts',(0.472242216999945,15.2,11.345208212));
#223655=CARTESIAN_POINT('Ctrl Pts',(0.472242216999945,11.6,11.345208212));
#223656=CARTESIAN_POINT('Ctrl Pts',(0.470605917999943,15.2,11.34197071));
#223657=CARTESIAN_POINT('Ctrl Pts',(0.470605917999943,11.6,11.34197071));
#223658=CARTESIAN_POINT('Ctrl Pts',(0.468974193999945,15.2,11.338736055));
#223659=CARTESIAN_POINT('Ctrl Pts',(0.468974193999945,11.6,11.338736055));
#223660=CARTESIAN_POINT('Ctrl Pts',(0.467347043999944,15.2,11.335504256));
#223661=CARTESIAN_POINT('Ctrl Pts',(0.467347043999944,11.6,11.335504256));
#223662=CARTESIAN_POINT('Ctrl Pts',(0.465724464999945,15.2,11.332275324));
#223663=CARTESIAN_POINT('Ctrl Pts',(0.465724464999945,11.6,11.332275324));
#223664=CARTESIAN_POINT('Ctrl Pts',(0.464106456999945,15.2,11.329049269));
#223665=CARTESIAN_POINT('Ctrl Pts',(0.464106456999945,11.6,11.329049269));
#223666=CARTESIAN_POINT('Ctrl Pts',(0.462493016999945,15.2,11.325826099));
#223667=CARTESIAN_POINT('Ctrl Pts',(0.462493016999945,11.6,11.325826099));
#223668=CARTESIAN_POINT('Ctrl Pts',(0.460884141999944,15.2,11.322605823));
#223669=CARTESIAN_POINT('Ctrl Pts',(0.460884141999944,11.6,11.322605823));
#223670=CARTESIAN_POINT('Ctrl Pts',(0.459279831999944,15.2,11.319388451));
#223671=CARTESIAN_POINT('Ctrl Pts',(0.459279831999944,11.6,11.319388451));
#223672=CARTESIAN_POINT('Ctrl Pts',(0.457680083999945,15.2,11.316173992));
#223673=CARTESIAN_POINT('Ctrl Pts',(0.457680083999945,11.6,11.316173992));
#223674=CARTESIAN_POINT('Ctrl Pts',(0.456084895999943,15.2,11.312962457));
#223675=CARTESIAN_POINT('Ctrl Pts',(0.456084895999943,11.6,11.312962457));
#223676=CARTESIAN_POINT('Ctrl Pts',(0.454494264999944,15.2,11.309753854));
#223677=CARTESIAN_POINT('Ctrl Pts',(0.454494264999944,11.6,11.309753854));
#223678=CARTESIAN_POINT('Ctrl Pts',(0.452908190999944,15.2,11.306548191));
#223679=CARTESIAN_POINT('Ctrl Pts',(0.452908190999944,11.6,11.306548191));
#223680=CARTESIAN_POINT('Ctrl Pts',(0.451326669999944,15.2,11.303345481));
#223681=CARTESIAN_POINT('Ctrl Pts',(0.451326669999944,11.6,11.303345481));
#223682=CARTESIAN_POINT('Ctrl Pts',(0.449749701999943,15.2,11.300145732));
#223683=CARTESIAN_POINT('Ctrl Pts',(0.449749701999943,11.6,11.300145732));
#223684=CARTESIAN_POINT('Ctrl Pts',(0.448177283999945,15.2,11.296948952));
#223685=CARTESIAN_POINT('Ctrl Pts',(0.448177283999945,11.6,11.296948952));
#223686=CARTESIAN_POINT('Ctrl Pts',(0.446609412999944,15.2,11.293755151));
#223687=CARTESIAN_POINT('Ctrl Pts',(0.446609412999944,11.6,11.293755151));
#223688=CARTESIAN_POINT('Ctrl Pts',(0.445046087999945,15.2,11.290564341));
#223689=CARTESIAN_POINT('Ctrl Pts',(0.445046087999945,11.6,11.290564341));
#223690=CARTESIAN_POINT('Ctrl Pts',(0.443487306999945,15.2,11.287376529));
#223691=CARTESIAN_POINT('Ctrl Pts',(0.443487306999945,11.6,11.287376529));
#223692=CARTESIAN_POINT('Ctrl Pts',(0.441933066999944,15.2,11.284191726));
#223693=CARTESIAN_POINT('Ctrl Pts',(0.441933066999944,11.6,11.284191726));
#223694=CARTESIAN_POINT('Ctrl Pts',(0.440383366999945,15.2,11.28100994));
#223695=CARTESIAN_POINT('Ctrl Pts',(0.440383366999945,11.6,11.28100994));
#223696=CARTESIAN_POINT('Ctrl Pts',(0.438838203999945,15.2,11.277831182));
#223697=CARTESIAN_POINT('Ctrl Pts',(0.438838203999945,11.6,11.277831182));
#223698=CARTESIAN_POINT('Ctrl Pts',(0.437297575999944,15.2,11.27465546));
#223699=CARTESIAN_POINT('Ctrl Pts',(0.437297575999944,11.6,11.27465546));
#223700=CARTESIAN_POINT('Ctrl Pts',(0.435761481999943,15.2,11.271482787));
#223701=CARTESIAN_POINT('Ctrl Pts',(0.435761481999943,11.6,11.271482787));
#223702=CARTESIAN_POINT('Ctrl Pts',(0.434229916999945,15.2,11.268313168));
#223703=CARTESIAN_POINT('Ctrl Pts',(0.434229916999945,11.6,11.268313168));
#223704=CARTESIAN_POINT('Ctrl Pts',(0.432702881999945,15.2,11.265146617));
#223705=CARTESIAN_POINT('Ctrl Pts',(0.432702881999945,11.6,11.265146617));
#223706=CARTESIAN_POINT('Ctrl Pts',(0.431180373999943,15.2,11.261983142));
#223707=CARTESIAN_POINT('Ctrl Pts',(0.431180373999943,11.6,11.261983142));
#223708=CARTESIAN_POINT('Ctrl Pts',(0.429662389999944,15.2,11.258822751));
#223709=CARTESIAN_POINT('Ctrl Pts',(0.429662389999944,11.6,11.258822751));
#223710=CARTESIAN_POINT('Ctrl Pts',(0.428148927999944,15.2,11.255665455));
#223711=CARTESIAN_POINT('Ctrl Pts',(0.428148927999944,11.6,11.255665455));
#223712=CARTESIAN_POINT('Ctrl Pts',(0.426639985999945,15.2,11.252511265));
#223713=CARTESIAN_POINT('Ctrl Pts',(0.426639985999945,11.6,11.252511265));
#223714=CARTESIAN_POINT('Ctrl Pts',(0.425135560999944,15.2,11.249360189));
#223715=CARTESIAN_POINT('Ctrl Pts',(0.425135560999944,11.6,11.249360189));
#223716=CARTESIAN_POINT('Ctrl Pts',(0.423635651999945,15.2,11.246212238));
#223717=CARTESIAN_POINT('Ctrl Pts',(0.423635651999945,11.6,11.246212238));
#223718=CARTESIAN_POINT('Ctrl Pts',(0.422140256999944,15.2,11.24306742));
#223719=CARTESIAN_POINT('Ctrl Pts',(0.422140256999944,11.6,11.24306742));
#223720=CARTESIAN_POINT('Ctrl Pts',(0.420649371999945,15.2,11.239925747));
#223721=CARTESIAN_POINT('Ctrl Pts',(0.420649371999945,11.6,11.239925747));
#223722=CARTESIAN_POINT('Ctrl Pts',(0.419162995999944,15.2,11.236787228));
#223723=CARTESIAN_POINT('Ctrl Pts',(0.419162995999944,11.6,11.236787228));
#223724=CARTESIAN_POINT('Ctrl Pts',(0.417681126999945,15.2,11.233651872));
#223725=CARTESIAN_POINT('Ctrl Pts',(0.417681126999945,11.6,11.233651872));
#223726=CARTESIAN_POINT('Ctrl Pts',(0.416203760999944,15.2,11.230519689));
#223727=CARTESIAN_POINT('Ctrl Pts',(0.416203760999944,11.6,11.230519689));
#223728=CARTESIAN_POINT('Ctrl Pts',(0.414730897999943,15.2,11.227390689));
#223729=CARTESIAN_POINT('Ctrl Pts',(0.414730897999943,11.6,11.227390689));
#223730=CARTESIAN_POINT('Ctrl Pts',(0.413262533999944,15.2,11.224264884));
#223731=CARTESIAN_POINT('Ctrl Pts',(0.413262533999944,11.6,11.224264884));
#223732=CARTESIAN_POINT('Ctrl Pts',(0.411798665999944,15.2,11.22114228));
#223733=CARTESIAN_POINT('Ctrl Pts',(0.411798665999944,11.6,11.22114228));
#223734=CARTESIAN_POINT('Ctrl Pts',(0.410339294999943,15.2,11.21802289));
#223735=CARTESIAN_POINT('Ctrl Pts',(0.410339294999943,11.6,11.21802289));
#223736=CARTESIAN_POINT('Ctrl Pts',(0.408884414999945,15.2,11.214906723));
#223737=CARTESIAN_POINT('Ctrl Pts',(0.408884414999945,11.6,11.214906723));
#223738=CARTESIAN_POINT('Ctrl Pts',(0.407434024999944,15.2,11.211793789));
#223739=CARTESIAN_POINT('Ctrl Pts',(0.407434024999944,11.6,11.211793789));
#223740=CARTESIAN_POINT('Ctrl Pts',(0.405988121999944,15.2,11.208684097));
#223741=CARTESIAN_POINT('Ctrl Pts',(0.405988121999944,11.6,11.208684097));
#223742=CARTESIAN_POINT('Ctrl Pts',(0.404546704999945,15.2,11.205577658));
#223743=CARTESIAN_POINT('Ctrl Pts',(0.404546704999945,11.6,11.205577658));
#223744=CARTESIAN_POINT('Ctrl Pts',(0.403109770999944,15.2,11.202474482));
#223745=CARTESIAN_POINT('Ctrl Pts',(0.403109770999944,11.6,11.202474482));
#223746=CARTESIAN_POINT('Ctrl Pts',(0.401677316999944,15.2,11.199374578));
#223747=CARTESIAN_POINT('Ctrl Pts',(0.401677316999944,11.6,11.199374578));
#223748=CARTESIAN_POINT('Ctrl Pts',(0.400249340999944,15.2,11.196277957));
#223749=CARTESIAN_POINT('Ctrl Pts',(0.400249340999944,11.6,11.196277957));
#223750=CARTESIAN_POINT('Ctrl Pts',(0.398825840999945,15.2,11.193184629));
#223751=CARTESIAN_POINT('Ctrl Pts',(0.398825840999945,11.6,11.193184629));
#223752=CARTESIAN_POINT('Ctrl Pts',(0.397406813999943,15.2,11.190094604));
#223753=CARTESIAN_POINT('Ctrl Pts',(0.397406813999943,11.6,11.190094604));
#223754=CARTESIAN_POINT('Ctrl Pts',(0.395992257999945,15.2,11.187007891));
#223755=CARTESIAN_POINT('Ctrl Pts',(0.395992257999945,11.6,11.187007891));
#223756=CARTESIAN_POINT('Ctrl Pts',(0.394582168999945,15.2,11.183924503));
#223757=CARTESIAN_POINT('Ctrl Pts',(0.394582168999945,11.6,11.183924503));
#223758=CARTESIAN_POINT('Ctrl Pts',(0.393176546999945,15.2,11.180844446));
#223759=CARTESIAN_POINT('Ctrl Pts',(0.393176546999945,11.6,11.180844446));
#223760=CARTESIAN_POINT('Ctrl Pts',(0.391775385999944,15.2,11.177767734));
#223761=CARTESIAN_POINT('Ctrl Pts',(0.391775385999944,11.6,11.177767734));
#223762=CARTESIAN_POINT('Ctrl Pts',(0.390378687999944,15.2,11.174694374));
#223763=CARTESIAN_POINT('Ctrl Pts',(0.390378687999944,11.6,11.174694374));
#223764=CARTESIAN_POINT('Ctrl Pts',(0.388986445999944,15.2,11.171624378));
#223765=CARTESIAN_POINT('Ctrl Pts',(0.388986445999944,11.6,11.171624378));
#223766=CARTESIAN_POINT('Ctrl Pts',(0.387598660999944,15.2,11.168557757));
#223767=CARTESIAN_POINT('Ctrl Pts',(0.387598660999944,11.6,11.168557757));
#223768=CARTESIAN_POINT('Ctrl Pts',(0.386215327999944,15.2,11.165494518));
#223769=CARTESIAN_POINT('Ctrl Pts',(0.386215327999944,11.6,11.165494518));
#223770=CARTESIAN_POINT('Ctrl Pts',(0.384836444999944,15.2,11.162434674));
#223771=CARTESIAN_POINT('Ctrl Pts',(0.384836444999944,11.6,11.162434674));
#223772=CARTESIAN_POINT('Ctrl Pts',(0.383462009999944,15.2,11.159378235));
#223773=CARTESIAN_POINT('Ctrl Pts',(0.383462009999944,11.6,11.159378235));
#223774=CARTESIAN_POINT('Ctrl Pts',(0.382092020999943,15.2,11.15632521));
#223775=CARTESIAN_POINT('Ctrl Pts',(0.382092020999943,11.6,11.15632521));
#223776=CARTESIAN_POINT('Ctrl Pts',(0.380726473999945,15.2,11.15327561));
#223777=CARTESIAN_POINT('Ctrl Pts',(0.380726473999945,11.6,11.15327561));
#223778=CARTESIAN_POINT('Ctrl Pts',(0.379365366999943,15.2,11.150229446));
#223779=CARTESIAN_POINT('Ctrl Pts',(0.379365366999943,11.6,11.150229446));
#223780=CARTESIAN_POINT('Ctrl Pts',(0.378008696999944,15.2,11.147186727));
#223781=CARTESIAN_POINT('Ctrl Pts',(0.378008696999944,11.6,11.147186727));
#223782=CARTESIAN_POINT('Ctrl Pts',(0.376656460999945,15.2,11.144147463));
#223783=CARTESIAN_POINT('Ctrl Pts',(0.376656460999945,11.6,11.144147463));
#223784=CARTESIAN_POINT('Ctrl Pts',(0.375308657999945,15.2,11.141111667));
#223785=CARTESIAN_POINT('Ctrl Pts',(0.375308657999945,11.6,11.141111667));
#223786=CARTESIAN_POINT('Ctrl Pts',(0.373965283999944,15.2,11.138079346));
#223787=CARTESIAN_POINT('Ctrl Pts',(0.373965283999944,11.6,11.138079346));
#223788=CARTESIAN_POINT('Ctrl Pts',(0.372626335999945,15.2,11.135050513));
#223789=CARTESIAN_POINT('Ctrl Pts',(0.372626335999945,11.6,11.135050513));
#223790=CARTESIAN_POINT('Ctrl Pts',(0.371291811999944,15.2,11.132025177));
#223791=CARTESIAN_POINT('Ctrl Pts',(0.371291811999944,11.6,11.132025177));
#223792=CARTESIAN_POINT('Ctrl Pts',(0.369961708999943,15.2,11.129003348));
#223793=CARTESIAN_POINT('Ctrl Pts',(0.369961708999943,11.6,11.129003348));
#223794=CARTESIAN_POINT('Ctrl Pts',(0.368636023999944,15.2,11.125985039));
#223795=CARTESIAN_POINT('Ctrl Pts',(0.368636023999944,11.6,11.125985039));
#223796=CARTESIAN_POINT('Ctrl Pts',(0.367314755999945,15.2,11.122970257));
#223797=CARTESIAN_POINT('Ctrl Pts',(0.367314755999945,11.6,11.122970257));
#223798=CARTESIAN_POINT('Ctrl Pts',(0.365997898999944,15.2,11.119959015));
#223799=CARTESIAN_POINT('Ctrl Pts',(0.365997898999944,11.6,11.119959015));
#223800=CARTESIAN_POINT('Ctrl Pts',(0.364685451999945,15.2,11.116951322));
#223801=CARTESIAN_POINT('Ctrl Pts',(0.364685451999945,11.6,11.116951322));
#223802=CARTESIAN_POINT('Ctrl Pts',(0.363377412999943,15.2,11.11394719));
#223803=CARTESIAN_POINT('Ctrl Pts',(0.363377412999943,11.6,11.11394719));
#223804=CARTESIAN_POINT('Ctrl Pts',(0.362073778999944,15.2,11.110946629));
#223805=CARTESIAN_POINT('Ctrl Pts',(0.362073778999944,11.6,11.110946629));
#223806=CARTESIAN_POINT('Ctrl Pts',(0.360774545999943,15.2,11.107949648));
#223807=CARTESIAN_POINT('Ctrl Pts',(0.360774545999943,11.6,11.107949648));
#223808=CARTESIAN_POINT('Ctrl Pts',(0.359479711999944,15.2,11.104956259));
#223809=CARTESIAN_POINT('Ctrl Pts',(0.359479711999944,11.6,11.104956259));
#223810=CARTESIAN_POINT('Ctrl Pts',(0.358189272999944,15.2,11.101966473));
#223811=CARTESIAN_POINT('Ctrl Pts',(0.358189272999944,11.6,11.101966473));
#223812=CARTESIAN_POINT('Ctrl Pts',(0.356903226999944,15.2,11.0989803));
#223813=CARTESIAN_POINT('Ctrl Pts',(0.356903226999944,11.6,11.0989803));
#223814=CARTESIAN_POINT('Ctrl Pts',(0.355621571999943,15.2,11.095997751));
#223815=CARTESIAN_POINT('Ctrl Pts',(0.355621571999943,11.6,11.095997751));
#223816=CARTESIAN_POINT('Ctrl Pts',(0.354344304999945,15.2,11.093018835));
#223817=CARTESIAN_POINT('Ctrl Pts',(0.354344304999945,11.6,11.093018835));
#223818=CARTESIAN_POINT('Ctrl Pts',(0.353071419999944,15.2,11.090043565));
#223819=CARTESIAN_POINT('Ctrl Pts',(0.353071419999944,11.6,11.090043565));
#223820=CARTESIAN_POINT('Ctrl Pts',(0.351802917999944,15.2,11.087071951));
#223821=CARTESIAN_POINT('Ctrl Pts',(0.351802917999944,11.6,11.087071951));
#223822=CARTESIAN_POINT('Ctrl Pts',(0.350538794999944,15.2,11.084104002));
#223823=CARTESIAN_POINT('Ctrl Pts',(0.350538794999944,11.6,11.084104002));
#223824=CARTESIAN_POINT('Ctrl Pts',(0.349279045999945,15.2,11.081139731));
#223825=CARTESIAN_POINT('Ctrl Pts',(0.349279045999945,11.6,11.081139731));
#223826=CARTESIAN_POINT('Ctrl Pts',(0.348023670999943,15.2,11.078179147));
#223827=CARTESIAN_POINT('Ctrl Pts',(0.348023670999943,11.6,11.078179147));
#223828=CARTESIAN_POINT('Ctrl Pts',(0.346772663999945,15.2,11.075222263));
#223829=CARTESIAN_POINT('Ctrl Pts',(0.346772663999945,11.6,11.075222263));
#223830=CARTESIAN_POINT('Ctrl Pts',(0.345526024999945,15.2,11.072269087));
#223831=CARTESIAN_POINT('Ctrl Pts',(0.345526024999945,11.6,11.072269087));
#223832=CARTESIAN_POINT('Ctrl Pts',(0.344283748999944,15.2,11.069319631));
#223833=CARTESIAN_POINT('Ctrl Pts',(0.344283748999944,11.6,11.069319631));
#223834=CARTESIAN_POINT('Ctrl Pts',(0.343045832999945,15.2,11.066373907));
#223835=CARTESIAN_POINT('Ctrl Pts',(0.343045832999945,11.6,11.066373907));
#223836=CARTESIAN_POINT('Ctrl Pts',(0.341812274999944,15.2,11.063431924));
#223837=CARTESIAN_POINT('Ctrl Pts',(0.341812274999944,11.6,11.063431924));
#223838=CARTESIAN_POINT('Ctrl Pts',(0.340583071999945,15.2,11.060493695));
#223839=CARTESIAN_POINT('Ctrl Pts',(0.340583071999945,11.6,11.060493695));
#223840=CARTESIAN_POINT('Ctrl Pts',(0.339358218999944,15.2,11.057559229));
#223841=CARTESIAN_POINT('Ctrl Pts',(0.339358218999944,11.6,11.057559229));
#223842=CARTESIAN_POINT('Ctrl Pts',(0.338137715999943,15.2,11.054628538));
#223843=CARTESIAN_POINT('Ctrl Pts',(0.338137715999943,11.6,11.054628538));
#223844=CARTESIAN_POINT('Ctrl Pts',(0.336921556999944,15.2,11.051701632));
#223845=CARTESIAN_POINT('Ctrl Pts',(0.336921556999944,11.6,11.051701632));
#223846=CARTESIAN_POINT('Ctrl Pts',(0.335709739999944,15.2,11.048778522));
#223847=CARTESIAN_POINT('Ctrl Pts',(0.335709739999944,11.6,11.048778522));
#223848=CARTESIAN_POINT('Ctrl Pts',(0.334502261999944,15.2,11.04585922));
#223849=CARTESIAN_POINT('Ctrl Pts',(0.334502261999944,11.6,11.04585922));
#223850=CARTESIAN_POINT('Ctrl Pts',(0.333299119999945,15.2,11.042943736));
#223851=CARTESIAN_POINT('Ctrl Pts',(0.333299119999945,11.6,11.042943736));
#223852=CARTESIAN_POINT('Ctrl Pts',(0.332100310999944,15.2,11.040032081));
#223853=CARTESIAN_POINT('Ctrl Pts',(0.332100310999944,11.6,11.040032081));
#223854=CARTESIAN_POINT('Ctrl Pts',(0.330905830999945,15.2,11.037124267));
#223855=CARTESIAN_POINT('Ctrl Pts',(0.330905830999945,11.6,11.037124267));
#223856=CARTESIAN_POINT('Ctrl Pts',(0.329715676999944,15.2,11.034220304));
#223857=CARTESIAN_POINT('Ctrl Pts',(0.329715676999944,11.6,11.034220304));
#223858=CARTESIAN_POINT('Ctrl Pts',(0.328529845999944,15.2,11.031320203));
#223859=CARTESIAN_POINT('Ctrl Pts',(0.328529845999944,11.6,11.031320203));
#223860=CARTESIAN_POINT('Ctrl Pts',(0.327348334999943,15.2,11.028423977));
#223861=CARTESIAN_POINT('Ctrl Pts',(0.327348334999943,11.6,11.028423977));
#223862=CARTESIAN_POINT('Ctrl Pts',(0.326171140999945,15.2,11.025531635));
#223863=CARTESIAN_POINT('Ctrl Pts',(0.326171140999945,11.6,11.025531635));
#223864=CARTESIAN_POINT('Ctrl Pts',(0.324998259999945,15.2,11.02264319));
#223865=CARTESIAN_POINT('Ctrl Pts',(0.324998259999945,11.6,11.02264319));
#223866=CARTESIAN_POINT('Ctrl Pts',(0.323829688999944,15.2,11.01975865));
#223867=CARTESIAN_POINT('Ctrl Pts',(0.323829688999944,11.6,11.01975865));
#223868=CARTESIAN_POINT('Ctrl Pts',(0.322665423999944,15.2,11.016878029));
#223869=CARTESIAN_POINT('Ctrl Pts',(0.322665423999944,11.6,11.016878029));
#223870=CARTESIAN_POINT('Ctrl Pts',(0.321505462999945,15.2,11.014001339));
#223871=CARTESIAN_POINT('Ctrl Pts',(0.321505462999945,11.6,11.014001339));
#223872=CARTESIAN_POINT('Ctrl Pts',(0.320349802999944,15.2,11.011128587));
#223873=CARTESIAN_POINT('Ctrl Pts',(0.320349802999944,11.6,11.011128587));
#223874=CARTESIAN_POINT('Ctrl Pts',(0.319198438999945,15.2,11.008259789));
#223875=CARTESIAN_POINT('Ctrl Pts',(0.319198438999945,11.6,11.008259789));
#223876=CARTESIAN_POINT('Ctrl Pts',(0.318051368999944,15.2,11.005394953));
#223877=CARTESIAN_POINT('Ctrl Pts',(0.318051368999944,11.6,11.005394953));
#223878=CARTESIAN_POINT('Ctrl Pts',(0.316908587999943,15.2,11.002534092));
#223879=CARTESIAN_POINT('Ctrl Pts',(0.316908587999943,11.6,11.002534092));
#223880=CARTESIAN_POINT('Ctrl Pts',(0.315770094999944,15.2,10.999677217));
#223881=CARTESIAN_POINT('Ctrl Pts',(0.315770094999944,11.6,10.999677217));
#223882=CARTESIAN_POINT('Ctrl Pts',(0.314635883999944,15.2,10.996824338));
#223883=CARTESIAN_POINT('Ctrl Pts',(0.314635883999944,11.6,10.996824338));
#223884=CARTESIAN_POINT('Ctrl Pts',(0.313505953999943,15.2,10.993975469));
#223885=CARTESIAN_POINT('Ctrl Pts',(0.313505953999943,11.6,10.993975469));
#223886=CARTESIAN_POINT('Ctrl Pts',(0.312380299999945,15.2,10.991130619));
#223887=CARTESIAN_POINT('Ctrl Pts',(0.312380299999945,11.6,10.991130619));
#223888=CARTESIAN_POINT('Ctrl Pts',(0.311258918999944,15.2,10.988289801));
#223889=CARTESIAN_POINT('Ctrl Pts',(0.311258918999944,11.6,10.988289801));
#223890=CARTESIAN_POINT('Ctrl Pts',(0.310141807999944,15.2,10.985453024));
#223891=CARTESIAN_POINT('Ctrl Pts',(0.310141807999944,11.6,10.985453024));
#223892=CARTESIAN_POINT('Ctrl Pts',(0.309028961999944,15.2,10.982620303));
#223893=CARTESIAN_POINT('Ctrl Pts',(0.309028961999944,11.6,10.982620303));
#223894=CARTESIAN_POINT('Ctrl Pts',(0.307920378999944,15.2,10.979791646));
#223895=CARTESIAN_POINT('Ctrl Pts',(0.307920378999944,11.6,10.979791646));
#223896=CARTESIAN_POINT('Ctrl Pts',(0.306816055999944,15.2,10.976967067));
#223897=CARTESIAN_POINT('Ctrl Pts',(0.306816055999944,11.6,10.976967067));
#223898=CARTESIAN_POINT('Ctrl Pts',(0.305715986999945,15.2,10.974146576));
#223899=CARTESIAN_POINT('Ctrl Pts',(0.305715986999945,11.6,10.974146576));
#223900=CARTESIAN_POINT('Ctrl Pts',(0.304620169999945,15.2,10.971330186));
#223901=CARTESIAN_POINT('Ctrl Pts',(0.304620169999945,11.6,10.971330186));
#223902=CARTESIAN_POINT('Ctrl Pts',(0.303528602999944,15.2,10.968517908));
#223903=CARTESIAN_POINT('Ctrl Pts',(0.303528602999944,11.6,10.968517908));
#223904=CARTESIAN_POINT('Ctrl Pts',(0.302441278999943,15.2,10.965709751));
#223905=CARTESIAN_POINT('Ctrl Pts',(0.302441278999943,11.6,10.965709751));
#223906=CARTESIAN_POINT('Ctrl Pts',(0.301358196999945,15.2,10.962905732));
#223907=CARTESIAN_POINT('Ctrl Pts',(0.301358196999945,11.6,10.962905732));
#223908=CARTESIAN_POINT('Ctrl Pts',(0.300279352999944,15.2,10.960105857));
#223909=CARTESIAN_POINT('Ctrl Pts',(0.300279352999944,11.6,10.960105857));
#223910=CARTESIAN_POINT('Ctrl Pts',(0.299204742999944,15.2,10.957310141));
#223911=CARTESIAN_POINT('Ctrl Pts',(0.299204742999944,11.6,10.957310141));
#223912=CARTESIAN_POINT('Ctrl Pts',(0.298134362999944,15.2,10.954518595));
#223913=CARTESIAN_POINT('Ctrl Pts',(0.298134362999944,11.6,10.954518595));
#223914=CARTESIAN_POINT('Ctrl Pts',(0.297068208999944,15.2,10.951731231));
#223915=CARTESIAN_POINT('Ctrl Pts',(0.297068208999944,11.6,10.951731231));
#223916=CARTESIAN_POINT('Ctrl Pts',(0.296006278999944,15.2,10.94894806));
#223917=CARTESIAN_POINT('Ctrl Pts',(0.296006278999944,11.6,10.94894806));
#223918=CARTESIAN_POINT('Ctrl Pts',(0.294948567999944,15.2,10.946169093));
#223919=CARTESIAN_POINT('Ctrl Pts',(0.294948567999944,11.6,10.946169093));
#223920=CARTESIAN_POINT('Ctrl Pts',(0.293895072999945,15.2,10.943394344));
#223921=CARTESIAN_POINT('Ctrl Pts',(0.293895072999945,11.6,10.943394344));
#223922=CARTESIAN_POINT('Ctrl Pts',(0.292845787999945,15.2,10.940623824));
#223923=CARTESIAN_POINT('Ctrl Pts',(0.292845787999945,11.6,10.940623824));
#223924=CARTESIAN_POINT('Ctrl Pts',(0.291800711999944,15.2,10.937857544));
#223925=CARTESIAN_POINT('Ctrl Pts',(0.291800711999944,11.6,10.937857544));
#223926=CARTESIAN_POINT('Ctrl Pts',(0.290759841999944,15.2,10.935095515));
#223927=CARTESIAN_POINT('Ctrl Pts',(0.290759841999944,11.6,10.935095515));
#223928=CARTESIAN_POINT('Ctrl Pts',(0.289723169999944,15.2,10.932337751));
#223929=CARTESIAN_POINT('Ctrl Pts',(0.289723169999944,11.6,10.932337751));
#223930=CARTESIAN_POINT('Ctrl Pts',(0.288690695999945,15.2,10.929584263));
#223931=CARTESIAN_POINT('Ctrl Pts',(0.288690695999945,11.6,10.929584263));
#223932=CARTESIAN_POINT('Ctrl Pts',(0.287662414999945,15.2,10.926835064));
#223933=CARTESIAN_POINT('Ctrl Pts',(0.287662414999945,11.6,10.926835064));
#223934=CARTESIAN_POINT('Ctrl Pts',(0.286638321999944,15.2,10.924090164));
#223935=CARTESIAN_POINT('Ctrl Pts',(0.286638321999944,11.6,10.924090164));
#223936=CARTESIAN_POINT('Ctrl Pts',(0.285618414999943,15.2,10.921349576));
#223937=CARTESIAN_POINT('Ctrl Pts',(0.285618414999943,11.6,10.921349576));
#223938=CARTESIAN_POINT('Ctrl Pts',(0.284602689999945,15.2,10.918613312));
#223939=CARTESIAN_POINT('Ctrl Pts',(0.284602689999945,11.6,10.918613312));
#223940=CARTESIAN_POINT('Ctrl Pts',(0.283591139999944,15.2,10.915881383));
#223941=CARTESIAN_POINT('Ctrl Pts',(0.283591139999944,11.6,10.915881383));
#223942=CARTESIAN_POINT('Ctrl Pts',(0.282583764999943,15.2,10.913153803));
#223943=CARTESIAN_POINT('Ctrl Pts',(0.282583764999943,11.6,10.913153803));
#223944=CARTESIAN_POINT('Ctrl Pts',(0.281580559999943,15.2,10.910430582));
#223945=CARTESIAN_POINT('Ctrl Pts',(0.281580559999943,11.6,10.910430582));
#223946=CARTESIAN_POINT('Ctrl Pts',(0.280581519999944,15.2,10.907711735));
#223947=CARTESIAN_POINT('Ctrl Pts',(0.280581519999944,11.6,10.907711735));
#223948=CARTESIAN_POINT('Ctrl Pts',(0.279586641999944,15.2,10.904997271));
#223949=CARTESIAN_POINT('Ctrl Pts',(0.279586641999944,11.6,10.904997271));
#223950=CARTESIAN_POINT('Ctrl Pts',(0.278595920999944,15.2,10.902287203));
#223951=CARTESIAN_POINT('Ctrl Pts',(0.278595920999944,11.6,10.902287203));
#223952=CARTESIAN_POINT('Ctrl Pts',(0.277609353999945,15.2,10.899581544));
#223953=CARTESIAN_POINT('Ctrl Pts',(0.277609353999945,11.6,10.899581544));
#223954=CARTESIAN_POINT('Ctrl Pts',(0.276626936999945,15.2,10.896880306));
#223955=CARTESIAN_POINT('Ctrl Pts',(0.276626936999945,11.6,10.896880306));
#223956=CARTESIAN_POINT('Ctrl Pts',(0.275648663999943,15.2,10.894183501));
#223957=CARTESIAN_POINT('Ctrl Pts',(0.275648663999943,11.6,10.894183501));
#223958=CARTESIAN_POINT('Ctrl Pts',(0.274674533999945,15.2,10.89149114));
#223959=CARTESIAN_POINT('Ctrl Pts',(0.274674533999945,11.6,10.89149114));
#223960=CARTESIAN_POINT('Ctrl Pts',(0.273704539999944,15.2,10.888803238));
#223961=CARTESIAN_POINT('Ctrl Pts',(0.273704539999944,11.6,10.888803238));
#223962=CARTESIAN_POINT('Ctrl Pts',(0.272738680999945,15.2,10.886119805));
#223963=CARTESIAN_POINT('Ctrl Pts',(0.272738680999945,11.6,10.886119805));
#223964=CARTESIAN_POINT('Ctrl Pts',(0.271776950999945,15.2,10.883440855));
#223965=CARTESIAN_POINT('Ctrl Pts',(0.271776950999945,11.6,10.883440855));
#223966=CARTESIAN_POINT('Ctrl Pts',(0.270819344999945,15.2,10.880766399));
#223967=CARTESIAN_POINT('Ctrl Pts',(0.270819344999945,11.6,10.880766399));
#223968=CARTESIAN_POINT('Ctrl Pts',(0.269865859999945,15.2,10.878096449));
#223969=CARTESIAN_POINT('Ctrl Pts',(0.269865859999945,11.6,10.878096449));
#223970=CARTESIAN_POINT('Ctrl Pts',(0.268916491999944,15.2,10.875431019));
#223971=CARTESIAN_POINT('Ctrl Pts',(0.268916491999944,11.6,10.875431019));
#223972=CARTESIAN_POINT('Ctrl Pts',(0.267971236999944,15.2,10.872770121));
#223973=CARTESIAN_POINT('Ctrl Pts',(0.267971236999944,11.6,10.872770121));
#223974=CARTESIAN_POINT('Ctrl Pts',(0.267030088999943,15.2,10.870113767));
#223975=CARTESIAN_POINT('Ctrl Pts',(0.267030088999943,11.6,10.870113767));
#223976=CARTESIAN_POINT('Ctrl Pts',(0.266093045999943,15.2,10.867461969));
#223977=CARTESIAN_POINT('Ctrl Pts',(0.266093045999943,11.6,10.867461969));
#223978=CARTESIAN_POINT('Ctrl Pts',(0.265160102999945,15.2,10.864814741));
#223979=CARTESIAN_POINT('Ctrl Pts',(0.265160102999945,11.6,10.864814741));
#223980=CARTESIAN_POINT('Ctrl Pts',(0.264231254999944,15.2,10.862172095));
#223981=CARTESIAN_POINT('Ctrl Pts',(0.264231254999944,11.6,10.862172095));
#223982=CARTESIAN_POINT('Ctrl Pts',(0.263306497999943,15.2,10.859534043));
#223983=CARTESIAN_POINT('Ctrl Pts',(0.263306497999943,11.6,10.859534043));
#223984=CARTESIAN_POINT('Ctrl Pts',(0.262385827999945,15.2,10.856900597));
#223985=CARTESIAN_POINT('Ctrl Pts',(0.262385827999945,11.6,10.856900597));
#223986=CARTESIAN_POINT('Ctrl Pts',(0.261469239999944,15.2,10.854271772));
#223987=CARTESIAN_POINT('Ctrl Pts',(0.261469239999944,11.6,10.854271772));
#223988=CARTESIAN_POINT('Ctrl Pts',(0.260556730999945,15.2,10.851647579));
#223989=CARTESIAN_POINT('Ctrl Pts',(0.260556730999945,11.6,10.851647579));
#223990=CARTESIAN_POINT('Ctrl Pts',(0.259648296999944,15.2,10.84902803));
#223991=CARTESIAN_POINT('Ctrl Pts',(0.259648296999944,11.6,10.84902803));
#223992=CARTESIAN_POINT('Ctrl Pts',(0.258743930999945,15.2,10.846413139));
#223993=CARTESIAN_POINT('Ctrl Pts',(0.258743930999945,11.6,10.846413139));
#223994=CARTESIAN_POINT('Ctrl Pts',(0.257843629999943,15.2,10.843802919));
#223995=CARTESIAN_POINT('Ctrl Pts',(0.257843629999943,11.6,10.843802919));
#223996=CARTESIAN_POINT('Ctrl Pts',(0.256947389999944,15.2,10.841197381));
#223997=CARTESIAN_POINT('Ctrl Pts',(0.256947389999944,11.6,10.841197381));
#223998=CARTESIAN_POINT('Ctrl Pts',(0.256055205999944,15.2,10.838596539));
#223999=CARTESIAN_POINT('Ctrl Pts',(0.256055205999944,11.6,10.838596539));
#224000=CARTESIAN_POINT('Ctrl Pts',(0.255167071999944,15.2,10.836000406));
#224001=CARTESIAN_POINT('Ctrl Pts',(0.255167071999944,11.6,10.836000406));
#224002=CARTESIAN_POINT('Ctrl Pts',(0.254282986999945,15.2,10.833408995));
#224003=CARTESIAN_POINT('Ctrl Pts',(0.254282986999945,11.6,10.833408995));
#224004=CARTESIAN_POINT('Ctrl Pts',(0.253402944999944,15.2,10.830822318));
#224005=CARTESIAN_POINT('Ctrl Pts',(0.253402944999944,11.6,10.830822318));
#224006=CARTESIAN_POINT('Ctrl Pts',(0.252526938999944,15.2,10.828240388));
#224007=CARTESIAN_POINT('Ctrl Pts',(0.252526938999944,11.6,10.828240388));
#224008=CARTESIAN_POINT('Ctrl Pts',(0.251654968999944,15.2,10.825663219));
#224009=CARTESIAN_POINT('Ctrl Pts',(0.251654968999944,11.6,10.825663219));
#224010=CARTESIAN_POINT('Ctrl Pts',(0.250787026999945,15.2,10.823090823));
#224011=CARTESIAN_POINT('Ctrl Pts',(0.250787026999945,11.6,10.823090823));
#224012=CARTESIAN_POINT('Ctrl Pts',(0.249923107999944,15.2,10.820523213));
#224013=CARTESIAN_POINT('Ctrl Pts',(0.249923107999944,11.6,10.820523213));
#224014=CARTESIAN_POINT('Ctrl Pts',(0.249063209999945,15.2,10.817960403));
#224015=CARTESIAN_POINT('Ctrl Pts',(0.249063209999945,11.6,10.817960403));
#224016=CARTESIAN_POINT('Ctrl Pts',(0.248207326999944,15.2,10.815402405));
#224017=CARTESIAN_POINT('Ctrl Pts',(0.248207326999944,11.6,10.815402405));
#224018=CARTESIAN_POINT('Ctrl Pts',(0.247355453999945,15.2,10.812849232));
#224019=CARTESIAN_POINT('Ctrl Pts',(0.247355453999945,11.6,10.812849232));
#224020=CARTESIAN_POINT('Ctrl Pts',(0.246507586999943,15.2,10.810300898));
#224021=CARTESIAN_POINT('Ctrl Pts',(0.246507586999943,11.6,10.810300898));
#224022=CARTESIAN_POINT('Ctrl Pts',(0.245663720999945,15.2,10.807757416));
#224023=CARTESIAN_POINT('Ctrl Pts',(0.245663720999945,11.6,10.807757416));
#224024=CARTESIAN_POINT('Ctrl Pts',(0.244823849999944,15.2,10.805218799));
#224025=CARTESIAN_POINT('Ctrl Pts',(0.244823849999944,11.6,10.805218799));
#224026=CARTESIAN_POINT('Ctrl Pts',(0.243987971999945,15.2,10.80268506));
#224027=CARTESIAN_POINT('Ctrl Pts',(0.243987971999945,11.6,10.80268506));
#224028=CARTESIAN_POINT('Ctrl Pts',(0.243156079999943,15.2,10.800156212));
#224029=CARTESIAN_POINT('Ctrl Pts',(0.243156079999943,11.6,10.800156212));
#224030=CARTESIAN_POINT('Ctrl Pts',(0.242328170999944,15.2,10.797632269));
#224031=CARTESIAN_POINT('Ctrl Pts',(0.242328170999944,11.6,10.797632269));
#224032=CARTESIAN_POINT('Ctrl Pts',(0.241504236999944,15.2,10.795113244));
#224033=CARTESIAN_POINT('Ctrl Pts',(0.241504236999944,11.6,10.795113244));
#224034=CARTESIAN_POINT('Ctrl Pts',(0.240684276999945,15.2,10.79259915));
#224035=CARTESIAN_POINT('Ctrl Pts',(0.240684276999945,11.6,10.79259915));
#224036=CARTESIAN_POINT('Ctrl Pts',(0.239868283999943,15.2,10.790090001));
#224037=CARTESIAN_POINT('Ctrl Pts',(0.239868283999943,11.6,10.790090001));
#224038=CARTESIAN_POINT('Ctrl Pts',(0.239056252999944,15.2,10.78758581));
#224039=CARTESIAN_POINT('Ctrl Pts',(0.239056252999944,11.6,10.78758581));
#224040=CARTESIAN_POINT('Ctrl Pts',(0.238248179999945,15.2,10.78508659));
#224041=CARTESIAN_POINT('Ctrl Pts',(0.238248179999945,11.6,10.78508659));
#224042=CARTESIAN_POINT('Ctrl Pts',(0.237444059999945,15.2,10.782592356));
#224043=CARTESIAN_POINT('Ctrl Pts',(0.237444059999945,11.6,10.782592356));
#224044=CARTESIAN_POINT('Ctrl Pts',(0.236643886999944,15.2,10.780103119));
#224045=CARTESIAN_POINT('Ctrl Pts',(0.236643886999944,11.6,10.780103119));
#224046=CARTESIAN_POINT('Ctrl Pts',(0.235847656999945,15.2,10.777618895));
#224047=CARTESIAN_POINT('Ctrl Pts',(0.235847656999945,11.6,10.777618895));
#224048=CARTESIAN_POINT('Ctrl Pts',(0.235055364999944,15.2,10.775139696));
#224049=CARTESIAN_POINT('Ctrl Pts',(0.235055364999944,11.6,10.775139696));
#224050=CARTESIAN_POINT('Ctrl Pts',(0.234267004999945,15.2,10.772665536));
#224051=CARTESIAN_POINT('Ctrl Pts',(0.234267004999945,11.6,10.772665536));
#224052=CARTESIAN_POINT('Ctrl Pts',(0.233482572999945,15.2,10.770196429));
#224053=CARTESIAN_POINT('Ctrl Pts',(0.233482572999945,11.6,10.770196429));
#224054=CARTESIAN_POINT('Ctrl Pts',(0.232702063999944,15.2,10.767732388));
#224055=CARTESIAN_POINT('Ctrl Pts',(0.232702063999944,11.6,10.767732388));
#224056=CARTESIAN_POINT('Ctrl Pts',(0.231925471999944,15.2,10.765273427));
#224057=CARTESIAN_POINT('Ctrl Pts',(0.231925471999944,11.6,10.765273427));
#224058=CARTESIAN_POINT('Ctrl Pts',(0.231152791999945,15.2,10.762819561));
#224059=CARTESIAN_POINT('Ctrl Pts',(0.231152791999945,11.6,10.762819561));
#224060=CARTESIAN_POINT('Ctrl Pts',(0.230384019999944,15.2,10.760370801));
#224061=CARTESIAN_POINT('Ctrl Pts',(0.230384019999944,11.6,10.760370801));
#224062=CARTESIAN_POINT('Ctrl Pts',(0.229619148999944,15.2,10.757927164));
#224063=CARTESIAN_POINT('Ctrl Pts',(0.229619148999944,11.6,10.757927164));
#224064=CARTESIAN_POINT('Ctrl Pts',(0.228858174999944,15.2,10.755488661));
#224065=CARTESIAN_POINT('Ctrl Pts',(0.228858174999944,11.6,10.755488661));
#224066=CARTESIAN_POINT('Ctrl Pts',(0.228101093999945,15.2,10.753055306));
#224067=CARTESIAN_POINT('Ctrl Pts',(0.228101093999945,11.6,10.753055306));
#224068=CARTESIAN_POINT('Ctrl Pts',(0.227347897999944,15.2,10.750627115));
#224069=CARTESIAN_POINT('Ctrl Pts',(0.227347897999944,11.6,10.750627115));
#224070=CARTESIAN_POINT('Ctrl Pts',(0.226598583999945,15.2,10.748204101));
#224071=CARTESIAN_POINT('Ctrl Pts',(0.226598583999945,11.6,10.748204101));
#224072=CARTESIAN_POINT('Ctrl Pts',(0.225853144999943,15.2,10.745786278));
#224073=CARTESIAN_POINT('Ctrl Pts',(0.225853144999943,11.6,10.745786278));
#224074=CARTESIAN_POINT('Ctrl Pts',(0.225111577999944,15.2,10.743373659));
#224075=CARTESIAN_POINT('Ctrl Pts',(0.225111577999944,11.6,10.743373659));
#224076=CARTESIAN_POINT('Ctrl Pts',(0.224373874999945,15.2,10.740966259));
#224077=CARTESIAN_POINT('Ctrl Pts',(0.224373874999945,11.6,10.740966259));
#224078=CARTESIAN_POINT('Ctrl Pts',(0.223640032999944,15.2,10.738564091));
#224079=CARTESIAN_POINT('Ctrl Pts',(0.223640032999944,11.6,10.738564091));
#224080=CARTESIAN_POINT('Ctrl Pts',(0.222910043999944,15.2,10.736167171));
#224081=CARTESIAN_POINT('Ctrl Pts',(0.222910043999944,11.6,10.736167171));
#224082=CARTESIAN_POINT('Ctrl Pts',(0.222183904999945,15.2,10.733775512));
#224083=CARTESIAN_POINT('Ctrl Pts',(0.222183904999945,11.6,10.733775512));
#224084=CARTESIAN_POINT('Ctrl Pts',(0.221461608999943,15.2,10.731389127));
#224085=CARTESIAN_POINT('Ctrl Pts',(0.221461608999943,11.6,10.731389127));
#224086=CARTESIAN_POINT('Ctrl Pts',(0.220743151999944,15.2,10.729008033));
#224087=CARTESIAN_POINT('Ctrl Pts',(0.220743151999944,11.6,10.729008033));
#224088=CARTESIAN_POINT('Ctrl Pts',(0.220028526999944,15.2,10.726632242));
#224089=CARTESIAN_POINT('Ctrl Pts',(0.220028526999944,11.6,10.726632242));
#224090=CARTESIAN_POINT('Ctrl Pts',(0.219317728999944,15.2,10.724261769));
#224091=CARTESIAN_POINT('Ctrl Pts',(0.219317728999944,11.6,10.724261769));
#224092=CARTESIAN_POINT('Ctrl Pts',(0.218610752999944,15.2,10.721896627));
#224093=CARTESIAN_POINT('Ctrl Pts',(0.218610752999944,11.6,10.721896627));
#224094=CARTESIAN_POINT('Ctrl Pts',(0.217907592999945,15.2,10.719536832));
#224095=CARTESIAN_POINT('Ctrl Pts',(0.217907592999945,11.6,10.719536832));
#224096=CARTESIAN_POINT('Ctrl Pts',(0.217208243999943,15.2,10.717182399));
#224097=CARTESIAN_POINT('Ctrl Pts',(0.217208243999943,11.6,10.717182399));
#224098=CARTESIAN_POINT('Ctrl Pts',(0.216512699999944,15.2,10.71483334));
#224099=CARTESIAN_POINT('Ctrl Pts',(0.216512699999944,11.6,10.71483334));
#224100=CARTESIAN_POINT('Ctrl Pts',(0.215820953999944,15.2,10.712489672));
#224101=CARTESIAN_POINT('Ctrl Pts',(0.215820953999944,11.6,10.712489672));
#224102=CARTESIAN_POINT('Ctrl Pts',(0.215133002999943,15.2,10.710151408));
#224103=CARTESIAN_POINT('Ctrl Pts',(0.215133002999943,11.6,10.710151408));
#224104=CARTESIAN_POINT('Ctrl Pts',(0.214448838999944,15.2,10.707818563));
#224105=CARTESIAN_POINT('Ctrl Pts',(0.214448838999944,11.6,10.707818563));
#224106=CARTESIAN_POINT('Ctrl Pts',(0.213768457999944,15.2,10.70549115));
#224107=CARTESIAN_POINT('Ctrl Pts',(0.213768457999944,11.6,10.70549115));
#224108=CARTESIAN_POINT('Ctrl Pts',(0.213091851999945,15.2,10.703169186));
#224109=CARTESIAN_POINT('Ctrl Pts',(0.213091851999945,11.6,10.703169186));
#224110=CARTESIAN_POINT('Ctrl Pts',(0.212419017999944,15.2,10.700852684));
#224111=CARTESIAN_POINT('Ctrl Pts',(0.212419017999944,11.6,10.700852684));
#224112=CARTESIAN_POINT('Ctrl Pts',(0.211749947999945,15.2,10.69854166));
#224113=CARTESIAN_POINT('Ctrl Pts',(0.211749947999945,11.6,10.69854166));
#224114=CARTESIAN_POINT('Ctrl Pts',(0.211084637999944,15.2,10.696236128));
#224115=CARTESIAN_POINT('Ctrl Pts',(0.211084637999944,11.6,10.696236128));
#224116=CARTESIAN_POINT('Ctrl Pts',(0.210423080999943,15.2,10.693936102));
#224117=CARTESIAN_POINT('Ctrl Pts',(0.210423080999943,11.6,10.693936102));
#224118=CARTESIAN_POINT('Ctrl Pts',(0.209765270999943,15.2,10.691641598));
#224119=CARTESIAN_POINT('Ctrl Pts',(0.209765270999943,11.6,10.691641598));
#224120=CARTESIAN_POINT('Ctrl Pts',(0.209111202999944,15.2,10.68935263));
#224121=CARTESIAN_POINT('Ctrl Pts',(0.209111202999944,11.6,10.68935263));
#224122=CARTESIAN_POINT('Ctrl Pts',(0.208460869999945,15.2,10.687069213));
#224123=CARTESIAN_POINT('Ctrl Pts',(0.208460869999945,11.6,10.687069213));
#224124=CARTESIAN_POINT('Ctrl Pts',(0.207814266999945,15.2,10.684791362));
#224125=CARTESIAN_POINT('Ctrl Pts',(0.207814266999945,11.6,10.684791362));
#224126=CARTESIAN_POINT('Ctrl Pts',(0.207171385999944,15.2,10.682519093));
#224127=CARTESIAN_POINT('Ctrl Pts',(0.207171385999944,11.6,10.682519093));
#224128=CARTESIAN_POINT('Ctrl Pts',(0.206532223999943,15.2,10.680252419));
#224129=CARTESIAN_POINT('Ctrl Pts',(0.206532223999943,11.6,10.680252419));
#224130=CARTESIAN_POINT('Ctrl Pts',(0.205896773999944,15.2,10.677991356));
#224131=CARTESIAN_POINT('Ctrl Pts',(0.205896773999944,11.6,10.677991356));
#224132=CARTESIAN_POINT('Ctrl Pts',(0.205265027999945,15.2,10.67573592));
#224133=CARTESIAN_POINT('Ctrl Pts',(0.205265027999945,11.6,10.67573592));
#224134=CARTESIAN_POINT('Ctrl Pts',(0.204636982999944,15.2,10.673486125));
#224135=CARTESIAN_POINT('Ctrl Pts',(0.204636982999944,11.6,10.673486125));
#224136=CARTESIAN_POINT('Ctrl Pts',(0.204012629999945,15.2,10.671241985));
#224137=CARTESIAN_POINT('Ctrl Pts',(0.204012629999945,11.6,10.671241985));
#224138=CARTESIAN_POINT('Ctrl Pts',(0.203391963999945,15.2,10.669003518));
#224139=CARTESIAN_POINT('Ctrl Pts',(0.203391963999945,11.6,10.669003518));
#224140=CARTESIAN_POINT('Ctrl Pts',(0.202774978999944,15.2,10.666770738));
#224141=CARTESIAN_POINT('Ctrl Pts',(0.202774978999944,11.6,10.666770738));
#224142=CARTESIAN_POINT('Ctrl Pts',(0.202161669999944,15.2,10.664543659));
#224143=CARTESIAN_POINT('Ctrl Pts',(0.202161669999944,11.6,10.664543659));
#224144=CARTESIAN_POINT('Ctrl Pts',(0.201552027999944,15.2,10.662322298));
#224145=CARTESIAN_POINT('Ctrl Pts',(0.201552027999944,11.6,10.662322298));
#224146=CARTESIAN_POINT('Ctrl Pts',(0.200946048999944,15.2,10.660106669));
#224147=CARTESIAN_POINT('Ctrl Pts',(0.200946048999944,11.6,10.660106669));
#224148=CARTESIAN_POINT('Ctrl Pts',(0.200343724999945,15.2,10.657896788));
#224149=CARTESIAN_POINT('Ctrl Pts',(0.200343724999945,11.6,10.657896788));
#224150=CARTESIAN_POINT('Ctrl Pts',(0.199745050999944,15.2,10.655692671));
#224151=CARTESIAN_POINT('Ctrl Pts',(0.199745050999944,11.6,10.655692671));
#224152=CARTESIAN_POINT('Ctrl Pts',(0.199150019999944,15.2,10.653494334));
#224153=CARTESIAN_POINT('Ctrl Pts',(0.199150019999944,11.6,10.653494334));
#224154=CARTESIAN_POINT('Ctrl Pts',(0.198558625999944,15.2,10.651301789));
#224155=CARTESIAN_POINT('Ctrl Pts',(0.198558625999944,11.6,10.651301789));
#224156=CARTESIAN_POINT('Ctrl Pts',(0.197970861999943,15.2,10.649115056));
#224157=CARTESIAN_POINT('Ctrl Pts',(0.197970861999943,11.6,10.649115056));
#224158=CARTESIAN_POINT('Ctrl Pts',(0.197386722999945,15.2,10.646934148));
#224159=CARTESIAN_POINT('Ctrl Pts',(0.197386722999945,11.6,10.646934148));
#224160=CARTESIAN_POINT('Ctrl Pts',(0.196806200999945,15.2,10.644759081));
#224161=CARTESIAN_POINT('Ctrl Pts',(0.196806200999945,11.6,10.644759081));
#224162=CARTESIAN_POINT('Ctrl Pts',(0.196229288999945,15.2,10.642589871));
#224163=CARTESIAN_POINT('Ctrl Pts',(0.196229288999945,11.6,10.642589871));
#224164=CARTESIAN_POINT('Ctrl Pts',(0.195655981999945,15.2,10.640426535));
#224165=CARTESIAN_POINT('Ctrl Pts',(0.195655981999945,11.6,10.640426535));
#224166=CARTESIAN_POINT('Ctrl Pts',(0.195086272999945,15.2,10.638269086));
#224167=CARTESIAN_POINT('Ctrl Pts',(0.195086272999945,11.6,10.638269086));
#224168=CARTESIAN_POINT('Ctrl Pts',(0.194520154999944,15.2,10.636117541));
#224169=CARTESIAN_POINT('Ctrl Pts',(0.194520154999944,11.6,10.636117541));
#224170=CARTESIAN_POINT('Ctrl Pts',(0.193957621999944,15.2,10.633971917));
#224171=CARTESIAN_POINT('Ctrl Pts',(0.193957621999944,11.6,10.633971917));
#224172=CARTESIAN_POINT('Ctrl Pts',(0.193398666999943,15.2,10.631832228));
#224173=CARTESIAN_POINT('Ctrl Pts',(0.193398666999943,11.6,10.631832228));
#224174=CARTESIAN_POINT('Ctrl Pts',(0.192843282999944,15.2,10.629698493));
#224175=CARTESIAN_POINT('Ctrl Pts',(0.192843282999944,11.6,10.629698493));
#224176=CARTESIAN_POINT('Ctrl Pts',(0.192291463999944,15.2,10.627570724));
#224177=CARTESIAN_POINT('Ctrl Pts',(0.192291463999944,11.6,10.627570724));
#224178=CARTESIAN_POINT('Ctrl Pts',(0.191743202999944,15.2,10.62544894));
#224179=CARTESIAN_POINT('Ctrl Pts',(0.191743202999944,11.6,10.62544894));
#224180=CARTESIAN_POINT('Ctrl Pts',(0.191198490999945,15.2,10.623333156));
#224181=CARTESIAN_POINT('Ctrl Pts',(0.191198490999945,11.6,10.623333156));
#224182=CARTESIAN_POINT('Ctrl Pts',(0.190657324999943,15.2,10.621223388));
#224183=CARTESIAN_POINT('Ctrl Pts',(0.190657324999943,11.6,10.621223388));
#224184=CARTESIAN_POINT('Ctrl Pts',(0.190119695999943,15.2,10.619119652));
#224185=CARTESIAN_POINT('Ctrl Pts',(0.190119695999943,11.6,10.619119652));
#224186=CARTESIAN_POINT('Ctrl Pts',(0.189585597999944,15.2,10.617021966));
#224187=CARTESIAN_POINT('Ctrl Pts',(0.189585597999944,11.6,10.617021966));
#224188=CARTESIAN_POINT('Ctrl Pts',(0.189055023999943,15.2,10.614930343));
#224189=CARTESIAN_POINT('Ctrl Pts',(0.189055023999943,11.6,10.614930343));
#224190=CARTESIAN_POINT('Ctrl Pts',(0.188527964999944,15.2,10.612844803));
#224191=CARTESIAN_POINT('Ctrl Pts',(0.188527964999944,11.6,10.612844803));
#224192=CARTESIAN_POINT('Ctrl Pts',(0.188004415999944,15.2,10.61076536));
#224193=CARTESIAN_POINT('Ctrl Pts',(0.188004415999944,11.6,10.61076536));
#224194=CARTESIAN_POINT('Ctrl Pts',(0.187484369999943,15.2,10.608692031));
#224195=CARTESIAN_POINT('Ctrl Pts',(0.187484369999943,11.6,10.608692031));
#224196=CARTESIAN_POINT('Ctrl Pts',(0.186967819999945,15.2,10.606624832));
#224197=CARTESIAN_POINT('Ctrl Pts',(0.186967819999945,11.6,10.606624832));
#224198=CARTESIAN_POINT('Ctrl Pts',(0.186454757999943,15.2,10.604563781));
#224199=CARTESIAN_POINT('Ctrl Pts',(0.186454757999943,11.6,10.604563781));
#224200=CARTESIAN_POINT('Ctrl Pts',(0.185945176999944,15.2,10.602508892));
#224201=CARTESIAN_POINT('Ctrl Pts',(0.185945176999944,11.6,10.602508892));
#224202=CARTESIAN_POINT('Ctrl Pts',(0.185439070999944,15.2,10.600460184));
#224203=CARTESIAN_POINT('Ctrl Pts',(0.185439070999944,11.6,10.600460184));
#224204=CARTESIAN_POINT('Ctrl Pts',(0.184936431999944,15.2,10.598417673));
#224205=CARTESIAN_POINT('Ctrl Pts',(0.184936431999944,11.6,10.598417673));
#224206=CARTESIAN_POINT('Ctrl Pts',(0.184437252999944,15.2,10.596381375));
#224207=CARTESIAN_POINT('Ctrl Pts',(0.184437252999944,11.6,10.596381375));
#224208=CARTESIAN_POINT('Ctrl Pts',(0.183941525999943,15.2,10.594351307));
#224209=CARTESIAN_POINT('Ctrl Pts',(0.183941525999943,11.6,10.594351307));
#224210=CARTESIAN_POINT('Ctrl Pts',(0.183449243999944,15.2,10.592327487));
#224211=CARTESIAN_POINT('Ctrl Pts',(0.183449243999944,11.6,10.592327487));
#224212=CARTESIAN_POINT('Ctrl Pts',(0.182960400999944,15.2,10.59030993));
#224213=CARTESIAN_POINT('Ctrl Pts',(0.182960400999944,11.6,10.59030993));
#224214=CARTESIAN_POINT('Ctrl Pts',(0.182474987999944,15.2,10.588298654));
#224215=CARTESIAN_POINT('Ctrl Pts',(0.182474987999944,11.6,10.588298654));
#224216=CARTESIAN_POINT('Ctrl Pts',(0.181992997999944,15.2,10.586293676));
#224217=CARTESIAN_POINT('Ctrl Pts',(0.181992997999944,11.6,10.586293676));
#224218=CARTESIAN_POINT('Ctrl Pts',(0.181514424999945,15.2,10.584295013));
#224219=CARTESIAN_POINT('Ctrl Pts',(0.181514424999945,11.6,10.584295013));
#224220=CARTESIAN_POINT('Ctrl Pts',(0.181039259999943,15.2,10.582302681));
#224221=CARTESIAN_POINT('Ctrl Pts',(0.181039259999943,11.6,10.582302681));
#224222=CARTESIAN_POINT('Ctrl Pts',(0.180567494999944,15.2,10.580316698));
#224223=CARTESIAN_POINT('Ctrl Pts',(0.180567494999944,11.6,10.580316698));
#224224=CARTESIAN_POINT('Ctrl Pts',(0.180099123999945,15.2,10.578337082));
#224225=CARTESIAN_POINT('Ctrl Pts',(0.180099123999945,11.6,10.578337082));
#224226=CARTESIAN_POINT('Ctrl Pts',(0.179634138999945,15.2,10.576363848));
#224227=CARTESIAN_POINT('Ctrl Pts',(0.179634138999945,11.6,10.576363848));
#224228=CARTESIAN_POINT('Ctrl Pts',(0.179172531999944,15.2,10.574397014));
#224229=CARTESIAN_POINT('Ctrl Pts',(0.179172531999944,11.6,10.574397014));
#224230=CARTESIAN_POINT('Ctrl Pts',(0.178714295999944,15.2,10.5724366));
#224231=CARTESIAN_POINT('Ctrl Pts',(0.178714295999944,11.6,10.5724366));
#224232=CARTESIAN_POINT('Ctrl Pts',(0.178259421999943,15.2,10.570482619));
#224233=CARTESIAN_POINT('Ctrl Pts',(0.178259421999943,11.6,10.570482619));
#224234=CARTESIAN_POINT('Ctrl Pts',(0.177807903999945,15.2,10.568535092));
#224235=CARTESIAN_POINT('Ctrl Pts',(0.177807903999945,11.6,10.568535092));
#224236=CARTESIAN_POINT('Ctrl Pts',(0.177359733999944,15.2,10.566594034));
#224237=CARTESIAN_POINT('Ctrl Pts',(0.177359733999944,11.6,10.566594034));
#224238=CARTESIAN_POINT('Ctrl Pts',(0.176914901999944,15.2,10.564659464));
#224239=CARTESIAN_POINT('Ctrl Pts',(0.176914901999944,11.6,10.564659464));
#224240=CARTESIAN_POINT('Ctrl Pts',(0.176473402999945,15.2,10.5627314));
#224241=CARTESIAN_POINT('Ctrl Pts',(0.176473402999945,11.6,10.5627314));
#224242=CARTESIAN_POINT('Ctrl Pts',(0.176035227999943,15.2,10.560809858));
#224243=CARTESIAN_POINT('Ctrl Pts',(0.176035227999943,11.6,10.560809858));
#224244=CARTESIAN_POINT('Ctrl Pts',(0.175600368999945,15.2,10.558894856));
#224245=CARTESIAN_POINT('Ctrl Pts',(0.175600368999945,11.6,10.558894856));
#224246=CARTESIAN_POINT('Ctrl Pts',(0.175168817999944,15.2,10.556986414));
#224247=CARTESIAN_POINT('Ctrl Pts',(0.175168817999944,11.6,10.556986414));
#224248=CARTESIAN_POINT('Ctrl Pts',(0.174740566999944,15.2,10.555084546));
#224249=CARTESIAN_POINT('Ctrl Pts',(0.174740566999944,11.6,10.555084546));
#224250=CARTESIAN_POINT('Ctrl Pts',(0.174315608999944,15.2,10.553189272));
#224251=CARTESIAN_POINT('Ctrl Pts',(0.174315608999944,11.6,10.553189272));
#224252=CARTESIAN_POINT('Ctrl Pts',(0.173893933999943,15.2,10.551300611));
#224253=CARTESIAN_POINT('Ctrl Pts',(0.173893933999943,11.6,10.551300611));
#224254=CARTESIAN_POINT('Ctrl Pts',(0.173475535999945,15.2,10.549418579));
#224255=CARTESIAN_POINT('Ctrl Pts',(0.173475535999945,11.6,10.549418579));
#224256=CARTESIAN_POINT('Ctrl Pts',(0.173060405999944,15.2,10.547543196));
#224257=CARTESIAN_POINT('Ctrl Pts',(0.173060405999944,11.6,10.547543196));
#224258=CARTESIAN_POINT('Ctrl Pts',(0.172648535999944,15.2,10.545674477));
#224259=CARTESIAN_POINT('Ctrl Pts',(0.172648535999944,11.6,10.545674477));
#224260=CARTESIAN_POINT('Ctrl Pts',(0.172239915999944,15.2,10.543812444));
#224261=CARTESIAN_POINT('Ctrl Pts',(0.172239915999944,11.6,10.543812444));
#224262=CARTESIAN_POINT('Ctrl Pts',(0.171834540999944,15.2,10.541957111));
#224263=CARTESIAN_POINT('Ctrl Pts',(0.171834540999944,11.6,10.541957111));
#224264=CARTESIAN_POINT('Ctrl Pts',(0.171432399999943,15.2,10.5401085));
#224265=CARTESIAN_POINT('Ctrl Pts',(0.171432399999943,11.6,10.5401085));
#224266=CARTESIAN_POINT('Ctrl Pts',(0.171033485999944,15.2,10.538266627));
#224267=CARTESIAN_POINT('Ctrl Pts',(0.171033485999944,11.6,10.538266627));
#224268=CARTESIAN_POINT('Ctrl Pts',(0.170637789999945,15.2,10.536431512));
#224269=CARTESIAN_POINT('Ctrl Pts',(0.170637789999945,11.6,10.536431512));
#224270=CARTESIAN_POINT('Ctrl Pts',(0.170245304999943,15.2,10.534603171));
#224271=CARTESIAN_POINT('Ctrl Pts',(0.170245304999943,11.6,10.534603171));
#224272=CARTESIAN_POINT('Ctrl Pts',(0.169856019999944,15.2,10.532781625));
#224273=CARTESIAN_POINT('Ctrl Pts',(0.169856019999944,11.6,10.532781625));
#224274=CARTESIAN_POINT('Ctrl Pts',(0.169469929999944,15.2,10.530966892));
#224275=CARTESIAN_POINT('Ctrl Pts',(0.169469929999944,11.6,10.530966892));
#224276=CARTESIAN_POINT('Ctrl Pts',(0.169087021999944,15.2,10.52915899));
#224277=CARTESIAN_POINT('Ctrl Pts',(0.169087021999944,11.6,10.52915899));
#224278=CARTESIAN_POINT('Ctrl Pts',(0.168707291999944,15.2,10.527357938));
#224279=CARTESIAN_POINT('Ctrl Pts',(0.168707291999944,11.6,10.527357938));
#224280=CARTESIAN_POINT('Ctrl Pts',(0.168330727999945,15.2,10.525563754));
#224281=CARTESIAN_POINT('Ctrl Pts',(0.168330727999945,11.6,10.525563754));
#224282=CARTESIAN_POINT('Ctrl Pts',(0.167957322999944,15.2,10.523776458));
#224283=CARTESIAN_POINT('Ctrl Pts',(0.167957322999944,11.6,10.523776458));
#224284=CARTESIAN_POINT('Ctrl Pts',(0.167587068999945,15.2,10.521996069));
#224285=CARTESIAN_POINT('Ctrl Pts',(0.167587068999945,11.6,10.521996069));
#224286=CARTESIAN_POINT('Ctrl Pts',(0.167219954999943,15.2,10.520222605));
#224287=CARTESIAN_POINT('Ctrl Pts',(0.167219954999943,11.6,10.520222605));
#224288=CARTESIAN_POINT('Ctrl Pts',(0.166855973999944,15.2,10.518456083));
#224289=CARTESIAN_POINT('Ctrl Pts',(0.166855973999944,11.6,10.518456083));
#224290=CARTESIAN_POINT('Ctrl Pts',(0.166495116999944,15.2,10.516696527));
#224291=CARTESIAN_POINT('Ctrl Pts',(0.166495116999944,11.6,10.516696527));
#224292=CARTESIAN_POINT('Ctrl Pts',(0.166137373999945,15.2,10.514943952));
#224293=CARTESIAN_POINT('Ctrl Pts',(0.166137373999945,11.6,10.514943952));
#224294=CARTESIAN_POINT('Ctrl Pts',(0.165782736999944,15.2,10.513198379));
#224295=CARTESIAN_POINT('Ctrl Pts',(0.165782736999944,11.6,10.513198379));
#224296=CARTESIAN_POINT('Ctrl Pts',(0.165431195999943,15.2,10.511459827));
#224297=CARTESIAN_POINT('Ctrl Pts',(0.165431195999943,11.6,10.511459827));
#224298=CARTESIAN_POINT('Ctrl Pts',(0.165082743999945,15.2,10.509728314));
#224299=CARTESIAN_POINT('Ctrl Pts',(0.165082743999945,11.6,10.509728314));
#224300=CARTESIAN_POINT('Ctrl Pts',(0.164737370999944,15.2,10.508003861));
#224301=CARTESIAN_POINT('Ctrl Pts',(0.164737370999944,11.6,10.508003861));
#224302=CARTESIAN_POINT('Ctrl Pts',(0.164395066999944,15.2,10.506286488));
#224303=CARTESIAN_POINT('Ctrl Pts',(0.164395066999944,11.6,10.506286488));
#224304=CARTESIAN_POINT('Ctrl Pts',(0.164055823999943,15.2,10.504576213));
#224305=CARTESIAN_POINT('Ctrl Pts',(0.164055823999943,11.6,10.504576213));
#224306=CARTESIAN_POINT('Ctrl Pts',(0.163719631999945,15.2,10.502873055));
#224307=CARTESIAN_POINT('Ctrl Pts',(0.163719631999945,11.6,10.502873055));
#224308=CARTESIAN_POINT('Ctrl Pts',(0.163386482999943,15.2,10.501177035));
#224309=CARTESIAN_POINT('Ctrl Pts',(0.163386482999943,11.6,10.501177035));
#224310=CARTESIAN_POINT('Ctrl Pts',(0.163056365999944,15.2,10.499488173));
#224311=CARTESIAN_POINT('Ctrl Pts',(0.163056365999944,11.6,10.499488173));
#224312=CARTESIAN_POINT('Ctrl Pts',(0.162729271999943,15.2,10.497806487));
#224313=CARTESIAN_POINT('Ctrl Pts',(0.162729271999943,11.6,10.497806487));
#224314=CARTESIAN_POINT('Ctrl Pts',(0.162405193999945,15.2,10.496131999));
#224315=CARTESIAN_POINT('Ctrl Pts',(0.162405193999945,11.6,10.496131999));
#224316=CARTESIAN_POINT('Ctrl Pts',(0.162084119999945,15.2,10.494464727));
#224317=CARTESIAN_POINT('Ctrl Pts',(0.162084119999945,11.6,10.494464727));
#224318=CARTESIAN_POINT('Ctrl Pts',(0.161766040999943,15.2,10.492804693));
#224319=CARTESIAN_POINT('Ctrl Pts',(0.161766040999943,11.6,10.492804693));
#224320=CARTESIAN_POINT('Ctrl Pts',(0.161450947999944,15.2,10.491151915));
#224321=CARTESIAN_POINT('Ctrl Pts',(0.161450947999944,11.6,10.491151915));
#224322=CARTESIAN_POINT('Ctrl Pts',(0.161138831999944,15.2,10.489506414));
#224323=CARTESIAN_POINT('Ctrl Pts',(0.161138831999944,11.6,10.489506414));
#224324=CARTESIAN_POINT('Ctrl Pts',(0.160829681999944,15.2,10.487868211));
#224325=CARTESIAN_POINT('Ctrl Pts',(0.160829681999944,11.6,10.487868211));
#224326=CARTESIAN_POINT('Ctrl Pts',(0.160523488999944,15.2,10.486237324));
#224327=CARTESIAN_POINT('Ctrl Pts',(0.160523488999944,11.6,10.486237324));
#224328=CARTESIAN_POINT('Ctrl Pts',(0.160220243999945,15.2,10.484613776));
#224329=CARTESIAN_POINT('Ctrl Pts',(0.160220243999945,11.6,10.484613776));
#224330=CARTESIAN_POINT('Ctrl Pts',(0.159919935999945,15.2,10.482997587));
#224331=CARTESIAN_POINT('Ctrl Pts',(0.159919935999945,11.6,10.482997587));
#224332=CARTESIAN_POINT('Ctrl Pts',(0.159622555999944,15.2,10.481388775));
#224333=CARTESIAN_POINT('Ctrl Pts',(0.159622555999944,11.6,10.481388775));
#224334=CARTESIAN_POINT('Ctrl Pts',(0.159328093999944,15.2,10.479787363));
#224335=CARTESIAN_POINT('Ctrl Pts',(0.159328093999944,11.6,10.479787363));
#224336=CARTESIAN_POINT('Ctrl Pts',(0.159036538999944,15.2,10.478193371));
#224337=CARTESIAN_POINT('Ctrl Pts',(0.159036538999944,11.6,10.478193371));
#224338=CARTESIAN_POINT('Ctrl Pts',(0.158747883999943,15.2,10.476606819));
#224339=CARTESIAN_POINT('Ctrl Pts',(0.158747883999943,11.6,10.476606819));
#224340=CARTESIAN_POINT('Ctrl Pts',(0.158462115999944,15.2,10.475027729));
#224341=CARTESIAN_POINT('Ctrl Pts',(0.158462115999944,11.6,10.475027729));
#224342=CARTESIAN_POINT('Ctrl Pts',(0.158179225999945,15.2,10.473456121));
#224343=CARTESIAN_POINT('Ctrl Pts',(0.158179225999945,11.6,10.473456121));
#224344=CARTESIAN_POINT('Ctrl Pts',(0.157899203999945,15.2,10.471892016));
#224345=CARTESIAN_POINT('Ctrl Pts',(0.157899203999945,11.6,10.471892016));
#224346=CARTESIAN_POINT('Ctrl Pts',(0.157622040999945,15.2,10.470335436));
#224347=CARTESIAN_POINT('Ctrl Pts',(0.157622040999945,11.6,10.470335436));
#224348=CARTESIAN_POINT('Ctrl Pts',(0.157347723999944,15.2,10.4687864));
#224349=CARTESIAN_POINT('Ctrl Pts',(0.157347723999944,11.6,10.4687864));
#224350=CARTESIAN_POINT('Ctrl Pts',(0.157076244999944,15.2,10.467244932));
#224351=CARTESIAN_POINT('Ctrl Pts',(0.157076244999944,11.6,10.467244932));
#224352=CARTESIAN_POINT('Ctrl Pts',(0.156807592999944,15.2,10.46571105));
#224353=CARTESIAN_POINT('Ctrl Pts',(0.156807592999944,11.6,10.46571105));
#224354=CARTESIAN_POINT('Ctrl Pts',(0.156541757999945,15.2,10.464184777));
#224355=CARTESIAN_POINT('Ctrl Pts',(0.156541757999945,11.6,10.464184777));
#224356=CARTESIAN_POINT('Ctrl Pts',(0.156278728999943,15.2,10.462666136));
#224357=CARTESIAN_POINT('Ctrl Pts',(0.156278728999943,11.6,10.462666136));
#224358=CARTESIAN_POINT('Ctrl Pts',(0.156018494999944,15.2,10.461155145));
#224359=CARTESIAN_POINT('Ctrl Pts',(0.156018494999944,11.6,10.461155145));
#224360=CARTESIAN_POINT('Ctrl Pts',(0.155761047999944,15.2,10.459651829));
#224361=CARTESIAN_POINT('Ctrl Pts',(0.155761047999944,11.6,10.459651829));
#224362=CARTESIAN_POINT('Ctrl Pts',(0.155506374999945,15.2,10.458156207));
#224363=CARTESIAN_POINT('Ctrl Pts',(0.155506374999945,11.6,10.458156207));
#224364=CARTESIAN_POINT('Ctrl Pts',(0.155254464999944,15.2,10.456668303));
#224365=CARTESIAN_POINT('Ctrl Pts',(0.155254464999944,11.6,10.456668303));
#224366=CARTESIAN_POINT('Ctrl Pts',(0.155005309999944,15.2,10.455188137));
#224367=CARTESIAN_POINT('Ctrl Pts',(0.155005309999944,11.6,10.455188137));
#224368=CARTESIAN_POINT('Ctrl Pts',(0.154758896999944,15.2,10.45371573));
#224369=CARTESIAN_POINT('Ctrl Pts',(0.154758896999944,11.6,10.45371573));
#224370=CARTESIAN_POINT('Ctrl Pts',(0.154515215999943,15.2,10.452251107));
#224371=CARTESIAN_POINT('Ctrl Pts',(0.154515215999943,11.6,10.452251107));
#224372=CARTESIAN_POINT('Ctrl Pts',(0.154274255999944,15.2,10.450794288));
#224373=CARTESIAN_POINT('Ctrl Pts',(0.154274255999944,11.6,10.450794288));
#224374=CARTESIAN_POINT('Ctrl Pts',(0.154036005999943,15.2,10.449345296));
#224375=CARTESIAN_POINT('Ctrl Pts',(0.154036005999943,11.6,10.449345296));
#224376=CARTESIAN_POINT('Ctrl Pts',(0.153800454999944,15.2,10.447904152));
#224377=CARTESIAN_POINT('Ctrl Pts',(0.153800454999944,11.6,10.447904152));
#224378=CARTESIAN_POINT('Ctrl Pts',(0.153567591999944,15.2,10.44647088));
#224379=CARTESIAN_POINT('Ctrl Pts',(0.153567591999944,11.6,10.44647088));
#224380=CARTESIAN_POINT('Ctrl Pts',(0.153337406999944,15.2,10.445045501));
#224381=CARTESIAN_POINT('Ctrl Pts',(0.153337406999944,11.6,10.445045501));
#224382=CARTESIAN_POINT('Ctrl Pts',(0.153109886999945,15.2,10.443628039));
#224383=CARTESIAN_POINT('Ctrl Pts',(0.153109886999945,11.6,10.443628039));
#224384=CARTESIAN_POINT('Ctrl Pts',(0.152885021999944,15.2,10.442218514));
#224385=CARTESIAN_POINT('Ctrl Pts',(0.152885021999944,11.6,10.442218514));
#224386=CARTESIAN_POINT('Ctrl Pts',(0.152662799999945,15.2,10.440816951));
#224387=CARTESIAN_POINT('Ctrl Pts',(0.152662799999945,11.6,10.440816951));
#224388=CARTESIAN_POINT('Ctrl Pts',(0.152443210999945,15.2,10.439423373));
#224389=CARTESIAN_POINT('Ctrl Pts',(0.152443210999945,11.6,10.439423373));
#224390=CARTESIAN_POINT('Ctrl Pts',(0.152226241999944,15.2,10.4380378));
#224391=CARTESIAN_POINT('Ctrl Pts',(0.152226241999944,11.6,10.4380378));
#224392=CARTESIAN_POINT('Ctrl Pts',(0.152011882999944,15.2,10.436660258));
#224393=CARTESIAN_POINT('Ctrl Pts',(0.152011882999944,11.6,10.436660258));
#224394=CARTESIAN_POINT('Ctrl Pts',(0.151800121999944,15.2,10.435290769));
#224395=CARTESIAN_POINT('Ctrl Pts',(0.151800121999944,11.6,10.435290769));
#224396=CARTESIAN_POINT('Ctrl Pts',(0.151590946999944,15.2,10.433929355));
#224397=CARTESIAN_POINT('Ctrl Pts',(0.151590946999944,11.6,10.433929355));
#224398=CARTESIAN_POINT('Ctrl Pts',(0.151384345999944,15.2,10.432576041));
#224399=CARTESIAN_POINT('Ctrl Pts',(0.151384345999944,11.6,10.432576041));
#224400=CARTESIAN_POINT('Ctrl Pts',(0.151180308999944,15.2,10.431230849));
#224401=CARTESIAN_POINT('Ctrl Pts',(0.151180308999944,11.6,10.431230849));
#224402=CARTESIAN_POINT('Ctrl Pts',(0.150978822999944,15.2,10.429893802));
#224403=CARTESIAN_POINT('Ctrl Pts',(0.150978822999944,11.6,10.429893802));
#224404=CARTESIAN_POINT('Ctrl Pts',(0.150779875999945,15.2,10.428564925));
#224405=CARTESIAN_POINT('Ctrl Pts',(0.150779875999945,11.6,10.428564925));
#224406=CARTESIAN_POINT('Ctrl Pts',(0.150583456999945,15.2,10.427244241));
#224407=CARTESIAN_POINT('Ctrl Pts',(0.150583456999945,11.6,10.427244241));
#224408=CARTESIAN_POINT('Ctrl Pts',(0.150389552999943,15.2,10.425931773));
#224409=CARTESIAN_POINT('Ctrl Pts',(0.150389552999943,11.6,10.425931773));
#224410=CARTESIAN_POINT('Ctrl Pts',(0.150198153999943,15.2,10.424627546));
#224411=CARTESIAN_POINT('Ctrl Pts',(0.150198153999943,11.6,10.424627546));
#224412=CARTESIAN_POINT('Ctrl Pts',(0.150009245999945,15.2,10.423331583));
#224413=CARTESIAN_POINT('Ctrl Pts',(0.150009245999945,11.6,10.423331583));
#224414=CARTESIAN_POINT('Ctrl Pts',(0.149822815999944,15.2,10.422043908));
#224415=CARTESIAN_POINT('Ctrl Pts',(0.149822815999944,11.6,10.422043908));
#224416=CARTESIAN_POINT('Ctrl Pts',(0.149638854999944,15.2,10.420764544));
#224417=CARTESIAN_POINT('Ctrl Pts',(0.149638854999944,11.6,10.420764544));
#224418=CARTESIAN_POINT('Ctrl Pts',(0.149457348999944,15.2,10.419493518));
#224419=CARTESIAN_POINT('Ctrl Pts',(0.149457348999944,11.6,10.419493518));
#224420=CARTESIAN_POINT('Ctrl Pts',(0.149278284999944,15.2,10.418230853));
#224421=CARTESIAN_POINT('Ctrl Pts',(0.149278284999944,11.6,10.418230853));
#224422=CARTESIAN_POINT('Ctrl Pts',(0.149101651999944,15.2,10.416976571));
#224423=CARTESIAN_POINT('Ctrl Pts',(0.149101651999944,11.6,10.416976571));
#224424=CARTESIAN_POINT('Ctrl Pts',(0.148927436999945,15.2,10.4157307));
#224425=CARTESIAN_POINT('Ctrl Pts',(0.148927436999945,11.6,10.4157307));
#224426=CARTESIAN_POINT('Ctrl Pts',(0.148755626999945,15.2,10.414493263));
#224427=CARTESIAN_POINT('Ctrl Pts',(0.148755626999945,11.6,10.414493263));
#224428=CARTESIAN_POINT('Ctrl Pts',(0.148586208999945,15.2,10.413264284));
#224429=CARTESIAN_POINT('Ctrl Pts',(0.148586208999945,11.6,10.413264284));
#224430=CARTESIAN_POINT('Ctrl Pts',(0.148419171999944,15.2,10.412043789));
#224431=CARTESIAN_POINT('Ctrl Pts',(0.148419171999944,11.6,10.412043789));
#224432=CARTESIAN_POINT('Ctrl Pts',(0.148254501999944,15.2,10.410831802));
#224433=CARTESIAN_POINT('Ctrl Pts',(0.148254501999944,11.6,10.410831802));
#224434=CARTESIAN_POINT('Ctrl Pts',(0.148092186999945,15.2,10.409628349));
#224435=CARTESIAN_POINT('Ctrl Pts',(0.148092186999945,11.6,10.409628349));
#224436=CARTESIAN_POINT('Ctrl Pts',(0.147932212999944,15.2,10.408433454));
#224437=CARTESIAN_POINT('Ctrl Pts',(0.147932212999944,11.6,10.408433454));
#224438=CARTESIAN_POINT('Ctrl Pts',(0.147774568999944,15.2,10.407247143));
#224439=CARTESIAN_POINT('Ctrl Pts',(0.147774568999944,11.6,10.407247143));
#224440=CARTESIAN_POINT('Ctrl Pts',(0.147619239999944,15.2,10.40606944));
#224441=CARTESIAN_POINT('Ctrl Pts',(0.147619239999944,11.6,10.40606944));
#224442=CARTESIAN_POINT('Ctrl Pts',(0.147466212999945,15.2,10.404900372));
#224443=CARTESIAN_POINT('Ctrl Pts',(0.147466212999945,11.6,10.404900372));
#224444=CARTESIAN_POINT('Ctrl Pts',(0.147315476999944,15.2,10.403739964));
#224445=CARTESIAN_POINT('Ctrl Pts',(0.147315476999944,11.6,10.403739964));
#224446=CARTESIAN_POINT('Ctrl Pts',(0.147167015999944,15.2,10.402588242));
#224447=CARTESIAN_POINT('Ctrl Pts',(0.147167015999944,11.6,10.402588242));
#224448=CARTESIAN_POINT('Ctrl Pts',(0.147020819999945,15.2,10.401445231));
#224449=CARTESIAN_POINT('Ctrl Pts',(0.147020819999945,11.6,10.401445231));
#224450=CARTESIAN_POINT('Ctrl Pts',(0.146876870999944,15.2,10.400310958));
#224451=CARTESIAN_POINT('Ctrl Pts',(0.146876870999944,11.6,10.400310958));
#224452=CARTESIAN_POINT('Ctrl Pts',(0.146735159999943,15.2,10.399185447));
#224453=CARTESIAN_POINT('Ctrl Pts',(0.146735159999943,11.6,10.399185447));
#224454=CARTESIAN_POINT('Ctrl Pts',(0.146595670999944,15.2,10.398068726));
#224455=CARTESIAN_POINT('Ctrl Pts',(0.146595670999944,11.6,10.398068726));
#224456=CARTESIAN_POINT('Ctrl Pts',(0.146458390999945,15.2,10.39696082));
#224457=CARTESIAN_POINT('Ctrl Pts',(0.146458390999945,11.6,10.39696082));
#224458=CARTESIAN_POINT('Ctrl Pts',(0.146323305999945,15.2,10.395861757));
#224459=CARTESIAN_POINT('Ctrl Pts',(0.146323305999945,11.6,10.395861757));
#224460=CARTESIAN_POINT('Ctrl Pts',(0.146190402999944,15.2,10.39477156));
#224461=CARTESIAN_POINT('Ctrl Pts',(0.146190402999944,11.6,10.39477156));
#224462=CARTESIAN_POINT('Ctrl Pts',(0.146059667999945,15.2,10.39369026));
#224463=CARTESIAN_POINT('Ctrl Pts',(0.146059667999945,11.6,10.39369026));
#224464=CARTESIAN_POINT('Ctrl Pts',(0.145931086999944,15.2,10.392617881));
#224465=CARTESIAN_POINT('Ctrl Pts',(0.145931086999944,11.6,10.392617881));
#224466=CARTESIAN_POINT('Ctrl Pts',(0.145804644999944,15.2,10.391554451));
#224467=CARTESIAN_POINT('Ctrl Pts',(0.145804644999944,11.6,10.391554451));
#224468=CARTESIAN_POINT('Ctrl Pts',(0.145680329999944,15.2,10.390499995));
#224469=CARTESIAN_POINT('Ctrl Pts',(0.145680329999944,11.6,10.390499995));
#224470=CARTESIAN_POINT('Ctrl Pts',(0.145558125999944,15.2,10.389454543));
#224471=CARTESIAN_POINT('Ctrl Pts',(0.145558125999944,11.6,10.389454543));
#224472=CARTESIAN_POINT('Ctrl Pts',(0.145438019999944,15.2,10.38841812));
#224473=CARTESIAN_POINT('Ctrl Pts',(0.145438019999944,11.6,10.38841812));
#224474=CARTESIAN_POINT('Ctrl Pts',(0.145319995999945,15.2,10.387390753));
#224475=CARTESIAN_POINT('Ctrl Pts',(0.145319995999945,11.6,10.387390753));
#224476=CARTESIAN_POINT('Ctrl Pts',(0.145204040999944,15.2,10.386372471));
#224477=CARTESIAN_POINT('Ctrl Pts',(0.145204040999944,11.6,10.386372471));
#224478=CARTESIAN_POINT('Ctrl Pts',(0.145090141999944,15.2,10.3853633));
#224479=CARTESIAN_POINT('Ctrl Pts',(0.145090141999944,11.6,10.3853633));
#224480=CARTESIAN_POINT('Ctrl Pts',(0.144978279999943,15.2,10.384363269));
#224481=CARTESIAN_POINT('Ctrl Pts',(0.144978279999943,11.6,10.384363269));
#224482=CARTESIAN_POINT('Ctrl Pts',(0.144868444999944,15.2,10.383372406));
#224483=CARTESIAN_POINT('Ctrl Pts',(0.144868444999944,11.6,10.383372406));
#224484=CARTESIAN_POINT('Ctrl Pts',(0.144760618999945,15.2,10.382390738));
#224485=CARTESIAN_POINT('Ctrl Pts',(0.144760618999945,11.6,10.382390738));
#224486=CARTESIAN_POINT('Ctrl Pts',(0.144654789999944,15.2,10.381418293));
#224487=CARTESIAN_POINT('Ctrl Pts',(0.144654789999944,11.6,10.381418293));
#224488=CARTESIAN_POINT('Ctrl Pts',(0.144550940999943,15.2,10.3804551));
#224489=CARTESIAN_POINT('Ctrl Pts',(0.144550940999943,11.6,10.3804551));
#224490=CARTESIAN_POINT('Ctrl Pts',(0.144449056999945,15.2,10.379501187));
#224491=CARTESIAN_POINT('Ctrl Pts',(0.144449056999945,11.6,10.379501187));
#224492=CARTESIAN_POINT('Ctrl Pts',(0.144349124999945,15.2,10.378556581));
#224493=CARTESIAN_POINT('Ctrl Pts',(0.144349124999945,11.6,10.378556581));
#224494=CARTESIAN_POINT('Ctrl Pts',(0.144251126999944,15.2,10.377621314));
#224495=CARTESIAN_POINT('Ctrl Pts',(0.144251126999944,11.6,10.377621314));
#224496=CARTESIAN_POINT('Ctrl Pts',(0.144155048999943,15.2,10.376695411));
#224497=CARTESIAN_POINT('Ctrl Pts',(0.144155048999943,11.6,10.376695411));
#224498=CARTESIAN_POINT('Ctrl Pts',(0.144061419999945,15.2,10.375784182));
#224499=CARTESIAN_POINT('Ctrl Pts',(0.144061419999945,11.6,10.375784182));
#224500=CARTESIAN_POINT('Ctrl Pts',(0.143988113999944,15.2,10.375063685));
#224501=CARTESIAN_POINT('Ctrl Pts',(0.143988113999944,11.6,10.375063685));
#224502=CARTESIAN_POINT('Ctrl Pts',(0.143934094999943,15.2,10.374528791));
#224503=CARTESIAN_POINT('Ctrl Pts',(0.143934094999943,11.6,10.374528791));
#224504=CARTESIAN_POINT('Ctrl Pts',(0.143898617999945,15.2,10.374175763));
#224505=CARTESIAN_POINT('Ctrl Pts',(0.143898617999945,11.6,10.374175763));
#224506=CARTESIAN_POINT('Ctrl Pts',(0.143881226999945,15.2,10.374002275));
#224507=CARTESIAN_POINT('Ctrl Pts',(0.143881226999945,11.6,10.374002275));
#224508=CARTESIAN_POINT('',(0.143881226999945,12.2,10.374002275));
#224509=CARTESIAN_POINT('',(0.143881226999945,15.2,10.374002275));
#224510=CARTESIAN_POINT('',(0.143881226999945,12.2,10.374002275));
#224511=CARTESIAN_POINT('Ctrl Pts',(0.546958305999944,12.2,11.486985532));
#224512=CARTESIAN_POINT('Ctrl Pts',(0.546590898999945,12.2,11.486315008));
#224513=CARTESIAN_POINT('Ctrl Pts',(0.545856550999945,12.2,11.484974209));
#224514=CARTESIAN_POINT('Ctrl Pts',(0.544756420999944,12.2,11.482963756));
#224515=CARTESIAN_POINT('Ctrl Pts',(0.543292368999944,12.2,11.480284644));
#224516=CARTESIAN_POINT('Ctrl Pts',(0.541466945999944,12.2,11.476938237));
#224517=CARTESIAN_POINT('Ctrl Pts',(0.539646165999944,12.2,11.473594318));
#224518=CARTESIAN_POINT('Ctrl Pts',(0.537830029999945,12.2,11.470252887));
#224519=CARTESIAN_POINT('Ctrl Pts',(0.536018536999944,12.2,11.466913949));
#224520=CARTESIAN_POINT('Ctrl Pts',(0.534211683999944,12.2,11.46357751));
#224521=CARTESIAN_POINT('Ctrl Pts',(0.532409473999944,12.2,11.460243578));
#224522=CARTESIAN_POINT('Ctrl Pts',(0.530611901999943,12.2,11.456912161));
#224523=CARTESIAN_POINT('Ctrl Pts',(0.528818964999944,12.2,11.453583273));
#224524=CARTESIAN_POINT('Ctrl Pts',(0.527030663999944,12.2,11.450256921));
#224525=CARTESIAN_POINT('Ctrl Pts',(0.525246995999944,12.2,11.446933119));
#224526=CARTESIAN_POINT('Ctrl Pts',(0.523467958999944,12.2,11.443611876));
#224527=CARTESIAN_POINT('Ctrl Pts',(0.521693550999944,12.2,11.440293201));
#224528=CARTESIAN_POINT('Ctrl Pts',(0.519923770999945,12.2,11.436977102));
#224529=CARTESIAN_POINT('Ctrl Pts',(0.518158616999944,12.2,11.43366359));
#224530=CARTESIAN_POINT('Ctrl Pts',(0.516398088999944,12.2,11.43035267));
#224531=CARTESIAN_POINT('Ctrl Pts',(0.514642183999944,12.2,11.427044351));
#224532=CARTESIAN_POINT('Ctrl Pts',(0.512890899999944,12.2,11.423738642));
#224533=CARTESIAN_POINT('Ctrl Pts',(0.511144237999944,12.2,11.420435552));
#224534=CARTESIAN_POINT('Ctrl Pts',(0.509402193999944,12.2,11.417135088));
#224535=CARTESIAN_POINT('Ctrl Pts',(0.507664765999943,12.2,11.413837262));
#224536=CARTESIAN_POINT('Ctrl Pts',(0.505931953999944,12.2,11.410542081));
#224537=CARTESIAN_POINT('Ctrl Pts',(0.504203755999945,12.2,11.407249557));
#224538=CARTESIAN_POINT('Ctrl Pts',(0.502480167999945,12.2,11.403959697));
#224539=CARTESIAN_POINT('Ctrl Pts',(0.500761191999944,12.2,11.400672511));
#224540=CARTESIAN_POINT('Ctrl Pts',(0.499046822999943,12.2,11.397388008));
#224541=CARTESIAN_POINT('Ctrl Pts',(0.497337059999945,12.2,11.394106196));
#224542=CARTESIAN_POINT('Ctrl Pts',(0.495631902999945,12.2,11.390827085));
#224543=CARTESIAN_POINT('Ctrl Pts',(0.493931348999944,12.2,11.387550685));
#224544=CARTESIAN_POINT('Ctrl Pts',(0.492235395999945,12.2,11.384277002));
#224545=CARTESIAN_POINT('Ctrl Pts',(0.490544042999945,12.2,11.381006048));
#224546=CARTESIAN_POINT('Ctrl Pts',(0.488857286999943,12.2,11.37773783));
#224547=CARTESIAN_POINT('Ctrl Pts',(0.487175127999944,12.2,11.374472358));
#224548=CARTESIAN_POINT('Ctrl Pts',(0.485497562999945,12.2,11.371209642));
#224549=CARTESIAN_POINT('Ctrl Pts',(0.483824590999945,12.2,11.36794969));
#224550=CARTESIAN_POINT('Ctrl Pts',(0.482156208999944,12.2,11.364692512));
#224551=CARTESIAN_POINT('Ctrl Pts',(0.480492415999944,12.2,11.361438117));
#224552=CARTESIAN_POINT('Ctrl Pts',(0.478833209999945,12.2,11.358186515));
#224553=CARTESIAN_POINT('Ctrl Pts',(0.477178588999945,12.2,11.354937714));
#224554=CARTESIAN_POINT('Ctrl Pts',(0.475528549999943,12.2,11.351691724));
#224555=CARTESIAN_POINT('Ctrl Pts',(0.473883093999945,12.2,11.348448553));
#224556=CARTESIAN_POINT('Ctrl Pts',(0.472242216999945,12.2,11.345208212));
#224557=CARTESIAN_POINT('Ctrl Pts',(0.470605917999943,12.2,11.34197071));
#224558=CARTESIAN_POINT('Ctrl Pts',(0.468974193999945,12.2,11.338736055));
#224559=CARTESIAN_POINT('Ctrl Pts',(0.467347043999944,12.2,11.335504256));
#224560=CARTESIAN_POINT('Ctrl Pts',(0.465724464999945,12.2,11.332275324));
#224561=CARTESIAN_POINT('Ctrl Pts',(0.464106456999945,12.2,11.329049269));
#224562=CARTESIAN_POINT('Ctrl Pts',(0.462493016999945,12.2,11.325826099));
#224563=CARTESIAN_POINT('Ctrl Pts',(0.460884141999944,12.2,11.322605823));
#224564=CARTESIAN_POINT('Ctrl Pts',(0.459279831999944,12.2,11.319388451));
#224565=CARTESIAN_POINT('Ctrl Pts',(0.457680083999945,12.2,11.316173992));
#224566=CARTESIAN_POINT('Ctrl Pts',(0.456084895999943,12.2,11.312962457));
#224567=CARTESIAN_POINT('Ctrl Pts',(0.454494264999944,12.2,11.309753854));
#224568=CARTESIAN_POINT('Ctrl Pts',(0.452908190999944,12.2,11.306548191));
#224569=CARTESIAN_POINT('Ctrl Pts',(0.451326669999944,12.2,11.303345481));
#224570=CARTESIAN_POINT('Ctrl Pts',(0.449749701999943,12.2,11.300145732));
#224571=CARTESIAN_POINT('Ctrl Pts',(0.448177283999945,12.2,11.296948952));
#224572=CARTESIAN_POINT('Ctrl Pts',(0.446609412999944,12.2,11.293755151));
#224573=CARTESIAN_POINT('Ctrl Pts',(0.445046087999945,12.2,11.290564341));
#224574=CARTESIAN_POINT('Ctrl Pts',(0.443487306999945,12.2,11.287376529));
#224575=CARTESIAN_POINT('Ctrl Pts',(0.441933066999944,12.2,11.284191726));
#224576=CARTESIAN_POINT('Ctrl Pts',(0.440383366999945,12.2,11.28100994));
#224577=CARTESIAN_POINT('Ctrl Pts',(0.438838203999945,12.2,11.277831182));
#224578=CARTESIAN_POINT('Ctrl Pts',(0.437297575999944,12.2,11.27465546));
#224579=CARTESIAN_POINT('Ctrl Pts',(0.435761481999943,12.2,11.271482787));
#224580=CARTESIAN_POINT('Ctrl Pts',(0.434229916999945,12.2,11.268313168));
#224581=CARTESIAN_POINT('Ctrl Pts',(0.432397475066523,12.2,11.2645133069381));
#224582=CARTESIAN_POINT('Ctrl Pts',(0.430571823466653,12.2,11.260718059531));
#224583=CARTESIAN_POINT('Ctrl Pts',(0.428752956533235,12.2,11.256927442469));
#224584=CARTESIAN_POINT('Ctrl Pts',(0.426940870933362,12.2,11.2531414800619));
#224585=CARTESIAN_POINT('Ctrl Pts',(0.425135560999944,12.2,11.249360189));
#224586=CARTESIAN_POINT('Ctrl Pts',(0.423635651999945,12.2,11.246212238));
#224587=CARTESIAN_POINT('Ctrl Pts',(0.422140256999944,12.2,11.24306742));
#224588=CARTESIAN_POINT('Ctrl Pts',(0.420649371999945,12.2,11.239925747));
#224589=CARTESIAN_POINT('Ctrl Pts',(0.419162995999944,12.2,11.236787228));
#224590=CARTESIAN_POINT('Ctrl Pts',(0.417681126999945,12.2,11.233651872));
#224591=CARTESIAN_POINT('Ctrl Pts',(0.416203760999944,12.2,11.230519689));
#224592=CARTESIAN_POINT('Ctrl Pts',(0.414730897999943,12.2,11.227390689));
#224593=CARTESIAN_POINT('Ctrl Pts',(0.413262533999944,12.2,11.224264884));
#224594=CARTESIAN_POINT('Ctrl Pts',(0.411798665999944,12.2,11.22114228));
#224595=CARTESIAN_POINT('Ctrl Pts',(0.410339294999943,12.2,11.21802289));
#224596=CARTESIAN_POINT('Ctrl Pts',(0.408884414999945,12.2,11.214906723));
#224597=CARTESIAN_POINT('Ctrl Pts',(0.407434024999944,12.2,11.211793789));
#224598=CARTESIAN_POINT('Ctrl Pts',(0.405988121999944,12.2,11.208684097));
#224599=CARTESIAN_POINT('Ctrl Pts',(0.404546704999945,12.2,11.205577658));
#224600=CARTESIAN_POINT('Ctrl Pts',(0.403109770999944,12.2,11.202474482));
#224601=CARTESIAN_POINT('Ctrl Pts',(0.401677316999944,12.2,11.199374578));
#224602=CARTESIAN_POINT('Ctrl Pts',(0.400249340999944,12.2,11.196277957));
#224603=CARTESIAN_POINT('Ctrl Pts',(0.398825840999945,12.2,11.193184629));
#224604=CARTESIAN_POINT('Ctrl Pts',(0.397406813999943,12.2,11.190094604));
#224605=CARTESIAN_POINT('Ctrl Pts',(0.395992257999945,12.2,11.187007891));
#224606=CARTESIAN_POINT('Ctrl Pts',(0.394582168999945,12.2,11.183924503));
#224607=CARTESIAN_POINT('Ctrl Pts',(0.393176546999945,12.2,11.180844446));
#224608=CARTESIAN_POINT('Ctrl Pts',(0.391775385999944,12.2,11.177767734));
#224609=CARTESIAN_POINT('Ctrl Pts',(0.390378687999944,12.2,11.174694374));
#224610=CARTESIAN_POINT('Ctrl Pts',(0.388986445999944,12.2,11.171624378));
#224611=CARTESIAN_POINT('Ctrl Pts',(0.387598660999944,12.2,11.168557757));
#224612=CARTESIAN_POINT('Ctrl Pts',(0.386215327999944,12.2,11.165494518));
#224613=CARTESIAN_POINT('Ctrl Pts',(0.384836444999944,12.2,11.162434674));
#224614=CARTESIAN_POINT('Ctrl Pts',(0.383462009999944,12.2,11.159378235));
#224615=CARTESIAN_POINT('Ctrl Pts',(0.382092020999943,12.2,11.15632521));
#224616=CARTESIAN_POINT('Ctrl Pts',(0.380726473999945,12.2,11.15327561));
#224617=CARTESIAN_POINT('Ctrl Pts',(0.379365366999943,12.2,11.150229446));
#224618=CARTESIAN_POINT('Ctrl Pts',(0.378008696999944,12.2,11.147186727));
#224619=CARTESIAN_POINT('Ctrl Pts',(0.376656460999945,12.2,11.144147463));
#224620=CARTESIAN_POINT('Ctrl Pts',(0.375308657999945,12.2,11.141111667));
#224621=CARTESIAN_POINT('Ctrl Pts',(0.373965283999944,12.2,11.138079346));
#224622=CARTESIAN_POINT('Ctrl Pts',(0.372626335999945,12.2,11.135050513));
#224623=CARTESIAN_POINT('Ctrl Pts',(0.371291811999944,12.2,11.132025177));
#224624=CARTESIAN_POINT('Ctrl Pts',(0.369961708999943,12.2,11.129003348));
#224625=CARTESIAN_POINT('Ctrl Pts',(0.368636023999944,12.2,11.125985039));
#224626=CARTESIAN_POINT('Ctrl Pts',(0.367314755999945,12.2,11.122970257));
#224627=CARTESIAN_POINT('Ctrl Pts',(0.365997898999944,12.2,11.119959015));
#224628=CARTESIAN_POINT('Ctrl Pts',(0.364685451999945,12.2,11.116951322));
#224629=CARTESIAN_POINT('Ctrl Pts',(0.363377412999943,12.2,11.11394719));
#224630=CARTESIAN_POINT('Ctrl Pts',(0.362073778999944,12.2,11.110946629));
#224631=CARTESIAN_POINT('Ctrl Pts',(0.360774545999943,12.2,11.107949648));
#224632=CARTESIAN_POINT('Ctrl Pts',(0.359479711999944,12.2,11.104956259));
#224633=CARTESIAN_POINT('Ctrl Pts',(0.358189272999944,12.2,11.101966473));
#224634=CARTESIAN_POINT('Ctrl Pts',(0.356903226999944,12.2,11.0989803));
#224635=CARTESIAN_POINT('Ctrl Pts',(0.355621571999943,12.2,11.095997751));
#224636=CARTESIAN_POINT('Ctrl Pts',(0.354344304999945,12.2,11.093018835));
#224637=CARTESIAN_POINT('Ctrl Pts',(0.353071419999944,12.2,11.090043565));
#224638=CARTESIAN_POINT('Ctrl Pts',(0.351802917999944,12.2,11.087071951));
#224639=CARTESIAN_POINT('Ctrl Pts',(0.350538794999944,12.2,11.084104002));
#224640=CARTESIAN_POINT('Ctrl Pts',(0.349279045999945,12.2,11.081139731));
#224641=CARTESIAN_POINT('Ctrl Pts',(0.348023670999943,12.2,11.078179147));
#224642=CARTESIAN_POINT('Ctrl Pts',(0.346772663999945,12.2,11.075222263));
#224643=CARTESIAN_POINT('Ctrl Pts',(0.345526024999945,12.2,11.072269087));
#224644=CARTESIAN_POINT('Ctrl Pts',(0.344283748999944,12.2,11.069319631));
#224645=CARTESIAN_POINT('Ctrl Pts',(0.343045832999945,12.2,11.066373907));
#224646=CARTESIAN_POINT('Ctrl Pts',(0.341812274999944,12.2,11.063431924));
#224647=CARTESIAN_POINT('Ctrl Pts',(0.340583071999945,12.2,11.060493695));
#224648=CARTESIAN_POINT('Ctrl Pts',(0.339358218999944,12.2,11.057559229));
#224649=CARTESIAN_POINT('Ctrl Pts',(0.338137715999943,12.2,11.054628538));
#224650=CARTESIAN_POINT('Ctrl Pts',(0.336921556999944,12.2,11.051701632));
#224651=CARTESIAN_POINT('Ctrl Pts',(0.335709739999944,12.2,11.048778522));
#224652=CARTESIAN_POINT('Ctrl Pts',(0.334502261999944,12.2,11.04585922));
#224653=CARTESIAN_POINT('Ctrl Pts',(0.333299119999945,12.2,11.042943736));
#224654=CARTESIAN_POINT('Ctrl Pts',(0.332100310999944,12.2,11.040032081));
#224655=CARTESIAN_POINT('Ctrl Pts',(0.330905830999945,12.2,11.037124267));
#224656=CARTESIAN_POINT('Ctrl Pts',(0.329715676999944,12.2,11.034220304));
#224657=CARTESIAN_POINT('Ctrl Pts',(0.328529845999944,12.2,11.031320203));
#224658=CARTESIAN_POINT('Ctrl Pts',(0.327348334999943,12.2,11.028423977));
#224659=CARTESIAN_POINT('Ctrl Pts',(0.326171140999945,12.2,11.025531635));
#224660=CARTESIAN_POINT('Ctrl Pts',(0.324998259999945,12.2,11.02264319));
#224661=CARTESIAN_POINT('Ctrl Pts',(0.323829688999944,12.2,11.01975865));
#224662=CARTESIAN_POINT('Ctrl Pts',(0.322665423999944,12.2,11.016878029));
#224663=CARTESIAN_POINT('Ctrl Pts',(0.321505462999945,12.2,11.014001339));
#224664=CARTESIAN_POINT('Ctrl Pts',(0.320349802999944,12.2,11.011128587));
#224665=CARTESIAN_POINT('Ctrl Pts',(0.319198438999945,12.2,11.008259789));
#224666=CARTESIAN_POINT('Ctrl Pts',(0.318051368999944,12.2,11.005394953));
#224667=CARTESIAN_POINT('Ctrl Pts',(0.316908587999943,12.2,11.002534092));
#224668=CARTESIAN_POINT('Ctrl Pts',(0.315770094999944,12.2,10.999677217));
#224669=CARTESIAN_POINT('Ctrl Pts',(0.314635883999944,12.2,10.996824338));
#224670=CARTESIAN_POINT('Ctrl Pts',(0.313505953999943,12.2,10.993975469));
#224671=CARTESIAN_POINT('Ctrl Pts',(0.312380299999945,12.2,10.991130619));
#224672=CARTESIAN_POINT('Ctrl Pts',(0.311258918999944,12.2,10.988289801));
#224673=CARTESIAN_POINT('Ctrl Pts',(0.310141807999944,12.2,10.985453024));
#224674=CARTESIAN_POINT('Ctrl Pts',(0.309028961999944,12.2,10.982620303));
#224675=CARTESIAN_POINT('Ctrl Pts',(0.307920378999944,12.2,10.979791646));
#224676=CARTESIAN_POINT('Ctrl Pts',(0.306816055999944,12.2,10.976967067));
#224677=CARTESIAN_POINT('Ctrl Pts',(0.305715986999945,12.2,10.974146576));
#224678=CARTESIAN_POINT('Ctrl Pts',(0.304620169999945,12.2,10.971330186));
#224679=CARTESIAN_POINT('Ctrl Pts',(0.303528602999944,12.2,10.968517908));
#224680=CARTESIAN_POINT('Ctrl Pts',(0.302441278999943,12.2,10.965709751));
#224681=CARTESIAN_POINT('Ctrl Pts',(0.301358196999945,12.2,10.962905732));
#224682=CARTESIAN_POINT('Ctrl Pts',(0.300279352999944,12.2,10.960105857));
#224683=CARTESIAN_POINT('Ctrl Pts',(0.299204742999944,12.2,10.957310141));
#224684=CARTESIAN_POINT('Ctrl Pts',(0.298134362999944,12.2,10.954518595));
#224685=CARTESIAN_POINT('Ctrl Pts',(0.297068208999944,12.2,10.951731231));
#224686=CARTESIAN_POINT('Ctrl Pts',(0.296006278999944,12.2,10.94894806));
#224687=CARTESIAN_POINT('Ctrl Pts',(0.294948567999944,12.2,10.946169093));
#224688=CARTESIAN_POINT('Ctrl Pts',(0.293895072999945,12.2,10.943394344));
#224689=CARTESIAN_POINT('Ctrl Pts',(0.292845787999945,12.2,10.940623824));
#224690=CARTESIAN_POINT('Ctrl Pts',(0.291800711999944,12.2,10.937857544));
#224691=CARTESIAN_POINT('Ctrl Pts',(0.290759841999944,12.2,10.935095515));
#224692=CARTESIAN_POINT('Ctrl Pts',(0.289723169999944,12.2,10.932337751));
#224693=CARTESIAN_POINT('Ctrl Pts',(0.288690695999945,12.2,10.929584263));
#224694=CARTESIAN_POINT('Ctrl Pts',(0.287662414999945,12.2,10.926835064));
#224695=CARTESIAN_POINT('Ctrl Pts',(0.286638321999944,12.2,10.924090164));
#224696=CARTESIAN_POINT('Ctrl Pts',(0.285618414999943,12.2,10.921349576));
#224697=CARTESIAN_POINT('Ctrl Pts',(0.284602689999945,12.2,10.918613312));
#224698=CARTESIAN_POINT('Ctrl Pts',(0.283591139999944,12.2,10.915881383));
#224699=CARTESIAN_POINT('Ctrl Pts',(0.282583764999943,12.2,10.913153803));
#224700=CARTESIAN_POINT('Ctrl Pts',(0.281580559999943,12.2,10.910430582));
#224701=CARTESIAN_POINT('Ctrl Pts',(0.280581519999944,12.2,10.907711735));
#224702=CARTESIAN_POINT('Ctrl Pts',(0.279586641999944,12.2,10.904997271));
#224703=CARTESIAN_POINT('Ctrl Pts',(0.278595920999944,12.2,10.902287203));
#224704=CARTESIAN_POINT('Ctrl Pts',(0.277609353999945,12.2,10.899581544));
#224705=CARTESIAN_POINT('Ctrl Pts',(0.276626936999945,12.2,10.896880306));
#224706=CARTESIAN_POINT('Ctrl Pts',(0.275648663999943,12.2,10.894183501));
#224707=CARTESIAN_POINT('Ctrl Pts',(0.274674533999945,12.2,10.89149114));
#224708=CARTESIAN_POINT('Ctrl Pts',(0.273704539999944,12.2,10.888803238));
#224709=CARTESIAN_POINT('Ctrl Pts',(0.272738680999945,12.2,10.886119805));
#224710=CARTESIAN_POINT('Ctrl Pts',(0.271776950999945,12.2,10.883440855));
#224711=CARTESIAN_POINT('Ctrl Pts',(0.270819344999945,12.2,10.880766399));
#224712=CARTESIAN_POINT('Ctrl Pts',(0.269865859999945,12.2,10.878096449));
#224713=CARTESIAN_POINT('Ctrl Pts',(0.268916491999944,12.2,10.875431019));
#224714=CARTESIAN_POINT('Ctrl Pts',(0.267971236999944,12.2,10.872770121));
#224715=CARTESIAN_POINT('Ctrl Pts',(0.267030088999943,12.2,10.870113767));
#224716=CARTESIAN_POINT('Ctrl Pts',(0.266093045999943,12.2,10.867461969));
#224717=CARTESIAN_POINT('Ctrl Pts',(0.265160102999945,12.2,10.864814741));
#224718=CARTESIAN_POINT('Ctrl Pts',(0.264231254999944,12.2,10.862172095));
#224719=CARTESIAN_POINT('Ctrl Pts',(0.263306497999943,12.2,10.859534043));
#224720=CARTESIAN_POINT('Ctrl Pts',(0.262385827999945,12.2,10.856900597));
#224721=CARTESIAN_POINT('Ctrl Pts',(0.261469239999944,12.2,10.854271772));
#224722=CARTESIAN_POINT('Ctrl Pts',(0.260556730999945,12.2,10.851647579));
#224723=CARTESIAN_POINT('Ctrl Pts',(0.259648296999944,12.2,10.84902803));
#224724=CARTESIAN_POINT('Ctrl Pts',(0.258743930999945,12.2,10.846413139));
#224725=CARTESIAN_POINT('Ctrl Pts',(0.257843629999943,12.2,10.843802919));
#224726=CARTESIAN_POINT('Ctrl Pts',(0.256947389999944,12.2,10.841197381));
#224727=CARTESIAN_POINT('Ctrl Pts',(0.256055205999944,12.2,10.838596539));
#224728=CARTESIAN_POINT('Ctrl Pts',(0.255167071999944,12.2,10.836000406));
#224729=CARTESIAN_POINT('Ctrl Pts',(0.254282986999945,12.2,10.833408995));
#224730=CARTESIAN_POINT('Ctrl Pts',(0.253402944999944,12.2,10.830822318));
#224731=CARTESIAN_POINT('Ctrl Pts',(0.252526938999944,12.2,10.828240388));
#224732=CARTESIAN_POINT('Ctrl Pts',(0.251654968999944,12.2,10.825663219));
#224733=CARTESIAN_POINT('Ctrl Pts',(0.250787026999945,12.2,10.823090823));
#224734=CARTESIAN_POINT('Ctrl Pts',(0.249923107999944,12.2,10.820523213));
#224735=CARTESIAN_POINT('Ctrl Pts',(0.249063209999945,12.2,10.817960403));
#224736=CARTESIAN_POINT('Ctrl Pts',(0.248207326999944,12.2,10.815402405));
#224737=CARTESIAN_POINT('Ctrl Pts',(0.247355453999945,12.2,10.812849232));
#224738=CARTESIAN_POINT('Ctrl Pts',(0.246507586999943,12.2,10.810300898));
#224739=CARTESIAN_POINT('Ctrl Pts',(0.245663720999945,12.2,10.807757416));
#224740=CARTESIAN_POINT('Ctrl Pts',(0.244823849999944,12.2,10.805218799));
#224741=CARTESIAN_POINT('Ctrl Pts',(0.243987971999945,12.2,10.80268506));
#224742=CARTESIAN_POINT('Ctrl Pts',(0.243156079999943,12.2,10.800156212));
#224743=CARTESIAN_POINT('Ctrl Pts',(0.242328170999944,12.2,10.797632269));
#224744=CARTESIAN_POINT('Ctrl Pts',(0.241504236999944,12.2,10.795113244));
#224745=CARTESIAN_POINT('Ctrl Pts',(0.240684276999945,12.2,10.79259915));
#224746=CARTESIAN_POINT('Ctrl Pts',(0.239868283999943,12.2,10.790090001));
#224747=CARTESIAN_POINT('Ctrl Pts',(0.239056252999944,12.2,10.78758581));
#224748=CARTESIAN_POINT('Ctrl Pts',(0.238248179999945,12.2,10.78508659));
#224749=CARTESIAN_POINT('Ctrl Pts',(0.237444059999945,12.2,10.782592356));
#224750=CARTESIAN_POINT('Ctrl Pts',(0.236643886999944,12.2,10.780103119));
#224751=CARTESIAN_POINT('Ctrl Pts',(0.235847656999945,12.2,10.777618895));
#224752=CARTESIAN_POINT('Ctrl Pts',(0.235055364999944,12.2,10.775139696));
#224753=CARTESIAN_POINT('Ctrl Pts',(0.234267004999945,12.2,10.772665536));
#224754=CARTESIAN_POINT('Ctrl Pts',(0.233482572999945,12.2,10.770196429));
#224755=CARTESIAN_POINT('Ctrl Pts',(0.232702063999944,12.2,10.767732388));
#224756=CARTESIAN_POINT('Ctrl Pts',(0.231925471999944,12.2,10.765273427));
#224757=CARTESIAN_POINT('Ctrl Pts',(0.231152791999945,12.2,10.762819561));
#224758=CARTESIAN_POINT('Ctrl Pts',(0.230384019999944,12.2,10.760370801));
#224759=CARTESIAN_POINT('Ctrl Pts',(0.229619148999944,12.2,10.757927164));
#224760=CARTESIAN_POINT('Ctrl Pts',(0.228858174999944,12.2,10.755488661));
#224761=CARTESIAN_POINT('Ctrl Pts',(0.228101093999945,12.2,10.753055306));
#224762=CARTESIAN_POINT('Ctrl Pts',(0.227347897999944,12.2,10.750627115));
#224763=CARTESIAN_POINT('Ctrl Pts',(0.226598583999945,12.2,10.748204101));
#224764=CARTESIAN_POINT('Ctrl Pts',(0.225853144999943,12.2,10.745786278));
#224765=CARTESIAN_POINT('Ctrl Pts',(0.225111577999944,12.2,10.743373659));
#224766=CARTESIAN_POINT('Ctrl Pts',(0.224373874999945,12.2,10.740966259));
#224767=CARTESIAN_POINT('Ctrl Pts',(0.223640032999944,12.2,10.738564091));
#224768=CARTESIAN_POINT('Ctrl Pts',(0.222910043999944,12.2,10.736167171));
#224769=CARTESIAN_POINT('Ctrl Pts',(0.222183904999945,12.2,10.733775512));
#224770=CARTESIAN_POINT('Ctrl Pts',(0.221461608999943,12.2,10.731389127));
#224771=CARTESIAN_POINT('Ctrl Pts',(0.220743151999944,12.2,10.729008033));
#224772=CARTESIAN_POINT('Ctrl Pts',(0.220028526999944,12.2,10.726632242));
#224773=CARTESIAN_POINT('Ctrl Pts',(0.219317728999944,12.2,10.724261769));
#224774=CARTESIAN_POINT('Ctrl Pts',(0.218610752999944,12.2,10.721896627));
#224775=CARTESIAN_POINT('Ctrl Pts',(0.217907592999945,12.2,10.719536832));
#224776=CARTESIAN_POINT('Ctrl Pts',(0.217208243999943,12.2,10.717182399));
#224777=CARTESIAN_POINT('Ctrl Pts',(0.216512699999944,12.2,10.71483334));
#224778=CARTESIAN_POINT('Ctrl Pts',(0.215820953999944,12.2,10.712489672));
#224779=CARTESIAN_POINT('Ctrl Pts',(0.215133002999943,12.2,10.710151408));
#224780=CARTESIAN_POINT('Ctrl Pts',(0.214448838999944,12.2,10.707818563));
#224781=CARTESIAN_POINT('Ctrl Pts',(0.213768457999944,12.2,10.70549115));
#224782=CARTESIAN_POINT('Ctrl Pts',(0.213091851999945,12.2,10.703169186));
#224783=CARTESIAN_POINT('Ctrl Pts',(0.212419017999944,12.2,10.700852684));
#224784=CARTESIAN_POINT('Ctrl Pts',(0.211749947999945,12.2,10.69854166));
#224785=CARTESIAN_POINT('Ctrl Pts',(0.211084637999944,12.2,10.696236128));
#224786=CARTESIAN_POINT('Ctrl Pts',(0.210423080999943,12.2,10.693936102));
#224787=CARTESIAN_POINT('Ctrl Pts',(0.209765270999943,12.2,10.691641598));
#224788=CARTESIAN_POINT('Ctrl Pts',(0.209111202999944,12.2,10.68935263));
#224789=CARTESIAN_POINT('Ctrl Pts',(0.208460869999945,12.2,10.687069213));
#224790=CARTESIAN_POINT('Ctrl Pts',(0.207814266999945,12.2,10.684791362));
#224791=CARTESIAN_POINT('Ctrl Pts',(0.207171385999944,12.2,10.682519093));
#224792=CARTESIAN_POINT('Ctrl Pts',(0.206532223999943,12.2,10.680252419));
#224793=CARTESIAN_POINT('Ctrl Pts',(0.205896773999944,12.2,10.677991356));
#224794=CARTESIAN_POINT('Ctrl Pts',(0.205265027999945,12.2,10.67573592));
#224795=CARTESIAN_POINT('Ctrl Pts',(0.204636982999944,12.2,10.673486125));
#224796=CARTESIAN_POINT('Ctrl Pts',(0.204012629999945,12.2,10.671241985));
#224797=CARTESIAN_POINT('Ctrl Pts',(0.203391963999945,12.2,10.669003518));
#224798=CARTESIAN_POINT('Ctrl Pts',(0.202774978999944,12.2,10.666770738));
#224799=CARTESIAN_POINT('Ctrl Pts',(0.202161669999944,12.2,10.664543659));
#224800=CARTESIAN_POINT('Ctrl Pts',(0.201552027999944,12.2,10.662322298));
#224801=CARTESIAN_POINT('Ctrl Pts',(0.200946048999944,12.2,10.660106669));
#224802=CARTESIAN_POINT('Ctrl Pts',(0.200343724999945,12.2,10.657896788));
#224803=CARTESIAN_POINT('Ctrl Pts',(0.199745050999944,12.2,10.655692671));
#224804=CARTESIAN_POINT('Ctrl Pts',(0.199150019999944,12.2,10.653494334));
#224805=CARTESIAN_POINT('Ctrl Pts',(0.198558625999944,12.2,10.651301789));
#224806=CARTESIAN_POINT('Ctrl Pts',(0.197970861999943,12.2,10.649115056));
#224807=CARTESIAN_POINT('Ctrl Pts',(0.197386722999945,12.2,10.646934148));
#224808=CARTESIAN_POINT('Ctrl Pts',(0.196806200999945,12.2,10.644759081));
#224809=CARTESIAN_POINT('Ctrl Pts',(0.196229288999945,12.2,10.642589871));
#224810=CARTESIAN_POINT('Ctrl Pts',(0.195655981999945,12.2,10.640426535));
#224811=CARTESIAN_POINT('Ctrl Pts',(0.195086272999945,12.2,10.638269086));
#224812=CARTESIAN_POINT('Ctrl Pts',(0.194520154999944,12.2,10.636117541));
#224813=CARTESIAN_POINT('Ctrl Pts',(0.193957621999944,12.2,10.633971917));
#224814=CARTESIAN_POINT('Ctrl Pts',(0.193398666999943,12.2,10.631832228));
#224815=CARTESIAN_POINT('Ctrl Pts',(0.192843282999944,12.2,10.629698493));
#224816=CARTESIAN_POINT('Ctrl Pts',(0.192291463999944,12.2,10.627570724));
#224817=CARTESIAN_POINT('Ctrl Pts',(0.191743202999944,12.2,10.62544894));
#224818=CARTESIAN_POINT('Ctrl Pts',(0.191198490999945,12.2,10.623333156));
#224819=CARTESIAN_POINT('Ctrl Pts',(0.190657324999943,12.2,10.621223388));
#224820=CARTESIAN_POINT('Ctrl Pts',(0.190119695999943,12.2,10.619119652));
#224821=CARTESIAN_POINT('Ctrl Pts',(0.189585597999944,12.2,10.617021966));
#224822=CARTESIAN_POINT('Ctrl Pts',(0.189055023999943,12.2,10.614930343));
#224823=CARTESIAN_POINT('Ctrl Pts',(0.188527964999944,12.2,10.612844803));
#224824=CARTESIAN_POINT('Ctrl Pts',(0.188004415999944,12.2,10.61076536));
#224825=CARTESIAN_POINT('Ctrl Pts',(0.187484369999943,12.2,10.608692031));
#224826=CARTESIAN_POINT('Ctrl Pts',(0.186967819999945,12.2,10.606624832));
#224827=CARTESIAN_POINT('Ctrl Pts',(0.186454757999943,12.2,10.604563781));
#224828=CARTESIAN_POINT('Ctrl Pts',(0.185945176999944,12.2,10.602508892));
#224829=CARTESIAN_POINT('Ctrl Pts',(0.185439070999944,12.2,10.600460184));
#224830=CARTESIAN_POINT('Ctrl Pts',(0.184936431999944,12.2,10.598417673));
#224831=CARTESIAN_POINT('Ctrl Pts',(0.184437252999944,12.2,10.596381375));
#224832=CARTESIAN_POINT('Ctrl Pts',(0.183941525999943,12.2,10.594351307));
#224833=CARTESIAN_POINT('Ctrl Pts',(0.183449243999944,12.2,10.592327487));
#224834=CARTESIAN_POINT('Ctrl Pts',(0.182960400999944,12.2,10.59030993));
#224835=CARTESIAN_POINT('Ctrl Pts',(0.182474987999944,12.2,10.588298654));
#224836=CARTESIAN_POINT('Ctrl Pts',(0.181992997999944,12.2,10.586293676));
#224837=CARTESIAN_POINT('Ctrl Pts',(0.181514424999945,12.2,10.584295013));
#224838=CARTESIAN_POINT('Ctrl Pts',(0.181039259999943,12.2,10.582302681));
#224839=CARTESIAN_POINT('Ctrl Pts',(0.180567494999944,12.2,10.580316698));
#224840=CARTESIAN_POINT('Ctrl Pts',(0.180099123999945,12.2,10.578337082));
#224841=CARTESIAN_POINT('Ctrl Pts',(0.179634138999945,12.2,10.576363848));
#224842=CARTESIAN_POINT('Ctrl Pts',(0.179172531999944,12.2,10.574397014));
#224843=CARTESIAN_POINT('Ctrl Pts',(0.178714295999944,12.2,10.5724366));
#224844=CARTESIAN_POINT('Ctrl Pts',(0.178259421999943,12.2,10.570482619));
#224845=CARTESIAN_POINT('Ctrl Pts',(0.177807903999945,12.2,10.568535092));
#224846=CARTESIAN_POINT('Ctrl Pts',(0.177359733999944,12.2,10.566594034));
#224847=CARTESIAN_POINT('Ctrl Pts',(0.176914901999944,12.2,10.564659464));
#224848=CARTESIAN_POINT('Ctrl Pts',(0.176473402999945,12.2,10.5627314));
#224849=CARTESIAN_POINT('Ctrl Pts',(0.176035227999943,12.2,10.560809858));
#224850=CARTESIAN_POINT('Ctrl Pts',(0.175600368999945,12.2,10.558894856));
#224851=CARTESIAN_POINT('Ctrl Pts',(0.175168817999944,12.2,10.556986414));
#224852=CARTESIAN_POINT('Ctrl Pts',(0.174740566999944,12.2,10.555084546));
#224853=CARTESIAN_POINT('Ctrl Pts',(0.174315608999944,12.2,10.553189272));
#224854=CARTESIAN_POINT('Ctrl Pts',(0.173893933999943,12.2,10.551300611));
#224855=CARTESIAN_POINT('Ctrl Pts',(0.173475535999945,12.2,10.549418579));
#224856=CARTESIAN_POINT('Ctrl Pts',(0.173060405999944,12.2,10.547543196));
#224857=CARTESIAN_POINT('Ctrl Pts',(0.172648535999944,12.2,10.545674477));
#224858=CARTESIAN_POINT('Ctrl Pts',(0.172239915999944,12.2,10.543812444));
#224859=CARTESIAN_POINT('Ctrl Pts',(0.171834540999944,12.2,10.541957111));
#224860=CARTESIAN_POINT('Ctrl Pts',(0.171432399999943,12.2,10.5401085));
#224861=CARTESIAN_POINT('Ctrl Pts',(0.171033485999944,12.2,10.538266627));
#224862=CARTESIAN_POINT('Ctrl Pts',(0.170637789999945,12.2,10.536431512));
#224863=CARTESIAN_POINT('Ctrl Pts',(0.170245304999943,12.2,10.534603171));
#224864=CARTESIAN_POINT('Ctrl Pts',(0.169856019999944,12.2,10.532781625));
#224865=CARTESIAN_POINT('Ctrl Pts',(0.169469929999944,12.2,10.530966892));
#224866=CARTESIAN_POINT('Ctrl Pts',(0.169087021999944,12.2,10.52915899));
#224867=CARTESIAN_POINT('Ctrl Pts',(0.168707291999944,12.2,10.527357938));
#224868=CARTESIAN_POINT('Ctrl Pts',(0.168330727999945,12.2,10.525563754));
#224869=CARTESIAN_POINT('Ctrl Pts',(0.167957322999944,12.2,10.523776458));
#224870=CARTESIAN_POINT('Ctrl Pts',(0.167587068999945,12.2,10.521996069));
#224871=CARTESIAN_POINT('Ctrl Pts',(0.167219954999943,12.2,10.520222605));
#224872=CARTESIAN_POINT('Ctrl Pts',(0.166855973999944,12.2,10.518456083));
#224873=CARTESIAN_POINT('Ctrl Pts',(0.166495116999944,12.2,10.516696527));
#224874=CARTESIAN_POINT('Ctrl Pts',(0.166137373999945,12.2,10.514943952));
#224875=CARTESIAN_POINT('Ctrl Pts',(0.165782736999944,12.2,10.513198379));
#224876=CARTESIAN_POINT('Ctrl Pts',(0.165431195999943,12.2,10.511459827));
#224877=CARTESIAN_POINT('Ctrl Pts',(0.165082743999945,12.2,10.509728314));
#224878=CARTESIAN_POINT('Ctrl Pts',(0.164737370999944,12.2,10.508003861));
#224879=CARTESIAN_POINT('Ctrl Pts',(0.164395066999944,12.2,10.506286488));
#224880=CARTESIAN_POINT('Ctrl Pts',(0.164055823999943,12.2,10.504576213));
#224881=CARTESIAN_POINT('Ctrl Pts',(0.163719631999945,12.2,10.502873055));
#224882=CARTESIAN_POINT('Ctrl Pts',(0.163386482999943,12.2,10.501177035));
#224883=CARTESIAN_POINT('Ctrl Pts',(0.163056365999944,12.2,10.499488173));
#224884=CARTESIAN_POINT('Ctrl Pts',(0.162729271999943,12.2,10.497806487));
#224885=CARTESIAN_POINT('Ctrl Pts',(0.162405193999945,12.2,10.496131999));
#224886=CARTESIAN_POINT('Ctrl Pts',(0.162084119999945,12.2,10.494464727));
#224887=CARTESIAN_POINT('Ctrl Pts',(0.161766040999943,12.2,10.492804693));
#224888=CARTESIAN_POINT('Ctrl Pts',(0.161450947999944,12.2,10.491151915));
#224889=CARTESIAN_POINT('Ctrl Pts',(0.161138831999944,12.2,10.489506414));
#224890=CARTESIAN_POINT('Ctrl Pts',(0.160829681999944,12.2,10.487868211));
#224891=CARTESIAN_POINT('Ctrl Pts',(0.160523488999944,12.2,10.486237324));
#224892=CARTESIAN_POINT('Ctrl Pts',(0.160220243999945,12.2,10.484613776));
#224893=CARTESIAN_POINT('Ctrl Pts',(0.159919935999945,12.2,10.482997587));
#224894=CARTESIAN_POINT('Ctrl Pts',(0.159622555999944,12.2,10.481388775));
#224895=CARTESIAN_POINT('Ctrl Pts',(0.159328093999944,12.2,10.479787363));
#224896=CARTESIAN_POINT('Ctrl Pts',(0.159036538999944,12.2,10.478193371));
#224897=CARTESIAN_POINT('Ctrl Pts',(0.158747883999943,12.2,10.476606819));
#224898=CARTESIAN_POINT('Ctrl Pts',(0.158462115999944,12.2,10.475027729));
#224899=CARTESIAN_POINT('Ctrl Pts',(0.158179225999945,12.2,10.473456121));
#224900=CARTESIAN_POINT('Ctrl Pts',(0.157899203999945,12.2,10.471892016));
#224901=CARTESIAN_POINT('Ctrl Pts',(0.157622040999945,12.2,10.470335436));
#224902=CARTESIAN_POINT('Ctrl Pts',(0.157347723999944,12.2,10.4687864));
#224903=CARTESIAN_POINT('Ctrl Pts',(0.157076244999944,12.2,10.467244932));
#224904=CARTESIAN_POINT('Ctrl Pts',(0.156807592999944,12.2,10.46571105));
#224905=CARTESIAN_POINT('Ctrl Pts',(0.156541757999945,12.2,10.464184777));
#224906=CARTESIAN_POINT('Ctrl Pts',(0.156278728999943,12.2,10.462666136));
#224907=CARTESIAN_POINT('Ctrl Pts',(0.156018494999944,12.2,10.461155145));
#224908=CARTESIAN_POINT('Ctrl Pts',(0.155761047999944,12.2,10.459651829));
#224909=CARTESIAN_POINT('Ctrl Pts',(0.155506374999945,12.2,10.458156207));
#224910=CARTESIAN_POINT('Ctrl Pts',(0.155254464999944,12.2,10.456668303));
#224911=CARTESIAN_POINT('Ctrl Pts',(0.155005309999944,12.2,10.455188137));
#224912=CARTESIAN_POINT('Ctrl Pts',(0.154758896999944,12.2,10.45371573));
#224913=CARTESIAN_POINT('Ctrl Pts',(0.154515215999943,12.2,10.452251107));
#224914=CARTESIAN_POINT('Ctrl Pts',(0.154274255999944,12.2,10.450794288));
#224915=CARTESIAN_POINT('Ctrl Pts',(0.154036005999943,12.2,10.449345296));
#224916=CARTESIAN_POINT('Ctrl Pts',(0.153800454999944,12.2,10.447904152));
#224917=CARTESIAN_POINT('Ctrl Pts',(0.153567591999944,12.2,10.44647088));
#224918=CARTESIAN_POINT('Ctrl Pts',(0.153337406999944,12.2,10.445045501));
#224919=CARTESIAN_POINT('Ctrl Pts',(0.153109886999945,12.2,10.443628039));
#224920=CARTESIAN_POINT('Ctrl Pts',(0.152885021999944,12.2,10.442218514));
#224921=CARTESIAN_POINT('Ctrl Pts',(0.152662799999945,12.2,10.440816951));
#224922=CARTESIAN_POINT('Ctrl Pts',(0.152443210999945,12.2,10.439423373));
#224923=CARTESIAN_POINT('Ctrl Pts',(0.152226241999944,12.2,10.4380378));
#224924=CARTESIAN_POINT('Ctrl Pts',(0.152011882999944,12.2,10.436660258));
#224925=CARTESIAN_POINT('Ctrl Pts',(0.151800121999944,12.2,10.435290769));
#224926=CARTESIAN_POINT('Ctrl Pts',(0.151590946999944,12.2,10.433929355));
#224927=CARTESIAN_POINT('Ctrl Pts',(0.151384345999944,12.2,10.432576041));
#224928=CARTESIAN_POINT('Ctrl Pts',(0.151180308999944,12.2,10.431230849));
#224929=CARTESIAN_POINT('Ctrl Pts',(0.150978822999944,12.2,10.429893802));
#224930=CARTESIAN_POINT('Ctrl Pts',(0.150779875999945,12.2,10.428564925));
#224931=CARTESIAN_POINT('Ctrl Pts',(0.150583456999945,12.2,10.427244241));
#224932=CARTESIAN_POINT('Ctrl Pts',(0.150389552999943,12.2,10.425931773));
#224933=CARTESIAN_POINT('Ctrl Pts',(0.150198153999943,12.2,10.424627546));
#224934=CARTESIAN_POINT('Ctrl Pts',(0.150009245999945,12.2,10.423331583));
#224935=CARTESIAN_POINT('Ctrl Pts',(0.149822815999944,12.2,10.422043908));
#224936=CARTESIAN_POINT('Ctrl Pts',(0.149638854999944,12.2,10.420764544));
#224937=CARTESIAN_POINT('Ctrl Pts',(0.149457348999944,12.2,10.419493518));
#224938=CARTESIAN_POINT('Ctrl Pts',(0.149278284999944,12.2,10.418230853));
#224939=CARTESIAN_POINT('Ctrl Pts',(0.149101651999944,12.2,10.416976571));
#224940=CARTESIAN_POINT('Ctrl Pts',(0.148927436999945,12.2,10.4157307));
#224941=CARTESIAN_POINT('Ctrl Pts',(0.148755626999945,12.2,10.414493263));
#224942=CARTESIAN_POINT('Ctrl Pts',(0.148586208999945,12.2,10.413264284));
#224943=CARTESIAN_POINT('Ctrl Pts',(0.148419171999944,12.2,10.412043789));
#224944=CARTESIAN_POINT('Ctrl Pts',(0.148254501999944,12.2,10.410831802));
#224945=CARTESIAN_POINT('Ctrl Pts',(0.148092186999945,12.2,10.409628349));
#224946=CARTESIAN_POINT('Ctrl Pts',(0.147932212999944,12.2,10.408433454));
#224947=CARTESIAN_POINT('Ctrl Pts',(0.147774568999944,12.2,10.407247143));
#224948=CARTESIAN_POINT('Ctrl Pts',(0.147619239999944,12.2,10.40606944));
#224949=CARTESIAN_POINT('Ctrl Pts',(0.147466212999945,12.2,10.404900372));
#224950=CARTESIAN_POINT('Ctrl Pts',(0.147315476999944,12.2,10.403739964));
#224951=CARTESIAN_POINT('Ctrl Pts',(0.147167015999944,12.2,10.402588242));
#224952=CARTESIAN_POINT('Ctrl Pts',(0.147020819999945,12.2,10.401445231));
#224953=CARTESIAN_POINT('Ctrl Pts',(0.146876870999944,12.2,10.400310958));
#224954=CARTESIAN_POINT('Ctrl Pts',(0.146735159999943,12.2,10.399185447));
#224955=CARTESIAN_POINT('Ctrl Pts',(0.146595670999944,12.2,10.398068726));
#224956=CARTESIAN_POINT('Ctrl Pts',(0.146458390999945,12.2,10.39696082));
#224957=CARTESIAN_POINT('Ctrl Pts',(0.146323305999945,12.2,10.395861757));
#224958=CARTESIAN_POINT('Ctrl Pts',(0.146190402999944,12.2,10.39477156));
#224959=CARTESIAN_POINT('Ctrl Pts',(0.146059667999945,12.2,10.39369026));
#224960=CARTESIAN_POINT('Ctrl Pts',(0.145931086999944,12.2,10.392617881));
#224961=CARTESIAN_POINT('Ctrl Pts',(0.145804644999944,12.2,10.391554451));
#224962=CARTESIAN_POINT('Ctrl Pts',(0.145680329999944,12.2,10.390499995));
#224963=CARTESIAN_POINT('Ctrl Pts',(0.145558125999944,12.2,10.389454543));
#224964=CARTESIAN_POINT('Ctrl Pts',(0.145438019999944,12.2,10.38841812));
#224965=CARTESIAN_POINT('Ctrl Pts',(0.145319995999945,12.2,10.387390753));
#224966=CARTESIAN_POINT('Ctrl Pts',(0.145204040999944,12.2,10.386372471));
#224967=CARTESIAN_POINT('Ctrl Pts',(0.145090141999944,12.2,10.3853633));
#224968=CARTESIAN_POINT('Ctrl Pts',(0.144978279999943,12.2,10.384363269));
#224969=CARTESIAN_POINT('Ctrl Pts',(0.144868444999944,12.2,10.383372406));
#224970=CARTESIAN_POINT('Ctrl Pts',(0.144760618999945,12.2,10.382390738));
#224971=CARTESIAN_POINT('Ctrl Pts',(0.144654789999944,12.2,10.381418293));
#224972=CARTESIAN_POINT('Ctrl Pts',(0.144550940999943,12.2,10.3804551));
#224973=CARTESIAN_POINT('Ctrl Pts',(0.144449056999945,12.2,10.379501187));
#224974=CARTESIAN_POINT('Ctrl Pts',(0.144349124999945,12.2,10.378556581));
#224975=CARTESIAN_POINT('Ctrl Pts',(0.144251126999944,12.2,10.377621314));
#224976=CARTESIAN_POINT('Ctrl Pts',(0.144155048999943,12.2,10.376695411));
#224977=CARTESIAN_POINT('Ctrl Pts',(0.144061419999945,12.2,10.375784182));
#224978=CARTESIAN_POINT('Ctrl Pts',(0.143988113999944,12.2,10.375063685));
#224979=CARTESIAN_POINT('Ctrl Pts',(0.143934094999943,12.2,10.374528791));
#224980=CARTESIAN_POINT('Ctrl Pts',(0.143898617999945,12.2,10.374175763));
#224981=CARTESIAN_POINT('Ctrl Pts',(0.143881226999945,12.2,10.374002275));
#224982=CARTESIAN_POINT('Ctrl Pts',(0.143881226999945,15.2,10.374002275));
#224983=CARTESIAN_POINT('Ctrl Pts',(0.143898617999945,15.2,10.374175763));
#224984=CARTESIAN_POINT('Ctrl Pts',(0.143934094999943,15.2,10.374528791));
#224985=CARTESIAN_POINT('Ctrl Pts',(0.143988113999944,15.2,10.375063685));
#224986=CARTESIAN_POINT('Ctrl Pts',(0.144061419999945,15.2,10.375784182));
#224987=CARTESIAN_POINT('Ctrl Pts',(0.144155048999943,15.2,10.376695411));
#224988=CARTESIAN_POINT('Ctrl Pts',(0.144251126999944,15.2,10.377621314));
#224989=CARTESIAN_POINT('Ctrl Pts',(0.144349124999945,15.2,10.378556581));
#224990=CARTESIAN_POINT('Ctrl Pts',(0.144449056999945,15.2,10.379501187));
#224991=CARTESIAN_POINT('Ctrl Pts',(0.144550940999943,15.2,10.3804551));
#224992=CARTESIAN_POINT('Ctrl Pts',(0.144654789999944,15.2,10.381418293));
#224993=CARTESIAN_POINT('Ctrl Pts',(0.144760618999945,15.2,10.382390738));
#224994=CARTESIAN_POINT('Ctrl Pts',(0.144868444999944,15.2,10.383372406));
#224995=CARTESIAN_POINT('Ctrl Pts',(0.144978279999943,15.2,10.384363269));
#224996=CARTESIAN_POINT('Ctrl Pts',(0.145090141999944,15.2,10.3853633));
#224997=CARTESIAN_POINT('Ctrl Pts',(0.145204040999944,15.2,10.386372471));
#224998=CARTESIAN_POINT('Ctrl Pts',(0.145319995999945,15.2,10.387390753));
#224999=CARTESIAN_POINT('Ctrl Pts',(0.145438019999944,15.2,10.38841812));
#225000=CARTESIAN_POINT('Ctrl Pts',(0.145558125999944,15.2,10.389454543));
#225001=CARTESIAN_POINT('Ctrl Pts',(0.145680329999944,15.2,10.390499995));
#225002=CARTESIAN_POINT('Ctrl Pts',(0.145804644999944,15.2,10.391554451));
#225003=CARTESIAN_POINT('Ctrl Pts',(0.145931086999944,15.2,10.392617881));
#225004=CARTESIAN_POINT('Ctrl Pts',(0.146059667999945,15.2,10.39369026));
#225005=CARTESIAN_POINT('Ctrl Pts',(0.146190402999944,15.2,10.39477156));
#225006=CARTESIAN_POINT('Ctrl Pts',(0.146323305999945,15.2,10.395861757));
#225007=CARTESIAN_POINT('Ctrl Pts',(0.146458390999945,15.2,10.39696082));
#225008=CARTESIAN_POINT('Ctrl Pts',(0.146595670999944,15.2,10.398068726));
#225009=CARTESIAN_POINT('Ctrl Pts',(0.146735159999943,15.2,10.399185447));
#225010=CARTESIAN_POINT('Ctrl Pts',(0.146876870999944,15.2,10.400310958));
#225011=CARTESIAN_POINT('Ctrl Pts',(0.147020819999945,15.2,10.401445231));
#225012=CARTESIAN_POINT('Ctrl Pts',(0.147167015999944,15.2,10.402588242));
#225013=CARTESIAN_POINT('Ctrl Pts',(0.147315476999944,15.2,10.403739964));
#225014=CARTESIAN_POINT('Ctrl Pts',(0.147466212999945,15.2,10.404900372));
#225015=CARTESIAN_POINT('Ctrl Pts',(0.147619239999944,15.2,10.40606944));
#225016=CARTESIAN_POINT('Ctrl Pts',(0.147774568999944,15.2,10.407247143));
#225017=CARTESIAN_POINT('Ctrl Pts',(0.147932212999944,15.2,10.408433454));
#225018=CARTESIAN_POINT('Ctrl Pts',(0.148092186999945,15.2,10.409628349));
#225019=CARTESIAN_POINT('Ctrl Pts',(0.148254501999944,15.2,10.410831802));
#225020=CARTESIAN_POINT('Ctrl Pts',(0.148419171999944,15.2,10.412043789));
#225021=CARTESIAN_POINT('Ctrl Pts',(0.148586208999945,15.2,10.413264284));
#225022=CARTESIAN_POINT('Ctrl Pts',(0.148755626999945,15.2,10.414493263));
#225023=CARTESIAN_POINT('Ctrl Pts',(0.148927436999945,15.2,10.4157307));
#225024=CARTESIAN_POINT('Ctrl Pts',(0.149101651999944,15.2,10.416976571));
#225025=CARTESIAN_POINT('Ctrl Pts',(0.149278284999944,15.2,10.418230853));
#225026=CARTESIAN_POINT('Ctrl Pts',(0.149457348999944,15.2,10.419493518));
#225027=CARTESIAN_POINT('Ctrl Pts',(0.149638854999944,15.2,10.420764544));
#225028=CARTESIAN_POINT('Ctrl Pts',(0.149822815999944,15.2,10.422043908));
#225029=CARTESIAN_POINT('Ctrl Pts',(0.150009245999945,15.2,10.423331583));
#225030=CARTESIAN_POINT('Ctrl Pts',(0.150198153999943,15.2,10.424627546));
#225031=CARTESIAN_POINT('Ctrl Pts',(0.150389552999943,15.2,10.425931773));
#225032=CARTESIAN_POINT('Ctrl Pts',(0.150583456999945,15.2,10.427244241));
#225033=CARTESIAN_POINT('Ctrl Pts',(0.150779875999945,15.2,10.428564925));
#225034=CARTESIAN_POINT('Ctrl Pts',(0.150978822999944,15.2,10.429893802));
#225035=CARTESIAN_POINT('Ctrl Pts',(0.151180308999944,15.2,10.431230849));
#225036=CARTESIAN_POINT('Ctrl Pts',(0.151384345999944,15.2,10.432576041));
#225037=CARTESIAN_POINT('Ctrl Pts',(0.151590946999944,15.2,10.433929355));
#225038=CARTESIAN_POINT('Ctrl Pts',(0.151800121999944,15.2,10.435290769));
#225039=CARTESIAN_POINT('Ctrl Pts',(0.152011882999944,15.2,10.436660258));
#225040=CARTESIAN_POINT('Ctrl Pts',(0.152226241999944,15.2,10.4380378));
#225041=CARTESIAN_POINT('Ctrl Pts',(0.152443210999945,15.2,10.439423373));
#225042=CARTESIAN_POINT('Ctrl Pts',(0.152662799999945,15.2,10.440816951));
#225043=CARTESIAN_POINT('Ctrl Pts',(0.152885021999944,15.2,10.442218514));
#225044=CARTESIAN_POINT('Ctrl Pts',(0.153109886999945,15.2,10.443628039));
#225045=CARTESIAN_POINT('Ctrl Pts',(0.153337406999944,15.2,10.445045501));
#225046=CARTESIAN_POINT('Ctrl Pts',(0.153567591999944,15.2,10.44647088));
#225047=CARTESIAN_POINT('Ctrl Pts',(0.153800454999944,15.2,10.447904152));
#225048=CARTESIAN_POINT('Ctrl Pts',(0.154036005999943,15.2,10.449345296));
#225049=CARTESIAN_POINT('Ctrl Pts',(0.154274255999944,15.2,10.450794288));
#225050=CARTESIAN_POINT('Ctrl Pts',(0.154515215999943,15.2,10.452251107));
#225051=CARTESIAN_POINT('Ctrl Pts',(0.154758896999944,15.2,10.45371573));
#225052=CARTESIAN_POINT('Ctrl Pts',(0.155005309999944,15.2,10.455188137));
#225053=CARTESIAN_POINT('Ctrl Pts',(0.155254464999944,15.2,10.456668303));
#225054=CARTESIAN_POINT('Ctrl Pts',(0.155506374999945,15.2,10.458156207));
#225055=CARTESIAN_POINT('Ctrl Pts',(0.155761047999944,15.2,10.459651829));
#225056=CARTESIAN_POINT('Ctrl Pts',(0.156018494999944,15.2,10.461155145));
#225057=CARTESIAN_POINT('Ctrl Pts',(0.156278728999943,15.2,10.462666136));
#225058=CARTESIAN_POINT('Ctrl Pts',(0.156541757999945,15.2,10.464184777));
#225059=CARTESIAN_POINT('Ctrl Pts',(0.156807592999944,15.2,10.46571105));
#225060=CARTESIAN_POINT('Ctrl Pts',(0.157076244999944,15.2,10.467244932));
#225061=CARTESIAN_POINT('Ctrl Pts',(0.157347723999944,15.2,10.4687864));
#225062=CARTESIAN_POINT('Ctrl Pts',(0.157622040999945,15.2,10.470335436));
#225063=CARTESIAN_POINT('Ctrl Pts',(0.157899203999945,15.2,10.471892016));
#225064=CARTESIAN_POINT('Ctrl Pts',(0.158179225999945,15.2,10.473456121));
#225065=CARTESIAN_POINT('Ctrl Pts',(0.158462115999944,15.2,10.475027729));
#225066=CARTESIAN_POINT('Ctrl Pts',(0.158747883999943,15.2,10.476606819));
#225067=CARTESIAN_POINT('Ctrl Pts',(0.159036538999944,15.2,10.478193371));
#225068=CARTESIAN_POINT('Ctrl Pts',(0.159328093999944,15.2,10.479787363));
#225069=CARTESIAN_POINT('Ctrl Pts',(0.159622555999944,15.2,10.481388775));
#225070=CARTESIAN_POINT('Ctrl Pts',(0.159919935999945,15.2,10.482997587));
#225071=CARTESIAN_POINT('Ctrl Pts',(0.160220243999945,15.2,10.484613776));
#225072=CARTESIAN_POINT('Ctrl Pts',(0.160523488999944,15.2,10.486237324));
#225073=CARTESIAN_POINT('Ctrl Pts',(0.160829681999944,15.2,10.487868211));
#225074=CARTESIAN_POINT('Ctrl Pts',(0.161138831999944,15.2,10.489506414));
#225075=CARTESIAN_POINT('Ctrl Pts',(0.161450947999944,15.2,10.491151915));
#225076=CARTESIAN_POINT('Ctrl Pts',(0.161766040999943,15.2,10.492804693));
#225077=CARTESIAN_POINT('Ctrl Pts',(0.162084119999945,15.2,10.494464727));
#225078=CARTESIAN_POINT('Ctrl Pts',(0.162405193999945,15.2,10.496131999));
#225079=CARTESIAN_POINT('Ctrl Pts',(0.162729271999943,15.2,10.497806487));
#225080=CARTESIAN_POINT('Ctrl Pts',(0.163056365999944,15.2,10.499488173));
#225081=CARTESIAN_POINT('Ctrl Pts',(0.163386482999943,15.2,10.501177035));
#225082=CARTESIAN_POINT('Ctrl Pts',(0.163719631999945,15.2,10.502873055));
#225083=CARTESIAN_POINT('Ctrl Pts',(0.164055823999943,15.2,10.504576213));
#225084=CARTESIAN_POINT('Ctrl Pts',(0.164395066999944,15.2,10.506286488));
#225085=CARTESIAN_POINT('Ctrl Pts',(0.164737370999944,15.2,10.508003861));
#225086=CARTESIAN_POINT('Ctrl Pts',(0.165082743999945,15.2,10.509728314));
#225087=CARTESIAN_POINT('Ctrl Pts',(0.165431195999943,15.2,10.511459827));
#225088=CARTESIAN_POINT('Ctrl Pts',(0.165782736999944,15.2,10.513198379));
#225089=CARTESIAN_POINT('Ctrl Pts',(0.166137373999945,15.2,10.514943952));
#225090=CARTESIAN_POINT('Ctrl Pts',(0.166495116999944,15.2,10.516696527));
#225091=CARTESIAN_POINT('Ctrl Pts',(0.166855973999944,15.2,10.518456083));
#225092=CARTESIAN_POINT('Ctrl Pts',(0.167219954999943,15.2,10.520222605));
#225093=CARTESIAN_POINT('Ctrl Pts',(0.167587068999945,15.2,10.521996069));
#225094=CARTESIAN_POINT('Ctrl Pts',(0.167957322999944,15.2,10.523776458));
#225095=CARTESIAN_POINT('Ctrl Pts',(0.168330727999945,15.2,10.525563754));
#225096=CARTESIAN_POINT('Ctrl Pts',(0.168707291999944,15.2,10.527357938));
#225097=CARTESIAN_POINT('Ctrl Pts',(0.169087021999944,15.2,10.52915899));
#225098=CARTESIAN_POINT('Ctrl Pts',(0.169469929999944,15.2,10.530966892));
#225099=CARTESIAN_POINT('Ctrl Pts',(0.169856019999944,15.2,10.532781625));
#225100=CARTESIAN_POINT('Ctrl Pts',(0.170245304999943,15.2,10.534603171));
#225101=CARTESIAN_POINT('Ctrl Pts',(0.170637789999945,15.2,10.536431512));
#225102=CARTESIAN_POINT('Ctrl Pts',(0.171033485999944,15.2,10.538266627));
#225103=CARTESIAN_POINT('Ctrl Pts',(0.171432399999943,15.2,10.5401085));
#225104=CARTESIAN_POINT('Ctrl Pts',(0.171834540999944,15.2,10.541957111));
#225105=CARTESIAN_POINT('Ctrl Pts',(0.172239915999944,15.2,10.543812444));
#225106=CARTESIAN_POINT('Ctrl Pts',(0.172648535999944,15.2,10.545674477));
#225107=CARTESIAN_POINT('Ctrl Pts',(0.173060405999944,15.2,10.547543196));
#225108=CARTESIAN_POINT('Ctrl Pts',(0.173475535999945,15.2,10.549418579));
#225109=CARTESIAN_POINT('Ctrl Pts',(0.173893933999943,15.2,10.551300611));
#225110=CARTESIAN_POINT('Ctrl Pts',(0.174315608999944,15.2,10.553189272));
#225111=CARTESIAN_POINT('Ctrl Pts',(0.174740566999944,15.2,10.555084546));
#225112=CARTESIAN_POINT('Ctrl Pts',(0.175168817999944,15.2,10.556986414));
#225113=CARTESIAN_POINT('Ctrl Pts',(0.175600368999945,15.2,10.558894856));
#225114=CARTESIAN_POINT('Ctrl Pts',(0.176035227999943,15.2,10.560809858));
#225115=CARTESIAN_POINT('Ctrl Pts',(0.176473402999945,15.2,10.5627314));
#225116=CARTESIAN_POINT('Ctrl Pts',(0.176914901999944,15.2,10.564659464));
#225117=CARTESIAN_POINT('Ctrl Pts',(0.177359733999944,15.2,10.566594034));
#225118=CARTESIAN_POINT('Ctrl Pts',(0.177807903999945,15.2,10.568535092));
#225119=CARTESIAN_POINT('Ctrl Pts',(0.178259421999943,15.2,10.570482619));
#225120=CARTESIAN_POINT('Ctrl Pts',(0.178714295999944,15.2,10.5724366));
#225121=CARTESIAN_POINT('Ctrl Pts',(0.179172531999944,15.2,10.574397014));
#225122=CARTESIAN_POINT('Ctrl Pts',(0.179634138999945,15.2,10.576363848));
#225123=CARTESIAN_POINT('Ctrl Pts',(0.180099123999945,15.2,10.578337082));
#225124=CARTESIAN_POINT('Ctrl Pts',(0.180567494999944,15.2,10.580316698));
#225125=CARTESIAN_POINT('Ctrl Pts',(0.181039259999943,15.2,10.582302681));
#225126=CARTESIAN_POINT('Ctrl Pts',(0.181514424999945,15.2,10.584295013));
#225127=CARTESIAN_POINT('Ctrl Pts',(0.181992997999944,15.2,10.586293676));
#225128=CARTESIAN_POINT('Ctrl Pts',(0.182474987999944,15.2,10.588298654));
#225129=CARTESIAN_POINT('Ctrl Pts',(0.182960400999944,15.2,10.59030993));
#225130=CARTESIAN_POINT('Ctrl Pts',(0.183449243999944,15.2,10.592327487));
#225131=CARTESIAN_POINT('Ctrl Pts',(0.183941525999943,15.2,10.594351307));
#225132=CARTESIAN_POINT('Ctrl Pts',(0.184437252999944,15.2,10.596381375));
#225133=CARTESIAN_POINT('Ctrl Pts',(0.184936431999944,15.2,10.598417673));
#225134=CARTESIAN_POINT('Ctrl Pts',(0.185439070999944,15.2,10.600460184));
#225135=CARTESIAN_POINT('Ctrl Pts',(0.185945176999944,15.2,10.602508892));
#225136=CARTESIAN_POINT('Ctrl Pts',(0.186454757999943,15.2,10.604563781));
#225137=CARTESIAN_POINT('Ctrl Pts',(0.186967819999945,15.2,10.606624832));
#225138=CARTESIAN_POINT('Ctrl Pts',(0.187484369999943,15.2,10.608692031));
#225139=CARTESIAN_POINT('Ctrl Pts',(0.188004415999944,15.2,10.61076536));
#225140=CARTESIAN_POINT('Ctrl Pts',(0.188527964999944,15.2,10.612844803));
#225141=CARTESIAN_POINT('Ctrl Pts',(0.189055023999943,15.2,10.614930343));
#225142=CARTESIAN_POINT('Ctrl Pts',(0.189585597999944,15.2,10.617021966));
#225143=CARTESIAN_POINT('Ctrl Pts',(0.190119695999943,15.2,10.619119652));
#225144=CARTESIAN_POINT('Ctrl Pts',(0.190657324999943,15.2,10.621223388));
#225145=CARTESIAN_POINT('Ctrl Pts',(0.191198490999945,15.2,10.623333156));
#225146=CARTESIAN_POINT('Ctrl Pts',(0.191743202999944,15.2,10.62544894));
#225147=CARTESIAN_POINT('Ctrl Pts',(0.192291463999944,15.2,10.627570724));
#225148=CARTESIAN_POINT('Ctrl Pts',(0.192843282999944,15.2,10.629698493));
#225149=CARTESIAN_POINT('Ctrl Pts',(0.193398666999943,15.2,10.631832228));
#225150=CARTESIAN_POINT('Ctrl Pts',(0.193957621999944,15.2,10.633971917));
#225151=CARTESIAN_POINT('Ctrl Pts',(0.194520154999944,15.2,10.636117541));
#225152=CARTESIAN_POINT('Ctrl Pts',(0.195086272999945,15.2,10.638269086));
#225153=CARTESIAN_POINT('Ctrl Pts',(0.195655981999945,15.2,10.640426535));
#225154=CARTESIAN_POINT('Ctrl Pts',(0.196229288999945,15.2,10.642589871));
#225155=CARTESIAN_POINT('Ctrl Pts',(0.196806200999945,15.2,10.644759081));
#225156=CARTESIAN_POINT('Ctrl Pts',(0.197386722999945,15.2,10.646934148));
#225157=CARTESIAN_POINT('Ctrl Pts',(0.197970861999943,15.2,10.649115056));
#225158=CARTESIAN_POINT('Ctrl Pts',(0.198558625999944,15.2,10.651301789));
#225159=CARTESIAN_POINT('Ctrl Pts',(0.199150019999944,15.2,10.653494334));
#225160=CARTESIAN_POINT('Ctrl Pts',(0.199745050999944,15.2,10.655692671));
#225161=CARTESIAN_POINT('Ctrl Pts',(0.200343724999945,15.2,10.657896788));
#225162=CARTESIAN_POINT('Ctrl Pts',(0.200946048999944,15.2,10.660106669));
#225163=CARTESIAN_POINT('Ctrl Pts',(0.201552027999944,15.2,10.662322298));
#225164=CARTESIAN_POINT('Ctrl Pts',(0.202161669999944,15.2,10.664543659));
#225165=CARTESIAN_POINT('Ctrl Pts',(0.202774978999944,15.2,10.666770738));
#225166=CARTESIAN_POINT('Ctrl Pts',(0.203391963999945,15.2,10.669003518));
#225167=CARTESIAN_POINT('Ctrl Pts',(0.204012629999945,15.2,10.671241985));
#225168=CARTESIAN_POINT('Ctrl Pts',(0.204636982999944,15.2,10.673486125));
#225169=CARTESIAN_POINT('Ctrl Pts',(0.205265027999945,15.2,10.67573592));
#225170=CARTESIAN_POINT('Ctrl Pts',(0.205896773999944,15.2,10.677991356));
#225171=CARTESIAN_POINT('Ctrl Pts',(0.206532223999943,15.2,10.680252419));
#225172=CARTESIAN_POINT('Ctrl Pts',(0.207171385999944,15.2,10.682519093));
#225173=CARTESIAN_POINT('Ctrl Pts',(0.207814266999945,15.2,10.684791362));
#225174=CARTESIAN_POINT('Ctrl Pts',(0.208460869999945,15.2,10.687069213));
#225175=CARTESIAN_POINT('Ctrl Pts',(0.209111202999944,15.2,10.68935263));
#225176=CARTESIAN_POINT('Ctrl Pts',(0.209765270999943,15.2,10.691641598));
#225177=CARTESIAN_POINT('Ctrl Pts',(0.210423080999943,15.2,10.693936102));
#225178=CARTESIAN_POINT('Ctrl Pts',(0.211084637999944,15.2,10.696236128));
#225179=CARTESIAN_POINT('Ctrl Pts',(0.211749947999945,15.2,10.69854166));
#225180=CARTESIAN_POINT('Ctrl Pts',(0.212419017999944,15.2,10.700852684));
#225181=CARTESIAN_POINT('Ctrl Pts',(0.213091851999945,15.2,10.703169186));
#225182=CARTESIAN_POINT('Ctrl Pts',(0.213768457999944,15.2,10.70549115));
#225183=CARTESIAN_POINT('Ctrl Pts',(0.214448838999944,15.2,10.707818563));
#225184=CARTESIAN_POINT('Ctrl Pts',(0.215133002999943,15.2,10.710151408));
#225185=CARTESIAN_POINT('Ctrl Pts',(0.215820953999944,15.2,10.712489672));
#225186=CARTESIAN_POINT('Ctrl Pts',(0.216512699999944,15.2,10.71483334));
#225187=CARTESIAN_POINT('Ctrl Pts',(0.217208243999943,15.2,10.717182399));
#225188=CARTESIAN_POINT('Ctrl Pts',(0.217907592999945,15.2,10.719536832));
#225189=CARTESIAN_POINT('Ctrl Pts',(0.218610752999944,15.2,10.721896627));
#225190=CARTESIAN_POINT('Ctrl Pts',(0.219317728999944,15.2,10.724261769));
#225191=CARTESIAN_POINT('Ctrl Pts',(0.220028526999944,15.2,10.726632242));
#225192=CARTESIAN_POINT('Ctrl Pts',(0.220743151999944,15.2,10.729008033));
#225193=CARTESIAN_POINT('Ctrl Pts',(0.221461608999943,15.2,10.731389127));
#225194=CARTESIAN_POINT('Ctrl Pts',(0.222183904999945,15.2,10.733775512));
#225195=CARTESIAN_POINT('Ctrl Pts',(0.222910043999944,15.2,10.736167171));
#225196=CARTESIAN_POINT('Ctrl Pts',(0.223640032999944,15.2,10.738564091));
#225197=CARTESIAN_POINT('Ctrl Pts',(0.224373874999945,15.2,10.740966259));
#225198=CARTESIAN_POINT('Ctrl Pts',(0.225111577999944,15.2,10.743373659));
#225199=CARTESIAN_POINT('Ctrl Pts',(0.225853144999943,15.2,10.745786278));
#225200=CARTESIAN_POINT('Ctrl Pts',(0.226598583999945,15.2,10.748204101));
#225201=CARTESIAN_POINT('Ctrl Pts',(0.227347897999944,15.2,10.750627115));
#225202=CARTESIAN_POINT('Ctrl Pts',(0.228101093999945,15.2,10.753055306));
#225203=CARTESIAN_POINT('Ctrl Pts',(0.228858174999944,15.2,10.755488661));
#225204=CARTESIAN_POINT('Ctrl Pts',(0.229619148999944,15.2,10.757927164));
#225205=CARTESIAN_POINT('Ctrl Pts',(0.230384019999944,15.2,10.760370801));
#225206=CARTESIAN_POINT('Ctrl Pts',(0.231152791999945,15.2,10.762819561));
#225207=CARTESIAN_POINT('Ctrl Pts',(0.231925471999944,15.2,10.765273427));
#225208=CARTESIAN_POINT('Ctrl Pts',(0.232702063999944,15.2,10.767732388));
#225209=CARTESIAN_POINT('Ctrl Pts',(0.233482572999945,15.2,10.770196429));
#225210=CARTESIAN_POINT('Ctrl Pts',(0.234267004999945,15.2,10.772665536));
#225211=CARTESIAN_POINT('Ctrl Pts',(0.235055364999944,15.2,10.775139696));
#225212=CARTESIAN_POINT('Ctrl Pts',(0.235847656999945,15.2,10.777618895));
#225213=CARTESIAN_POINT('Ctrl Pts',(0.236643886999944,15.2,10.780103119));
#225214=CARTESIAN_POINT('Ctrl Pts',(0.237444059999945,15.2,10.782592356));
#225215=CARTESIAN_POINT('Ctrl Pts',(0.238248179999945,15.2,10.78508659));
#225216=CARTESIAN_POINT('Ctrl Pts',(0.239056252999944,15.2,10.78758581));
#225217=CARTESIAN_POINT('Ctrl Pts',(0.239868283999943,15.2,10.790090001));
#225218=CARTESIAN_POINT('Ctrl Pts',(0.240684276999945,15.2,10.79259915));
#225219=CARTESIAN_POINT('Ctrl Pts',(0.241504236999944,15.2,10.795113244));
#225220=CARTESIAN_POINT('Ctrl Pts',(0.242328170999944,15.2,10.797632269));
#225221=CARTESIAN_POINT('Ctrl Pts',(0.243156079999943,15.2,10.800156212));
#225222=CARTESIAN_POINT('Ctrl Pts',(0.243987971999945,15.2,10.80268506));
#225223=CARTESIAN_POINT('Ctrl Pts',(0.244823849999944,15.2,10.805218799));
#225224=CARTESIAN_POINT('Ctrl Pts',(0.245663720999945,15.2,10.807757416));
#225225=CARTESIAN_POINT('Ctrl Pts',(0.246507586999943,15.2,10.810300898));
#225226=CARTESIAN_POINT('Ctrl Pts',(0.247355453999945,15.2,10.812849232));
#225227=CARTESIAN_POINT('Ctrl Pts',(0.248207326999944,15.2,10.815402405));
#225228=CARTESIAN_POINT('Ctrl Pts',(0.249063209999945,15.2,10.817960403));
#225229=CARTESIAN_POINT('Ctrl Pts',(0.249923107999944,15.2,10.820523213));
#225230=CARTESIAN_POINT('Ctrl Pts',(0.250787026999945,15.2,10.823090823));
#225231=CARTESIAN_POINT('Ctrl Pts',(0.251654968999944,15.2,10.825663219));
#225232=CARTESIAN_POINT('Ctrl Pts',(0.252526938999944,15.2,10.828240388));
#225233=CARTESIAN_POINT('Ctrl Pts',(0.253402944999944,15.2,10.830822318));
#225234=CARTESIAN_POINT('Ctrl Pts',(0.254282986999945,15.2,10.833408995));
#225235=CARTESIAN_POINT('Ctrl Pts',(0.255167071999944,15.2,10.836000406));
#225236=CARTESIAN_POINT('Ctrl Pts',(0.256055205999944,15.2,10.838596539));
#225237=CARTESIAN_POINT('Ctrl Pts',(0.256947389999944,15.2,10.841197381));
#225238=CARTESIAN_POINT('Ctrl Pts',(0.257843629999943,15.2,10.843802919));
#225239=CARTESIAN_POINT('Ctrl Pts',(0.258743930999945,15.2,10.846413139));
#225240=CARTESIAN_POINT('Ctrl Pts',(0.259648296999944,15.2,10.84902803));
#225241=CARTESIAN_POINT('Ctrl Pts',(0.260556730999945,15.2,10.851647579));
#225242=CARTESIAN_POINT('Ctrl Pts',(0.261469239999944,15.2,10.854271772));
#225243=CARTESIAN_POINT('Ctrl Pts',(0.262385827999945,15.2,10.856900597));
#225244=CARTESIAN_POINT('Ctrl Pts',(0.263306497999943,15.2,10.859534043));
#225245=CARTESIAN_POINT('Ctrl Pts',(0.264231254999944,15.2,10.862172095));
#225246=CARTESIAN_POINT('Ctrl Pts',(0.265160102999945,15.2,10.864814741));
#225247=CARTESIAN_POINT('Ctrl Pts',(0.266093045999943,15.2,10.867461969));
#225248=CARTESIAN_POINT('Ctrl Pts',(0.267030088999943,15.2,10.870113767));
#225249=CARTESIAN_POINT('Ctrl Pts',(0.267971236999944,15.2,10.872770121));
#225250=CARTESIAN_POINT('Ctrl Pts',(0.268916491999944,15.2,10.875431019));
#225251=CARTESIAN_POINT('Ctrl Pts',(0.269865859999945,15.2,10.878096449));
#225252=CARTESIAN_POINT('Ctrl Pts',(0.270819344999945,15.2,10.880766399));
#225253=CARTESIAN_POINT('Ctrl Pts',(0.271776950999945,15.2,10.883440855));
#225254=CARTESIAN_POINT('Ctrl Pts',(0.272738680999945,15.2,10.886119805));
#225255=CARTESIAN_POINT('Ctrl Pts',(0.273704539999944,15.2,10.888803238));
#225256=CARTESIAN_POINT('Ctrl Pts',(0.274674533999945,15.2,10.89149114));
#225257=CARTESIAN_POINT('Ctrl Pts',(0.275648663999943,15.2,10.894183501));
#225258=CARTESIAN_POINT('Ctrl Pts',(0.276626936999945,15.2,10.896880306));
#225259=CARTESIAN_POINT('Ctrl Pts',(0.277609353999945,15.2,10.899581544));
#225260=CARTESIAN_POINT('Ctrl Pts',(0.278595920999944,15.2,10.902287203));
#225261=CARTESIAN_POINT('Ctrl Pts',(0.279586641999944,15.2,10.904997271));
#225262=CARTESIAN_POINT('Ctrl Pts',(0.280581519999944,15.2,10.907711735));
#225263=CARTESIAN_POINT('Ctrl Pts',(0.281580559999943,15.2,10.910430582));
#225264=CARTESIAN_POINT('Ctrl Pts',(0.282583764999943,15.2,10.913153803));
#225265=CARTESIAN_POINT('Ctrl Pts',(0.283591139999944,15.2,10.915881383));
#225266=CARTESIAN_POINT('Ctrl Pts',(0.284602689999945,15.2,10.918613312));
#225267=CARTESIAN_POINT('Ctrl Pts',(0.285618414999943,15.2,10.921349576));
#225268=CARTESIAN_POINT('Ctrl Pts',(0.286638321999944,15.2,10.924090164));
#225269=CARTESIAN_POINT('Ctrl Pts',(0.287662414999945,15.2,10.926835064));
#225270=CARTESIAN_POINT('Ctrl Pts',(0.288690695999945,15.2,10.929584263));
#225271=CARTESIAN_POINT('Ctrl Pts',(0.289723169999944,15.2,10.932337751));
#225272=CARTESIAN_POINT('Ctrl Pts',(0.290759841999944,15.2,10.935095515));
#225273=CARTESIAN_POINT('Ctrl Pts',(0.291800711999944,15.2,10.937857544));
#225274=CARTESIAN_POINT('Ctrl Pts',(0.292845787999945,15.2,10.940623824));
#225275=CARTESIAN_POINT('Ctrl Pts',(0.293895072999945,15.2,10.943394344));
#225276=CARTESIAN_POINT('Ctrl Pts',(0.294948567999944,15.2,10.946169093));
#225277=CARTESIAN_POINT('Ctrl Pts',(0.296006278999944,15.2,10.94894806));
#225278=CARTESIAN_POINT('Ctrl Pts',(0.297068208999944,15.2,10.951731231));
#225279=CARTESIAN_POINT('Ctrl Pts',(0.298134362999944,15.2,10.954518595));
#225280=CARTESIAN_POINT('Ctrl Pts',(0.299204742999944,15.2,10.957310141));
#225281=CARTESIAN_POINT('Ctrl Pts',(0.300279352999944,15.2,10.960105857));
#225282=CARTESIAN_POINT('Ctrl Pts',(0.301358196999945,15.2,10.962905732));
#225283=CARTESIAN_POINT('Ctrl Pts',(0.302441278999943,15.2,10.965709751));
#225284=CARTESIAN_POINT('Ctrl Pts',(0.303528602999944,15.2,10.968517908));
#225285=CARTESIAN_POINT('Ctrl Pts',(0.304620169999945,15.2,10.971330186));
#225286=CARTESIAN_POINT('Ctrl Pts',(0.305715986999945,15.2,10.974146576));
#225287=CARTESIAN_POINT('Ctrl Pts',(0.306816055999944,15.2,10.976967067));
#225288=CARTESIAN_POINT('Ctrl Pts',(0.307920378999944,15.2,10.979791646));
#225289=CARTESIAN_POINT('Ctrl Pts',(0.309028961999944,15.2,10.982620303));
#225290=CARTESIAN_POINT('Ctrl Pts',(0.310141807999944,15.2,10.985453024));
#225291=CARTESIAN_POINT('Ctrl Pts',(0.311258918999944,15.2,10.988289801));
#225292=CARTESIAN_POINT('Ctrl Pts',(0.312380299999945,15.2,10.991130619));
#225293=CARTESIAN_POINT('Ctrl Pts',(0.313505953999943,15.2,10.993975469));
#225294=CARTESIAN_POINT('Ctrl Pts',(0.314635883999944,15.2,10.996824338));
#225295=CARTESIAN_POINT('Ctrl Pts',(0.315770094999944,15.2,10.999677217));
#225296=CARTESIAN_POINT('Ctrl Pts',(0.316908587999943,15.2,11.002534092));
#225297=CARTESIAN_POINT('Ctrl Pts',(0.318051368999944,15.2,11.005394953));
#225298=CARTESIAN_POINT('Ctrl Pts',(0.319198438999945,15.2,11.008259789));
#225299=CARTESIAN_POINT('Ctrl Pts',(0.320349802999944,15.2,11.011128587));
#225300=CARTESIAN_POINT('Ctrl Pts',(0.321505462999945,15.2,11.014001339));
#225301=CARTESIAN_POINT('Ctrl Pts',(0.322665423999944,15.2,11.016878029));
#225302=CARTESIAN_POINT('Ctrl Pts',(0.323829688999944,15.2,11.01975865));
#225303=CARTESIAN_POINT('Ctrl Pts',(0.324998259999945,15.2,11.02264319));
#225304=CARTESIAN_POINT('Ctrl Pts',(0.326171140999945,15.2,11.025531635));
#225305=CARTESIAN_POINT('Ctrl Pts',(0.327348334999943,15.2,11.028423977));
#225306=CARTESIAN_POINT('Ctrl Pts',(0.328529845999944,15.2,11.031320203));
#225307=CARTESIAN_POINT('Ctrl Pts',(0.329715676999944,15.2,11.034220304));
#225308=CARTESIAN_POINT('Ctrl Pts',(0.330905830999945,15.2,11.037124267));
#225309=CARTESIAN_POINT('Ctrl Pts',(0.332100310999944,15.2,11.040032081));
#225310=CARTESIAN_POINT('Ctrl Pts',(0.333299119999945,15.2,11.042943736));
#225311=CARTESIAN_POINT('Ctrl Pts',(0.334502261999944,15.2,11.04585922));
#225312=CARTESIAN_POINT('Ctrl Pts',(0.335709739999944,15.2,11.048778522));
#225313=CARTESIAN_POINT('Ctrl Pts',(0.336921556999944,15.2,11.051701632));
#225314=CARTESIAN_POINT('Ctrl Pts',(0.338137715999943,15.2,11.054628538));
#225315=CARTESIAN_POINT('Ctrl Pts',(0.339358218999944,15.2,11.057559229));
#225316=CARTESIAN_POINT('Ctrl Pts',(0.340583071999945,15.2,11.060493695));
#225317=CARTESIAN_POINT('Ctrl Pts',(0.341812274999944,15.2,11.063431924));
#225318=CARTESIAN_POINT('Ctrl Pts',(0.343045832999945,15.2,11.066373907));
#225319=CARTESIAN_POINT('Ctrl Pts',(0.344283748999944,15.2,11.069319631));
#225320=CARTESIAN_POINT('Ctrl Pts',(0.345526024999945,15.2,11.072269087));
#225321=CARTESIAN_POINT('Ctrl Pts',(0.346772663999945,15.2,11.075222263));
#225322=CARTESIAN_POINT('Ctrl Pts',(0.348023670999943,15.2,11.078179147));
#225323=CARTESIAN_POINT('Ctrl Pts',(0.349279045999945,15.2,11.081139731));
#225324=CARTESIAN_POINT('Ctrl Pts',(0.350538794999944,15.2,11.084104002));
#225325=CARTESIAN_POINT('Ctrl Pts',(0.351802917999944,15.2,11.087071951));
#225326=CARTESIAN_POINT('Ctrl Pts',(0.353071419999944,15.2,11.090043565));
#225327=CARTESIAN_POINT('Ctrl Pts',(0.354344304999945,15.2,11.093018835));
#225328=CARTESIAN_POINT('Ctrl Pts',(0.355621571999943,15.2,11.095997751));
#225329=CARTESIAN_POINT('Ctrl Pts',(0.356903226999944,15.2,11.0989803));
#225330=CARTESIAN_POINT('Ctrl Pts',(0.358189272999944,15.2,11.101966473));
#225331=CARTESIAN_POINT('Ctrl Pts',(0.359479711999944,15.2,11.104956259));
#225332=CARTESIAN_POINT('Ctrl Pts',(0.360774545999943,15.2,11.107949648));
#225333=CARTESIAN_POINT('Ctrl Pts',(0.362073778999944,15.2,11.110946629));
#225334=CARTESIAN_POINT('Ctrl Pts',(0.363377412999943,15.2,11.11394719));
#225335=CARTESIAN_POINT('Ctrl Pts',(0.364685451999945,15.2,11.116951322));
#225336=CARTESIAN_POINT('Ctrl Pts',(0.365997898999944,15.2,11.119959015));
#225337=CARTESIAN_POINT('Ctrl Pts',(0.367314755999945,15.2,11.122970257));
#225338=CARTESIAN_POINT('Ctrl Pts',(0.368636023999944,15.2,11.125985039));
#225339=CARTESIAN_POINT('Ctrl Pts',(0.369961708999943,15.2,11.129003348));
#225340=CARTESIAN_POINT('Ctrl Pts',(0.371291811999944,15.2,11.132025177));
#225341=CARTESIAN_POINT('Ctrl Pts',(0.372626335999945,15.2,11.135050513));
#225342=CARTESIAN_POINT('Ctrl Pts',(0.373965283999944,15.2,11.138079346));
#225343=CARTESIAN_POINT('Ctrl Pts',(0.375308657999945,15.2,11.141111667));
#225344=CARTESIAN_POINT('Ctrl Pts',(0.376656460999945,15.2,11.144147463));
#225345=CARTESIAN_POINT('Ctrl Pts',(0.378008696999944,15.2,11.147186727));
#225346=CARTESIAN_POINT('Ctrl Pts',(0.379365366999943,15.2,11.150229446));
#225347=CARTESIAN_POINT('Ctrl Pts',(0.380726473999945,15.2,11.15327561));
#225348=CARTESIAN_POINT('Ctrl Pts',(0.382092020999943,15.2,11.15632521));
#225349=CARTESIAN_POINT('Ctrl Pts',(0.383462009999944,15.2,11.159378235));
#225350=CARTESIAN_POINT('Ctrl Pts',(0.384836444999944,15.2,11.162434674));
#225351=CARTESIAN_POINT('Ctrl Pts',(0.386215327999944,15.2,11.165494518));
#225352=CARTESIAN_POINT('Ctrl Pts',(0.387598660999944,15.2,11.168557757));
#225353=CARTESIAN_POINT('Ctrl Pts',(0.388986445999944,15.2,11.171624378));
#225354=CARTESIAN_POINT('Ctrl Pts',(0.390378687999944,15.2,11.174694374));
#225355=CARTESIAN_POINT('Ctrl Pts',(0.391775385999944,15.2,11.177767734));
#225356=CARTESIAN_POINT('Ctrl Pts',(0.393176546999945,15.2,11.180844446));
#225357=CARTESIAN_POINT('Ctrl Pts',(0.394582168999945,15.2,11.183924503));
#225358=CARTESIAN_POINT('Ctrl Pts',(0.395992257999945,15.2,11.187007891));
#225359=CARTESIAN_POINT('Ctrl Pts',(0.397406813999943,15.2,11.190094604));
#225360=CARTESIAN_POINT('Ctrl Pts',(0.398825840999945,15.2,11.193184629));
#225361=CARTESIAN_POINT('Ctrl Pts',(0.400249340999944,15.2,11.196277957));
#225362=CARTESIAN_POINT('Ctrl Pts',(0.401677316999944,15.2,11.199374578));
#225363=CARTESIAN_POINT('Ctrl Pts',(0.403109770999944,15.2,11.202474482));
#225364=CARTESIAN_POINT('Ctrl Pts',(0.404546704999945,15.2,11.205577658));
#225365=CARTESIAN_POINT('Ctrl Pts',(0.405988121999944,15.2,11.208684097));
#225366=CARTESIAN_POINT('Ctrl Pts',(0.407434024999944,15.2,11.211793789));
#225367=CARTESIAN_POINT('Ctrl Pts',(0.408884414999945,15.2,11.214906723));
#225368=CARTESIAN_POINT('Ctrl Pts',(0.410339294999943,15.2,11.21802289));
#225369=CARTESIAN_POINT('Ctrl Pts',(0.411798665999944,15.2,11.22114228));
#225370=CARTESIAN_POINT('Ctrl Pts',(0.413262533999944,15.2,11.224264884));
#225371=CARTESIAN_POINT('Ctrl Pts',(0.414730897999943,15.2,11.227390689));
#225372=CARTESIAN_POINT('Ctrl Pts',(0.416203760999944,15.2,11.230519689));
#225373=CARTESIAN_POINT('Ctrl Pts',(0.417681126999945,15.2,11.233651872));
#225374=CARTESIAN_POINT('Ctrl Pts',(0.419162995999944,15.2,11.236787228));
#225375=CARTESIAN_POINT('Ctrl Pts',(0.420649371999945,15.2,11.239925747));
#225376=CARTESIAN_POINT('Ctrl Pts',(0.422140256999944,15.2,11.24306742));
#225377=CARTESIAN_POINT('Ctrl Pts',(0.423635651999945,15.2,11.246212238));
#225378=CARTESIAN_POINT('Ctrl Pts',(0.425135560999944,15.2,11.249360189));
#225379=CARTESIAN_POINT('Ctrl Pts',(0.426940870934353,15.2,11.2531414800626));
#225380=CARTESIAN_POINT('Ctrl Pts',(0.42875295653274,15.2,11.2569274424687));
#225381=CARTESIAN_POINT('Ctrl Pts',(0.430571823467149,15.2,11.2607180595313));
#225382=CARTESIAN_POINT('Ctrl Pts',(0.432397475065532,15.2,11.2645133069374));
#225383=CARTESIAN_POINT('Ctrl Pts',(0.434229916999945,15.2,11.268313168));
#225384=CARTESIAN_POINT('Ctrl Pts',(0.435761481999943,15.2,11.271482787));
#225385=CARTESIAN_POINT('Ctrl Pts',(0.437297575999944,15.2,11.27465546));
#225386=CARTESIAN_POINT('Ctrl Pts',(0.438838203999945,15.2,11.277831182));
#225387=CARTESIAN_POINT('Ctrl Pts',(0.440383366999945,15.2,11.28100994));
#225388=CARTESIAN_POINT('Ctrl Pts',(0.441933066999944,15.2,11.284191726));
#225389=CARTESIAN_POINT('Ctrl Pts',(0.443487306999945,15.2,11.287376529));
#225390=CARTESIAN_POINT('Ctrl Pts',(0.445046087999945,15.2,11.290564341));
#225391=CARTESIAN_POINT('Ctrl Pts',(0.446609412999944,15.2,11.293755151));
#225392=CARTESIAN_POINT('Ctrl Pts',(0.448177283999945,15.2,11.296948952));
#225393=CARTESIAN_POINT('Ctrl Pts',(0.449749701999943,15.2,11.300145732));
#225394=CARTESIAN_POINT('Ctrl Pts',(0.451326669999944,15.2,11.303345481));
#225395=CARTESIAN_POINT('Ctrl Pts',(0.452908190999944,15.2,11.306548191));
#225396=CARTESIAN_POINT('Ctrl Pts',(0.454494264999944,15.2,11.309753854));
#225397=CARTESIAN_POINT('Ctrl Pts',(0.456084895999943,15.2,11.312962457));
#225398=CARTESIAN_POINT('Ctrl Pts',(0.457680083999945,15.2,11.316173992));
#225399=CARTESIAN_POINT('Ctrl Pts',(0.459279831999944,15.2,11.319388451));
#225400=CARTESIAN_POINT('Ctrl Pts',(0.460884141999944,15.2,11.322605823));
#225401=CARTESIAN_POINT('Ctrl Pts',(0.462493016999945,15.2,11.325826099));
#225402=CARTESIAN_POINT('Ctrl Pts',(0.464106456999945,15.2,11.329049269));
#225403=CARTESIAN_POINT('Ctrl Pts',(0.465724464999945,15.2,11.332275324));
#225404=CARTESIAN_POINT('Ctrl Pts',(0.467347043999944,15.2,11.335504256));
#225405=CARTESIAN_POINT('Ctrl Pts',(0.468974193999945,15.2,11.338736055));
#225406=CARTESIAN_POINT('Ctrl Pts',(0.470605917999943,15.2,11.34197071));
#225407=CARTESIAN_POINT('Ctrl Pts',(0.472242216999945,15.2,11.345208212));
#225408=CARTESIAN_POINT('Ctrl Pts',(0.473883093999945,15.2,11.348448553));
#225409=CARTESIAN_POINT('Ctrl Pts',(0.475528549999943,15.2,11.351691724));
#225410=CARTESIAN_POINT('Ctrl Pts',(0.477178588999945,15.2,11.354937714));
#225411=CARTESIAN_POINT('Ctrl Pts',(0.478833209999945,15.2,11.358186515));
#225412=CARTESIAN_POINT('Ctrl Pts',(0.480492415999944,15.2,11.361438117));
#225413=CARTESIAN_POINT('Ctrl Pts',(0.482156208999944,15.2,11.364692512));
#225414=CARTESIAN_POINT('Ctrl Pts',(0.483824590999945,15.2,11.36794969));
#225415=CARTESIAN_POINT('Ctrl Pts',(0.485497562999945,15.2,11.371209642));
#225416=CARTESIAN_POINT('Ctrl Pts',(0.487175127999944,15.2,11.374472358));
#225417=CARTESIAN_POINT('Ctrl Pts',(0.488857286999943,15.2,11.37773783));
#225418=CARTESIAN_POINT('Ctrl Pts',(0.490544042999945,15.2,11.381006048));
#225419=CARTESIAN_POINT('Ctrl Pts',(0.492235395999945,15.2,11.384277002));
#225420=CARTESIAN_POINT('Ctrl Pts',(0.493931348999944,15.2,11.387550685));
#225421=CARTESIAN_POINT('Ctrl Pts',(0.495631902999945,15.2,11.390827085));
#225422=CARTESIAN_POINT('Ctrl Pts',(0.497337059999945,15.2,11.394106196));
#225423=CARTESIAN_POINT('Ctrl Pts',(0.499046822999943,15.2,11.397388008));
#225424=CARTESIAN_POINT('Ctrl Pts',(0.500761191999944,15.2,11.400672511));
#225425=CARTESIAN_POINT('Ctrl Pts',(0.502480167999945,15.2,11.403959697));
#225426=CARTESIAN_POINT('Ctrl Pts',(0.504203755999945,15.2,11.407249557));
#225427=CARTESIAN_POINT('Ctrl Pts',(0.505931953999944,15.2,11.410542081));
#225428=CARTESIAN_POINT('Ctrl Pts',(0.507664765999943,15.2,11.413837262));
#225429=CARTESIAN_POINT('Ctrl Pts',(0.509402193999944,15.2,11.417135088));
#225430=CARTESIAN_POINT('Ctrl Pts',(0.511144237999944,15.2,11.420435552));
#225431=CARTESIAN_POINT('Ctrl Pts',(0.512890899999944,15.2,11.423738642));
#225432=CARTESIAN_POINT('Ctrl Pts',(0.514642183999944,15.2,11.427044351));
#225433=CARTESIAN_POINT('Ctrl Pts',(0.516398088999944,15.2,11.43035267));
#225434=CARTESIAN_POINT('Ctrl Pts',(0.518158616999944,15.2,11.43366359));
#225435=CARTESIAN_POINT('Ctrl Pts',(0.519923770999945,15.2,11.436977102));
#225436=CARTESIAN_POINT('Ctrl Pts',(0.521693550999944,15.2,11.440293201));
#225437=CARTESIAN_POINT('Ctrl Pts',(0.523467958999944,15.2,11.443611876));
#225438=CARTESIAN_POINT('Ctrl Pts',(0.525246995999944,15.2,11.446933119));
#225439=CARTESIAN_POINT('Ctrl Pts',(0.527030663999944,15.2,11.450256921));
#225440=CARTESIAN_POINT('Ctrl Pts',(0.528818964999944,15.2,11.453583273));
#225441=CARTESIAN_POINT('Ctrl Pts',(0.530611901999943,15.2,11.456912161));
#225442=CARTESIAN_POINT('Ctrl Pts',(0.532409473999944,15.2,11.460243578));
#225443=CARTESIAN_POINT('Ctrl Pts',(0.534211683999944,15.2,11.46357751));
#225444=CARTESIAN_POINT('Ctrl Pts',(0.536018536999944,15.2,11.466913949));
#225445=CARTESIAN_POINT('Ctrl Pts',(0.537830029999945,15.2,11.470252887));
#225446=CARTESIAN_POINT('Ctrl Pts',(0.539646165999944,15.2,11.473594318));
#225447=CARTESIAN_POINT('Ctrl Pts',(0.541466945999944,15.2,11.476938237));
#225448=CARTESIAN_POINT('Ctrl Pts',(0.543292368999944,15.2,11.480284644));
#225449=CARTESIAN_POINT('Ctrl Pts',(0.544756420999944,15.2,11.482963756));
#225450=CARTESIAN_POINT('Ctrl Pts',(0.545856550999945,15.2,11.484974209));
#225451=CARTESIAN_POINT('Ctrl Pts',(0.546590898999945,15.2,11.486315008));
#225452=CARTESIAN_POINT('Ctrl Pts',(0.546958305999944,15.2,11.486985532));
#225453=CARTESIAN_POINT('Ctrl Pts',(1.18690176599994,15.2,10.306885525));
#225454=CARTESIAN_POINT('Ctrl Pts',(1.18690176599994,11.6,10.306885525));
#225455=CARTESIAN_POINT('Ctrl Pts',(1.18690675299994,15.2,10.307059811));
#225456=CARTESIAN_POINT('Ctrl Pts',(1.18690675299994,11.6,10.307059811));
#225457=CARTESIAN_POINT('Ctrl Pts',(1.18691681599994,15.2,10.307414474));
#225458=CARTESIAN_POINT('Ctrl Pts',(1.18691681599994,11.6,10.307414474));
#225459=CARTESIAN_POINT('Ctrl Pts',(1.18693179799994,15.2,10.30795188));
#225460=CARTESIAN_POINT('Ctrl Pts',(1.18693179799994,11.6,10.30795188));
#225461=CARTESIAN_POINT('Ctrl Pts',(1.18695143899994,15.2,10.30867583));
#225462=CARTESIAN_POINT('Ctrl Pts',(1.18695143899994,11.6,10.30867583));
#225463=CARTESIAN_POINT('Ctrl Pts',(1.18697536999994,15.2,10.309591544));
#225464=CARTESIAN_POINT('Ctrl Pts',(1.18697536999994,11.6,10.309591544));
#225465=CARTESIAN_POINT('Ctrl Pts',(1.18699875399994,15.2,10.310522124));
#225466=CARTESIAN_POINT('Ctrl Pts',(1.18699875399994,11.6,10.310522124));
#225467=CARTESIAN_POINT('Ctrl Pts',(1.18702143499994,15.2,10.311462238));
#225468=CARTESIAN_POINT('Ctrl Pts',(1.18702143499994,11.6,10.311462238));
#225469=CARTESIAN_POINT('Ctrl Pts',(1.18704339299994,15.2,10.312411862));
#225470=CARTESIAN_POINT('Ctrl Pts',(1.18704339299994,11.6,10.312411862));
#225471=CARTESIAN_POINT('Ctrl Pts',(1.18706460899994,15.2,10.313370965));
#225472=CARTESIAN_POINT('Ctrl Pts',(1.18706460899994,11.6,10.313370965));
#225473=CARTESIAN_POINT('Ctrl Pts',(1.18708506599994,15.2,10.314339525));
#225474=CARTESIAN_POINT('Ctrl Pts',(1.18708506599994,11.6,10.314339525));
#225475=CARTESIAN_POINT('Ctrl Pts',(1.18710474299994,15.2,10.315317514));
#225476=CARTESIAN_POINT('Ctrl Pts',(1.18710474299994,11.6,10.315317514));
#225477=CARTESIAN_POINT('Ctrl Pts',(1.18712362299994,15.2,10.316304905));
#225478=CARTESIAN_POINT('Ctrl Pts',(1.18712362299994,11.6,10.316304905));
#225479=CARTESIAN_POINT('Ctrl Pts',(1.18714168899994,15.2,10.317301674));
#225480=CARTESIAN_POINT('Ctrl Pts',(1.18714168899994,11.6,10.317301674));
#225481=CARTESIAN_POINT('Ctrl Pts',(1.18715892199994,15.2,10.318307794));
#225482=CARTESIAN_POINT('Ctrl Pts',(1.18715892199994,11.6,10.318307794));
#225483=CARTESIAN_POINT('Ctrl Pts',(1.18717530199994,15.2,10.319323239));
#225484=CARTESIAN_POINT('Ctrl Pts',(1.18717530199994,11.6,10.319323239));
#225485=CARTESIAN_POINT('Ctrl Pts',(1.18719081299994,15.2,10.320347985));
#225486=CARTESIAN_POINT('Ctrl Pts',(1.18719081299994,11.6,10.320347985));
#225487=CARTESIAN_POINT('Ctrl Pts',(1.18720543699994,15.2,10.321382005));
#225488=CARTESIAN_POINT('Ctrl Pts',(1.18720543699994,11.6,10.321382005));
#225489=CARTESIAN_POINT('Ctrl Pts',(1.18721915499994,15.2,10.322425274));
#225490=CARTESIAN_POINT('Ctrl Pts',(1.18721915499994,11.6,10.322425274));
#225491=CARTESIAN_POINT('Ctrl Pts',(1.18723195099994,15.2,10.323477767));
#225492=CARTESIAN_POINT('Ctrl Pts',(1.18723195099994,11.6,10.323477767));
#225493=CARTESIAN_POINT('Ctrl Pts',(1.18724380599994,15.2,10.324539459));
#225494=CARTESIAN_POINT('Ctrl Pts',(1.18724380599994,11.6,10.324539459));
#225495=CARTESIAN_POINT('Ctrl Pts',(1.18725470299994,15.2,10.325610325));
#225496=CARTESIAN_POINT('Ctrl Pts',(1.18725470299994,11.6,10.325610325));
#225497=CARTESIAN_POINT('Ctrl Pts',(1.18726462499994,15.2,10.326690339));
#225498=CARTESIAN_POINT('Ctrl Pts',(1.18726462499994,11.6,10.326690339));
#225499=CARTESIAN_POINT('Ctrl Pts',(1.18727355399994,15.2,10.327779478));
#225500=CARTESIAN_POINT('Ctrl Pts',(1.18727355399994,11.6,10.327779478));
#225501=CARTESIAN_POINT('Ctrl Pts',(1.18728147299994,15.2,10.328877715));
#225502=CARTESIAN_POINT('Ctrl Pts',(1.18728147299994,11.6,10.328877715));
#225503=CARTESIAN_POINT('Ctrl Pts',(1.18728836599994,15.2,10.329985029));
#225504=CARTESIAN_POINT('Ctrl Pts',(1.18728836599994,11.6,10.329985029));
#225505=CARTESIAN_POINT('Ctrl Pts',(1.18729421399994,15.2,10.331101392));
#225506=CARTESIAN_POINT('Ctrl Pts',(1.18729421399994,11.6,10.331101392));
#225507=CARTESIAN_POINT('Ctrl Pts',(1.18729900199994,15.2,10.332226781));
#225508=CARTESIAN_POINT('Ctrl Pts',(1.18729900199994,11.6,10.332226781));
#225509=CARTESIAN_POINT('Ctrl Pts',(1.18730271099994,15.2,10.333361172));
#225510=CARTESIAN_POINT('Ctrl Pts',(1.18730271099994,11.6,10.333361172));
#225511=CARTESIAN_POINT('Ctrl Pts',(1.18730532599994,15.2,10.334504539));
#225512=CARTESIAN_POINT('Ctrl Pts',(1.18730532599994,11.6,10.334504539));
#225513=CARTESIAN_POINT('Ctrl Pts',(1.18730682999994,15.2,10.335656861));
#225514=CARTESIAN_POINT('Ctrl Pts',(1.18730682999994,11.6,10.335656861));
#225515=CARTESIAN_POINT('Ctrl Pts',(1.18730720499994,15.2,10.336818113));
#225516=CARTESIAN_POINT('Ctrl Pts',(1.18730720499994,11.6,10.336818113));
#225517=CARTESIAN_POINT('Ctrl Pts',(1.18730643699994,15.2,10.33798827));
#225518=CARTESIAN_POINT('Ctrl Pts',(1.18730643699994,11.6,10.33798827));
#225519=CARTESIAN_POINT('Ctrl Pts',(1.18730450699994,15.2,10.339167309));
#225520=CARTESIAN_POINT('Ctrl Pts',(1.18730450699994,11.6,10.339167309));
#225521=CARTESIAN_POINT('Ctrl Pts',(1.18730140099994,15.2,10.340355206));
#225522=CARTESIAN_POINT('Ctrl Pts',(1.18730140099994,11.6,10.340355206));
#225523=CARTESIAN_POINT('Ctrl Pts',(1.18729710199994,15.2,10.341551938));
#225524=CARTESIAN_POINT('Ctrl Pts',(1.18729710199994,11.6,10.341551938));
#225525=CARTESIAN_POINT('Ctrl Pts',(1.18729159299995,15.2,10.342757482));
#225526=CARTESIAN_POINT('Ctrl Pts',(1.18729159299995,11.6,10.342757482));
#225527=CARTESIAN_POINT('Ctrl Pts',(1.18728485799994,15.2,10.343971813));
#225528=CARTESIAN_POINT('Ctrl Pts',(1.18728485799994,11.6,10.343971813));
#225529=CARTESIAN_POINT('Ctrl Pts',(1.18727688199994,15.2,10.345194909));
#225530=CARTESIAN_POINT('Ctrl Pts',(1.18727688199994,11.6,10.345194909));
#225531=CARTESIAN_POINT('Ctrl Pts',(1.18726764899994,15.2,10.346426747));
#225532=CARTESIAN_POINT('Ctrl Pts',(1.18726764899994,11.6,10.346426747));
#225533=CARTESIAN_POINT('Ctrl Pts',(1.18725714199994,15.2,10.347667304));
#225534=CARTESIAN_POINT('Ctrl Pts',(1.18725714199994,11.6,10.347667304));
#225535=CARTESIAN_POINT('Ctrl Pts',(1.18724534799994,15.2,10.348916556));
#225536=CARTESIAN_POINT('Ctrl Pts',(1.18724534799994,11.6,10.348916556));
#225537=CARTESIAN_POINT('Ctrl Pts',(1.18723224699994,15.2,10.350174481));
#225538=CARTESIAN_POINT('Ctrl Pts',(1.18723224699994,11.6,10.350174481));
#225539=CARTESIAN_POINT('Ctrl Pts',(1.18721782699994,15.2,10.351441056));
#225540=CARTESIAN_POINT('Ctrl Pts',(1.18721782699994,11.6,10.351441056));
#225541=CARTESIAN_POINT('Ctrl Pts',(1.18720207099994,15.2,10.352716258));
#225542=CARTESIAN_POINT('Ctrl Pts',(1.18720207099994,11.6,10.352716258));
#225543=CARTESIAN_POINT('Ctrl Pts',(1.18718496499994,15.2,10.354000065));
#225544=CARTESIAN_POINT('Ctrl Pts',(1.18718496499994,11.6,10.354000065));
#225545=CARTESIAN_POINT('Ctrl Pts',(1.18716649099994,15.2,10.355292454));
#225546=CARTESIAN_POINT('Ctrl Pts',(1.18716649099994,11.6,10.355292454));
#225547=CARTESIAN_POINT('Ctrl Pts',(1.18714663599994,15.2,10.356593403));
#225548=CARTESIAN_POINT('Ctrl Pts',(1.18714663599994,11.6,10.356593403));
#225549=CARTESIAN_POINT('Ctrl Pts',(1.18712538499994,15.2,10.35790289));
#225550=CARTESIAN_POINT('Ctrl Pts',(1.18712538499994,11.6,10.35790289));
#225551=CARTESIAN_POINT('Ctrl Pts',(1.18710272199994,15.2,10.359220892));
#225552=CARTESIAN_POINT('Ctrl Pts',(1.18710272199994,11.6,10.359220892));
#225553=CARTESIAN_POINT('Ctrl Pts',(1.18707863099994,15.2,10.360547387));
#225554=CARTESIAN_POINT('Ctrl Pts',(1.18707863099994,11.6,10.360547387));
#225555=CARTESIAN_POINT('Ctrl Pts',(1.18705309899994,15.2,10.361882353));
#225556=CARTESIAN_POINT('Ctrl Pts',(1.18705309899994,11.6,10.361882353));
#225557=CARTESIAN_POINT('Ctrl Pts',(1.18702610999994,15.2,10.363225769));
#225558=CARTESIAN_POINT('Ctrl Pts',(1.18702610999994,11.6,10.363225769));
#225559=CARTESIAN_POINT('Ctrl Pts',(1.18699764999994,15.2,10.364577612));
#225560=CARTESIAN_POINT('Ctrl Pts',(1.18699764999994,11.6,10.364577612));
#225561=CARTESIAN_POINT('Ctrl Pts',(1.18696770299994,15.2,10.365937861));
#225562=CARTESIAN_POINT('Ctrl Pts',(1.18696770299994,11.6,10.365937861));
#225563=CARTESIAN_POINT('Ctrl Pts',(1.18693625599994,15.2,10.367306493));
#225564=CARTESIAN_POINT('Ctrl Pts',(1.18693625599994,11.6,10.367306493));
#225565=CARTESIAN_POINT('Ctrl Pts',(1.18690329299994,15.2,10.368683488));
#225566=CARTESIAN_POINT('Ctrl Pts',(1.18690329299994,11.6,10.368683488));
#225567=CARTESIAN_POINT('Ctrl Pts',(1.18686879999994,15.2,10.370068824));
#225568=CARTESIAN_POINT('Ctrl Pts',(1.18686879999994,11.6,10.370068824));
#225569=CARTESIAN_POINT('Ctrl Pts',(1.18683276299994,15.2,10.371462478));
#225570=CARTESIAN_POINT('Ctrl Pts',(1.18683276299994,11.6,10.371462478));
#225571=CARTESIAN_POINT('Ctrl Pts',(1.18679516799994,15.2,10.372864432));
#225572=CARTESIAN_POINT('Ctrl Pts',(1.18679516799994,11.6,10.372864432));
#225573=CARTESIAN_POINT('Ctrl Pts',(1.18675599899994,15.2,10.37427466));
#225574=CARTESIAN_POINT('Ctrl Pts',(1.18675599899994,11.6,10.37427466));
#225575=CARTESIAN_POINT('Ctrl Pts',(1.18671524299994,15.2,10.375693146));
#225576=CARTESIAN_POINT('Ctrl Pts',(1.18671524299994,11.6,10.375693146));
#225577=CARTESIAN_POINT('Ctrl Pts',(1.18667288599994,15.2,10.377119865));
#225578=CARTESIAN_POINT('Ctrl Pts',(1.18667288599994,11.6,10.377119865));
#225579=CARTESIAN_POINT('Ctrl Pts',(1.18662891299994,15.2,10.378554798));
#225580=CARTESIAN_POINT('Ctrl Pts',(1.18662891299994,11.6,10.378554798));
#225581=CARTESIAN_POINT('Ctrl Pts',(1.18658331199994,15.2,10.379997924));
#225582=CARTESIAN_POINT('Ctrl Pts',(1.18658331199994,11.6,10.379997924));
#225583=CARTESIAN_POINT('Ctrl Pts',(1.18653606599994,15.2,10.38144922));
#225584=CARTESIAN_POINT('Ctrl Pts',(1.18653606599994,11.6,10.38144922));
#225585=CARTESIAN_POINT('Ctrl Pts',(1.18648716499994,15.2,10.382908668));
#225586=CARTESIAN_POINT('Ctrl Pts',(1.18648716499994,11.6,10.382908668));
#225587=CARTESIAN_POINT('Ctrl Pts',(1.18643659099994,15.2,10.384376246));
#225588=CARTESIAN_POINT('Ctrl Pts',(1.18643659099994,11.6,10.384376246));
#225589=CARTESIAN_POINT('Ctrl Pts',(1.18638433299994,15.2,10.385851932));
#225590=CARTESIAN_POINT('Ctrl Pts',(1.18638433299994,11.6,10.385851932));
#225591=CARTESIAN_POINT('Ctrl Pts',(1.18633037699994,15.2,10.387335709));
#225592=CARTESIAN_POINT('Ctrl Pts',(1.18633037699994,11.6,10.387335709));
#225593=CARTESIAN_POINT('Ctrl Pts',(1.18627470899994,15.2,10.388827552));
#225594=CARTESIAN_POINT('Ctrl Pts',(1.18627470899994,11.6,10.388827552));
#225595=CARTESIAN_POINT('Ctrl Pts',(1.18621731499994,15.2,10.390327445));
#225596=CARTESIAN_POINT('Ctrl Pts',(1.18621731499994,11.6,10.390327445));
#225597=CARTESIAN_POINT('Ctrl Pts',(1.18615818399994,15.2,10.391835364));
#225598=CARTESIAN_POINT('Ctrl Pts',(1.18615818399994,11.6,10.391835364));
#225599=CARTESIAN_POINT('Ctrl Pts',(1.18609729899994,15.2,10.393351292));
#225600=CARTESIAN_POINT('Ctrl Pts',(1.18609729899994,11.6,10.393351292));
#225601=CARTESIAN_POINT('Ctrl Pts',(1.18603464799994,15.2,10.394875207));
#225602=CARTESIAN_POINT('Ctrl Pts',(1.18603464799994,11.6,10.394875207));
#225603=CARTESIAN_POINT('Ctrl Pts',(1.18597021899994,15.2,10.396407089));
#225604=CARTESIAN_POINT('Ctrl Pts',(1.18597021899994,11.6,10.396407089));
#225605=CARTESIAN_POINT('Ctrl Pts',(1.18590399799994,15.2,10.397946917));
#225606=CARTESIAN_POINT('Ctrl Pts',(1.18590399799994,11.6,10.397946917));
#225607=CARTESIAN_POINT('Ctrl Pts',(1.18583597199994,15.2,10.399494672));
#225608=CARTESIAN_POINT('Ctrl Pts',(1.18583597199994,11.6,10.399494672));
#225609=CARTESIAN_POINT('Ctrl Pts',(1.18576612699994,15.2,10.401050336));
#225610=CARTESIAN_POINT('Ctrl Pts',(1.18576612699994,11.6,10.401050336));
#225611=CARTESIAN_POINT('Ctrl Pts',(1.18569445199994,15.2,10.402613886));
#225612=CARTESIAN_POINT('Ctrl Pts',(1.18569445199994,11.6,10.402613886));
#225613=CARTESIAN_POINT('Ctrl Pts',(1.18562093099994,15.2,10.404185304));
#225614=CARTESIAN_POINT('Ctrl Pts',(1.18562093099994,11.6,10.404185304));
#225615=CARTESIAN_POINT('Ctrl Pts',(1.18554555399994,15.2,10.405764571));
#225616=CARTESIAN_POINT('Ctrl Pts',(1.18554555399994,11.6,10.405764571));
#225617=CARTESIAN_POINT('Ctrl Pts',(1.18546830699994,15.2,10.407351665));
#225618=CARTESIAN_POINT('Ctrl Pts',(1.18546830699994,11.6,10.407351665));
#225619=CARTESIAN_POINT('Ctrl Pts',(1.18538917699994,15.2,10.408946569));
#225620=CARTESIAN_POINT('Ctrl Pts',(1.18538917699994,11.6,10.408946569));
#225621=CARTESIAN_POINT('Ctrl Pts',(1.18530815299994,15.2,10.410549261));
#225622=CARTESIAN_POINT('Ctrl Pts',(1.18530815299994,11.6,10.410549261));
#225623=CARTESIAN_POINT('Ctrl Pts',(1.18522521999994,15.2,10.412159724));
#225624=CARTESIAN_POINT('Ctrl Pts',(1.18522521999994,11.6,10.412159724));
#225625=CARTESIAN_POINT('Ctrl Pts',(1.18514036599994,15.2,10.413777937));
#225626=CARTESIAN_POINT('Ctrl Pts',(1.18514036599994,11.6,10.413777937));
#225627=CARTESIAN_POINT('Ctrl Pts',(1.18505357899994,15.2,10.415403882));
#225628=CARTESIAN_POINT('Ctrl Pts',(1.18505357899994,11.6,10.415403882));
#225629=CARTESIAN_POINT('Ctrl Pts',(1.18496484699994,15.2,10.417037539));
#225630=CARTESIAN_POINT('Ctrl Pts',(1.18496484699994,11.6,10.417037539));
#225631=CARTESIAN_POINT('Ctrl Pts',(1.18487415699994,15.2,10.418678889));
#225632=CARTESIAN_POINT('Ctrl Pts',(1.18487415699994,11.6,10.418678889));
#225633=CARTESIAN_POINT('Ctrl Pts',(1.18478149599994,15.2,10.420327914));
#225634=CARTESIAN_POINT('Ctrl Pts',(1.18478149599994,11.6,10.420327914));
#225635=CARTESIAN_POINT('Ctrl Pts',(1.18468685299994,15.2,10.421984593));
#225636=CARTESIAN_POINT('Ctrl Pts',(1.18468685299994,11.6,10.421984593));
#225637=CARTESIAN_POINT('Ctrl Pts',(1.18459021499994,15.2,10.423648908));
#225638=CARTESIAN_POINT('Ctrl Pts',(1.18459021499994,11.6,10.423648908));
#225639=CARTESIAN_POINT('Ctrl Pts',(1.18449156999994,15.2,10.42532084));
#225640=CARTESIAN_POINT('Ctrl Pts',(1.18449156999994,11.6,10.42532084));
#225641=CARTESIAN_POINT('Ctrl Pts',(1.18439090699994,15.2,10.427000372));
#225642=CARTESIAN_POINT('Ctrl Pts',(1.18439090699994,11.6,10.427000372));
#225643=CARTESIAN_POINT('Ctrl Pts',(1.18428821199994,15.2,10.428687483));
#225644=CARTESIAN_POINT('Ctrl Pts',(1.18428821199994,11.6,10.428687483));
#225645=CARTESIAN_POINT('Ctrl Pts',(1.18418347299994,15.2,10.430382155));
#225646=CARTESIAN_POINT('Ctrl Pts',(1.18418347299994,11.6,10.430382155));
#225647=CARTESIAN_POINT('Ctrl Pts',(1.18407667999994,15.2,10.432084369));
#225648=CARTESIAN_POINT('Ctrl Pts',(1.18407667999994,11.6,10.432084369));
#225649=CARTESIAN_POINT('Ctrl Pts',(1.18396781899994,15.2,10.433794108));
#225650=CARTESIAN_POINT('Ctrl Pts',(1.18396781899994,11.6,10.433794108));
#225651=CARTESIAN_POINT('Ctrl Pts',(1.18385688099994,15.2,10.435511351));
#225652=CARTESIAN_POINT('Ctrl Pts',(1.18385688099994,11.6,10.435511351));
#225653=CARTESIAN_POINT('Ctrl Pts',(1.18374385099994,15.2,10.437236081));
#225654=CARTESIAN_POINT('Ctrl Pts',(1.18374385099994,11.6,10.437236081));
#225655=CARTESIAN_POINT('Ctrl Pts',(1.18362871899994,15.2,10.438968281));
#225656=CARTESIAN_POINT('Ctrl Pts',(1.18362871899994,11.6,10.438968281));
#225657=CARTESIAN_POINT('Ctrl Pts',(1.18351147299994,15.2,10.440707931));
#225658=CARTESIAN_POINT('Ctrl Pts',(1.18351147299994,11.6,10.440707931));
#225659=CARTESIAN_POINT('Ctrl Pts',(1.18339210199994,15.2,10.442455013));
#225660=CARTESIAN_POINT('Ctrl Pts',(1.18339210199994,11.6,10.442455013));
#225661=CARTESIAN_POINT('Ctrl Pts',(1.18327059299994,15.2,10.444209509));
#225662=CARTESIAN_POINT('Ctrl Pts',(1.18327059299994,11.6,10.444209509));
#225663=CARTESIAN_POINT('Ctrl Pts',(1.18314693599994,15.2,10.445971401));
#225664=CARTESIAN_POINT('Ctrl Pts',(1.18314693599994,11.6,10.445971401));
#225665=CARTESIAN_POINT('Ctrl Pts',(1.18302111899994,15.2,10.44774067));
#225666=CARTESIAN_POINT('Ctrl Pts',(1.18302111899994,11.6,10.44774067));
#225667=CARTESIAN_POINT('Ctrl Pts',(1.18289312999994,15.2,10.4495173));
#225668=CARTESIAN_POINT('Ctrl Pts',(1.18289312999994,11.6,10.4495173));
#225669=CARTESIAN_POINT('Ctrl Pts',(1.18276295899994,15.2,10.45130127));
#225670=CARTESIAN_POINT('Ctrl Pts',(1.18276295899994,11.6,10.45130127));
#225671=CARTESIAN_POINT('Ctrl Pts',(1.18263059299994,15.2,10.453092566));
#225672=CARTESIAN_POINT('Ctrl Pts',(1.18263059299994,11.6,10.453092566));
#225673=CARTESIAN_POINT('Ctrl Pts',(1.18249602099994,15.2,10.454891167));
#225674=CARTESIAN_POINT('Ctrl Pts',(1.18249602099994,11.6,10.454891167));
#225675=CARTESIAN_POINT('Ctrl Pts',(1.18235923399994,15.2,10.456697057));
#225676=CARTESIAN_POINT('Ctrl Pts',(1.18235923399994,11.6,10.456697057));
#225677=CARTESIAN_POINT('Ctrl Pts',(1.18222021799994,15.2,10.458510218));
#225678=CARTESIAN_POINT('Ctrl Pts',(1.18222021799994,11.6,10.458510218));
#225679=CARTESIAN_POINT('Ctrl Pts',(1.18207896399994,15.2,10.460330631));
#225680=CARTESIAN_POINT('Ctrl Pts',(1.18207896399994,11.6,10.460330631));
#225681=CARTESIAN_POINT('Ctrl Pts',(1.18193546099994,15.2,10.46215828));
#225682=CARTESIAN_POINT('Ctrl Pts',(1.18193546099994,11.6,10.46215828));
#225683=CARTESIAN_POINT('Ctrl Pts',(1.18178969499994,15.2,10.463993147));
#225684=CARTESIAN_POINT('Ctrl Pts',(1.18178969499994,11.6,10.463993147));
#225685=CARTESIAN_POINT('Ctrl Pts',(1.18164165899994,15.2,10.465835214));
#225686=CARTESIAN_POINT('Ctrl Pts',(1.18164165899994,11.6,10.465835214));
#225687=CARTESIAN_POINT('Ctrl Pts',(1.18149133899994,15.2,10.467684465));
#225688=CARTESIAN_POINT('Ctrl Pts',(1.18149133899994,11.6,10.467684465));
#225689=CARTESIAN_POINT('Ctrl Pts',(1.18133872599994,15.2,10.469540881));
#225690=CARTESIAN_POINT('Ctrl Pts',(1.18133872599994,11.6,10.469540881));
#225691=CARTESIAN_POINT('Ctrl Pts',(1.18118380799994,15.2,10.471404446));
#225692=CARTESIAN_POINT('Ctrl Pts',(1.18118380799994,11.6,10.471404446));
#225693=CARTESIAN_POINT('Ctrl Pts',(1.18102657599994,15.2,10.473275141));
#225694=CARTESIAN_POINT('Ctrl Pts',(1.18102657599994,11.6,10.473275141));
#225695=CARTESIAN_POINT('Ctrl Pts',(1.18086701799994,15.2,10.475152951));
#225696=CARTESIAN_POINT('Ctrl Pts',(1.18086701799994,11.6,10.475152951));
#225697=CARTESIAN_POINT('Ctrl Pts',(1.18070512299994,15.2,10.477037857));
#225698=CARTESIAN_POINT('Ctrl Pts',(1.18070512299994,11.6,10.477037857));
#225699=CARTESIAN_POINT('Ctrl Pts',(1.18054088199994,15.2,10.478929843));
#225700=CARTESIAN_POINT('Ctrl Pts',(1.18054088199994,11.6,10.478929843));
#225701=CARTESIAN_POINT('Ctrl Pts',(1.18037428299994,15.2,10.480828891));
#225702=CARTESIAN_POINT('Ctrl Pts',(1.18037428299994,11.6,10.480828891));
#225703=CARTESIAN_POINT('Ctrl Pts',(1.18020531499994,15.2,10.482734986));
#225704=CARTESIAN_POINT('Ctrl Pts',(1.18020531499994,11.6,10.482734986));
#225705=CARTESIAN_POINT('Ctrl Pts',(1.18003396899994,15.2,10.484648108));
#225706=CARTESIAN_POINT('Ctrl Pts',(1.18003396899994,11.6,10.484648108));
#225707=CARTESIAN_POINT('Ctrl Pts',(1.17986023499994,15.2,10.486568243));
#225708=CARTESIAN_POINT('Ctrl Pts',(1.17986023499994,11.6,10.486568243));
#225709=CARTESIAN_POINT('Ctrl Pts',(1.17968410099994,15.2,10.488495372));
#225710=CARTESIAN_POINT('Ctrl Pts',(1.17968410099994,11.6,10.488495372));
#225711=CARTESIAN_POINT('Ctrl Pts',(1.17950555699994,15.2,10.49042948));
#225712=CARTESIAN_POINT('Ctrl Pts',(1.17950555699994,11.6,10.49042948));
#225713=CARTESIAN_POINT('Ctrl Pts',(1.17932459299994,15.2,10.492370549));
#225714=CARTESIAN_POINT('Ctrl Pts',(1.17932459299994,11.6,10.492370549));
#225715=CARTESIAN_POINT('Ctrl Pts',(1.17914119899994,15.2,10.494318564));
#225716=CARTESIAN_POINT('Ctrl Pts',(1.17914119899994,11.6,10.494318564));
#225717=CARTESIAN_POINT('Ctrl Pts',(1.17895536499994,15.2,10.496273505));
#225718=CARTESIAN_POINT('Ctrl Pts',(1.17895536499994,11.6,10.496273505));
#225719=CARTESIAN_POINT('Ctrl Pts',(1.17876707999994,15.2,10.498235359));
#225720=CARTESIAN_POINT('Ctrl Pts',(1.17876707999994,11.6,10.498235359));
#225721=CARTESIAN_POINT('Ctrl Pts',(1.17857633499994,15.2,10.500204107));
#225722=CARTESIAN_POINT('Ctrl Pts',(1.17857633499994,11.6,10.500204107));
#225723=CARTESIAN_POINT('Ctrl Pts',(1.17838311899994,15.2,10.502179735));
#225724=CARTESIAN_POINT('Ctrl Pts',(1.17838311899994,11.6,10.502179735));
#225725=CARTESIAN_POINT('Ctrl Pts',(1.17818742199994,15.2,10.504162224));
#225726=CARTESIAN_POINT('Ctrl Pts',(1.17818742199994,11.6,10.504162224));
#225727=CARTESIAN_POINT('Ctrl Pts',(1.17798923499994,15.2,10.50615156));
#225728=CARTESIAN_POINT('Ctrl Pts',(1.17798923499994,11.6,10.50615156));
#225729=CARTESIAN_POINT('Ctrl Pts',(1.17778854699994,15.2,10.508147724));
#225730=CARTESIAN_POINT('Ctrl Pts',(1.17778854699994,11.6,10.508147724));
#225731=CARTESIAN_POINT('Ctrl Pts',(1.17758534899994,15.2,10.510150701));
#225732=CARTESIAN_POINT('Ctrl Pts',(1.17758534899994,11.6,10.510150701));
#225733=CARTESIAN_POINT('Ctrl Pts',(1.17737963099994,15.2,10.512160476));
#225734=CARTESIAN_POINT('Ctrl Pts',(1.17737963099994,11.6,10.512160476));
#225735=CARTESIAN_POINT('Ctrl Pts',(1.17717138199994,15.2,10.514177031));
#225736=CARTESIAN_POINT('Ctrl Pts',(1.17717138199994,11.6,10.514177031));
#225737=CARTESIAN_POINT('Ctrl Pts',(1.17696059399994,15.2,10.51620035));
#225738=CARTESIAN_POINT('Ctrl Pts',(1.17696059399994,11.6,10.51620035));
#225739=CARTESIAN_POINT('Ctrl Pts',(1.17674725699994,15.2,10.518230418));
#225740=CARTESIAN_POINT('Ctrl Pts',(1.17674725699994,11.6,10.518230418));
#225741=CARTESIAN_POINT('Ctrl Pts',(1.17653135999994,15.2,10.520267219));
#225742=CARTESIAN_POINT('Ctrl Pts',(1.17653135999994,11.6,10.520267219));
#225743=CARTESIAN_POINT('Ctrl Pts',(1.17631289399994,15.2,10.522310736));
#225744=CARTESIAN_POINT('Ctrl Pts',(1.17631289399994,11.6,10.522310736));
#225745=CARTESIAN_POINT('Ctrl Pts',(1.17609184899994,15.2,10.524360953));
#225746=CARTESIAN_POINT('Ctrl Pts',(1.17609184899994,11.6,10.524360953));
#225747=CARTESIAN_POINT('Ctrl Pts',(1.17586821799994,15.2,10.526417855));
#225748=CARTESIAN_POINT('Ctrl Pts',(1.17586821799994,11.6,10.526417855));
#225749=CARTESIAN_POINT('Ctrl Pts',(1.17564198899994,15.2,10.528481426));
#225750=CARTESIAN_POINT('Ctrl Pts',(1.17564198899994,11.6,10.528481426));
#225751=CARTESIAN_POINT('Ctrl Pts',(1.17541315199994,15.2,10.530551649));
#225752=CARTESIAN_POINT('Ctrl Pts',(1.17541315199994,11.6,10.530551649));
#225753=CARTESIAN_POINT('Ctrl Pts',(1.17518169999994,15.2,10.53262851));
#225754=CARTESIAN_POINT('Ctrl Pts',(1.17518169999994,11.6,10.53262851));
#225755=CARTESIAN_POINT('Ctrl Pts',(1.17494762299994,15.2,10.534711991));
#225756=CARTESIAN_POINT('Ctrl Pts',(1.17494762299994,11.6,10.534711991));
#225757=CARTESIAN_POINT('Ctrl Pts',(1.17471090899994,15.2,10.536802079));
#225758=CARTESIAN_POINT('Ctrl Pts',(1.17471090899994,11.6,10.536802079));
#225759=CARTESIAN_POINT('Ctrl Pts',(1.17447155199994,15.2,10.538898756));
#225760=CARTESIAN_POINT('Ctrl Pts',(1.17447155199994,11.6,10.538898756));
#225761=CARTESIAN_POINT('Ctrl Pts',(1.17422954199994,15.2,10.541002008));
#225762=CARTESIAN_POINT('Ctrl Pts',(1.17422954199994,11.6,10.541002008));
#225763=CARTESIAN_POINT('Ctrl Pts',(1.17398486799994,15.2,10.543111819));
#225764=CARTESIAN_POINT('Ctrl Pts',(1.17398486799994,11.6,10.543111819));
#225765=CARTESIAN_POINT('Ctrl Pts',(1.17373752299994,15.2,10.545228173));
#225766=CARTESIAN_POINT('Ctrl Pts',(1.17373752299994,11.6,10.545228173));
#225767=CARTESIAN_POINT('Ctrl Pts',(1.17348749699994,15.2,10.547351055));
#225768=CARTESIAN_POINT('Ctrl Pts',(1.17348749699994,11.6,10.547351055));
#225769=CARTESIAN_POINT('Ctrl Pts',(1.17323478099994,15.2,10.549480449));
#225770=CARTESIAN_POINT('Ctrl Pts',(1.17323478099994,11.6,10.549480449));
#225771=CARTESIAN_POINT('Ctrl Pts',(1.17297936399994,15.2,10.551616341));
#225772=CARTESIAN_POINT('Ctrl Pts',(1.17297936399994,11.6,10.551616341));
#225773=CARTESIAN_POINT('Ctrl Pts',(1.17272123999994,15.2,10.553758715));
#225774=CARTESIAN_POINT('Ctrl Pts',(1.17272123999994,11.6,10.553758715));
#225775=CARTESIAN_POINT('Ctrl Pts',(1.17246039899994,15.2,10.555907554));
#225776=CARTESIAN_POINT('Ctrl Pts',(1.17246039899994,11.6,10.555907554));
#225777=CARTESIAN_POINT('Ctrl Pts',(1.17219683199994,15.2,10.558062846));
#225778=CARTESIAN_POINT('Ctrl Pts',(1.17219683199994,11.6,10.558062846));
#225779=CARTESIAN_POINT('Ctrl Pts',(1.17193052999994,15.2,10.560224573));
#225780=CARTESIAN_POINT('Ctrl Pts',(1.17193052999994,11.6,10.560224573));
#225781=CARTESIAN_POINT('Ctrl Pts',(1.17166148399994,15.2,10.562392721));
#225782=CARTESIAN_POINT('Ctrl Pts',(1.17166148399994,11.6,10.562392721));
#225783=CARTESIAN_POINT('Ctrl Pts',(1.17138968499995,15.2,10.564567275));
#225784=CARTESIAN_POINT('Ctrl Pts',(1.17138968499995,11.6,10.564567275));
#225785=CARTESIAN_POINT('Ctrl Pts',(1.17111512399994,15.2,10.566748219));
#225786=CARTESIAN_POINT('Ctrl Pts',(1.17111512399994,11.6,10.566748219));
#225787=CARTESIAN_POINT('Ctrl Pts',(1.17083779399994,15.2,10.56893554));
#225788=CARTESIAN_POINT('Ctrl Pts',(1.17083779399994,11.6,10.56893554));
#225789=CARTESIAN_POINT('Ctrl Pts',(1.17055768399994,15.2,10.57112922));
#225790=CARTESIAN_POINT('Ctrl Pts',(1.17055768399994,11.6,10.57112922));
#225791=CARTESIAN_POINT('Ctrl Pts',(1.17027478699994,15.2,10.573329246));
#225792=CARTESIAN_POINT('Ctrl Pts',(1.17027478699994,11.6,10.573329246));
#225793=CARTESIAN_POINT('Ctrl Pts',(1.16998909399994,15.2,10.575535604));
#225794=CARTESIAN_POINT('Ctrl Pts',(1.16998909399994,11.6,10.575535604));
#225795=CARTESIAN_POINT('Ctrl Pts',(1.16970059499994,15.2,10.577748277));
#225796=CARTESIAN_POINT('Ctrl Pts',(1.16970059499994,11.6,10.577748277));
#225797=CARTESIAN_POINT('Ctrl Pts',(1.16940928299994,15.2,10.579967251));
#225798=CARTESIAN_POINT('Ctrl Pts',(1.16940928299994,11.6,10.579967251));
#225799=CARTESIAN_POINT('Ctrl Pts',(1.16911514899994,15.2,10.582192511));
#225800=CARTESIAN_POINT('Ctrl Pts',(1.16911514899994,11.6,10.582192511));
#225801=CARTESIAN_POINT('Ctrl Pts',(1.16881818499994,15.2,10.584424043));
#225802=CARTESIAN_POINT('Ctrl Pts',(1.16881818499994,11.6,10.584424043));
#225803=CARTESIAN_POINT('Ctrl Pts',(1.16851838099994,15.2,10.586661831));
#225804=CARTESIAN_POINT('Ctrl Pts',(1.16851838099994,11.6,10.586661831));
#225805=CARTESIAN_POINT('Ctrl Pts',(1.16821573099994,15.2,10.588905861));
#225806=CARTESIAN_POINT('Ctrl Pts',(1.16821573099994,11.6,10.588905861));
#225807=CARTESIAN_POINT('Ctrl Pts',(1.16791022399994,15.2,10.59115612));
#225808=CARTESIAN_POINT('Ctrl Pts',(1.16791022399994,11.6,10.59115612));
#225809=CARTESIAN_POINT('Ctrl Pts',(1.16760185299994,15.2,10.59341259));
#225810=CARTESIAN_POINT('Ctrl Pts',(1.16760185299994,11.6,10.59341259));
#225811=CARTESIAN_POINT('Ctrl Pts',(1.16729060999994,15.2,10.595675259));
#225812=CARTESIAN_POINT('Ctrl Pts',(1.16729060999994,11.6,10.595675259));
#225813=CARTESIAN_POINT('Ctrl Pts',(1.16697648499994,15.2,10.597944112));
#225814=CARTESIAN_POINT('Ctrl Pts',(1.16697648499994,11.6,10.597944112));
#225815=CARTESIAN_POINT('Ctrl Pts',(1.16665947299994,15.2,10.600219134));
#225816=CARTESIAN_POINT('Ctrl Pts',(1.16665947299994,11.6,10.600219134));
#225817=CARTESIAN_POINT('Ctrl Pts',(1.16633956199994,15.2,10.602500311));
#225818=CARTESIAN_POINT('Ctrl Pts',(1.16633956199994,11.6,10.602500311));
#225819=CARTESIAN_POINT('Ctrl Pts',(1.16601674699994,15.2,10.604787627));
#225820=CARTESIAN_POINT('Ctrl Pts',(1.16601674699994,11.6,10.604787627));
#225821=CARTESIAN_POINT('Ctrl Pts',(1.16569101699994,15.2,10.60708107));
#225822=CARTESIAN_POINT('Ctrl Pts',(1.16569101699994,11.6,10.60708107));
#225823=CARTESIAN_POINT('Ctrl Pts',(1.16536236599994,15.2,10.609380625));
#225824=CARTESIAN_POINT('Ctrl Pts',(1.16536236599994,11.6,10.609380625));
#225825=CARTESIAN_POINT('Ctrl Pts',(1.16503078499994,15.2,10.611686276));
#225826=CARTESIAN_POINT('Ctrl Pts',(1.16503078499994,11.6,10.611686276));
#225827=CARTESIAN_POINT('Ctrl Pts',(1.16469626699994,15.2,10.61399801));
#225828=CARTESIAN_POINT('Ctrl Pts',(1.16469626699994,11.6,10.61399801));
#225829=CARTESIAN_POINT('Ctrl Pts',(1.16435880199994,15.2,10.616315815));
#225830=CARTESIAN_POINT('Ctrl Pts',(1.16435880199994,11.6,10.616315815));
#225831=CARTESIAN_POINT('Ctrl Pts',(1.16401838399994,15.2,10.618639673));
#225832=CARTESIAN_POINT('Ctrl Pts',(1.16401838399994,11.6,10.618639673));
#225833=CARTESIAN_POINT('Ctrl Pts',(1.16367500499994,15.2,10.620969571));
#225834=CARTESIAN_POINT('Ctrl Pts',(1.16367500499994,11.6,10.620969571));
#225835=CARTESIAN_POINT('Ctrl Pts',(1.16332865499994,15.2,10.623305496));
#225836=CARTESIAN_POINT('Ctrl Pts',(1.16332865499994,11.6,10.623305496));
#225837=CARTESIAN_POINT('Ctrl Pts',(1.16297932699994,15.2,10.625647434));
#225838=CARTESIAN_POINT('Ctrl Pts',(1.16297932699994,11.6,10.625647434));
#225839=CARTESIAN_POINT('Ctrl Pts',(1.16262701499994,15.2,10.627995369));
#225840=CARTESIAN_POINT('Ctrl Pts',(1.16262701499994,11.6,10.627995369));
#225841=CARTESIAN_POINT('Ctrl Pts',(1.16227170899994,15.2,10.630349289));
#225842=CARTESIAN_POINT('Ctrl Pts',(1.16227170899994,11.6,10.630349289));
#225843=CARTESIAN_POINT('Ctrl Pts',(1.16191340199994,15.2,10.632709178));
#225844=CARTESIAN_POINT('Ctrl Pts',(1.16191340199994,11.6,10.632709178));
#225845=CARTESIAN_POINT('Ctrl Pts',(1.16155208699994,15.2,10.635075024));
#225846=CARTESIAN_POINT('Ctrl Pts',(1.16155208699994,11.6,10.635075024));
#225847=CARTESIAN_POINT('Ctrl Pts',(1.16118775499994,15.2,10.637446813));
#225848=CARTESIAN_POINT('Ctrl Pts',(1.16118775499994,11.6,10.637446813));
#225849=CARTESIAN_POINT('Ctrl Pts',(1.16082039799994,15.2,10.639824529));
#225850=CARTESIAN_POINT('Ctrl Pts',(1.16082039799994,11.6,10.639824529));
#225851=CARTESIAN_POINT('Ctrl Pts',(1.16045000999994,15.2,10.642208161));
#225852=CARTESIAN_POINT('Ctrl Pts',(1.16045000999994,11.6,10.642208161));
#225853=CARTESIAN_POINT('Ctrl Pts',(1.16007658299994,15.2,10.644597693));
#225854=CARTESIAN_POINT('Ctrl Pts',(1.16007658299994,11.6,10.644597693));
#225855=CARTESIAN_POINT('Ctrl Pts',(1.15970010799994,15.2,10.646993112));
#225856=CARTESIAN_POINT('Ctrl Pts',(1.15970010799994,11.6,10.646993112));
#225857=CARTESIAN_POINT('Ctrl Pts',(1.15932057899994,15.2,10.649394405));
#225858=CARTESIAN_POINT('Ctrl Pts',(1.15932057899994,11.6,10.649394405));
#225859=CARTESIAN_POINT('Ctrl Pts',(1.15893798699994,15.2,10.651801557));
#225860=CARTESIAN_POINT('Ctrl Pts',(1.15893798699994,11.6,10.651801557));
#225861=CARTESIAN_POINT('Ctrl Pts',(1.15855232599994,15.2,10.654214555));
#225862=CARTESIAN_POINT('Ctrl Pts',(1.15855232599994,11.6,10.654214555));
#225863=CARTESIAN_POINT('Ctrl Pts',(1.15816358799994,15.2,10.656633385));
#225864=CARTESIAN_POINT('Ctrl Pts',(1.15816358799994,11.6,10.656633385));
#225865=CARTESIAN_POINT('Ctrl Pts',(1.15777176599994,15.2,10.659058034));
#225866=CARTESIAN_POINT('Ctrl Pts',(1.15777176599994,11.6,10.659058034));
#225867=CARTESIAN_POINT('Ctrl Pts',(1.15737685099994,15.2,10.661488488));
#225868=CARTESIAN_POINT('Ctrl Pts',(1.15737685099994,11.6,10.661488488));
#225869=CARTESIAN_POINT('Ctrl Pts',(1.15697883699994,15.2,10.663924734));
#225870=CARTESIAN_POINT('Ctrl Pts',(1.15697883699994,11.6,10.663924734));
#225871=CARTESIAN_POINT('Ctrl Pts',(1.15657771599994,15.2,10.666366756));
#225872=CARTESIAN_POINT('Ctrl Pts',(1.15657771599994,11.6,10.666366756));
#225873=CARTESIAN_POINT('Ctrl Pts',(1.15617348099994,15.2,10.668814545));
#225874=CARTESIAN_POINT('Ctrl Pts',(1.15617348099994,11.6,10.668814545));
#225875=CARTESIAN_POINT('Ctrl Pts',(1.15576612399995,15.2,10.671268084));
#225876=CARTESIAN_POINT('Ctrl Pts',(1.15576612399995,11.6,10.671268084));
#225877=CARTESIAN_POINT('Ctrl Pts',(1.15535563899994,15.2,10.67372736));
#225878=CARTESIAN_POINT('Ctrl Pts',(1.15535563899994,11.6,10.67372736));
#225879=CARTESIAN_POINT('Ctrl Pts',(1.15494201899994,15.2,10.676192361));
#225880=CARTESIAN_POINT('Ctrl Pts',(1.15494201899994,11.6,10.676192361));
#225881=CARTESIAN_POINT('Ctrl Pts',(1.15452525499994,15.2,10.678663074));
#225882=CARTESIAN_POINT('Ctrl Pts',(1.15452525499994,11.6,10.678663074));
#225883=CARTESIAN_POINT('Ctrl Pts',(1.15410534099994,15.2,10.681139484));
#225884=CARTESIAN_POINT('Ctrl Pts',(1.15410534099994,11.6,10.681139484));
#225885=CARTESIAN_POINT('Ctrl Pts',(1.15368226999994,15.2,10.683621578));
#225886=CARTESIAN_POINT('Ctrl Pts',(1.15368226999994,11.6,10.683621578));
#225887=CARTESIAN_POINT('Ctrl Pts',(1.15325603399994,15.2,10.686109343));
#225888=CARTESIAN_POINT('Ctrl Pts',(1.15325603399994,11.6,10.686109343));
#225889=CARTESIAN_POINT('Ctrl Pts',(1.15282662699994,15.2,10.688602766));
#225890=CARTESIAN_POINT('Ctrl Pts',(1.15282662699994,11.6,10.688602766));
#225891=CARTESIAN_POINT('Ctrl Pts',(1.15239403999994,15.2,10.691101834));
#225892=CARTESIAN_POINT('Ctrl Pts',(1.15239403999994,11.6,10.691101834));
#225893=CARTESIAN_POINT('Ctrl Pts',(1.15195826899994,15.2,10.693606533));
#225894=CARTESIAN_POINT('Ctrl Pts',(1.15195826899994,11.6,10.693606533));
#225895=CARTESIAN_POINT('Ctrl Pts',(1.15151930399994,15.2,10.696116851));
#225896=CARTESIAN_POINT('Ctrl Pts',(1.15151930399994,11.6,10.696116851));
#225897=CARTESIAN_POINT('Ctrl Pts',(1.15107714099994,15.2,10.698632774));
#225898=CARTESIAN_POINT('Ctrl Pts',(1.15107714099994,11.6,10.698632774));
#225899=CARTESIAN_POINT('Ctrl Pts',(1.15063176999994,15.2,10.701154289));
#225900=CARTESIAN_POINT('Ctrl Pts',(1.15063176999994,11.6,10.701154289));
#225901=CARTESIAN_POINT('Ctrl Pts',(1.15018318599994,15.2,10.703681383));
#225902=CARTESIAN_POINT('Ctrl Pts',(1.15018318599994,11.6,10.703681383));
#225903=CARTESIAN_POINT('Ctrl Pts',(1.14973138199994,15.2,10.706214044));
#225904=CARTESIAN_POINT('Ctrl Pts',(1.14973138199994,11.6,10.706214044));
#225905=CARTESIAN_POINT('Ctrl Pts',(1.14927634999994,15.2,10.708752258));
#225906=CARTESIAN_POINT('Ctrl Pts',(1.14927634999994,11.6,10.708752258));
#225907=CARTESIAN_POINT('Ctrl Pts',(1.14881808499994,15.2,10.711296011));
#225908=CARTESIAN_POINT('Ctrl Pts',(1.14881808499994,11.6,10.711296011));
#225909=CARTESIAN_POINT('Ctrl Pts',(1.14835657799994,15.2,10.713845293));
#225910=CARTESIAN_POINT('Ctrl Pts',(1.14835657799994,11.6,10.713845293));
#225911=CARTESIAN_POINT('Ctrl Pts',(1.14789182399994,15.2,10.716400089));
#225912=CARTESIAN_POINT('Ctrl Pts',(1.14789182399994,11.6,10.716400089));
#225913=CARTESIAN_POINT('Ctrl Pts',(1.14742381599994,15.2,10.718960386));
#225914=CARTESIAN_POINT('Ctrl Pts',(1.14742381599994,11.6,10.718960386));
#225915=CARTESIAN_POINT('Ctrl Pts',(1.14695254499994,15.2,10.721526172));
#225916=CARTESIAN_POINT('Ctrl Pts',(1.14695254499994,11.6,10.721526172));
#225917=CARTESIAN_POINT('Ctrl Pts',(1.14647800799994,15.2,10.724097434));
#225918=CARTESIAN_POINT('Ctrl Pts',(1.14647800799994,11.6,10.724097434));
#225919=CARTESIAN_POINT('Ctrl Pts',(1.14600019599994,15.2,10.726674159));
#225920=CARTESIAN_POINT('Ctrl Pts',(1.14600019599994,11.6,10.726674159));
#225921=CARTESIAN_POINT('Ctrl Pts',(1.14551910299994,15.2,10.729256335));
#225922=CARTESIAN_POINT('Ctrl Pts',(1.14551910299994,11.6,10.729256335));
#225923=CARTESIAN_POINT('Ctrl Pts',(1.14503472199994,15.2,10.731843948));
#225924=CARTESIAN_POINT('Ctrl Pts',(1.14503472199994,11.6,10.731843948));
#225925=CARTESIAN_POINT('Ctrl Pts',(1.14454704599994,15.2,10.734436985));
#225926=CARTESIAN_POINT('Ctrl Pts',(1.14454704599994,11.6,10.734436985));
#225927=CARTESIAN_POINT('Ctrl Pts',(1.14405606999994,15.2,10.737035436));
#225928=CARTESIAN_POINT('Ctrl Pts',(1.14405606999994,11.6,10.737035436));
#225929=CARTESIAN_POINT('Ctrl Pts',(1.14356178599994,15.2,10.739639287));
#225930=CARTESIAN_POINT('Ctrl Pts',(1.14356178599994,11.6,10.739639287));
#225931=CARTESIAN_POINT('Ctrl Pts',(1.14306418799994,15.2,10.742248524));
#225932=CARTESIAN_POINT('Ctrl Pts',(1.14306418799994,11.6,10.742248524));
#225933=CARTESIAN_POINT('Ctrl Pts',(1.14256327099994,15.2,10.744863136));
#225934=CARTESIAN_POINT('Ctrl Pts',(1.14256327099994,11.6,10.744863136));
#225935=CARTESIAN_POINT('Ctrl Pts',(1.14205902599994,15.2,10.74748311));
#225936=CARTESIAN_POINT('Ctrl Pts',(1.14205902599994,11.6,10.74748311));
#225937=CARTESIAN_POINT('Ctrl Pts',(1.14155144699994,15.2,10.750108434));
#225938=CARTESIAN_POINT('Ctrl Pts',(1.14155144699994,11.6,10.750108434));
#225939=CARTESIAN_POINT('Ctrl Pts',(1.14104052899994,15.2,10.752739094));
#225940=CARTESIAN_POINT('Ctrl Pts',(1.14104052899994,11.6,10.752739094));
#225941=CARTESIAN_POINT('Ctrl Pts',(1.14052626499994,15.2,10.755375079));
#225942=CARTESIAN_POINT('Ctrl Pts',(1.14052626499994,11.6,10.755375079));
#225943=CARTESIAN_POINT('Ctrl Pts',(1.14000864799994,15.2,10.758016376));
#225944=CARTESIAN_POINT('Ctrl Pts',(1.14000864799994,11.6,10.758016376));
#225945=CARTESIAN_POINT('Ctrl Pts',(1.13948767199994,15.2,10.760662973));
#225946=CARTESIAN_POINT('Ctrl Pts',(1.13948767199994,11.6,10.760662973));
#225947=CARTESIAN_POINT('Ctrl Pts',(1.13896333099994,15.2,10.763314857));
#225948=CARTESIAN_POINT('Ctrl Pts',(1.13896333099994,11.6,10.763314857));
#225949=CARTESIAN_POINT('Ctrl Pts',(1.13843561899994,15.2,10.765972015));
#225950=CARTESIAN_POINT('Ctrl Pts',(1.13843561899994,11.6,10.765972015));
#225951=CARTESIAN_POINT('Ctrl Pts',(1.13790452899994,15.2,10.768634437));
#225952=CARTESIAN_POINT('Ctrl Pts',(1.13790452899994,11.6,10.768634437));
#225953=CARTESIAN_POINT('Ctrl Pts',(1.13737005499994,15.2,10.771302109));
#225954=CARTESIAN_POINT('Ctrl Pts',(1.13737005499994,11.6,10.771302109));
#225955=CARTESIAN_POINT('Ctrl Pts',(1.13683219099994,15.2,10.773975018));
#225956=CARTESIAN_POINT('Ctrl Pts',(1.13683219099994,11.6,10.773975018));
#225957=CARTESIAN_POINT('Ctrl Pts',(1.13629093099994,15.2,10.776653154));
#225958=CARTESIAN_POINT('Ctrl Pts',(1.13629093099994,11.6,10.776653154));
#225959=CARTESIAN_POINT('Ctrl Pts',(1.13574626799994,15.2,10.779336503));
#225960=CARTESIAN_POINT('Ctrl Pts',(1.13574626799994,11.6,10.779336503));
#225961=CARTESIAN_POINT('Ctrl Pts',(1.13519819699994,15.2,10.782025053));
#225962=CARTESIAN_POINT('Ctrl Pts',(1.13519819699994,11.6,10.782025053));
#225963=CARTESIAN_POINT('Ctrl Pts',(1.13464671099994,15.2,10.784718793));
#225964=CARTESIAN_POINT('Ctrl Pts',(1.13464671099994,11.6,10.784718793));
#225965=CARTESIAN_POINT('Ctrl Pts',(1.13409180399994,15.2,10.787417709));
#225966=CARTESIAN_POINT('Ctrl Pts',(1.13409180399994,11.6,10.787417709));
#225967=CARTESIAN_POINT('Ctrl Pts',(1.13353346999994,15.2,10.790121791));
#225968=CARTESIAN_POINT('Ctrl Pts',(1.13353346999994,11.6,10.790121791));
#225969=CARTESIAN_POINT('Ctrl Pts',(1.13297170399994,15.2,10.792831025));
#225970=CARTESIAN_POINT('Ctrl Pts',(1.13297170399994,11.6,10.792831025));
#225971=CARTESIAN_POINT('Ctrl Pts',(1.13240649799994,15.2,10.7955454));
#225972=CARTESIAN_POINT('Ctrl Pts',(1.13240649799994,11.6,10.7955454));
#225973=CARTESIAN_POINT('Ctrl Pts',(1.13183784799994,15.2,10.798264905));
#225974=CARTESIAN_POINT('Ctrl Pts',(1.13183784799994,11.6,10.798264905));
#225975=CARTESIAN_POINT('Ctrl Pts',(1.13126574599994,15.2,10.800989525));
#225976=CARTESIAN_POINT('Ctrl Pts',(1.13126574599994,11.6,10.800989525));
#225977=CARTESIAN_POINT('Ctrl Pts',(1.13069018799994,15.2,10.803719251));
#225978=CARTESIAN_POINT('Ctrl Pts',(1.13069018799994,11.6,10.803719251));
#225979=CARTESIAN_POINT('Ctrl Pts',(1.13011116699994,15.2,10.806454068));
#225980=CARTESIAN_POINT('Ctrl Pts',(1.13011116699994,11.6,10.806454068));
#225981=CARTESIAN_POINT('Ctrl Pts',(1.12952867699994,15.2,10.809193967));
#225982=CARTESIAN_POINT('Ctrl Pts',(1.12952867699994,11.6,10.809193967));
#225983=CARTESIAN_POINT('Ctrl Pts',(1.12894271299994,15.2,10.811938934));
#225984=CARTESIAN_POINT('Ctrl Pts',(1.12894271299994,11.6,10.811938934));
#225985=CARTESIAN_POINT('Ctrl Pts',(1.12835326899994,15.2,10.814688958));
#225986=CARTESIAN_POINT('Ctrl Pts',(1.12835326899994,11.6,10.814688958));
#225987=CARTESIAN_POINT('Ctrl Pts',(1.12776033799994,15.2,10.817444028));
#225988=CARTESIAN_POINT('Ctrl Pts',(1.12776033799994,11.6,10.817444028));
#225989=CARTESIAN_POINT('Ctrl Pts',(1.12716391599994,15.2,10.820204131));
#225990=CARTESIAN_POINT('Ctrl Pts',(1.12716391599994,11.6,10.820204131));
#225991=CARTESIAN_POINT('Ctrl Pts',(1.12656399599994,15.2,10.822969256));
#225992=CARTESIAN_POINT('Ctrl Pts',(1.12656399599994,11.6,10.822969256));
#225993=CARTESIAN_POINT('Ctrl Pts',(1.12596057199994,15.2,10.825739389));
#225994=CARTESIAN_POINT('Ctrl Pts',(1.12596057199994,11.6,10.825739389));
#225995=CARTESIAN_POINT('Ctrl Pts',(1.12535363899994,15.2,10.828514521));
#225996=CARTESIAN_POINT('Ctrl Pts',(1.12535363899994,11.6,10.828514521));
#225997=CARTESIAN_POINT('Ctrl Pts',(1.12474319099995,15.2,10.831294639));
#225998=CARTESIAN_POINT('Ctrl Pts',(1.12474319099995,11.6,10.831294639));
#225999=CARTESIAN_POINT('Ctrl Pts',(1.12412922199994,15.2,10.834079731));
#226000=CARTESIAN_POINT('Ctrl Pts',(1.12412922199994,11.6,10.834079731));
#226001=CARTESIAN_POINT('Ctrl Pts',(1.12351172699994,15.2,10.836869786));
#226002=CARTESIAN_POINT('Ctrl Pts',(1.12351172699994,11.6,10.836869786));
#226003=CARTESIAN_POINT('Ctrl Pts',(1.12289069999994,15.2,10.839664792));
#226004=CARTESIAN_POINT('Ctrl Pts',(1.12289069999994,11.6,10.839664792));
#226005=CARTESIAN_POINT('Ctrl Pts',(1.12226613599994,15.2,10.842464738));
#226006=CARTESIAN_POINT('Ctrl Pts',(1.12226613599994,11.6,10.842464738));
#226007=CARTESIAN_POINT('Ctrl Pts',(1.12163802699994,15.2,10.84526961));
#226008=CARTESIAN_POINT('Ctrl Pts',(1.12163802699994,11.6,10.84526961));
#226009=CARTESIAN_POINT('Ctrl Pts',(1.12100637099994,15.2,10.848079399));
#226010=CARTESIAN_POINT('Ctrl Pts',(1.12100637099994,11.6,10.848079399));
#226011=CARTESIAN_POINT('Ctrl Pts',(1.12037115999994,15.2,10.850894093));
#226012=CARTESIAN_POINT('Ctrl Pts',(1.12037115999994,11.6,10.850894093));
#226013=CARTESIAN_POINT('Ctrl Pts',(1.11973238899994,15.2,10.85371368));
#226014=CARTESIAN_POINT('Ctrl Pts',(1.11973238899994,11.6,10.85371368));
#226015=CARTESIAN_POINT('Ctrl Pts',(1.11909005399994,15.2,10.856538148));
#226016=CARTESIAN_POINT('Ctrl Pts',(1.11909005399994,11.6,10.856538148));
#226017=CARTESIAN_POINT('Ctrl Pts',(1.11844414599994,15.2,10.859367487));
#226018=CARTESIAN_POINT('Ctrl Pts',(1.11844414599994,11.6,10.859367487));
#226019=CARTESIAN_POINT('Ctrl Pts',(1.11779466299994,15.2,10.862201683));
#226020=CARTESIAN_POINT('Ctrl Pts',(1.11779466299994,11.6,10.862201683));
#226021=CARTESIAN_POINT('Ctrl Pts',(1.11714159699994,15.2,10.865040727));
#226022=CARTESIAN_POINT('Ctrl Pts',(1.11714159699994,11.6,10.865040727));
#226023=CARTESIAN_POINT('Ctrl Pts',(1.11648494499994,15.2,10.867884606));
#226024=CARTESIAN_POINT('Ctrl Pts',(1.11648494499994,11.6,10.867884606));
#226025=CARTESIAN_POINT('Ctrl Pts',(1.11582469999994,15.2,10.870733309));
#226026=CARTESIAN_POINT('Ctrl Pts',(1.11582469999994,11.6,10.870733309));
#226027=CARTESIAN_POINT('Ctrl Pts',(1.11516085699994,15.2,10.873586825));
#226028=CARTESIAN_POINT('Ctrl Pts',(1.11516085699994,11.6,10.873586825));
#226029=CARTESIAN_POINT('Ctrl Pts',(1.11449341099994,15.2,10.876445142));
#226030=CARTESIAN_POINT('Ctrl Pts',(1.11449341099994,11.6,10.876445142));
#226031=CARTESIAN_POINT('Ctrl Pts',(1.11382235499994,15.2,10.879308249));
#226032=CARTESIAN_POINT('Ctrl Pts',(1.11382235499994,11.6,10.879308249));
#226033=CARTESIAN_POINT('Ctrl Pts',(1.11314768699994,15.2,10.882176136));
#226034=CARTESIAN_POINT('Ctrl Pts',(1.11314768699994,11.6,10.882176136));
#226035=CARTESIAN_POINT('Ctrl Pts',(1.11246939799994,15.2,10.885048788));
#226036=CARTESIAN_POINT('Ctrl Pts',(1.11246939799994,11.6,10.885048788));
#226037=CARTESIAN_POINT('Ctrl Pts',(1.11178748599994,15.2,10.887926198));
#226038=CARTESIAN_POINT('Ctrl Pts',(1.11178748599994,11.6,10.887926198));
#226039=CARTESIAN_POINT('Ctrl Pts',(1.11110194299994,15.2,10.890808352));
#226040=CARTESIAN_POINT('Ctrl Pts',(1.11110194299994,11.6,10.890808352));
#226041=CARTESIAN_POINT('Ctrl Pts',(1.11041276399995,15.2,10.89369524));
#226042=CARTESIAN_POINT('Ctrl Pts',(1.11041276399995,11.6,10.89369524));
#226043=CARTESIAN_POINT('Ctrl Pts',(1.10971994499994,15.2,10.89658685));
#226044=CARTESIAN_POINT('Ctrl Pts',(1.10971994499994,11.6,10.89658685));
#226045=CARTESIAN_POINT('Ctrl Pts',(1.10902348199994,15.2,10.899483171));
#226046=CARTESIAN_POINT('Ctrl Pts',(1.10902348199994,11.6,10.899483171));
#226047=CARTESIAN_POINT('Ctrl Pts',(1.10832336799994,15.2,10.902384192));
#226048=CARTESIAN_POINT('Ctrl Pts',(1.10832336799994,11.6,10.902384192));
#226049=CARTESIAN_POINT('Ctrl Pts',(1.10761959699994,15.2,10.905289901));
#226050=CARTESIAN_POINT('Ctrl Pts',(1.10761959699994,11.6,10.905289901));
#226051=CARTESIAN_POINT('Ctrl Pts',(1.10691216499994,15.2,10.908200289));
#226052=CARTESIAN_POINT('Ctrl Pts',(1.10691216499994,11.6,10.908200289));
#226053=CARTESIAN_POINT('Ctrl Pts',(1.10620106799994,15.2,10.911115343));
#226054=CARTESIAN_POINT('Ctrl Pts',(1.10620106799994,11.6,10.911115343));
#226055=CARTESIAN_POINT('Ctrl Pts',(1.10548629899994,15.2,10.914035053));
#226056=CARTESIAN_POINT('Ctrl Pts',(1.10548629899994,11.6,10.914035053));
#226057=CARTESIAN_POINT('Ctrl Pts',(1.10476785399995,15.2,10.916959407));
#226058=CARTESIAN_POINT('Ctrl Pts',(1.10476785399995,11.6,10.916959407));
#226059=CARTESIAN_POINT('Ctrl Pts',(1.10404572799994,15.2,10.919888394));
#226060=CARTESIAN_POINT('Ctrl Pts',(1.10404572799994,11.6,10.919888394));
#226061=CARTESIAN_POINT('Ctrl Pts',(1.10331991399994,15.2,10.922822003));
#226062=CARTESIAN_POINT('Ctrl Pts',(1.10331991399994,11.6,10.922822003));
#226063=CARTESIAN_POINT('Ctrl Pts',(1.10259040999994,15.2,10.925760224));
#226064=CARTESIAN_POINT('Ctrl Pts',(1.10259040999994,11.6,10.925760224));
#226065=CARTESIAN_POINT('Ctrl Pts',(1.10185720999994,15.2,10.928703045));
#226066=CARTESIAN_POINT('Ctrl Pts',(1.10185720999994,11.6,10.928703045));
#226067=CARTESIAN_POINT('Ctrl Pts',(1.10112030699994,15.2,10.931650455));
#226068=CARTESIAN_POINT('Ctrl Pts',(1.10112030699994,11.6,10.931650455));
#226069=CARTESIAN_POINT('Ctrl Pts',(1.10037969999994,15.2,10.934602444));
#226070=CARTESIAN_POINT('Ctrl Pts',(1.10037969999994,11.6,10.934602444));
#226071=CARTESIAN_POINT('Ctrl Pts',(1.09963537999994,15.2,10.937559));
#226072=CARTESIAN_POINT('Ctrl Pts',(1.09963537999994,11.6,10.937559));
#226073=CARTESIAN_POINT('Ctrl Pts',(1.09888734499994,15.2,10.940520113));
#226074=CARTESIAN_POINT('Ctrl Pts',(1.09888734499994,11.6,10.940520113));
#226075=CARTESIAN_POINT('Ctrl Pts',(1.09813558699994,15.2,10.943485772));
#226076=CARTESIAN_POINT('Ctrl Pts',(1.09813558699994,11.6,10.943485772));
#226077=CARTESIAN_POINT('Ctrl Pts',(1.09738010399994,15.2,10.946455965));
#226078=CARTESIAN_POINT('Ctrl Pts',(1.09738010399994,11.6,10.946455965));
#226079=CARTESIAN_POINT('Ctrl Pts',(1.09662089099994,15.2,10.949430682));
#226080=CARTESIAN_POINT('Ctrl Pts',(1.09662089099994,11.6,10.949430682));
#226081=CARTESIAN_POINT('Ctrl Pts',(1.09585794199994,15.2,10.952409912));
#226082=CARTESIAN_POINT('Ctrl Pts',(1.09585794199994,11.6,10.952409912));
#226083=CARTESIAN_POINT('Ctrl Pts',(1.09509125199994,15.2,10.955393644));
#226084=CARTESIAN_POINT('Ctrl Pts',(1.09509125199994,11.6,10.955393644));
#226085=CARTESIAN_POINT('Ctrl Pts',(1.09432081599994,15.2,10.958381869));
#226086=CARTESIAN_POINT('Ctrl Pts',(1.09432081599994,11.6,10.958381869));
#226087=CARTESIAN_POINT('Ctrl Pts',(1.09354663099994,15.2,10.961374573));
#226088=CARTESIAN_POINT('Ctrl Pts',(1.09354663099994,11.6,10.961374573));
#226089=CARTESIAN_POINT('Ctrl Pts',(1.09276869099994,15.2,10.964371748));
#226090=CARTESIAN_POINT('Ctrl Pts',(1.09276869099994,11.6,10.964371748));
#226091=CARTESIAN_POINT('Ctrl Pts',(1.09198699099994,15.2,10.967373382));
#226092=CARTESIAN_POINT('Ctrl Pts',(1.09198699099994,11.6,10.967373382));
#226093=CARTESIAN_POINT('Ctrl Pts',(1.09120152699994,15.2,10.970379465));
#226094=CARTESIAN_POINT('Ctrl Pts',(1.09120152699994,11.6,10.970379465));
#226095=CARTESIAN_POINT('Ctrl Pts',(1.09041229399994,15.2,10.973389986));
#226096=CARTESIAN_POINT('Ctrl Pts',(1.09041229399994,11.6,10.973389986));
#226097=CARTESIAN_POINT('Ctrl Pts',(1.08961928699994,15.2,10.976404933));
#226098=CARTESIAN_POINT('Ctrl Pts',(1.08961928699994,11.6,10.976404933));
#226099=CARTESIAN_POINT('Ctrl Pts',(1.08882250299994,15.2,10.979424298));
#226100=CARTESIAN_POINT('Ctrl Pts',(1.08882250299994,11.6,10.979424298));
#226101=CARTESIAN_POINT('Ctrl Pts',(1.08802193399994,15.2,10.982448068));
#226102=CARTESIAN_POINT('Ctrl Pts',(1.08802193399994,11.6,10.982448068));
#226103=CARTESIAN_POINT('Ctrl Pts',(1.08721757799994,15.2,10.985476233));
#226104=CARTESIAN_POINT('Ctrl Pts',(1.08721757799994,11.6,10.985476233));
#226105=CARTESIAN_POINT('Ctrl Pts',(1.08640942899994,15.2,10.988508784));
#226106=CARTESIAN_POINT('Ctrl Pts',(1.08640942899994,11.6,10.988508784));
#226107=CARTESIAN_POINT('Ctrl Pts',(1.08559748399994,15.2,10.991545709));
#226108=CARTESIAN_POINT('Ctrl Pts',(1.08559748399994,11.6,10.991545709));
#226109=CARTESIAN_POINT('Ctrl Pts',(1.08478173699994,15.2,10.994586997));
#226110=CARTESIAN_POINT('Ctrl Pts',(1.08478173699994,11.6,10.994586997));
#226111=CARTESIAN_POINT('Ctrl Pts',(1.08396218399994,15.2,10.997632638));
#226112=CARTESIAN_POINT('Ctrl Pts',(1.08396218399994,11.6,10.997632638));
#226113=CARTESIAN_POINT('Ctrl Pts',(1.08313882099994,15.2,11.000682622));
#226114=CARTESIAN_POINT('Ctrl Pts',(1.08313882099994,11.6,11.000682622));
#226115=CARTESIAN_POINT('Ctrl Pts',(1.08231164199994,15.2,11.003736938));
#226116=CARTESIAN_POINT('Ctrl Pts',(1.08231164199994,11.6,11.003736938));
#226117=CARTESIAN_POINT('Ctrl Pts',(1.08148064399994,15.2,11.006795575));
#226118=CARTESIAN_POINT('Ctrl Pts',(1.08148064399994,11.6,11.006795575));
#226119=CARTESIAN_POINT('Ctrl Pts',(1.08064582099994,15.2,11.009858524));
#226120=CARTESIAN_POINT('Ctrl Pts',(1.08064582099994,11.6,11.009858524));
#226121=CARTESIAN_POINT('Ctrl Pts',(1.07980716999994,15.2,11.012925773));
#226122=CARTESIAN_POINT('Ctrl Pts',(1.07980716999994,11.6,11.012925773));
#226123=CARTESIAN_POINT('Ctrl Pts',(1.07896468599994,15.2,11.015997312));
#226124=CARTESIAN_POINT('Ctrl Pts',(1.07896468599994,11.6,11.015997312));
#226125=CARTESIAN_POINT('Ctrl Pts',(1.07811836399994,15.2,11.019073132));
#226126=CARTESIAN_POINT('Ctrl Pts',(1.07811836399994,11.6,11.019073132));
#226127=CARTESIAN_POINT('Ctrl Pts',(1.07726819999994,15.2,11.022153221));
#226128=CARTESIAN_POINT('Ctrl Pts',(1.07726819999994,11.6,11.022153221));
#226129=CARTESIAN_POINT('Ctrl Pts',(1.07641418999994,15.2,11.025237569));
#226130=CARTESIAN_POINT('Ctrl Pts',(1.07641418999994,11.6,11.025237569));
#226131=CARTESIAN_POINT('Ctrl Pts',(1.07555632999994,15.2,11.028326166));
#226132=CARTESIAN_POINT('Ctrl Pts',(1.07555632999994,11.6,11.028326166));
#226133=CARTESIAN_POINT('Ctrl Pts',(1.07469461299994,15.2,11.031419001));
#226134=CARTESIAN_POINT('Ctrl Pts',(1.07469461299994,11.6,11.031419001));
#226135=CARTESIAN_POINT('Ctrl Pts',(1.07382903699994,15.2,11.034516064));
#226136=CARTESIAN_POINT('Ctrl Pts',(1.07382903699994,11.6,11.034516064));
#226137=CARTESIAN_POINT('Ctrl Pts',(1.07295959799994,15.2,11.037617346));
#226138=CARTESIAN_POINT('Ctrl Pts',(1.07295959799994,11.6,11.037617346));
#226139=CARTESIAN_POINT('Ctrl Pts',(1.07208628999994,15.2,11.040722834));
#226140=CARTESIAN_POINT('Ctrl Pts',(1.07208628999994,11.6,11.040722834));
#226141=CARTESIAN_POINT('Ctrl Pts',(1.07120910999994,15.2,11.043832521));
#226142=CARTESIAN_POINT('Ctrl Pts',(1.07120910999994,11.6,11.043832521));
#226143=CARTESIAN_POINT('Ctrl Pts',(1.07032805399994,15.2,11.046946393));
#226144=CARTESIAN_POINT('Ctrl Pts',(1.07032805399994,11.6,11.046946393));
#226145=CARTESIAN_POINT('Ctrl Pts',(1.06944311599994,15.2,11.050064443));
#226146=CARTESIAN_POINT('Ctrl Pts',(1.06944311599994,11.6,11.050064443));
#226147=CARTESIAN_POINT('Ctrl Pts',(1.06855429299994,15.2,11.05318666));
#226148=CARTESIAN_POINT('Ctrl Pts',(1.06855429299994,11.6,11.05318666));
#226149=CARTESIAN_POINT('Ctrl Pts',(1.06766158099994,15.2,11.056313033));
#226150=CARTESIAN_POINT('Ctrl Pts',(1.06766158099994,11.6,11.056313033));
#226151=CARTESIAN_POINT('Ctrl Pts',(1.06676497399994,15.2,11.059443552));
#226152=CARTESIAN_POINT('Ctrl Pts',(1.06676497399994,11.6,11.059443552));
#226153=CARTESIAN_POINT('Ctrl Pts',(1.06586446999994,15.2,11.062578207));
#226154=CARTESIAN_POINT('Ctrl Pts',(1.06586446999994,11.6,11.062578207));
#226155=CARTESIAN_POINT('Ctrl Pts',(1.06496006399994,15.2,11.065716989));
#226156=CARTESIAN_POINT('Ctrl Pts',(1.06496006399994,11.6,11.065716989));
#226157=CARTESIAN_POINT('Ctrl Pts',(1.06405175099994,15.2,11.068859885));
#226158=CARTESIAN_POINT('Ctrl Pts',(1.06405175099994,11.6,11.068859885));
#226159=CARTESIAN_POINT('Ctrl Pts',(1.06313952799994,15.2,11.072006888));
#226160=CARTESIAN_POINT('Ctrl Pts',(1.06313952799994,11.6,11.072006888));
#226161=CARTESIAN_POINT('Ctrl Pts',(1.06222338999994,15.2,11.075157987));
#226162=CARTESIAN_POINT('Ctrl Pts',(1.06222338999994,11.6,11.075157987));
#226163=CARTESIAN_POINT('Ctrl Pts',(1.06130333399994,15.2,11.078313171));
#226164=CARTESIAN_POINT('Ctrl Pts',(1.06130333399994,11.6,11.078313171));
#226165=CARTESIAN_POINT('Ctrl Pts',(1.06037935499994,15.2,11.081472431));
#226166=CARTESIAN_POINT('Ctrl Pts',(1.06037935499994,11.6,11.081472431));
#226167=CARTESIAN_POINT('Ctrl Pts',(1.05945144799994,15.2,11.084635756));
#226168=CARTESIAN_POINT('Ctrl Pts',(1.05945144799994,11.6,11.084635756));
#226169=CARTESIAN_POINT('Ctrl Pts',(1.05851961199994,15.2,11.087803136));
#226170=CARTESIAN_POINT('Ctrl Pts',(1.05851961199994,11.6,11.087803136));
#226171=CARTESIAN_POINT('Ctrl Pts',(1.05758383899994,15.2,11.090974562));
#226172=CARTESIAN_POINT('Ctrl Pts',(1.05758383899994,11.6,11.090974562));
#226173=CARTESIAN_POINT('Ctrl Pts',(1.05664412899994,15.2,11.094150023));
#226174=CARTESIAN_POINT('Ctrl Pts',(1.05664412899994,11.6,11.094150023));
#226175=CARTESIAN_POINT('Ctrl Pts',(1.05570047399994,15.2,11.097329511));
#226176=CARTESIAN_POINT('Ctrl Pts',(1.05570047399994,11.6,11.097329511));
#226177=CARTESIAN_POINT('Ctrl Pts',(1.05475287399994,15.2,11.100513013));
#226178=CARTESIAN_POINT('Ctrl Pts',(1.05475287399994,11.6,11.100513013));
#226179=CARTESIAN_POINT('Ctrl Pts',(1.05380132099994,15.2,11.103700521));
#226180=CARTESIAN_POINT('Ctrl Pts',(1.05380132099994,11.6,11.103700521));
#226181=CARTESIAN_POINT('Ctrl Pts',(1.05284581299994,15.2,11.106892026));
#226182=CARTESIAN_POINT('Ctrl Pts',(1.05284581299994,11.6,11.106892026));
#226183=CARTESIAN_POINT('Ctrl Pts',(1.05188634699994,15.2,11.110087516));
#226184=CARTESIAN_POINT('Ctrl Pts',(1.05188634699994,11.6,11.110087516));
#226185=CARTESIAN_POINT('Ctrl Pts',(1.05092291799994,15.2,11.113286982));
#226186=CARTESIAN_POINT('Ctrl Pts',(1.05092291799994,11.6,11.113286982));
#226187=CARTESIAN_POINT('Ctrl Pts',(1.04995552099994,15.2,11.116490413));
#226188=CARTESIAN_POINT('Ctrl Pts',(1.04995552099994,11.6,11.116490413));
#226189=CARTESIAN_POINT('Ctrl Pts',(1.04898415399994,15.2,11.119697801));
#226190=CARTESIAN_POINT('Ctrl Pts',(1.04898415399994,11.6,11.119697801));
#226191=CARTESIAN_POINT('Ctrl Pts',(1.04800881199994,15.2,11.122909136));
#226192=CARTESIAN_POINT('Ctrl Pts',(1.04800881199994,11.6,11.122909136));
#226193=CARTESIAN_POINT('Ctrl Pts',(1.04702949199994,15.2,11.126124407));
#226194=CARTESIAN_POINT('Ctrl Pts',(1.04702949199994,11.6,11.126124407));
#226195=CARTESIAN_POINT('Ctrl Pts',(1.04604618899994,15.2,11.129343605));
#226196=CARTESIAN_POINT('Ctrl Pts',(1.04604618899994,11.6,11.129343605));
#226197=CARTESIAN_POINT('Ctrl Pts',(1.04505889899994,15.2,11.13256672));
#226198=CARTESIAN_POINT('Ctrl Pts',(1.04505889899994,11.6,11.13256672));
#226199=CARTESIAN_POINT('Ctrl Pts',(1.04406761999994,15.2,11.135793742));
#226200=CARTESIAN_POINT('Ctrl Pts',(1.04406761999994,11.6,11.135793742));
#226201=CARTESIAN_POINT('Ctrl Pts',(1.04307234599994,15.2,11.139024661));
#226202=CARTESIAN_POINT('Ctrl Pts',(1.04307234599994,11.6,11.139024661));
#226203=CARTESIAN_POINT('Ctrl Pts',(1.04207307499994,15.2,11.142259469));
#226204=CARTESIAN_POINT('Ctrl Pts',(1.04207307499994,11.6,11.142259469));
#226205=CARTESIAN_POINT('Ctrl Pts',(1.04106980299994,15.2,11.145498154));
#226206=CARTESIAN_POINT('Ctrl Pts',(1.04106980299994,11.6,11.145498154));
#226207=CARTESIAN_POINT('Ctrl Pts',(1.04006252399994,15.2,11.148740708));
#226208=CARTESIAN_POINT('Ctrl Pts',(1.04006252399994,11.6,11.148740708));
#226209=CARTESIAN_POINT('Ctrl Pts',(1.03905123799994,15.2,11.15198712));
#226210=CARTESIAN_POINT('Ctrl Pts',(1.03905123799994,11.6,11.15198712));
#226211=CARTESIAN_POINT('Ctrl Pts',(1.03803593699994,15.2,11.15523738));
#226212=CARTESIAN_POINT('Ctrl Pts',(1.03803593699994,11.6,11.15523738));
#226213=CARTESIAN_POINT('Ctrl Pts',(1.03701662099994,15.2,11.158491481));
#226214=CARTESIAN_POINT('Ctrl Pts',(1.03701662099994,11.6,11.158491481));
#226215=CARTESIAN_POINT('Ctrl Pts',(1.03599328299994,15.2,11.161749411));
#226216=CARTESIAN_POINT('Ctrl Pts',(1.03599328299994,11.6,11.161749411));
#226217=CARTESIAN_POINT('Ctrl Pts',(1.03496592299994,15.2,11.165011161));
#226218=CARTESIAN_POINT('Ctrl Pts',(1.03496592299994,11.6,11.165011161));
#226219=CARTESIAN_POINT('Ctrl Pts',(1.03393453399994,15.2,11.168276721));
#226220=CARTESIAN_POINT('Ctrl Pts',(1.03393453399994,11.6,11.168276721));
#226221=CARTESIAN_POINT('Ctrl Pts',(1.03289911299994,15.2,11.171546082));
#226222=CARTESIAN_POINT('Ctrl Pts',(1.03289911299994,11.6,11.171546082));
#226223=CARTESIAN_POINT('Ctrl Pts',(1.03185965899994,15.2,11.174819234));
#226224=CARTESIAN_POINT('Ctrl Pts',(1.03185965899994,11.6,11.174819234));
#226225=CARTESIAN_POINT('Ctrl Pts',(1.03081616499994,15.2,11.178096167));
#226226=CARTESIAN_POINT('Ctrl Pts',(1.03081616499994,11.6,11.178096167));
#226227=CARTESIAN_POINT('Ctrl Pts',(1.02976862899994,15.2,11.181376874));
#226228=CARTESIAN_POINT('Ctrl Pts',(1.02976862899994,11.6,11.181376874));
#226229=CARTESIAN_POINT('Ctrl Pts',(1.02871704699994,15.2,11.184661342));
#226230=CARTESIAN_POINT('Ctrl Pts',(1.02871704699994,11.6,11.184661342));
#226231=CARTESIAN_POINT('Ctrl Pts',(1.02766141499994,15.2,11.187949564));
#226232=CARTESIAN_POINT('Ctrl Pts',(1.02766141499994,11.6,11.187949564));
#226233=CARTESIAN_POINT('Ctrl Pts',(1.02660172999994,15.2,11.191241528));
#226234=CARTESIAN_POINT('Ctrl Pts',(1.02660172999994,11.6,11.191241528));
#226235=CARTESIAN_POINT('Ctrl Pts',(1.02553798899994,15.2,11.194537227));
#226236=CARTESIAN_POINT('Ctrl Pts',(1.02553798899994,11.6,11.194537227));
#226237=CARTESIAN_POINT('Ctrl Pts',(1.02447018799994,15.2,11.19783665));
#226238=CARTESIAN_POINT('Ctrl Pts',(1.02447018799994,11.6,11.19783665));
#226239=CARTESIAN_POINT('Ctrl Pts',(1.02339832299994,15.2,11.201139789));
#226240=CARTESIAN_POINT('Ctrl Pts',(1.02339832299994,11.6,11.201139789));
#226241=CARTESIAN_POINT('Ctrl Pts',(1.02232238999994,15.2,11.204446633));
#226242=CARTESIAN_POINT('Ctrl Pts',(1.02232238999994,11.6,11.204446633));
#226243=CARTESIAN_POINT('Ctrl Pts',(1.02124238599994,15.2,11.207757173));
#226244=CARTESIAN_POINT('Ctrl Pts',(1.02124238599994,11.6,11.207757173));
#226245=CARTESIAN_POINT('Ctrl Pts',(1.02015830899994,15.2,11.2110714));
#226246=CARTESIAN_POINT('Ctrl Pts',(1.02015830899994,11.6,11.2110714));
#226247=CARTESIAN_POINT('Ctrl Pts',(1.01907015299994,15.2,11.214389305));
#226248=CARTESIAN_POINT('Ctrl Pts',(1.01907015299994,11.6,11.214389305));
#226249=CARTESIAN_POINT('Ctrl Pts',(1.01797791699994,15.2,11.217710876));
#226250=CARTESIAN_POINT('Ctrl Pts',(1.01797791699994,11.6,11.217710876));
#226251=CARTESIAN_POINT('Ctrl Pts',(1.01688159499994,15.2,11.221036107));
#226252=CARTESIAN_POINT('Ctrl Pts',(1.01688159499994,11.6,11.221036107));
#226253=CARTESIAN_POINT('Ctrl Pts',(1.01578118499994,15.2,11.224364988));
#226254=CARTESIAN_POINT('Ctrl Pts',(1.01578118499994,11.6,11.224364988));
#226255=CARTESIAN_POINT('Ctrl Pts',(1.01467668399994,15.2,11.227697508));
#226256=CARTESIAN_POINT('Ctrl Pts',(1.01467668399994,11.6,11.227697508));
#226257=CARTESIAN_POINT('Ctrl Pts',(1.01356808799994,15.2,11.231033658));
#226258=CARTESIAN_POINT('Ctrl Pts',(1.01356808799994,11.6,11.231033658));
#226259=CARTESIAN_POINT('Ctrl Pts',(1.01245539399994,15.2,11.23437343));
#226260=CARTESIAN_POINT('Ctrl Pts',(1.01245539399994,11.6,11.23437343));
#226261=CARTESIAN_POINT('Ctrl Pts',(1.01133859699994,15.2,11.237716814));
#226262=CARTESIAN_POINT('Ctrl Pts',(1.01133859699994,11.6,11.237716814));
#226263=CARTESIAN_POINT('Ctrl Pts',(1.01021769499994,15.2,11.2410638));
#226264=CARTESIAN_POINT('Ctrl Pts',(1.01021769499994,11.6,11.2410638));
#226265=CARTESIAN_POINT('Ctrl Pts',(1.00909268499994,15.2,11.244414379));
#226266=CARTESIAN_POINT('Ctrl Pts',(1.00909268499994,11.6,11.244414379));
#226267=CARTESIAN_POINT('Ctrl Pts',(1.00796356299994,15.2,11.247768542));
#226268=CARTESIAN_POINT('Ctrl Pts',(1.00796356299994,11.6,11.247768542));
#226269=CARTESIAN_POINT('Ctrl Pts',(1.00683032599994,15.2,11.251126281));
#226270=CARTESIAN_POINT('Ctrl Pts',(1.00683032599994,11.6,11.251126281));
#226271=CARTESIAN_POINT('Ctrl Pts',(1.00569296899994,15.2,11.254487586));
#226272=CARTESIAN_POINT('Ctrl Pts',(1.00569296899994,11.6,11.254487586));
#226273=CARTESIAN_POINT('Ctrl Pts',(1.00455149199994,15.2,11.257852446));
#226274=CARTESIAN_POINT('Ctrl Pts',(1.00455149199994,11.6,11.257852446));
#226275=CARTESIAN_POINT('Ctrl Pts',(1.00340588899994,15.2,11.261220854));
#226276=CARTESIAN_POINT('Ctrl Pts',(1.00340588899994,11.6,11.261220854));
#226277=CARTESIAN_POINT('Ctrl Pts',(1.00225615799994,15.2,11.2645928));
#226278=CARTESIAN_POINT('Ctrl Pts',(1.00225615799994,11.6,11.2645928));
#226279=CARTESIAN_POINT('Ctrl Pts',(1.00110229499994,15.2,11.267968273));
#226280=CARTESIAN_POINT('Ctrl Pts',(1.00110229499994,11.6,11.267968273));
#226281=CARTESIAN_POINT('Ctrl Pts',(0.999944296999944,15.2,11.271347268));
#226282=CARTESIAN_POINT('Ctrl Pts',(0.999944296999944,11.6,11.271347268));
#226283=CARTESIAN_POINT('Ctrl Pts',(0.998782160999945,15.2,11.274729773));
#226284=CARTESIAN_POINT('Ctrl Pts',(0.998782160999945,11.6,11.274729773));
#226285=CARTESIAN_POINT('Ctrl Pts',(0.997615883999944,15.2,11.278115779));
#226286=CARTESIAN_POINT('Ctrl Pts',(0.997615883999944,11.6,11.278115779));
#226287=CARTESIAN_POINT('Ctrl Pts',(0.996445460999944,15.2,11.281505278));
#226288=CARTESIAN_POINT('Ctrl Pts',(0.996445460999944,11.6,11.281505278));
#226289=CARTESIAN_POINT('Ctrl Pts',(0.995270891999944,15.2,11.284898259));
#226290=CARTESIAN_POINT('Ctrl Pts',(0.995270891999944,11.6,11.284898259));
#226291=CARTESIAN_POINT('Ctrl Pts',(0.994092170999944,15.2,11.288294714));
#226292=CARTESIAN_POINT('Ctrl Pts',(0.994092170999944,11.6,11.288294714));
#226293=CARTESIAN_POINT('Ctrl Pts',(0.992909295999944,15.2,11.291694635));
#226294=CARTESIAN_POINT('Ctrl Pts',(0.992909295999944,11.6,11.291694635));
#226295=CARTESIAN_POINT('Ctrl Pts',(0.991722263999945,15.2,11.295098011));
#226296=CARTESIAN_POINT('Ctrl Pts',(0.991722263999945,11.6,11.295098011));
#226297=CARTESIAN_POINT('Ctrl Pts',(0.990531070999944,15.2,11.298504835));
#226298=CARTESIAN_POINT('Ctrl Pts',(0.990531070999944,11.6,11.298504835));
#226299=CARTESIAN_POINT('Ctrl Pts',(0.989335713999945,15.2,11.301915096));
#226300=CARTESIAN_POINT('Ctrl Pts',(0.989335713999945,11.6,11.301915096));
#226301=CARTESIAN_POINT('Ctrl Pts',(0.988136190999944,15.2,11.305328786));
#226302=CARTESIAN_POINT('Ctrl Pts',(0.988136190999944,11.6,11.305328786));
#226303=CARTESIAN_POINT('Ctrl Pts',(0.986932497999944,15.2,11.308745896));
#226304=CARTESIAN_POINT('Ctrl Pts',(0.986932497999944,11.6,11.308745896));
#226305=CARTESIAN_POINT('Ctrl Pts',(0.985724631999945,15.2,11.312166416));
#226306=CARTESIAN_POINT('Ctrl Pts',(0.985724631999945,11.6,11.312166416));
#226307=CARTESIAN_POINT('Ctrl Pts',(0.984512589999944,15.2,11.315590338));
#226308=CARTESIAN_POINT('Ctrl Pts',(0.984512589999944,11.6,11.315590338));
#226309=CARTESIAN_POINT('Ctrl Pts',(0.983296368999944,15.2,11.319017653));
#226310=CARTESIAN_POINT('Ctrl Pts',(0.983296368999944,11.6,11.319017653));
#226311=CARTESIAN_POINT('Ctrl Pts',(0.982075964999944,15.2,11.322448352));
#226312=CARTESIAN_POINT('Ctrl Pts',(0.982075964999944,11.6,11.322448352));
#226313=CARTESIAN_POINT('Ctrl Pts',(0.980851376999944,15.2,11.325882426));
#226314=CARTESIAN_POINT('Ctrl Pts',(0.980851376999944,11.6,11.325882426));
#226315=CARTESIAN_POINT('Ctrl Pts',(0.979622599999944,15.2,11.329319866));
#226316=CARTESIAN_POINT('Ctrl Pts',(0.979622599999944,11.6,11.329319866));
#226317=CARTESIAN_POINT('Ctrl Pts',(0.978389631999944,15.2,11.332760663));
#226318=CARTESIAN_POINT('Ctrl Pts',(0.978389631999944,11.6,11.332760663));
#226319=CARTESIAN_POINT('Ctrl Pts',(0.977152469999945,15.2,11.336204808));
#226320=CARTESIAN_POINT('Ctrl Pts',(0.977152469999945,11.6,11.336204808));
#226321=CARTESIAN_POINT('Ctrl Pts',(0.975911110999944,15.2,11.339652292));
#226322=CARTESIAN_POINT('Ctrl Pts',(0.975911110999944,11.6,11.339652292));
#226323=CARTESIAN_POINT('Ctrl Pts',(0.974665549999945,15.2,11.343103107));
#226324=CARTESIAN_POINT('Ctrl Pts',(0.974665549999945,11.6,11.343103107));
#226325=CARTESIAN_POINT('Ctrl Pts',(0.973415787999944,15.2,11.346557243));
#226326=CARTESIAN_POINT('Ctrl Pts',(0.973415787999944,11.6,11.346557243));
#226327=CARTESIAN_POINT('Ctrl Pts',(0.972161818999945,15.2,11.350014692));
#226328=CARTESIAN_POINT('Ctrl Pts',(0.972161818999945,11.6,11.350014692));
#226329=CARTESIAN_POINT('Ctrl Pts',(0.970903640999944,15.2,11.353475445));
#226330=CARTESIAN_POINT('Ctrl Pts',(0.970903640999944,11.6,11.353475445));
#226331=CARTESIAN_POINT('Ctrl Pts',(0.969641250999944,15.2,11.356939492));
#226332=CARTESIAN_POINT('Ctrl Pts',(0.969641250999944,11.6,11.356939492));
#226333=CARTESIAN_POINT('Ctrl Pts',(0.968374644999944,15.2,11.360406825));
#226334=CARTESIAN_POINT('Ctrl Pts',(0.968374644999944,11.6,11.360406825));
#226335=CARTESIAN_POINT('Ctrl Pts',(0.967103821999945,15.2,11.363877435));
#226336=CARTESIAN_POINT('Ctrl Pts',(0.967103821999945,11.6,11.363877435));
#226337=CARTESIAN_POINT('Ctrl Pts',(0.965828776999944,15.2,11.367351315));
#226338=CARTESIAN_POINT('Ctrl Pts',(0.965828776999944,11.6,11.367351315));
#226339=CARTESIAN_POINT('Ctrl Pts',(0.964549509999945,15.2,11.370828453));
#226340=CARTESIAN_POINT('Ctrl Pts',(0.964549509999945,11.6,11.370828453));
#226341=CARTESIAN_POINT('Ctrl Pts',(0.963266015999944,15.2,11.374308844));
#226342=CARTESIAN_POINT('Ctrl Pts',(0.963266015999944,11.6,11.374308844));
#226343=CARTESIAN_POINT('Ctrl Pts',(0.961978292999944,15.2,11.377792477));
#226344=CARTESIAN_POINT('Ctrl Pts',(0.961978292999944,11.6,11.377792477));
#226345=CARTESIAN_POINT('Ctrl Pts',(0.960686336999944,15.2,11.381279343));
#226346=CARTESIAN_POINT('Ctrl Pts',(0.960686336999944,11.6,11.381279343));
#226347=CARTESIAN_POINT('Ctrl Pts',(0.959390145999944,15.2,11.384769435));
#226348=CARTESIAN_POINT('Ctrl Pts',(0.959390145999944,11.6,11.384769435));
#226349=CARTESIAN_POINT('Ctrl Pts',(0.958089717999945,15.2,11.388262743));
#226350=CARTESIAN_POINT('Ctrl Pts',(0.958089717999945,11.6,11.388262743));
#226351=CARTESIAN_POINT('Ctrl Pts',(0.956785049999944,15.2,11.391759258));
#226352=CARTESIAN_POINT('Ctrl Pts',(0.956785049999944,11.6,11.391759258));
#226353=CARTESIAN_POINT('Ctrl Pts',(0.955476135999944,15.2,11.395258971));
#226354=CARTESIAN_POINT('Ctrl Pts',(0.955476135999944,11.6,11.395258971));
#226355=CARTESIAN_POINT('Ctrl Pts',(0.954162975999945,15.2,11.398761871));
#226356=CARTESIAN_POINT('Ctrl Pts',(0.954162975999945,11.6,11.398761871));
#226357=CARTESIAN_POINT('Ctrl Pts',(0.952845566999944,15.2,11.402267953));
#226358=CARTESIAN_POINT('Ctrl Pts',(0.952845566999944,11.6,11.402267953));
#226359=CARTESIAN_POINT('Ctrl Pts',(0.951523905999945,15.2,11.405777206));
#226360=CARTESIAN_POINT('Ctrl Pts',(0.951523905999945,11.6,11.405777206));
#226361=CARTESIAN_POINT('Ctrl Pts',(0.950197990999944,15.2,11.409289625));
#226362=CARTESIAN_POINT('Ctrl Pts',(0.950197990999944,11.6,11.409289625));
#226363=CARTESIAN_POINT('Ctrl Pts',(0.948867817999944,15.2,11.4128052));
#226364=CARTESIAN_POINT('Ctrl Pts',(0.948867817999944,11.6,11.4128052));
#226365=CARTESIAN_POINT('Ctrl Pts',(0.947533385999945,15.2,11.416323924));
#226366=CARTESIAN_POINT('Ctrl Pts',(0.947533385999945,11.6,11.416323924));
#226367=CARTESIAN_POINT('Ctrl Pts',(0.946194692999944,15.2,11.419845788));
#226368=CARTESIAN_POINT('Ctrl Pts',(0.946194692999944,11.6,11.419845788));
#226369=CARTESIAN_POINT('Ctrl Pts',(0.944851733999944,15.2,11.423370785));
#226370=CARTESIAN_POINT('Ctrl Pts',(0.944851733999944,11.6,11.423370785));
#226371=CARTESIAN_POINT('Ctrl Pts',(0.943504507999945,15.2,11.426898902));
#226372=CARTESIAN_POINT('Ctrl Pts',(0.943504507999945,11.6,11.426898902));
#226373=CARTESIAN_POINT('Ctrl Pts',(0.942153009999944,15.2,11.430430131));
#226374=CARTESIAN_POINT('Ctrl Pts',(0.942153009999944,11.6,11.430430131));
#226375=CARTESIAN_POINT('Ctrl Pts',(0.940797236999944,15.2,11.43396446));
#226376=CARTESIAN_POINT('Ctrl Pts',(0.940797236999944,11.6,11.43396446));
#226377=CARTESIAN_POINT('Ctrl Pts',(0.939437186999944,15.2,11.437501879));
#226378=CARTESIAN_POINT('Ctrl Pts',(0.939437186999944,11.6,11.437501879));
#226379=CARTESIAN_POINT('Ctrl Pts',(0.938072854999944,15.2,11.441042379));
#226380=CARTESIAN_POINT('Ctrl Pts',(0.938072854999944,11.6,11.441042379));
#226381=CARTESIAN_POINT('Ctrl Pts',(0.936704240999945,15.2,11.444585952));
#226382=CARTESIAN_POINT('Ctrl Pts',(0.936704240999945,11.6,11.444585952));
#226383=CARTESIAN_POINT('Ctrl Pts',(0.935331340999944,15.2,11.448132591));
#226384=CARTESIAN_POINT('Ctrl Pts',(0.935331340999944,11.6,11.448132591));
#226385=CARTESIAN_POINT('Ctrl Pts',(0.933954155999944,15.2,11.451682296));
#226386=CARTESIAN_POINT('Ctrl Pts',(0.933954155999944,11.6,11.451682296));
#226387=CARTESIAN_POINT('Ctrl Pts',(0.932572683999945,15.2,11.45523506));
#226388=CARTESIAN_POINT('Ctrl Pts',(0.932572683999945,11.6,11.45523506));
#226389=CARTESIAN_POINT('Ctrl Pts',(0.931464076999945,15.2,11.458079719));
#226390=CARTESIAN_POINT('Ctrl Pts',(0.931464076999945,11.6,11.458079719));
#226391=CARTESIAN_POINT('Ctrl Pts',(0.930630692999944,15.2,11.460214592));
#226392=CARTESIAN_POINT('Ctrl Pts',(0.930630692999944,11.6,11.460214592));
#226393=CARTESIAN_POINT('Ctrl Pts',(0.930074245999944,15.2,11.461638451));
#226394=CARTESIAN_POINT('Ctrl Pts',(0.930074245999944,11.6,11.461638451));
#226395=CARTESIAN_POINT('Ctrl Pts',(0.929795807999944,15.2,11.462350533));
#226396=CARTESIAN_POINT('Ctrl Pts',(0.929795807999944,11.6,11.462350533));
#226397=CARTESIAN_POINT('Ctrl Pts',(1.18690176599994,15.2,10.306885525));
#226398=CARTESIAN_POINT('Ctrl Pts',(1.18695286801371,15.2,10.3086714414971));
#226399=CARTESIAN_POINT('Ctrl Pts',(1.18700024370246,15.2,10.3105146695817));
#226400=CARTESIAN_POINT('Ctrl Pts',(1.18704320751191,15.2,10.3124142316168));
#226401=CARTESIAN_POINT('Ctrl Pts',(1.18708637851457,15.2,10.3143229543003));
#226402=CARTESIAN_POINT('Ctrl Pts',(1.18712509878331,15.2,10.3162885644145));
#226403=CARTESIAN_POINT('Ctrl Pts',(1.18715870878653,15.2,10.3183101254623));
#226404=CARTESIAN_POINT('Ctrl Pts',(1.18720912378677,15.2,10.3213424667585));
#226405=CARTESIAN_POINT('Ctrl Pts',(1.18724803363287,15.2,10.3245006945537));
#226406=CARTESIAN_POINT('Ctrl Pts',(1.18727330150735,15.2,10.3277817524309));
#226407=CARTESIAN_POINT('Ctrl Pts',(1.18729014675699,15.2,10.329969124349));
#226408=CARTESIAN_POINT('Ctrl Pts',(1.18730093215753,15.2,10.3322110923867));
#226409=CARTESIAN_POINT('Ctrl Pts',(1.18730504824117,15.2,10.3345067774663));
#226410=CARTESIAN_POINT('Ctrl Pts',(1.18730916432518,15.2,10.3368024627545));
#226411=CARTESIAN_POINT('Ctrl Pts',(1.18730661025857,15.2,10.3391518689812));
#226412=CARTESIAN_POINT('Ctrl Pts',(1.18729679950772,15.2,10.3415541411144));
#226413=CARTESIAN_POINT('Ctrl Pts',(1.18728698875776,15.2,10.3439564130294));
#226414=CARTESIAN_POINT('Ctrl Pts',(1.18726991898249,15.2,10.3464115510702));
#226415=CARTESIAN_POINT('Ctrl Pts',(1.18724502131664,15.2,10.3489187242404));
#226416=CARTESIAN_POINT('Ctrl Pts',(1.18720767481559,15.2,10.3526794842235));
#226417=CARTESIAN_POINT('Ctrl Pts',(1.18715270884723,15.2,10.3565573188216));
#226418=CARTESIAN_POINT('Ctrl Pts',(1.18707827071955,15.2,10.3605495050483));
#226419=CARTESIAN_POINT('Ctrl Pts',(1.1870286453041,15.2,10.3632109623717));
#226420=CARTESIAN_POINT('Ctrl Pts',(1.18697036882753,15.2,10.3659232462405));
#226421=CARTESIAN_POINT('Ctrl Pts',(1.18690291049625,15.2,10.3686855733923));
#226422=CARTESIAN_POINT('Ctrl Pts',(1.18683545216496,15.2,10.3714479005441));
#226423=CARTESIAN_POINT('Ctrl Pts',(1.18675881427607,15.2,10.3742602697669));
#226424=CARTESIAN_POINT('Ctrl Pts',(1.18667248202963,15.2,10.3771219183275));
#226425=CARTESIAN_POINT('Ctrl Pts',(1.18657176107022,15.2,10.3804605084881));
#226426=CARTESIAN_POINT('Ctrl Pts',(1.18645784638535,15.2,10.3838661730002));
#226427=CARTESIAN_POINT('Ctrl Pts',(1.18632994899394,15.2,10.3873377257373));
#226428=CARTESIAN_POINT('Ctrl Pts',(1.18622032266415,15.2,10.3903133422146));
#226429=CARTESIAN_POINT('Ctrl Pts',(1.18610042326015,15.2,10.3933373687964));
#226430=CARTESIAN_POINT('Ctrl Pts',(1.18596977101537,15.2,10.3964090753493));
#226431=CARTESIAN_POINT('Ctrl Pts',(1.18579556801838,15.2,10.4005046841795));
#226432=CARTESIAN_POINT('Ctrl Pts',(1.1856022450273,15.2,10.4046850589283));
#226433=CARTESIAN_POINT('Ctrl Pts',(1.18538870347531,15.2,10.4089485158675));
#226434=CARTESIAN_POINT('Ctrl Pts',(1.18522854730041,15.2,10.4121461087897));
#226435=CARTESIAN_POINT('Ctrl Pts',(1.18505701725744,15.2,10.4153904361511));
#226436=CARTESIAN_POINT('Ctrl Pts',(1.18487366424664,15.2,10.4186808080836));
#226437=CARTESIAN_POINT('Ctrl Pts',(1.18453751708517,15.1999999999999,10.424713156178));
#226438=CARTESIAN_POINT('Ctrl Pts',(1.18416162582464,15.2,10.4309002494383));
#226439=CARTESIAN_POINT('Ctrl Pts',(1.18374332547081,15.2,10.4372379486635));
#226440=CARTESIAN_POINT('Ctrl Pts',(1.18347713432714,15.2,10.4412710301313));
#226441=CARTESIAN_POINT('Ctrl Pts',(1.18319377335533,15.2,10.4453651054476));
#226442=CARTESIAN_POINT('Ctrl Pts',(1.18289258444682,15.2,10.4495191354464));
#226443=CARTESIAN_POINT('Ctrl Pts',(1.18263442253865,15.2,10.4530797324033));
#226444=CARTESIAN_POINT('Ctrl Pts',(1.18236316078296,15.2,10.4566843811463));
#226445=CARTESIAN_POINT('Ctrl Pts',(1.18207840170939,15.2,10.4603324401822));
#226446=CARTESIAN_POINT('Ctrl Pts',(1.18174618277298,15.2,10.4645885092785));
#226447=CARTESIAN_POINT('Ctrl Pts',(1.18139558505007,15.2,10.4689036675259));
#226448=CARTESIAN_POINT('Ctrl Pts',(1.18102599447377,15.2,10.4732769201252));
#226449=CARTESIAN_POINT('Ctrl Pts',(1.18070920256766,15.2,10.4770254221585));
#226450=CARTESIAN_POINT('Ctrl Pts',(1.18037845378586,15.2,10.4808166073047));
#226451=CARTESIAN_POINT('Ctrl Pts',(1.18003337196443,15.2,10.4846498614173));
#226452=CARTESIAN_POINT('Ctrl Pts',(1.17963077648521,15.2,10.4891219914475));
#226453=CARTESIAN_POINT('Ctrl Pts',(1.17920866856116,15.2,10.4936513837703));
#226454=CARTESIAN_POINT('Ctrl Pts',(1.17876646494199,15.2,10.49823708297));
#226455=CARTESIAN_POINT('Ctrl Pts',(1.17838743328808,15.2,10.5021676820801));
#226456=CARTESIAN_POINT('Ctrl Pts',(1.17799363670509,15.2,10.5061396515878));
#226457=CARTESIAN_POINT('Ctrl Pts',(1.17758471896929,15.2,10.5101524006938));
#226458=CARTESIAN_POINT('Ctrl Pts',(1.17717580123348,15.2,10.5141651497998));
#226459=CARTESIAN_POINT('Ctrl Pts',(1.1767517616989,15.2,10.518218679519));
#226460=CARTESIAN_POINT('Ctrl Pts',(1.17631224929886,15.2,10.5223124107853));
#226461=CARTESIAN_POINT('Ctrl Pts',(1.17594598895219,15.2,10.5257238536312));
#226462=CARTESIAN_POINT('Ctrl Pts',(1.17556898609636,15.2,10.5291632155101));
#226463=CARTESIAN_POINT('Ctrl Pts',(1.17518104373351,15.2,10.5326301650397));
#226464=CARTESIAN_POINT('Ctrl Pts',(1.17479310137067,15.2,10.5360971145692));
#226465=CARTESIAN_POINT('Ctrl Pts',(1.17439421723886,15.2,10.5395916527444));
#226466=CARTESIAN_POINT('Ctrl Pts',(1.17398420022497,15.2,10.5431134547582));
#226467=CARTESIAN_POINT('Ctrl Pts',(1.17357418321109,15.2,10.5466352567721));
#226468=CARTESIAN_POINT('Ctrl Pts',(1.17315303291284,15.2,10.5501843224578));
#226469=CARTESIAN_POINT('Ctrl Pts',(1.17272056075807,15.2,10.5537603312935));
#226470=CARTESIAN_POINT('Ctrl Pts',(1.1722015941912,15.2,10.5580515417405));
#226471=CARTESIAN_POINT('Ctrl Pts',(1.17166632422587,15.2,10.5623815507141));
#226472=CARTESIAN_POINT('Ctrl Pts',(1.17111443174665,15.2,10.5667498129703));
#226473=CARTESIAN_POINT('Ctrl Pts',(1.17056253921729,15.2,10.5711180756234));
#226474=CARTESIAN_POINT('Ctrl Pts',(1.16999402489421,15.2,10.5755245911646));
#226475=CARTESIAN_POINT('Ctrl Pts',(1.16940857744449,15.2,10.5799688229927));
#226476=CARTESIAN_POINT('Ctrl Pts',(1.16892070464949,15.2,10.5836723489106));
#226477=CARTESIAN_POINT('Ctrl Pts',(1.16842107404348,15.2,10.5874020673035));
#226478=CARTESIAN_POINT('Ctrl Pts',(1.16790950805855,15.2,10.5911576723087));
#226479=CARTESIAN_POINT('Ctrl Pts',(1.16719331559044,15.2,10.5964155199709));
#226480=CARTESIAN_POINT('Ctrl Pts',(1.16645373272989,15.2,10.6017241030071));
#226481=CARTESIAN_POINT('Ctrl Pts',(1.16569028676057,15.2,10.6070825977414));
#226482=CARTESIAN_POINT('Ctrl Pts',(1.16514496821954,15.2,10.6109100939206));
#226483=CARTESIAN_POINT('Ctrl Pts',(1.16458747581952,15.2,10.6147630547858));
#226484=CARTESIAN_POINT('Ctrl Pts',(1.16401764373362,15.2,10.6186411829978));
#226485=CARTESIAN_POINT('Ctrl Pts',(1.16333384525538,15.2,10.6232949366832));
#226486=CARTESIAN_POINT('Ctrl Pts',(1.16263227336771,15.2,10.6279849340589));
#226487=CARTESIAN_POINT('Ctrl Pts',(1.16191265006174,15.2,10.6327106667182));
#226488=CARTESIAN_POINT('Ctrl Pts',(1.16119302669041,15.2,10.6374363998066));
#226489=CARTESIAN_POINT('Ctrl Pts',(1.16045534972569,15.2,10.6421978708152));
#226490=CARTESIAN_POINT('Ctrl Pts',(1.1596993444337,15.2,10.6469945807448));
#226491=CARTESIAN_POINT('Ctrl Pts',(1.15906934005804,15.2,10.6509918388016));
#226492=CARTESIAN_POINT('Ctrl Pts',(1.15842660794081,15.2,10.6550135682326));
#226493=CARTESIAN_POINT('Ctrl Pts',(1.15777099269882,15.2,10.659059485728));
#226494=CARTESIAN_POINT('Ctrl Pts',(1.15711537745684,15.2,10.6631054032235));
#226495=CARTESIAN_POINT('Ctrl Pts',(1.15644687780632,15.2,10.667175508028));
#226496=CARTESIAN_POINT('Ctrl Pts',(1.15576534190249,15.2,10.6712695187938));
#226497=CARTESIAN_POINT('Ctrl Pts',(1.155220113224,15.2,10.6745447271386));
#226498=CARTESIAN_POINT('Ctrl Pts',(1.15466654257434,15.2,10.6778352371122));
#226499=CARTESIAN_POINT('Ctrl Pts',(1.15410455178751,15.2,10.6811409047298));
#226500=CARTESIAN_POINT('Ctrl Pts',(1.1535425609241,15.2,10.6844465727978));
#226501=CARTESIAN_POINT('Ctrl Pts',(1.15297215003825,15.2,10.6877673986787));
#226502=CARTESIAN_POINT('Ctrl Pts',(1.15239324386593,15.2,10.6911032422507));
#226503=CARTESIAN_POINT('Ctrl Pts',(1.15166961118997,15.2,10.6952730464885));
#226504=CARTESIAN_POINT('Ctrl Pts',(1.1509327052696,15.2,10.6994663145884));
#226505=CARTESIAN_POINT('Ctrl Pts',(1.1501823808935,15.2,10.7036827752848));
#226506=CARTESIAN_POINT('Ctrl Pts',(1.14928199167489,15.2,10.7087425279366));
#226507=CARTESIAN_POINT('Ctrl Pts',(1.14836228026973,15.2,10.7138356774902));
#226508=CARTESIAN_POINT('Ctrl Pts',(1.14742300029955,15.2,10.7189617582439));
#226509=CARTESIAN_POINT('Ctrl Pts',(1.1467968136812,15.2,10.7223791452579));
#226510=CARTESIAN_POINT('Ctrl Pts',(1.1461619311628,15.2,10.725811169478));
#226511=CARTESIAN_POINT('Ctrl Pts',(1.14551828110521,15.2,10.7292576936948));
#226512=CARTESIAN_POINT('Ctrl Pts',(1.1443918933948,15.2,10.7352891116611));
#226513=CARTESIAN_POINT('Ctrl Pts',(1.14323865498352,15.2,10.7413649352983));
#226514=CARTESIAN_POINT('Ctrl Pts',(1.14205819256337,15.2,10.7474844471975));
#226515=CARTESIAN_POINT('Ctrl Pts',(1.14138364258275,15.2,10.7509813112761));
#226516=CARTESIAN_POINT('Ctrl Pts',(1.14070020422257,15.2,10.7544924398559));
#226517=CARTESIAN_POINT('Ctrl Pts',(1.14000780814946,15.2,10.7580177015032));
#226518=CARTESIAN_POINT('Ctrl Pts',(1.13896921413414,15.2,10.7633055934938));
#226519=CARTESIAN_POINT('Ctrl Pts',(1.13791046703578,15.2,10.768625281911));
#226520=CARTESIAN_POINT('Ctrl Pts',(1.13683134199165,15.2,10.7739763247166));
#226521=CARTESIAN_POINT('Ctrl Pts',(1.13611192523021,15.2,10.7775436869111));
#226522=CARTESIAN_POINT('Ctrl Pts',(1.13538345167051,15.2,10.7811249847571));
#226523=CARTESIAN_POINT('Ctrl Pts',(1.13464585562938,15.2,10.7847200876211));
#226524=CARTESIAN_POINT('Ctrl Pts',(1.13372386072871,15.2,10.7892139654663));
#226525=CARTESIAN_POINT('Ctrl Pts',(1.13278761255285,15.2,10.7937294145361));
#226526=CARTESIAN_POINT('Ctrl Pts',(1.13183698515765,15.2,10.7982661832065));
#226527=CARTESIAN_POINT('Ctrl Pts',(1.13107648311716,15.2,10.8018955987362));
#226528=CARTESIAN_POINT('Ctrl Pts',(1.13030677847856,15.2,10.8055386578811));
#226529=CARTESIAN_POINT('Ctrl Pts',(1.12952780849165,15.2,10.8091952340249));
#226530=CARTESIAN_POINT('Ctrl Pts',(1.12835935361742,15.2,10.8146800977424));
#226531=CARTESIAN_POINT('Ctrl Pts',(1.12717005279062,15.2,10.8201953749398));
#226532=CARTESIAN_POINT('Ctrl Pts',(1.12595969485868,15.2,10.8257406381802));
#226533=CARTESIAN_POINT('Ctrl Pts',(1.12474933681681,15.2,10.8312859019244));
#226534=CARTESIAN_POINT('Ctrl Pts',(1.12351792356648,15.2,10.8368611537618));
#226535=CARTESIAN_POINT('Ctrl Pts',(1.12226524966344,15.2,10.8424659701525));
#226536=CARTESIAN_POINT('Ctrl Pts',(1.12122135480113,15.2,10.8471366502236));
#226537=CARTESIAN_POINT('Ctrl Pts',(1.12016269726633,15.2,10.8518278621646));
#226538=CARTESIAN_POINT('Ctrl Pts',(1.11908916066789,15.2,10.8565393663329));
#226539=CARTESIAN_POINT('Ctrl Pts',(1.11801562418647,15.2,10.8612508699876));
#226540=CARTESIAN_POINT('Ctrl Pts',(1.11692720788392,15.2,10.8659826645702));
#226541=CARTESIAN_POINT('Ctrl Pts',(1.1158238006443,15.2,10.8707345116201));
#226542=CARTESIAN_POINT('Ctrl Pts',(1.11494107470829,15.2,10.8745359898815));
#226543=CARTESIAN_POINT('Ctrl Pts',(1.11404875380192,15.2,10.8783503023303));
#226544=CARTESIAN_POINT('Ctrl Pts',(1.11314678180832,15.2,10.8821773273166));
#226545=CARTESIAN_POINT('Ctrl Pts',(1.11179382394082,15.2,10.8879178642746));
#226546=CARTESIAN_POINT('Ctrl Pts',(1.11041914749445,15.2,10.8936870052702));
#226547=CARTESIAN_POINT('Ctrl Pts',(1.10902256939336,15.2,10.8994843454308));
#226548=CARTESIAN_POINT('Ctrl Pts',(1.10785875426684,15.2,10.9043154624069));
#226549=CARTESIAN_POINT('Ctrl Pts',(1.10667972569385,15.2,10.9091661619548));
#226550=CARTESIAN_POINT('Ctrl Pts',(1.10548538006967,15.2,10.9140362136899));
#226551=CARTESIAN_POINT('Ctrl Pts',(1.10429103444549,15.2,10.9189062654249));
#226552=CARTESIAN_POINT('Ctrl Pts',(1.1030813707681,15.2,10.9237956675634));
#226553=CARTESIAN_POINT('Ctrl Pts',(1.10185628438001,15.2,10.9287041919374));
#226554=CARTESIAN_POINT('Ctrl Pts',(1.10014116340998,15.2,10.935576126168));
#226555=CARTESIAN_POINT('Ctrl Pts',(1.09839581377953,15.2,10.9424855407517));
#226556=CARTESIAN_POINT('Ctrl Pts',(1.09661995700762,15.2,10.9494318102527));
#226557=CARTESIAN_POINT('Ctrl Pts',(1.09509779413927,15.2,10.9553857552302));
#226558=CARTESIAN_POINT('Ctrl Pts',(1.09355321476903,15.2,10.9613667788838));
#226559=CARTESIAN_POINT('Ctrl Pts',(1.09198605007697,15.2,10.9673744939143));
#226560=CARTESIAN_POINT('Ctrl Pts',(1.09094127352069,15.2,10.9713796376318));
#226561=CARTESIAN_POINT('Ctrl Pts',(1.08988645932708,15.2,10.9753966439952));
#226562=CARTESIAN_POINT('Ctrl Pts',(1.08882155671283,15.2,10.9794253996044));
#226563=CARTESIAN_POINT('Ctrl Pts',(1.08775665424368,15.2,10.9834541546647));
#226564=CARTESIAN_POINT('Ctrl Pts',(1.08668166219425,15.2,10.9874946584668));
#226565=CARTESIAN_POINT('Ctrl Pts',(1.08559653367406,15.2,10.9915467991703));
#226566=CARTESIAN_POINT('Ctrl Pts',(1.08369755857891,15.2,10.9986380460917));
#226567=CARTESIAN_POINT('Ctrl Pts',(1.08176753691945,15.2,11.0057649279105));
#226568=CARTESIAN_POINT('Ctrl Pts',(1.07980621174998,15.2,11.0129268455083));
#226569=CARTESIAN_POINT('Ctrl Pts',(1.07868545446665,15.2,11.0170193700092));
#226570=CARTESIAN_POINT('Ctrl Pts',(1.07755447462942,15.2,11.021123336189));
#226571=CARTESIAN_POINT('Ctrl Pts',(1.07641322728838,15.2,11.0252386319145));
#226572=CARTESIAN_POINT('Ctrl Pts',(1.07527198010284,15.2,11.0293539270792));
#226573=CARTESIAN_POINT('Ctrl Pts',(1.07412046251936,15.2,11.0334805523111));
#226574=CARTESIAN_POINT('Ctrl Pts',(1.07295863077578,15.2,11.0376183975471));
#226575=CARTESIAN_POINT('Ctrl Pts',(1.0717967988739,15.2,11.0417562433469));
#226576=CARTESIAN_POINT('Ctrl Pts',(1.07062465233603,15.2,11.0459053084245));
#226577=CARTESIAN_POINT('Ctrl Pts',(1.06944214454831,15.2,11.0500654854301));
#226578=CARTESIAN_POINT('Ctrl Pts',(1.0682596369217,15.2,11.0542256618689));
#226579=CARTESIAN_POINT('Ctrl Pts',(1.06706676838811,15.2,11.0583969486063));
#226580=CARTESIAN_POINT('Ctrl Pts',(1.06586349459825,15.2,11.0625792383748));
#226581=CARTESIAN_POINT('Ctrl Pts',(1.06435940223797,15.2,11.0678071010129));
#226582=CARTESIAN_POINT('Ctrl Pts',(1.06283904978554,15.2,11.0730521546788));
#226583=CARTESIAN_POINT('Ctrl Pts',(1.06130235325082,15.2,11.0783141899804));
#226584=CARTESIAN_POINT('Ctrl Pts',(1.06007299595604,15.2,11.0825238184512));
#226585=CARTESIAN_POINT('Ctrl Pts',(1.05883317699255,15.2,11.0867443142906));
#226586=CARTESIAN_POINT('Ctrl Pts',(1.05758285447889,15.2,11.0909755714668));
#226587=CARTESIAN_POINT('Ctrl Pts',(1.05601995142198,15.2,11.0962646426487));
#226588=CARTESIAN_POINT('Ctrl Pts',(1.05444063549815,15.2,11.1015705285948));
#226589=CARTESIAN_POINT('Ctrl Pts',(1.05284482327458,15.2,11.1068930229711));
#226590=CARTESIAN_POINT('Ctrl Pts',(1.05156817360009,15.2,11.1111510181241));
#226591=CARTESIAN_POINT('Ctrl Pts',(1.05028096661174,15.2,11.1154196405691));
#226592=CARTESIAN_POINT('Ctrl Pts',(1.04898316026753,15.2,11.1196987877387));
#226593=CARTESIAN_POINT('Ctrl Pts',(1.04736090220466,15.2,11.1250477221379));
#226594=CARTESIAN_POINT('Ctrl Pts',(1.04572208267221,15.2,11.1304131000166));
#226595=CARTESIAN_POINT('Ctrl Pts',(1.04406662128332,15.2,11.1357947162666));
#226596=CARTESIAN_POINT('Ctrl Pts',(1.04307334448608,15.2,11.1390236858993));
#226597=CARTESIAN_POINT('Ctrl Pts',(1.0420740771224,15.2,11.1422585022818));
#226598=CARTESIAN_POINT('Ctrl Pts',(1.04106880140946,15.2,11.1454991208718));
#226599=CARTESIAN_POINT('Ctrl Pts',(1.03972843367046,15.2,11.149819946051));
#226600=CARTESIAN_POINT('Ctrl Pts',(1.03837738522607,15.2,11.1541510856172));
#226601=CARTESIAN_POINT('Ctrl Pts',(1.03701561536066,15.2,11.158492438905));
#226602=CARTESIAN_POINT('Ctrl Pts',(1.03565384568079,15.2,11.1628337916012));
#226603=CARTESIAN_POINT('Ctrl Pts',(1.03428135514361,15.2,11.1671853555285));
#226604=CARTESIAN_POINT('Ctrl Pts',(1.03289810481297,15.2,11.1715470293935));
#226605=CARTESIAN_POINT('Ctrl Pts',(1.03116904175831,15.2,11.1769991221704));
#226606=CARTESIAN_POINT('Ctrl Pts',(1.02942316644761,15.2,11.18246701217));
#226607=CARTESIAN_POINT('Ctrl Pts',(1.02766040186517,15.2,11.1879504991831));
#226608=CARTESIAN_POINT('Ctrl Pts',(1.02589763728273,15.2,11.1934339861961));
#226609=CARTESIAN_POINT('Ctrl Pts',(1.02411798678128,15.2,11.1989330715553));
#226610=CARTESIAN_POINT('Ctrl Pts',(1.0223213722593,15.2,11.2044475569969));
#226611=CARTESIAN_POINT('Ctrl Pts',(1.02124340358528,15.2,11.2077562481417));
#226612=CARTESIAN_POINT('Ctrl Pts',(1.02015932932857,15.2,11.2110704840593));
#226613=CARTESIAN_POINT('Ctrl Pts',(1.01906913307705,15.2,11.2143902211882));
#226614=CARTESIAN_POINT('Ctrl Pts',(1.01797893682553,15.2,11.2177099583171));
#226615=CARTESIAN_POINT('Ctrl Pts',(1.01688261823276,15.2,11.2210351974956));
#226616=CARTESIAN_POINT('Ctrl Pts',(1.01578016248198,15.2,11.2243658970405));
#226617=CARTESIAN_POINT('Ctrl Pts',(1.01467770653093,15.2,11.2276965971905));
#226618=CARTESIAN_POINT('Ctrl Pts',(1.01356911398648,15.2,11.2310327560754));
#226619=CARTESIAN_POINT('Ctrl Pts',(1.01245436803196,15.2,11.2343743337284));
#226620=CARTESIAN_POINT('Ctrl Pts',(1.01096804043012,15.2,11.2388297695874));
#226621=CARTESIAN_POINT('Ctrl Pts',(1.00947077389564,15.2,11.2432948359924));
#226622=CARTESIAN_POINT('Ctrl Pts',(1.00796253423434,15.2,11.2477694359802));
#226623=CARTESIAN_POINT('Ctrl Pts',(1.00683135443699,15.2,11.2511253861235));
#226624=CARTESIAN_POINT('Ctrl Pts',(1.0056940009491,15.2,11.2544866994392));
#226625=CARTESIAN_POINT('Ctrl Pts',(1.00455046065786,15.2,11.2578533326081));
#226626=CARTESIAN_POINT('Ctrl Pts',(1.00302574013104,15.2,11.262342177241));
#226627=CARTESIAN_POINT('Ctrl Pts',(1.00149001879179,15.2,11.2668404801473));
#226628=CARTESIAN_POINT('Ctrl Pts',(0.999943262373438,15.2,11.2713481458935));
#226629=CARTESIAN_POINT('Ctrl Pts',(0.998783195165049,15.2,11.2747288948962));
#226630=CARTESIAN_POINT('Ctrl Pts',(0.997616920657404,15.2,11.2781149094398));
#226631=CARTESIAN_POINT('Ctrl Pts',(0.996444424449991,15.2,11.2815061485249));
#226632=CARTESIAN_POINT('Ctrl Pts',(0.995271928242578,15.2,11.2848973876101));
#226633=CARTESIAN_POINT('Ctrl Pts',(0.994093210618774,15.2,11.2882938507866));
#226634=CARTESIAN_POINT('Ctrl Pts',(0.992908256870712,15.2,11.2916954984126));
#226635=CARTESIAN_POINT('Ctrl Pts',(0.99172330312265,15.2,11.2950971460385));
#226636=CARTESIAN_POINT('Ctrl Pts',(0.990532112980523,15.2,11.298503977744));
#226637=CARTESIAN_POINT('Ctrl Pts',(0.989334672714937,15.2,11.3019159525815));
#226638=CARTESIAN_POINT('Ctrl Pts',(0.988137232449352,15.2,11.3053279274191));
#226639=CARTESIAN_POINT('Ctrl Pts',(0.986933542468933,15.2,11.308745045579));
#226640=CARTESIAN_POINT('Ctrl Pts',(0.985723588263753,15.2,11.3121672657456));
#226641=CARTESIAN_POINT('Ctrl Pts',(0.984513633838765,15.2,11.3155894865339));
#226642=CARTESIAN_POINT('Ctrl Pts',(0.983297415128669,15.2,11.3190168102487));
#226643=CARTESIAN_POINT('Ctrl Pts',(0.982074918700141,15.2,11.3224491964982));
#226644=CARTESIAN_POINT('Ctrl Pts',(0.980852422493701,15.2,11.3258815821242));
#226645=CARTESIAN_POINT('Ctrl Pts',(0.979623648570926,15.2,11.3293190302499));
#226646=CARTESIAN_POINT('Ctrl Pts',(0.978388583365259,15.2,11.3327615003753));
#226647=CARTESIAN_POINT('Ctrl Pts',(0.976330141281025,15.2,11.3384989507926));
#226648=CARTESIAN_POINT('Ctrl Pts',(0.97425422278491,15.2,11.3442503513581));
#226649=CARTESIAN_POINT('Ctrl Pts',(0.972160766498573,15.2,11.3500155186609));
#226650=CARTESIAN_POINT('Ctrl Pts',(0.970067310212236,15.2,11.3557806859637));
#226651=CARTESIAN_POINT('Ctrl Pts',(0.967956314861861,15.2,11.3615596164955));
#226652=CARTESIAN_POINT('Ctrl Pts',(0.965827721179896,15.2,11.367352130316));
#226653=CARTESIAN_POINT('Ctrl Pts',(0.96455056501712,15.2,11.370827638482));
#226654=CARTESIAN_POINT('Ctrl Pts',(0.963267074329644,15.2,11.3743080369395));
#226655=CARTESIAN_POINT('Ctrl Pts',(0.961977234625954,15.2,11.3777932856466));
#226656=CARTESIAN_POINT('Ctrl Pts',(0.960687394922265,15.2,11.3812785343537));
#226657=CARTESIAN_POINT('Ctrl Pts',(0.959391206307425,15.2,11.3847686341142));
#226658=CARTESIAN_POINT('Ctrl Pts',(0.958088657973805,15.2,11.3882635447531));
#226659=CARTESIAN_POINT('Ctrl Pts',(0.956786109640184,15.2,11.391758455392));
#226660=CARTESIAN_POINT('Ctrl Pts',(0.955477198459337,15.2,11.3952581762249));
#226661=CARTESIAN_POINT('Ctrl Pts',(0.954161913751181,15.2,11.3987626664468));
#226662=CARTESIAN_POINT('Ctrl Pts',(0.951969772491273,15.2,11.4046034836955));
#226663=CARTESIAN_POINT('Ctrl Pts',(0.949759925377751,15.2,11.4104575534611));
#226664=CARTESIAN_POINT('Ctrl Pts',(0.947532320724996,15.2,11.4163247090166));
#226665=CARTESIAN_POINT('Ctrl Pts',(0.945750236905668,15.2,11.4210184337168));
#226666=CARTESIAN_POINT('Ctrl Pts',(0.943956788673861,15.2,11.4257205357515));
#226667=CARTESIAN_POINT('Ctrl Pts',(0.942151940963227,15.2,11.4304309067868));
#226668=CARTESIAN_POINT('Ctrl Pts',(0.940798305303206,15.2,11.4339636847424));
#226669=CARTESIAN_POINT('Ctrl Pts',(0.93943825738824,15.2,11.4375011120198));
#226670=CARTESIAN_POINT('Ctrl Pts',(0.938071784202212,15.2,11.4410431479436));
#226671=CARTESIAN_POINT('Ctrl Pts',(0.936705311016184,15.2,11.4445851838674));
#226672=CARTESIAN_POINT('Ctrl Pts',(0.935332412639122,15.2,11.4481318270972));
#226673=CARTESIAN_POINT('Ctrl Pts',(0.933953084118917,15.2,11.4516830612001));
#226674=CARTESIAN_POINT('Ctrl Pts',(0.932573755598712,15.2,11.4552342953029));
#226675=CARTESIAN_POINT('Ctrl Pts',(0.931187998930692,15.2,11.4587901206197));
#226676=CARTESIAN_POINT('Ctrl Pts',(0.929795807999944,15.2,11.462350533));
#226677=CARTESIAN_POINT('Ctrl Pts',(1.18690176599994,12.2,10.306885525));
#226678=CARTESIAN_POINT('Ctrl Pts',(1.18695286801371,12.2,10.3086714414971));
#226679=CARTESIAN_POINT('Ctrl Pts',(1.18700024370246,12.2,10.3105146695817));
#226680=CARTESIAN_POINT('Ctrl Pts',(1.18704320751191,12.2,10.3124142316168));
#226681=CARTESIAN_POINT('Ctrl Pts',(1.18708637851457,12.2,10.3143229543003));
#226682=CARTESIAN_POINT('Ctrl Pts',(1.18712509878331,12.2,10.3162885644145));
#226683=CARTESIAN_POINT('Ctrl Pts',(1.18715870878653,12.2,10.3183101254623));
#226684=CARTESIAN_POINT('Ctrl Pts',(1.18719792045236,12.2,10.3206686130759));
#226685=CARTESIAN_POINT('Ctrl Pts',(1.18723017380984,12.2,10.3231032567151));
#226686=CARTESIAN_POINT('Ctrl Pts',(1.18725445923935,12.2,10.3256126117905));
#226687=CARTESIAN_POINT('Ctrl Pts',(1.18727527532422,12.2,10.3277634878206));
#226688=CARTESIAN_POINT('Ctrl Pts',(1.18729023811691,12.2,10.3299692556294));
#226689=CARTESIAN_POINT('Ctrl Pts',(1.18729873228409,12.2,10.332229031702));
#226690=CARTESIAN_POINT('Ctrl Pts',(1.1873072264505,12.2,10.3344888075693));
#226691=CARTESIAN_POINT('Ctrl Pts',(1.18730925155811,12.2,10.3368025915109));
#226692=CARTESIAN_POINT('Ctrl Pts',(1.18730421297496,12.2,10.3391695235082));
#226693=CARTESIAN_POINT('Ctrl Pts',(1.18729917439181,12.2,10.3415364555056));
#226694=CARTESIAN_POINT('Ctrl Pts',(1.18728707303501,12.2,10.3439565353885));
#226695=CARTESIAN_POINT('Ctrl Pts',(1.18726733053518,12.2,10.3464289265025));
#226696=CARTESIAN_POINT('Ctrl Pts',(1.18724758803356,12.2,10.3489013178411));
#226697=CARTESIAN_POINT('Ctrl Pts',(1.18722020562358,12.2,10.3514260183951));
#226698=CARTESIAN_POINT('Ctrl Pts',(1.18718462303775,12.2,10.354002210789));
#226699=CARTESIAN_POINT('Ctrl Pts',(1.18714311002579,12.2,10.357007768231));
#226700=CARTESIAN_POINT('Ctrl Pts',(1.18709043565391,12.2,10.3600834109926));
#226701=CARTESIAN_POINT('Ctrl Pts',(1.18702574223863,12.2,10.363227875506));
#226702=CARTESIAN_POINT('Ctrl Pts',(1.18697029073335,12.2,10.3659231311179));
#226703=CARTESIAN_POINT('Ctrl Pts',(1.18690600797991,12.2,10.3686689487489));
#226704=CARTESIAN_POINT('Ctrl Pts',(1.18683237347527,12.2,10.371464553238));
#226705=CARTESIAN_POINT('Ctrl Pts',(1.1867587389773,12.2,10.3742601574731));
#226706=CARTESIAN_POINT('Ctrl Pts',(1.18667575005532,12.2,10.3771055480514));
#226707=CARTESIAN_POINT('Ctrl Pts',(1.18658290080825,12.2,10.3799999665429));
#226708=CARTESIAN_POINT('Ctrl Pts',(1.18649005156118,12.2,10.3828943850343));
#226709=CARTESIAN_POINT('Ctrl Pts',(1.18638734160986,12.2,10.3858378317145));
#226710=CARTESIAN_POINT('Ctrl Pts',(1.18627427753108,12.2,10.3888295642704));
#226711=CARTESIAN_POINT('Ctrl Pts',(1.18616121344203,12.2,10.391821297098));
#226712=CARTESIAN_POINT('Ctrl Pts',(1.18603779598505,12.2,10.3948613190067));
#226713=CARTESIAN_POINT('Ctrl Pts',(1.18590354672699,12.2,10.3979488990948));
#226714=CARTESIAN_POINT('Ctrl Pts',(1.18576929748114,12.2,10.4010364789024));
#226715=CARTESIAN_POINT('Ctrl Pts',(1.18562421525287,12.2,10.4041716229954));
#226716=CARTESIAN_POINT('Ctrl Pts',(1.18546783625806,12.2,10.4073536176319));
#226717=CARTESIAN_POINT('Ctrl Pts',(1.18531145726325,12.2,10.4105356122684));
#226718=CARTESIAN_POINT('Ctrl Pts',(1.18514378166932,12.2,10.4137644582844));
#226719=CARTESIAN_POINT('Ctrl Pts',(1.18496435750969,12.2,10.4170394620799));
#226720=CARTESIAN_POINT('Ctrl Pts',(1.18478493333377,12.2,10.420314466173));
#226721=CARTESIAN_POINT('Ctrl Pts',(1.18459375917304,12.2,10.4236356272053));
#226722=CARTESIAN_POINT('Ctrl Pts',(1.18439039899446,12.2,10.4270022671419));
#226723=CARTESIAN_POINT('Ctrl Pts',(1.18418703883435,12.2,10.4303689067727));
#226724=CARTESIAN_POINT('Ctrl Pts',(1.1839714892964,12.2,10.4337810218705));
#226725=CARTESIAN_POINT('Ctrl Pts',(1.18374332547081,12.2,10.4372379486635));
#226726=CARTESIAN_POINT('Ctrl Pts',(1.18351516164522,12.2,10.4406948754565));
#226727=CARTESIAN_POINT('Ctrl Pts',(1.18327438385395,12.2,10.4441966142294));
#226728=CARTESIAN_POINT('Ctrl Pts',(1.18302057603041,12.2,10.4477425100152));
#226729=CARTESIAN_POINT('Ctrl Pts',(1.18276676820687,12.2,10.451288405801));
#226730=CARTESIAN_POINT('Ctrl Pts',(1.18249993016942,12.2,10.4548784596805));
#226731=CARTESIAN_POINT('Ctrl Pts',(1.18221965851385,12.2,10.4585120306289));
#226732=CARTESIAN_POINT('Ctrl Pts',(1.18193938683282,12.2,10.4621456019073));
#226733=CARTESIAN_POINT('Ctrl Pts',(1.18164568252551,12.2,10.4658226901399));
#226734=CARTESIAN_POINT('Ctrl Pts',(1.18133814975815,12.2,10.4695426684278));
#226735=CARTESIAN_POINT('Ctrl Pts',(1.18097936157147,12.2,10.4738826425902));
#226736=CARTESIAN_POINT('Ctrl Pts',(1.18060175535009,12.2,10.4782809928034));
#226737=CARTESIAN_POINT('Ctrl Pts',(1.18020472052873,12.2,10.4827367423836));
#226738=CARTESIAN_POINT('Ctrl Pts',(1.17986440492782,12.2,10.4865559567556));
#226739=CARTESIAN_POINT('Ctrl Pts',(1.17950981874221,12.2,10.4904173423067));
#226740=CARTESIAN_POINT('Ctrl Pts',(1.17914058897145,12.2,10.4943202957711));
#226741=CARTESIAN_POINT('Ctrl Pts',(1.17870982095588,12.2,10.4988737409479));
#226742=CARTESIAN_POINT('Ctrl Pts',(1.17825912168566,12.2,10.5034837655246));
#226743=CARTESIAN_POINT('Ctrl Pts',(1.17778791953566,12.2,10.508149426814));
#226744=CARTESIAN_POINT('Ctrl Pts',(1.17745134655041,12.2,10.5114820422283));
#226745=CARTESIAN_POINT('Ctrl Pts',(1.17710431345143,12.2,10.5148430455923));
#226746=CARTESIAN_POINT('Ctrl Pts',(1.17674661706342,12.2,10.5182321007983));
#226747=CARTESIAN_POINT('Ctrl Pts',(1.17638892067541,12.2,10.5216211560043));
#226748=CARTESIAN_POINT('Ctrl Pts',(1.17602055993437,12.2,10.5250382622744));
#226749=CARTESIAN_POINT('Ctrl Pts',(1.17564133706896,12.2,10.5284830886251));
#226750=CARTESIAN_POINT('Ctrl Pts',(1.17526211420355,12.2,10.5319279149758));
#226751=CARTESIAN_POINT('Ctrl Pts',(1.17487202939223,12.2,10.5354004607559));
#226752=CARTESIAN_POINT('Ctrl Pts',(1.17447088876781,12.2,10.5389003995045));
#226753=CARTESIAN_POINT('Ctrl Pts',(1.17406974814338,12.2,10.5424003382531));
#226754=CARTESIAN_POINT('Ctrl Pts',(1.17365755116589,12.2,10.5459276703358));
#226755=CARTESIAN_POINT('Ctrl Pts',(1.17323410581927,12.2,10.5494820732509));
#226756=CARTESIAN_POINT('Ctrl Pts',(1.17281066047264,12.2,10.5530364761661));
#226757=CARTESIAN_POINT('Ctrl Pts',(1.17237596858554,12.2,10.5566179510706));
#226758=CARTESIAN_POINT('Ctrl Pts',(1.17192984400021,12.2,10.5602261782397));
#226759=CARTESIAN_POINT('Ctrl Pts',(1.17148371941488,12.2,10.5638344054087));
#226760=CARTESIAN_POINT('Ctrl Pts',(1.17102616084442,12.2,10.5674693866999));
#226761=CARTESIAN_POINT('Ctrl Pts',(1.17055698723331,12.2,10.5711308064916));
#226762=CARTESIAN_POINT('Ctrl Pts',(1.1700878136222,12.2,10.5747922262832));
#226763=CARTESIAN_POINT('Ctrl Pts',(1.16960702440198,12.2,10.5784800877183));
#226764=CARTESIAN_POINT('Ctrl Pts',(1.16911444148304,12.2,10.5821940789853));
#226765=CARTESIAN_POINT('Ctrl Pts',(1.1686218585641,12.2,10.5859080702522));
#226766=CARTESIAN_POINT('Ctrl Pts',(1.16811748120008,12.2,10.5896481926784));
#226767=CARTESIAN_POINT('Ctrl Pts',(1.16760113494947,12.2,10.5934141399714));
#226768=CARTESIAN_POINT('Ctrl Pts',(1.16698151947124,12.2,10.5979332765587));
#226769=CARTESIAN_POINT('Ctrl Pts',(1.16634466898602,12.2,10.6024896024933));
#226770=CARTESIAN_POINT('Ctrl Pts',(1.16569028676057,12.2,10.6070825977414));
#226771=CARTESIAN_POINT('Ctrl Pts',(1.16492684079125,12.2,10.6124410924757));
#226772=CARTESIAN_POINT('Ctrl Pts',(1.1641395360811,12.2,10.6178494954848));
#226773=CARTESIAN_POINT('Ctrl Pts',(1.16332791047032,12.2,10.6233069994883));
#226774=CARTESIAN_POINT('Ctrl Pts',(1.16263223141148,12.2,10.62798485982));
#226775=CARTESIAN_POINT('Ctrl Pts',(1.16191868894575,12.2,10.6326987919569));
#226776=CARTESIAN_POINT('Ctrl Pts',(1.16118699880644,12.2,10.6374482945329));
#226777=CARTESIAN_POINT('Ctrl Pts',(1.16057725700153,12.2,10.64140621349));
#226778=CARTESIAN_POINT('Ctrl Pts',(1.15995491519076,12.2,10.6453888339504));
#226779=CARTESIAN_POINT('Ctrl Pts',(1.15931981331644,12.2,10.6493958695047));
#226780=CARTESIAN_POINT('Ctrl Pts',(1.15868471144211,12.2,10.6534029050589));
#226781=CARTESIAN_POINT('Ctrl Pts',(1.15803685137552,12.2,10.6574343546349));
#226782=CARTESIAN_POINT('Ctrl Pts',(1.15737607623367,12.2,10.6614899359727));
#226783=CARTESIAN_POINT('Ctrl Pts',(1.15671530109181,12.2,10.6655455173105));
#226784=CARTESIAN_POINT('Ctrl Pts',(1.15604161051109,12.2,10.669625228811));
#226785=CARTESIAN_POINT('Ctrl Pts',(1.15535485523331,12.2,10.6737287912416));
#226786=CARTESIAN_POINT('Ctrl Pts',(1.15480545098114,12.2,10.677011641365));
#226787=CARTESIAN_POINT('Ctrl Pts',(1.15424768415023,12.2,10.6803097582206));
#226788=CARTESIAN_POINT('Ctrl Pts',(1.15368147867406,12.2,10.6836229962916));
#226789=CARTESIAN_POINT('Ctrl Pts',(1.15311527327504,12.2,10.6869362339113));
#226790=CARTESIAN_POINT('Ctrl Pts',(1.15254062861643,12.2,10.6902645947669));
#226791=CARTESIAN_POINT('Ctrl Pts',(1.15195747055037,12.2,10.693607937731));
#226792=CARTESIAN_POINT('Ctrl Pts',(1.15137431240486,12.2,10.6969512811505));
#226793=CARTESIAN_POINT('Ctrl Pts',(1.15078264042709,12.2,10.7003096065438));
#226794=CARTESIAN_POINT('Ctrl Pts',(1.1501823808935,12.2,10.7036827752848));
#226795=CARTESIAN_POINT('Ctrl Pts',(1.14958212144169,12.2,10.7070559435661));
#226796=CARTESIAN_POINT('Ctrl Pts',(1.14897327423266,12.2,10.7104439544066));
#226797=CARTESIAN_POINT('Ctrl Pts',(1.14835576628371,12.2,10.7138466712386));
#226798=CARTESIAN_POINT('Ctrl Pts',(1.14773825825063,12.2,10.7172493885341));
#226799=CARTESIAN_POINT('Ctrl Pts',(1.14711208941654,12.2,10.7206668099522));
#226800=CARTESIAN_POINT('Ctrl Pts',(1.1464771891828,12.2,10.7240988002563));
#226801=CARTESIAN_POINT('Ctrl Pts',(1.14584228903557,12.2,10.7275307900929));
#226802=CARTESIAN_POINT('Ctrl Pts',(1.14519865636321,12.2,10.730977347801));
#226803=CARTESIAN_POINT('Ctrl Pts',(1.14454622102823,12.2,10.7344383381838));
#226804=CARTESIAN_POINT('Ctrl Pts',(1.14373067679283,12.2,10.738764576516));
#226805=CARTESIAN_POINT('Ctrl Pts',(1.1429013799932,12.2,10.7431133673376));
#226806=CARTESIAN_POINT('Ctrl Pts',(1.14205819256337,12.2,10.7474844471975));
#226807=CARTESIAN_POINT('Ctrl Pts',(1.14138364258275,12.2,10.7509813112761));
#226808=CARTESIAN_POINT('Ctrl Pts',(1.14070020422257,12.2,10.7544924398559));
#226809=CARTESIAN_POINT('Ctrl Pts',(1.14000780814946,12.2,10.7580177015032));
#226810=CARTESIAN_POINT('Ctrl Pts',(1.13931541217069,12.2,10.7615429626701));
#226811=CARTESIAN_POINT('Ctrl Pts',(1.13861405966597,12.2,10.7650823550093));
#226812=CARTESIAN_POINT('Ctrl Pts',(1.13790368305797,12.2,10.7686357492179));
#226813=CARTESIAN_POINT('Ctrl Pts',(1.13719330635317,12.2,10.7721891439107));
#226814=CARTESIAN_POINT('Ctrl Pts',(1.13647390596397,12.2,10.7757565386328));
#226815=CARTESIAN_POINT('Ctrl Pts',(1.13574541592367,12.2,10.7793378035512));
#226816=CARTESIAN_POINT('Ctrl Pts',(1.13501692598263,12.2,10.7829190679815));
#226817=CARTESIAN_POINT('Ctrl Pts',(1.1342793461143,12.2,10.7865142026728));
#226818=CARTESIAN_POINT('Ctrl Pts',(1.13353261208329,12.2,10.7901230785013));
#226819=CARTESIAN_POINT('Ctrl Pts',(1.13278587795053,12.2,10.7937319548215));
#226820=CARTESIAN_POINT('Ctrl Pts',(1.13202998923243,12.2,10.7973545722149));
#226821=CARTESIAN_POINT('Ctrl Pts',(1.13126488191235,12.2,10.8009908017473));
#226822=CARTESIAN_POINT('Ctrl Pts',(1.13049977469651,12.2,10.8046270307843));
#226823=CARTESIAN_POINT('Ctrl Pts',(1.1297254491103,12.2,10.8082768718408));
#226824=CARTESIAN_POINT('Ctrl Pts',(1.12894184311976,12.2,10.811940197651));
#226825=CARTESIAN_POINT('Ctrl Pts',(1.12815823702246,12.2,10.8156035239603));
#226826=CARTESIAN_POINT('Ctrl Pts',(1.1273653499996,12.2,10.819280337104));
#226827=CARTESIAN_POINT('Ctrl Pts',(1.12656312000776,12.2,10.8229705080441));
#226828=CARTESIAN_POINT('Ctrl Pts',(1.12576089012523,12.2,10.8266606784815));
#226829=CARTESIAN_POINT('Ctrl Pts',(1.12494931716891,12.2,10.8303642080502));
#226830=CARTESIAN_POINT('Ctrl Pts',(1.12412834062587,12.2,10.8340809711339));
#226831=CARTESIAN_POINT('Ctrl Pts',(1.12330736397098,12.2,10.837797734724));
#226832=CARTESIAN_POINT('Ctrl Pts',(1.12247698413465,12.2,10.8415277328543));
#226833=CARTESIAN_POINT('Ctrl Pts',(1.12163714019998,12.2,10.845270839225));
#226834=CARTESIAN_POINT('Ctrl Pts',(1.12079729626531,12.2,10.8490139455957));
#226835=CARTESIAN_POINT('Ctrl Pts',(1.11994798999345,12.2,10.8527701627928));
#226836=CARTESIAN_POINT('Ctrl Pts',(1.11908916066789,12.2,10.8565393663329));
#226837=CARTESIAN_POINT('Ctrl Pts',(1.11801562418647,12.2,10.8612508699876));
#226838=CARTESIAN_POINT('Ctrl Pts',(1.11692720788392,12.2,10.8659826645702));
#226839=CARTESIAN_POINT('Ctrl Pts',(1.1158238006443,12.2,10.8707345116201));
#226840=CARTESIAN_POINT('Ctrl Pts',(1.11494107470829,12.2,10.8745359898815));
#226841=CARTESIAN_POINT('Ctrl Pts',(1.11404875380191,12.2,10.8783503023303));
#226842=CARTESIAN_POINT('Ctrl Pts',(1.11314678180832,12.2,10.8821773273166));
#226843=CARTESIAN_POINT('Ctrl Pts',(1.11224480981472,12.2,10.8860043523029));
#226844=CARTESIAN_POINT('Ctrl Pts',(1.11133318634499,12.2,10.8898440902047));
#226845=CARTESIAN_POINT('Ctrl Pts',(1.11041185384934,12.2,10.8936964211382));
#226846=CARTESIAN_POINT('Ctrl Pts',(1.10949052147921,12.2,10.8975487515468));
#226847=CARTESIAN_POINT('Ctrl Pts',(1.1085594841224,12.2,10.9014136742356));
#226848=CARTESIAN_POINT('Ctrl Pts',(1.10761868175062,12.2,10.905291070714));
#226849=CARTESIAN_POINT('Ctrl Pts',(1.10667787925066,12.2,10.9091684677206));
#226850=CARTESIAN_POINT('Ctrl Pts',(1.10572731496296,12.2,10.9130583395629));
#226851=CARTESIAN_POINT('Ctrl Pts',(1.10476693357629,12.2,10.916960565888));
#226852=CARTESIAN_POINT('Ctrl Pts',(1.10380655232046,12.2,10.9208627916813));
#226853=CARTESIAN_POINT('Ctrl Pts',(1.10283635341036,12.2,10.9247773727592));
#226854=CARTESIAN_POINT('Ctrl Pts',(1.10185628438001,12.2,10.9287041919374));
#226855=CARTESIAN_POINT('Ctrl Pts',(1.10063119799192,12.2,10.9336127163114));
#226856=CARTESIAN_POINT('Ctrl Pts',(1.09939069045902,12.2,10.9385403633886));
#226857=CARTESIAN_POINT('Ctrl Pts',(1.09813465580703,12.2,10.9434869051932));
#226858=CARTESIAN_POINT('Ctrl Pts',(1.09712982803067,12.2,10.9474441388526));
#226859=CARTESIAN_POINT('Ctrl Pts',(1.09611506658692,12.2,10.9514134639803));
#226860=CARTESIAN_POINT('Ctrl Pts',(1.09509031536789,12.2,10.9553947677861));
#226861=CARTESIAN_POINT('Ctrl Pts',(1.09406556428849,12.2,10.9593760710494));
#226862=CARTESIAN_POINT('Ctrl Pts',(1.09303082649089,12.2,10.9633693507425));
#226863=CARTESIAN_POINT('Ctrl Pts',(1.09198605007697,12.2,10.9673744939143));
#226864=CARTESIAN_POINT('Ctrl Pts',(1.09094127352069,12.2,10.9713796376318));
#226865=CARTESIAN_POINT('Ctrl Pts',(1.08988645932708,12.2,10.9753966439952));
#226866=CARTESIAN_POINT('Ctrl Pts',(1.08882155671283,12.2,10.9794253996044));
#226867=CARTESIAN_POINT('Ctrl Pts',(1.08775665424368,12.2,10.9834541546647));
#226868=CARTESIAN_POINT('Ctrl Pts',(1.08668166219425,12.2,10.9874946584668));
#226869=CARTESIAN_POINT('Ctrl Pts',(1.08559653367406,12.2,10.9915467991703));
#226870=CARTESIAN_POINT('Ctrl Pts',(1.08424012291293,12.2,10.9966119754639));
#226871=CARTESIAN_POINT('Ctrl Pts',(1.08286787265651,12.2,11.001695332434));
#226872=CARTESIAN_POINT('Ctrl Pts',(1.08147968786568,12.2,11.0067966526414));
#226873=CARTESIAN_POINT('Ctrl Pts',(1.08036913997248,12.2,11.0108777090298));
#226874=CARTESIAN_POINT('Ctrl Pts',(1.07924839458084,12.2,11.0149702612667));
#226875=CARTESIAN_POINT('Ctrl Pts',(1.07811740340743,12.2,11.0190741996022));
#226876=CARTESIAN_POINT('Ctrl Pts',(1.07698641238811,12.2,11.0231781373786));
#226877=CARTESIAN_POINT('Ctrl Pts',(1.07584517736287,12.2,11.0272934599305));
#226878=CARTESIAN_POINT('Ctrl Pts',(1.07469364840036,12.2,11.0314200574095));
#226879=CARTESIAN_POINT('Ctrl Pts',(1.07296635472125,12.2,11.0376099544714));
#226880=CARTESIAN_POINT('Ctrl Pts',(1.07121590622989,12.2,11.0438252199217));
#226881=CARTESIAN_POINT('Ctrl Pts',(1.06944214454831,12.2,11.0500654854301));
#226882=CARTESIAN_POINT('Ctrl Pts',(1.0682596369217,12.2,11.0542256618689));
#226883=CARTESIAN_POINT('Ctrl Pts',(1.06706676838811,12.2,11.0583969486063));
#226884=CARTESIAN_POINT('Ctrl Pts',(1.06586349459826,12.2,11.0625792383748));
#226885=CARTESIAN_POINT('Ctrl Pts',(1.06466022064445,12.2,11.0667615287132));
#226886=CARTESIAN_POINT('Ctrl Pts',(1.06344654021219,12.2,11.0709548208811));
#226887=CARTESIAN_POINT('Ctrl Pts',(1.06222241030563,12.2,11.0751590088767));
#226888=CARTESIAN_POINT('Ctrl Pts',(1.06099828056586,12.2,11.0793631962996));
#226889=CARTESIAN_POINT('Ctrl Pts',(1.05976370092697,12.2,11.0835782779285));
#226890=CARTESIAN_POINT('Ctrl Pts',(1.05851862791834,12.2,11.0878041471379));
#226891=CARTESIAN_POINT('Ctrl Pts',(1.05727355474007,12.2,11.0920300169231));
#226892=CARTESIAN_POINT('Ctrl Pts',(1.05601798832163,12.2,11.0962666755512));
#226893=CARTESIAN_POINT('Ctrl Pts',(1.05475188569638,12.2,11.1005140148389));
#226894=CARTESIAN_POINT('Ctrl Pts',(1.05348578324364,12.2,11.104761353548));
#226895=CARTESIAN_POINT('Ctrl Pts',(1.05220914389209,12.2,11.1090193758478));
#226896=CARTESIAN_POINT('Ctrl Pts',(1.05092192621171,12.2,11.1132879726556));
#226897=CARTESIAN_POINT('Ctrl Pts',(1.04995651290758,12.2,11.1164894204069));
#226898=CARTESIAN_POINT('Ctrl Pts',(1.04898514899338,12.2,11.119696817267));
#226899=CARTESIAN_POINT('Ctrl Pts',(1.04800781769637,12.2,11.1229101193161));
#226900=CARTESIAN_POINT('Ctrl Pts',(1.04703048622182,12.2,11.126123421949));
#226901=CARTESIAN_POINT('Ctrl Pts',(1.0460471864789,12.2,11.1293426293168));
#226902=CARTESIAN_POINT('Ctrl Pts',(1.04505790150098,12.2,11.132567697453));
#226903=CARTESIAN_POINT('Ctrl Pts',(1.04406861670277,12.2,11.1357927650033));
#226904=CARTESIAN_POINT('Ctrl Pts',(1.04307334650489,12.2,11.1390236930866));
#226905=CARTESIAN_POINT('Ctrl Pts',(1.04207207462408,12.2,11.1422604386362));
#226906=CARTESIAN_POINT('Ctrl Pts',(1.04107080274327,12.2,11.1454971841858));
#226907=CARTESIAN_POINT('Ctrl Pts',(1.04006352811688,12.2,11.1487397468395));
#226908=CARTESIAN_POINT('Ctrl Pts',(1.03905023431573,12.2,11.1519880820279));
#226909=CARTESIAN_POINT('Ctrl Pts',(1.03803694051458,12.2,11.1552364172163));
#226910=CARTESIAN_POINT('Ctrl Pts',(1.03701762670163,12.2,11.158490526884));
#226911=CARTESIAN_POINT('Ctrl Pts',(1.03599227744259,12.2,11.1617503659886));
#226912=CARTESIAN_POINT('Ctrl Pts',(1.03496692818354,12.2,11.1650102050933));
#226913=CARTESIAN_POINT('Ctrl Pts',(1.03393554260807,12.2,11.1682757738462));
#226914=CARTESIAN_POINT('Ctrl Pts',(1.03289810481297,12.2,11.1715470293935));
#226915=CARTESIAN_POINT('Ctrl Pts',(1.03186066701787,12.2,11.1748182849407));
#226916=CARTESIAN_POINT('Ctrl Pts',(1.03081717702315,12.2,11.1780952270377));
#226917=CARTESIAN_POINT('Ctrl Pts',(1.02976761772878,12.2,11.1813778135844));
#226918=CARTESIAN_POINT('Ctrl Pts',(1.02871805824375,12.2,11.1846604007273));
#226919=CARTESIAN_POINT('Ctrl Pts',(1.027662429207,12.2,11.1879486312052));
#226920=CARTESIAN_POINT('Ctrl Pts',(1.02660071576019,12.2,11.1912424624347));
#226921=CARTESIAN_POINT('Ctrl Pts',(1.02553900250626,12.2,11.1945362930658));
#226922=CARTESIAN_POINT('Ctrl Pts',(1.0244712051075,12.2,11.1978357251937));
#226923=CARTESIAN_POINT('Ctrl Pts',(1.02339730580049,12.2,11.2011407159061));
#226924=CARTESIAN_POINT('Ctrl Pts',(1.02196544012284,12.2,11.2055473699891));
#226925=CARTESIAN_POINT('Ctrl Pts',(1.02052272801306,12.2,11.2099639052174));
#226926=CARTESIAN_POINT('Ctrl Pts',(1.01906913307705,12.2,11.2143902211882));
#226927=CARTESIAN_POINT('Ctrl Pts',(1.01797893682553,12.2,11.2177099583171));
#226928=CARTESIAN_POINT('Ctrl Pts',(1.01688261823276,12.2,11.2210351974956));
#226929=CARTESIAN_POINT('Ctrl Pts',(1.01578016248198,12.2,11.2243658970405));
#226930=CARTESIAN_POINT('Ctrl Pts',(1.01467770653093,12.2,11.2276965971905));
#226931=CARTESIAN_POINT('Ctrl Pts',(1.01356911398648,12.2,11.2310327560754));
#226932=CARTESIAN_POINT('Ctrl Pts',(1.01245436803196,12.2,11.2343743337284));
#226933=CARTESIAN_POINT('Ctrl Pts',(1.01133962227995,12.2,11.2377159107744));
#226934=CARTESIAN_POINT('Ctrl Pts',(1.01021872309793,12.2,11.241062905319));
#226935=CARTESIAN_POINT('Ctrl Pts',(1.0090916567902,12.2,11.2444152756569));
#226936=CARTESIAN_POINT('Ctrl Pts',(1.00758890178147,12.2,11.2488851025712));
#226937=CARTESIAN_POINT('Ctrl Pts',(1.00607518097694,12.2,11.2533644885868));
#226938=CARTESIAN_POINT('Ctrl Pts',(1.00455046065786,12.2,11.2578533326081));
#226939=CARTESIAN_POINT('Ctrl Pts',(1.00340692036662,12.2,11.261219965777));
#226940=CARTESIAN_POINT('Ctrl Pts',(1.00225719220913,12.2,11.2645919195371));
#226941=CARTESIAN_POINT('Ctrl Pts',(1.00110126150197,12.2,11.2679691527054));
#226942=CARTESIAN_POINT('Ctrl Pts',(0.999945330584818,12.2,11.2713463864872));
#226943=CARTESIAN_POINT('Ctrl Pts',(0.998783197665939,12.2,11.2747289007621));
#226944=CARTESIAN_POINT('Ctrl Pts',(0.99761484728694,12.2,11.2781166529635));
#226945=CARTESIAN_POINT('Ctrl Pts',(0.996446497120191,12.2,11.2815044045495));
#226946=CARTESIAN_POINT('Ctrl Pts',(0.995271930528823,12.2,11.2848973937601));
#226947=CARTESIAN_POINT('Ctrl Pts',(0.994091132362839,12.2,11.2882955808454));
#226948=CARTESIAN_POINT('Ctrl Pts',(0.992910334196854,12.2,11.2916937679308));
#226949=CARTESIAN_POINT('Ctrl Pts',(0.991723305177649,12.2,11.2950971526781));
#226950=CARTESIAN_POINT('Ctrl Pts',(0.990530030007237,12.2,11.298505694278));
#226951=CARTESIAN_POINT('Ctrl Pts',(0.98893899651895,12.2,11.3030504162049));
#226952=CARTESIAN_POINT('Ctrl Pts',(0.987336860464056,12.2,11.3076043057307));
#226953=CARTESIAN_POINT('Ctrl Pts',(0.985723588263753,12.2,11.3121672657456));
#226954=CARTESIAN_POINT('Ctrl Pts',(0.984513633838765,12.2,11.3155894865339));
#226955=CARTESIAN_POINT('Ctrl Pts',(0.983297415128669,12.2,11.3190168102487));
#226956=CARTESIAN_POINT('Ctrl Pts',(0.982074918700141,12.2,11.3224491964982));
#226957=CARTESIAN_POINT('Ctrl Pts',(0.980444923832249,12.2,11.3270257104583));
#226958=CARTESIAN_POINT('Ctrl Pts',(0.97880376851027,12.2,11.33161122437));
#226959=CARTESIAN_POINT('Ctrl Pts',(0.977151420868294,12.2,11.3362056423828));
#226960=CARTESIAN_POINT('Ctrl Pts',(0.975912160080528,12.2,11.3396514560488));
#226961=CARTESIAN_POINT('Ctrl Pts',(0.974666602375131,12.2,11.3431022787349));
#226962=CARTESIAN_POINT('Ctrl Pts',(0.973414736525461,12.2,11.3465580705731));
#226963=CARTESIAN_POINT('Ctrl Pts',(0.972162870675792,12.2,11.3500138624113));
#226964=CARTESIAN_POINT('Ctrl Pts',(0.970904695462171,12.2,11.353474623571));
#226965=CARTESIAN_POINT('Ctrl Pts',(0.969640197300644,12.2,11.3569403127361));
#226966=CARTESIAN_POINT('Ctrl Pts',(0.968375698909399,12.2,11.3604060025308));
#226967=CARTESIAN_POINT('Ctrl Pts',(0.967104877574688,12.2,11.3638766215186));
#226968=CARTESIAN_POINT('Ctrl Pts',(0.965827721179895,12.2,11.367352130316));
#226969=CARTESIAN_POINT('Ctrl Pts',(0.964124846373533,12.2,11.3719861409935));
#226970=CARTESIAN_POINT('Ctrl Pts',(0.962410709804703,12.2,11.3766288450867));
#226971=CARTESIAN_POINT('Ctrl Pts',(0.960685278390935,12.2,11.3812801490948));
#226972=CARTESIAN_POINT('Ctrl Pts',(0.959391204771838,12.2,11.3847686272593));
#226973=CARTESIAN_POINT('Ctrl Pts',(0.95809078006983,12.2,11.3882619435928));
#226974=CARTESIAN_POINT('Ctrl Pts',(0.956783988802754,12.2,11.3917600568065));
#226975=CARTESIAN_POINT('Ctrl Pts',(0.955477197535678,12.2,11.3952581700203));
#226976=CARTESIAN_POINT('Ctrl Pts',(0.954164039455502,12.2,11.39876107833));
#226977=CARTESIAN_POINT('Ctrl Pts',(0.952844504295974,12.2,11.4022687450353));
#226978=CARTESIAN_POINT('Ctrl Pts',(0.951524968896731,12.2,11.4057764123778));
#226979=CARTESIAN_POINT('Ctrl Pts',(0.950199055770689,12.2,11.4092888386549));
#226980=CARTESIAN_POINT('Ctrl Pts',(0.948866752951208,12.2,11.412805988));
#226981=CARTESIAN_POINT('Ctrl Pts',(0.947534450373763,12.2,11.4163231367062));
#226982=CARTESIAN_POINT('Ctrl Pts',(0.946195759771612,12.2,11.4198450094288));
#226983=CARTESIAN_POINT('Ctrl Pts',(0.944850667069934,12.2,11.4233715654261));
#226984=CARTESIAN_POINT('Ctrl Pts',(0.943505574368256,12.2,11.4268981214234));
#226985=CARTESIAN_POINT('Ctrl Pts',(0.942154079472279,12.2,11.4304293594156));
#226986=CARTESIAN_POINT('Ctrl Pts',(0.940796167723754,12.2,11.4339652325115));
#226987=CARTESIAN_POINT('Ctrl Pts',(0.938532981393982,12.2,11.4398583545522));
#226988=CARTESIAN_POINT('Ctrl Pts',(0.936251965069451,12.2,11.4457643374802));
#226989=CARTESIAN_POINT('Ctrl Pts',(0.933953084118917,12.2,11.4516830612001));
#226990=CARTESIAN_POINT('Ctrl Pts',(0.932573755598712,12.2,11.4552342953029));
#226991=CARTESIAN_POINT('Ctrl Pts',(0.931187998930692,12.2,11.4587901206197));
#226992=CARTESIAN_POINT('Ctrl Pts',(0.929795807999944,12.2,11.462350533));
#226993=CARTESIAN_POINT('Origin',(-5.66257110645729E-14,15.2,-1.77635683940025E-14));
#226994=CARTESIAN_POINT('',(-0.292001929325956,15.2,10.370890023736));
#226995=CARTESIAN_POINT('',(-0.292001929325956,12.2,10.370890023736));
#226996=CARTESIAN_POINT('',(-0.292001929000056,15.2,10.370890024));
#226997=CARTESIAN_POINT('Origin',(-5.66257110645729E-14,12.2,-1.77635683940025E-14));
#226998=CARTESIAN_POINT('Origin',(-5.66257110645729E-14,15.2,-1.77635683940025E-14));
#226999=CARTESIAN_POINT('Origin',(-5.66257110645729E-14,15.2,-1.77635683940025E-14));
#227000=CARTESIAN_POINT('',(-0.710930735000056,15.2,11.478004073));
#227001=CARTESIAN_POINT('',(-1.09337743000006,15.2,11.447904865));
#227002=CARTESIAN_POINT('Origin',(-5.66257110645729E-14,15.2,-1.77635683940025E-14));
#227003=CARTESIAN_POINT('',(-1.09337743000006,12.2,11.447904865));
#227004=CARTESIAN_POINT('',(-1.09337743000006,15.2,11.447904865));
#227005=CARTESIAN_POINT('',(-0.710930735000056,12.2,11.478004073));
#227006=CARTESIAN_POINT('Origin',(-5.66257110645729E-14,12.2,-1.77635683940025E-14));
#227007=CARTESIAN_POINT('',(-0.710930735000056,15.2,11.478004073));
#227008=CARTESIAN_POINT('Ctrl Pts',(-0.292001930000056,15.2,10.370890024));
#227009=CARTESIAN_POINT('Ctrl Pts',(-0.292001930000056,11.6,10.370890024));
#227010=CARTESIAN_POINT('Ctrl Pts',(-0.292021796000055,15.2,10.371063246));
#227011=CARTESIAN_POINT('Ctrl Pts',(-0.292021796000055,11.6,10.371063246));
#227012=CARTESIAN_POINT('Ctrl Pts',(-0.292062309000055,15.2,10.371415731));
#227013=CARTESIAN_POINT('Ctrl Pts',(-0.292062309000055,11.6,10.371415731));
#227014=CARTESIAN_POINT('Ctrl Pts',(-0.292123962000056,15.2,10.3719498));
#227015=CARTESIAN_POINT('Ctrl Pts',(-0.292123962000056,11.6,10.3719498));
#227016=CARTESIAN_POINT('Ctrl Pts',(-0.292207548000055,15.2,10.372669177));
#227017=CARTESIAN_POINT('Ctrl Pts',(-0.292207548000055,11.6,10.372669177));
#227018=CARTESIAN_POINT('Ctrl Pts',(-0.292314181000056,15.2,10.373578975));
#227019=CARTESIAN_POINT('Ctrl Pts',(-0.292314181000056,11.6,10.373578975));
#227020=CARTESIAN_POINT('Ctrl Pts',(-0.292423470000056,15.2,10.374503411));
#227021=CARTESIAN_POINT('Ctrl Pts',(-0.292423470000056,11.6,10.374503411));
#227022=CARTESIAN_POINT('Ctrl Pts',(-0.292534812000056,15.2,10.375437185));
#227023=CARTESIAN_POINT('Ctrl Pts',(-0.292534812000056,11.6,10.375437185));
#227024=CARTESIAN_POINT('Ctrl Pts',(-0.292648223000055,15.2,10.376380267));
#227025=CARTESIAN_POINT('Ctrl Pts',(-0.292648223000055,11.6,10.376380267));
#227026=CARTESIAN_POINT('Ctrl Pts',(-0.292763718000056,15.2,10.377332628));
#227027=CARTESIAN_POINT('Ctrl Pts',(-0.292763718000056,11.6,10.377332628));
#227028=CARTESIAN_POINT('Ctrl Pts',(-0.292881311000055,15.2,10.37829424));
#227029=CARTESIAN_POINT('Ctrl Pts',(-0.292881311000055,11.6,10.37829424));
#227030=CARTESIAN_POINT('Ctrl Pts',(-0.293001016000056,15.2,10.379265074));
#227031=CARTESIAN_POINT('Ctrl Pts',(-0.293001016000056,11.6,10.379265074));
#227032=CARTESIAN_POINT('Ctrl Pts',(-0.293122847000056,15.2,10.380245102));
#227033=CARTESIAN_POINT('Ctrl Pts',(-0.293122847000056,11.6,10.380245102));
#227034=CARTESIAN_POINT('Ctrl Pts',(-0.293246820000055,15.2,10.381234296));
#227035=CARTESIAN_POINT('Ctrl Pts',(-0.293246820000055,11.6,10.381234296));
#227036=CARTESIAN_POINT('Ctrl Pts',(-0.293372949000055,15.2,10.382232628));
#227037=CARTESIAN_POINT('Ctrl Pts',(-0.293372949000055,11.6,10.382232628));
#227038=CARTESIAN_POINT('Ctrl Pts',(-0.293501249000055,15.2,10.383240069));
#227039=CARTESIAN_POINT('Ctrl Pts',(-0.293501249000055,11.6,10.383240069));
#227040=CARTESIAN_POINT('Ctrl Pts',(-0.293631732000056,15.2,10.384256592));
#227041=CARTESIAN_POINT('Ctrl Pts',(-0.293631732000056,11.6,10.384256592));
#227042=CARTESIAN_POINT('Ctrl Pts',(-0.293764414000056,15.2,10.385282169));
#227043=CARTESIAN_POINT('Ctrl Pts',(-0.293764414000056,11.6,10.385282169));
#227044=CARTESIAN_POINT('Ctrl Pts',(-0.293899307000055,15.2,10.38631677));
#227045=CARTESIAN_POINT('Ctrl Pts',(-0.293899307000055,11.6,10.38631677));
#227046=CARTESIAN_POINT('Ctrl Pts',(-0.294036428000056,15.2,10.387360372));
#227047=CARTESIAN_POINT('Ctrl Pts',(-0.294036428000056,11.6,10.387360372));
#227048=CARTESIAN_POINT('Ctrl Pts',(-0.294175788000055,15.2,10.388412944));
#227049=CARTESIAN_POINT('Ctrl Pts',(-0.294175788000055,11.6,10.388412944));
#227050=CARTESIAN_POINT('Ctrl Pts',(-0.294317401000056,15.2,10.389474461));
#227051=CARTESIAN_POINT('Ctrl Pts',(-0.294317401000056,11.6,10.389474461));
#227052=CARTESIAN_POINT('Ctrl Pts',(-0.294461282000055,15.2,10.390544895));
#227053=CARTESIAN_POINT('Ctrl Pts',(-0.294461282000055,11.6,10.390544895));
#227054=CARTESIAN_POINT('Ctrl Pts',(-0.294607445000056,15.2,10.391624218));
#227055=CARTESIAN_POINT('Ctrl Pts',(-0.294607445000056,11.6,10.391624218));
#227056=CARTESIAN_POINT('Ctrl Pts',(-0.294755901000056,15.2,10.392712405));
#227057=CARTESIAN_POINT('Ctrl Pts',(-0.294755901000056,11.6,10.392712405));
#227058=CARTESIAN_POINT('Ctrl Pts',(-0.294906666000055,15.2,10.393809428));
#227059=CARTESIAN_POINT('Ctrl Pts',(-0.294906666000055,11.6,10.393809428));
#227060=CARTESIAN_POINT('Ctrl Pts',(-0.295059753000055,15.2,10.39491526));
#227061=CARTESIAN_POINT('Ctrl Pts',(-0.295059753000055,11.6,10.39491526));
#227062=CARTESIAN_POINT('Ctrl Pts',(-0.295215174000055,15.2,10.396029876));
#227063=CARTESIAN_POINT('Ctrl Pts',(-0.295215174000055,11.6,10.396029876));
#227064=CARTESIAN_POINT('Ctrl Pts',(-0.295372942000055,15.2,10.397153247));
#227065=CARTESIAN_POINT('Ctrl Pts',(-0.295372942000055,11.6,10.397153247));
#227066=CARTESIAN_POINT('Ctrl Pts',(-0.295533072000056,15.2,10.398285351));
#227067=CARTESIAN_POINT('Ctrl Pts',(-0.295533072000056,11.6,10.398285351));
#227068=CARTESIAN_POINT('Ctrl Pts',(-0.295695577000057,15.2,10.399426157));
#227069=CARTESIAN_POINT('Ctrl Pts',(-0.295695577000057,11.6,10.399426157));
#227070=CARTESIAN_POINT('Ctrl Pts',(-0.295860468000055,15.2,10.400575642));
#227071=CARTESIAN_POINT('Ctrl Pts',(-0.295860468000055,11.6,10.400575642));
#227072=CARTESIAN_POINT('Ctrl Pts',(-0.296027759000056,15.2,10.401733779));
#227073=CARTESIAN_POINT('Ctrl Pts',(-0.296027759000056,11.6,10.401733779));
#227074=CARTESIAN_POINT('Ctrl Pts',(-0.296197463000055,15.2,10.402900543));
#227075=CARTESIAN_POINT('Ctrl Pts',(-0.296197463000055,11.6,10.402900543));
#227076=CARTESIAN_POINT('Ctrl Pts',(-0.296369593000056,15.2,10.404075907));
#227077=CARTESIAN_POINT('Ctrl Pts',(-0.296369593000056,11.6,10.404075907));
#227078=CARTESIAN_POINT('Ctrl Pts',(-0.296544162000056,15.2,10.405259846));
#227079=CARTESIAN_POINT('Ctrl Pts',(-0.296544162000056,11.6,10.405259846));
#227080=CARTESIAN_POINT('Ctrl Pts',(-0.296721182000056,15.2,10.406452335));
#227081=CARTESIAN_POINT('Ctrl Pts',(-0.296721182000056,11.6,10.406452335));
#227082=CARTESIAN_POINT('Ctrl Pts',(-0.296900665000056,15.2,10.407653348));
#227083=CARTESIAN_POINT('Ctrl Pts',(-0.296900665000056,11.6,10.407653348));
#227084=CARTESIAN_POINT('Ctrl Pts',(-0.297082625000057,15.2,10.408862859));
#227085=CARTESIAN_POINT('Ctrl Pts',(-0.297082625000057,11.6,10.408862859));
#227086=CARTESIAN_POINT('Ctrl Pts',(-0.297267073000055,15.2,10.410080845));
#227087=CARTESIAN_POINT('Ctrl Pts',(-0.297267073000055,11.6,10.410080845));
#227088=CARTESIAN_POINT('Ctrl Pts',(-0.297454022000055,15.2,10.411307279));
#227089=CARTESIAN_POINT('Ctrl Pts',(-0.297454022000055,11.6,10.411307279));
#227090=CARTESIAN_POINT('Ctrl Pts',(-0.297643484000056,15.2,10.412542136));
#227091=CARTESIAN_POINT('Ctrl Pts',(-0.297643484000056,11.6,10.412542136));
#227092=CARTESIAN_POINT('Ctrl Pts',(-0.297835473000055,15.2,10.413785393));
#227093=CARTESIAN_POINT('Ctrl Pts',(-0.297835473000055,11.6,10.413785393));
#227094=CARTESIAN_POINT('Ctrl Pts',(-0.298029998000056,15.2,10.415037024));
#227095=CARTESIAN_POINT('Ctrl Pts',(-0.298029998000056,11.6,10.415037024));
#227096=CARTESIAN_POINT('Ctrl Pts',(-0.298227074000056,15.2,10.416297004));
#227097=CARTESIAN_POINT('Ctrl Pts',(-0.298227074000056,11.6,10.416297004));
#227098=CARTESIAN_POINT('Ctrl Pts',(-0.298426711000056,15.2,10.41756531));
#227099=CARTESIAN_POINT('Ctrl Pts',(-0.298426711000056,11.6,10.41756531));
#227100=CARTESIAN_POINT('Ctrl Pts',(-0.298628923000056,15.2,10.418841915));
#227101=CARTESIAN_POINT('Ctrl Pts',(-0.298628923000056,11.6,10.418841915));
#227102=CARTESIAN_POINT('Ctrl Pts',(-0.298833720000056,15.2,10.420126797));
#227103=CARTESIAN_POINT('Ctrl Pts',(-0.298833720000056,11.6,10.420126797));
#227104=CARTESIAN_POINT('Ctrl Pts',(-0.299041114000056,15.2,10.42141993));
#227105=CARTESIAN_POINT('Ctrl Pts',(-0.299041114000056,11.6,10.42141993));
#227106=CARTESIAN_POINT('Ctrl Pts',(-0.299251119000056,15.2,10.422721291));
#227107=CARTESIAN_POINT('Ctrl Pts',(-0.299251119000056,11.6,10.422721291));
#227108=CARTESIAN_POINT('Ctrl Pts',(-0.299463743000056,15.2,10.424030857));
#227109=CARTESIAN_POINT('Ctrl Pts',(-0.299463743000056,11.6,10.424030857));
#227110=CARTESIAN_POINT('Ctrl Pts',(-0.299679001000056,15.2,10.425348601));
#227111=CARTESIAN_POINT('Ctrl Pts',(-0.299679001000056,11.6,10.425348601));
#227112=CARTESIAN_POINT('Ctrl Pts',(-0.299896903000055,15.2,10.426674502));
#227113=CARTESIAN_POINT('Ctrl Pts',(-0.299896903000055,11.6,10.426674502));
#227114=CARTESIAN_POINT('Ctrl Pts',(-0.300117461000056,15.2,10.428008535));
#227115=CARTESIAN_POINT('Ctrl Pts',(-0.300117461000056,11.6,10.428008535));
#227116=CARTESIAN_POINT('Ctrl Pts',(-0.300340687000055,15.2,10.429350676));
#227117=CARTESIAN_POINT('Ctrl Pts',(-0.300340687000055,11.6,10.429350676));
#227118=CARTESIAN_POINT('Ctrl Pts',(-0.300566590000055,15.2,10.430700903));
#227119=CARTESIAN_POINT('Ctrl Pts',(-0.300566590000055,11.6,10.430700903));
#227120=CARTESIAN_POINT('Ctrl Pts',(-0.300795185000055,15.2,10.432059191));
#227121=CARTESIAN_POINT('Ctrl Pts',(-0.300795185000055,11.6,10.432059191));
#227122=CARTESIAN_POINT('Ctrl Pts',(-0.301026480000056,15.2,10.433425517));
#227123=CARTESIAN_POINT('Ctrl Pts',(-0.301026480000056,11.6,10.433425517));
#227124=CARTESIAN_POINT('Ctrl Pts',(-0.301260488000056,15.2,10.434799857));
#227125=CARTESIAN_POINT('Ctrl Pts',(-0.301260488000056,11.6,10.434799857));
#227126=CARTESIAN_POINT('Ctrl Pts',(-0.301497220000057,15.2,10.43618219));
#227127=CARTESIAN_POINT('Ctrl Pts',(-0.301497220000057,11.6,10.43618219));
#227128=CARTESIAN_POINT('Ctrl Pts',(-0.301736686000057,15.2,10.437572491));
#227129=CARTESIAN_POINT('Ctrl Pts',(-0.301736686000057,11.6,10.437572491));
#227130=CARTESIAN_POINT('Ctrl Pts',(-0.301978899000056,15.2,10.438970738));
#227131=CARTESIAN_POINT('Ctrl Pts',(-0.301978899000056,11.6,10.438970738));
#227132=CARTESIAN_POINT('Ctrl Pts',(-0.302223868000056,15.2,10.440376907));
#227133=CARTESIAN_POINT('Ctrl Pts',(-0.302223868000056,11.6,10.440376907));
#227134=CARTESIAN_POINT('Ctrl Pts',(-0.302471605000055,15.2,10.441790977));
#227135=CARTESIAN_POINT('Ctrl Pts',(-0.302471605000055,11.6,10.441790977));
#227136=CARTESIAN_POINT('Ctrl Pts',(-0.302722121000055,15.2,10.443212923));
#227137=CARTESIAN_POINT('Ctrl Pts',(-0.302722121000055,11.6,10.443212923));
#227138=CARTESIAN_POINT('Ctrl Pts',(-0.302975427000056,15.2,10.444642724));
#227139=CARTESIAN_POINT('Ctrl Pts',(-0.302975427000056,11.6,10.444642724));
#227140=CARTESIAN_POINT('Ctrl Pts',(-0.303231532000057,15.2,10.446080358));
#227141=CARTESIAN_POINT('Ctrl Pts',(-0.303231532000057,11.6,10.446080358));
#227142=CARTESIAN_POINT('Ctrl Pts',(-0.303490448000057,15.2,10.4475258));
#227143=CARTESIAN_POINT('Ctrl Pts',(-0.303490448000057,11.6,10.4475258));
#227144=CARTESIAN_POINT('Ctrl Pts',(-0.303752187000056,15.2,10.44897903));
#227145=CARTESIAN_POINT('Ctrl Pts',(-0.303752187000056,11.6,10.44897903));
#227146=CARTESIAN_POINT('Ctrl Pts',(-0.304016757000056,15.2,10.450440024));
#227147=CARTESIAN_POINT('Ctrl Pts',(-0.304016757000056,11.6,10.450440024));
#227148=CARTESIAN_POINT('Ctrl Pts',(-0.304284170000055,15.2,10.451908761));
#227149=CARTESIAN_POINT('Ctrl Pts',(-0.304284170000055,11.6,10.451908761));
#227150=CARTESIAN_POINT('Ctrl Pts',(-0.304554437000055,15.2,10.453385219));
#227151=CARTESIAN_POINT('Ctrl Pts',(-0.304554437000055,11.6,10.453385219));
#227152=CARTESIAN_POINT('Ctrl Pts',(-0.304827566000055,15.2,10.454869375));
#227153=CARTESIAN_POINT('Ctrl Pts',(-0.304827566000055,11.6,10.454869375));
#227154=CARTESIAN_POINT('Ctrl Pts',(-0.305103570000057,15.2,10.456361207));
#227155=CARTESIAN_POINT('Ctrl Pts',(-0.305103570000057,11.6,10.456361207));
#227156=CARTESIAN_POINT('Ctrl Pts',(-0.305382458000055,15.2,10.457860694));
#227157=CARTESIAN_POINT('Ctrl Pts',(-0.305382458000055,11.6,10.457860694));
#227158=CARTESIAN_POINT('Ctrl Pts',(-0.305664241000055,15.2,10.459367814));
#227159=CARTESIAN_POINT('Ctrl Pts',(-0.305664241000055,11.6,10.459367814));
#227160=CARTESIAN_POINT('Ctrl Pts',(-0.305948929000056,15.2,10.460882546));
#227161=CARTESIAN_POINT('Ctrl Pts',(-0.305948929000056,11.6,10.460882546));
#227162=CARTESIAN_POINT('Ctrl Pts',(-0.306236530000056,15.2,10.462404866));
#227163=CARTESIAN_POINT('Ctrl Pts',(-0.306236530000056,11.6,10.462404866));
#227164=CARTESIAN_POINT('Ctrl Pts',(-0.306527058000056,15.2,10.463934755));
#227165=CARTESIAN_POINT('Ctrl Pts',(-0.306527058000056,11.6,10.463934755));
#227166=CARTESIAN_POINT('Ctrl Pts',(-0.306820521000055,15.2,10.465472191));
#227167=CARTESIAN_POINT('Ctrl Pts',(-0.306820521000055,11.6,10.465472191));
#227168=CARTESIAN_POINT('Ctrl Pts',(-0.307116929000056,15.2,10.467017151));
#227169=CARTESIAN_POINT('Ctrl Pts',(-0.307116929000056,11.6,10.467017151));
#227170=CARTESIAN_POINT('Ctrl Pts',(-0.307416292000056,15.2,10.468569615));
#227171=CARTESIAN_POINT('Ctrl Pts',(-0.307416292000056,11.6,10.468569615));
#227172=CARTESIAN_POINT('Ctrl Pts',(-0.307718620000056,15.2,10.470129562));
#227173=CARTESIAN_POINT('Ctrl Pts',(-0.307718620000056,11.6,10.470129562));
#227174=CARTESIAN_POINT('Ctrl Pts',(-0.308023922000055,15.2,10.47169697));
#227175=CARTESIAN_POINT('Ctrl Pts',(-0.308023922000055,11.6,10.47169697));
#227176=CARTESIAN_POINT('Ctrl Pts',(-0.308332210000056,15.2,10.473271818));
#227177=CARTESIAN_POINT('Ctrl Pts',(-0.308332210000056,11.6,10.473271818));
#227178=CARTESIAN_POINT('Ctrl Pts',(-0.308643491000057,15.2,10.474854086));
#227179=CARTESIAN_POINT('Ctrl Pts',(-0.308643491000057,11.6,10.474854086));
#227180=CARTESIAN_POINT('Ctrl Pts',(-0.308957777000056,15.2,10.476443753));
#227181=CARTESIAN_POINT('Ctrl Pts',(-0.308957777000056,11.6,10.476443753));
#227182=CARTESIAN_POINT('Ctrl Pts',(-0.309275077000055,15.2,10.478040797));
#227183=CARTESIAN_POINT('Ctrl Pts',(-0.309275077000055,11.6,10.478040797));
#227184=CARTESIAN_POINT('Ctrl Pts',(-0.309595400000056,15.2,10.479645197));
#227185=CARTESIAN_POINT('Ctrl Pts',(-0.309595400000056,11.6,10.479645197));
#227186=CARTESIAN_POINT('Ctrl Pts',(-0.309918755000057,15.2,10.481256935));
#227187=CARTESIAN_POINT('Ctrl Pts',(-0.309918755000057,11.6,10.481256935));
#227188=CARTESIAN_POINT('Ctrl Pts',(-0.310245153000055,15.2,10.482875987));
#227189=CARTESIAN_POINT('Ctrl Pts',(-0.310245153000055,11.6,10.482875987));
#227190=CARTESIAN_POINT('Ctrl Pts',(-0.310574603000056,15.2,10.484502335));
#227191=CARTESIAN_POINT('Ctrl Pts',(-0.310574603000056,11.6,10.484502335));
#227192=CARTESIAN_POINT('Ctrl Pts',(-0.310907114000055,15.2,10.486135956));
#227193=CARTESIAN_POINT('Ctrl Pts',(-0.310907114000055,11.6,10.486135956));
#227194=CARTESIAN_POINT('Ctrl Pts',(-0.311242695000056,15.2,10.487776833));
#227195=CARTESIAN_POINT('Ctrl Pts',(-0.311242695000056,11.6,10.487776833));
#227196=CARTESIAN_POINT('Ctrl Pts',(-0.311581357000056,15.2,10.489424943));
#227197=CARTESIAN_POINT('Ctrl Pts',(-0.311581357000056,11.6,10.489424943));
#227198=CARTESIAN_POINT('Ctrl Pts',(-0.311923108000055,15.2,10.491080266));
#227199=CARTESIAN_POINT('Ctrl Pts',(-0.311923108000055,11.6,10.491080266));
#227200=CARTESIAN_POINT('Ctrl Pts',(-0.312267957000056,15.2,10.492742783));
#227201=CARTESIAN_POINT('Ctrl Pts',(-0.312267957000056,11.6,10.492742783));
#227202=CARTESIAN_POINT('Ctrl Pts',(-0.312615913000055,15.2,10.494412473));
#227203=CARTESIAN_POINT('Ctrl Pts',(-0.312615913000055,11.6,10.494412473));
#227204=CARTESIAN_POINT('Ctrl Pts',(-0.312966986000056,15.2,10.496089317));
#227205=CARTESIAN_POINT('Ctrl Pts',(-0.312966986000056,11.6,10.496089317));
#227206=CARTESIAN_POINT('Ctrl Pts',(-0.313321186000056,15.2,10.497773292));
#227207=CARTESIAN_POINT('Ctrl Pts',(-0.313321186000056,11.6,10.497773292));
#227208=CARTESIAN_POINT('Ctrl Pts',(-0.313678519000057,15.2,10.499464382));
#227209=CARTESIAN_POINT('Ctrl Pts',(-0.313678519000057,11.6,10.499464382));
#227210=CARTESIAN_POINT('Ctrl Pts',(-0.314038998000056,15.2,10.501162565));
#227211=CARTESIAN_POINT('Ctrl Pts',(-0.314038998000056,11.6,10.501162565));
#227212=CARTESIAN_POINT('Ctrl Pts',(-0.314402627000057,15.2,10.502867822));
#227213=CARTESIAN_POINT('Ctrl Pts',(-0.314402627000057,11.6,10.502867822));
#227214=CARTESIAN_POINT('Ctrl Pts',(-0.314769419000056,15.2,10.504580133));
#227215=CARTESIAN_POINT('Ctrl Pts',(-0.314769419000056,11.6,10.504580133));
#227216=CARTESIAN_POINT('Ctrl Pts',(-0.315139383000057,15.2,10.506299478));
#227217=CARTESIAN_POINT('Ctrl Pts',(-0.315139383000057,11.6,10.506299478));
#227218=CARTESIAN_POINT('Ctrl Pts',(-0.315512524000056,15.2,10.508025839));
#227219=CARTESIAN_POINT('Ctrl Pts',(-0.315512524000056,11.6,10.508025839));
#227220=CARTESIAN_POINT('Ctrl Pts',(-0.315888854000056,15.2,10.509759194));
#227221=CARTESIAN_POINT('Ctrl Pts',(-0.315888854000056,11.6,10.509759194));
#227222=CARTESIAN_POINT('Ctrl Pts',(-0.316268381000055,15.2,10.511499524));
#227223=CARTESIAN_POINT('Ctrl Pts',(-0.316268381000055,11.6,10.511499524));
#227224=CARTESIAN_POINT('Ctrl Pts',(-0.316651113000056,15.2,10.513246813));
#227225=CARTESIAN_POINT('Ctrl Pts',(-0.316651113000056,11.6,10.513246813));
#227226=CARTESIAN_POINT('Ctrl Pts',(-0.317037059000055,15.2,10.515001037));
#227227=CARTESIAN_POINT('Ctrl Pts',(-0.317037059000055,11.6,10.515001037));
#227228=CARTESIAN_POINT('Ctrl Pts',(-0.317426228000055,15.2,10.51676218));
#227229=CARTESIAN_POINT('Ctrl Pts',(-0.317426228000055,11.6,10.51676218));
#227230=CARTESIAN_POINT('Ctrl Pts',(-0.317818629000056,15.2,10.518530221));
#227231=CARTESIAN_POINT('Ctrl Pts',(-0.317818629000056,11.6,10.518530221));
#227232=CARTESIAN_POINT('Ctrl Pts',(-0.318214269000056,15.2,10.520305142));
#227233=CARTESIAN_POINT('Ctrl Pts',(-0.318214269000056,11.6,10.520305142));
#227234=CARTESIAN_POINT('Ctrl Pts',(-0.318613157000056,15.2,10.522086924));
#227235=CARTESIAN_POINT('Ctrl Pts',(-0.318613157000056,11.6,10.522086924));
#227236=CARTESIAN_POINT('Ctrl Pts',(-0.319015302000055,15.2,10.523875548));
#227237=CARTESIAN_POINT('Ctrl Pts',(-0.319015302000055,11.6,10.523875548));
#227238=CARTESIAN_POINT('Ctrl Pts',(-0.319420712000056,15.2,10.525670994));
#227239=CARTESIAN_POINT('Ctrl Pts',(-0.319420712000056,11.6,10.525670994));
#227240=CARTESIAN_POINT('Ctrl Pts',(-0.319829395000056,15.2,10.527473244));
#227241=CARTESIAN_POINT('Ctrl Pts',(-0.319829395000056,11.6,10.527473244));
#227242=CARTESIAN_POINT('Ctrl Pts',(-0.320241361000055,15.2,10.529282278));
#227243=CARTESIAN_POINT('Ctrl Pts',(-0.320241361000055,11.6,10.529282278));
#227244=CARTESIAN_POINT('Ctrl Pts',(-0.320656616000056,15.2,10.53109808));
#227245=CARTESIAN_POINT('Ctrl Pts',(-0.320656616000056,11.6,10.53109808));
#227246=CARTESIAN_POINT('Ctrl Pts',(-0.321075169000055,15.2,10.53292063));
#227247=CARTESIAN_POINT('Ctrl Pts',(-0.321075169000055,11.6,10.53292063));
#227248=CARTESIAN_POINT('Ctrl Pts',(-0.321497030000056,15.2,10.534749908));
#227249=CARTESIAN_POINT('Ctrl Pts',(-0.321497030000056,11.6,10.534749908));
#227250=CARTESIAN_POINT('Ctrl Pts',(-0.321922204000057,15.2,10.536585896));
#227251=CARTESIAN_POINT('Ctrl Pts',(-0.321922204000057,11.6,10.536585896));
#227252=CARTESIAN_POINT('Ctrl Pts',(-0.322350700000056,15.2,10.538428577));
#227253=CARTESIAN_POINT('Ctrl Pts',(-0.322350700000056,11.6,10.538428577));
#227254=CARTESIAN_POINT('Ctrl Pts',(-0.322782528000056,15.2,10.540277931));
#227255=CARTESIAN_POINT('Ctrl Pts',(-0.322782528000056,11.6,10.540277931));
#227256=CARTESIAN_POINT('Ctrl Pts',(-0.323217694000055,15.2,10.542133941));
#227257=CARTESIAN_POINT('Ctrl Pts',(-0.323217694000055,11.6,10.542133941));
#227258=CARTESIAN_POINT('Ctrl Pts',(-0.323656207000056,15.2,10.543996587));
#227259=CARTESIAN_POINT('Ctrl Pts',(-0.323656207000056,11.6,10.543996587));
#227260=CARTESIAN_POINT('Ctrl Pts',(-0.324098075000055,15.2,10.545865852));
#227261=CARTESIAN_POINT('Ctrl Pts',(-0.324098075000055,11.6,10.545865852));
#227262=CARTESIAN_POINT('Ctrl Pts',(-0.324543305000056,15.2,10.547741717));
#227263=CARTESIAN_POINT('Ctrl Pts',(-0.324543305000056,11.6,10.547741717));
#227264=CARTESIAN_POINT('Ctrl Pts',(-0.324991905000056,15.2,10.549624165));
#227265=CARTESIAN_POINT('Ctrl Pts',(-0.324991905000056,11.6,10.549624165));
#227266=CARTESIAN_POINT('Ctrl Pts',(-0.325443884000055,15.2,10.551513177));
#227267=CARTESIAN_POINT('Ctrl Pts',(-0.325443884000055,11.6,10.551513177));
#227268=CARTESIAN_POINT('Ctrl Pts',(-0.325899249000056,15.2,10.553408734));
#227269=CARTESIAN_POINT('Ctrl Pts',(-0.325899249000056,11.6,10.553408734));
#227270=CARTESIAN_POINT('Ctrl Pts',(-0.326358007000056,15.2,10.555310822));
#227271=CARTESIAN_POINT('Ctrl Pts',(-0.326358007000056,11.6,10.555310822));
#227272=CARTESIAN_POINT('Ctrl Pts',(-0.326820167000056,15.2,10.557219418));
#227273=CARTESIAN_POINT('Ctrl Pts',(-0.326820167000056,11.6,10.557219418));
#227274=CARTESIAN_POINT('Ctrl Pts',(-0.327285737000055,15.2,10.559134507));
#227275=CARTESIAN_POINT('Ctrl Pts',(-0.327285737000055,11.6,10.559134507));
#227276=CARTESIAN_POINT('Ctrl Pts',(-0.327754722000057,15.2,10.561056071));
#227277=CARTESIAN_POINT('Ctrl Pts',(-0.327754722000057,11.6,10.561056071));
#227278=CARTESIAN_POINT('Ctrl Pts',(-0.328227133000055,15.2,10.562984091));
#227279=CARTESIAN_POINT('Ctrl Pts',(-0.328227133000055,11.6,10.562984091));
#227280=CARTESIAN_POINT('Ctrl Pts',(-0.328702975000056,15.2,10.564918551));
#227281=CARTESIAN_POINT('Ctrl Pts',(-0.328702975000056,11.6,10.564918551));
#227282=CARTESIAN_POINT('Ctrl Pts',(-0.329182257000056,15.2,10.566859433));
#227283=CARTESIAN_POINT('Ctrl Pts',(-0.329182257000056,11.6,10.566859433));
#227284=CARTESIAN_POINT('Ctrl Pts',(-0.329664986000056,15.2,10.568806718));
#227285=CARTESIAN_POINT('Ctrl Pts',(-0.329664986000056,11.6,10.568806718));
#227286=CARTESIAN_POINT('Ctrl Pts',(-0.330151168000056,15.2,10.57076039));
#227287=CARTESIAN_POINT('Ctrl Pts',(-0.330151168000056,11.6,10.57076039));
#227288=CARTESIAN_POINT('Ctrl Pts',(-0.330640814000055,15.2,10.572720431));
#227289=CARTESIAN_POINT('Ctrl Pts',(-0.330640814000055,11.6,10.572720431));
#227290=CARTESIAN_POINT('Ctrl Pts',(-0.331133929000057,15.2,10.574686824));
#227291=CARTESIAN_POINT('Ctrl Pts',(-0.331133929000057,11.6,10.574686824));
#227292=CARTESIAN_POINT('Ctrl Pts',(-0.331630520000056,15.2,10.576659551));
#227293=CARTESIAN_POINT('Ctrl Pts',(-0.331630520000056,11.6,10.576659551));
#227294=CARTESIAN_POINT('Ctrl Pts',(-0.332130595000055,15.2,10.578638594));
#227295=CARTESIAN_POINT('Ctrl Pts',(-0.332130595000055,11.6,10.578638594));
#227296=CARTESIAN_POINT('Ctrl Pts',(-0.332634161000056,15.2,10.580623938));
#227297=CARTESIAN_POINT('Ctrl Pts',(-0.332634161000056,11.6,10.580623938));
#227298=CARTESIAN_POINT('Ctrl Pts',(-0.333141226000055,15.2,10.582615563));
#227299=CARTESIAN_POINT('Ctrl Pts',(-0.333141226000055,11.6,10.582615563));
#227300=CARTESIAN_POINT('Ctrl Pts',(-0.333651796000056,15.2,10.584613455));
#227301=CARTESIAN_POINT('Ctrl Pts',(-0.333651796000056,11.6,10.584613455));
#227302=CARTESIAN_POINT('Ctrl Pts',(-0.334165879000056,15.2,10.586617594));
#227303=CARTESIAN_POINT('Ctrl Pts',(-0.334165879000056,11.6,10.586617594));
#227304=CARTESIAN_POINT('Ctrl Pts',(-0.334683483000056,15.2,10.588627965));
#227305=CARTESIAN_POINT('Ctrl Pts',(-0.334683483000056,11.6,10.588627965));
#227306=CARTESIAN_POINT('Ctrl Pts',(-0.335204614000055,15.2,10.590644549));
#227307=CARTESIAN_POINT('Ctrl Pts',(-0.335204614000055,11.6,10.590644549));
#227308=CARTESIAN_POINT('Ctrl Pts',(-0.335729278000055,15.2,10.592667331));
#227309=CARTESIAN_POINT('Ctrl Pts',(-0.335729278000055,11.6,10.592667331));
#227310=CARTESIAN_POINT('Ctrl Pts',(-0.336257484000055,15.2,10.594696294));
#227311=CARTESIAN_POINT('Ctrl Pts',(-0.336257484000055,11.6,10.594696294));
#227312=CARTESIAN_POINT('Ctrl Pts',(-0.336789237000056,15.2,10.596731419));
#227313=CARTESIAN_POINT('Ctrl Pts',(-0.336789237000056,11.6,10.596731419));
#227314=CARTESIAN_POINT('Ctrl Pts',(-0.337324546000056,15.2,10.598772692));
#227315=CARTESIAN_POINT('Ctrl Pts',(-0.337324546000056,11.6,10.598772692));
#227316=CARTESIAN_POINT('Ctrl Pts',(-0.337863418000056,15.2,10.600820093));
#227317=CARTESIAN_POINT('Ctrl Pts',(-0.337863418000056,11.6,10.600820093));
#227318=CARTESIAN_POINT('Ctrl Pts',(-0.338405859000056,15.2,10.602873609));
#227319=CARTESIAN_POINT('Ctrl Pts',(-0.338405859000056,11.6,10.602873609));
#227320=CARTESIAN_POINT('Ctrl Pts',(-0.338951875000056,15.2,10.604933221));
#227321=CARTESIAN_POINT('Ctrl Pts',(-0.338951875000056,11.6,10.604933221));
#227322=CARTESIAN_POINT('Ctrl Pts',(-0.339501474000056,15.2,10.606998913));
#227323=CARTESIAN_POINT('Ctrl Pts',(-0.339501474000056,11.6,10.606998913));
#227324=CARTESIAN_POINT('Ctrl Pts',(-0.340054663000057,15.2,10.609070668));
#227325=CARTESIAN_POINT('Ctrl Pts',(-0.340054663000057,11.6,10.609070668));
#227326=CARTESIAN_POINT('Ctrl Pts',(-0.340611447000055,15.2,10.61114847));
#227327=CARTESIAN_POINT('Ctrl Pts',(-0.340611447000055,11.6,10.61114847));
#227328=CARTESIAN_POINT('Ctrl Pts',(-0.341171835000056,15.2,10.613232302));
#227329=CARTESIAN_POINT('Ctrl Pts',(-0.341171835000056,11.6,10.613232302));
#227330=CARTESIAN_POINT('Ctrl Pts',(-0.341735833000056,15.2,10.615322148));
#227331=CARTESIAN_POINT('Ctrl Pts',(-0.341735833000056,11.6,10.615322148));
#227332=CARTESIAN_POINT('Ctrl Pts',(-0.342303447000055,15.2,10.617417992));
#227333=CARTESIAN_POINT('Ctrl Pts',(-0.342303447000055,11.6,10.617417992));
#227334=CARTESIAN_POINT('Ctrl Pts',(-0.342874686000056,15.2,10.619519817));
#227335=CARTESIAN_POINT('Ctrl Pts',(-0.342874686000056,11.6,10.619519817));
#227336=CARTESIAN_POINT('Ctrl Pts',(-0.343449552000056,15.2,10.621627607));
#227337=CARTESIAN_POINT('Ctrl Pts',(-0.343449552000056,11.6,10.621627607));
#227338=CARTESIAN_POINT('Ctrl Pts',(-0.344028056000055,15.2,10.623741346));
#227339=CARTESIAN_POINT('Ctrl Pts',(-0.344028056000055,11.6,10.623741346));
#227340=CARTESIAN_POINT('Ctrl Pts',(-0.344610203000055,15.2,10.625861018));
#227341=CARTESIAN_POINT('Ctrl Pts',(-0.344610203000055,11.6,10.625861018));
#227342=CARTESIAN_POINT('Ctrl Pts',(-0.345195998000056,15.2,10.627986606));
#227343=CARTESIAN_POINT('Ctrl Pts',(-0.345195998000056,11.6,10.627986606));
#227344=CARTESIAN_POINT('Ctrl Pts',(-0.345785451000056,15.2,10.630118095));
#227345=CARTESIAN_POINT('Ctrl Pts',(-0.345785451000056,11.6,10.630118095));
#227346=CARTESIAN_POINT('Ctrl Pts',(-0.346378564000055,15.2,10.632255468));
#227347=CARTESIAN_POINT('Ctrl Pts',(-0.346378564000055,11.6,10.632255468));
#227348=CARTESIAN_POINT('Ctrl Pts',(-0.346975348000056,15.2,10.634398709));
#227349=CARTESIAN_POINT('Ctrl Pts',(-0.346975348000056,11.6,10.634398709));
#227350=CARTESIAN_POINT('Ctrl Pts',(-0.347575806000057,15.2,10.636547802));
#227351=CARTESIAN_POINT('Ctrl Pts',(-0.347575806000057,11.6,10.636547802));
#227352=CARTESIAN_POINT('Ctrl Pts',(-0.348179945000057,15.2,10.638702733));
#227353=CARTESIAN_POINT('Ctrl Pts',(-0.348179945000057,11.6,10.638702733));
#227354=CARTESIAN_POINT('Ctrl Pts',(-0.348787773000057,15.2,10.640863484));
#227355=CARTESIAN_POINT('Ctrl Pts',(-0.348787773000057,11.6,10.640863484));
#227356=CARTESIAN_POINT('Ctrl Pts',(-0.349399295000056,15.2,10.643030039));
#227357=CARTESIAN_POINT('Ctrl Pts',(-0.349399295000056,11.6,10.643030039));
#227358=CARTESIAN_POINT('Ctrl Pts',(-0.350014517000057,15.2,10.645202383));
#227359=CARTESIAN_POINT('Ctrl Pts',(-0.350014517000057,11.6,10.645202383));
#227360=CARTESIAN_POINT('Ctrl Pts',(-0.350633446000056,15.2,10.6473805));
#227361=CARTESIAN_POINT('Ctrl Pts',(-0.350633446000056,11.6,10.6473805));
#227362=CARTESIAN_POINT('Ctrl Pts',(-0.351256088000056,15.2,10.649564376));
#227363=CARTESIAN_POINT('Ctrl Pts',(-0.351256088000056,11.6,10.649564376));
#227364=CARTESIAN_POINT('Ctrl Pts',(-0.351882450000056,15.2,10.651753994));
#227365=CARTESIAN_POINT('Ctrl Pts',(-0.351882450000056,11.6,10.651753994));
#227366=CARTESIAN_POINT('Ctrl Pts',(-0.352512536000056,15.2,10.653949337));
#227367=CARTESIAN_POINT('Ctrl Pts',(-0.352512536000056,11.6,10.653949337));
#227368=CARTESIAN_POINT('Ctrl Pts',(-0.353146354000057,15.2,10.656150391));
#227369=CARTESIAN_POINT('Ctrl Pts',(-0.353146354000057,11.6,10.656150391));
#227370=CARTESIAN_POINT('Ctrl Pts',(-0.353783911000055,15.2,10.658357142));
#227371=CARTESIAN_POINT('Ctrl Pts',(-0.353783911000055,11.6,10.658357142));
#227372=CARTESIAN_POINT('Ctrl Pts',(-0.354425210000056,15.2,10.66056957));
#227373=CARTESIAN_POINT('Ctrl Pts',(-0.354425210000056,11.6,10.66056957));
#227374=CARTESIAN_POINT('Ctrl Pts',(-0.355070259000057,15.2,10.662787665));
#227375=CARTESIAN_POINT('Ctrl Pts',(-0.355070259000057,11.6,10.662787665));
#227376=CARTESIAN_POINT('Ctrl Pts',(-0.355719064000055,15.2,10.665011408));
#227377=CARTESIAN_POINT('Ctrl Pts',(-0.355719064000055,11.6,10.665011408));
#227378=CARTESIAN_POINT('Ctrl Pts',(-0.356371630000056,15.2,10.667240784));
#227379=CARTESIAN_POINT('Ctrl Pts',(-0.356371630000056,11.6,10.667240784));
#227380=CARTESIAN_POINT('Ctrl Pts',(-0.357027964000055,15.2,10.669475779));
#227381=CARTESIAN_POINT('Ctrl Pts',(-0.357027964000055,11.6,10.669475779));
#227382=CARTESIAN_POINT('Ctrl Pts',(-0.357688072000055,15.2,10.671716376));
#227383=CARTESIAN_POINT('Ctrl Pts',(-0.357688072000055,11.6,10.671716376));
#227384=CARTESIAN_POINT('Ctrl Pts',(-0.358351960000055,15.2,10.673962562));
#227385=CARTESIAN_POINT('Ctrl Pts',(-0.358351960000055,11.6,10.673962562));
#227386=CARTESIAN_POINT('Ctrl Pts',(-0.359019632000056,15.2,10.67621432));
#227387=CARTESIAN_POINT('Ctrl Pts',(-0.359019632000056,11.6,10.67621432));
#227388=CARTESIAN_POINT('Ctrl Pts',(-0.359691096000055,15.2,10.678471636));
#227389=CARTESIAN_POINT('Ctrl Pts',(-0.359691096000055,11.6,10.678471636));
#227390=CARTESIAN_POINT('Ctrl Pts',(-0.360366357000055,15.2,10.680734494));
#227391=CARTESIAN_POINT('Ctrl Pts',(-0.360366357000055,11.6,10.680734494));
#227392=CARTESIAN_POINT('Ctrl Pts',(-0.361045421000057,15.2,10.683002879));
#227393=CARTESIAN_POINT('Ctrl Pts',(-0.361045421000057,11.6,10.683002879));
#227394=CARTESIAN_POINT('Ctrl Pts',(-0.361728294000055,15.2,10.685276776));
#227395=CARTESIAN_POINT('Ctrl Pts',(-0.361728294000055,11.6,10.685276776));
#227396=CARTESIAN_POINT('Ctrl Pts',(-0.362414981000055,15.2,10.687556171));
#227397=CARTESIAN_POINT('Ctrl Pts',(-0.362414981000055,11.6,10.687556171));
#227398=CARTESIAN_POINT('Ctrl Pts',(-0.363105488000055,15.2,10.689841048));
#227399=CARTESIAN_POINT('Ctrl Pts',(-0.363105488000055,11.6,10.689841048));
#227400=CARTESIAN_POINT('Ctrl Pts',(-0.363799821000056,15.2,10.692131392));
#227401=CARTESIAN_POINT('Ctrl Pts',(-0.363799821000056,11.6,10.692131392));
#227402=CARTESIAN_POINT('Ctrl Pts',(-0.364497985000056,15.2,10.694427189));
#227403=CARTESIAN_POINT('Ctrl Pts',(-0.364497985000056,11.6,10.694427189));
#227404=CARTESIAN_POINT('Ctrl Pts',(-0.365199987000056,15.2,10.696728424));
#227405=CARTESIAN_POINT('Ctrl Pts',(-0.365199987000056,11.6,10.696728424));
#227406=CARTESIAN_POINT('Ctrl Pts',(-0.365905831000056,15.2,10.699035082));
#227407=CARTESIAN_POINT('Ctrl Pts',(-0.365905831000056,11.6,10.699035082));
#227408=CARTESIAN_POINT('Ctrl Pts',(-0.366615524000055,15.2,10.701347148));
#227409=CARTESIAN_POINT('Ctrl Pts',(-0.366615524000055,11.6,10.701347148));
#227410=CARTESIAN_POINT('Ctrl Pts',(-0.367329070000055,15.2,10.703664608));
#227411=CARTESIAN_POINT('Ctrl Pts',(-0.367329070000055,11.6,10.703664608));
#227412=CARTESIAN_POINT('Ctrl Pts',(-0.368046475000057,15.2,10.705987446));
#227413=CARTESIAN_POINT('Ctrl Pts',(-0.368046475000057,11.6,10.705987446));
#227414=CARTESIAN_POINT('Ctrl Pts',(-0.368767746000056,15.2,10.708315648));
#227415=CARTESIAN_POINT('Ctrl Pts',(-0.368767746000056,11.6,10.708315648));
#227416=CARTESIAN_POINT('Ctrl Pts',(-0.369492887000057,15.2,10.7106492));
#227417=CARTESIAN_POINT('Ctrl Pts',(-0.369492887000057,11.6,10.7106492));
#227418=CARTESIAN_POINT('Ctrl Pts',(-0.370221904000055,15.2,10.712988087));
#227419=CARTESIAN_POINT('Ctrl Pts',(-0.370221904000055,11.6,10.712988087));
#227420=CARTESIAN_POINT('Ctrl Pts',(-0.370954802000056,15.2,10.715332294));
#227421=CARTESIAN_POINT('Ctrl Pts',(-0.370954802000056,11.6,10.715332294));
#227422=CARTESIAN_POINT('Ctrl Pts',(-0.371691587000056,15.2,10.717681807));
#227423=CARTESIAN_POINT('Ctrl Pts',(-0.371691587000056,11.6,10.717681807));
#227424=CARTESIAN_POINT('Ctrl Pts',(-0.372432264000055,15.2,10.720036611));
#227425=CARTESIAN_POINT('Ctrl Pts',(-0.372432264000055,11.6,10.720036611));
#227426=CARTESIAN_POINT('Ctrl Pts',(-0.373176838000056,15.2,10.722396693));
#227427=CARTESIAN_POINT('Ctrl Pts',(-0.373176838000056,11.6,10.722396693));
#227428=CARTESIAN_POINT('Ctrl Pts',(-0.373925315000055,15.2,10.724762038));
#227429=CARTESIAN_POINT('Ctrl Pts',(-0.373925315000055,11.6,10.724762038));
#227430=CARTESIAN_POINT('Ctrl Pts',(-0.374677700000056,15.2,10.72713263));
#227431=CARTESIAN_POINT('Ctrl Pts',(-0.374677700000056,11.6,10.72713263));
#227432=CARTESIAN_POINT('Ctrl Pts',(-0.375433998000055,15.2,10.729508458));
#227433=CARTESIAN_POINT('Ctrl Pts',(-0.375433998000055,11.6,10.729508458));
#227434=CARTESIAN_POINT('Ctrl Pts',(-0.376194216000056,15.2,10.731889504));
#227435=CARTESIAN_POINT('Ctrl Pts',(-0.376194216000056,11.6,10.731889504));
#227436=CARTESIAN_POINT('Ctrl Pts',(-0.376958356000056,15.2,10.734275756));
#227437=CARTESIAN_POINT('Ctrl Pts',(-0.376958356000056,11.6,10.734275756));
#227438=CARTESIAN_POINT('Ctrl Pts',(-0.377726425000056,15.2,10.7366672));
#227439=CARTESIAN_POINT('Ctrl Pts',(-0.377726425000056,11.6,10.7366672));
#227440=CARTESIAN_POINT('Ctrl Pts',(-0.378498429000055,15.2,10.739063821));
#227441=CARTESIAN_POINT('Ctrl Pts',(-0.378498429000055,11.6,10.739063821));
#227442=CARTESIAN_POINT('Ctrl Pts',(-0.379274373000056,15.2,10.741465604));
#227443=CARTESIAN_POINT('Ctrl Pts',(-0.379274373000056,11.6,10.741465604));
#227444=CARTESIAN_POINT('Ctrl Pts',(-0.380054260000057,15.2,10.743872536));
#227445=CARTESIAN_POINT('Ctrl Pts',(-0.380054260000057,11.6,10.743872536));
#227446=CARTESIAN_POINT('Ctrl Pts',(-0.380838098000057,15.2,10.746284603));
#227447=CARTESIAN_POINT('Ctrl Pts',(-0.380838098000057,11.6,10.746284603));
#227448=CARTESIAN_POINT('Ctrl Pts',(-0.381625890000056,15.2,10.748701792));
#227449=CARTESIAN_POINT('Ctrl Pts',(-0.381625890000056,11.6,10.748701792));
#227450=CARTESIAN_POINT('Ctrl Pts',(-0.382417641000057,15.2,10.751124087));
#227451=CARTESIAN_POINT('Ctrl Pts',(-0.382417641000057,11.6,10.751124087));
#227452=CARTESIAN_POINT('Ctrl Pts',(-0.383213358000055,15.2,10.753551475));
#227453=CARTESIAN_POINT('Ctrl Pts',(-0.383213358000055,11.6,10.753551475));
#227454=CARTESIAN_POINT('Ctrl Pts',(-0.384013044000057,15.2,10.755983943));
#227455=CARTESIAN_POINT('Ctrl Pts',(-0.384013044000057,11.6,10.755983943));
#227456=CARTESIAN_POINT('Ctrl Pts',(-0.384816706000055,15.2,10.758421474));
#227457=CARTESIAN_POINT('Ctrl Pts',(-0.384816706000055,11.6,10.758421474));
#227458=CARTESIAN_POINT('Ctrl Pts',(-0.385624346000055,15.2,10.760864058));
#227459=CARTESIAN_POINT('Ctrl Pts',(-0.385624346000055,11.6,10.760864058));
#227460=CARTESIAN_POINT('Ctrl Pts',(-0.386435972000055,15.2,10.763311678));
#227461=CARTESIAN_POINT('Ctrl Pts',(-0.386435972000055,11.6,10.763311678));
#227462=CARTESIAN_POINT('Ctrl Pts',(-0.387251587000056,15.2,10.765764322));
#227463=CARTESIAN_POINT('Ctrl Pts',(-0.387251587000056,11.6,10.765764322));
#227464=CARTESIAN_POINT('Ctrl Pts',(-0.388071197000055,15.2,10.768221976));
#227465=CARTESIAN_POINT('Ctrl Pts',(-0.388071197000055,11.6,10.768221976));
#227466=CARTESIAN_POINT('Ctrl Pts',(-0.388894805000056,15.2,10.770684627));
#227467=CARTESIAN_POINT('Ctrl Pts',(-0.388894805000056,11.6,10.770684627));
#227468=CARTESIAN_POINT('Ctrl Pts',(-0.389722418000057,15.2,10.773152259));
#227469=CARTESIAN_POINT('Ctrl Pts',(-0.389722418000057,11.6,10.773152259));
#227470=CARTESIAN_POINT('Ctrl Pts',(-0.390554041000056,15.2,10.77562486));
#227471=CARTESIAN_POINT('Ctrl Pts',(-0.390554041000056,11.6,10.77562486));
#227472=CARTESIAN_POINT('Ctrl Pts',(-0.391389677000056,15.2,10.778102417));
#227473=CARTESIAN_POINT('Ctrl Pts',(-0.391389677000056,11.6,10.778102417));
#227474=CARTESIAN_POINT('Ctrl Pts',(-0.392229332000056,15.2,10.780584915));
#227475=CARTESIAN_POINT('Ctrl Pts',(-0.392229332000056,11.6,10.780584915));
#227476=CARTESIAN_POINT('Ctrl Pts',(-0.393073010000055,15.2,10.783072341));
#227477=CARTESIAN_POINT('Ctrl Pts',(-0.393073010000055,11.6,10.783072341));
#227478=CARTESIAN_POINT('Ctrl Pts',(-0.393920716000055,15.2,10.785564682));
#227479=CARTESIAN_POINT('Ctrl Pts',(-0.393920716000055,11.6,10.785564682));
#227480=CARTESIAN_POINT('Ctrl Pts',(-0.394772455000056,15.2,10.788061923));
#227481=CARTESIAN_POINT('Ctrl Pts',(-0.394772455000056,11.6,10.788061923));
#227482=CARTESIAN_POINT('Ctrl Pts',(-0.395628232000057,15.2,10.790564052));
#227483=CARTESIAN_POINT('Ctrl Pts',(-0.395628232000057,11.6,10.790564052));
#227484=CARTESIAN_POINT('Ctrl Pts',(-0.396488052000056,15.2,10.793071055));
#227485=CARTESIAN_POINT('Ctrl Pts',(-0.396488052000056,11.6,10.793071055));
#227486=CARTESIAN_POINT('Ctrl Pts',(-0.397351918000056,15.2,10.795582918));
#227487=CARTESIAN_POINT('Ctrl Pts',(-0.397351918000056,11.6,10.795582918));
#227488=CARTESIAN_POINT('Ctrl Pts',(-0.398219836000056,15.2,10.798099629));
#227489=CARTESIAN_POINT('Ctrl Pts',(-0.398219836000056,11.6,10.798099629));
#227490=CARTESIAN_POINT('Ctrl Pts',(-0.399091809000056,15.2,10.800621175));
#227491=CARTESIAN_POINT('Ctrl Pts',(-0.399091809000056,11.6,10.800621175));
#227492=CARTESIAN_POINT('Ctrl Pts',(-0.399967843000055,15.2,10.80314754));
#227493=CARTESIAN_POINT('Ctrl Pts',(-0.399967843000055,11.6,10.80314754));
#227494=CARTESIAN_POINT('Ctrl Pts',(-0.400847943000056,15.2,10.805678712));
#227495=CARTESIAN_POINT('Ctrl Pts',(-0.400847943000056,11.6,10.805678712));
#227496=CARTESIAN_POINT('Ctrl Pts',(-0.401732113000056,15.2,10.80821468));
#227497=CARTESIAN_POINT('Ctrl Pts',(-0.401732113000056,11.6,10.80821468));
#227498=CARTESIAN_POINT('Ctrl Pts',(-0.402620357000056,15.2,10.810755427));
#227499=CARTESIAN_POINT('Ctrl Pts',(-0.402620357000056,11.6,10.810755427));
#227500=CARTESIAN_POINT('Ctrl Pts',(-0.403512680000055,15.2,10.813300943));
#227501=CARTESIAN_POINT('Ctrl Pts',(-0.403512680000055,11.6,10.813300943));
#227502=CARTESIAN_POINT('Ctrl Pts',(-0.404409086000056,15.2,10.815851213));
#227503=CARTESIAN_POINT('Ctrl Pts',(-0.404409086000056,11.6,10.815851213));
#227504=CARTESIAN_POINT('Ctrl Pts',(-0.405309580000056,15.2,10.818406224));
#227505=CARTESIAN_POINT('Ctrl Pts',(-0.405309580000056,11.6,10.818406224));
#227506=CARTESIAN_POINT('Ctrl Pts',(-0.406214167000056,15.2,10.820965965));
#227507=CARTESIAN_POINT('Ctrl Pts',(-0.406214167000056,11.6,10.820965965));
#227508=CARTESIAN_POINT('Ctrl Pts',(-0.407122850000056,15.2,10.82353042));
#227509=CARTESIAN_POINT('Ctrl Pts',(-0.407122850000056,11.6,10.82353042));
#227510=CARTESIAN_POINT('Ctrl Pts',(-0.408035634000056,15.2,10.826099577));
#227511=CARTESIAN_POINT('Ctrl Pts',(-0.408035634000056,11.6,10.826099577));
#227512=CARTESIAN_POINT('Ctrl Pts',(-0.408952523000057,15.2,10.828673423));
#227513=CARTESIAN_POINT('Ctrl Pts',(-0.408952523000057,11.6,10.828673423));
#227514=CARTESIAN_POINT('Ctrl Pts',(-0.409873522000056,15.2,10.831251946));
#227515=CARTESIAN_POINT('Ctrl Pts',(-0.409873522000056,11.6,10.831251946));
#227516=CARTESIAN_POINT('Ctrl Pts',(-0.410798636000056,15.2,10.833835133));
#227517=CARTESIAN_POINT('Ctrl Pts',(-0.410798636000056,11.6,10.833835133));
#227518=CARTESIAN_POINT('Ctrl Pts',(-0.411727868000057,15.2,10.836422969));
#227519=CARTESIAN_POINT('Ctrl Pts',(-0.411727868000057,11.6,10.836422969));
#227520=CARTESIAN_POINT('Ctrl Pts',(-0.412661222000056,15.2,10.839015444));
#227521=CARTESIAN_POINT('Ctrl Pts',(-0.412661222000056,11.6,10.839015444));
#227522=CARTESIAN_POINT('Ctrl Pts',(-0.413598704000057,15.2,10.841612542));
#227523=CARTESIAN_POINT('Ctrl Pts',(-0.413598704000057,11.6,10.841612542));
#227524=CARTESIAN_POINT('Ctrl Pts',(-0.414540317000055,15.2,10.844214253));
#227525=CARTESIAN_POINT('Ctrl Pts',(-0.414540317000055,11.6,10.844214253));
#227526=CARTESIAN_POINT('Ctrl Pts',(-0.415486065000056,15.2,10.846820562));
#227527=CARTESIAN_POINT('Ctrl Pts',(-0.415486065000056,11.6,10.846820562));
#227528=CARTESIAN_POINT('Ctrl Pts',(-0.416435953000055,15.2,10.849431458));
#227529=CARTESIAN_POINT('Ctrl Pts',(-0.416435953000055,11.6,10.849431458));
#227530=CARTESIAN_POINT('Ctrl Pts',(-0.417389986000056,15.2,10.852046927));
#227531=CARTESIAN_POINT('Ctrl Pts',(-0.417389986000056,11.6,10.852046927));
#227532=CARTESIAN_POINT('Ctrl Pts',(-0.418348166000057,15.2,10.854666957));
#227533=CARTESIAN_POINT('Ctrl Pts',(-0.418348166000057,11.6,10.854666957));
#227534=CARTESIAN_POINT('Ctrl Pts',(-0.419310498000056,15.2,10.857291536));
#227535=CARTESIAN_POINT('Ctrl Pts',(-0.419310498000056,11.6,10.857291536));
#227536=CARTESIAN_POINT('Ctrl Pts',(-0.420276987000056,15.2,10.859920649));
#227537=CARTESIAN_POINT('Ctrl Pts',(-0.420276987000056,11.6,10.859920649));
#227538=CARTESIAN_POINT('Ctrl Pts',(-0.421247636000055,15.2,10.862554285));
#227539=CARTESIAN_POINT('Ctrl Pts',(-0.421247636000055,11.6,10.862554285));
#227540=CARTESIAN_POINT('Ctrl Pts',(-0.422222450000056,15.2,10.865192432));
#227541=CARTESIAN_POINT('Ctrl Pts',(-0.422222450000056,11.6,10.865192432));
#227542=CARTESIAN_POINT('Ctrl Pts',(-0.423201433000056,15.2,10.867835076));
#227543=CARTESIAN_POINT('Ctrl Pts',(-0.423201433000056,11.6,10.867835076));
#227544=CARTESIAN_POINT('Ctrl Pts',(-0.424184589000056,15.2,10.870482205));
#227545=CARTESIAN_POINT('Ctrl Pts',(-0.424184589000056,11.6,10.870482205));
#227546=CARTESIAN_POINT('Ctrl Pts',(-0.425171920000055,15.2,10.873133807));
#227547=CARTESIAN_POINT('Ctrl Pts',(-0.425171920000055,11.6,10.873133807));
#227548=CARTESIAN_POINT('Ctrl Pts',(-0.426163434000056,15.2,10.875789869));
#227549=CARTESIAN_POINT('Ctrl Pts',(-0.426163434000056,11.6,10.875789869));
#227550=CARTESIAN_POINT('Ctrl Pts',(-0.427159131000057,15.2,10.878450378));
#227551=CARTESIAN_POINT('Ctrl Pts',(-0.427159131000057,11.6,10.878450378));
#227552=CARTESIAN_POINT('Ctrl Pts',(-0.428159019000055,15.2,10.881115323));
#227553=CARTESIAN_POINT('Ctrl Pts',(-0.428159019000055,11.6,10.881115323));
#227554=CARTESIAN_POINT('Ctrl Pts',(-0.429163097000057,15.2,10.88378469));
#227555=CARTESIAN_POINT('Ctrl Pts',(-0.429163097000057,11.6,10.88378469));
#227556=CARTESIAN_POINT('Ctrl Pts',(-0.430171373000056,15.2,10.886458467));
#227557=CARTESIAN_POINT('Ctrl Pts',(-0.430171373000056,11.6,10.886458467));
#227558=CARTESIAN_POINT('Ctrl Pts',(-0.431183850000056,15.2,10.889136642));
#227559=CARTESIAN_POINT('Ctrl Pts',(-0.431183850000056,11.6,10.889136642));
#227560=CARTESIAN_POINT('Ctrl Pts',(-0.432200532000057,15.2,10.891819204));
#227561=CARTESIAN_POINT('Ctrl Pts',(-0.432200532000057,11.6,10.891819204));
#227562=CARTESIAN_POINT('Ctrl Pts',(-0.433221421000055,15.2,10.894506138));
#227563=CARTESIAN_POINT('Ctrl Pts',(-0.433221421000055,11.6,10.894506138));
#227564=CARTESIAN_POINT('Ctrl Pts',(-0.434246523000056,15.2,10.897197433));
#227565=CARTESIAN_POINT('Ctrl Pts',(-0.434246523000056,11.6,10.897197433));
#227566=CARTESIAN_POINT('Ctrl Pts',(-0.435275841000056,15.2,10.899893078));
#227567=CARTESIAN_POINT('Ctrl Pts',(-0.435275841000056,11.6,10.899893078));
#227568=CARTESIAN_POINT('Ctrl Pts',(-0.436309379000056,15.2,10.902593058));
#227569=CARTESIAN_POINT('Ctrl Pts',(-0.436309379000056,11.6,10.902593058));
#227570=CARTESIAN_POINT('Ctrl Pts',(-0.437347140000056,15.2,10.905297364));
#227571=CARTESIAN_POINT('Ctrl Pts',(-0.437347140000056,11.6,10.905297364));
#227572=CARTESIAN_POINT('Ctrl Pts',(-0.438389130000055,15.2,10.908005982));
#227573=CARTESIAN_POINT('Ctrl Pts',(-0.438389130000055,11.6,10.908005982));
#227574=CARTESIAN_POINT('Ctrl Pts',(-0.439435351000055,15.2,10.910718899));
#227575=CARTESIAN_POINT('Ctrl Pts',(-0.439435351000055,11.6,10.910718899));
#227576=CARTESIAN_POINT('Ctrl Pts',(-0.440485807000056,15.2,10.913436104));
#227577=CARTESIAN_POINT('Ctrl Pts',(-0.440485807000056,11.6,10.913436104));
#227578=CARTESIAN_POINT('Ctrl Pts',(-0.441540501000055,15.2,10.916157585));
#227579=CARTESIAN_POINT('Ctrl Pts',(-0.441540501000055,11.6,10.916157585));
#227580=CARTESIAN_POINT('Ctrl Pts',(-0.442599439000055,15.2,10.91888333));
#227581=CARTESIAN_POINT('Ctrl Pts',(-0.442599439000055,11.6,10.91888333));
#227582=CARTESIAN_POINT('Ctrl Pts',(-0.443662622000056,15.2,10.921613326));
#227583=CARTESIAN_POINT('Ctrl Pts',(-0.443662622000056,11.6,10.921613326));
#227584=CARTESIAN_POINT('Ctrl Pts',(-0.444730056000056,15.2,10.924347563));
#227585=CARTESIAN_POINT('Ctrl Pts',(-0.444730056000056,11.6,10.924347563));
#227586=CARTESIAN_POINT('Ctrl Pts',(-0.445801744000055,15.2,10.927086027));
#227587=CARTESIAN_POINT('Ctrl Pts',(-0.445801744000055,11.6,10.927086027));
#227588=CARTESIAN_POINT('Ctrl Pts',(-0.446877689000056,15.2,10.929828706));
#227589=CARTESIAN_POINT('Ctrl Pts',(-0.446877689000056,11.6,10.929828706));
#227590=CARTESIAN_POINT('Ctrl Pts',(-0.447957894000056,15.2,10.932575589));
#227591=CARTESIAN_POINT('Ctrl Pts',(-0.447957894000056,11.6,10.932575589));
#227592=CARTESIAN_POINT('Ctrl Pts',(-0.449042364000055,15.2,10.935326665));
#227593=CARTESIAN_POINT('Ctrl Pts',(-0.449042364000055,11.6,10.935326665));
#227594=CARTESIAN_POINT('Ctrl Pts',(-0.450131103000055,15.2,10.938081919));
#227595=CARTESIAN_POINT('Ctrl Pts',(-0.450131103000055,11.6,10.938081919));
#227596=CARTESIAN_POINT('Ctrl Pts',(-0.451224113000055,15.2,10.940841342));
#227597=CARTESIAN_POINT('Ctrl Pts',(-0.451224113000055,11.6,10.940841342));
#227598=CARTESIAN_POINT('Ctrl Pts',(-0.452321398000055,15.2,10.943604922));
#227599=CARTESIAN_POINT('Ctrl Pts',(-0.452321398000055,11.6,10.943604922));
#227600=CARTESIAN_POINT('Ctrl Pts',(-0.453422963000056,15.2,10.946372645));
#227601=CARTESIAN_POINT('Ctrl Pts',(-0.453422963000056,11.6,10.946372645));
#227602=CARTESIAN_POINT('Ctrl Pts',(-0.454528809000055,15.2,10.949144502));
#227603=CARTESIAN_POINT('Ctrl Pts',(-0.454528809000055,11.6,10.949144502));
#227604=CARTESIAN_POINT('Ctrl Pts',(-0.455638942000055,15.2,10.951920479));
#227605=CARTESIAN_POINT('Ctrl Pts',(-0.455638942000055,11.6,10.951920479));
#227606=CARTESIAN_POINT('Ctrl Pts',(-0.456753365000055,15.2,10.954700564));
#227607=CARTESIAN_POINT('Ctrl Pts',(-0.456753365000055,11.6,10.954700564));
#227608=CARTESIAN_POINT('Ctrl Pts',(-0.457872079000056,15.2,10.957484748));
#227609=CARTESIAN_POINT('Ctrl Pts',(-0.457872079000056,11.6,10.957484748));
#227610=CARTESIAN_POINT('Ctrl Pts',(-0.458995091000055,15.2,10.960273017));
#227611=CARTESIAN_POINT('Ctrl Pts',(-0.458995091000055,11.6,10.960273017));
#227612=CARTESIAN_POINT('Ctrl Pts',(-0.460122403000056,15.2,10.963065359));
#227613=CARTESIAN_POINT('Ctrl Pts',(-0.460122403000056,11.6,10.963065359));
#227614=CARTESIAN_POINT('Ctrl Pts',(-0.461254017000057,15.2,10.965861764));
#227615=CARTESIAN_POINT('Ctrl Pts',(-0.461254017000057,11.6,10.965861764));
#227616=CARTESIAN_POINT('Ctrl Pts',(-0.462389938000056,15.2,10.96866222));
#227617=CARTESIAN_POINT('Ctrl Pts',(-0.462389938000056,11.6,10.96866222));
#227618=CARTESIAN_POINT('Ctrl Pts',(-0.463530169000055,15.2,10.971466714));
#227619=CARTESIAN_POINT('Ctrl Pts',(-0.463530169000055,11.6,10.971466714));
#227620=CARTESIAN_POINT('Ctrl Pts',(-0.464674714000056,15.2,10.974275236));
#227621=CARTESIAN_POINT('Ctrl Pts',(-0.464674714000056,11.6,10.974275236));
#227622=CARTESIAN_POINT('Ctrl Pts',(-0.465823576000056,15.2,10.977087774));
#227623=CARTESIAN_POINT('Ctrl Pts',(-0.465823576000056,11.6,10.977087774));
#227624=CARTESIAN_POINT('Ctrl Pts',(-0.466976757000056,15.2,10.979904316));
#227625=CARTESIAN_POINT('Ctrl Pts',(-0.466976757000056,11.6,10.979904316));
#227626=CARTESIAN_POINT('Ctrl Pts',(-0.468134263000056,15.2,10.982724851));
#227627=CARTESIAN_POINT('Ctrl Pts',(-0.468134263000056,11.6,10.982724851));
#227628=CARTESIAN_POINT('Ctrl Pts',(-0.469296095000056,15.2,10.985549367));
#227629=CARTESIAN_POINT('Ctrl Pts',(-0.469296095000056,11.6,10.985549367));
#227630=CARTESIAN_POINT('Ctrl Pts',(-0.470462257000056,15.2,10.988377854));
#227631=CARTESIAN_POINT('Ctrl Pts',(-0.470462257000056,11.6,10.988377854));
#227632=CARTESIAN_POINT('Ctrl Pts',(-0.471632753000056,15.2,10.991210298));
#227633=CARTESIAN_POINT('Ctrl Pts',(-0.471632753000056,11.6,10.991210298));
#227634=CARTESIAN_POINT('Ctrl Pts',(-0.472807585000057,15.2,10.99404669));
#227635=CARTESIAN_POINT('Ctrl Pts',(-0.472807585000057,11.6,10.99404669));
#227636=CARTESIAN_POINT('Ctrl Pts',(-0.473986758000056,15.2,10.996887017));
#227637=CARTESIAN_POINT('Ctrl Pts',(-0.473986758000056,11.6,10.996887017));
#227638=CARTESIAN_POINT('Ctrl Pts',(-0.475170273000056,15.2,10.999731268));
#227639=CARTESIAN_POINT('Ctrl Pts',(-0.475170273000056,11.6,10.999731268));
#227640=CARTESIAN_POINT('Ctrl Pts',(-0.476358135000057,15.2,11.002579432));
#227641=CARTESIAN_POINT('Ctrl Pts',(-0.476358135000057,11.6,11.002579432));
#227642=CARTESIAN_POINT('Ctrl Pts',(-0.477550347000056,15.2,11.005431497));
#227643=CARTESIAN_POINT('Ctrl Pts',(-0.477550347000056,11.6,11.005431497));
#227644=CARTESIAN_POINT('Ctrl Pts',(-0.478746911000056,15.2,11.008287452));
#227645=CARTESIAN_POINT('Ctrl Pts',(-0.478746911000056,11.6,11.008287452));
#227646=CARTESIAN_POINT('Ctrl Pts',(-0.479947831000055,15.2,11.011147286));
#227647=CARTESIAN_POINT('Ctrl Pts',(-0.479947831000055,11.6,11.011147286));
#227648=CARTESIAN_POINT('Ctrl Pts',(-0.481153110000055,15.2,11.014010989));
#227649=CARTESIAN_POINT('Ctrl Pts',(-0.481153110000055,11.6,11.014010989));
#227650=CARTESIAN_POINT('Ctrl Pts',(-0.482362752000055,15.2,11.016878547));
#227651=CARTESIAN_POINT('Ctrl Pts',(-0.482362752000055,11.6,11.016878547));
#227652=CARTESIAN_POINT('Ctrl Pts',(-0.483576758000056,15.2,11.01974995));
#227653=CARTESIAN_POINT('Ctrl Pts',(-0.483576758000056,11.6,11.01974995));
#227654=CARTESIAN_POINT('Ctrl Pts',(-0.484795134000056,15.2,11.022625187));
#227655=CARTESIAN_POINT('Ctrl Pts',(-0.484795134000056,11.6,11.022625187));
#227656=CARTESIAN_POINT('Ctrl Pts',(-0.486017882000055,15.2,11.025504248));
#227657=CARTESIAN_POINT('Ctrl Pts',(-0.486017882000055,11.6,11.025504248));
#227658=CARTESIAN_POINT('Ctrl Pts',(-0.487245003000056,15.2,11.028387119));
#227659=CARTESIAN_POINT('Ctrl Pts',(-0.487245003000056,11.6,11.028387119));
#227660=CARTESIAN_POINT('Ctrl Pts',(-0.488476503000056,15.2,11.031273791));
#227661=CARTESIAN_POINT('Ctrl Pts',(-0.488476503000056,11.6,11.031273791));
#227662=CARTESIAN_POINT('Ctrl Pts',(-0.489712382000055,15.2,11.034164252));
#227663=CARTESIAN_POINT('Ctrl Pts',(-0.489712382000055,11.6,11.034164252));
#227664=CARTESIAN_POINT('Ctrl Pts',(-0.490952647000055,15.2,11.037058492));
#227665=CARTESIAN_POINT('Ctrl Pts',(-0.490952647000055,11.6,11.037058492));
#227666=CARTESIAN_POINT('Ctrl Pts',(-0.492197298000056,15.2,11.039956498));
#227667=CARTESIAN_POINT('Ctrl Pts',(-0.492197298000056,11.6,11.039956498));
#227668=CARTESIAN_POINT('Ctrl Pts',(-0.493446339000055,15.2,11.042858261));
#227669=CARTESIAN_POINT('Ctrl Pts',(-0.493446339000055,11.6,11.042858261));
#227670=CARTESIAN_POINT('Ctrl Pts',(-0.494699772000056,15.2,11.045763768));
#227671=CARTESIAN_POINT('Ctrl Pts',(-0.494699772000056,11.6,11.045763768));
#227672=CARTESIAN_POINT('Ctrl Pts',(-0.495957601000055,15.2,11.04867301));
#227673=CARTESIAN_POINT('Ctrl Pts',(-0.495957601000055,11.6,11.04867301));
#227674=CARTESIAN_POINT('Ctrl Pts',(-0.497219830000055,15.2,11.051585974));
#227675=CARTESIAN_POINT('Ctrl Pts',(-0.497219830000055,11.6,11.051585974));
#227676=CARTESIAN_POINT('Ctrl Pts',(-0.498486460000055,15.2,11.054502651));
#227677=CARTESIAN_POINT('Ctrl Pts',(-0.498486460000055,11.6,11.054502651));
#227678=CARTESIAN_POINT('Ctrl Pts',(-0.499757495000056,15.2,11.057423028));
#227679=CARTESIAN_POINT('Ctrl Pts',(-0.499757495000056,11.6,11.057423028));
#227680=CARTESIAN_POINT('Ctrl Pts',(-0.501032937000057,15.2,11.060347096));
#227681=CARTESIAN_POINT('Ctrl Pts',(-0.501032937000057,11.6,11.060347096));
#227682=CARTESIAN_POINT('Ctrl Pts',(-0.502312790000056,15.2,11.063274844));
#227683=CARTESIAN_POINT('Ctrl Pts',(-0.502312790000056,11.6,11.063274844));
#227684=CARTESIAN_POINT('Ctrl Pts',(-0.503597056000055,15.2,11.06620626));
#227685=CARTESIAN_POINT('Ctrl Pts',(-0.503597056000055,11.6,11.06620626));
#227686=CARTESIAN_POINT('Ctrl Pts',(-0.504885739000055,15.2,11.069141332));
#227687=CARTESIAN_POINT('Ctrl Pts',(-0.504885739000055,11.6,11.069141332));
#227688=CARTESIAN_POINT('Ctrl Pts',(-0.506178839000055,15.2,11.072080052));
#227689=CARTESIAN_POINT('Ctrl Pts',(-0.506178839000055,11.6,11.072080052));
#227690=CARTESIAN_POINT('Ctrl Pts',(-0.507476363000056,15.2,11.075022407));
#227691=CARTESIAN_POINT('Ctrl Pts',(-0.507476363000056,11.6,11.075022407));
#227692=CARTESIAN_POINT('Ctrl Pts',(-0.508778311000055,15.2,11.077968388));
#227693=CARTESIAN_POINT('Ctrl Pts',(-0.508778311000055,11.6,11.077968388));
#227694=CARTESIAN_POINT('Ctrl Pts',(-0.510084686000055,15.2,11.080917983));
#227695=CARTESIAN_POINT('Ctrl Pts',(-0.510084686000055,11.6,11.080917983));
#227696=CARTESIAN_POINT('Ctrl Pts',(-0.511395493000055,15.2,11.08387118));
#227697=CARTESIAN_POINT('Ctrl Pts',(-0.511395493000055,11.6,11.08387118));
#227698=CARTESIAN_POINT('Ctrl Pts',(-0.512710732000056,15.2,11.086827971));
#227699=CARTESIAN_POINT('Ctrl Pts',(-0.512710732000056,11.6,11.086827971));
#227700=CARTESIAN_POINT('Ctrl Pts',(-0.514030407000057,15.2,11.089788344));
#227701=CARTESIAN_POINT('Ctrl Pts',(-0.514030407000057,11.6,11.089788344));
#227702=CARTESIAN_POINT('Ctrl Pts',(-0.515354521000055,15.2,11.092752288));
#227703=CARTESIAN_POINT('Ctrl Pts',(-0.515354521000055,11.6,11.092752288));
#227704=CARTESIAN_POINT('Ctrl Pts',(-0.516683076000056,15.2,11.095719793));
#227705=CARTESIAN_POINT('Ctrl Pts',(-0.516683076000056,11.6,11.095719793));
#227706=CARTESIAN_POINT('Ctrl Pts',(-0.518016075000055,15.2,11.098690848));
#227707=CARTESIAN_POINT('Ctrl Pts',(-0.518016075000055,11.6,11.098690848));
#227708=CARTESIAN_POINT('Ctrl Pts',(-0.519353523000056,15.2,11.101665442));
#227709=CARTESIAN_POINT('Ctrl Pts',(-0.519353523000056,11.6,11.101665442));
#227710=CARTESIAN_POINT('Ctrl Pts',(-0.520695418000056,15.2,11.104643565));
#227711=CARTESIAN_POINT('Ctrl Pts',(-0.520695418000056,11.6,11.104643565));
#227712=CARTESIAN_POINT('Ctrl Pts',(-0.522041766000055,15.2,11.107625205));
#227713=CARTESIAN_POINT('Ctrl Pts',(-0.522041766000055,11.6,11.107625205));
#227714=CARTESIAN_POINT('Ctrl Pts',(-0.523392569000055,15.2,11.110610353));
#227715=CARTESIAN_POINT('Ctrl Pts',(-0.523392569000055,11.6,11.110610353));
#227716=CARTESIAN_POINT('Ctrl Pts',(-0.524747830000055,15.2,11.113598997));
#227717=CARTESIAN_POINT('Ctrl Pts',(-0.524747830000055,11.6,11.113598997));
#227718=CARTESIAN_POINT('Ctrl Pts',(-0.526107551000056,15.2,11.116591128));
#227719=CARTESIAN_POINT('Ctrl Pts',(-0.526107551000056,11.6,11.116591128));
#227720=CARTESIAN_POINT('Ctrl Pts',(-0.527471735000056,15.2,11.119586736));
#227721=CARTESIAN_POINT('Ctrl Pts',(-0.527471735000056,11.6,11.119586736));
#227722=CARTESIAN_POINT('Ctrl Pts',(-0.528840384000056,15.2,11.122585808));
#227723=CARTESIAN_POINT('Ctrl Pts',(-0.528840384000056,11.6,11.122585808));
#227724=CARTESIAN_POINT('Ctrl Pts',(-0.530213502000055,15.2,11.125588335));
#227725=CARTESIAN_POINT('Ctrl Pts',(-0.530213502000055,11.6,11.125588335));
#227726=CARTESIAN_POINT('Ctrl Pts',(-0.531591090000055,15.2,11.128594306));
#227727=CARTESIAN_POINT('Ctrl Pts',(-0.531591090000055,11.6,11.128594306));
#227728=CARTESIAN_POINT('Ctrl Pts',(-0.532973152000055,15.2,11.131603711));
#227729=CARTESIAN_POINT('Ctrl Pts',(-0.532973152000055,11.6,11.131603711));
#227730=CARTESIAN_POINT('Ctrl Pts',(-0.534359689000056,15.2,11.134616539));
#227731=CARTESIAN_POINT('Ctrl Pts',(-0.534359689000056,11.6,11.134616539));
#227732=CARTESIAN_POINT('Ctrl Pts',(-0.535750704000056,15.2,11.137632782));
#227733=CARTESIAN_POINT('Ctrl Pts',(-0.535750704000056,11.6,11.137632782));
#227734=CARTESIAN_POINT('Ctrl Pts',(-0.537146201000055,15.2,11.140652425));
#227735=CARTESIAN_POINT('Ctrl Pts',(-0.537146201000055,11.6,11.140652425));
#227736=CARTESIAN_POINT('Ctrl Pts',(-0.538546181000056,15.2,11.143675461));
#227737=CARTESIAN_POINT('Ctrl Pts',(-0.538546181000056,11.6,11.143675461));
#227738=CARTESIAN_POINT('Ctrl Pts',(-0.539950647000056,15.2,11.14670188));
#227739=CARTESIAN_POINT('Ctrl Pts',(-0.539950647000056,11.6,11.14670188));
#227740=CARTESIAN_POINT('Ctrl Pts',(-0.541359602000057,15.2,11.149731669));
#227741=CARTESIAN_POINT('Ctrl Pts',(-0.541359602000057,11.6,11.149731669));
#227742=CARTESIAN_POINT('Ctrl Pts',(-0.542773047000056,15.2,11.15276482));
#227743=CARTESIAN_POINT('Ctrl Pts',(-0.542773047000056,11.6,11.15276482));
#227744=CARTESIAN_POINT('Ctrl Pts',(-0.544190986000055,15.2,11.155801321));
#227745=CARTESIAN_POINT('Ctrl Pts',(-0.544190986000055,11.6,11.155801321));
#227746=CARTESIAN_POINT('Ctrl Pts',(-0.545613422000055,15.2,11.158841163));
#227747=CARTESIAN_POINT('Ctrl Pts',(-0.545613422000055,11.6,11.158841163));
#227748=CARTESIAN_POINT('Ctrl Pts',(-0.547040355000057,15.2,11.161884336));
#227749=CARTESIAN_POINT('Ctrl Pts',(-0.547040355000057,11.6,11.161884336));
#227750=CARTESIAN_POINT('Ctrl Pts',(-0.548471788000056,15.2,11.164930828));
#227751=CARTESIAN_POINT('Ctrl Pts',(-0.548471788000056,11.6,11.164930828));
#227752=CARTESIAN_POINT('Ctrl Pts',(-0.549907726000055,15.2,11.167980631));
#227753=CARTESIAN_POINT('Ctrl Pts',(-0.549907726000055,11.6,11.167980631));
#227754=CARTESIAN_POINT('Ctrl Pts',(-0.551348168000055,15.2,11.171033732));
#227755=CARTESIAN_POINT('Ctrl Pts',(-0.551348168000055,11.6,11.171033732));
#227756=CARTESIAN_POINT('Ctrl Pts',(-0.552793119000056,15.2,11.174090124));
#227757=CARTESIAN_POINT('Ctrl Pts',(-0.552793119000056,11.6,11.174090124));
#227758=CARTESIAN_POINT('Ctrl Pts',(-0.554242580000055,15.2,11.177149794));
#227759=CARTESIAN_POINT('Ctrl Pts',(-0.554242580000055,11.6,11.177149794));
#227760=CARTESIAN_POINT('Ctrl Pts',(-0.555696553000056,15.2,11.180212734));
#227761=CARTESIAN_POINT('Ctrl Pts',(-0.555696553000056,11.6,11.180212734));
#227762=CARTESIAN_POINT('Ctrl Pts',(-0.557155043000056,15.2,11.183278932));
#227763=CARTESIAN_POINT('Ctrl Pts',(-0.557155043000056,11.6,11.183278932));
#227764=CARTESIAN_POINT('Ctrl Pts',(-0.558618050000056,15.2,11.18634838));
#227765=CARTESIAN_POINT('Ctrl Pts',(-0.558618050000056,11.6,11.18634838));
#227766=CARTESIAN_POINT('Ctrl Pts',(-0.560085576000056,15.2,11.189421065));
#227767=CARTESIAN_POINT('Ctrl Pts',(-0.560085576000056,11.6,11.189421065));
#227768=CARTESIAN_POINT('Ctrl Pts',(-0.561557624000055,15.2,11.192496979));
#227769=CARTESIAN_POINT('Ctrl Pts',(-0.561557624000055,11.6,11.192496979));
#227770=CARTESIAN_POINT('Ctrl Pts',(-0.563034196000055,15.2,11.195576112));
#227771=CARTESIAN_POINT('Ctrl Pts',(-0.563034196000055,11.6,11.195576112));
#227772=CARTESIAN_POINT('Ctrl Pts',(-0.564515296000057,15.2,11.198658454));
#227773=CARTESIAN_POINT('Ctrl Pts',(-0.564515296000057,11.6,11.198658454));
#227774=CARTESIAN_POINT('Ctrl Pts',(-0.566000924000055,15.2,11.201743993));
#227775=CARTESIAN_POINT('Ctrl Pts',(-0.566000924000055,11.6,11.201743993));
#227776=CARTESIAN_POINT('Ctrl Pts',(-0.567491083000055,15.2,11.204832722));
#227777=CARTESIAN_POINT('Ctrl Pts',(-0.567491083000055,11.6,11.204832722));
#227778=CARTESIAN_POINT('Ctrl Pts',(-0.568985776000056,15.2,11.207924627));
#227779=CARTESIAN_POINT('Ctrl Pts',(-0.568985776000056,11.6,11.207924627));
#227780=CARTESIAN_POINT('Ctrl Pts',(-0.570485006000055,15.2,11.211019702));
#227781=CARTESIAN_POINT('Ctrl Pts',(-0.570485006000055,11.6,11.211019702));
#227782=CARTESIAN_POINT('Ctrl Pts',(-0.571988772000056,15.2,11.214117935));
#227783=CARTESIAN_POINT('Ctrl Pts',(-0.571988772000056,11.6,11.214117935));
#227784=CARTESIAN_POINT('Ctrl Pts',(-0.573497080000056,15.2,11.217219317));
#227785=CARTESIAN_POINT('Ctrl Pts',(-0.573497080000056,11.6,11.217219317));
#227786=CARTESIAN_POINT('Ctrl Pts',(-0.575009929000055,15.2,11.220323837));
#227787=CARTESIAN_POINT('Ctrl Pts',(-0.575009929000055,11.6,11.220323837));
#227788=CARTESIAN_POINT('Ctrl Pts',(-0.576527323000056,15.2,11.223431485));
#227789=CARTESIAN_POINT('Ctrl Pts',(-0.576527323000056,11.6,11.223431485));
#227790=CARTESIAN_POINT('Ctrl Pts',(-0.578049263000056,15.2,11.226542252));
#227791=CARTESIAN_POINT('Ctrl Pts',(-0.578049263000056,11.6,11.226542252));
#227792=CARTESIAN_POINT('Ctrl Pts',(-0.579575753000056,15.2,11.229656129));
#227793=CARTESIAN_POINT('Ctrl Pts',(-0.579575753000056,11.6,11.229656129));
#227794=CARTESIAN_POINT('Ctrl Pts',(-0.581106795000055,15.2,11.232773103));
#227795=CARTESIAN_POINT('Ctrl Pts',(-0.581106795000055,11.6,11.232773103));
#227796=CARTESIAN_POINT('Ctrl Pts',(-0.582642388000056,15.2,11.235893167));
#227797=CARTESIAN_POINT('Ctrl Pts',(-0.582642388000056,11.6,11.235893167));
#227798=CARTESIAN_POINT('Ctrl Pts',(-0.584182538000055,15.2,11.239016311));
#227799=CARTESIAN_POINT('Ctrl Pts',(-0.584182538000055,11.6,11.239016311));
#227800=CARTESIAN_POINT('Ctrl Pts',(-0.585727245000056,15.2,11.242142523));
#227801=CARTESIAN_POINT('Ctrl Pts',(-0.585727245000056,11.6,11.242142523));
#227802=CARTESIAN_POINT('Ctrl Pts',(-0.587276512000056,15.2,11.245271795));
#227803=CARTESIAN_POINT('Ctrl Pts',(-0.587276512000056,11.6,11.245271795));
#227804=CARTESIAN_POINT('Ctrl Pts',(-0.588830340000056,15.2,11.248404117));
#227805=CARTESIAN_POINT('Ctrl Pts',(-0.588830340000056,11.6,11.248404117));
#227806=CARTESIAN_POINT('Ctrl Pts',(-0.590388732000056,15.2,11.251539479));
#227807=CARTESIAN_POINT('Ctrl Pts',(-0.590388732000056,11.6,11.251539479));
#227808=CARTESIAN_POINT('Ctrl Pts',(-0.591951691000056,15.2,11.254677871));
#227809=CARTESIAN_POINT('Ctrl Pts',(-0.591951691000056,11.6,11.254677871));
#227810=CARTESIAN_POINT('Ctrl Pts',(-0.593519216000056,15.2,11.257819284));
#227811=CARTESIAN_POINT('Ctrl Pts',(-0.593519216000056,11.6,11.257819284));
#227812=CARTESIAN_POINT('Ctrl Pts',(-0.595091313000056,15.2,11.260963708));
#227813=CARTESIAN_POINT('Ctrl Pts',(-0.595091313000056,11.6,11.260963708));
#227814=CARTESIAN_POINT('Ctrl Pts',(-0.596667980000056,15.2,11.264111132));
#227815=CARTESIAN_POINT('Ctrl Pts',(-0.596667980000056,11.6,11.264111132));
#227816=CARTESIAN_POINT('Ctrl Pts',(-0.598249223000057,15.2,11.267261549));
#227817=CARTESIAN_POINT('Ctrl Pts',(-0.598249223000057,11.6,11.267261549));
#227818=CARTESIAN_POINT('Ctrl Pts',(-0.599835040000055,15.2,11.270414946));
#227819=CARTESIAN_POINT('Ctrl Pts',(-0.599835040000055,11.6,11.270414946));
#227820=CARTESIAN_POINT('Ctrl Pts',(-0.601425437000056,15.2,11.273571316));
#227821=CARTESIAN_POINT('Ctrl Pts',(-0.601425437000056,11.6,11.273571316));
#227822=CARTESIAN_POINT('Ctrl Pts',(-0.603020414000056,15.2,11.276730648));
#227823=CARTESIAN_POINT('Ctrl Pts',(-0.603020414000056,11.6,11.276730648));
#227824=CARTESIAN_POINT('Ctrl Pts',(-0.604619973000055,15.2,11.279892933));
#227825=CARTESIAN_POINT('Ctrl Pts',(-0.604619973000055,11.6,11.279892933));
#227826=CARTESIAN_POINT('Ctrl Pts',(-0.606224115000057,15.2,11.283058162));
#227827=CARTESIAN_POINT('Ctrl Pts',(-0.606224115000057,11.6,11.283058162));
#227828=CARTESIAN_POINT('Ctrl Pts',(-0.607832844000056,15.2,11.286226324));
#227829=CARTESIAN_POINT('Ctrl Pts',(-0.607832844000056,11.6,11.286226324));
#227830=CARTESIAN_POINT('Ctrl Pts',(-0.609446161000056,15.2,11.28939741));
#227831=CARTESIAN_POINT('Ctrl Pts',(-0.609446161000056,11.6,11.28939741));
#227832=CARTESIAN_POINT('Ctrl Pts',(-0.611064067000056,15.2,11.29257141));
#227833=CARTESIAN_POINT('Ctrl Pts',(-0.611064067000056,11.6,11.29257141));
#227834=CARTESIAN_POINT('Ctrl Pts',(-0.612686566000056,15.2,11.295748316));
#227835=CARTESIAN_POINT('Ctrl Pts',(-0.612686566000056,11.6,11.295748316));
#227836=CARTESIAN_POINT('Ctrl Pts',(-0.614313657000055,15.2,11.298928116));
#227837=CARTESIAN_POINT('Ctrl Pts',(-0.614313657000055,11.6,11.298928116));
#227838=CARTESIAN_POINT('Ctrl Pts',(-0.615945345000056,15.2,11.302110802));
#227839=CARTESIAN_POINT('Ctrl Pts',(-0.615945345000056,11.6,11.302110802));
#227840=CARTESIAN_POINT('Ctrl Pts',(-0.617581631000055,15.2,11.305296366));
#227841=CARTESIAN_POINT('Ctrl Pts',(-0.617581631000055,11.6,11.305296366));
#227842=CARTESIAN_POINT('Ctrl Pts',(-0.619222515000055,15.2,11.308484795));
#227843=CARTESIAN_POINT('Ctrl Pts',(-0.619222515000055,11.6,11.308484795));
#227844=CARTESIAN_POINT('Ctrl Pts',(-0.620868001000057,15.2,11.311676083));
#227845=CARTESIAN_POINT('Ctrl Pts',(-0.620868001000057,11.6,11.311676083));
#227846=CARTESIAN_POINT('Ctrl Pts',(-0.622518091000056,15.2,11.314870218));
#227847=CARTESIAN_POINT('Ctrl Pts',(-0.622518091000056,11.6,11.314870218));
#227848=CARTESIAN_POINT('Ctrl Pts',(-0.624172785000056,15.2,11.318067191));
#227849=CARTESIAN_POINT('Ctrl Pts',(-0.624172785000056,11.6,11.318067191));
#227850=CARTESIAN_POINT('Ctrl Pts',(-0.625832086000055,15.2,11.321266994));
#227851=CARTESIAN_POINT('Ctrl Pts',(-0.625832086000055,11.6,11.321266994));
#227852=CARTESIAN_POINT('Ctrl Pts',(-0.627495995000055,15.2,11.324469616));
#227853=CARTESIAN_POINT('Ctrl Pts',(-0.627495995000055,11.6,11.324469616));
#227854=CARTESIAN_POINT('Ctrl Pts',(-0.629164516000056,15.2,11.327675048));
#227855=CARTESIAN_POINT('Ctrl Pts',(-0.629164516000056,11.6,11.327675048));
#227856=CARTESIAN_POINT('Ctrl Pts',(-0.630837649000057,15.2,11.330883282));
#227857=CARTESIAN_POINT('Ctrl Pts',(-0.630837649000057,11.6,11.330883282));
#227858=CARTESIAN_POINT('Ctrl Pts',(-0.632515395000055,15.2,11.334094308));
#227859=CARTESIAN_POINT('Ctrl Pts',(-0.632515395000055,11.6,11.334094308));
#227860=CARTESIAN_POINT('Ctrl Pts',(-0.634197757000056,15.2,11.337308114));
#227861=CARTESIAN_POINT('Ctrl Pts',(-0.634197757000056,11.6,11.337308114));
#227862=CARTESIAN_POINT('Ctrl Pts',(-0.635884738000057,15.2,11.340524695));
#227863=CARTESIAN_POINT('Ctrl Pts',(-0.635884738000057,11.6,11.340524695));
#227864=CARTESIAN_POINT('Ctrl Pts',(-0.637576337000055,15.2,11.343744039));
#227865=CARTESIAN_POINT('Ctrl Pts',(-0.637576337000055,11.6,11.343744039));
#227866=CARTESIAN_POINT('Ctrl Pts',(-0.639272558000057,15.2,11.346966136));
#227867=CARTESIAN_POINT('Ctrl Pts',(-0.639272558000057,11.6,11.346966136));
#227868=CARTESIAN_POINT('Ctrl Pts',(-0.640973402000055,15.2,11.350190979));
#227869=CARTESIAN_POINT('Ctrl Pts',(-0.640973402000055,11.6,11.350190979));
#227870=CARTESIAN_POINT('Ctrl Pts',(-0.642678870000056,15.2,11.353418558));
#227871=CARTESIAN_POINT('Ctrl Pts',(-0.642678870000056,11.6,11.353418558));
#227872=CARTESIAN_POINT('Ctrl Pts',(-0.644388964000056,15.2,11.356648862));
#227873=CARTESIAN_POINT('Ctrl Pts',(-0.644388964000056,11.6,11.356648862));
#227874=CARTESIAN_POINT('Ctrl Pts',(-0.646103687000057,15.2,11.359881884));
#227875=CARTESIAN_POINT('Ctrl Pts',(-0.646103687000057,11.6,11.359881884));
#227876=CARTESIAN_POINT('Ctrl Pts',(-0.647823040000055,15.2,11.363117614));
#227877=CARTESIAN_POINT('Ctrl Pts',(-0.647823040000055,11.6,11.363117614));
#227878=CARTESIAN_POINT('Ctrl Pts',(-0.649547023000056,15.2,11.366356043));
#227879=CARTESIAN_POINT('Ctrl Pts',(-0.649547023000056,11.6,11.366356043));
#227880=CARTESIAN_POINT('Ctrl Pts',(-0.651275640000056,15.2,11.369597161));
#227881=CARTESIAN_POINT('Ctrl Pts',(-0.651275640000056,11.6,11.369597161));
#227882=CARTESIAN_POINT('Ctrl Pts',(-0.653008892000055,15.2,11.37284096));
#227883=CARTESIAN_POINT('Ctrl Pts',(-0.653008892000055,11.6,11.37284096));
#227884=CARTESIAN_POINT('Ctrl Pts',(-0.654746780000056,15.2,11.37608743));
#227885=CARTESIAN_POINT('Ctrl Pts',(-0.654746780000056,11.6,11.37608743));
#227886=CARTESIAN_POINT('Ctrl Pts',(-0.656489306000055,15.2,11.379336561));
#227887=CARTESIAN_POINT('Ctrl Pts',(-0.656489306000055,11.6,11.379336561));
#227888=CARTESIAN_POINT('Ctrl Pts',(-0.658236473000056,15.2,11.382588344));
#227889=CARTESIAN_POINT('Ctrl Pts',(-0.658236473000056,11.6,11.382588344));
#227890=CARTESIAN_POINT('Ctrl Pts',(-0.659988281000056,15.2,11.385842773));
#227891=CARTESIAN_POINT('Ctrl Pts',(-0.659988281000056,11.6,11.385842773));
#227892=CARTESIAN_POINT('Ctrl Pts',(-0.661744730000056,15.2,11.389099835));
#227893=CARTESIAN_POINT('Ctrl Pts',(-0.661744730000056,11.6,11.389099835));
#227894=CARTESIAN_POINT('Ctrl Pts',(-0.663505825000056,15.2,11.392359523));
#227895=CARTESIAN_POINT('Ctrl Pts',(-0.663505825000056,11.6,11.392359523));
#227896=CARTESIAN_POINT('Ctrl Pts',(-0.665271567000056,15.2,11.395621828));
#227897=CARTESIAN_POINT('Ctrl Pts',(-0.665271567000056,11.6,11.395621828));
#227898=CARTESIAN_POINT('Ctrl Pts',(-0.667041956000055,15.2,11.398886739));
#227899=CARTESIAN_POINT('Ctrl Pts',(-0.667041956000055,11.6,11.398886739));
#227900=CARTESIAN_POINT('Ctrl Pts',(-0.668816993000056,15.2,11.402154251));
#227901=CARTESIAN_POINT('Ctrl Pts',(-0.668816993000056,11.6,11.402154251));
#227902=CARTESIAN_POINT('Ctrl Pts',(-0.670596683000056,15.2,11.405424351));
#227903=CARTESIAN_POINT('Ctrl Pts',(-0.670596683000056,11.6,11.405424351));
#227904=CARTESIAN_POINT('Ctrl Pts',(-0.672381024000056,15.2,11.408697033));
#227905=CARTESIAN_POINT('Ctrl Pts',(-0.672381024000056,11.6,11.408697033));
#227906=CARTESIAN_POINT('Ctrl Pts',(-0.674170019000057,15.2,11.411972284));
#227907=CARTESIAN_POINT('Ctrl Pts',(-0.674170019000057,11.6,11.411972284));
#227908=CARTESIAN_POINT('Ctrl Pts',(-0.675963671000056,15.2,11.415250096));
#227909=CARTESIAN_POINT('Ctrl Pts',(-0.675963671000056,11.6,11.415250096));
#227910=CARTESIAN_POINT('Ctrl Pts',(-0.677761979000057,15.2,11.418530461));
#227911=CARTESIAN_POINT('Ctrl Pts',(-0.677761979000057,11.6,11.418530461));
#227912=CARTESIAN_POINT('Ctrl Pts',(-0.679564947000056,15.2,11.421813369));
#227913=CARTESIAN_POINT('Ctrl Pts',(-0.679564947000056,11.6,11.421813369));
#227914=CARTESIAN_POINT('Ctrl Pts',(-0.681372573000055,15.2,11.425098812));
#227915=CARTESIAN_POINT('Ctrl Pts',(-0.681372573000055,11.6,11.425098812));
#227916=CARTESIAN_POINT('Ctrl Pts',(-0.683184863000056,15.2,11.428386781));
#227917=CARTESIAN_POINT('Ctrl Pts',(-0.683184863000056,11.6,11.428386781));
#227918=CARTESIAN_POINT('Ctrl Pts',(-0.685001814000056,15.2,11.431677269));
#227919=CARTESIAN_POINT('Ctrl Pts',(-0.685001814000056,11.6,11.431677269));
#227920=CARTESIAN_POINT('Ctrl Pts',(-0.686823430000055,15.2,11.434970269));
#227921=CARTESIAN_POINT('Ctrl Pts',(-0.686823430000055,11.6,11.434970269));
#227922=CARTESIAN_POINT('Ctrl Pts',(-0.688649711000057,15.2,11.438265769));
#227923=CARTESIAN_POINT('Ctrl Pts',(-0.688649711000057,11.6,11.438265769));
#227924=CARTESIAN_POINT('Ctrl Pts',(-0.690480660000056,15.2,11.441563763));
#227925=CARTESIAN_POINT('Ctrl Pts',(-0.690480660000056,11.6,11.441563763));
#227926=CARTESIAN_POINT('Ctrl Pts',(-0.692316277000057,15.2,11.444864239));
#227927=CARTESIAN_POINT('Ctrl Pts',(-0.692316277000057,11.6,11.444864239));
#227928=CARTESIAN_POINT('Ctrl Pts',(-0.694156564000057,15.2,11.448167187));
#227929=CARTESIAN_POINT('Ctrl Pts',(-0.694156564000057,11.6,11.448167187));
#227930=CARTESIAN_POINT('Ctrl Pts',(-0.696001525000056,15.2,11.451472594));
#227931=CARTESIAN_POINT('Ctrl Pts',(-0.696001525000056,11.6,11.451472594));
#227932=CARTESIAN_POINT('Ctrl Pts',(-0.697851160000056,15.2,11.454780452));
#227933=CARTESIAN_POINT('Ctrl Pts',(-0.697851160000056,11.6,11.454780452));
#227934=CARTESIAN_POINT('Ctrl Pts',(-0.699705469000056,15.2,11.458090751));
#227935=CARTESIAN_POINT('Ctrl Pts',(-0.699705469000056,11.6,11.458090751));
#227936=CARTESIAN_POINT('Ctrl Pts',(-0.701564456000057,15.2,11.461403481));
#227937=CARTESIAN_POINT('Ctrl Pts',(-0.701564456000057,11.6,11.461403481));
#227938=CARTESIAN_POINT('Ctrl Pts',(-0.703428121000057,15.2,11.464718637));
#227939=CARTESIAN_POINT('Ctrl Pts',(-0.703428121000057,11.6,11.464718637));
#227940=CARTESIAN_POINT('Ctrl Pts',(-0.705296465000057,15.2,11.468036216));
#227941=CARTESIAN_POINT('Ctrl Pts',(-0.705296465000057,11.6,11.468036216));
#227942=CARTESIAN_POINT('Ctrl Pts',(-0.707169486000057,15.2,11.471356215));
#227943=CARTESIAN_POINT('Ctrl Pts',(-0.707169486000057,11.6,11.471356215));
#227944=CARTESIAN_POINT('Ctrl Pts',(-0.708671646000055,15.2,11.474014149));
#227945=CARTESIAN_POINT('Ctrl Pts',(-0.708671646000055,11.6,11.474014149));
#227946=CARTESIAN_POINT('Ctrl Pts',(-0.709800371000057,15.2,11.476008688));
#227947=CARTESIAN_POINT('Ctrl Pts',(-0.709800371000057,11.6,11.476008688));
#227948=CARTESIAN_POINT('Ctrl Pts',(-0.710553791000056,15.2,11.477338864));
#227949=CARTESIAN_POINT('Ctrl Pts',(-0.710553791000056,11.6,11.477338864));
#227950=CARTESIAN_POINT('Ctrl Pts',(-0.710930735000056,15.2,11.478004073));
#227951=CARTESIAN_POINT('Ctrl Pts',(-0.710930735000056,11.6,11.478004073));
#227952=CARTESIAN_POINT('Ctrl Pts',(-0.292001930000056,15.2,10.370890024));
#227953=CARTESIAN_POINT('Ctrl Pts',(-0.29220549901488,15.2,10.372665048257));
#227954=CARTESIAN_POINT('Ctrl Pts',(-0.292420934152544,15.2,10.3744962450942));
#227955=CARTESIAN_POINT('Ctrl Pts',(-0.29264874396675,15.2,10.3763825865516));
#227956=CARTESIAN_POINT('Ctrl Pts',(-0.292877652395031,15.2,10.378278024901));
#227957=CARTESIAN_POINT('Ctrl Pts',(-0.293119060472346,15.2,10.3802291369147));
#227958=CARTESIAN_POINT('Ctrl Pts',(-0.293373491749677,15.2,10.3822349054607));
#227959=CARTESIAN_POINT('Ctrl Pts',(-0.293712733429673,15.2,10.3849092633399));
#227960=CARTESIAN_POINT('Ctrl Pts',(-0.294075124384088,15.2,10.3876807806492));
#227961=CARTESIAN_POINT('Ctrl Pts',(-0.294461852490938,15.2,10.3905471173926));
#227962=CARTESIAN_POINT('Ctrl Pts',(-0.294751898564489,15.2,10.3926968699013));
#227963=CARTESIAN_POINT('Ctrl Pts',(-0.295055632160027,15.2,10.3948999596624));
#227964=CARTESIAN_POINT('Ctrl Pts',(-0.295373532483221,15.2,10.3971554301739));
#227965=CARTESIAN_POINT('Ctrl Pts',(-0.295691432806416,15.2,10.3994109006854));
#227966=CARTESIAN_POINT('Ctrl Pts',(-0.296023501634165,15.2,10.4017187517486));
#227967=CARTESIAN_POINT('Ctrl Pts',(-0.296370202703911,15.2,10.4040780504928));
#227968=CARTESIAN_POINT('Ctrl Pts',(-0.29671690380515,15.2,10.4064373494512));
#227969=CARTESIAN_POINT('Ctrl Pts',(-0.297078237096281,15.2,10.4088480977447));
#227970=CARTESIAN_POINT('Ctrl Pts',(-0.297454650303147,15.2,10.4113093850048));
#227971=CARTESIAN_POINT('Ctrl Pts',(-0.297893798993205,15.2,10.4141808864729));
#227972=CARTESIAN_POINT('Ctrl Pts',(-0.298353477225178,15.2,10.4171211802824));
#227973=CARTESIAN_POINT('Ctrl Pts',(-0.298834369221771,15.2,10.4201288594939));
#227974=CARTESIAN_POINT('Ctrl Pts',(-0.299246562409847,15.2,10.4227068705477));
#227975=CARTESIAN_POINT('Ctrl Pts',(-0.299674342220718,15.2,10.4253343918266));
#227976=CARTESIAN_POINT('Ctrl Pts',(-0.300118128017998,15.2,10.4280105622756));
#227977=CARTESIAN_POINT('Ctrl Pts',(-0.300561913774966,15.2,10.4306867324815));
#227978=CARTESIAN_POINT('Ctrl Pts',(-0.301021703625674,15.2,10.4334115520424));
#227979=CARTESIAN_POINT('Ctrl Pts',(-0.301497903525024,15.2,10.4361841820249));
#227980=CARTESIAN_POINT('Ctrl Pts',(-0.301974103424374,15.2,10.4389568120074));
#227981=CARTESIAN_POINT('Ctrl Pts',(-0.302466713969813,15.2,10.4417772508279));
#227982=CARTESIAN_POINT('Ctrl Pts',(-0.30297612672579,15.2,10.4446446819476));
#227983=CARTESIAN_POINT('Ctrl Pts',(-0.30348553952804,15.2,10.4475121133278));
#227984=CARTESIAN_POINT('Ctrl Pts',(-0.304011754820135,15.2,10.4504265334164));
#227985=CARTESIAN_POINT('Ctrl Pts',(-0.304555152600927,15.2,10.453387143831));
#227986=CARTESIAN_POINT('Ctrl Pts',(-0.305189116604479,15.2,10.4568411889112));
#227987=CARTESIAN_POINT('Ctrl Pts',(-0.305846467136494,15.2,10.4603581000338));
#227988=CARTESIAN_POINT('Ctrl Pts',(-0.306527791710242,15.2,10.463936641445));
#227989=CARTESIAN_POINT('Ctrl Pts',(-0.307111784270228,15.2,10.4670039630128));
#227990=CARTESIAN_POINT('Ctrl Pts',(-0.307713387740921,15.2,10.4701165605774));
#227991=CARTESIAN_POINT('Ctrl Pts',(-0.308332958359225,15.2,10.4732736733357));
#227992=CARTESIAN_POINT('Ctrl Pts',(-0.308952528921253,15.2,10.4764307858073));
#227993=CARTESIAN_POINT('Ctrl Pts',(-0.309590066523853,15.2,10.4796324144928));
#227994=CARTESIAN_POINT('Ctrl Pts',(-0.310245916000022,15.2,10.4828778109582));
#227995=CARTESIAN_POINT('Ctrl Pts',(-0.310901765476191,15.2,10.4861232074236));
#227996=CARTESIAN_POINT('Ctrl Pts',(-0.311575927099688,15.2,10.4894123722348));
#227997=CARTESIAN_POINT('Ctrl Pts',(-0.312268733691382,15.2,10.4927445759443));
#227998=CARTESIAN_POINT('Ctrl Pts',(-0.312961540346006,15.2,10.4960767799566));
#227999=CARTESIAN_POINT('Ctrl Pts',(-0.313672994921877,15.2,10.4994520210167));
#228000=CARTESIAN_POINT('Ctrl Pts',(-0.31440341779631,15.2,10.5028695858724));
#228001=CARTESIAN_POINT('Ctrl Pts',(-0.315620789121003,15.2,10.5085655266779));
#228002=CARTESIAN_POINT('Ctrl Pts',(-0.316890865154458,15.2,10.5143790241343));
#228003=CARTESIAN_POINT('Ctrl Pts',(-0.318215080913419,15.2,10.5203068568622));
#228004=CARTESIAN_POINT('Ctrl Pts',(-0.319009610455399,15.2,10.5238635568866));
#228005=CARTESIAN_POINT('Ctrl Pts',(-0.31982363092424,15.2,10.5274614183316));
#228006=CARTESIAN_POINT('Ctrl Pts',(-0.320657440553881,15.2,10.5310997671984));
#228007=CARTESIAN_POINT('Ctrl Pts',(-0.321491250107784,15.2,10.5347381157346));
#228008=CARTESIAN_POINT('Ctrl Pts',(-0.322344850352457,15.2,10.5384169472249));
#228009=CARTESIAN_POINT('Ctrl Pts',(-0.323218530741291,15.2,10.5421356000232));
#228010=CARTESIAN_POINT('Ctrl Pts',(-0.324092211130125,15.2,10.5458542528215));
#228011=CARTESIAN_POINT('Ctrl Pts',(-0.324985972868309,15.2,10.549612724485));
#228012=CARTESIAN_POINT('Ctrl Pts',(-0.325900097167055,15.2,10.553410366261));
#228013=CARTESIAN_POINT('Ctrl Pts',(-0.326814221548833,15.2,10.557208008382));
#228014=CARTESIAN_POINT('Ctrl Pts',(-0.327748709641514,15.2,10.5610448175429));
#228015=CARTESIAN_POINT('Ctrl Pts',(-0.3287038350758,15.2,10.5649201568666));
#228016=CARTESIAN_POINT('Ctrl Pts',(-0.329499772894327,15.2,10.568149606127));
#228017=CARTESIAN_POINT('Ctrl Pts',(-0.330310042073378,15.2,10.5714058104271));
#228018=CARTESIAN_POINT('Ctrl Pts',(-0.331134798116238,15.2,10.5746884079293));
#228019=CARTESIAN_POINT('Ctrl Pts',(-0.331959554159098,15.2,10.5779710054315));
#228020=CARTESIAN_POINT('Ctrl Pts',(-0.332798795749401,15.2,10.5812799938229));
#228021=CARTESIAN_POINT('Ctrl Pts',(-0.333652674361709,15.2,10.5846150172278));
#228022=CARTESIAN_POINT('Ctrl Pts',(-0.334506552880944,15.2,10.5879500402692));
#228023=CARTESIAN_POINT('Ctrl Pts',(-0.335375070626419,15.2,10.5913110967615));
#228024=CARTESIAN_POINT('Ctrl Pts',(-0.336258370667821,15.2,10.5946978340986));
#228025=CARTESIAN_POINT('Ctrl Pts',(-0.337318330890808,15.2,10.5987619195676));
#228026=CARTESIAN_POINT('Ctrl Pts',(-0.338399582482505,15.2,10.6028629845068));
#228027=CARTESIAN_POINT('Ctrl Pts',(-0.339502371543545,15.2,10.6070004289839));
#228028=CARTESIAN_POINT('Ctrl Pts',(-0.340605160504416,15.2,10.6111378730852));
#228029=CARTESIAN_POINT('Ctrl Pts',(-0.341729486777676,15.2,10.6153116960487));
#228030=CARTESIAN_POINT('Ctrl Pts',(-0.3428755928245,15.2,10.619521308248));
#228031=CARTESIAN_POINT('Ctrl Pts',(-0.344021698871324,15.2,10.6237309204474));
#228032=CARTESIAN_POINT('Ctrl Pts',(-0.345189583431716,15.2,10.6279763233579));
#228033=CARTESIAN_POINT('Ctrl Pts',(-0.346379481553657,15.2,10.6322569345333));
#228034=CARTESIAN_POINT('Ctrl Pts',(-0.34756937978368,15.2,10.6365375460976));
#228035=CARTESIAN_POINT('Ctrl Pts',(-0.348781291647598,15.2,10.6408533677311));
#228036=CARTESIAN_POINT('Ctrl Pts',(-0.350015443861127,15.2,10.6452038266875));
#228037=CARTESIAN_POINT('Ctrl Pts',(-0.35145528794209,15.2,10.6502793615439));
#228038=CARTESIAN_POINT('Ctrl Pts',(-0.352925406743964,15.2,10.6554020458361));
#228039=CARTESIAN_POINT('Ctrl Pts',(-0.354426147343142,15.2,10.660570986192));
#228040=CARTESIAN_POINT('Ctrl Pts',(-0.355712496578379,15.2,10.6650015070145));
#228041=CARTESIAN_POINT('Ctrl Pts',(-0.357021345021807,15.2,10.6694660135717));
#228042=CARTESIAN_POINT('Ctrl Pts',(-0.358352906162216,15.2,10.6739639554601));
#228043=CARTESIAN_POINT('Ctrl Pts',(-0.359462540385416,15.2,10.6777122401629));
#228044=CARTESIAN_POINT('Ctrl Pts',(-0.360587946892452,15.2,10.6814837430611));
#228045=CARTESIAN_POINT('Ctrl Pts',(-0.361729247657636,15.2,10.6852781509796));
#228046=CARTESIAN_POINT('Ctrl Pts',(-0.36287054842282,15.2,10.6890725588981));
#228047=CARTESIAN_POINT('Ctrl Pts',(-0.364027741913281,15.2,10.6928898715004));
#228048=CARTESIAN_POINT('Ctrl Pts',(-0.365200947678475,15.2,10.6967297802522));
#228049=CARTESIAN_POINT('Ctrl Pts',(-0.36637415344367,15.2,10.700569689004));
#228050=CARTESIAN_POINT('Ctrl Pts',(-0.36756336964523,15.2,10.7044321930117));
#228051=CARTESIAN_POINT('Ctrl Pts',(-0.368768713674349,15.2,10.7083169859997));
#228052=CARTESIAN_POINT('Ctrl Pts',(-0.369974057572086,15.2,10.7122017785643));
#228053=CARTESIAN_POINT('Ctrl Pts',(-0.371195528302116,15.2,10.7161088606771));
#228054=CARTESIAN_POINT('Ctrl Pts',(-0.372433238096463,15.2,10.7200379299694));
#228055=CARTESIAN_POINT('Ctrl Pts',(-0.373670948025721,15.2,10.7239669996899));
#228056=CARTESIAN_POINT('Ctrl Pts',(-0.374924897418553,15.2,10.7279180584377));
#228057=CARTESIAN_POINT('Ctrl Pts',(-0.376195196375531,15.2,10.7318908049636));
#228058=CARTESIAN_POINT('Ctrl Pts',(-0.377211435596498,15.2,10.7350690023576));
#228059=CARTESIAN_POINT('Ctrl Pts',(-0.37823813745333,15.2,10.7382610825544));
#228060=CARTESIAN_POINT('Ctrl Pts',(-0.379275358792392,15.2,10.7414668912438));
#228061=CARTESIAN_POINT('Ctrl Pts',(-0.380312579990132,15.2,10.7446726994963));
#228062=CARTESIAN_POINT('Ctrl Pts',(-0.381360319825712,15.2,10.7478922394315));
#228063=CARTESIAN_POINT('Ctrl Pts',(-0.382418632293648,15.2,10.7511253597213));
#228064=CARTESIAN_POINT('Ctrl Pts',(-0.383476944905779,15.2,10.7543584804516));
#228065=CARTESIAN_POINT('Ctrl Pts',(-0.384545831121746,15.2,10.7576051824751));
#228066=CARTESIAN_POINT('Ctrl Pts',(-0.385625342458339,15.2,10.7608653170416));
#228067=CARTESIAN_POINT('Ctrl Pts',(-0.386704853794932,15.2,10.7641254516081));
#228068=CARTESIAN_POINT('Ctrl Pts',(-0.387794991685586,15.2,10.7673990188624));
#228069=CARTESIAN_POINT('Ctrl Pts',(-0.388895806413339,15.2,10.7706858728207));
#228070=CARTESIAN_POINT('Ctrl Pts',(-0.390271824598052,15.2,10.7747944395968));
#228071=CARTESIAN_POINT('Ctrl Pts',(-0.391664529609553,15.2,10.7789237657556));
#228072=CARTESIAN_POINT('Ctrl Pts',(-0.39307401681565,15.2,10.7830735691905));
#228073=CARTESIAN_POINT('Ctrl Pts',(-0.394201606764888,15.2,10.7863934124811));
#228074=CARTESIAN_POINT('Ctrl Pts',(-0.395339938962376,15.2,10.789726360612));
#228075=CARTESIAN_POINT('Ctrl Pts',(-0.396489063525012,15.2,10.7930722700166));
#228076=CARTESIAN_POINT('Ctrl Pts',(-0.397638188087647,15.2,10.7964181794212));
#228077=CARTESIAN_POINT('Ctrl Pts',(-0.398798103118186,15.2,10.7997770520689));
#228078=CARTESIAN_POINT('Ctrl Pts',(-0.399968859683108,15.2,10.8031487423096));
#228079=CARTESIAN_POINT('Ctrl Pts',(-0.401139616088514,15.2,10.8065204320908));
#228080=CARTESIAN_POINT('Ctrl Pts',(-0.402321214349639,15.2,10.8099049426655));
#228081=CARTESIAN_POINT('Ctrl Pts',(-0.403513700757539,15.2,10.8133021315143));
#228082=CARTESIAN_POINT('Ctrl Pts',(-0.404706187327917,15.2,10.816699320826));
#228083=CARTESIAN_POINT('Ctrl Pts',(-0.405909563539603,15.2,10.8201091892523));
#228084=CARTESIAN_POINT('Ctrl Pts',(-0.407123875440221,15.2,10.8235315960512));
#228085=CARTESIAN_POINT('Ctrl Pts',(-0.408338187175388,15.2,10.8269540023837));
#228086=CARTESIAN_POINT('Ctrl Pts',(-0.409563434453614,15.2,10.8303889480148));
#228087=CARTESIAN_POINT('Ctrl Pts',(-0.410799665407387,15.2,10.8338362950099));
#228088=CARTESIAN_POINT('Ctrl Pts',(-0.412654011922266,15.2,10.8390073157375));
#228089=CARTESIAN_POINT('Ctrl Pts',(-0.41453306750502,15.2,10.8442062380553));
#228090=CARTESIAN_POINT('Ctrl Pts',(-0.416436989017487,15.2,10.8494326006969));
#228091=CARTESIAN_POINT('Ctrl Pts',(-0.417706270141092,15.2,10.8529168427745));
#228092=CARTESIAN_POINT('Ctrl Pts',(-0.418986601168512,15.2,10.8564132814948));
#228093=CARTESIAN_POINT('Ctrl Pts',(-0.420278027016682,15.2,10.8599217797416));
#228094=CARTESIAN_POINT('Ctrl Pts',(-0.421892309238915,15.2,10.8643074023111));
#228095=CARTESIAN_POINT('Ctrl Pts',(-0.423523927621153,15.2,10.8687118704544));
#228096=CARTESIAN_POINT('Ctrl Pts',(-0.425172965684246,15.2,10.8731349220024));
#228097=CARTESIAN_POINT('Ctrl Pts',(-0.426492196026873,15.2,10.8766733629514));
#228098=CARTESIAN_POINT('Ctrl Pts',(-0.42782257640538,15.2,10.8802236975433));
#228099=CARTESIAN_POINT('Ctrl Pts',(-0.429164146239003,15.2,10.8837857919175));
#228100=CARTESIAN_POINT('Ctrl Pts',(-0.430505716255415,15.2,10.8873478867771));
#228101=CARTESIAN_POINT('Ctrl Pts',(-0.431858479650664,15.2,10.8909217432767));
#228102=CARTESIAN_POINT('Ctrl Pts',(-0.433222474225011,15.2,10.8945072282499));
#228103=CARTESIAN_POINT('Ctrl Pts',(-0.434586468799358,15.2,10.8980927132232));
#228104=CARTESIAN_POINT('Ctrl Pts',(-0.435961696255549,15.2,10.9016898279004));
#228105=CARTESIAN_POINT('Ctrl Pts',(-0.437348197443381,15.2,10.9052984425983));
#228106=CARTESIAN_POINT('Ctrl Pts',(-0.439081323644806,15.2,10.9098092102331));
#228107=CARTESIAN_POINT('Ctrl Pts',(-0.440832065601813,15.2,10.9143379434412));
#228108=CARTESIAN_POINT('Ctrl Pts',(-0.442600500060369,15.2,10.9188843921803));
#228109=CARTESIAN_POINT('Ctrl Pts',(-0.444015247858525,15.2,10.9225215517662));
#228110=CARTESIAN_POINT('Ctrl Pts',(-0.445441320160564,15.2,10.9261700500227));
#228111=CARTESIAN_POINT('Ctrl Pts',(-0.446878754016672,15.2,10.9298297569999));
#228112=CARTESIAN_POINT('Ctrl Pts',(-0.449034904604986,15.2,10.9353193169671));
#228113=CARTESIAN_POINT('Ctrl Pts',(-0.451216621466244,15.2,10.940834099765));
#228114=CARTESIAN_POINT('Ctrl Pts',(-0.4534240330782,15.2,10.9463736779224));
#228115=CARTESIAN_POINT('Ctrl Pts',(-0.454895640953175,15.2,10.9500667303629));
#228116=CARTESIAN_POINT('Ctrl Pts',(-0.456378668998441,15.2,10.9537708021451));
#228117=CARTESIAN_POINT('Ctrl Pts',(-0.457873153580622,15.2,10.9574857695704));
#228118=CARTESIAN_POINT('Ctrl Pts',(-0.460114880250268,15.2,10.9630582202023));
#228119=CARTESIAN_POINT('Ctrl Pts',(-0.462382385784579,15.2,10.968655181899));
#228120=CARTESIAN_POINT('Ctrl Pts',(-0.464675793116795,15.2,10.9742762396937));
#228121=CARTESIAN_POINT('Ctrl Pts',(-0.466969200657329,15.2,10.979897297999));
#228122=CARTESIAN_POINT('Ctrl Pts',(-0.469288508567733,15.2,10.9855424511073));
#228123=CARTESIAN_POINT('Ctrl Pts',(-0.471633837280656,15.2,10.9912112855845));
#228124=CARTESIAN_POINT('Ctrl Pts',(-0.473197389542904,15.2,10.9949905080544));
#228125=CARTESIAN_POINT('Ctrl Pts',(-0.474772506335361,15.2,10.9987802561602));
#228126=CARTESIAN_POINT('Ctrl Pts',(-0.476359222490603,15.2,11.0025804072557));
#228127=CARTESIAN_POINT('Ctrl Pts',(-0.477945938862034,15.2,11.0063805588689));
#228128=CARTESIAN_POINT('Ctrl Pts',(-0.479544253288192,15.2,11.0101911138653));
#228129=CARTESIAN_POINT('Ctrl Pts',(-0.481154200988244,15.2,11.014011953408));
#228130=CARTESIAN_POINT('Ctrl Pts',(-0.482764148468941,15.2,11.01783279243));
#228131=CARTESIAN_POINT('Ctrl Pts',(-0.484385728903638,15.2,11.0216639138201));
#228132=CARTESIAN_POINT('Ctrl Pts',(-0.486018975158269,15.2,11.0255052002277));
#228133=CARTESIAN_POINT('Ctrl Pts',(-0.487652221635429,15.2,11.0293464871587));
#228134=CARTESIAN_POINT('Ctrl Pts',(-0.48929713271086,15.2,11.0331979375784));
#228135=CARTESIAN_POINT('Ctrl Pts',(-0.490953743773792,15.2,11.0370594340937));
#228136=CARTESIAN_POINT('Ctrl Pts',(-0.493024507489601,15.2,11.0418863044747));
#228137=CARTESIAN_POINT('Ctrl Pts',(-0.49511354770195,15.2,11.0467288702119));
#228138=CARTESIAN_POINT('Ctrl Pts',(-0.497220930550665,15.2,11.0515869028521));
#228139=CARTESIAN_POINT('Ctrl Pts',(-0.498906836691815,15.2,11.0554733286465));
#228140=CARTESIAN_POINT('Ctrl Pts',(-0.500604480267564,15.2,11.0593696530007));
#228141=CARTESIAN_POINT('Ctrl Pts',(-0.502313893127041,15.2,11.0632757606807));
#228142=CARTESIAN_POINT('Ctrl Pts',(-0.504450659376066,15.2,11.0681583956799));
#228143=CARTESIAN_POINT('Ctrl Pts',(-0.506605814700106,15.2,11.0730563131416));
#228144=CARTESIAN_POINT('Ctrl Pts',(-0.508779417765496,15.2,11.0779692914973));
#228145=CARTESIAN_POINT('Ctrl Pts',(-0.510518300312577,15.2,11.081899674396));
#228146=CARTESIAN_POINT('Ctrl Pts',(-0.512268990654795,15.2,11.0858396936878));
#228147=CARTESIAN_POINT('Ctrl Pts',(-0.514031517029858,15.2,11.089789237404));
#228148=CARTESIAN_POINT('Ctrl Pts',(-0.515794043164776,15.2,11.0937387805822));
#228149=CARTESIAN_POINT('Ctrl Pts',(-0.517568405928673,15.2,11.0976978474562));
#228150=CARTESIAN_POINT('Ctrl Pts',(-0.519354634670766,15.2,11.101666323909));
#228151=CARTESIAN_POINT('Ctrl Pts',(-0.521587420780912,15.2,11.1066269198804));
#228152=CARTESIAN_POINT('Ctrl Pts',(-0.523838745549627,15.2,11.1116022162968));
#228153=CARTESIAN_POINT('Ctrl Pts',(-0.52610866674044,15.2,11.1165919972222));
#228154=CARTESIAN_POINT('Ctrl Pts',(-0.52792460379206,15.2,11.1205838221801));
#228155=CARTESIAN_POINT('Ctrl Pts',(-0.529752441729908,15.2,11.1245849154279));
#228156=CARTESIAN_POINT('Ctrl Pts',(-0.531592208775819,15.2,11.1285951651473));
#228157=CARTESIAN_POINT('Ctrl Pts',(-0.533891917457873,15.2,11.1336079770234));
#228158=CARTESIAN_POINT('Ctrl Pts',(-0.536210264054167,15.2,11.1386350964804));
#228159=CARTESIAN_POINT('Ctrl Pts',(-0.5385473028057,15.2,11.1436763073843));
#228160=CARTESIAN_POINT('Ctrl Pts',(-0.539949526005673,15.2,11.1467010338168));
#228161=CARTESIAN_POINT('Ctrl Pts',(-0.541358478453927,15.2,11.1497308329453));
#228162=CARTESIAN_POINT('Ctrl Pts',(-0.54277417076564,15.2,11.1527656581122));
#228163=CARTESIAN_POINT('Ctrl Pts',(-0.545133658037555,15.2,11.1578237002407));
#228164=CARTESIAN_POINT('Ctrl Pts',(-0.547511868750903,15.2,11.1628957042696));
#228165=CARTESIAN_POINT('Ctrl Pts',(-0.549908852363539,15.2,11.1679814562152));
#228166=CARTESIAN_POINT('Ctrl Pts',(-0.551347042478867,15.2,11.1710329072716));
#228167=CARTESIAN_POINT('Ctrl Pts',(-0.552791990943856,15.2,11.1740893077445));
#228168=CARTESIAN_POINT('Ctrl Pts',(-0.554243708183353,15.2,11.1771506118004));
#228169=CARTESIAN_POINT('Ctrl Pts',(-0.55569542542285,15.2,11.1802119158562));
#228170=CARTESIAN_POINT('Ctrl Pts',(-0.557153913097895,15.2,11.183278123767));
#228171=CARTESIAN_POINT('Ctrl Pts',(-0.558619179759674,15.2,11.1863491892944));
#228172=CARTESIAN_POINT('Ctrl Pts',(-0.560084446421453,15.2,11.1894202548218));
#228173=CARTESIAN_POINT('Ctrl Pts',(-0.561556491845709,15.2,11.1924961777451));
#228174=CARTESIAN_POINT('Ctrl Pts',(-0.56303532796533,15.2,11.1955769142305));
#228175=CARTESIAN_POINT('Ctrl Pts',(-0.564514164084952,15.2,11.1986576507159));
#228176=CARTESIAN_POINT('Ctrl Pts',(-0.565999790142274,15.2,11.2017431996759));
#228177=CARTESIAN_POINT('Ctrl Pts',(-0.567492216337446,15.2,11.2048335157299));
#228178=CARTESIAN_POINT('Ctrl Pts',(-0.569482118111756,15.2,11.2089539375094));
#228179=CARTESIAN_POINT('Ctrl Pts',(-0.571484110512555,15.2,11.2130828347872));
#228180=CARTESIAN_POINT('Ctrl Pts',(-0.57349821545644,15.2,11.2172201018466));
#228181=CARTESIAN_POINT('Ctrl Pts',(-0.575008794027143,15.2,11.2203230518592));
#228182=CARTESIAN_POINT('Ctrl Pts',(-0.576526185283166,15.2,11.2234307084851));
#228183=CARTESIAN_POINT('Ctrl Pts',(-0.578050400484732,15.2,11.2265430294695));
#228184=CARTESIAN_POINT('Ctrl Pts',(-0.579574615686298,15.2,11.2296553504539));
#228185=CARTESIAN_POINT('Ctrl Pts',(-0.581105655497523,15.2,11.2327723339964));
#228186=CARTESIAN_POINT('Ctrl Pts',(-0.582643527198618,15.2,11.2358939369805));
#228187=CARTESIAN_POINT('Ctrl Pts',(-0.584181398899714,15.2,11.2390155399646));
#228188=CARTESIAN_POINT('Ctrl Pts',(-0.585726104487975,15.2,11.2421417611063));
#228189=CARTESIAN_POINT('Ctrl Pts',(-0.587277652097671,15.2,11.2452725571588));
#228190=CARTESIAN_POINT('Ctrl Pts',(-0.589346382431842,15.2,11.2494469522746));
#228191=CARTESIAN_POINT('Ctrl Pts',(-0.591427277434147,15.2,11.2536294800221));
#228192=CARTESIAN_POINT('Ctrl Pts',(-0.59352035910457,15.2,11.2578200370843));
#228193=CARTESIAN_POINT('Ctrl Pts',(-0.595090170214797,15.2,11.2609629545955));
#228194=CARTESIAN_POINT('Ctrl Pts',(-0.596666836451787,15.2,11.2641103879864));
#228195=CARTESIAN_POINT('Ctrl Pts',(-0.598250366568114,15.2,11.2672622940528));
#228196=CARTESIAN_POINT('Ctrl Pts',(-0.599833896684441,15.2,11.2704142001192));
#228197=CARTESIAN_POINT('Ctrl Pts',(-0.601424291416032,15.2,11.2735705785976));
#228198=CARTESIAN_POINT('Ctrl Pts',(-0.60302155949023,15.2,11.2767313862471));
#228199=CARTESIAN_POINT('Ctrl Pts',(-0.60568367304395,15.2,11.2819993991877));
#228200=CARTESIAN_POINT('Ctrl Pts',(-0.608364877499989,15.2,11.2872797161888));
#228201=CARTESIAN_POINT('Ctrl Pts',(-0.611065215208339,15.2,11.2925721364666));
#228202=CARTESIAN_POINT('Ctrl Pts',(-0.612685417774481,15.2,11.2957475885179));
#228203=CARTESIAN_POINT('Ctrl Pts',(-0.614312507332004,15.2,11.2989273971024));
#228204=CARTESIAN_POINT('Ctrl Pts',(-0.615946494313679,15.2,11.3021115211113));
#228205=CARTESIAN_POINT('Ctrl Pts',(-0.617580481295354,15.2,11.3052956451202));
#228206=CARTESIAN_POINT('Ctrl Pts',(-0.619221363601611,15.2,11.3084840835705));
#228207=CARTESIAN_POINT('Ctrl Pts',(-0.620869151624126,15.2,11.3116767940789));
#228208=CARTESIAN_POINT('Ctrl Pts',(-0.622516939945989,15.2,11.3148695051673));
#228209=CARTESIAN_POINT('Ctrl Pts',(-0.62417163293648,15.2,11.318066487332));
#228210=CARTESIAN_POINT('Ctrl Pts',(-0.625833238387245,15.2,11.3212676994645));
#228211=CARTESIAN_POINT('Ctrl Pts',(-0.628048711818499,15.2,11.3255359813386));
#228212=CARTESIAN_POINT('Ctrl Pts',(-0.63027647683816,15.2,11.3298117829972));
#228213=CARTESIAN_POINT('Ctrl Pts',(-0.632516548998486,15.2,11.3340950030554));
#228214=CARTESIAN_POINT('Ctrl Pts',(-0.634196603195032,15.2,11.3373074182449));
#228215=CARTESIAN_POINT('Ctrl Pts',(-0.635883582144314,15.2,11.3405240072497));
#228216=CARTESIAN_POINT('Ctrl Pts',(-0.637577492290494,15.2,11.343744726924));
#228217=CARTESIAN_POINT('Ctrl Pts',(-0.639271402436673,15.2,11.3469654465983));
#228218=CARTESIAN_POINT('Ctrl Pts',(-0.640972244990714,15.2,11.3501902979473));
#228219=CARTESIAN_POINT('Ctrl Pts',(-0.642680026136049,15.2,11.3534192385794));
#228220=CARTESIAN_POINT('Ctrl Pts',(-0.64438780759163,15.2,11.3566481797981));
#228221=CARTESIAN_POINT('Ctrl Pts',(-0.646102529490854,15.2,11.359881210268));
#228222=CARTESIAN_POINT('Ctrl Pts',(-0.647824197908676,15.2,11.3631182894473));
#228223=CARTESIAN_POINT('Ctrl Pts',(-0.650119755277823,15.2,11.3674343940396));
#228224=CARTESIAN_POINT('Ctrl Pts',(-0.652427663408144,15.2,11.3717576959785));
#228225=CARTESIAN_POINT('Ctrl Pts',(-0.654747939506772,15.2,11.3760880952554));
#228226=CARTESIAN_POINT('Ctrl Pts',(-0.657068215921539,15.2,11.3804184951222));
#228227=CARTESIAN_POINT('Ctrl Pts',(-0.659400862054365,15.2,11.384755992845));
#228228=CARTESIAN_POINT('Ctrl Pts',(-0.6617458918501,15.2,11.3891004921936));
#228229=CARTESIAN_POINT('Ctrl Pts',(-0.663504664037145,15.2,11.3923588664091));
#228230=CARTESIAN_POINT('Ctrl Pts',(-0.665270405040484,15.2,11.3956211789077));
#228231=CARTESIAN_POINT('Ctrl Pts',(-0.667043118226683,15.2,11.3988873895394));
#228232=CARTESIAN_POINT('Ctrl Pts',(-0.669406735700934,15.2,11.4032423368505));
#228233=CARTESIAN_POINT('Ctrl Pts',(-0.671782751502728,15.2,11.4076042159778));
#228234=CARTESIAN_POINT('Ctrl Pts',(-0.674171182870168,15.2,11.4119729236161));
#228235=CARTESIAN_POINT('Ctrl Pts',(-0.675962506477103,15.2,11.4152494544936));
#228236=CARTESIAN_POINT('Ctrl Pts',(-0.677760814073012,15.2,11.4185298273539));
#228237=CARTESIAN_POINT('Ctrl Pts',(-0.679566111173121,15.2,11.4218140020257));
#228238=CARTESIAN_POINT('Ctrl Pts',(-0.681371408601192,15.2,11.4250981772941));
#228239=CARTESIAN_POINT('Ctrl Pts',(-0.683183696681263,15.2,11.4283861539887));
#228240=CARTESIAN_POINT('Ctrl Pts',(-0.685002980613288,15.2,11.4316778976759));
#228241=CARTESIAN_POINT('Ctrl Pts',(-0.687428691971815,15.2,11.4360668882622));
#228242=CARTESIAN_POINT('Ctrl Pts',(-0.689866841517626,15.2,11.4404625755866));
#228243=CARTESIAN_POINT('Ctrl Pts',(-0.692317444316457,15.2,11.4448648566151));
#228244=CARTESIAN_POINT('Ctrl Pts',(-0.694155396499053,15.2,11.4481665675365));
#228245=CARTESIAN_POINT('Ctrl Pts',(-0.696000355984013,15.2,11.4514719838984));
#228246=CARTESIAN_POINT('Ctrl Pts',(-0.697852328175099,15.2,11.4547810616098));
#228247=CARTESIAN_POINT('Ctrl Pts',(-0.699704300366184,15.2,11.4580901393211));
#228248=CARTESIAN_POINT('Ctrl Pts',(-0.701563285928658,15.2,11.461402874898));
#228249=CARTESIAN_POINT('Ctrl Pts',(-0.703429290318224,15.2,11.464719242027));
#228250=CARTESIAN_POINT('Ctrl Pts',(-0.705917296396971,15.2,11.4691410652673));
#228251=CARTESIAN_POINT('Ctrl Pts',(-0.708417774315274,15.2,11.4735693451248));
#228252=CARTESIAN_POINT('Ctrl Pts',(-0.710930735000056,15.2,11.478004073));
#228253=CARTESIAN_POINT('Ctrl Pts',(-0.292001930000056,12.2,10.370890024));
#228254=CARTESIAN_POINT('Ctrl Pts',(-0.29220549901488,12.2,10.372665048257));
#228255=CARTESIAN_POINT('Ctrl Pts',(-0.292420934152544,12.2,10.3744962450942));
#228256=CARTESIAN_POINT('Ctrl Pts',(-0.29264874396675,12.2,10.3763825865516));
#228257=CARTESIAN_POINT('Ctrl Pts',(-0.292877652395031,12.2,10.378278024901));
#228258=CARTESIAN_POINT('Ctrl Pts',(-0.293119060472346,12.2,10.3802291369147));
#228259=CARTESIAN_POINT('Ctrl Pts',(-0.293373491749677,12.2,10.3822349054607));
#228260=CARTESIAN_POINT('Ctrl Pts',(-0.293627923003897,12.2,10.3842406738245));
#228261=CARTESIAN_POINT('Ctrl Pts',(-0.29389537585191,12.2,10.3863010957184));
#228262=CARTESIAN_POINT('Ctrl Pts',(-0.294176351258366,12.2,10.3884151802249));
#228263=CARTESIAN_POINT('Ctrl Pts',(-0.294457326664821,12.2,10.3905292647314));
#228264=CARTESIAN_POINT('Ctrl Pts',(-0.294751826391833,12.2,10.3926970122247));
#228265=CARTESIAN_POINT('Ctrl Pts',(-0.295060336478553,12.2,10.3949174557519));
#228266=CARTESIAN_POINT('Ctrl Pts',(-0.295368846593297,12.2,10.3971378994807));
#228267=CARTESIAN_POINT('Ctrl Pts',(-0.295691365100748,12.2,10.3994110391898));
#228268=CARTESIAN_POINT('Ctrl Pts',(-0.296028362286767,12.2,10.4017359359867));
#228269=CARTESIAN_POINT('Ctrl Pts',(-0.29642152562454,12.2,10.4044483152663));
#228270=CARTESIAN_POINT('Ctrl Pts',(-0.296834399281608,12.2,10.407231138541));
#228271=CARTESIAN_POINT('Ctrl Pts',(-0.297267698205805,12.2,10.4100829567802));
#228272=CARTESIAN_POINT('Ctrl Pts',(-0.297639097327062,12.2,10.4125273726993));
#228273=CARTESIAN_POINT('Ctrl Pts',(-0.298025503737548,12.2,10.4150224780102));
#228274=CARTESIAN_POINT('Ctrl Pts',(-0.298427354760501,12.2,10.417567385069));
#228275=CARTESIAN_POINT('Ctrl Pts',(-0.298829205746953,12.2,10.4201122918966));
#228276=CARTESIAN_POINT('Ctrl Pts',(-0.2992465001973,12.2,10.4227069991351));
#228277=CARTESIAN_POINT('Ctrl Pts',(-0.299679662016898,12.2,10.4253506402178));
#228278=CARTESIAN_POINT('Ctrl Pts',(-0.300112823836495,12.2,10.4279942813005));
#228279=CARTESIAN_POINT('Ctrl Pts',(-0.300561853225689,12.2,10.4306868582274));
#228280=CARTESIAN_POINT('Ctrl Pts',(-0.301027158208068,12.2,10.4334275203757));
#228281=CARTESIAN_POINT('Ctrl Pts',(-0.301492463232712,12.2,10.4361681827729));
#228282=CARTESIAN_POINT('Ctrl Pts',(-0.301974044942714,12.2,10.4389569340179));
#228283=CARTESIAN_POINT('Ctrl Pts',(-0.30247229980434,12.2,10.4417929463424));
#228284=CARTESIAN_POINT('Ctrl Pts',(-0.303053597075016,12.2,10.4451016270012));
#228285=CARTESIAN_POINT('Ctrl Pts',(-0.303657588305184,12.2,10.4484746348393));
#228286=CARTESIAN_POINT('Ctrl Pts',(-0.304284883445796,12.2,10.4519106910813));
#228287=CARTESIAN_POINT('Ctrl Pts',(-0.304822565057686,12.2,10.4548558824898));
#228288=CARTESIAN_POINT('Ctrl Pts',(-0.305377366496697,12.2,10.4578473947873));
#228289=CARTESIAN_POINT('Ctrl Pts',(-0.305949657362403,12.2,10.4608844433726));
#228290=CARTESIAN_POINT('Ctrl Pts',(-0.306521948176124,12.2,10.463921491682));
#228291=CARTESIAN_POINT('Ctrl Pts',(-0.307111731829524,12.2,10.4670040761239));
#228292=CARTESIAN_POINT('Ctrl Pts',(-0.307719363558214,12.2,10.4701314274289));
#228293=CARTESIAN_POINT('Ctrl Pts',(-0.308326995286904,12.2,10.4732587787338));
#228294=CARTESIAN_POINT('Ctrl Pts',(-0.308952478339206,12.2,10.4764308968936));
#228295=CARTESIAN_POINT('Ctrl Pts',(-0.30959615798169,12.2,10.4796470312748));
#228296=CARTESIAN_POINT('Ctrl Pts',(-0.310239837682641,12.2,10.4828631659482));
#228297=CARTESIAN_POINT('Ctrl Pts',(-0.310901714877504,12.2,10.4861233166853));
#228298=CARTESIAN_POINT('Ctrl Pts',(-0.311582129332527,12.2,10.4894267466183));
#228299=CARTESIAN_POINT('Ctrl Pts',(-0.312262543725746,12.2,10.4927301762513));
#228300=CARTESIAN_POINT('Ctrl Pts',(-0.312961492072808,12.2,10.4960768859977));
#228301=CARTESIAN_POINT('Ctrl Pts',(-0.313679305464225,12.2,10.4994661554598));
#228302=CARTESIAN_POINT('Ctrl Pts',(-0.314397118855642,12.2,10.5028554249219));
#228303=CARTESIAN_POINT('Ctrl Pts',(-0.315133794903881,12.2,10.5062872556305));
#228304=CARTESIAN_POINT('Ctrl Pts',(-0.315889653208907,12.2,10.5097609375858));
#228305=CARTESIAN_POINT('Ctrl Pts',(-0.316645511513932,12.2,10.513234619541));
#228306=CARTESIAN_POINT('Ctrl Pts',(-0.317420551443608,12.2,10.5167501571609));
#228307=CARTESIAN_POINT('Ctrl Pts',(-0.318215080913418,12.2,10.5203068568622));
#228308=CARTESIAN_POINT('Ctrl Pts',(-0.319009610455398,12.2,10.5238635568866));
#228309=CARTESIAN_POINT('Ctrl Pts',(-0.319823630924239,12.2,10.5274614183316));
#228310=CARTESIAN_POINT('Ctrl Pts',(-0.320657440553881,12.2,10.5310997671984));
#228311=CARTESIAN_POINT('Ctrl Pts',(-0.321491250107784,12.2,10.5347381157346));
#228312=CARTESIAN_POINT('Ctrl Pts',(-0.322344850352457,12.2,10.5384169472249));
#228313=CARTESIAN_POINT('Ctrl Pts',(-0.323218530741291,12.2,10.5421356000232));
#228314=CARTESIAN_POINT('Ctrl Pts',(-0.324092211130125,12.2,10.5458542528215));
#228315=CARTESIAN_POINT('Ctrl Pts',(-0.324985972868309,12.2,10.549612724485));
#228316=CARTESIAN_POINT('Ctrl Pts',(-0.325900097167055,12.2,10.553410366261));
#228317=CARTESIAN_POINT('Ctrl Pts',(-0.326814221548832,12.2,10.557208008382));
#228318=CARTESIAN_POINT('Ctrl Pts',(-0.327748709641513,12.2,10.5610448175429));
#228319=CARTESIAN_POINT('Ctrl Pts',(-0.3287038350758,12.2,10.5649201568666));
#228320=CARTESIAN_POINT('Ctrl Pts',(-0.329499772894327,12.2,10.568149606127));
#228321=CARTESIAN_POINT('Ctrl Pts',(-0.330310042073378,12.2,10.5714058104271));
#228322=CARTESIAN_POINT('Ctrl Pts',(-0.331134798116238,12.2,10.5746884079293));
#228323=CARTESIAN_POINT('Ctrl Pts',(-0.331959554159098,12.2,10.5779710054315));
#228324=CARTESIAN_POINT('Ctrl Pts',(-0.332798795749401,12.2,10.5812799938229));
#228325=CARTESIAN_POINT('Ctrl Pts',(-0.333652674361709,12.2,10.5846150172278));
#228326=CARTESIAN_POINT('Ctrl Pts',(-0.334506552880944,12.2,10.5879500402692));
#228327=CARTESIAN_POINT('Ctrl Pts',(-0.335375070626421,12.2,10.5913110967615));
#228328=CARTESIAN_POINT('Ctrl Pts',(-0.336258370667824,12.2,10.5946978340986));
#228329=CARTESIAN_POINT('Ctrl Pts',(-0.33731833089081,12.2,10.5987619195676));
#228330=CARTESIAN_POINT('Ctrl Pts',(-0.338399582482504,12.2,10.6028629845068));
#228331=CARTESIAN_POINT('Ctrl Pts',(-0.339502371543545,12.2,10.6070004289839));
#228332=CARTESIAN_POINT('Ctrl Pts',(-0.34042136237766,12.2,10.6104482991936));
#228333=CARTESIAN_POINT('Ctrl Pts',(-0.34135530832287,12.2,10.6139214322795));
#228334=CARTESIAN_POINT('Ctrl Pts',(-0.342304353301911,12.2,10.6174194876644));
#228335=CARTESIAN_POINT('Ctrl Pts',(-0.343253398280953,12.2,10.6209175430493));
#228336=CARTESIAN_POINT('Ctrl Pts',(-0.344217538393549,12.2,10.6244405197508));
#228337=CARTESIAN_POINT('Ctrl Pts',(-0.345196912561453,12.2,10.6279880816973));
#228338=CARTESIAN_POINT('Ctrl Pts',(-0.346176286729357,12.2,10.6315356436437));
#228339=CARTESIAN_POINT('Ctrl Pts',(-0.347170893953096,12.2,10.6351077891795));
#228340=CARTESIAN_POINT('Ctrl Pts',(-0.348180867357127,12.2,10.638704188487));
#228341=CARTESIAN_POINT('Ctrl Pts',(-0.349190840651072,12.2,10.6423005874025));
#228342=CARTESIAN_POINT('Ctrl Pts',(-0.350216180523041,12.2,10.6459212354502));
#228343=CARTESIAN_POINT('Ctrl Pts',(-0.351257017838883,12.2,10.6495658110232));
#228344=CARTESIAN_POINT('Ctrl Pts',(-0.352297855268177,12.2,10.6532103869935));
#228345=CARTESIAN_POINT('Ctrl Pts',(-0.353354189705533,12.2,10.6568788857078));
#228346=CARTESIAN_POINT('Ctrl Pts',(-0.354426147343142,12.2,10.660570986192));
#228347=CARTESIAN_POINT('Ctrl Pts',(-0.355712496578379,12.2,10.6650015070145));
#228348=CARTESIAN_POINT('Ctrl Pts',(-0.357021345021807,12.2,10.6694660135717));
#228349=CARTESIAN_POINT('Ctrl Pts',(-0.358352906162216,12.2,10.6739639554601));
#228350=CARTESIAN_POINT('Ctrl Pts',(-0.359462540385416,12.2,10.6777122401629));
#228351=CARTESIAN_POINT('Ctrl Pts',(-0.360587946892449,12.2,10.681483743061));
#228352=CARTESIAN_POINT('Ctrl Pts',(-0.361729247657633,12.2,10.6852781509796));
#228353=CARTESIAN_POINT('Ctrl Pts',(-0.362870548422817,12.2,10.6890725588981));
#228354=CARTESIAN_POINT('Ctrl Pts',(-0.364027741913281,12.2,10.6928898715004));
#228355=CARTESIAN_POINT('Ctrl Pts',(-0.365200947678475,12.2,10.6967297802522));
#228356=CARTESIAN_POINT('Ctrl Pts',(-0.36637415344367,12.2,10.700569689004));
#228357=CARTESIAN_POINT('Ctrl Pts',(-0.36756336964523,12.2,10.7044321930117));
#228358=CARTESIAN_POINT('Ctrl Pts',(-0.368768713674349,12.2,10.7083169859997));
#228359=CARTESIAN_POINT('Ctrl Pts',(-0.369974057572086,12.2,10.7122017785643));
#228360=CARTESIAN_POINT('Ctrl Pts',(-0.371195528302116,12.2,10.7161088606771));
#228361=CARTESIAN_POINT('Ctrl Pts',(-0.372433238096463,12.2,10.7200379299694));
#228362=CARTESIAN_POINT('Ctrl Pts',(-0.37367094802572,12.2,10.7239669996899));
#228363=CARTESIAN_POINT('Ctrl Pts',(-0.374924897418553,12.2,10.7279180584377));
#228364=CARTESIAN_POINT('Ctrl Pts',(-0.376195196375531,12.2,10.7318908049636));
#228365=CARTESIAN_POINT('Ctrl Pts',(-0.377211435596498,12.2,10.7350690023576));
#228366=CARTESIAN_POINT('Ctrl Pts',(-0.37823813745333,12.2,10.7382610825544));
#228367=CARTESIAN_POINT('Ctrl Pts',(-0.379275358792392,12.2,10.7414668912438));
#228368=CARTESIAN_POINT('Ctrl Pts',(-0.380312579990132,12.2,10.7446726994963));
#228369=CARTESIAN_POINT('Ctrl Pts',(-0.381360319825717,12.2,10.7478922394315));
#228370=CARTESIAN_POINT('Ctrl Pts',(-0.382418632293654,12.2,10.7511253597213));
#228371=CARTESIAN_POINT('Ctrl Pts',(-0.383476944905785,12.2,10.7543584804516));
#228372=CARTESIAN_POINT('Ctrl Pts',(-0.384545831121746,12.2,10.7576051824751));
#228373=CARTESIAN_POINT('Ctrl Pts',(-0.385625342458339,12.2,10.7608653170416));
#228374=CARTESIAN_POINT('Ctrl Pts',(-0.386704853794931,12.2,10.7641254516081));
#228375=CARTESIAN_POINT('Ctrl Pts',(-0.387794991685585,12.2,10.7673990188624));
#228376=CARTESIAN_POINT('Ctrl Pts',(-0.388895806413339,12.2,10.7706858728207));
#228377=CARTESIAN_POINT('Ctrl Pts',(-0.389996620991107,12.2,10.7739727263311));
#228378=CARTESIAN_POINT('Ctrl Pts',(-0.391108115344244,12.2,10.7772728660313));
#228379=CARTESIAN_POINT('Ctrl Pts',(-0.392230337757589,12.2,10.7805861469977));
#228380=CARTESIAN_POINT('Ctrl Pts',(-0.393352560323837,12.2,10.7838994284156));
#228381=CARTESIAN_POINT('Ctrl Pts',(-0.394485511079143,12.2,10.7872258510848));
#228382=CARTESIAN_POINT('Ctrl Pts',(-0.395629242920353,12.2,10.7905652710459));
#228383=CARTESIAN_POINT('Ctrl Pts',(-0.396772974605729,12.2,10.793904690552));
#228384=CARTESIAN_POINT('Ctrl Pts',(-0.39792748563137,12.2,10.7972571073398));
#228385=CARTESIAN_POINT('Ctrl Pts',(-0.399092824146519,12.2,10.8006223795083));
#228386=CARTESIAN_POINT('Ctrl Pts',(-0.400258162820446,12.2,10.8039876521353));
#228387=CARTESIAN_POINT('Ctrl Pts',(-0.401434331622365,12.2,10.8073657787339));
#228388=CARTESIAN_POINT('Ctrl Pts',(-0.402621376913991,12.2,10.8107566197004));
#228389=CARTESIAN_POINT('Ctrl Pts',(-0.403808422043882,12.2,10.8141474602048));
#228390=CARTESIAN_POINT('Ctrl Pts',(-0.4050063439064,12.2,10.8175510144232));
#228391=CARTESIAN_POINT('Ctrl Pts',(-0.406215190917957,12.2,10.8209671432541));
#228392=CARTESIAN_POINT('Ctrl Pts',(-0.40742403809422,12.2,10.8243832725505));
#228393=CARTESIAN_POINT('Ctrl Pts',(-0.408643808321823,12.2,10.8278119736319));
#228394=CARTESIAN_POINT('Ctrl Pts',(-0.409874550834068,12.2,10.8312531122647));
#228395=CARTESIAN_POINT('Ctrl Pts',(-0.411105293178624,12.2,10.8346942504287));
#228396=CARTESIAN_POINT('Ctrl Pts',(-0.412347006228511,12.2,10.8381478235389));
#228397=CARTESIAN_POINT('Ctrl Pts',(-0.413599736576627,12.2,10.8416136947054));
#228398=CARTESIAN_POINT('Ctrl Pts',(-0.414852467095428,12.2,10.8450795663442));
#228399=CARTESIAN_POINT('Ctrl Pts',(-0.416116213753581,12.2,10.8485577360111));
#228400=CARTESIAN_POINT('Ctrl Pts',(-0.417391022879335,12.2,10.8520480675354));
#228401=CARTESIAN_POINT('Ctrl Pts',(-0.418665831831396,12.2,10.8555383985842));
#228402=CARTESIAN_POINT('Ctrl Pts',(-0.419951701303461,12.2,10.8590408918916));
#228403=CARTESIAN_POINT('Ctrl Pts',(-0.421248677029627,12.2,10.8625554121587));
#228404=CARTESIAN_POINT('Ctrl Pts',(-0.422545652932505,12.2,10.8660699329045));
#228405=CARTESIAN_POINT('Ctrl Pts',(-0.423853735161873,12.2,10.8695964805712));
#228406=CARTESIAN_POINT('Ctrl Pts',(-0.425172965684246,12.2,10.8731349220024));
#228407=CARTESIAN_POINT('Ctrl Pts',(-0.426492196026873,12.2,10.8766733629514));
#228408=CARTESIAN_POINT('Ctrl Pts',(-0.42782257640538,12.2,10.8802236975433));
#228409=CARTESIAN_POINT('Ctrl Pts',(-0.429164146239003,12.2,10.8837857919175));
#228410=CARTESIAN_POINT('Ctrl Pts',(-0.430505716255415,12.2,10.8873478867771));
#228411=CARTESIAN_POINT('Ctrl Pts',(-0.431858479650664,12.2,10.8909217432767));
#228412=CARTESIAN_POINT('Ctrl Pts',(-0.433222474225011,12.2,10.8945072282499));
#228413=CARTESIAN_POINT('Ctrl Pts',(-0.434586468799358,12.2,10.8980927132232));
#228414=CARTESIAN_POINT('Ctrl Pts',(-0.435961696255549,12.2,10.9016898279004));
#228415=CARTESIAN_POINT('Ctrl Pts',(-0.437348197443381,12.2,10.9052984425983));
#228416=CARTESIAN_POINT('Ctrl Pts',(-0.439081323644806,12.2,10.9098092102331));
#228417=CARTESIAN_POINT('Ctrl Pts',(-0.440832065601813,12.2,10.9143379434412));
#228418=CARTESIAN_POINT('Ctrl Pts',(-0.442600500060369,12.2,10.9188843921803));
#228419=CARTESIAN_POINT('Ctrl Pts',(-0.444015247858525,12.2,10.9225215517662));
#228420=CARTESIAN_POINT('Ctrl Pts',(-0.445441320160564,12.2,10.9261700500227));
#228421=CARTESIAN_POINT('Ctrl Pts',(-0.446878754016672,12.2,10.9298297569999));
#228422=CARTESIAN_POINT('Ctrl Pts',(-0.448316187872781,12.2,10.9334894639771));
#228423=CARTESIAN_POINT('Ctrl Pts',(-0.449764984749679,12.2,10.9371603810779));
#228424=CARTESIAN_POINT('Ctrl Pts',(-0.451225181997092,12.2,10.9408423818353));
#228425=CARTESIAN_POINT('Ctrl Pts',(-0.452685379045552,12.2,10.944524382091));
#228426=CARTESIAN_POINT('Ctrl Pts',(-0.454156977041318,12.2,10.9482174661418));
#228427=CARTESIAN_POINT('Ctrl Pts',(-0.455640014482341,12.2,10.9519215060224));
#228428=CARTESIAN_POINT('Ctrl Pts',(-0.457123052125427,12.2,10.9556255464078));
#228429=CARTESIAN_POINT('Ctrl Pts',(-0.45861752763244,12.2,10.9593405450272));
#228430=CARTESIAN_POINT('Ctrl Pts',(-0.460123478771237,12.2,10.9630663753424));
#228431=CARTESIAN_POINT('Ctrl Pts',(-0.461629429704847,12.2,10.9667922051501));
#228432=CARTESIAN_POINT('Ctrl Pts',(-0.463146854964757,12.2,10.9705288680007));
#228433=CARTESIAN_POINT('Ctrl Pts',(-0.464675793116795,12.2,10.9742762396937));
#228434=CARTESIAN_POINT('Ctrl Pts',(-0.466586965963081,12.2,10.9789604546928));
#228435=CARTESIAN_POINT('Ctrl Pts',(-0.468516124940402,12.2,10.9836614020813));
#228436=CARTESIAN_POINT('Ctrl Pts',(-0.470463340356108,12.2,10.9883788429832));
#228437=CARTESIAN_POINT('Ctrl Pts',(-0.472021112773571,12.2,10.9921527959104));
#228438=CARTESIAN_POINT('Ctrl Pts',(-0.473590441352209,12.2,10.9959373043395));
#228439=CARTESIAN_POINT('Ctrl Pts',(-0.475171359962806,12.2,10.9997322467923));
#228440=CARTESIAN_POINT('Ctrl Pts',(-0.476752278358003,12.2,11.0035271887281));
#228441=CARTESIAN_POINT('Ctrl Pts',(-0.478344787703661,12.2,11.0073325632174));
#228442=CARTESIAN_POINT('Ctrl Pts',(-0.479948920627313,12.2,11.0111482529048));
#228443=CARTESIAN_POINT('Ctrl Pts',(-0.481954086945801,12.2,11.0159178654039));
#228444=CARTESIAN_POINT('Ctrl Pts',(-0.483977417173082,12.2,11.0207035918257));
#228445=CARTESIAN_POINT('Ctrl Pts',(-0.486018975158267,12.2,11.0255052002277));
#228446=CARTESIAN_POINT('Ctrl Pts',(-0.487652221635427,12.2,11.0293464871587));
#228447=CARTESIAN_POINT('Ctrl Pts',(-0.489297132710859,12.2,11.0331979375784));
#228448=CARTESIAN_POINT('Ctrl Pts',(-0.490953743773791,12.2,11.0370594340937));
#228449=CARTESIAN_POINT('Ctrl Pts',(-0.49261035461101,12.2,11.0409209300828));
#228450=CARTESIAN_POINT('Ctrl Pts',(-0.494278662031432,12.2,11.0447924710896));
#228451=CARTESIAN_POINT('Ctrl Pts',(-0.495958700837779,12.2,11.0486739402161));
#228452=CARTESIAN_POINT('Ctrl Pts',(-0.497638739873032,12.2,11.0525554098714));
#228453=CARTESIAN_POINT('Ctrl Pts',(-0.499330509445771,12.2,11.0564468067085));
#228454=CARTESIAN_POINT('Ctrl Pts',(-0.501034039872722,12.2,11.0603480163106));
#228455=CARTESIAN_POINT('Ctrl Pts',(-0.502737570067566,12.2,11.0642492253813));
#228456=CARTESIAN_POINT('Ctrl Pts',(-0.504452861691518,12.2,11.0681602448955));
#228457=CARTESIAN_POINT('Ctrl Pts',(-0.50617994469113,12.2,11.0720809602144));
#228458=CARTESIAN_POINT('Ctrl Pts',(-0.50833879861713,12.2,11.0769818547637));
#228459=CARTESIAN_POINT('Ctrl Pts',(-0.510516078696392,12.2,11.0818978977839));
#228460=CARTESIAN_POINT('Ctrl Pts',(-0.512711840848184,12.2,11.0868288661859));
#228461=CARTESIAN_POINT('Ctrl Pts',(-0.514468450665353,12.2,11.0907736411224));
#228462=CARTESIAN_POINT('Ctrl Pts',(-0.51623688907285,12.2,11.0947279680324));
#228463=CARTESIAN_POINT('Ctrl Pts',(-0.518017187337333,12.2,11.0986917330824));
#228464=CARTESIAN_POINT('Ctrl Pts',(-0.519797485359249,12.2,11.1026554975924));
#228465=CARTESIAN_POINT('Ctrl Pts',(-0.521589640343912,12.2,11.1066286997412));
#228466=CARTESIAN_POINT('Ctrl Pts',(-0.523393683229959,12.2,11.1106112264471));
#228467=CARTESIAN_POINT('Ctrl Pts',(-0.525197726361805,12.2,11.1145937536956));
#228468=CARTESIAN_POINT('Ctrl Pts',(-0.527013656329686,12.2,11.1185856069529));
#228469=CARTESIAN_POINT('Ctrl Pts',(-0.528841501374546,12.2,11.1225866720605));
#228470=CARTESIAN_POINT('Ctrl Pts',(-0.5311263075561,12.2,11.1275880031724));
#228471=CARTESIAN_POINT('Ctrl Pts',(-0.533429730945455,12.2,11.1326037289227));
#228472=CARTESIAN_POINT('Ctrl Pts',(-0.535751824626986,12.2,11.1376336323957));
#228473=CARTESIAN_POINT('Ctrl Pts',(-0.537609499420346,12.2,11.1416575548451));
#228474=CARTESIAN_POINT('Ctrl Pts',(-0.539479124035124,12.2,11.1456905501205));
#228475=CARTESIAN_POINT('Ctrl Pts',(-0.541360724252043,12.2,11.1497325088802));
#228476=CARTESIAN_POINT('Ctrl Pts',(-0.542771924478824,12.2,11.1527639780875));
#228477=CARTESIAN_POINT('Ctrl Pts',(-0.544189861392124,12.2,11.1558004885981));
#228478=CARTESIAN_POINT('Ctrl Pts',(-0.545614545964432,12.2,11.1588419950702));
#228479=CARTESIAN_POINT('Ctrl Pts',(-0.547039230795557,12.2,11.1618835020949));
#228480=CARTESIAN_POINT('Ctrl Pts',(-0.54847066198694,12.2,11.1649300046044));
#228481=CARTESIAN_POINT('Ctrl Pts',(-0.549908852363539,12.2,11.1679814562152));
#228482=CARTESIAN_POINT('Ctrl Pts',(-0.551347042478867,12.2,11.1710329072716));
#228483=CARTESIAN_POINT('Ctrl Pts',(-0.552791990943856,12.2,11.1740893077445));
#228484=CARTESIAN_POINT('Ctrl Pts',(-0.554243708183353,12.2,11.1771506118004));
#228485=CARTESIAN_POINT('Ctrl Pts',(-0.55569542542285,12.2,11.1802119158562));
#228486=CARTESIAN_POINT('Ctrl Pts',(-0.557153913097895,12.2,11.183278123767));
#228487=CARTESIAN_POINT('Ctrl Pts',(-0.558619179759674,12.2,11.1863491892944));
#228488=CARTESIAN_POINT('Ctrl Pts',(-0.560084446421453,12.2,11.1894202548218));
#228489=CARTESIAN_POINT('Ctrl Pts',(-0.561556491845709,12.2,11.1924961777451));
#228490=CARTESIAN_POINT('Ctrl Pts',(-0.56303532796533,12.2,11.1955769142305));
#228491=CARTESIAN_POINT('Ctrl Pts',(-0.564514164084952,12.2,11.1986576507159));
#228492=CARTESIAN_POINT('Ctrl Pts',(-0.565999790142274,12.2,11.2017431996759));
#228493=CARTESIAN_POINT('Ctrl Pts',(-0.567492216337446,12.2,11.2048335157299));
#228494=CARTESIAN_POINT('Ctrl Pts',(-0.568984642532617,12.2,11.2079238317838));
#228495=CARTESIAN_POINT('Ctrl Pts',(-0.570483869960694,12.2,11.2110189150042));
#228496=CARTESIAN_POINT('Ctrl Pts',(-0.571989907113364,12.2,11.2141187215575));
#228497=CARTESIAN_POINT('Ctrl Pts',(-0.573495944539631,12.2,11.217218528674));
#228498=CARTESIAN_POINT('Ctrl Pts',(-0.575008792426188,12.2,11.2203230582253));
#228499=CARTESIAN_POINT('Ctrl Pts',(-0.576528459856301,12.2,11.2234322654278));
#228500=CARTESIAN_POINT('Ctrl Pts',(-0.57804812701034,12.2,11.2265414720654));
#228501=CARTESIAN_POINT('Ctrl Pts',(-0.579574615375054,12.2,11.2296553577437));
#228502=CARTESIAN_POINT('Ctrl Pts',(-0.581107933105065,12.2,11.2327738760784));
#228503=CARTESIAN_POINT('Ctrl Pts',(-0.583152356652229,12.2,11.2369319003357));
#228504=CARTESIAN_POINT('Ctrl Pts',(-0.585208922045364,12.2,11.2410981626117));
#228505=CARTESIAN_POINT('Ctrl Pts',(-0.58727765209767,12.2,11.2452725571588));
#228506=CARTESIAN_POINT('Ctrl Pts',(-0.588829199707366,12.2,11.2484033532113));
#228507=CARTESIAN_POINT('Ctrl Pts',(-0.590387590066615,12.2,11.2515387239635));
#228508=CARTESIAN_POINT('Ctrl Pts',(-0.591952832217119,12.2,11.2546786255571));
#228509=CARTESIAN_POINT('Ctrl Pts',(-0.593518074651977,12.2,11.2578185277211));
#228510=CARTESIAN_POINT('Ctrl Pts',(-0.59509016888047,12.2,11.2609629607615));
#228511=CARTESIAN_POINT('Ctrl Pts',(-0.596669124277563,12.2,11.2641118808864));
#228512=CARTESIAN_POINT('Ctrl Pts',(-0.598248079387812,12.2,11.2672608004393));
#228513=CARTESIAN_POINT('Ctrl Pts',(-0.599833895219053,12.2,11.2704142069174));
#228514=CARTESIAN_POINT('Ctrl Pts',(-0.601426582324892,12.2,11.2735720571276));
#228515=CARTESIAN_POINT('Ctrl Pts',(-0.603019269430731,12.2,11.2767299073379));
#228516=CARTESIAN_POINT('Ctrl Pts',(-0.60461882624966,12.2,11.2798922010599));
#228517=CARTESIAN_POINT('Ctrl Pts',(-0.606225261900224,12.2,11.2830588956119));
#228518=CARTESIAN_POINT('Ctrl Pts',(-0.607831697550787,12.2,11.2862255901638));
#228519=CARTESIAN_POINT('Ctrl Pts',(-0.609445012642199,12.2,11.2893966844153));
#228520=CARTESIAN_POINT('Ctrl Pts',(-0.611065215208341,12.2,11.2925721364666));
#228521=CARTESIAN_POINT('Ctrl Pts',(-0.612685417774483,12.2,11.2957475885179));
#228522=CARTESIAN_POINT('Ctrl Pts',(-0.614312507332006,12.2,11.2989273971024));
#228523=CARTESIAN_POINT('Ctrl Pts',(-0.615946494313681,12.2,11.3021115211113));
#228524=CARTESIAN_POINT('Ctrl Pts',(-0.617580481295356,12.2,11.3052956451202));
#228525=CARTESIAN_POINT('Ctrl Pts',(-0.619221363601612,12.2,11.3084840835705));
#228526=CARTESIAN_POINT('Ctrl Pts',(-0.620869151624128,12.2,11.3116767940789));
#228527=CARTESIAN_POINT('Ctrl Pts',(-0.622516939945991,12.2,11.3148695051673));
#228528=CARTESIAN_POINT('Ctrl Pts',(-0.624171632936478,12.2,11.318066487332));
#228529=CARTESIAN_POINT('Ctrl Pts',(-0.625833238387243,12.2,11.3212676994645));
#228530=CARTESIAN_POINT('Ctrl Pts',(-0.627494843536147,12.2,11.3244689110154));
#228531=CARTESIAN_POINT('Ctrl Pts',(-0.629163362900605,12.2,11.3276743514768));
#228532=CARTESIAN_POINT('Ctrl Pts',(-0.630838802590896,12.2,11.3308839806043));
#228533=CARTESIAN_POINT('Ctrl Pts',(-0.633072722076496,12.2,11.3351634859133));
#228534=CARTESIAN_POINT('Ctrl Pts',(-0.635318945531495,12.2,11.33945043422));
#228535=CARTESIAN_POINT('Ctrl Pts',(-0.637577492290492,12.2,11.343744726924));
#228536=CARTESIAN_POINT('Ctrl Pts',(-0.639271402436672,12.2,11.3469654465983));
#228537=CARTESIAN_POINT('Ctrl Pts',(-0.640972244990713,12.2,11.3501902979473));
#228538=CARTESIAN_POINT('Ctrl Pts',(-0.642680026136048,12.2,11.3534192385794));
#228539=CARTESIAN_POINT('Ctrl Pts',(-0.644387807591629,12.2,11.3566481797981));
#228540=CARTESIAN_POINT('Ctrl Pts',(-0.646102529490848,12.2,11.359881210268));
#228541=CARTESIAN_POINT('Ctrl Pts',(-0.64782419790867,12.2,11.3631182894473));
#228542=CARTESIAN_POINT('Ctrl Pts',(-0.649545866013722,12.2,11.3663553680386));
#228543=CARTESIAN_POINT('Ctrl Pts',(-0.65127448119475,12.2,11.3695964946665));
#228544=CARTESIAN_POINT('Ctrl Pts',(-0.653010051344197,12.2,11.3728416283778));
#228545=CARTESIAN_POINT('Ctrl Pts',(-0.654745621493644,12.2,11.3760867620892));
#228546=CARTESIAN_POINT('Ctrl Pts',(-0.656488146003774,12.2,11.3793359007058));
#228547=CARTESIAN_POINT('Ctrl Pts',(-0.658237633440817,12.2,11.3825890057963));
#228548=CARTESIAN_POINT('Ctrl Pts',(-0.660570283250933,12.2,11.3869264790533));
#228549=CARTESIAN_POINT('Ctrl Pts',(-0.662915307844703,12.2,11.3912710027505));
#228550=CARTESIAN_POINT('Ctrl Pts',(-0.665272728372901,12.2,11.3956224788385));
#228551=CARTESIAN_POINT('Ctrl Pts',(-0.667630149222297,12.2,11.3999739555193));
#228552=CARTESIAN_POINT('Ctrl Pts',(-0.669999963027594,12.2,11.4043323875368));
#228553=CARTESIAN_POINT('Ctrl Pts',(-0.672382187501631,12.2,11.4086976752946));
#228554=CARTESIAN_POINT('Ctrl Pts',(-0.674168855694871,12.2,11.4119716408156));
#228555=CARTESIAN_POINT('Ctrl Pts',(-0.675962505922318,12.2,11.415249461118));
#228556=CARTESIAN_POINT('Ctrl Pts',(-0.677763143948374,12.2,11.4185310967636));
#228557=CARTESIAN_POINT('Ctrl Pts',(-0.67956378197443,12.2,11.4218127324093));
#228558=CARTESIAN_POINT('Ctrl Pts',(-0.68137140763554,12.2,11.4250981825947));
#228559=CARTESIAN_POINT('Ctrl Pts',(-0.683186028110665,12.2,11.4283874103915));
#228560=CARTESIAN_POINT('Ctrl Pts',(-0.685000648585788,12.2,11.4316766381883));
#228561=CARTESIAN_POINT('Ctrl Pts',(-0.686822262518783,12.2,11.4349696456016));
#228562=CARTESIAN_POINT('Ctrl Pts',(-0.688650877576374,12.2,11.4382663917313));
#228563=CARTESIAN_POINT('Ctrl Pts',(-0.690479492966162,12.2,11.4415631384599));
#228564=CARTESIAN_POINT('Ctrl Pts',(-0.692315108432972,12.2,11.4448636254063));
#228565=CARTESIAN_POINT('Ctrl Pts',(-0.694157732868378,12.2,11.4481678025119));
#228566=CARTESIAN_POINT('Ctrl Pts',(-0.696000356969041,12.2,11.4514719790174));
#228567=CARTESIAN_POINT('Ctrl Pts',(-0.697849990633181,12.2,11.4547798455118));
#228568=CARTESIAN_POINT('Ctrl Pts',(-0.699706638825956,12.2,11.4580913594324));
#228569=CARTESIAN_POINT('Ctrl Pts',(-0.701563287018731,12.2,11.4614028733529));
#228570=CARTESIAN_POINT('Ctrl Pts',(-0.703426952058125,12.2,11.4647180326881));
#228571=CARTESIAN_POINT('Ctrl Pts',(-0.705297634486514,12.2,11.4680368213728));
#228572=CARTESIAN_POINT('Ctrl Pts',(-0.707168316914903,12.2,11.4713556100575));
#228573=CARTESIAN_POINT('Ctrl Pts',(-0.709046014657665,12.2,11.4746780273957));
#228574=CARTESIAN_POINT('Ctrl Pts',(-0.710930735000056,12.2,11.478004073));
#228575=CARTESIAN_POINT('Ctrl Pts',(-1.09337743000006,15.2,11.447904865));
#228576=CARTESIAN_POINT('Ctrl Pts',(-1.09337743000006,11.6,11.447904865));
#228577=CARTESIAN_POINT('Ctrl Pts',(-1.09364567100006,15.2,11.447188879));
#228578=CARTESIAN_POINT('Ctrl Pts',(-1.09364567100006,11.6,11.447188879));
#228579=CARTESIAN_POINT('Ctrl Pts',(-1.09418172900006,15.2,11.445757219));
#228580=CARTESIAN_POINT('Ctrl Pts',(-1.09418172900006,11.6,11.445757219));
#228581=CARTESIAN_POINT('Ctrl Pts',(-1.09498454400006,15.2,11.443610665));
#228582=CARTESIAN_POINT('Ctrl Pts',(-1.09498454400006,11.6,11.443610665));
#228583=CARTESIAN_POINT('Ctrl Pts',(-1.09605241700006,15.2,11.440750464));
#228584=CARTESIAN_POINT('Ctrl Pts',(-1.09605241700006,11.6,11.440750464));
#228585=CARTESIAN_POINT('Ctrl Pts',(-1.09738301600006,15.2,11.437178336));
#228586=CARTESIAN_POINT('Ctrl Pts',(-1.09738301600006,11.6,11.437178336));
#228587=CARTESIAN_POINT('Ctrl Pts',(-1.09870937300006,15.2,11.433609329));
#228588=CARTESIAN_POINT('Ctrl Pts',(-1.09870937300006,11.6,11.433609329));
#228589=CARTESIAN_POINT('Ctrl Pts',(-1.10003148900006,15.2,11.430043446));
#228590=CARTESIAN_POINT('Ctrl Pts',(-1.10003148900006,11.6,11.430043446));
#228591=CARTESIAN_POINT('Ctrl Pts',(-1.10134936300006,15.2,11.42648069));
#228592=CARTESIAN_POINT('Ctrl Pts',(-1.10134936300006,11.6,11.42648069));
#228593=CARTESIAN_POINT('Ctrl Pts',(-1.10266299900006,15.2,11.42292107));
#228594=CARTESIAN_POINT('Ctrl Pts',(-1.10266299900006,11.6,11.42292107));
#228595=CARTESIAN_POINT('Ctrl Pts',(-1.10397239800006,15.2,11.419364591));
#228596=CARTESIAN_POINT('Ctrl Pts',(-1.10397239800006,11.6,11.419364591));
#228597=CARTESIAN_POINT('Ctrl Pts',(-1.10527756400006,15.2,11.415811262));
#228598=CARTESIAN_POINT('Ctrl Pts',(-1.10527756400006,11.6,11.415811262));
#228599=CARTESIAN_POINT('Ctrl Pts',(-1.10657850100006,15.2,11.412261095));
#228600=CARTESIAN_POINT('Ctrl Pts',(-1.10657850100006,11.6,11.412261095));
#228601=CARTESIAN_POINT('Ctrl Pts',(-1.10787521000006,15.2,11.408714099));
#228602=CARTESIAN_POINT('Ctrl Pts',(-1.10787521000006,11.6,11.408714099));
#228603=CARTESIAN_POINT('Ctrl Pts',(-1.10916769700006,15.2,11.405170286));
#228604=CARTESIAN_POINT('Ctrl Pts',(-1.10916769700006,11.6,11.405170286));
#228605=CARTESIAN_POINT('Ctrl Pts',(-1.11045596300006,15.2,11.401629665));
#228606=CARTESIAN_POINT('Ctrl Pts',(-1.11045596300006,11.6,11.401629665));
#228607=CARTESIAN_POINT('Ctrl Pts',(-1.11174001400006,15.2,11.398092245));
#228608=CARTESIAN_POINT('Ctrl Pts',(-1.11174001400006,11.6,11.398092245));
#228609=CARTESIAN_POINT('Ctrl Pts',(-1.11301985000006,15.2,11.394558034));
#228610=CARTESIAN_POINT('Ctrl Pts',(-1.11301985000006,11.6,11.394558034));
#228611=CARTESIAN_POINT('Ctrl Pts',(-1.11429547500006,15.2,11.391027041));
#228612=CARTESIAN_POINT('Ctrl Pts',(-1.11429547500006,11.6,11.391027041));
#228613=CARTESIAN_POINT('Ctrl Pts',(-1.11556689100005,15.2,11.387499272));
#228614=CARTESIAN_POINT('Ctrl Pts',(-1.11556689100005,11.6,11.387499272));
#228615=CARTESIAN_POINT('Ctrl Pts',(-1.11683410000005,15.2,11.383974736));
#228616=CARTESIAN_POINT('Ctrl Pts',(-1.11683410000005,11.6,11.383974736));
#228617=CARTESIAN_POINT('Ctrl Pts',(-1.11809710700006,15.2,11.38045344));
#228618=CARTESIAN_POINT('Ctrl Pts',(-1.11809710700006,11.6,11.38045344));
#228619=CARTESIAN_POINT('Ctrl Pts',(-1.11935591200006,15.2,11.376935394));
#228620=CARTESIAN_POINT('Ctrl Pts',(-1.11935591200006,11.6,11.376935394));
#228621=CARTESIAN_POINT('Ctrl Pts',(-1.12061052000006,15.2,11.373420606));
#228622=CARTESIAN_POINT('Ctrl Pts',(-1.12061052000006,11.6,11.373420606));
#228623=CARTESIAN_POINT('Ctrl Pts',(-1.12186093300006,15.2,11.369909085));
#228624=CARTESIAN_POINT('Ctrl Pts',(-1.12186093300006,11.6,11.369909085));
#228625=CARTESIAN_POINT('Ctrl Pts',(-1.12310715500006,15.2,11.36640084));
#228626=CARTESIAN_POINT('Ctrl Pts',(-1.12310715500006,11.6,11.36640084));
#228627=CARTESIAN_POINT('Ctrl Pts',(-1.12434918700006,15.2,11.36289588));
#228628=CARTESIAN_POINT('Ctrl Pts',(-1.12434918700006,11.6,11.36289588));
#228629=CARTESIAN_POINT('Ctrl Pts',(-1.12558703500006,15.2,11.359394214));
#228630=CARTESIAN_POINT('Ctrl Pts',(-1.12558703500006,11.6,11.359394214));
#228631=CARTESIAN_POINT('Ctrl Pts',(-1.12682070000006,15.2,11.355895852));
#228632=CARTESIAN_POINT('Ctrl Pts',(-1.12682070000006,11.6,11.355895852));
#228633=CARTESIAN_POINT('Ctrl Pts',(-1.12805018600006,15.2,11.352400799));
#228634=CARTESIAN_POINT('Ctrl Pts',(-1.12805018600006,11.6,11.352400799));
#228635=CARTESIAN_POINT('Ctrl Pts',(-1.12927549500006,15.2,11.348909068));
#228636=CARTESIAN_POINT('Ctrl Pts',(-1.12927549500006,11.6,11.348909068));
#228637=CARTESIAN_POINT('Ctrl Pts',(-1.13049663000006,15.2,11.345420664));
#228638=CARTESIAN_POINT('Ctrl Pts',(-1.13049663000006,11.6,11.345420664));
#228639=CARTESIAN_POINT('Ctrl Pts',(-1.13171359400006,15.2,11.341935598));
#228640=CARTESIAN_POINT('Ctrl Pts',(-1.13171359400006,11.6,11.341935598));
#228641=CARTESIAN_POINT('Ctrl Pts',(-1.13292639100006,15.2,11.338453878));
#228642=CARTESIAN_POINT('Ctrl Pts',(-1.13292639100006,11.6,11.338453878));
#228643=CARTESIAN_POINT('Ctrl Pts',(-1.13413502300006,15.2,11.334975512));
#228644=CARTESIAN_POINT('Ctrl Pts',(-1.13413502300006,11.6,11.334975512));
#228645=CARTESIAN_POINT('Ctrl Pts',(-1.13533949400005,15.2,11.33150051));
#228646=CARTESIAN_POINT('Ctrl Pts',(-1.13533949400005,11.6,11.33150051));
#228647=CARTESIAN_POINT('Ctrl Pts',(-1.13653980600006,15.2,11.328028879));
#228648=CARTESIAN_POINT('Ctrl Pts',(-1.13653980600006,11.6,11.328028879));
#228649=CARTESIAN_POINT('Ctrl Pts',(-1.13773596300006,15.2,11.324560631));
#228650=CARTESIAN_POINT('Ctrl Pts',(-1.13773596300006,11.6,11.324560631));
#228651=CARTESIAN_POINT('Ctrl Pts',(-1.13892796700006,15.2,11.321095772));
#228652=CARTESIAN_POINT('Ctrl Pts',(-1.13892796700006,11.6,11.321095772));
#228653=CARTESIAN_POINT('Ctrl Pts',(-1.14011582300006,15.2,11.317634313));
#228654=CARTESIAN_POINT('Ctrl Pts',(-1.14011582300006,11.6,11.317634313));
#228655=CARTESIAN_POINT('Ctrl Pts',(-1.14129953300006,15.2,11.31417626));
#228656=CARTESIAN_POINT('Ctrl Pts',(-1.14129953300006,11.6,11.31417626));
#228657=CARTESIAN_POINT('Ctrl Pts',(-1.14247909900006,15.2,11.310721624));
#228658=CARTESIAN_POINT('Ctrl Pts',(-1.14247909900006,11.6,11.310721624));
#228659=CARTESIAN_POINT('Ctrl Pts',(-1.14365452600006,15.2,11.307270414));
#228660=CARTESIAN_POINT('Ctrl Pts',(-1.14365452600006,11.6,11.307270414));
#228661=CARTESIAN_POINT('Ctrl Pts',(-1.14482581600006,15.2,11.303822638));
#228662=CARTESIAN_POINT('Ctrl Pts',(-1.14482581600006,11.6,11.303822638));
#228663=CARTESIAN_POINT('Ctrl Pts',(-1.14599297300006,15.2,11.300378306));
#228664=CARTESIAN_POINT('Ctrl Pts',(-1.14599297300006,11.6,11.300378306));
#228665=CARTESIAN_POINT('Ctrl Pts',(-1.14715599900006,15.2,11.296937425));
#228666=CARTESIAN_POINT('Ctrl Pts',(-1.14715599900006,11.6,11.296937425));
#228667=CARTESIAN_POINT('Ctrl Pts',(-1.14831489900006,15.2,11.293500007));
#228668=CARTESIAN_POINT('Ctrl Pts',(-1.14831489900006,11.6,11.293500007));
#228669=CARTESIAN_POINT('Ctrl Pts',(-1.14946967500006,15.2,11.290066056));
#228670=CARTESIAN_POINT('Ctrl Pts',(-1.14946967500006,11.6,11.290066056));
#228671=CARTESIAN_POINT('Ctrl Pts',(-1.15062033100006,15.2,11.286635586));
#228672=CARTESIAN_POINT('Ctrl Pts',(-1.15062033100006,11.6,11.286635586));
#228673=CARTESIAN_POINT('Ctrl Pts',(-1.15176686800006,15.2,11.283208603));
#228674=CARTESIAN_POINT('Ctrl Pts',(-1.15176686800006,11.6,11.283208603));
#228675=CARTESIAN_POINT('Ctrl Pts',(-1.15290929200005,15.2,11.279785118));
#228676=CARTESIAN_POINT('Ctrl Pts',(-1.15290929200005,11.6,11.279785118));
#228677=CARTESIAN_POINT('Ctrl Pts',(-1.15404760400006,15.2,11.276365138));
#228678=CARTESIAN_POINT('Ctrl Pts',(-1.15404760400006,11.6,11.276365138));
#228679=CARTESIAN_POINT('Ctrl Pts',(-1.15518181000006,15.2,11.272948674));
#228680=CARTESIAN_POINT('Ctrl Pts',(-1.15518181000006,11.6,11.272948674));
#228681=CARTESIAN_POINT('Ctrl Pts',(-1.15631191200006,15.2,11.269535733));
#228682=CARTESIAN_POINT('Ctrl Pts',(-1.15631191200006,11.6,11.269535733));
#228683=CARTESIAN_POINT('Ctrl Pts',(-1.15743791100006,15.2,11.266126325));
#228684=CARTESIAN_POINT('Ctrl Pts',(-1.15743791100006,11.6,11.266126325));
#228685=CARTESIAN_POINT('Ctrl Pts',(-1.15855981400006,15.2,11.262720459));
#228686=CARTESIAN_POINT('Ctrl Pts',(-1.15855981400006,11.6,11.262720459));
#228687=CARTESIAN_POINT('Ctrl Pts',(-1.15967762200005,15.2,11.259318144));
#228688=CARTESIAN_POINT('Ctrl Pts',(-1.15967762200005,11.6,11.259318144));
#228689=CARTESIAN_POINT('Ctrl Pts',(-1.16079133800006,15.2,11.25591939));
#228690=CARTESIAN_POINT('Ctrl Pts',(-1.16079133800006,11.6,11.25591939));
#228691=CARTESIAN_POINT('Ctrl Pts',(-1.16190096800006,15.2,11.252524204));
#228692=CARTESIAN_POINT('Ctrl Pts',(-1.16190096800006,11.6,11.252524204));
#228693=CARTESIAN_POINT('Ctrl Pts',(-1.16300651300006,15.2,11.249132598));
#228694=CARTESIAN_POINT('Ctrl Pts',(-1.16300651300006,11.6,11.249132598));
#228695=CARTESIAN_POINT('Ctrl Pts',(-1.16410797800006,15.2,11.245744578));
#228696=CARTESIAN_POINT('Ctrl Pts',(-1.16410797800006,11.6,11.245744578));
#228697=CARTESIAN_POINT('Ctrl Pts',(-1.16520536400005,15.2,11.242360155));
#228698=CARTESIAN_POINT('Ctrl Pts',(-1.16520536400005,11.6,11.242360155));
#228699=CARTESIAN_POINT('Ctrl Pts',(-1.16629867800006,15.2,11.238979337));
#228700=CARTESIAN_POINT('Ctrl Pts',(-1.16629867800006,11.6,11.238979337));
#228701=CARTESIAN_POINT('Ctrl Pts',(-1.16738792000006,15.2,11.235602136));
#228702=CARTESIAN_POINT('Ctrl Pts',(-1.16738792000006,11.6,11.235602136));
#228703=CARTESIAN_POINT('Ctrl Pts',(-1.16847309500006,15.2,11.232228557));
#228704=CARTESIAN_POINT('Ctrl Pts',(-1.16847309500006,11.6,11.232228557));
#228705=CARTESIAN_POINT('Ctrl Pts',(-1.16955420600006,15.2,11.228858613));
#228706=CARTESIAN_POINT('Ctrl Pts',(-1.16955420600006,11.6,11.228858613));
#228707=CARTESIAN_POINT('Ctrl Pts',(-1.17063125700006,15.2,11.22549231));
#228708=CARTESIAN_POINT('Ctrl Pts',(-1.17063125700006,11.6,11.22549231));
#228709=CARTESIAN_POINT('Ctrl Pts',(-1.17170425100006,15.2,11.222129659));
#228710=CARTESIAN_POINT('Ctrl Pts',(-1.17170425100006,11.6,11.222129659));
#228711=CARTESIAN_POINT('Ctrl Pts',(-1.17277319200006,15.2,11.218770669));
#228712=CARTESIAN_POINT('Ctrl Pts',(-1.17277319200006,11.6,11.218770669));
#228713=CARTESIAN_POINT('Ctrl Pts',(-1.17383808200006,15.2,11.215415349));
#228714=CARTESIAN_POINT('Ctrl Pts',(-1.17383808200006,11.6,11.215415349));
#228715=CARTESIAN_POINT('Ctrl Pts',(-1.17489892800006,15.2,11.212063709));
#228716=CARTESIAN_POINT('Ctrl Pts',(-1.17489892800006,11.6,11.212063709));
#228717=CARTESIAN_POINT('Ctrl Pts',(-1.17595573000006,15.2,11.208715757));
#228718=CARTESIAN_POINT('Ctrl Pts',(-1.17595573000006,11.6,11.208715757));
#228719=CARTESIAN_POINT('Ctrl Pts',(-1.17700849300006,15.2,11.205371502));
#228720=CARTESIAN_POINT('Ctrl Pts',(-1.17700849300006,11.6,11.205371502));
#228721=CARTESIAN_POINT('Ctrl Pts',(-1.17805722000006,15.2,11.202030956));
#228722=CARTESIAN_POINT('Ctrl Pts',(-1.17805722000006,11.6,11.202030956));
#228723=CARTESIAN_POINT('Ctrl Pts',(-1.17910191400005,15.2,11.198694126));
#228724=CARTESIAN_POINT('Ctrl Pts',(-1.17910191400005,11.6,11.198694126));
#228725=CARTESIAN_POINT('Ctrl Pts',(-1.18014258100006,15.2,11.195361021));
#228726=CARTESIAN_POINT('Ctrl Pts',(-1.18014258100006,11.6,11.195361021));
#228727=CARTESIAN_POINT('Ctrl Pts',(-1.18117922300006,15.2,11.192031652));
#228728=CARTESIAN_POINT('Ctrl Pts',(-1.18117922300006,11.6,11.192031652));
#228729=CARTESIAN_POINT('Ctrl Pts',(-1.18221184300006,15.2,11.188706028));
#228730=CARTESIAN_POINT('Ctrl Pts',(-1.18221184300006,11.6,11.188706028));
#228731=CARTESIAN_POINT('Ctrl Pts',(-1.18324044700006,15.2,11.185384157));
#228732=CARTESIAN_POINT('Ctrl Pts',(-1.18324044700006,11.6,11.185384157));
#228733=CARTESIAN_POINT('Ctrl Pts',(-1.18426503600006,15.2,11.18206605));
#228734=CARTESIAN_POINT('Ctrl Pts',(-1.18426503600006,11.6,11.18206605));
#228735=CARTESIAN_POINT('Ctrl Pts',(-1.18528561400006,15.2,11.178751716));
#228736=CARTESIAN_POINT('Ctrl Pts',(-1.18528561400006,11.6,11.178751716));
#228737=CARTESIAN_POINT('Ctrl Pts',(-1.18630218600006,15.2,11.175441163));
#228738=CARTESIAN_POINT('Ctrl Pts',(-1.18630218600006,11.6,11.175441163));
#228739=CARTESIAN_POINT('Ctrl Pts',(-1.18731475500006,15.2,11.172134402));
#228740=CARTESIAN_POINT('Ctrl Pts',(-1.18731475500006,11.6,11.172134402));
#228741=CARTESIAN_POINT('Ctrl Pts',(-1.18832332500006,15.2,11.168831442));
#228742=CARTESIAN_POINT('Ctrl Pts',(-1.18832332500006,11.6,11.168831442));
#228743=CARTESIAN_POINT('Ctrl Pts',(-1.18932789900006,15.2,11.165532292));
#228744=CARTESIAN_POINT('Ctrl Pts',(-1.18932789900006,11.6,11.165532292));
#228745=CARTESIAN_POINT('Ctrl Pts',(-1.19032848200006,15.2,11.162236963));
#228746=CARTESIAN_POINT('Ctrl Pts',(-1.19032848200006,11.6,11.162236963));
#228747=CARTESIAN_POINT('Ctrl Pts',(-1.19132507600006,15.2,11.158945463));
#228748=CARTESIAN_POINT('Ctrl Pts',(-1.19132507600006,11.6,11.158945463));
#228749=CARTESIAN_POINT('Ctrl Pts',(-1.19231768600006,15.2,11.155657801));
#228750=CARTESIAN_POINT('Ctrl Pts',(-1.19231768600006,11.6,11.155657801));
#228751=CARTESIAN_POINT('Ctrl Pts',(-1.19330631700006,15.2,11.152373988));
#228752=CARTESIAN_POINT('Ctrl Pts',(-1.19330631700006,11.6,11.152373988));
#228753=CARTESIAN_POINT('Ctrl Pts',(-1.19429096900006,15.2,11.149094033));
#228754=CARTESIAN_POINT('Ctrl Pts',(-1.19429096900006,11.6,11.149094033));
#228755=CARTESIAN_POINT('Ctrl Pts',(-1.19527164900005,15.2,11.145817946));
#228756=CARTESIAN_POINT('Ctrl Pts',(-1.19527164900005,11.6,11.145817946));
#228757=CARTESIAN_POINT('Ctrl Pts',(-1.19624836000006,15.2,11.142545735));
#228758=CARTESIAN_POINT('Ctrl Pts',(-1.19624836000006,11.6,11.142545735));
#228759=CARTESIAN_POINT('Ctrl Pts',(-1.19722110600006,15.2,11.139277411));
#228760=CARTESIAN_POINT('Ctrl Pts',(-1.19722110600006,11.6,11.139277411));
#228761=CARTESIAN_POINT('Ctrl Pts',(-1.19818989100006,15.2,11.136012984));
#228762=CARTESIAN_POINT('Ctrl Pts',(-1.19818989100006,11.6,11.136012984));
#228763=CARTESIAN_POINT('Ctrl Pts',(-1.19915471800006,15.2,11.132752462));
#228764=CARTESIAN_POINT('Ctrl Pts',(-1.19915471800006,11.6,11.132752462));
#228765=CARTESIAN_POINT('Ctrl Pts',(-1.20011559100006,15.2,11.129495856));
#228766=CARTESIAN_POINT('Ctrl Pts',(-1.20011559100006,11.6,11.129495856));
#228767=CARTESIAN_POINT('Ctrl Pts',(-1.20107251500006,15.2,11.126243174));
#228768=CARTESIAN_POINT('Ctrl Pts',(-1.20107251500006,11.6,11.126243174));
#228769=CARTESIAN_POINT('Ctrl Pts',(-1.20202549300006,15.2,11.122994428));
#228770=CARTESIAN_POINT('Ctrl Pts',(-1.20202549300006,11.6,11.122994428));
#228771=CARTESIAN_POINT('Ctrl Pts',(-1.20297452900005,15.2,11.119749626));
#228772=CARTESIAN_POINT('Ctrl Pts',(-1.20297452900005,11.6,11.119749626));
#228773=CARTESIAN_POINT('Ctrl Pts',(-1.20391962700006,15.2,11.116508777));
#228774=CARTESIAN_POINT('Ctrl Pts',(-1.20391962700006,11.6,11.116508777));
#228775=CARTESIAN_POINT('Ctrl Pts',(-1.20486079100006,15.2,11.113271893));
#228776=CARTESIAN_POINT('Ctrl Pts',(-1.20486079100006,11.6,11.113271893));
#228777=CARTESIAN_POINT('Ctrl Pts',(-1.20579802500006,15.2,11.110038983));
#228778=CARTESIAN_POINT('Ctrl Pts',(-1.20579802500006,11.6,11.110038983));
#228779=CARTESIAN_POINT('Ctrl Pts',(-1.20673133300006,15.2,11.106810056));
#228780=CARTESIAN_POINT('Ctrl Pts',(-1.20673133300006,11.6,11.106810056));
#228781=CARTESIAN_POINT('Ctrl Pts',(-1.20766072000006,15.2,11.103585122));
#228782=CARTESIAN_POINT('Ctrl Pts',(-1.20766072000006,11.6,11.103585122));
#228783=CARTESIAN_POINT('Ctrl Pts',(-1.20858618900006,15.2,11.10036419));
#228784=CARTESIAN_POINT('Ctrl Pts',(-1.20858618900006,11.6,11.10036419));
#228785=CARTESIAN_POINT('Ctrl Pts',(-1.20950774300006,15.2,11.097147269));
#228786=CARTESIAN_POINT('Ctrl Pts',(-1.20950774300006,11.6,11.097147269));
#228787=CARTESIAN_POINT('Ctrl Pts',(-1.21042538700006,15.2,11.093934373));
#228788=CARTESIAN_POINT('Ctrl Pts',(-1.21042538700006,11.6,11.093934373));
#228789=CARTESIAN_POINT('Ctrl Pts',(-1.21133912600005,15.2,11.090725508));
#228790=CARTESIAN_POINT('Ctrl Pts',(-1.21133912600005,11.6,11.090725508));
#228791=CARTESIAN_POINT('Ctrl Pts',(-1.21224896300006,15.2,11.087520686));
#228792=CARTESIAN_POINT('Ctrl Pts',(-1.21224896300006,11.6,11.087520686));
#228793=CARTESIAN_POINT('Ctrl Pts',(-1.21315490300006,15.2,11.084319914));
#228794=CARTESIAN_POINT('Ctrl Pts',(-1.21315490300006,11.6,11.084319914));
#228795=CARTESIAN_POINT('Ctrl Pts',(-1.21405694800006,15.2,11.081123205));
#228796=CARTESIAN_POINT('Ctrl Pts',(-1.21405694800006,11.6,11.081123205));
#228797=CARTESIAN_POINT('Ctrl Pts',(-1.21495510500006,15.2,11.077930567));
#228798=CARTESIAN_POINT('Ctrl Pts',(-1.21495510500006,11.6,11.077930567));
#228799=CARTESIAN_POINT('Ctrl Pts',(-1.21584937600006,15.2,11.074742011));
#228800=CARTESIAN_POINT('Ctrl Pts',(-1.21584937600006,11.6,11.074742011));
#228801=CARTESIAN_POINT('Ctrl Pts',(-1.21673976600006,15.2,11.071557546));
#228802=CARTESIAN_POINT('Ctrl Pts',(-1.21673976600006,11.6,11.071557546));
#228803=CARTESIAN_POINT('Ctrl Pts',(-1.21762628000006,15.2,11.068377182));
#228804=CARTESIAN_POINT('Ctrl Pts',(-1.21762628000006,11.6,11.068377182));
#228805=CARTESIAN_POINT('Ctrl Pts',(-1.21850892000006,15.2,11.065200929));
#228806=CARTESIAN_POINT('Ctrl Pts',(-1.21850892000006,11.6,11.065200929));
#228807=CARTESIAN_POINT('Ctrl Pts',(-1.21938769300006,15.2,11.062028798));
#228808=CARTESIAN_POINT('Ctrl Pts',(-1.21938769300006,11.6,11.062028798));
#228809=CARTESIAN_POINT('Ctrl Pts',(-1.22026260100006,15.2,11.058860798));
#228810=CARTESIAN_POINT('Ctrl Pts',(-1.22026260100006,11.6,11.058860798));
#228811=CARTESIAN_POINT('Ctrl Pts',(-1.22113364900006,15.2,11.055696939));
#228812=CARTESIAN_POINT('Ctrl Pts',(-1.22113364900006,11.6,11.055696939));
#228813=CARTESIAN_POINT('Ctrl Pts',(-1.22200084200006,15.2,11.05253723));
#228814=CARTESIAN_POINT('Ctrl Pts',(-1.22200084200006,11.6,11.05253723));
#228815=CARTESIAN_POINT('Ctrl Pts',(-1.22286418200006,15.2,11.049381684));
#228816=CARTESIAN_POINT('Ctrl Pts',(-1.22286418200006,11.6,11.049381684));
#228817=CARTESIAN_POINT('Ctrl Pts',(-1.22372367600006,15.2,11.046230308));
#228818=CARTESIAN_POINT('Ctrl Pts',(-1.22372367600006,11.6,11.046230308));
#228819=CARTESIAN_POINT('Ctrl Pts',(-1.22457932700006,15.2,11.043083114));
#228820=CARTESIAN_POINT('Ctrl Pts',(-1.22457932700006,11.6,11.043083114));
#228821=CARTESIAN_POINT('Ctrl Pts',(-1.22543114100006,15.2,11.039940111));
#228822=CARTESIAN_POINT('Ctrl Pts',(-1.22543114100006,11.6,11.039940111));
#228823=CARTESIAN_POINT('Ctrl Pts',(-1.22627911900006,15.2,11.036801309));
#228824=CARTESIAN_POINT('Ctrl Pts',(-1.22627911900006,11.6,11.036801309));
#228825=CARTESIAN_POINT('Ctrl Pts',(-1.22712326800006,15.2,11.033666719));
#228826=CARTESIAN_POINT('Ctrl Pts',(-1.22712326800006,11.6,11.033666719));
#228827=CARTESIAN_POINT('Ctrl Pts',(-1.22796359200006,15.2,11.03053635));
#228828=CARTESIAN_POINT('Ctrl Pts',(-1.22796359200006,11.6,11.03053635));
#228829=CARTESIAN_POINT('Ctrl Pts',(-1.22880009300006,15.2,11.027410214));
#228830=CARTESIAN_POINT('Ctrl Pts',(-1.22880009300006,11.6,11.027410214));
#228831=CARTESIAN_POINT('Ctrl Pts',(-1.22963277900006,15.2,11.024288319));
#228832=CARTESIAN_POINT('Ctrl Pts',(-1.22963277900006,11.6,11.024288319));
#228833=CARTESIAN_POINT('Ctrl Pts',(-1.23046165300006,15.2,11.021170677));
#228834=CARTESIAN_POINT('Ctrl Pts',(-1.23046165300006,11.6,11.021170677));
#228835=CARTESIAN_POINT('Ctrl Pts',(-1.23128671900006,15.2,11.018057297));
#228836=CARTESIAN_POINT('Ctrl Pts',(-1.23128671900006,11.6,11.018057297));
#228837=CARTESIAN_POINT('Ctrl Pts',(-1.23210798200006,15.2,11.014948189));
#228838=CARTESIAN_POINT('Ctrl Pts',(-1.23210798200006,11.6,11.014948189));
#228839=CARTESIAN_POINT('Ctrl Pts',(-1.23292544600006,15.2,11.011843364));
#228840=CARTESIAN_POINT('Ctrl Pts',(-1.23292544600006,11.6,11.011843364));
#228841=CARTESIAN_POINT('Ctrl Pts',(-1.23373911600006,15.2,11.008742833));
#228842=CARTESIAN_POINT('Ctrl Pts',(-1.23373911600006,11.6,11.008742833));
#228843=CARTESIAN_POINT('Ctrl Pts',(-1.23454899600006,15.2,11.005646604));
#228844=CARTESIAN_POINT('Ctrl Pts',(-1.23454899600006,11.6,11.005646604));
#228845=CARTESIAN_POINT('Ctrl Pts',(-1.23535509200006,15.2,11.00255469));
#228846=CARTESIAN_POINT('Ctrl Pts',(-1.23535509200006,11.6,11.00255469));
#228847=CARTESIAN_POINT('Ctrl Pts',(-1.23615740600005,15.2,10.999467099));
#228848=CARTESIAN_POINT('Ctrl Pts',(-1.23615740600005,11.6,10.999467099));
#228849=CARTESIAN_POINT('Ctrl Pts',(-1.23695594400006,15.2,10.996383843));
#228850=CARTESIAN_POINT('Ctrl Pts',(-1.23695594400006,11.6,10.996383843));
#228851=CARTESIAN_POINT('Ctrl Pts',(-1.23775071100006,15.2,10.99330493));
#228852=CARTESIAN_POINT('Ctrl Pts',(-1.23775071100006,11.6,10.99330493));
#228853=CARTESIAN_POINT('Ctrl Pts',(-1.23854171100006,15.2,10.990230373));
#228854=CARTESIAN_POINT('Ctrl Pts',(-1.23854171100006,11.6,10.990230373));
#228855=CARTESIAN_POINT('Ctrl Pts',(-1.23932894900006,15.2,10.987160181));
#228856=CARTESIAN_POINT('Ctrl Pts',(-1.23932894900006,11.6,10.987160181));
#228857=CARTESIAN_POINT('Ctrl Pts',(-1.24011243000006,15.2,10.984094365));
#228858=CARTESIAN_POINT('Ctrl Pts',(-1.24011243000006,11.6,10.984094365));
#228859=CARTESIAN_POINT('Ctrl Pts',(-1.24089215700006,15.2,10.981032934));
#228860=CARTESIAN_POINT('Ctrl Pts',(-1.24089215700006,11.6,10.981032934));
#228861=CARTESIAN_POINT('Ctrl Pts',(-1.24166813600006,15.2,10.977975901));
#228862=CARTESIAN_POINT('Ctrl Pts',(-1.24166813600006,11.6,10.977975901));
#228863=CARTESIAN_POINT('Ctrl Pts',(-1.24244037200006,15.2,10.974923274));
#228864=CARTESIAN_POINT('Ctrl Pts',(-1.24244037200006,11.6,10.974923274));
#228865=CARTESIAN_POINT('Ctrl Pts',(-1.24320886800006,15.2,10.971875065));
#228866=CARTESIAN_POINT('Ctrl Pts',(-1.24320886800006,11.6,10.971875065));
#228867=CARTESIAN_POINT('Ctrl Pts',(-1.24397363200006,15.2,10.968831284));
#228868=CARTESIAN_POINT('Ctrl Pts',(-1.24397363200006,11.6,10.968831284));
#228869=CARTESIAN_POINT('Ctrl Pts',(-1.24473466500006,15.2,10.965791942));
#228870=CARTESIAN_POINT('Ctrl Pts',(-1.24473466500006,11.6,10.965791942));
#228871=CARTESIAN_POINT('Ctrl Pts',(-1.24549197400005,15.2,10.962757048));
#228872=CARTESIAN_POINT('Ctrl Pts',(-1.24549197400005,11.6,10.962757048));
#228873=CARTESIAN_POINT('Ctrl Pts',(-1.24624556200006,15.2,10.959726614));
#228874=CARTESIAN_POINT('Ctrl Pts',(-1.24624556200006,11.6,10.959726614));
#228875=CARTESIAN_POINT('Ctrl Pts',(-1.24699543600006,15.2,10.95670065));
#228876=CARTESIAN_POINT('Ctrl Pts',(-1.24699543600006,11.6,10.95670065));
#228877=CARTESIAN_POINT('Ctrl Pts',(-1.24774160000006,15.2,10.953679167));
#228878=CARTESIAN_POINT('Ctrl Pts',(-1.24774160000006,11.6,10.953679167));
#228879=CARTESIAN_POINT('Ctrl Pts',(-1.24848405900006,15.2,10.950662174));
#228880=CARTESIAN_POINT('Ctrl Pts',(-1.24848405900006,11.6,10.950662174));
#228881=CARTESIAN_POINT('Ctrl Pts',(-1.24922281700006,15.2,10.947649683));
#228882=CARTESIAN_POINT('Ctrl Pts',(-1.24922281700006,11.6,10.947649683));
#228883=CARTESIAN_POINT('Ctrl Pts',(-1.24995788000006,15.2,10.944641706));
#228884=CARTESIAN_POINT('Ctrl Pts',(-1.24995788000006,11.6,10.944641706));
#228885=CARTESIAN_POINT('Ctrl Pts',(-1.25068925200006,15.2,10.941638251));
#228886=CARTESIAN_POINT('Ctrl Pts',(-1.25068925200006,11.6,10.941638251));
#228887=CARTESIAN_POINT('Ctrl Pts',(-1.25141693800006,15.2,10.93863933));
#228888=CARTESIAN_POINT('Ctrl Pts',(-1.25141693800006,11.6,10.93863933));
#228889=CARTESIAN_POINT('Ctrl Pts',(-1.25214094400006,15.2,10.935644954));
#228890=CARTESIAN_POINT('Ctrl Pts',(-1.25214094400006,11.6,10.935644954));
#228891=CARTESIAN_POINT('Ctrl Pts',(-1.25286127400006,15.2,10.932655133));
#228892=CARTESIAN_POINT('Ctrl Pts',(-1.25286127400006,11.6,10.932655133));
#228893=CARTESIAN_POINT('Ctrl Pts',(-1.25357793200006,15.2,10.929669878));
#228894=CARTESIAN_POINT('Ctrl Pts',(-1.25357793200006,11.6,10.929669878));
#228895=CARTESIAN_POINT('Ctrl Pts',(-1.25429092600006,15.2,10.926689199));
#228896=CARTESIAN_POINT('Ctrl Pts',(-1.25429092600006,11.6,10.926689199));
#228897=CARTESIAN_POINT('Ctrl Pts',(-1.25500025800006,15.2,10.923713109));
#228898=CARTESIAN_POINT('Ctrl Pts',(-1.25500025800006,11.6,10.923713109));
#228899=CARTESIAN_POINT('Ctrl Pts',(-1.25570593400006,15.2,10.920741617));
#228900=CARTESIAN_POINT('Ctrl Pts',(-1.25570593400006,11.6,10.920741617));
#228901=CARTESIAN_POINT('Ctrl Pts',(-1.25640795900006,15.2,10.917774733));
#228902=CARTESIAN_POINT('Ctrl Pts',(-1.25640795900006,11.6,10.917774733));
#228903=CARTESIAN_POINT('Ctrl Pts',(-1.25710633900006,15.2,10.914812471));
#228904=CARTESIAN_POINT('Ctrl Pts',(-1.25710633900006,11.6,10.914812471));
#228905=CARTESIAN_POINT('Ctrl Pts',(-1.25780107900006,15.2,10.911854838));
#228906=CARTESIAN_POINT('Ctrl Pts',(-1.25780107900006,11.6,10.911854838));
#228907=CARTESIAN_POINT('Ctrl Pts',(-1.25849218300006,15.2,10.908901847));
#228908=CARTESIAN_POINT('Ctrl Pts',(-1.25849218300006,11.6,10.908901847));
#228909=CARTESIAN_POINT('Ctrl Pts',(-1.25917965600006,15.2,10.905953509));
#228910=CARTESIAN_POINT('Ctrl Pts',(-1.25917965600006,11.6,10.905953509));
#228911=CARTESIAN_POINT('Ctrl Pts',(-1.25986350500006,15.2,10.903009835));
#228912=CARTESIAN_POINT('Ctrl Pts',(-1.25986350500006,11.6,10.903009835));
#228913=CARTESIAN_POINT('Ctrl Pts',(-1.26054373300006,15.2,10.900070834));
#228914=CARTESIAN_POINT('Ctrl Pts',(-1.26054373300006,11.6,10.900070834));
#228915=CARTESIAN_POINT('Ctrl Pts',(-1.26122034700006,15.2,10.897136519));
#228916=CARTESIAN_POINT('Ctrl Pts',(-1.26122034700006,11.6,10.897136519));
#228917=CARTESIAN_POINT('Ctrl Pts',(-1.26189335100006,15.2,10.894206902));
#228918=CARTESIAN_POINT('Ctrl Pts',(-1.26189335100006,11.6,10.894206902));
#228919=CARTESIAN_POINT('Ctrl Pts',(-1.26256275000006,15.2,10.891281991));
#228920=CARTESIAN_POINT('Ctrl Pts',(-1.26256275000006,11.6,10.891281991));
#228921=CARTESIAN_POINT('Ctrl Pts',(-1.26322855100006,15.2,10.888361797));
#228922=CARTESIAN_POINT('Ctrl Pts',(-1.26322855100006,11.6,10.888361797));
#228923=CARTESIAN_POINT('Ctrl Pts',(-1.26389075800006,15.2,10.885446334));
#228924=CARTESIAN_POINT('Ctrl Pts',(-1.26389075800006,11.6,10.885446334));
#228925=CARTESIAN_POINT('Ctrl Pts',(-1.26454937500006,15.2,10.882535612));
#228926=CARTESIAN_POINT('Ctrl Pts',(-1.26454937500006,11.6,10.882535612));
#228927=CARTESIAN_POINT('Ctrl Pts',(-1.26520441000006,15.2,10.879629641));
#228928=CARTESIAN_POINT('Ctrl Pts',(-1.26520441000006,11.6,10.879629641));
#228929=CARTESIAN_POINT('Ctrl Pts',(-1.26585586800006,15.2,10.876728433));
#228930=CARTESIAN_POINT('Ctrl Pts',(-1.26585586800006,11.6,10.876728433));
#228931=CARTESIAN_POINT('Ctrl Pts',(-1.26650375300006,15.2,10.873831998));
#228932=CARTESIAN_POINT('Ctrl Pts',(-1.26650375300006,11.6,10.873831998));
#228933=CARTESIAN_POINT('Ctrl Pts',(-1.26714807000006,15.2,10.870940349));
#228934=CARTESIAN_POINT('Ctrl Pts',(-1.26714807000006,11.6,10.870940349));
#228935=CARTESIAN_POINT('Ctrl Pts',(-1.26778882500005,15.2,10.868053496));
#228936=CARTESIAN_POINT('Ctrl Pts',(-1.26778882500005,11.6,10.868053496));
#228937=CARTESIAN_POINT('Ctrl Pts',(-1.26842602500005,15.2,10.86517145));
#228938=CARTESIAN_POINT('Ctrl Pts',(-1.26842602500005,11.6,10.86517145));
#228939=CARTESIAN_POINT('Ctrl Pts',(-1.26905967300006,15.2,10.862294222));
#228940=CARTESIAN_POINT('Ctrl Pts',(-1.26905967300006,11.6,10.862294222));
#228941=CARTESIAN_POINT('Ctrl Pts',(-1.26968977600006,15.2,10.859421824));
#228942=CARTESIAN_POINT('Ctrl Pts',(-1.26968977600006,11.6,10.859421824));
#228943=CARTESIAN_POINT('Ctrl Pts',(-1.27031633900006,15.2,10.856554268));
#228944=CARTESIAN_POINT('Ctrl Pts',(-1.27031633900006,11.6,10.856554268));
#228945=CARTESIAN_POINT('Ctrl Pts',(-1.27093936800006,15.2,10.853691564));
#228946=CARTESIAN_POINT('Ctrl Pts',(-1.27093936800006,11.6,10.853691564));
#228947=CARTESIAN_POINT('Ctrl Pts',(-1.27155886700006,15.2,10.850833723));
#228948=CARTESIAN_POINT('Ctrl Pts',(-1.27155886700006,11.6,10.850833723));
#228949=CARTESIAN_POINT('Ctrl Pts',(-1.27217484300005,15.2,10.847980757));
#228950=CARTESIAN_POINT('Ctrl Pts',(-1.27217484300005,11.6,10.847980757));
#228951=CARTESIAN_POINT('Ctrl Pts',(-1.27278730200006,15.2,10.845132678));
#228952=CARTESIAN_POINT('Ctrl Pts',(-1.27278730200006,11.6,10.845132678));
#228953=CARTESIAN_POINT('Ctrl Pts',(-1.27339624900006,15.2,10.842289496));
#228954=CARTESIAN_POINT('Ctrl Pts',(-1.27339624900006,11.6,10.842289496));
#228955=CARTESIAN_POINT('Ctrl Pts',(-1.27400168800005,15.2,10.839451223));
#228956=CARTESIAN_POINT('Ctrl Pts',(-1.27400168800005,11.6,10.839451223));
#228957=CARTESIAN_POINT('Ctrl Pts',(-1.27460362700006,15.2,10.836617871));
#228958=CARTESIAN_POINT('Ctrl Pts',(-1.27460362700006,11.6,10.836617871));
#228959=CARTESIAN_POINT('Ctrl Pts',(-1.27520207000006,15.2,10.83378945));
#228960=CARTESIAN_POINT('Ctrl Pts',(-1.27520207000006,11.6,10.83378945));
#228961=CARTESIAN_POINT('Ctrl Pts',(-1.27579702400006,15.2,10.830965973));
#228962=CARTESIAN_POINT('Ctrl Pts',(-1.27579702400006,11.6,10.830965973));
#228963=CARTESIAN_POINT('Ctrl Pts',(-1.27638849400006,15.2,10.82814745));
#228964=CARTESIAN_POINT('Ctrl Pts',(-1.27638849400006,11.6,10.82814745));
#228965=CARTESIAN_POINT('Ctrl Pts',(-1.27697648500006,15.2,10.825333894));
#228966=CARTESIAN_POINT('Ctrl Pts',(-1.27697648500006,11.6,10.825333894));
#228967=CARTESIAN_POINT('Ctrl Pts',(-1.27756100500006,15.2,10.822525316));
#228968=CARTESIAN_POINT('Ctrl Pts',(-1.27756100500006,11.6,10.822525316));
#228969=CARTESIAN_POINT('Ctrl Pts',(-1.27814205700005,15.2,10.819721727));
#228970=CARTESIAN_POINT('Ctrl Pts',(-1.27814205700005,11.6,10.819721727));
#228971=CARTESIAN_POINT('Ctrl Pts',(-1.27871964800006,15.2,10.816923139));
#228972=CARTESIAN_POINT('Ctrl Pts',(-1.27871964800006,11.6,10.816923139));
#228973=CARTESIAN_POINT('Ctrl Pts',(-1.27929378500006,15.2,10.814129563));
#228974=CARTESIAN_POINT('Ctrl Pts',(-1.27929378500006,11.6,10.814129563));
#228975=CARTESIAN_POINT('Ctrl Pts',(-1.27986447300006,15.2,10.811341012));
#228976=CARTESIAN_POINT('Ctrl Pts',(-1.27986447300006,11.6,10.811341012));
#228977=CARTESIAN_POINT('Ctrl Pts',(-1.28043171600006,15.2,10.808557496));
#228978=CARTESIAN_POINT('Ctrl Pts',(-1.28043171600006,11.6,10.808557496));
#228979=CARTESIAN_POINT('Ctrl Pts',(-1.28099552200006,15.2,10.805779029));
#228980=CARTESIAN_POINT('Ctrl Pts',(-1.28099552200006,11.6,10.805779029));
#228981=CARTESIAN_POINT('Ctrl Pts',(-1.28155589700006,15.2,10.803005619));
#228982=CARTESIAN_POINT('Ctrl Pts',(-1.28155589700006,11.6,10.803005619));
#228983=CARTESIAN_POINT('Ctrl Pts',(-1.28211284600006,15.2,10.800237282));
#228984=CARTESIAN_POINT('Ctrl Pts',(-1.28211284600006,11.6,10.800237282));
#228985=CARTESIAN_POINT('Ctrl Pts',(-1.28266637500006,15.2,10.797474027));
#228986=CARTESIAN_POINT('Ctrl Pts',(-1.28266637500006,11.6,10.797474027));
#228987=CARTESIAN_POINT('Ctrl Pts',(-1.28321649000006,15.2,10.794715865));
#228988=CARTESIAN_POINT('Ctrl Pts',(-1.28321649000006,11.6,10.794715865));
#228989=CARTESIAN_POINT('Ctrl Pts',(-1.28376319800006,15.2,10.79196281));
#228990=CARTESIAN_POINT('Ctrl Pts',(-1.28376319800006,11.6,10.79196281));
#228991=CARTESIAN_POINT('Ctrl Pts',(-1.28430650400006,15.2,10.789214874));
#228992=CARTESIAN_POINT('Ctrl Pts',(-1.28430650400006,11.6,10.789214874));
#228993=CARTESIAN_POINT('Ctrl Pts',(-1.28484641400005,15.2,10.786472066));
#228994=CARTESIAN_POINT('Ctrl Pts',(-1.28484641400005,11.6,10.786472066));
#228995=CARTESIAN_POINT('Ctrl Pts',(-1.28538293400006,15.2,10.783734401));
#228996=CARTESIAN_POINT('Ctrl Pts',(-1.28538293400006,11.6,10.783734401));
#228997=CARTESIAN_POINT('Ctrl Pts',(-1.28591607100006,15.2,10.781001889));
#228998=CARTESIAN_POINT('Ctrl Pts',(-1.28591607100006,11.6,10.781001889));
#228999=CARTESIAN_POINT('Ctrl Pts',(-1.28644583000006,15.2,10.778274542));
#229000=CARTESIAN_POINT('Ctrl Pts',(-1.28644583000006,11.6,10.778274542));
#229001=CARTESIAN_POINT('Ctrl Pts',(-1.28697221900006,15.2,10.775552373));
#229002=CARTESIAN_POINT('Ctrl Pts',(-1.28697221900006,11.6,10.775552373));
#229003=CARTESIAN_POINT('Ctrl Pts',(-1.28749524100006,15.2,10.772835393));
#229004=CARTESIAN_POINT('Ctrl Pts',(-1.28749524100006,11.6,10.772835393));
#229005=CARTESIAN_POINT('Ctrl Pts',(-1.28801490600006,15.2,10.770123615));
#229006=CARTESIAN_POINT('Ctrl Pts',(-1.28801490600006,11.6,10.770123615));
#229007=CARTESIAN_POINT('Ctrl Pts',(-1.28853121600006,15.2,10.767417049));
#229008=CARTESIAN_POINT('Ctrl Pts',(-1.28853121600006,11.6,10.767417049));
#229009=CARTESIAN_POINT('Ctrl Pts',(-1.28904418100006,15.2,10.764715709));
#229010=CARTESIAN_POINT('Ctrl Pts',(-1.28904418100006,11.6,10.764715709));
#229011=CARTESIAN_POINT('Ctrl Pts',(-1.28955380600006,15.2,10.762019607));
#229012=CARTESIAN_POINT('Ctrl Pts',(-1.28955380600006,11.6,10.762019607));
#229013=CARTESIAN_POINT('Ctrl Pts',(-1.29006009600006,15.2,10.759328754));
#229014=CARTESIAN_POINT('Ctrl Pts',(-1.29006009600006,11.6,10.759328754));
#229015=CARTESIAN_POINT('Ctrl Pts',(-1.29056305900005,15.2,10.756643162));
#229016=CARTESIAN_POINT('Ctrl Pts',(-1.29056305900005,11.6,10.756643162));
#229017=CARTESIAN_POINT('Ctrl Pts',(-1.29106270000006,15.2,10.753962845));
#229018=CARTESIAN_POINT('Ctrl Pts',(-1.29106270000006,11.6,10.753962845));
#229019=CARTESIAN_POINT('Ctrl Pts',(-1.29155902700006,15.2,10.751287813));
#229020=CARTESIAN_POINT('Ctrl Pts',(-1.29155902700006,11.6,10.751287813));
#229021=CARTESIAN_POINT('Ctrl Pts',(-1.29205204400006,15.2,10.748618079));
#229022=CARTESIAN_POINT('Ctrl Pts',(-1.29205204400006,11.6,10.748618079));
#229023=CARTESIAN_POINT('Ctrl Pts',(-1.29254176000006,15.2,10.745953656));
#229024=CARTESIAN_POINT('Ctrl Pts',(-1.29254176000006,11.6,10.745953656));
#229025=CARTESIAN_POINT('Ctrl Pts',(-1.29302817900006,15.2,10.743294555));
#229026=CARTESIAN_POINT('Ctrl Pts',(-1.29302817900006,11.6,10.743294555));
#229027=CARTESIAN_POINT('Ctrl Pts',(-1.29351131000006,15.2,10.740640789));
#229028=CARTESIAN_POINT('Ctrl Pts',(-1.29351131000006,11.6,10.740640789));
#229029=CARTESIAN_POINT('Ctrl Pts',(-1.29399115800006,15.2,10.73799237));
#229030=CARTESIAN_POINT('Ctrl Pts',(-1.29399115800006,11.6,10.73799237));
#229031=CARTESIAN_POINT('Ctrl Pts',(-1.29446772900006,15.2,10.73534931));
#229032=CARTESIAN_POINT('Ctrl Pts',(-1.29446772900006,11.6,10.73534931));
#229033=CARTESIAN_POINT('Ctrl Pts',(-1.29494103100006,15.2,10.732711622));
#229034=CARTESIAN_POINT('Ctrl Pts',(-1.29494103100006,11.6,10.732711622));
#229035=CARTESIAN_POINT('Ctrl Pts',(-1.29541106900006,15.2,10.730079318));
#229036=CARTESIAN_POINT('Ctrl Pts',(-1.29541106900006,11.6,10.730079318));
#229037=CARTESIAN_POINT('Ctrl Pts',(-1.29587785100005,15.2,10.727452412));
#229038=CARTESIAN_POINT('Ctrl Pts',(-1.29587785100005,11.6,10.727452412));
#229039=CARTESIAN_POINT('Ctrl Pts',(-1.29634138200006,15.2,10.724830913));
#229040=CARTESIAN_POINT('Ctrl Pts',(-1.29634138200006,11.6,10.724830913));
#229041=CARTESIAN_POINT('Ctrl Pts',(-1.29680167100006,15.2,10.722214836));
#229042=CARTESIAN_POINT('Ctrl Pts',(-1.29680167100006,11.6,10.722214836));
#229043=CARTESIAN_POINT('Ctrl Pts',(-1.29725872200006,15.2,10.719604193));
#229044=CARTESIAN_POINT('Ctrl Pts',(-1.29725872200006,11.6,10.719604193));
#229045=CARTESIAN_POINT('Ctrl Pts',(-1.29771254400006,15.2,10.716998997));
#229046=CARTESIAN_POINT('Ctrl Pts',(-1.29771254400006,11.6,10.716998997));
#229047=CARTESIAN_POINT('Ctrl Pts',(-1.29816314300006,15.2,10.714399259));
#229048=CARTESIAN_POINT('Ctrl Pts',(-1.29816314300006,11.6,10.714399259));
#229049=CARTESIAN_POINT('Ctrl Pts',(-1.29861052400006,15.2,10.711804993));
#229050=CARTESIAN_POINT('Ctrl Pts',(-1.29861052400006,11.6,10.711804993));
#229051=CARTESIAN_POINT('Ctrl Pts',(-1.29905469700006,15.2,10.709216211));
#229052=CARTESIAN_POINT('Ctrl Pts',(-1.29905469700006,11.6,10.709216211));
#229053=CARTESIAN_POINT('Ctrl Pts',(-1.29949566600006,15.2,10.706632926));
#229054=CARTESIAN_POINT('Ctrl Pts',(-1.29949566600006,11.6,10.706632926));
#229055=CARTESIAN_POINT('Ctrl Pts',(-1.29993343800006,15.2,10.70405515));
#229056=CARTESIAN_POINT('Ctrl Pts',(-1.29993343800006,11.6,10.70405515));
#229057=CARTESIAN_POINT('Ctrl Pts',(-1.30036802200006,15.2,10.701482895));
#229058=CARTESIAN_POINT('Ctrl Pts',(-1.30036802200006,11.6,10.701482895));
#229059=CARTESIAN_POINT('Ctrl Pts',(-1.30079942300006,15.2,10.698916176));
#229060=CARTESIAN_POINT('Ctrl Pts',(-1.30079942300006,11.6,10.698916176));
#229061=CARTESIAN_POINT('Ctrl Pts',(-1.30122764900006,15.2,10.696355005));
#229062=CARTESIAN_POINT('Ctrl Pts',(-1.30122764900006,11.6,10.696355005));
#229063=CARTESIAN_POINT('Ctrl Pts',(-1.30165270600005,15.2,10.693799394));
#229064=CARTESIAN_POINT('Ctrl Pts',(-1.30165270600005,11.6,10.693799394));
#229065=CARTESIAN_POINT('Ctrl Pts',(-1.30207460100006,15.2,10.691249355));
#229066=CARTESIAN_POINT('Ctrl Pts',(-1.30207460100006,11.6,10.691249355));
#229067=CARTESIAN_POINT('Ctrl Pts',(-1.30249334300006,15.2,10.688704903));
#229068=CARTESIAN_POINT('Ctrl Pts',(-1.30249334300006,11.6,10.688704903));
#229069=CARTESIAN_POINT('Ctrl Pts',(-1.30290893600006,15.2,10.686166049));
#229070=CARTESIAN_POINT('Ctrl Pts',(-1.30290893600006,11.6,10.686166049));
#229071=CARTESIAN_POINT('Ctrl Pts',(-1.30332138800005,15.2,10.683632807));
#229072=CARTESIAN_POINT('Ctrl Pts',(-1.30332138800005,11.6,10.683632807));
#229073=CARTESIAN_POINT('Ctrl Pts',(-1.30373070700006,15.2,10.681105189));
#229074=CARTESIAN_POINT('Ctrl Pts',(-1.30373070700006,11.6,10.681105189));
#229075=CARTESIAN_POINT('Ctrl Pts',(-1.30413690000006,15.2,10.678583208));
#229076=CARTESIAN_POINT('Ctrl Pts',(-1.30413690000006,11.6,10.678583208));
#229077=CARTESIAN_POINT('Ctrl Pts',(-1.30453997400006,15.2,10.676066878));
#229078=CARTESIAN_POINT('Ctrl Pts',(-1.30453997400006,11.6,10.676066878));
#229079=CARTESIAN_POINT('Ctrl Pts',(-1.30493993500005,15.2,10.673556212));
#229080=CARTESIAN_POINT('Ctrl Pts',(-1.30493993500005,11.6,10.673556212));
#229081=CARTESIAN_POINT('Ctrl Pts',(-1.30533679100005,15.2,10.671051222));
#229082=CARTESIAN_POINT('Ctrl Pts',(-1.30533679100005,11.6,10.671051222));
#229083=CARTESIAN_POINT('Ctrl Pts',(-1.30573055000006,15.2,10.668551921));
#229084=CARTESIAN_POINT('Ctrl Pts',(-1.30573055000006,11.6,10.668551921));
#229085=CARTESIAN_POINT('Ctrl Pts',(-1.30612121800006,15.2,10.666058323));
#229086=CARTESIAN_POINT('Ctrl Pts',(-1.30612121800006,11.6,10.666058323));
#229087=CARTESIAN_POINT('Ctrl Pts',(-1.30650880400006,15.2,10.663570442));
#229088=CARTESIAN_POINT('Ctrl Pts',(-1.30650880400006,11.6,10.663570442));
#229089=CARTESIAN_POINT('Ctrl Pts',(-1.30689331300006,15.2,10.661088288));
#229090=CARTESIAN_POINT('Ctrl Pts',(-1.30689331300006,11.6,10.661088288));
#229091=CARTESIAN_POINT('Ctrl Pts',(-1.30727475400006,15.2,10.658611876));
#229092=CARTESIAN_POINT('Ctrl Pts',(-1.30727475400006,11.6,10.658611876));
#229093=CARTESIAN_POINT('Ctrl Pts',(-1.30765313300006,15.2,10.656141221));
#229094=CARTESIAN_POINT('Ctrl Pts',(-1.30765313300006,11.6,10.656141221));
#229095=CARTESIAN_POINT('Ctrl Pts',(-1.30802846000006,15.2,10.653676333));
#229096=CARTESIAN_POINT('Ctrl Pts',(-1.30802846000006,11.6,10.653676333));
#229097=CARTESIAN_POINT('Ctrl Pts',(-1.30840073900006,15.2,10.651217227));
#229098=CARTESIAN_POINT('Ctrl Pts',(-1.30840073900006,11.6,10.651217227));
#229099=CARTESIAN_POINT('Ctrl Pts',(-1.30876997900006,15.2,10.648763916));
#229100=CARTESIAN_POINT('Ctrl Pts',(-1.30876997900006,11.6,10.648763916));
#229101=CARTESIAN_POINT('Ctrl Pts',(-1.30913618800006,15.2,10.646316414));
#229102=CARTESIAN_POINT('Ctrl Pts',(-1.30913618800006,11.6,10.646316414));
#229103=CARTESIAN_POINT('Ctrl Pts',(-1.30949937300006,15.2,10.643874734));
#229104=CARTESIAN_POINT('Ctrl Pts',(-1.30949937300006,11.6,10.643874734));
#229105=CARTESIAN_POINT('Ctrl Pts',(-1.30985954300006,15.2,10.641438888));
#229106=CARTESIAN_POINT('Ctrl Pts',(-1.30985954300006,11.6,10.641438888));
#229107=CARTESIAN_POINT('Ctrl Pts',(-1.31021670300006,15.2,10.639008892));
#229108=CARTESIAN_POINT('Ctrl Pts',(-1.31021670300006,11.6,10.639008892));
#229109=CARTESIAN_POINT('Ctrl Pts',(-1.31057086200006,15.2,10.636584757));
#229110=CARTESIAN_POINT('Ctrl Pts',(-1.31057086200006,11.6,10.636584757));
#229111=CARTESIAN_POINT('Ctrl Pts',(-1.31092202700006,15.2,10.634166497));
#229112=CARTESIAN_POINT('Ctrl Pts',(-1.31092202700006,11.6,10.634166497));
#229113=CARTESIAN_POINT('Ctrl Pts',(-1.31127020600006,15.2,10.631754128));
#229114=CARTESIAN_POINT('Ctrl Pts',(-1.31127020600006,11.6,10.631754128));
#229115=CARTESIAN_POINT('Ctrl Pts',(-1.31161540800006,15.2,10.629347661));
#229116=CARTESIAN_POINT('Ctrl Pts',(-1.31161540800006,11.6,10.629347661));
#229117=CARTESIAN_POINT('Ctrl Pts',(-1.31195763900006,15.2,10.62694711));
#229118=CARTESIAN_POINT('Ctrl Pts',(-1.31195763900006,11.6,10.62694711));
#229119=CARTESIAN_POINT('Ctrl Pts',(-1.31229690700006,15.2,10.624552489));
#229120=CARTESIAN_POINT('Ctrl Pts',(-1.31229690700006,11.6,10.624552489));
#229121=CARTESIAN_POINT('Ctrl Pts',(-1.31263322100006,15.2,10.622163811));
#229122=CARTESIAN_POINT('Ctrl Pts',(-1.31263322100006,11.6,10.622163811));
#229123=CARTESIAN_POINT('Ctrl Pts',(-1.31296658700006,15.2,10.619781092));
#229124=CARTESIAN_POINT('Ctrl Pts',(-1.31296658700006,11.6,10.619781092));
#229125=CARTESIAN_POINT('Ctrl Pts',(-1.31329701400006,15.2,10.617404342));
#229126=CARTESIAN_POINT('Ctrl Pts',(-1.31329701400006,11.6,10.617404342));
#229127=CARTESIAN_POINT('Ctrl Pts',(-1.31362451000006,15.2,10.615033579));
#229128=CARTESIAN_POINT('Ctrl Pts',(-1.31362451000006,11.6,10.615033579));
#229129=CARTESIAN_POINT('Ctrl Pts',(-1.31394908200006,15.2,10.612668813));
#229130=CARTESIAN_POINT('Ctrl Pts',(-1.31394908200006,11.6,10.612668813));
#229131=CARTESIAN_POINT('Ctrl Pts',(-1.31427073800006,15.2,10.61031006));
#229132=CARTESIAN_POINT('Ctrl Pts',(-1.31427073800006,11.6,10.61031006));
#229133=CARTESIAN_POINT('Ctrl Pts',(-1.31458948800006,15.2,10.607957333));
#229134=CARTESIAN_POINT('Ctrl Pts',(-1.31458948800006,11.6,10.607957333));
#229135=CARTESIAN_POINT('Ctrl Pts',(-1.31490533800006,15.2,10.605610646));
#229136=CARTESIAN_POINT('Ctrl Pts',(-1.31490533800006,11.6,10.605610646));
#229137=CARTESIAN_POINT('Ctrl Pts',(-1.31521829600006,15.2,10.603270014));
#229138=CARTESIAN_POINT('Ctrl Pts',(-1.31521829600006,11.6,10.603270014));
#229139=CARTESIAN_POINT('Ctrl Pts',(-1.31552837100006,15.2,10.60093545));
#229140=CARTESIAN_POINT('Ctrl Pts',(-1.31552837100006,11.6,10.60093545));
#229141=CARTESIAN_POINT('Ctrl Pts',(-1.31583557200006,15.2,10.598606967));
#229142=CARTESIAN_POINT('Ctrl Pts',(-1.31583557200006,11.6,10.598606967));
#229143=CARTESIAN_POINT('Ctrl Pts',(-1.31613990500006,15.2,10.596284581));
#229144=CARTESIAN_POINT('Ctrl Pts',(-1.31613990500006,11.6,10.596284581));
#229145=CARTESIAN_POINT('Ctrl Pts',(-1.31644137900006,15.2,10.593968305));
#229146=CARTESIAN_POINT('Ctrl Pts',(-1.31644137900006,11.6,10.593968305));
#229147=CARTESIAN_POINT('Ctrl Pts',(-1.31674000300006,15.2,10.591658154));
#229148=CARTESIAN_POINT('Ctrl Pts',(-1.31674000300006,11.6,10.591658154));
#229149=CARTESIAN_POINT('Ctrl Pts',(-1.31703578300006,15.2,10.589354141));
#229150=CARTESIAN_POINT('Ctrl Pts',(-1.31703578300006,11.6,10.589354141));
#229151=CARTESIAN_POINT('Ctrl Pts',(-1.31732873000006,15.2,10.58705628));
#229152=CARTESIAN_POINT('Ctrl Pts',(-1.31732873000006,11.6,10.58705628));
#229153=CARTESIAN_POINT('Ctrl Pts',(-1.31761885100006,15.2,10.584764587));
#229154=CARTESIAN_POINT('Ctrl Pts',(-1.31761885100006,11.6,10.584764587));
#229155=CARTESIAN_POINT('Ctrl Pts',(-1.31790615400006,15.2,10.582479075));
#229156=CARTESIAN_POINT('Ctrl Pts',(-1.31790615400006,11.6,10.582479075));
#229157=CARTESIAN_POINT('Ctrl Pts',(-1.31819064900006,15.2,10.580199759));
#229158=CARTESIAN_POINT('Ctrl Pts',(-1.31819064900006,11.6,10.580199759));
#229159=CARTESIAN_POINT('Ctrl Pts',(-1.31847234300006,15.2,10.577926652));
#229160=CARTESIAN_POINT('Ctrl Pts',(-1.31847234300006,11.6,10.577926652));
#229161=CARTESIAN_POINT('Ctrl Pts',(-1.31875124500006,15.2,10.575659769));
#229162=CARTESIAN_POINT('Ctrl Pts',(-1.31875124500006,11.6,10.575659769));
#229163=CARTESIAN_POINT('Ctrl Pts',(-1.31902736400006,15.2,10.573399125));
#229164=CARTESIAN_POINT('Ctrl Pts',(-1.31902736400006,11.6,10.573399125));
#229165=CARTESIAN_POINT('Ctrl Pts',(-1.31930070600006,15.2,10.571144734));
#229166=CARTESIAN_POINT('Ctrl Pts',(-1.31930070600006,11.6,10.571144734));
#229167=CARTESIAN_POINT('Ctrl Pts',(-1.31957128300005,15.2,10.568896611));
#229168=CARTESIAN_POINT('Ctrl Pts',(-1.31957128300005,11.6,10.568896611));
#229169=CARTESIAN_POINT('Ctrl Pts',(-1.31983910100006,15.2,10.566654769));
#229170=CARTESIAN_POINT('Ctrl Pts',(-1.31983910100006,11.6,10.566654769));
#229171=CARTESIAN_POINT('Ctrl Pts',(-1.32010417000005,15.2,10.564419225));
#229172=CARTESIAN_POINT('Ctrl Pts',(-1.32010417000005,11.6,10.564419225));
#229173=CARTESIAN_POINT('Ctrl Pts',(-1.32036649900006,15.2,10.562189991));
#229174=CARTESIAN_POINT('Ctrl Pts',(-1.32036649900006,11.6,10.562189991));
#229175=CARTESIAN_POINT('Ctrl Pts',(-1.32062609500006,15.2,10.559967083));
#229176=CARTESIAN_POINT('Ctrl Pts',(-1.32062609500006,11.6,10.559967083));
#229177=CARTESIAN_POINT('Ctrl Pts',(-1.32088296800006,15.2,10.557750516));
#229178=CARTESIAN_POINT('Ctrl Pts',(-1.32088296800006,11.6,10.557750516));
#229179=CARTESIAN_POINT('Ctrl Pts',(-1.32113712700006,15.2,10.555540305));
#229180=CARTESIAN_POINT('Ctrl Pts',(-1.32113712700006,11.6,10.555540305));
#229181=CARTESIAN_POINT('Ctrl Pts',(-1.32138858000006,15.2,10.553336463));
#229182=CARTESIAN_POINT('Ctrl Pts',(-1.32138858000006,11.6,10.553336463));
#229183=CARTESIAN_POINT('Ctrl Pts',(-1.32163733600006,15.2,10.551139006));
#229184=CARTESIAN_POINT('Ctrl Pts',(-1.32163733600006,11.6,10.551139006));
#229185=CARTESIAN_POINT('Ctrl Pts',(-1.32188340500006,15.2,10.548947949));
#229186=CARTESIAN_POINT('Ctrl Pts',(-1.32188340500006,11.6,10.548947949));
#229187=CARTESIAN_POINT('Ctrl Pts',(-1.32212679500006,15.2,10.546763307));
#229188=CARTESIAN_POINT('Ctrl Pts',(-1.32212679500006,11.6,10.546763307));
#229189=CARTESIAN_POINT('Ctrl Pts',(-1.32236751400006,15.2,10.544585094));
#229190=CARTESIAN_POINT('Ctrl Pts',(-1.32236751400006,11.6,10.544585094));
#229191=CARTESIAN_POINT('Ctrl Pts',(-1.32260557300006,15.2,10.542413324));
#229192=CARTESIAN_POINT('Ctrl Pts',(-1.32260557300006,11.6,10.542413324));
#229193=CARTESIAN_POINT('Ctrl Pts',(-1.32284098000006,15.2,10.540248015));
#229194=CARTESIAN_POINT('Ctrl Pts',(-1.32284098000006,11.6,10.540248015));
#229195=CARTESIAN_POINT('Ctrl Pts',(-1.32307374400006,15.2,10.538089179));
#229196=CARTESIAN_POINT('Ctrl Pts',(-1.32307374400006,11.6,10.538089179));
#229197=CARTESIAN_POINT('Ctrl Pts',(-1.32330387400006,15.2,10.535936834));
#229198=CARTESIAN_POINT('Ctrl Pts',(-1.32330387400006,11.6,10.535936834));
#229199=CARTESIAN_POINT('Ctrl Pts',(-1.32353137900005,15.2,10.533790993));
#229200=CARTESIAN_POINT('Ctrl Pts',(-1.32353137900005,11.6,10.533790993));
#229201=CARTESIAN_POINT('Ctrl Pts',(-1.32375627000005,15.2,10.531651672));
#229202=CARTESIAN_POINT('Ctrl Pts',(-1.32375627000005,11.6,10.531651672));
#229203=CARTESIAN_POINT('Ctrl Pts',(-1.32397855300006,15.2,10.529518886));
#229204=CARTESIAN_POINT('Ctrl Pts',(-1.32397855300006,11.6,10.529518886));
#229205=CARTESIAN_POINT('Ctrl Pts',(-1.32419824100006,15.2,10.52739265));
#229206=CARTESIAN_POINT('Ctrl Pts',(-1.32419824100006,11.6,10.52739265));
#229207=CARTESIAN_POINT('Ctrl Pts',(-1.32441534000006,15.2,10.52527298));
#229208=CARTESIAN_POINT('Ctrl Pts',(-1.32441534000006,11.6,10.52527298));
#229209=CARTESIAN_POINT('Ctrl Pts',(-1.32462986200006,15.2,10.52315989));
#229210=CARTESIAN_POINT('Ctrl Pts',(-1.32462986200006,11.6,10.52315989));
#229211=CARTESIAN_POINT('Ctrl Pts',(-1.32484181500006,15.2,10.521053397));
#229212=CARTESIAN_POINT('Ctrl Pts',(-1.32484181500006,11.6,10.521053397));
#229213=CARTESIAN_POINT('Ctrl Pts',(-1.32505120800006,15.2,10.518953515));
#229214=CARTESIAN_POINT('Ctrl Pts',(-1.32505120800006,11.6,10.518953515));
#229215=CARTESIAN_POINT('Ctrl Pts',(-1.32525805200006,15.2,10.516860261));
#229216=CARTESIAN_POINT('Ctrl Pts',(-1.32525805200006,11.6,10.516860261));
#229217=CARTESIAN_POINT('Ctrl Pts',(-1.32546235400006,15.2,10.514773649));
#229218=CARTESIAN_POINT('Ctrl Pts',(-1.32546235400006,11.6,10.514773649));
#229219=CARTESIAN_POINT('Ctrl Pts',(-1.32566412700006,15.2,10.512693695));
#229220=CARTESIAN_POINT('Ctrl Pts',(-1.32566412700006,11.6,10.512693695));
#229221=CARTESIAN_POINT('Ctrl Pts',(-1.32586337700006,15.2,10.510620415));
#229222=CARTESIAN_POINT('Ctrl Pts',(-1.32586337700006,11.6,10.510620415));
#229223=CARTESIAN_POINT('Ctrl Pts',(-1.32606011800006,15.2,10.508553824));
#229224=CARTESIAN_POINT('Ctrl Pts',(-1.32606011800006,11.6,10.508553824));
#229225=CARTESIAN_POINT('Ctrl Pts',(-1.32625435500006,15.2,10.506493939));
#229226=CARTESIAN_POINT('Ctrl Pts',(-1.32625435500006,11.6,10.506493939));
#229227=CARTESIAN_POINT('Ctrl Pts',(-1.32644610000006,15.2,10.504440774));
#229228=CARTESIAN_POINT('Ctrl Pts',(-1.32644610000006,11.6,10.504440774));
#229229=CARTESIAN_POINT('Ctrl Pts',(-1.32663536400006,15.2,10.502394347));
#229230=CARTESIAN_POINT('Ctrl Pts',(-1.32663536400006,11.6,10.502394347));
#229231=CARTESIAN_POINT('Ctrl Pts',(-1.32682215400005,15.2,10.500354671));
#229232=CARTESIAN_POINT('Ctrl Pts',(-1.32682215400005,11.6,10.500354671));
#229233=CARTESIAN_POINT('Ctrl Pts',(-1.32700648100006,15.2,10.498321763));
#229234=CARTESIAN_POINT('Ctrl Pts',(-1.32700648100006,11.6,10.498321763));
#229235=CARTESIAN_POINT('Ctrl Pts',(-1.32718835600006,15.2,10.49629564));
#229236=CARTESIAN_POINT('Ctrl Pts',(-1.32718835600006,11.6,10.49629564));
#229237=CARTESIAN_POINT('Ctrl Pts',(-1.32736778800005,15.2,10.494276317));
#229238=CARTESIAN_POINT('Ctrl Pts',(-1.32736778800005,11.6,10.494276317));
#229239=CARTESIAN_POINT('Ctrl Pts',(-1.32754478700006,15.2,10.49226381));
#229240=CARTESIAN_POINT('Ctrl Pts',(-1.32754478700006,11.6,10.49226381));
#229241=CARTESIAN_POINT('Ctrl Pts',(-1.32771936300006,15.2,10.490258135));
#229242=CARTESIAN_POINT('Ctrl Pts',(-1.32771936300006,11.6,10.490258135));
#229243=CARTESIAN_POINT('Ctrl Pts',(-1.32789152600005,15.2,10.488259309));
#229244=CARTESIAN_POINT('Ctrl Pts',(-1.32789152600005,11.6,10.488259309));
#229245=CARTESIAN_POINT('Ctrl Pts',(-1.32806128600006,15.2,10.486267346));
#229246=CARTESIAN_POINT('Ctrl Pts',(-1.32806128600006,11.6,10.486267346));
#229247=CARTESIAN_POINT('Ctrl Pts',(-1.32822865400006,15.2,10.484282264));
#229248=CARTESIAN_POINT('Ctrl Pts',(-1.32822865400006,11.6,10.484282264));
#229249=CARTESIAN_POINT('Ctrl Pts',(-1.32839364000006,15.2,10.48230408));
#229250=CARTESIAN_POINT('Ctrl Pts',(-1.32839364000006,11.6,10.48230408));
#229251=CARTESIAN_POINT('Ctrl Pts',(-1.32855625300005,15.2,10.480332808));
#229252=CARTESIAN_POINT('Ctrl Pts',(-1.32855625300005,11.6,10.480332808));
#229253=CARTESIAN_POINT('Ctrl Pts',(-1.32871650400006,15.2,10.478368466));
#229254=CARTESIAN_POINT('Ctrl Pts',(-1.32871650400006,11.6,10.478368466));
#229255=CARTESIAN_POINT('Ctrl Pts',(-1.32887440300006,15.2,10.47641107));
#229256=CARTESIAN_POINT('Ctrl Pts',(-1.32887440300006,11.6,10.47641107));
#229257=CARTESIAN_POINT('Ctrl Pts',(-1.32902996200006,15.2,10.474460635));
#229258=CARTESIAN_POINT('Ctrl Pts',(-1.32902996200006,11.6,10.474460635));
#229259=CARTESIAN_POINT('Ctrl Pts',(-1.32918319000006,15.2,10.47251718));
#229260=CARTESIAN_POINT('Ctrl Pts',(-1.32918319000006,11.6,10.47251718));
#229261=CARTESIAN_POINT('Ctrl Pts',(-1.32933409700006,15.2,10.47058072));
#229262=CARTESIAN_POINT('Ctrl Pts',(-1.32933409700006,11.6,10.47058072));
#229263=CARTESIAN_POINT('Ctrl Pts',(-1.32948269500006,15.2,10.468651272));
#229264=CARTESIAN_POINT('Ctrl Pts',(-1.32948269500006,11.6,10.468651272));
#229265=CARTESIAN_POINT('Ctrl Pts',(-1.32962899400005,15.2,10.466728852));
#229266=CARTESIAN_POINT('Ctrl Pts',(-1.32962899400005,11.6,10.466728852));
#229267=CARTESIAN_POINT('Ctrl Pts',(-1.32977300300006,15.2,10.464813478));
#229268=CARTESIAN_POINT('Ctrl Pts',(-1.32977300300006,11.6,10.464813478));
#229269=CARTESIAN_POINT('Ctrl Pts',(-1.32991473600006,15.2,10.462905165));
#229270=CARTESIAN_POINT('Ctrl Pts',(-1.32991473600006,11.6,10.462905165));
#229271=CARTESIAN_POINT('Ctrl Pts',(-1.33005420100006,15.2,10.461003931));
#229272=CARTESIAN_POINT('Ctrl Pts',(-1.33005420100006,11.6,10.461003931));
#229273=CARTESIAN_POINT('Ctrl Pts',(-1.33019140900006,15.2,10.459109793));
#229274=CARTESIAN_POINT('Ctrl Pts',(-1.33019140900006,11.6,10.459109793));
#229275=CARTESIAN_POINT('Ctrl Pts',(-1.33032637200006,15.2,10.457222767));
#229276=CARTESIAN_POINT('Ctrl Pts',(-1.33032637200006,11.6,10.457222767));
#229277=CARTESIAN_POINT('Ctrl Pts',(-1.33045910000006,15.2,10.455342871));
#229278=CARTESIAN_POINT('Ctrl Pts',(-1.33045910000006,11.6,10.455342871));
#229279=CARTESIAN_POINT('Ctrl Pts',(-1.33058960300006,15.2,10.453470121));
#229280=CARTESIAN_POINT('Ctrl Pts',(-1.33058960300006,11.6,10.453470121));
#229281=CARTESIAN_POINT('Ctrl Pts',(-1.33071789300006,15.2,10.451604534));
#229282=CARTESIAN_POINT('Ctrl Pts',(-1.33071789300006,11.6,10.451604534));
#229283=CARTESIAN_POINT('Ctrl Pts',(-1.33084398200006,15.2,10.449746128));
#229284=CARTESIAN_POINT('Ctrl Pts',(-1.33084398200006,11.6,10.449746128));
#229285=CARTESIAN_POINT('Ctrl Pts',(-1.33096788000006,15.2,10.447894919));
#229286=CARTESIAN_POINT('Ctrl Pts',(-1.33096788000006,11.6,10.447894919));
#229287=CARTESIAN_POINT('Ctrl Pts',(-1.33108959800005,15.2,10.446050926));
#229288=CARTESIAN_POINT('Ctrl Pts',(-1.33108959800005,11.6,10.446050926));
#229289=CARTESIAN_POINT('Ctrl Pts',(-1.33120914700006,15.2,10.444214164));
#229290=CARTESIAN_POINT('Ctrl Pts',(-1.33120914700006,11.6,10.444214164));
#229291=CARTESIAN_POINT('Ctrl Pts',(-1.33132653900006,15.2,10.442384653));
#229292=CARTESIAN_POINT('Ctrl Pts',(-1.33132653900006,11.6,10.442384653));
#229293=CARTESIAN_POINT('Ctrl Pts',(-1.33144178500006,15.2,10.440562408));
#229294=CARTESIAN_POINT('Ctrl Pts',(-1.33144178500006,11.6,10.440562408));
#229295=CARTESIAN_POINT('Ctrl Pts',(-1.33155489500006,15.2,10.438747447));
#229296=CARTESIAN_POINT('Ctrl Pts',(-1.33155489500006,11.6,10.438747447));
#229297=CARTESIAN_POINT('Ctrl Pts',(-1.33166588100006,15.2,10.436939787));
#229298=CARTESIAN_POINT('Ctrl Pts',(-1.33166588100006,11.6,10.436939787));
#229299=CARTESIAN_POINT('Ctrl Pts',(-1.33177475500006,15.2,10.435139449));
#229300=CARTESIAN_POINT('Ctrl Pts',(-1.33177475500006,11.6,10.435139449));
#229301=CARTESIAN_POINT('Ctrl Pts',(-1.33188152900006,15.2,10.433346446));
#229302=CARTESIAN_POINT('Ctrl Pts',(-1.33188152900006,11.6,10.433346446));
#229303=CARTESIAN_POINT('Ctrl Pts',(-1.33198621300005,15.2,10.431560798));
#229304=CARTESIAN_POINT('Ctrl Pts',(-1.33198621300005,11.6,10.431560798));
#229305=CARTESIAN_POINT('Ctrl Pts',(-1.33208882000006,15.2,10.429782522));
#229306=CARTESIAN_POINT('Ctrl Pts',(-1.33208882000006,11.6,10.429782522));
#229307=CARTESIAN_POINT('Ctrl Pts',(-1.33218935900006,15.2,10.428011636));
#229308=CARTESIAN_POINT('Ctrl Pts',(-1.33218935900006,11.6,10.428011636));
#229309=CARTESIAN_POINT('Ctrl Pts',(-1.33228784600006,15.2,10.426248158));
#229310=CARTESIAN_POINT('Ctrl Pts',(-1.33228784600006,11.6,10.426248158));
#229311=CARTESIAN_POINT('Ctrl Pts',(-1.33238428800006,15.2,10.424492106));
#229312=CARTESIAN_POINT('Ctrl Pts',(-1.33238428800006,11.6,10.424492106));
#229313=CARTESIAN_POINT('Ctrl Pts',(-1.33247870000006,15.2,10.422743498));
#229314=CARTESIAN_POINT('Ctrl Pts',(-1.33247870000006,11.6,10.422743498));
#229315=CARTESIAN_POINT('Ctrl Pts',(-1.33257109300006,15.2,10.421002351));
#229316=CARTESIAN_POINT('Ctrl Pts',(-1.33257109300006,11.6,10.421002351));
#229317=CARTESIAN_POINT('Ctrl Pts',(-1.33266147800006,15.2,10.419268684));
#229318=CARTESIAN_POINT('Ctrl Pts',(-1.33266147800006,11.6,10.419268684));
#229319=CARTESIAN_POINT('Ctrl Pts',(-1.33274986800005,15.2,10.417542516));
#229320=CARTESIAN_POINT('Ctrl Pts',(-1.33274986800005,11.6,10.417542516));
#229321=CARTESIAN_POINT('Ctrl Pts',(-1.33283627400006,15.2,10.415823863));
#229322=CARTESIAN_POINT('Ctrl Pts',(-1.33283627400006,11.6,10.415823863));
#229323=CARTESIAN_POINT('Ctrl Pts',(-1.33292070900006,15.2,10.414112744));
#229324=CARTESIAN_POINT('Ctrl Pts',(-1.33292070900006,11.6,10.414112744));
#229325=CARTESIAN_POINT('Ctrl Pts',(-1.33300318500006,15.2,10.412409178));
#229326=CARTESIAN_POINT('Ctrl Pts',(-1.33300318500006,11.6,10.412409178));
#229327=CARTESIAN_POINT('Ctrl Pts',(-1.33308371300006,15.2,10.410713184));
#229328=CARTESIAN_POINT('Ctrl Pts',(-1.33308371300006,11.6,10.410713184));
#229329=CARTESIAN_POINT('Ctrl Pts',(-1.33316230700006,15.2,10.409024779));
#229330=CARTESIAN_POINT('Ctrl Pts',(-1.33316230700006,11.6,10.409024779));
#229331=CARTESIAN_POINT('Ctrl Pts',(-1.33323897800006,15.2,10.407343981));
#229332=CARTESIAN_POINT('Ctrl Pts',(-1.33323897800006,11.6,10.407343981));
#229333=CARTESIAN_POINT('Ctrl Pts',(-1.33331373800006,15.2,10.40567081));
#229334=CARTESIAN_POINT('Ctrl Pts',(-1.33331373800006,11.6,10.40567081));
#229335=CARTESIAN_POINT('Ctrl Pts',(-1.33338660000006,15.2,10.404005284));
#229336=CARTESIAN_POINT('Ctrl Pts',(-1.33338660000006,11.6,10.404005284));
#229337=CARTESIAN_POINT('Ctrl Pts',(-1.33345757800006,15.2,10.402347423));
#229338=CARTESIAN_POINT('Ctrl Pts',(-1.33345757800006,11.6,10.402347423));
#229339=CARTESIAN_POINT('Ctrl Pts',(-1.33352668100006,15.2,10.400697244));
#229340=CARTESIAN_POINT('Ctrl Pts',(-1.33352668100006,11.6,10.400697244));
#229341=CARTESIAN_POINT('Ctrl Pts',(-1.33359392500006,15.2,10.399054765));
#229342=CARTESIAN_POINT('Ctrl Pts',(-1.33359392500006,11.6,10.399054765));
#229343=CARTESIAN_POINT('Ctrl Pts',(-1.33365932000006,15.2,10.397420008));
#229344=CARTESIAN_POINT('Ctrl Pts',(-1.33365932000006,11.6,10.397420008));
#229345=CARTESIAN_POINT('Ctrl Pts',(-1.33372288000006,15.2,10.39579299));
#229346=CARTESIAN_POINT('Ctrl Pts',(-1.33372288000006,11.6,10.39579299));
#229347=CARTESIAN_POINT('Ctrl Pts',(-1.33378461800006,15.2,10.39417373));
#229348=CARTESIAN_POINT('Ctrl Pts',(-1.33378461800006,11.6,10.39417373));
#229349=CARTESIAN_POINT('Ctrl Pts',(-1.33384454600006,15.2,10.392562247));
#229350=CARTESIAN_POINT('Ctrl Pts',(-1.33384454600006,11.6,10.392562247));
#229351=CARTESIAN_POINT('Ctrl Pts',(-1.33390267700006,15.2,10.390958561));
#229352=CARTESIAN_POINT('Ctrl Pts',(-1.33390267700006,11.6,10.390958561));
#229353=CARTESIAN_POINT('Ctrl Pts',(-1.33395902400006,15.2,10.38936269));
#229354=CARTESIAN_POINT('Ctrl Pts',(-1.33395902400006,11.6,10.38936269));
#229355=CARTESIAN_POINT('Ctrl Pts',(-1.33401360000006,15.2,10.387774655));
#229356=CARTESIAN_POINT('Ctrl Pts',(-1.33401360000006,11.6,10.387774655));
#229357=CARTESIAN_POINT('Ctrl Pts',(-1.33406641900006,15.2,10.386194473));
#229358=CARTESIAN_POINT('Ctrl Pts',(-1.33406641900006,11.6,10.386194473));
#229359=CARTESIAN_POINT('Ctrl Pts',(-1.33411749200006,15.2,10.384622166));
#229360=CARTESIAN_POINT('Ctrl Pts',(-1.33411749200006,11.6,10.384622166));
#229361=CARTESIAN_POINT('Ctrl Pts',(-1.33416683400006,15.2,10.383057751));
#229362=CARTESIAN_POINT('Ctrl Pts',(-1.33416683400006,11.6,10.383057751));
#229363=CARTESIAN_POINT('Ctrl Pts',(-1.33421445700006,15.2,10.381501249));
#229364=CARTESIAN_POINT('Ctrl Pts',(-1.33421445700006,11.6,10.381501249));
#229365=CARTESIAN_POINT('Ctrl Pts',(-1.33426037600006,15.2,10.37995268));
#229366=CARTESIAN_POINT('Ctrl Pts',(-1.33426037600006,11.6,10.37995268));
#229367=CARTESIAN_POINT('Ctrl Pts',(-1.33430460300006,15.2,10.378412062));
#229368=CARTESIAN_POINT('Ctrl Pts',(-1.33430460300006,11.6,10.378412062));
#229369=CARTESIAN_POINT('Ctrl Pts',(-1.33434715000006,15.2,10.376879417));
#229370=CARTESIAN_POINT('Ctrl Pts',(-1.33434715000006,11.6,10.376879417));
#229371=CARTESIAN_POINT('Ctrl Pts',(-1.33438803300006,15.2,10.375354763));
#229372=CARTESIAN_POINT('Ctrl Pts',(-1.33438803300006,11.6,10.375354763));
#229373=CARTESIAN_POINT('Ctrl Pts',(-1.33442726500006,15.2,10.373838121));
#229374=CARTESIAN_POINT('Ctrl Pts',(-1.33442726500006,11.6,10.373838121));
#229375=CARTESIAN_POINT('Ctrl Pts',(-1.33446485900006,15.2,10.37232951));
#229376=CARTESIAN_POINT('Ctrl Pts',(-1.33446485900006,11.6,10.37232951));
#229377=CARTESIAN_POINT('Ctrl Pts',(-1.33450082900006,15.2,10.370828952));
#229378=CARTESIAN_POINT('Ctrl Pts',(-1.33450082900006,11.6,10.370828952));
#229379=CARTESIAN_POINT('Ctrl Pts',(-1.33453518800006,15.2,10.369336464));
#229380=CARTESIAN_POINT('Ctrl Pts',(-1.33453518800006,11.6,10.369336464));
#229381=CARTESIAN_POINT('Ctrl Pts',(-1.33456795200006,15.2,10.367852069));
#229382=CARTESIAN_POINT('Ctrl Pts',(-1.33456795200006,11.6,10.367852069));
#229383=CARTESIAN_POINT('Ctrl Pts',(-1.33459913200006,15.2,10.366375787));
#229384=CARTESIAN_POINT('Ctrl Pts',(-1.33459913200006,11.6,10.366375787));
#229385=CARTESIAN_POINT('Ctrl Pts',(-1.33462874400006,15.2,10.364907636));
#229386=CARTESIAN_POINT('Ctrl Pts',(-1.33462874400006,11.6,10.364907636));
#229387=CARTESIAN_POINT('Ctrl Pts',(-1.33465680200006,15.2,10.36344764));
#229388=CARTESIAN_POINT('Ctrl Pts',(-1.33465680200006,11.6,10.36344764));
#229389=CARTESIAN_POINT('Ctrl Pts',(-1.33468331800006,15.2,10.361995816));
#229390=CARTESIAN_POINT('Ctrl Pts',(-1.33468331800006,11.6,10.361995816));
#229391=CARTESIAN_POINT('Ctrl Pts',(-1.33470830800006,15.2,10.360552186));
#229392=CARTESIAN_POINT('Ctrl Pts',(-1.33470830800006,11.6,10.360552186));
#229393=CARTESIAN_POINT('Ctrl Pts',(-1.33473178600006,15.2,10.359116772));
#229394=CARTESIAN_POINT('Ctrl Pts',(-1.33473178600006,11.6,10.359116772));
#229395=CARTESIAN_POINT('Ctrl Pts',(-1.33475376600006,15.2,10.357689593));
#229396=CARTESIAN_POINT('Ctrl Pts',(-1.33475376600006,11.6,10.357689593));
#229397=CARTESIAN_POINT('Ctrl Pts',(-1.33477426300006,15.2,10.35627067));
#229398=CARTESIAN_POINT('Ctrl Pts',(-1.33477426300006,11.6,10.35627067));
#229399=CARTESIAN_POINT('Ctrl Pts',(-1.33479329000005,15.2,10.354860025));
#229400=CARTESIAN_POINT('Ctrl Pts',(-1.33479329000005,11.6,10.354860025));
#229401=CARTESIAN_POINT('Ctrl Pts',(-1.33481086200006,15.2,10.353457679));
#229402=CARTESIAN_POINT('Ctrl Pts',(-1.33481086200006,11.6,10.353457679));
#229403=CARTESIAN_POINT('Ctrl Pts',(-1.33482699600005,15.2,10.352063651));
#229404=CARTESIAN_POINT('Ctrl Pts',(-1.33482699600005,11.6,10.352063651));
#229405=CARTESIAN_POINT('Ctrl Pts',(-1.33484170300005,15.2,10.350677965));
#229406=CARTESIAN_POINT('Ctrl Pts',(-1.33484170300005,11.6,10.350677965));
#229407=CARTESIAN_POINT('Ctrl Pts',(-1.33485499900006,15.2,10.34930064));
#229408=CARTESIAN_POINT('Ctrl Pts',(-1.33485499900006,11.6,10.34930064));
#229409=CARTESIAN_POINT('Ctrl Pts',(-1.33486690000006,15.2,10.347931698));
#229410=CARTESIAN_POINT('Ctrl Pts',(-1.33486690000006,11.6,10.347931698));
#229411=CARTESIAN_POINT('Ctrl Pts',(-1.33487742000006,15.2,10.34657116));
#229412=CARTESIAN_POINT('Ctrl Pts',(-1.33487742000006,11.6,10.34657116));
#229413=CARTESIAN_POINT('Ctrl Pts',(-1.33488657400005,15.2,10.345219048));
#229414=CARTESIAN_POINT('Ctrl Pts',(-1.33488657400005,11.6,10.345219048));
#229415=CARTESIAN_POINT('Ctrl Pts',(-1.33489437700006,15.2,10.343875385));
#229416=CARTESIAN_POINT('Ctrl Pts',(-1.33489437700006,11.6,10.343875385));
#229417=CARTESIAN_POINT('Ctrl Pts',(-1.33490084400006,15.2,10.34254019));
#229418=CARTESIAN_POINT('Ctrl Pts',(-1.33490084400006,11.6,10.34254019));
#229419=CARTESIAN_POINT('Ctrl Pts',(-1.33490598900006,15.2,10.341213486));
#229420=CARTESIAN_POINT('Ctrl Pts',(-1.33490598900006,11.6,10.341213486));
#229421=CARTESIAN_POINT('Ctrl Pts',(-1.33490983000006,15.2,10.339895295));
#229422=CARTESIAN_POINT('Ctrl Pts',(-1.33490983000006,11.6,10.339895295));
#229423=CARTESIAN_POINT('Ctrl Pts',(-1.33491238100006,15.2,10.338585638));
#229424=CARTESIAN_POINT('Ctrl Pts',(-1.33491238100006,11.6,10.338585638));
#229425=CARTESIAN_POINT('Ctrl Pts',(-1.33491365600006,15.2,10.337284538));
#229426=CARTESIAN_POINT('Ctrl Pts',(-1.33491365600006,11.6,10.337284538));
#229427=CARTESIAN_POINT('Ctrl Pts',(-1.33491367300006,15.2,10.335992017));
#229428=CARTESIAN_POINT('Ctrl Pts',(-1.33491367300006,11.6,10.335992017));
#229429=CARTESIAN_POINT('Ctrl Pts',(-1.33491244700006,15.2,10.334708096));
#229430=CARTESIAN_POINT('Ctrl Pts',(-1.33491244700006,11.6,10.334708096));
#229431=CARTESIAN_POINT('Ctrl Pts',(-1.33490999100006,15.2,10.333432799));
#229432=CARTESIAN_POINT('Ctrl Pts',(-1.33490999100006,11.6,10.333432799));
#229433=CARTESIAN_POINT('Ctrl Pts',(-1.33490632300005,15.2,10.332166147));
#229434=CARTESIAN_POINT('Ctrl Pts',(-1.33490632300005,11.6,10.332166147));
#229435=CARTESIAN_POINT('Ctrl Pts',(-1.33490146100006,15.2,10.330908164));
#229436=CARTESIAN_POINT('Ctrl Pts',(-1.33490146100006,11.6,10.330908164));
#229437=CARTESIAN_POINT('Ctrl Pts',(-1.33489541600005,15.2,10.329658871));
#229438=CARTESIAN_POINT('Ctrl Pts',(-1.33489541600005,11.6,10.329658871));
#229439=CARTESIAN_POINT('Ctrl Pts',(-1.33488820600006,15.2,10.32841829));
#229440=CARTESIAN_POINT('Ctrl Pts',(-1.33488820600006,11.6,10.32841829));
#229441=CARTESIAN_POINT('Ctrl Pts',(-1.33487984900006,15.2,10.327186446));
#229442=CARTESIAN_POINT('Ctrl Pts',(-1.33487984900006,11.6,10.327186446));
#229443=CARTESIAN_POINT('Ctrl Pts',(-1.33487035900006,15.2,10.325963361));
#229444=CARTESIAN_POINT('Ctrl Pts',(-1.33487035900006,11.6,10.325963361));
#229445=CARTESIAN_POINT('Ctrl Pts',(-1.33485975300006,15.2,10.324749057));
#229446=CARTESIAN_POINT('Ctrl Pts',(-1.33485975300006,11.6,10.324749057));
#229447=CARTESIAN_POINT('Ctrl Pts',(-1.33484804700006,15.2,10.323543557));
#229448=CARTESIAN_POINT('Ctrl Pts',(-1.33484804700006,11.6,10.323543557));
#229449=CARTESIAN_POINT('Ctrl Pts',(-1.33483525700006,15.2,10.322346887));
#229450=CARTESIAN_POINT('Ctrl Pts',(-1.33483525700006,11.6,10.322346887));
#229451=CARTESIAN_POINT('Ctrl Pts',(-1.33482140000006,15.2,10.321159066));
#229452=CARTESIAN_POINT('Ctrl Pts',(-1.33482140000006,11.6,10.321159066));
#229453=CARTESIAN_POINT('Ctrl Pts',(-1.33480649300005,15.2,10.31998012));
#229454=CARTESIAN_POINT('Ctrl Pts',(-1.33480649300005,11.6,10.31998012));
#229455=CARTESIAN_POINT('Ctrl Pts',(-1.33479055200006,15.2,10.31881007));
#229456=CARTESIAN_POINT('Ctrl Pts',(-1.33479055200006,11.6,10.31881007));
#229457=CARTESIAN_POINT('Ctrl Pts',(-1.33477359500006,15.2,10.317648944));
#229458=CARTESIAN_POINT('Ctrl Pts',(-1.33477359500006,11.6,10.317648944));
#229459=CARTESIAN_POINT('Ctrl Pts',(-1.33475563700006,15.2,10.31649676));
#229460=CARTESIAN_POINT('Ctrl Pts',(-1.33475563700006,11.6,10.31649676));
#229461=CARTESIAN_POINT('Ctrl Pts',(-1.33473669500005,15.2,10.315353546));
#229462=CARTESIAN_POINT('Ctrl Pts',(-1.33473669500005,11.6,10.315353546));
#229463=CARTESIAN_POINT('Ctrl Pts',(-1.33471678800006,15.2,10.314219324));
#229464=CARTESIAN_POINT('Ctrl Pts',(-1.33471678800006,11.6,10.314219324));
#229465=CARTESIAN_POINT('Ctrl Pts',(-1.33469593100006,15.2,10.313094118));
#229466=CARTESIAN_POINT('Ctrl Pts',(-1.33469593100006,11.6,10.313094118));
#229467=CARTESIAN_POINT('Ctrl Pts',(-1.33467414200006,15.2,10.311977953));
#229468=CARTESIAN_POINT('Ctrl Pts',(-1.33467414200006,11.6,10.311977953));
#229469=CARTESIAN_POINT('Ctrl Pts',(-1.33465143900006,15.2,10.310870851));
#229470=CARTESIAN_POINT('Ctrl Pts',(-1.33465143900006,11.6,10.310870851));
#229471=CARTESIAN_POINT('Ctrl Pts',(-1.33462783800006,15.2,10.309772838));
#229472=CARTESIAN_POINT('Ctrl Pts',(-1.33462783800006,11.6,10.309772838));
#229473=CARTESIAN_POINT('Ctrl Pts',(-1.33460335700006,15.2,10.308683939));
#229474=CARTESIAN_POINT('Ctrl Pts',(-1.33460335700006,11.6,10.308683939));
#229475=CARTESIAN_POINT('Ctrl Pts',(-1.33457801400006,15.2,10.307604176));
#229476=CARTESIAN_POINT('Ctrl Pts',(-1.33457801400006,11.6,10.307604176));
#229477=CARTESIAN_POINT('Ctrl Pts',(-1.33455182600006,15.2,10.306533574));
#229478=CARTESIAN_POINT('Ctrl Pts',(-1.33455182600006,11.6,10.306533574));
#229479=CARTESIAN_POINT('Ctrl Pts',(-1.33452481200006,15.2,10.30547216));
#229480=CARTESIAN_POINT('Ctrl Pts',(-1.33452481200006,11.6,10.30547216));
#229481=CARTESIAN_POINT('Ctrl Pts',(-1.33449698900006,15.2,10.304419957));
#229482=CARTESIAN_POINT('Ctrl Pts',(-1.33449698900006,11.6,10.304419957));
#229483=CARTESIAN_POINT('Ctrl Pts',(-1.33446837400006,15.2,10.30337699));
#229484=CARTESIAN_POINT('Ctrl Pts',(-1.33446837400006,11.6,10.30337699));
#229485=CARTESIAN_POINT('Ctrl Pts',(-1.33443898700006,15.2,10.302343284));
#229486=CARTESIAN_POINT('Ctrl Pts',(-1.33443898700006,11.6,10.302343284));
#229487=CARTESIAN_POINT('Ctrl Pts',(-1.33440884500006,15.2,10.301318864));
#229488=CARTESIAN_POINT('Ctrl Pts',(-1.33440884500006,11.6,10.301318864));
#229489=CARTESIAN_POINT('Ctrl Pts',(-1.33437796600006,15.2,10.300303756));
#229490=CARTESIAN_POINT('Ctrl Pts',(-1.33437796600006,11.6,10.300303756));
#229491=CARTESIAN_POINT('Ctrl Pts',(-1.33434636900006,15.2,10.299297985));
#229492=CARTESIAN_POINT('Ctrl Pts',(-1.33434636900006,11.6,10.299297985));
#229493=CARTESIAN_POINT('Ctrl Pts',(-1.33431407200006,15.2,10.298301576));
#229494=CARTESIAN_POINT('Ctrl Pts',(-1.33431407200006,11.6,10.298301576));
#229495=CARTESIAN_POINT('Ctrl Pts',(-1.33428109400006,15.2,10.297314554));
#229496=CARTESIAN_POINT('Ctrl Pts',(-1.33428109400006,11.6,10.297314554));
#229497=CARTESIAN_POINT('Ctrl Pts',(-1.33424745300006,15.2,10.296336947));
#229498=CARTESIAN_POINT('Ctrl Pts',(-1.33424745300006,11.6,10.296336947));
#229499=CARTESIAN_POINT('Ctrl Pts',(-1.33421316800006,15.2,10.295368779));
#229500=CARTESIAN_POINT('Ctrl Pts',(-1.33421316800006,11.6,10.295368779));
#229501=CARTESIAN_POINT('Ctrl Pts',(-1.33417825800006,15.2,10.294410074));
#229502=CARTESIAN_POINT('Ctrl Pts',(-1.33417825800006,11.6,10.294410074));
#229503=CARTESIAN_POINT('Ctrl Pts',(-1.33414274300006,15.2,10.293460863));
#229504=CARTESIAN_POINT('Ctrl Pts',(-1.33414274300006,11.6,10.293460863));
#229505=CARTESIAN_POINT('Ctrl Pts',(-1.33410664000006,15.2,10.292521168));
#229506=CARTESIAN_POINT('Ctrl Pts',(-1.33410664000006,11.6,10.292521168));
#229507=CARTESIAN_POINT('Ctrl Pts',(-1.33406997000006,15.2,10.291591016));
#229508=CARTESIAN_POINT('Ctrl Pts',(-1.33406997000006,11.6,10.291591016));
#229509=CARTESIAN_POINT('Ctrl Pts',(-1.33403296600005,15.2,10.290675737));
#229510=CARTESIAN_POINT('Ctrl Pts',(-1.33403296600005,11.6,10.290675737));
#229511=CARTESIAN_POINT('Ctrl Pts',(-1.33400298800006,15.2,10.289952142));
#229512=CARTESIAN_POINT('Ctrl Pts',(-1.33400298800006,11.6,10.289952142));
#229513=CARTESIAN_POINT('Ctrl Pts',(-1.33398033300006,15.2,10.289415004));
#229514=CARTESIAN_POINT('Ctrl Pts',(-1.33398033300006,11.6,10.289415004));
#229515=CARTESIAN_POINT('Ctrl Pts',(-1.33396520800006,15.2,10.289060521));
#229516=CARTESIAN_POINT('Ctrl Pts',(-1.33396520800006,11.6,10.289060521));
#229517=CARTESIAN_POINT('Ctrl Pts',(-1.33395773200006,15.2,10.288886324));
#229518=CARTESIAN_POINT('Ctrl Pts',(-1.33395773200006,11.6,10.288886324));
#229519=CARTESIAN_POINT('',(-1.33395773266456,12.2,10.2888863233166));
#229520=CARTESIAN_POINT('',(-1.33395773266456,15.2,10.2888863233166));
#229521=CARTESIAN_POINT('',(-1.33395773300006,12.2,10.288886323));
#229522=CARTESIAN_POINT('Ctrl Pts',(-1.09337743000006,12.2,11.447904865));
#229523=CARTESIAN_POINT('Ctrl Pts',(-1.09471863524371,12.2,11.4443249343496));
#229524=CARTESIAN_POINT('Ctrl Pts',(-1.09605347736072,12.2,11.4407496840126));
#229525=CARTESIAN_POINT('Ctrl Pts',(-1.09738195536205,12.2,11.4371791166813));
#229526=CARTESIAN_POINT('Ctrl Pts',(-1.09871043336338,12.2,11.43360854935));
#229527=CARTESIAN_POINT('Ctrl Pts',(-1.10003254799348,12.2,11.4300426621214));
#229528=CARTESIAN_POINT('Ctrl Pts',(-1.10134830322047,12.2,11.4264814746557));
#229529=CARTESIAN_POINT('Ctrl Pts',(-1.10266405844746,12.2,11.42292028719));
#229530=CARTESIAN_POINT('Ctrl Pts',(-1.10397345477917,12.2,11.4193638002458));
#229531=CARTESIAN_POINT('Ctrl Pts',(-1.10527650644103,12.2,11.4158120532492));
#229532=CARTESIAN_POINT('Ctrl Pts',(-1.10657955833961,12.2,11.4122603056074));
#229533=CARTESIAN_POINT('Ctrl Pts',(-1.10787626509472,12.2,11.4087132999919));
#229534=CARTESIAN_POINT('Ctrl Pts',(-1.10916664207306,12.2,11.4051710832278));
#229535=CARTESIAN_POINT('Ctrl Pts',(-1.11088714432015,12.2,11.4004481286147));
#229536=CARTESIAN_POINT('Ctrl Pts',(-1.11259639519372,12.2,11.3957336875256));
#229537=CARTESIAN_POINT('Ctrl Pts',(-1.11429442261118,12.2,11.3910278474097));
#229538=CARTESIAN_POINT('Ctrl Pts',(-1.11556794323211,12.2,11.3874984671626));
#229539=CARTESIAN_POINT('Ctrl Pts',(-1.11683515007152,12.2,11.3839739234628));
#229540=CARTESIAN_POINT('Ctrl Pts',(-1.11809605629775,12.2,11.3804542531643));
#229541=CARTESIAN_POINT('Ctrl Pts',(-1.11935696252398,12.2,11.3769345828658));
#229542=CARTESIAN_POINT('Ctrl Pts',(-1.12061156728913,12.2,11.3734197868882));
#229543=CARTESIAN_POINT('Ctrl Pts',(-1.12185988495296,12.2,11.3699099047651));
#229544=CARTESIAN_POINT('Ctrl Pts',(-1.12310820284356,12.2,11.3664000220044));
#229545=CARTESIAN_POINT('Ctrl Pts',(-1.12435023265742,12.2,11.3628950530783));
#229546=CARTESIAN_POINT('Ctrl Pts',(-1.12558598954449,12.2,11.3593950391953));
#229547=CARTESIAN_POINT('Ctrl Pts',(-1.12682174620705,12.2,11.3558950259482));
#229548=CARTESIAN_POINT('Ctrl Pts',(-1.12805122942831,12.2,11.3523999661257));
#229549=CARTESIAN_POINT('Ctrl Pts',(-1.12927445163333,12.2,11.3489098994196));
#229550=CARTESIAN_POINT('Ctrl Pts',(-1.13049767383834,12.2,11.3454198327135));
#229551=CARTESIAN_POINT('Ctrl Pts',(-1.13171463505637,12.2,11.3419347586528));
#229552=CARTESIAN_POINT('Ctrl Pts',(-1.13292534976787,12.2,11.3384547165134));
#229553=CARTESIAN_POINT('Ctrl Pts',(-1.13413606447937,12.2,11.3349746743741));
#229554=CARTESIAN_POINT('Ctrl Pts',(-1.1353405325204,12.2,11.3314996633428));
#229555=CARTESIAN_POINT('Ctrl Pts',(-1.13653876723234,12.2,11.3280297247031));
#229556=CARTESIAN_POINT('Ctrl Pts',(-1.13773700194428,12.2,11.3245597860634));
#229557=CARTESIAN_POINT('Ctrl Pts',(-1.13892900324662,12.2,11.3210949200852));
#229558=CARTESIAN_POINT('Ctrl Pts',(-1.14011478637075,12.2,11.3176351649188));
#229559=CARTESIAN_POINT('Ctrl Pts',(-1.14130056949487,12.2,11.3141754097524));
#229560=CARTESIAN_POINT('Ctrl Pts',(-1.14248013280275,12.2,11.310720765394));
#229561=CARTESIAN_POINT('Ctrl Pts',(-1.14365349151097,12.2,11.3072712732686));
#229562=CARTESIAN_POINT('Ctrl Pts',(-1.14482685043236,12.2,11.3038217805165));
#229563=CARTESIAN_POINT('Ctrl Pts',(-1.14599400426863,12.2,11.300377439266));
#229564=CARTESIAN_POINT('Ctrl Pts',(-1.14715496772818,12.2,11.2969382899336));
#229565=CARTESIAN_POINT('Ctrl Pts',(-1.14831593097682,12.2,11.2934991412259));
#229566=CARTESIAN_POINT('Ctrl Pts',(-1.14947070470733,12.2,11.2900651829661));
#229567=CARTESIAN_POINT('Ctrl Pts',(-1.15061930151393,12.2,11.2866364571283));
#229568=CARTESIAN_POINT('Ctrl Pts',(-1.15176789832052,12.2,11.2832077312905));
#229569=CARTESIAN_POINT('Ctrl Pts',(-1.152910318299,12.2,11.2797842377195));
#229570=CARTESIAN_POINT('Ctrl Pts',(-1.15404657759052,12.2,11.2763660165941));
#229571=CARTESIAN_POINT('Ctrl Pts',(-1.15518283688203,12.2,11.2729477954687));
#229572=CARTESIAN_POINT('Ctrl Pts',(-1.15631293565759,12.2,11.2695348466262));
#229573=CARTESIAN_POINT('Ctrl Pts',(-1.1574368869501,12.2,11.2661272104999));
#229574=CARTESIAN_POINT('Ctrl Pts',(-1.15856083824261,12.2,11.2627195743737));
#229575=CARTESIAN_POINT('Ctrl Pts',(-1.15967864308535,12.2,11.2593172514973));
#229576=CARTESIAN_POINT('Ctrl Pts',(-1.16079031633716,12.2,11.255920282412));
#229577=CARTESIAN_POINT('Ctrl Pts',(-1.16190198958896,12.2,11.2525233133266));
#229578=CARTESIAN_POINT('Ctrl Pts',(-1.16300753226618,12.2,11.2491316985492));
#229579=CARTESIAN_POINT('Ctrl Pts',(-1.16410695806042,12.2,11.2457454779631));
#229580=CARTESIAN_POINT('Ctrl Pts',(-1.16520638405438,12.2,11.2423592567619));
#229581=CARTESIAN_POINT('Ctrl Pts',(-1.16629969447993,12.2,11.2389784305706));
#229582=CARTESIAN_POINT('Ctrl Pts',(-1.16738690347044,12.2,11.2356030408308));
#229583=CARTESIAN_POINT('Ctrl Pts',(-1.16847411226344,12.2,11.2322276517042));
#229584=CARTESIAN_POINT('Ctrl Pts',(-1.16955522016075,12.2,11.2288576985443));
#229585=CARTESIAN_POINT('Ctrl Pts',(-1.17063024296636,12.2,11.2254932223324));
#229586=CARTESIAN_POINT('Ctrl Pts',(-1.17170526577197,12.2,11.2221287461205));
#229587=CARTESIAN_POINT('Ctrl Pts',(-1.172774202805,12.2,11.2187697477455));
#229588=CARTESIAN_POINT('Ctrl Pts',(-1.17383707105751,12.2,11.2154162686179));
#229589=CARTESIAN_POINT('Ctrl Pts',(-1.17489993931003,12.2,11.2120627894902));
#229590=CARTESIAN_POINT('Ctrl Pts',(-1.17595673878829,12.2,11.2087148287951));
#229591=CARTESIAN_POINT('Ctrl Pts',(-1.1770074840001,12.2,11.2053724292083));
#229592=CARTESIAN_POINT('Ctrl Pts',(-1.17805822921191,12.2,11.2020300296214));
#229593=CARTESIAN_POINT('Ctrl Pts',(-1.17910291997399,12.2,11.1986931913926));
#229594=CARTESIAN_POINT('Ctrl Pts',(-1.18014157464512,12.2,11.1953619553465));
#229595=CARTESIAN_POINT('Ctrl Pts',(-1.18118022931625,12.2,11.1920307193003));
#229596=CARTESIAN_POINT('Ctrl Pts',(-1.18221284635339,12.2,11.1887050868382));
#229597=CARTESIAN_POINT('Ctrl Pts',(-1.18323944307642,12.2,11.1853850986257));
#229598=CARTESIAN_POINT('Ctrl Pts',(-1.18426603979944,12.2,11.1820651104131));
#229599=CARTESIAN_POINT('Ctrl Pts',(-1.18528661428163,12.2,11.1787507677518));
#229600=CARTESIAN_POINT('Ctrl Pts',(-1.18630118503725,12.2,11.1754421117046));
#229601=CARTESIAN_POINT('Ctrl Pts',(-1.18731575597719,12.2,11.1721334550563));
#229602=CARTESIAN_POINT('Ctrl Pts',(-1.18832432250709,12.2,11.1688304856929));
#229603=CARTESIAN_POINT('Ctrl Pts',(-1.18932690144366,12.2,11.1655332465062));
#229604=CARTESIAN_POINT('Ctrl Pts',(-1.19066367305552,12.2,11.1611369285888));
#229605=CARTESIAN_POINT('Ctrl Pts',(-1.19198979991875,12.2,11.1567507967868));
#229606=CARTESIAN_POINT('Ctrl Pts',(-1.19330532220079,12.2,11.1523749528661));
#229607=CARTESIAN_POINT('Ctrl Pts',(-1.19429196395713,12.2,11.1490930697765));
#229608=CARTESIAN_POINT('Ctrl Pts',(-1.19527263971414,12.2,11.1458169740446));
#229609=CARTESIAN_POINT('Ctrl Pts',(-1.19624736856145,12.2,11.1425467073744));
#229610=CARTESIAN_POINT('Ctrl Pts',(-1.19722209740877,12.2,11.1392764407041));
#229611=CARTESIAN_POINT('Ctrl Pts',(-1.1981908789577,12.2,11.136012004776));
#229612=CARTESIAN_POINT('Ctrl Pts',(-1.19915372929852,12.2,11.1327534416853));
#229613=CARTESIAN_POINT('Ctrl Pts',(-1.20011657981426,12.2,11.1294948780026));
#229614=CARTESIAN_POINT('Ctrl Pts',(-1.20107350023667,12.2,11.1262421870632));
#229615=CARTESIAN_POINT('Ctrl Pts',(-1.2020245077074,12.2,11.1229954133005));
#229616=CARTESIAN_POINT('Ctrl Pts',(-1.20297551500537,12.2,11.1197486401276));
#229617=CARTESIAN_POINT('Ctrl Pts',(-1.20392060930367,12.2,11.1165077822794));
#229618=CARTESIAN_POINT('Ctrl Pts',(-1.20485980860238,12.2,11.1132728861474));
#229619=CARTESIAN_POINT('Ctrl Pts',(-1.20579900790108,12.2,11.1100379900154));
#229620=CARTESIAN_POINT('Ctrl Pts',(-1.20673231228045,12.2,11.1068090546445));
#229621=CARTESIAN_POINT('Ctrl Pts',(-1.20765974050094,12.2,11.103586122497));
#229622=CARTESIAN_POINT('Ctrl Pts',(-1.20858716872143,12.2,11.1003631903495));
#229623=CARTESIAN_POINT('Ctrl Pts',(-1.20950871892835,12.2,11.0971462604508));
#229624=CARTESIAN_POINT('Ctrl Pts',(-1.2104244107326,12.2,11.0939353808029));
#229625=CARTESIAN_POINT('Ctrl Pts',(-1.21164533324916,12.2,11.0896542075501));
#229626=CARTESIAN_POINT('Ctrl Pts',(-1.21285584092362,12.2,11.0853837859207));
#229627=CARTESIAN_POINT('Ctrl Pts',(-1.21405597615465,12.2,11.0811242220785));
#229628=CARTESIAN_POINT('Ctrl Pts',(-1.21525611122216,12.2,11.0768646588167));
#229629=CARTESIAN_POINT('Ctrl Pts',(-1.21644587504099,12.2,11.0726159532591));
#229630=CARTESIAN_POINT('Ctrl Pts',(-1.21762531144525,12.2,11.0683782101048));
#229631=CARTESIAN_POINT('Ctrl Pts',(-1.2188047480102,12.2,11.0641404663731));
#229632=CARTESIAN_POINT('Ctrl Pts',(-1.21997385755081,12.2,11.0599136871388));
#229633=CARTESIAN_POINT('Ctrl Pts',(-1.22113268539319,12.2,11.0556979759216));
#229634=CARTESIAN_POINT('Ctrl Pts',(-1.22229151307767,12.2,11.0514822652789));
#229635=CARTESIAN_POINT('Ctrl Pts',(-1.22344005731877,12.2,11.0472776253702));
#229636=CARTESIAN_POINT('Ctrl Pts',(-1.22457836761528,12.2,11.0430841621012));
#229637=CARTESIAN_POINT('Ctrl Pts',(-1.22600125560224,12.2,11.0378423325863));
#229638=CARTESIAN_POINT('Ctrl Pts',(-1.22740814918597,12.2,11.032617965736));
#229639=CARTESIAN_POINT('Ctrl Pts',(-1.22879913911737,12.2,11.0274112746239));
#229640=CARTESIAN_POINT('Ctrl Pts',(-1.22991193112313,12.2,11.0232459215072));
#229641=CARTESIAN_POINT('Ctrl Pts',(-1.23101454713699,12.2,11.0190918803584));
#229642=CARTESIAN_POINT('Ctrl Pts',(-1.2321070324169,12.2,11.0149492591489));
#229643=CARTESIAN_POINT('Ctrl Pts',(-1.23319951754795,12.2,11.0108066385038));
#229644=CARTESIAN_POINT('Ctrl Pts',(-1.23428187275489,12.2,11.0066754396731));
#229645=CARTESIAN_POINT('Ctrl Pts',(-1.23535414644568,12.2,11.0025557711202));
#229646=CARTESIAN_POINT('Ctrl Pts',(-1.23669448866874,12.2,10.9974061850081));
#229647=CARTESIAN_POINT('Ctrl Pts',(-1.23801907659135,12.2,10.9922746139299));
#229648=CARTESIAN_POINT('Ctrl Pts',(-1.23932800964773,12.2,10.9871612753178));
#229649=CARTESIAN_POINT('Ctrl Pts',(-1.24063694270411,12.2,10.9820479367057));
#229650=CARTESIAN_POINT('Ctrl Pts',(-1.24193021764355,12.2,10.9769528289092));
#229651=CARTESIAN_POINT('Ctrl Pts',(-1.24320793494107,12.2,10.971876172011));
#229652=CARTESIAN_POINT('Ctrl Pts',(-1.24423010883479,12.2,10.9678148462712));
#229653=CARTESIAN_POINT('Ctrl Pts',(-1.24524232497424,12.2,10.963765328567));
#229654=CARTESIAN_POINT('Ctrl Pts',(-1.24624463363897,12.2,10.9597277308481));
#229655=CARTESIAN_POINT('Ctrl Pts',(-1.24724694216714,12.2,10.9556901336794));
#229656=CARTESIAN_POINT('Ctrl Pts',(-1.2482393453438,12.2,10.9516644556897));
#229657=CARTESIAN_POINT('Ctrl Pts',(-1.24922189315301,12.2,10.9476508117948));
#229658=CARTESIAN_POINT('Ctrl Pts',(-1.25020444109609,12.2,10.9436371673531));
#229659=CARTESIAN_POINT('Ctrl Pts',(-1.25117713392891,12.2,10.9396355560951));
#229660=CARTESIAN_POINT('Ctrl Pts',(-1.25214002513976,12.2,10.9356460921794));
#229661=CARTESIAN_POINT('Ctrl Pts',(-1.25334363908772,12.2,10.9306592625566));
#229662=CARTESIAN_POINT('Ctrl Pts',(-1.25453193648254,12.2,10.9256914133845));
#229663=CARTESIAN_POINT('Ctrl Pts',(-1.25570502141186,12.2,10.920742768386));
#229664=CARTESIAN_POINT('Ctrl Pts',(-1.25664348927859,12.2,10.9167838527109));
#229665=CARTESIAN_POINT('Ctrl Pts',(-1.25757222326605,12.2,10.9128372283619));
#229666=CARTESIAN_POINT('Ctrl Pts',(-1.25849127519153,12.2,10.9089030105717));
#229667=CARTESIAN_POINT('Ctrl Pts',(-1.25941032724225,12.2,10.9049687922454));
#229668=CARTESIAN_POINT('Ctrl Pts',(-1.26031969870015,12.2,10.9010469802483));
#229669=CARTESIAN_POINT('Ctrl Pts',(-1.26121944458189,12.2,10.8971376931471));
#229670=CARTESIAN_POINT('Ctrl Pts',(-1.26211919034104,12.2,10.8932284065787));
#229671=CARTESIAN_POINT('Ctrl Pts',(-1.26300931043274,12.2,10.8893316419135));
#229672=CARTESIAN_POINT('Ctrl Pts',(-1.2638898604056,12.2,10.8854475198136));
#229673=CARTESIAN_POINT('Ctrl Pts',(-1.26499054796166,12.2,10.8805923667918));
#229674=CARTESIAN_POINT('Ctrl Pts',(-1.26607628520143,12.2,10.8757569651993));
#229675=CARTESIAN_POINT('Ctrl Pts',(-1.2671471794383,12.2,10.8709415483233));
#229676=CARTESIAN_POINT('Ctrl Pts',(-1.26821807367517,12.2,10.8661261314473));
#229677=CARTESIAN_POINT('Ctrl Pts',(-1.26927412805335,12.2,10.8613306965301));
#229678=CARTESIAN_POINT('Ctrl Pts',(-1.27031545541524,12.2,10.8565554813207));
#229679=CARTESIAN_POINT('Ctrl Pts',(-1.27114851735014,12.2,10.852735308945));
#229680=CARTESIAN_POINT('Ctrl Pts',(-1.27197215285895,12.2,10.8489280748891));
#229681=CARTESIAN_POINT('Ctrl Pts',(-1.27278642410986,12.2,10.8451339017161));
#229682=CARTESIAN_POINT('Ctrl Pts',(-1.27360069524983,12.2,10.8413397290601));
#229683=CARTESIAN_POINT('Ctrl Pts',(-1.27440559906606,12.2,10.8375586166981));
#229684=CARTESIAN_POINT('Ctrl Pts',(-1.2752011976683,12.2,10.8337906862831));
#229685=CARTESIAN_POINT('Ctrl Pts',(-1.27599679637893,12.2,10.8300227553547));
#229686=CARTESIAN_POINT('Ctrl Pts',(-1.27678308949955,12.2,10.8262680065445));
#229687=CARTESIAN_POINT('Ctrl Pts',(-1.27756013809686,12.2,10.8225265629525));
#229688=CARTESIAN_POINT('Ctrl Pts',(-1.2783371865883,12.2,10.8187851198703));
#229689=CARTESIAN_POINT('Ctrl Pts',(-1.27910499036327,12.2,10.8150569812055));
#229690=CARTESIAN_POINT('Ctrl Pts',(-1.2798636116733,12.2,10.8113422713224));
#229691=CARTESIAN_POINT('Ctrl Pts',(-1.28062223308668,12.2,10.8076275609331));
#229692=CARTESIAN_POINT('Ctrl Pts',(-1.28137167168744,12.2,10.8039262793042));
#229693=CARTESIAN_POINT('Ctrl Pts',(-1.28211199106053,12.2,10.8002385522153));
#229694=CARTESIAN_POINT('Ctrl Pts',(-1.28285231033274,12.2,10.7965508256287));
#229695=CARTESIAN_POINT('Ctrl Pts',(-1.28358351027346,12.2,10.7928766510173));
#229696=CARTESIAN_POINT('Ctrl Pts',(-1.28430565488202,12.2,10.7892161566484));
#229697=CARTESIAN_POINT('Ctrl Pts',(-1.28502779958897,12.2,10.7855556617808));
#229698=CARTESIAN_POINT('Ctrl Pts',(-1.28574088813958,12.2,10.7819088460286));
#229699=CARTESIAN_POINT('Ctrl Pts',(-1.2864449874589,12.2,10.7782758364808));
#229700=CARTESIAN_POINT('Ctrl Pts',(-1.28714908668229,12.2,10.774642827428));
#229701=CARTESIAN_POINT('Ctrl Pts',(-1.28784419548474,12.2,10.7710236250016));
#229702=CARTESIAN_POINT('Ctrl Pts',(-1.28853037959623,12.2,10.7674183560727));
#229703=CARTESIAN_POINT('Ctrl Pts',(-1.28921656380121,12.2,10.7638130866526));
#229704=CARTESIAN_POINT('Ctrl Pts',(-1.28989382509978,12.2,10.7602217522449));
#229705=CARTESIAN_POINT('Ctrl Pts',(-1.29056222852509,12.2,10.7566444807166));
#229706=CARTESIAN_POINT('Ctrl Pts',(-1.29123063195041,12.2,10.7530672091883));
#229707=CARTESIAN_POINT('Ctrl Pts',(-1.29189017847469,12.2,10.749504000795));
#229708=CARTESIAN_POINT('Ctrl Pts',(-1.29254093589815,12.2,10.7459549859363));
#229709=CARTESIAN_POINT('Ctrl Pts',(-1.29319169323294,12.2,10.7424059715613));
#229710=CARTESIAN_POINT('Ctrl Pts',(-1.29383366238463,12.2,10.73887115));
#229711=CARTESIAN_POINT('Ctrl Pts',(-1.29446691172466,12.2,10.735350652994));
#229712=CARTESIAN_POINT('Ctrl Pts',(-1.29510016115096,12.2,10.7318301555083));
#229713=CARTESIAN_POINT('Ctrl Pts',(-1.29572469080421,12.2,10.7283239839262));
#229714=CARTESIAN_POINT('Ctrl Pts',(-1.29634057155912,12.2,10.724832267904));
#229715=CARTESIAN_POINT('Ctrl Pts',(-1.29695645223011,12.2,10.7213405523576));
#229716=CARTESIAN_POINT('Ctrl Pts',(-1.29756368437444,12.2,10.7178632948732));
#229717=CARTESIAN_POINT('Ctrl Pts',(-1.29816233849274,12.2,10.7144006272665));
#229718=CARTESIAN_POINT('Ctrl Pts',(-1.29876099269259,12.2,10.7109379591879));
#229719=CARTESIAN_POINT('Ctrl Pts',(-1.29935106954665,12.2,10.7074898826341));
#229720=CARTESIAN_POINT('Ctrl Pts',(-1.2999326410511,12.2,10.7040565297768));
#229721=CARTESIAN_POINT('Ctrl Pts',(-1.30051421247631,12.2,10.7006231773873));
#229722=CARTESIAN_POINT('Ctrl Pts',(-1.30108727996058,12.2,10.6972045521927));
#229723=CARTESIAN_POINT('Ctrl Pts',(-1.30165191547052,12.2,10.6938007873033));
#229724=CARTESIAN_POINT('Ctrl Pts',(-1.30235770991564,12.2,10.6895460808438));
#229725=CARTESIAN_POINT('Ctrl Pts',(-1.30305033114932,12.2,10.6853145958265));
#229726=CARTESIAN_POINT('Ctrl Pts',(-1.30372992545557,12.2,10.6811065985336));
#229727=CARTESIAN_POINT('Ctrl Pts',(-1.30440951976181,12.2,10.6768986012407));
#229728=CARTESIAN_POINT('Ctrl Pts',(-1.30507608706339,12.2,10.6727140939934));
#229729=CARTESIAN_POINT('Ctrl Pts',(-1.30572977727473,12.2,10.6685533467522));
#229730=CARTESIAN_POINT('Ctrl Pts',(-1.3062527294723,12.2,10.6652247487778));
#229731=CARTESIAN_POINT('Ctrl Pts',(-1.3067674410339,12.2,10.661911358125));
#229732=CARTESIAN_POINT('Ctrl Pts',(-1.30727398861624,12.2,10.658613314669));
#229733=CARTESIAN_POINT('Ctrl Pts',(-1.30790717305964,12.2,10.6544907605738));
#229734=CARTESIAN_POINT('Ctrl Pts',(-1.30852760265283,12.2,10.650392185554));
#229735=CARTESIAN_POINT('Ctrl Pts',(-1.30913543209625,12.2,10.6463178689587));
#229736=CARTESIAN_POINT('Ctrl Pts',(-1.30974326147342,12.2,10.6422435528075));
#229737=CARTESIAN_POINT('Ctrl Pts',(-1.31033849264746,12.2,10.6381934920898));
#229738=CARTESIAN_POINT('Ctrl Pts',(-1.31092128043219,12.2,10.6341679702348));
#229739=CARTESIAN_POINT('Ctrl Pts',(-1.31150406828044,12.2,10.630142447941));
#229740=CARTESIAN_POINT('Ctrl Pts',(-1.31207441624275,12.2,10.6261414635832));
#229741=CARTESIAN_POINT('Ctrl Pts',(-1.31263248395209,12.2,10.62216530122));
#229742=CARTESIAN_POINT('Ctrl Pts',(-1.31319055166142,12.2,10.6181891388569));
#229743=CARTESIAN_POINT('Ctrl Pts',(-1.31373633861817,12.2,10.6142377984822));
#229744=CARTESIAN_POINT('Ctrl Pts',(-1.31427001139695,12.2,10.6103115670218));
#229745=CARTESIAN_POINT('Ctrl Pts',(-1.31480368417572,12.2,10.6063853355614));
#229746=CARTESIAN_POINT('Ctrl Pts',(-1.31532524223126,12.2,10.6024842140231));
#229747=CARTESIAN_POINT('Ctrl Pts',(-1.31583485496588,12.2,10.5986084916749));
#229748=CARTESIAN_POINT('Ctrl Pts',(-1.31634446770052,12.2,10.5947327693267));
#229749=CARTESIAN_POINT('Ctrl Pts',(-1.31684213243429,12.2,10.590882448546));
#229750=CARTESIAN_POINT('Ctrl Pts',(-1.31732802347657,12.2,10.5870578222252));
#229751=CARTESIAN_POINT('Ctrl Pts',(-1.31781391451885,12.2,10.5832331959044));
#229752=CARTESIAN_POINT('Ctrl Pts',(-1.31828803065249,12.2,10.5794342661427));
#229753=CARTESIAN_POINT('Ctrl Pts',(-1.31875054919477,12.2,10.5756613289885));
#229754=CARTESIAN_POINT('Ctrl Pts',(-1.31939807516404,12.2,10.5703792168904));
#229755=CARTESIAN_POINT('Ctrl Pts',(-1.32002286524739,12.2,10.5651480526702));
#229756=CARTESIAN_POINT('Ctrl Pts',(-1.32062541426983,12.2,10.5599686680081));
#229757=CARTESIAN_POINT('Ctrl Pts',(-1.32105580642201,12.2,10.5562691075929));
#229758=CARTESIAN_POINT('Ctrl Pts',(-1.32147485166617,12.2,10.5525959663213));
#229759=CARTESIAN_POINT('Ctrl Pts',(-1.32188273527669,12.2,10.5489495525033));
#229760=CARTESIAN_POINT('Ctrl Pts',(-1.32229061888722,12.2,10.5453031386853));
#229761=CARTESIAN_POINT('Ctrl Pts',(-1.32268733927631,12.2,10.5416834501495));
#229762=CARTESIAN_POINT('Ctrl Pts',(-1.32307308554482,12.2,10.5380908012913));
#229763=CARTESIAN_POINT('Ctrl Pts',(-1.32345883181334,12.2,10.5344981524331));
#229764=CARTESIAN_POINT('Ctrl Pts',(-1.3238336034319,12.2,10.5309325439349));
#229765=CARTESIAN_POINT('Ctrl Pts',(-1.32419759384769,12.2,10.5273942910204));
#229766=CARTESIAN_POINT('Ctrl Pts',(-1.32463438233077,12.2,10.5231483876774));
#229767=CARTESIAN_POINT('Ctrl Pts',(-1.32505564512154,12.2,10.5189418766988));
#229768=CARTESIAN_POINT('Ctrl Pts',(-1.32546172169193,12.2,10.514775313498));
#229769=CARTESIAN_POINT('Ctrl Pts',(-1.32580011884622,12.2,10.5113031773712));
#229770=CARTESIAN_POINT('Ctrl Pts',(-1.32612797098799,12.2,10.5078587827475));
#229771=CARTESIAN_POINT('Ctrl Pts',(-1.32644547973745,12.2,10.504442458235));
#229772=CARTESIAN_POINT('Ctrl Pts',(-1.32676298848692,12.2,10.5010261337225));
#229773=CARTESIAN_POINT('Ctrl Pts',(-1.32707015254776,12.2,10.49763787689));
#229774=CARTESIAN_POINT('Ctrl Pts',(-1.32736717976944,12.2,10.4942780207804));
#229775=CARTESIAN_POINT('Ctrl Pts',(-1.32766420699113,12.2,10.4909181646708));
#229776=CARTESIAN_POINT('Ctrl Pts',(-1.3279510955246,12.2,10.4875867077685));
#229777=CARTESIAN_POINT('Ctrl Pts',(-1.32822805852386,12.2,10.4842839880916));
#229778=CARTESIAN_POINT('Ctrl Pts',(-1.3285604141109,12.2,10.4803207246233));
#229779=CARTESIAN_POINT('Ctrl Pts',(-1.32887847294447,12.2,10.4763988409589));
#229780=CARTESIAN_POINT('Ctrl Pts',(-1.32918260976675,12.2,10.4725189287666));
#229781=CARTESIAN_POINT('Ctrl Pts',(-1.32948674658902,12.2,10.4686390165743));
#229782=CARTESIAN_POINT('Ctrl Pts',(-1.32977696181039,12.2,10.464801074663));
#229783=CARTESIAN_POINT('Ctrl Pts',(-1.33005363673162,12.2,10.4610057053588));
#229784=CARTESIAN_POINT('Ctrl Pts',(-1.33033031167796,12.2,10.4572103357099));
#229785=CARTESIAN_POINT('Ctrl Pts',(-1.33059344552293,12.2,10.4534575391531));
#229786=CARTESIAN_POINT('Ctrl Pts',(-1.33084343428566,12.2,10.4497479268706));
#229787=CARTESIAN_POINT('Ctrl Pts',(-1.33109342302568,12.2,10.446038314925));
#229788=CARTESIAN_POINT('Ctrl Pts',(-1.33133026600734,12.2,10.4423718899996));
#229789=CARTESIAN_POINT('Ctrl Pts',(-1.33155436400018,12.2,10.4387492722816));
#229790=CARTESIAN_POINT('Ctrl Pts',(-1.33177846199302,12.2,10.4351266545636));
#229791=CARTESIAN_POINT('Ctrl Pts',(-1.33198981800421,12.2,10.4315478490662));
#229792=CARTESIAN_POINT('Ctrl Pts',(-1.33218884591418,12.2,10.4280134881927));
#229793=CARTESIAN_POINT('Ctrl Pts',(-1.33238787384223,12.2,10.4244791269982));
#229794=CARTESIAN_POINT('Ctrl Pts',(-1.33257457402707,12.2,10.4209892126675));
#229795=CARTESIAN_POINT('Ctrl Pts',(-1.33274937203579,12.2,10.4175443943994));
#229796=CARTESIAN_POINT('Ctrl Pts',(-1.33295330302215,12.2,10.4135254402227));
#229797=CARTESIAN_POINT('Ctrl Pts',(-1.33314103521879,12.2,10.4095678640141));
#229798=CARTESIAN_POINT('Ctrl Pts',(-1.33331326350032,12.2,10.4056727214487));
#229799=CARTESIAN_POINT('Ctrl Pts',(-1.33346088775886,12.2,10.4023340274313));
#229800=CARTESIAN_POINT('Ctrl Pts',(-1.33359712441598,12.2,10.3990412041531));
#229801=CARTESIAN_POINT('Ctrl Pts',(-1.3337224245054,12.2,10.3957949291461));
#229802=CARTESIAN_POINT('Ctrl Pts',(-1.33384772458343,12.2,10.3925486544339));
#229803=CARTESIAN_POINT('Ctrl Pts',(-1.33396208837012,12.2,10.3893489273564));
#229804=CARTESIAN_POINT('Ctrl Pts',(-1.33406598253345,12.2,10.3861964417068));
#229805=CARTESIAN_POINT('Ctrl Pts',(-1.33416987669679,12.2,10.3830439560572));
#229806=CARTESIAN_POINT('Ctrl Pts',(-1.33426330155641,12.2,10.3799387105827));
#229807=CARTESIAN_POINT('Ctrl Pts',(-1.33434673397048,12.2,10.3768814149417));
#229808=CARTESIAN_POINT('Ctrl Pts',(-1.33443016639213,12.2,10.373824119023));
#229809=CARTESIAN_POINT('Ctrl Pts',(-1.33450360979587,12.2,10.370814770902));
#229810=CARTESIAN_POINT('Ctrl Pts',(-1.33456755604871,12.2,10.3678540969105));
#229811=CARTESIAN_POINT('Ctrl Pts',(-1.33463150229574,12.2,10.364893423188));
#229812=CARTESIAN_POINT('Ctrl Pts',(-1.33468595109622,12.2,10.3619814201713));
#229813=CARTESIAN_POINT('Ctrl Pts',(-1.33473141151084,12.2,10.3591188306107));
#229814=CARTESIAN_POINT('Ctrl Pts',(-1.33477687192547,12.2,10.3562562410502));
#229815=CARTESIAN_POINT('Ctrl Pts',(-1.33481334458249,12.2,10.3534430629109));
#229816=CARTESIAN_POINT('Ctrl Pts',(-1.33484135024851,12.2,10.3506800554257));
#229817=CARTESIAN_POINT('Ctrl Pts',(-1.33486935591453,12.2,10.3479170479405));
#229818=CARTESIAN_POINT('Ctrl Pts',(-1.33488889886535,12.2,10.3452042081885));
#229819=CARTESIAN_POINT('Ctrl Pts',(-1.33490051353214,12.2,10.3425423130317));
#229820=CARTESIAN_POINT('Ctrl Pts',(-1.33491212819997,12.2,10.3398804176332));
#229821=CARTESIAN_POINT('Ctrl Pts',(-1.33491581895869,12.2,10.3372694662229));
#229822=CARTESIAN_POINT('Ctrl Pts',(-1.3349121395415,12.2,10.3347102518356));
#229823=CARTESIAN_POINT('Ctrl Pts',(-1.33490846012465,12.2,10.3321510376808));
#229824=CARTESIAN_POINT('Ctrl Pts',(-1.33489741019116,12.2,10.3296435610064));
#229825=CARTESIAN_POINT('Ctrl Pts',(-1.33487956577508,12.2,10.327188635751));
#229826=CARTESIAN_POINT('Ctrl Pts',(-1.33486172135899,12.2,10.3247337104956));
#229827=CARTESIAN_POINT('Ctrl Pts',(-1.33483707968522,12.2,10.3223313361492));
#229828=CARTESIAN_POINT('Ctrl Pts',(-1.33480623452009,12.2,10.3199823443143));
#229829=CARTESIAN_POINT('Ctrl Pts',(-1.33477538935217,12.2,10.317633352266));
#229830=CARTESIAN_POINT('Ctrl Pts',(-1.3347383410007,12.2,10.3153377453225));
#229831=CARTESIAN_POINT('Ctrl Pts',(-1.33469569799593,12.2,10.3130963780082));
#229832=CARTESIAN_POINT('Ctrl Pts',(-1.33465305499502,12.2,10.3108550108975));
#229833=CARTESIAN_POINT('Ctrl Pts',(-1.33460481848147,12.2,10.3086678827224));
#229834=CARTESIAN_POINT('Ctrl Pts',(-1.3345516194834,12.2,10.3065358709665));
#229835=CARTESIAN_POINT('Ctrl Pts',(-1.33449842048533,12.2,10.3044038592106));
#229836=CARTESIAN_POINT('Ctrl Pts',(-1.33444025941503,12.2,10.3023269653096));
#229837=CARTESIAN_POINT('Ctrl Pts',(-1.33437778649776,12.2,10.3003060904455));
#229838=CARTESIAN_POINT('Ctrl Pts',(-1.33431531357482,12.2,10.2982852153979));
#229839=CARTESIAN_POINT('Ctrl Pts',(-1.33424852863814,12.2,10.2963203589004));
#229840=CARTESIAN_POINT('Ctrl Pts',(-1.33417810671739,12.2,10.2944124472169));
#229841=CARTESIAN_POINT('Ctrl Pts',(-1.33410802277682,12.2,10.2925136922895));
#229842=CARTESIAN_POINT('Ctrl Pts',(-1.33403433934042,12.2,10.2906713385628));
#229843=CARTESIAN_POINT('Ctrl Pts',(-1.33395773200006,12.2,10.288886324));
#229844=CARTESIAN_POINT('Ctrl Pts',(-1.33395773200006,15.2,10.288886324));
#229845=CARTESIAN_POINT('Ctrl Pts',(-1.33403433934042,15.2,10.2906713385628));
#229846=CARTESIAN_POINT('Ctrl Pts',(-1.33410802277682,15.2,10.2925136922895));
#229847=CARTESIAN_POINT('Ctrl Pts',(-1.33417810671739,15.2,10.2944124472169));
#229848=CARTESIAN_POINT('Ctrl Pts',(-1.33424852863814,15.2,10.2963203589004));
#229849=CARTESIAN_POINT('Ctrl Pts',(-1.33431531357482,15.2,10.2982852153978));
#229850=CARTESIAN_POINT('Ctrl Pts',(-1.33437778649776,15.2,10.3003060904455));
#229851=CARTESIAN_POINT('Ctrl Pts',(-1.33444025941503,15.2,10.3023269653096));
#229852=CARTESIAN_POINT('Ctrl Pts',(-1.33449842048533,15.2,10.3044038592107));
#229853=CARTESIAN_POINT('Ctrl Pts',(-1.3345516194834,15.2,10.3065358709666));
#229854=CARTESIAN_POINT('Ctrl Pts',(-1.33460481848146,15.2,10.3086678827224));
#229855=CARTESIAN_POINT('Ctrl Pts',(-1.33465305499502,15.2,10.3108550108974));
#229856=CARTESIAN_POINT('Ctrl Pts',(-1.33469569799593,15.2,10.3130963780082));
#229857=CARTESIAN_POINT('Ctrl Pts',(-1.3347383410007,15.2,10.3153377453225));
#229858=CARTESIAN_POINT('Ctrl Pts',(-1.33477538935217,15.2,10.317633352266));
#229859=CARTESIAN_POINT('Ctrl Pts',(-1.33480623452009,15.2,10.3199823443143));
#229860=CARTESIAN_POINT('Ctrl Pts',(-1.33483707968522,15.2,10.3223313361492));
#229861=CARTESIAN_POINT('Ctrl Pts',(-1.33486172135899,15.2,10.3247337104956));
#229862=CARTESIAN_POINT('Ctrl Pts',(-1.33487956577508,15.2,10.327188635751));
#229863=CARTESIAN_POINT('Ctrl Pts',(-1.33489741019116,15.2,10.3296435610064));
#229864=CARTESIAN_POINT('Ctrl Pts',(-1.33490846012465,15.2,10.3321510376809));
#229865=CARTESIAN_POINT('Ctrl Pts',(-1.3349121395415,15.2,10.3347102518356));
#229866=CARTESIAN_POINT('Ctrl Pts',(-1.33491581895869,15.2,10.3372694662229));
#229867=CARTESIAN_POINT('Ctrl Pts',(-1.33491212819997,15.2,10.3398804176332));
#229868=CARTESIAN_POINT('Ctrl Pts',(-1.33490051353214,15.2,10.3425423130317));
#229869=CARTESIAN_POINT('Ctrl Pts',(-1.33488889886535,15.2,10.3452042081885));
#229870=CARTESIAN_POINT('Ctrl Pts',(-1.33486935591453,15.2,10.3479170479406));
#229871=CARTESIAN_POINT('Ctrl Pts',(-1.33484135024851,15.2,10.3506800554257));
#229872=CARTESIAN_POINT('Ctrl Pts',(-1.33481334458249,15.2,10.3534430629108));
#229873=CARTESIAN_POINT('Ctrl Pts',(-1.33477687192547,15.2,10.3562562410502));
#229874=CARTESIAN_POINT('Ctrl Pts',(-1.33473141151084,15.2,10.3591188306108));
#229875=CARTESIAN_POINT('Ctrl Pts',(-1.33468595109622,15.2,10.3619814201713));
#229876=CARTESIAN_POINT('Ctrl Pts',(-1.33463150229574,15.2,10.3648934231881));
#229877=CARTESIAN_POINT('Ctrl Pts',(-1.33456755604871,15.2,10.3678540969105));
#229878=CARTESIAN_POINT('Ctrl Pts',(-1.33448229437826,15.2,10.3718016622324));
#229879=CARTESIAN_POINT('Ctrl Pts',(-1.33438015033105,15.2,10.3758357563356));
#229880=CARTESIAN_POINT('Ctrl Pts',(-1.33425995299025,15.2,10.37995466812));
#229881=CARTESIAN_POINT('Ctrl Pts',(-1.33415478032932,15.2,10.3835587155104));
#229882=CARTESIAN_POINT('Ctrl Pts',(-1.33403579119185,15.2,10.3872277021273));
#229883=CARTESIAN_POINT('Ctrl Pts',(-1.33390223100627,15.2,10.3909605146007));
#229884=CARTESIAN_POINT('Ctrl Pts',(-1.33378775083383,15.2,10.3941600685231));
#229885=CARTESIAN_POINT('Ctrl Pts',(-1.33366256536007,15.2,10.3974065145429));
#229886=CARTESIAN_POINT('Ctrl Pts',(-1.33352621618521,15.2,10.4006991693921));
#229887=CARTESIAN_POINT('Ctrl Pts',(-1.33336714216645,15.2,10.404540599601));
#229888=CARTESIAN_POINT('Ctrl Pts',(-1.33319287180157,15.2,10.4084449208732));
#229889=CARTESIAN_POINT('Ctrl Pts',(-1.33300269804082,15.2,10.4124110706545));
#229890=CARTESIAN_POINT('Ctrl Pts',(-1.33283969194114,15.2,10.4158106280069));
#229891=CARTESIAN_POINT('Ctrl Pts',(-1.33266500207405,15.2,10.4192556114537));
#229892=CARTESIAN_POINT('Ctrl Pts',(-1.33247819522971,15.2,10.422745363647));
#229893=CARTESIAN_POINT('Ctrl Pts',(-1.33229138840234,15.2,10.4262351155232));
#229894=CARTESIAN_POINT('Ctrl Pts',(-1.33209246643496,15.2,10.4297696369234));
#229895=CARTESIAN_POINT('Ctrl Pts',(-1.33188100652498,15.2,10.4333482847265));
#229896=CARTESIAN_POINT('Ctrl Pts',(-1.33163430328387,15.2,10.4375233740468));
#229897=CARTESIAN_POINT('Ctrl Pts',(-1.3313705361403,15.2,10.4417585233586));
#229898=CARTESIAN_POINT('Ctrl Pts',(-1.33108905573211,15.2,10.4460527341928));
#229899=CARTESIAN_POINT('Ctrl Pts',(-1.33080757534583,15.2,10.4503469446927));
#229900=CARTESIAN_POINT('Ctrl Pts',(-1.3305083827271,15.2,10.4547002160138));
#229901=CARTESIAN_POINT('Ctrl Pts',(-1.33019084775971,15.2,10.4591115706509));
#229902=CARTESIAN_POINT('Ctrl Pts',(-1.32991867489873,15.2,10.46289273221));
#229903=CARTESIAN_POINT('Ctrl Pts',(-1.32963302655136,15.2,10.4667165679494));
#229904=CARTESIAN_POINT('Ctrl Pts',(-1.32933351970076,15.2,10.470582473413));
#229905=CARTESIAN_POINT('Ctrl Pts',(-1.32903401287737,15.2,10.4744483785254));
#229906=CARTESIAN_POINT('Ctrl Pts',(-1.32872064742288,15.2,10.4783563548272));
#229907=CARTESIAN_POINT('Ctrl Pts',(-1.3283930467666,15.2,10.4823058080351));
#229908=CARTESIAN_POINT('Ctrl Pts',(-1.32784704565295,15.2,10.4888882302873));
#229909=CARTESIAN_POINT('Ctrl Pts',(-1.32726150468059,15.2,10.4955858675033));
#229910=CARTESIAN_POINT('Ctrl Pts',(-1.32663474551286,15.2,10.5023960350061));
#229911=CARTESIAN_POINT('Ctrl Pts',(-1.32632136592899,15.2,10.5058011187576));
#229912=CARTESIAN_POINT('Ctrl Pts',(-1.32599768351757,15.2,10.509234337538));
#229913=CARTESIAN_POINT('Ctrl Pts',(-1.32566349627792,15.2,10.5126953638935));
#229914=CARTESIAN_POINT('Ctrl Pts',(-1.32519563417155,15.2,10.5175408004892));
#229915=CARTESIAN_POINT('Ctrl Pts',(-1.32470718039805,15.2,10.5224407372488));
#229916=CARTESIAN_POINT('Ctrl Pts',(-1.32419759384769,15.2,10.5273942910205));
#229917=CARTESIAN_POINT('Ctrl Pts',(-1.32383360343191,15.2,10.5309325439348));
#229918=CARTESIAN_POINT('Ctrl Pts',(-1.32345883181334,15.2,10.5344981524331));
#229919=CARTESIAN_POINT('Ctrl Pts',(-1.32307308554483,15.2,10.5380908012913));
#229920=CARTESIAN_POINT('Ctrl Pts',(-1.32268733927631,15.2,10.5416834501495));
#229921=CARTESIAN_POINT('Ctrl Pts',(-1.32229061888723,15.2,10.5453031386852));
#229922=CARTESIAN_POINT('Ctrl Pts',(-1.32188273527669,15.2,10.5489495525033));
#229923=CARTESIAN_POINT('Ctrl Pts',(-1.32147485166616,15.2,10.5525959663214));
#229924=CARTESIAN_POINT('Ctrl Pts',(-1.32105580642201,15.2,10.5562691075929));
#229925=CARTESIAN_POINT('Ctrl Pts',(-1.32062541426983,15.2,10.5599686680081));
#229926=CARTESIAN_POINT('Ctrl Pts',(-1.32002286524739,15.2,10.5651480526701));
#229927=CARTESIAN_POINT('Ctrl Pts',(-1.31939807516402,15.2,10.5703792168905));
#229928=CARTESIAN_POINT('Ctrl Pts',(-1.31875054919476,15.2,10.5756613289885));
#229929=CARTESIAN_POINT('Ctrl Pts',(-1.3182880306525,15.2,10.5794342661426));
#229930=CARTESIAN_POINT('Ctrl Pts',(-1.31781391451886,15.2,10.5832331959043));
#229931=CARTESIAN_POINT('Ctrl Pts',(-1.31732802347657,15.2,10.5870578222252));
#229932=CARTESIAN_POINT('Ctrl Pts',(-1.31684213243428,15.2,10.5908824485461));
#229933=CARTESIAN_POINT('Ctrl Pts',(-1.31634446770051,15.2,10.5947327693267));
#229934=CARTESIAN_POINT('Ctrl Pts',(-1.31583485496588,15.2,10.5986084916749));
#229935=CARTESIAN_POINT('Ctrl Pts',(-1.31532524223126,15.2,10.6024842140231));
#229936=CARTESIAN_POINT('Ctrl Pts',(-1.31480368417572,15.2,10.6063853355614));
#229937=CARTESIAN_POINT('Ctrl Pts',(-1.31427001139694,15.2,10.6103115670218));
#229938=CARTESIAN_POINT('Ctrl Pts',(-1.3135228695532,15.2,10.6158082907241));
#229939=CARTESIAN_POINT('Ctrl Pts',(-1.3127519821012,15.2,10.6213542276119));
#229940=CARTESIAN_POINT('Ctrl Pts',(-1.3119568983327,15.2,10.6269485919689));
#229941=CARTESIAN_POINT('Ctrl Pts',(-1.31127539788012,15.2,10.6317437619777));
#229942=CARTESIAN_POINT('Ctrl Pts',(-1.31057612170664,15.2,10.6365745106687));
#229943=CARTESIAN_POINT('Ctrl Pts',(-1.30985879046398,15.2,10.6414403509291));
#229944=CARTESIAN_POINT('Ctrl Pts',(-1.30926101446102,15.2,10.6454952175917));
#229945=CARTESIAN_POINT('Ctrl Pts',(-1.30865070386409,15.2,10.6495744526291));
#229946=CARTESIAN_POINT('Ctrl Pts',(-1.30802769796026,15.2,10.65367777902));
#229947=CARTESIAN_POINT('Ctrl Pts',(-1.30752929327794,15.2,10.6569604398644));
#229948=CARTESIAN_POINT('Ctrl Pts',(-1.30702276556058,15.2,10.660258518515));
#229949=CARTESIAN_POINT('Ctrl Pts',(-1.30650803482543,15.2,10.6635718735209));
#229950=CARTESIAN_POINT('Ctrl Pts',(-1.30599330402014,15.2,10.6668852289782));
#229951=CARTESIAN_POINT('Ctrl Pts',(-1.30547037095139,15.2,10.6702138618652));
#229952=CARTESIAN_POINT('Ctrl Pts',(-1.30493915867296,15.2,10.6735576314935));
#229953=CARTESIAN_POINT('Ctrl Pts',(-1.30400953729426,15.2,10.6794092276599));
#229954=CARTESIAN_POINT('Ctrl Pts',(-1.30305455716802,15.2,10.6853071812285));
#229955=CARTESIAN_POINT('Ctrl Pts',(-1.30207381280005,15.2,10.6912507511613));
#229956=CARTESIAN_POINT('Ctrl Pts',(-1.30123317467218,15.2,10.6963452402701));
#229957=CARTESIAN_POINT('Ctrl Pts',(-1.30037360910795,15.2,10.7014732442082));
#229958=CARTESIAN_POINT('Ctrl Pts',(-1.2994948666817,15.2,10.7066343037493));
#229959=CARTESIAN_POINT('Ctrl Pts',(-1.29890903847735,15.2,10.7100750096412));
#229960=CARTESIAN_POINT('Ctrl Pts',(-1.29831468618556,15.2,10.7135304069149));
#229961=CARTESIAN_POINT('Ctrl Pts',(-1.29771173829097,15.2,10.7170003612414));
#229962=CARTESIAN_POINT('Ctrl Pts',(-1.29665657937275,15.2,10.7230727819037));
#229963=CARTESIAN_POINT('Ctrl Pts',(-1.29557509817755,15.2,10.7291897826339));
#229964=CARTESIAN_POINT('Ctrl Pts',(-1.29446691172466,15.2,10.735350652994));
#229965=CARTESIAN_POINT('Ctrl Pts',(-1.29367534998492,15.2,10.7397512746113));
#229966=CARTESIAN_POINT('Ctrl Pts',(-1.29287016372494,15.2,10.7441742778563));
#229967=CARTESIAN_POINT('Ctrl Pts',(-1.29205121865479,15.2,10.7486194070241));
#229968=CARTESIAN_POINT('Ctrl Pts',(-1.29139606265222,15.2,10.7521755100676));
#229969=CARTESIAN_POINT('Ctrl Pts',(-1.29073210033475,15.2,10.7557457737527));
#229970=CARTESIAN_POINT('Ctrl Pts',(-1.2900592643351,15.2,10.7593300686806));
#229971=CARTESIAN_POINT('Ctrl Pts',(-1.28921821926677,15.2,10.7638104377067));
#229972=CARTESIAN_POINT('Ctrl Pts',(-1.28836330849334,15.2,10.7683127293226));
#229973=CARTESIAN_POINT('Ctrl Pts',(-1.28749440178425,15.2,10.7728366929498));
#229974=CARTESIAN_POINT('Ctrl Pts',(-1.28679927637909,15.2,10.7764558640489));
#229975=CARTESIAN_POINT('Ctrl Pts',(-1.28609519354783,15.2,10.7800889059208));
#229976=CARTESIAN_POINT('Ctrl Pts',(-1.28538208817504,15.2,10.7837356895648));
#229977=CARTESIAN_POINT('Ctrl Pts',(-1.28431243021302,15.2,10.7892058645341));
#229978=CARTESIAN_POINT('Ctrl Pts',(-1.28322247001929,15.2,10.7947069620842));
#229979=CARTESIAN_POINT('Ctrl Pts',(-1.28211199106053,15.2,10.8002385522152));
#229980=CARTESIAN_POINT('Ctrl Pts',(-1.28137167168744,15.2,10.8039262793042));
#229981=CARTESIAN_POINT('Ctrl Pts',(-1.28062223308668,15.2,10.8076275609331));
#229982=CARTESIAN_POINT('Ctrl Pts',(-1.27986361167329,15.2,10.8113422713224));
#229983=CARTESIAN_POINT('Ctrl Pts',(-1.2785360243549,15.2,10.8178430137444));
#229984=CARTESIAN_POINT('Ctrl Pts',(-1.27718031534707,15.2,10.8243848802251));
#229985=CARTESIAN_POINT('Ctrl Pts',(-1.27579615312941,15.2,10.83096721091));
#229986=CARTESIAN_POINT('Ctrl Pts',(-1.27500520319837,15.2,10.8347285431691));
#229987=CARTESIAN_POINT('Ctrl Pts',(-1.27420496341403,15.2,10.8385030876955));
#229988=CARTESIAN_POINT('Ctrl Pts',(-1.27339537203287,15.2,10.8422907232525));
#229989=CARTESIAN_POINT('Ctrl Pts',(-1.27258578076202,15.2,10.8460783582935));
#229990=CARTESIAN_POINT('Ctrl Pts',(-1.27176683820296,15.2,10.8498790840589));
#229991=CARTESIAN_POINT('Ctrl Pts',(-1.27093848566053,15.2,10.8536927791347));
#229992=CARTESIAN_POINT('Ctrl Pts',(-1.27011013300523,15.2,10.8575064747301));
#229993=CARTESIAN_POINT('Ctrl Pts',(-1.26927236963515,15.2,10.8613331395768));
#229994=CARTESIAN_POINT('Ctrl Pts',(-1.26842513703343,15.2,10.8651726545083));
#229995=CARTESIAN_POINT('Ctrl Pts',(-1.26757790443171,15.2,10.8690121694397));
#229996=CARTESIAN_POINT('Ctrl Pts',(-1.26672120383163,15.2,10.8728645326394));
#229997=CARTESIAN_POINT('Ctrl Pts',(-1.2658549746168,15.2,10.8767296269069));
#229998=CARTESIAN_POINT('Ctrl Pts',(-1.26477218827528,15.2,10.8815609939513));
#229999=CARTESIAN_POINT('Ctrl Pts',(-1.26367451792866,15.2,10.8864122510732));
#230000=CARTESIAN_POINT('Ctrl Pts',(-1.26256185062063,15.2,10.8912831696378));
#230001=CARTESIAN_POINT('Ctrl Pts',(-1.26144918319131,15.2,10.8961540887334));
#230002=CARTESIAN_POINT('Ctrl Pts',(-1.26032151914277,15.2,10.9010446657315));
#230003=CARTESIAN_POINT('Ctrl Pts',(-1.25917875011623,15.2,10.905954674341));
#230004=CARTESIAN_POINT('Ctrl Pts',(-1.25826453484518,15.2,10.9098826814427));
#230005=CARTESIAN_POINT('Ctrl Pts',(-1.2573406517371,15.2,10.9138231253928));
#230006=CARTESIAN_POINT('Ctrl Pts',(-1.25640704774176,15.2,10.9177758884416));
#230007=CARTESIAN_POINT('Ctrl Pts',(-1.25547344374643,15.2,10.9217286514904));
#230008=CARTESIAN_POINT('Ctrl Pts',(-1.25453011773608,15.2,10.9256937344017));
#230009=CARTESIAN_POINT('Ctrl Pts',(-1.25357701579425,15.2,10.9296710226752));
#230010=CARTESIAN_POINT('Ctrl Pts',(-1.25262391398229,15.2,10.9336483104068));
#230011=CARTESIAN_POINT('Ctrl Pts',(-1.2516610363784,15.2,10.9376378020757));
#230012=CARTESIAN_POINT('Ctrl Pts',(-1.25068833050909,15.2,10.9416393844889));
#230013=CARTESIAN_POINT('Ctrl Pts',(-1.24947244807305,15.2,10.9466413629143));
#230014=CARTESIAN_POINT('Ctrl Pts',(-1.24824120746676,15.2,10.9516622324555));
#230015=CARTESIAN_POINT('Ctrl Pts',(-1.24699450850843,15.2,10.9567017702333));
#230016=CARTESIAN_POINT('Ctrl Pts',(-1.24599714928742,15.2,10.9607334006752));
#230017=CARTESIAN_POINT('Ctrl Pts',(-1.24498989763467,15.2,10.9647769799519));
#230018=CARTESIAN_POINT('Ctrl Pts',(-1.24397269913378,15.2,10.9688323943963));
#230019=CARTESIAN_POINT('Ctrl Pts',(-1.24270120121554,15.2,10.9739016616231));
#230020=CARTESIAN_POINT('Ctrl Pts',(-1.24141416551056,15.2,10.9789894235345));
#230021=CARTESIAN_POINT('Ctrl Pts',(-1.24011149169548,15.2,10.9840954606154));
#230022=CARTESIAN_POINT('Ctrl Pts',(-1.23880881773842,15.2,10.9892014982528));
#230023=CARTESIAN_POINT('Ctrl Pts',(-1.23749050626219,15.2,10.9943258109343));
#230024=CARTESIAN_POINT('Ctrl Pts',(-1.23615646216625,15.2,10.999468182044));
#230025=CARTESIAN_POINT('Ctrl Pts',(-1.23482241807032,15.2,11.0046105531536));
#230026=CARTESIAN_POINT('Ctrl Pts',(-1.23347263894236,15.2,11.0097709829192));
#230027=CARTESIAN_POINT('Ctrl Pts',(-1.2321070324169,15.2,11.0149492591489));
#230028=CARTESIAN_POINT('Ctrl Pts',(-1.23101454713699,15.2,11.0190918803584));
#230029=CARTESIAN_POINT('Ctrl Pts',(-1.22991193112312,15.2,11.0232459215073));
#230030=CARTESIAN_POINT('Ctrl Pts',(-1.22879913911736,15.2,11.0274112746239));
#230031=CARTESIAN_POINT('Ctrl Pts',(-1.22768634726322,15.2,11.031576627173));
#230032=CARTESIAN_POINT('Ctrl Pts',(-1.22656337725278,15.2,11.0357532920838));
#230033=CARTESIAN_POINT('Ctrl Pts',(-1.22543018223537,15.2,11.0399411605736));
#230034=CARTESIAN_POINT('Ctrl Pts',(-1.22429698706356,15.2,11.0441290296339));
#230035=CARTESIAN_POINT('Ctrl Pts',(-1.2231535680258,15.2,11.0483281015653));
#230036=CARTESIAN_POINT('Ctrl Pts',(-1.22199987879097,15.2,11.0525382707028));
#230037=CARTESIAN_POINT('Ctrl Pts',(-1.22084618971334,15.2,11.0567484392667));
#230038=CARTESIAN_POINT('Ctrl Pts',(-1.2196822291367,15.2,11.0609697042495));
#230039=CARTESIAN_POINT('Ctrl Pts',(-1.21850795340042,15.2,11.0652019587913));
#230040=CARTESIAN_POINT('Ctrl Pts',(-1.216746539556,15.2,11.0715503414689));
#230041=CARTESIAN_POINT('Ctrl Pts',(-1.21496191504266,15.2,11.0779234504574));
#230042=CARTESIAN_POINT('Ctrl Pts',(-1.21315392919313,15.2,11.084320930057));
#230043=CARTESIAN_POINT('Ctrl Pts',(-1.21194860545767,15.2,11.0885859158757));
#230044=CARTESIAN_POINT('Ctrl Pts',(-1.21073289819365,15.2,11.0928617311429));
#230045=CARTESIAN_POINT('Ctrl Pts',(-1.20950676567796,15.2,11.0971482745613));
#230046=CARTESIAN_POINT('Ctrl Pts',(-1.20858716624943,15.2,11.1003631822712));
#230047=CARTESIAN_POINT('Ctrl Pts',(-1.20766170073515,15.2,11.1035841239479));
#230048=CARTESIAN_POINT('Ctrl Pts',(-1.20673035293646,15.2,11.1068110535381));
#230049=CARTESIAN_POINT('Ctrl Pts',(-1.20517810654891,15.2,11.1121892697173));
#230050=CARTESIAN_POINT('Ctrl Pts',(-1.20360951992828,15.2,11.1175841244824));
#230051=CARTESIAN_POINT('Ctrl Pts',(-1.20202450770741,15.2,11.1229954133005));
#230052=CARTESIAN_POINT('Ctrl Pts',(-1.2007564978616,15.2,11.1273244445909));
#230053=CARTESIAN_POINT('Ctrl Pts',(-1.19947797663925,15.2,11.1316639950766));
#230054=CARTESIAN_POINT('Ctrl Pts',(-1.19818890150755,15.2,11.1360139602779));
#230055=CARTESIAN_POINT('Ctrl Pts',(-1.19722209524659,15.2,11.1392764338826));
#230056=CARTESIAN_POINT('Ctrl Pts',(-1.19624935251984,15.2,11.1425447669178));
#230057=CARTESIAN_POINT('Ctrl Pts',(-1.19527065675932,15.2,11.145818915022));
#230058=CARTESIAN_POINT('Ctrl Pts',(-1.19396572896009,15.2,11.1501844462241));
#230059=CARTESIAN_POINT('Ctrl Pts',(-1.19265021641218,15.2,11.1545603161048));
#230060=CARTESIAN_POINT('Ctrl Pts',(-1.19132407978327,15.2,11.1589464232337));
#230061=CARTESIAN_POINT('Ctrl Pts',(-1.19032947740193,15.2,11.1622360032817));
#230062=CARTESIAN_POINT('Ctrl Pts',(-1.18932889820423,15.2,11.1655313408293));
#230063=CARTESIAN_POINT('Ctrl Pts',(-1.18832232590695,15.2,11.1688323948765));
#230064=CARTESIAN_POINT('Ctrl Pts',(-1.18698022957153,15.2,11.1732338000729));
#230065=CARTESIAN_POINT('Ctrl Pts',(-1.1856274785786,15.2,11.1776453663527));
#230066=CARTESIAN_POINT('Ctrl Pts',(-1.18426403345622,15.2,11.1820669926001));
#230067=CARTESIAN_POINT('Ctrl Pts',(-1.18324144956799,15.2,11.1853832124362));
#230068=CARTESIAN_POINT('Ctrl Pts',(-1.18221284908723,15.2,11.1887050918462));
#230069=CARTESIAN_POINT('Ctrl Pts',(-1.18117821775065,15.2,11.1920325875162));
#230070=CARTESIAN_POINT('Ctrl Pts',(-1.17979870917657,15.2,11.1964692488125));
#230071=CARTESIAN_POINT('Ctrl Pts',(-1.17840847774311,15.2,11.200915896021));
#230072=CARTESIAN_POINT('Ctrl Pts',(-1.17700748400011,15.2,11.2053724292083));
#230073=CARTESIAN_POINT('Ctrl Pts',(-1.1759567387883,15.2,11.2087148287951));
#230074=CARTESIAN_POINT('Ctrl Pts',(-1.17489993931003,15.2,11.2120627894902));
#230075=CARTESIAN_POINT('Ctrl Pts',(-1.17383707105752,15.2,11.2154162686178));
#230076=CARTESIAN_POINT('Ctrl Pts',(-1.172774202805,15.2,11.2187697477455));
#230077=CARTESIAN_POINT('Ctrl Pts',(-1.17170526577197,15.2,11.2221287461205));
#230078=CARTESIAN_POINT('Ctrl Pts',(-1.17063024296636,15.2,11.2254932223324));
#230079=CARTESIAN_POINT('Ctrl Pts',(-1.16955522016075,15.2,11.2288576985443));
#230080=CARTESIAN_POINT('Ctrl Pts',(-1.16847411226343,15.2,11.2322276517042));
#230081=CARTESIAN_POINT('Ctrl Pts',(-1.16738690347044,15.2,11.2356030408308));
#230082=CARTESIAN_POINT('Ctrl Pts',(-1.16629969447994,15.2,11.2389784305706));
#230083=CARTESIAN_POINT('Ctrl Pts',(-1.16520638405436,15.2,11.242359256762));
#230084=CARTESIAN_POINT('Ctrl Pts',(-1.16410695806042,15.2,11.2457454779632));
#230085=CARTESIAN_POINT('Ctrl Pts',(-1.1630075322662,15.2,11.2491316985492));
#230086=CARTESIAN_POINT('Ctrl Pts',(-1.16190198958896,15.2,11.2525233133266));
#230087=CARTESIAN_POINT('Ctrl Pts',(-1.16079031633715,15.2,11.255920282412));
#230088=CARTESIAN_POINT('Ctrl Pts',(-1.15930808540207,15.2,11.2604495743201));
#230089=CARTESIAN_POINT('Ctrl Pts',(-1.15781495419971,15.2,11.2649883842597));
#230090=CARTESIAN_POINT('Ctrl Pts',(-1.15631088654601,15.2,11.269536615498));
#230091=CARTESIAN_POINT('Ctrl Pts',(-1.15518283554958,15.2,11.2729477897013));
#230092=CARTESIAN_POINT('Ctrl Pts',(-1.15404863225139,15.2,11.2763642627813));
#230093=CARTESIAN_POINT('Ctrl Pts',(-1.15290826379315,15.2,11.2797859950292));
#230094=CARTESIAN_POINT('Ctrl Pts',(-1.15176789554209,15.2,11.2832077266556));
#230095=CARTESIAN_POINT('Ctrl Pts',(-1.15062136097677,15.2,11.2866347171334));
#230096=CARTESIAN_POINT('Ctrl Pts',(-1.14946864475202,15.2,11.2900669268474));
#230097=CARTESIAN_POINT('Ctrl Pts',(-1.1475474509743,15.2,11.2957872765786));
#230098=CARTESIAN_POINT('Ctrl Pts',(-1.14560908942906,15.2,11.3015221195174));
#230099=CARTESIAN_POINT('Ctrl Pts',(-1.14365349151096,15.2,11.3072712732686));
#230100=CARTESIAN_POINT('Ctrl Pts',(-1.14248013280273,15.2,11.310720765394));
#230101=CARTESIAN_POINT('Ctrl Pts',(-1.14130056949487,15.2,11.3141754097524));
#230102=CARTESIAN_POINT('Ctrl Pts',(-1.14011478637074,15.2,11.3176351649188));
#230103=CARTESIAN_POINT('Ctrl Pts',(-1.13853374227705,15.2,11.3222481715979));
#230104=CARTESIAN_POINT('Ctrl Pts',(-1.13694164344741,15.2,11.3268702646566));
#230105=CARTESIAN_POINT('Ctrl Pts',(-1.13533845449933,15.2,11.3315013521197));
#230106=CARTESIAN_POINT('Ctrl Pts',(-1.13413606273367,15.2,11.3349746678748));
#230107=CARTESIAN_POINT('Ctrl Pts',(-1.13292743320328,15.2,11.3384530415345));
#230108=CARTESIAN_POINT('Ctrl Pts',(-1.13171255249827,15.2,11.3419364337406));
#230109=CARTESIAN_POINT('Ctrl Pts',(-1.1296877512497,15.2,11.3477420876283));
#230110=CARTESIAN_POINT('Ctrl Pts',(-1.12764558405698,15.2,11.3535616835713));
#230111=CARTESIAN_POINT('Ctrl Pts',(-1.12558598954449,15.2,11.3593950391953));
#230112=CARTESIAN_POINT('Ctrl Pts',(-1.1243502326574,15.2,11.3628950530783));
#230113=CARTESIAN_POINT('Ctrl Pts',(-1.12310820284356,15.2,11.3664000220044));
#230114=CARTESIAN_POINT('Ctrl Pts',(-1.12185988495296,15.2,11.3699099047651));
#230115=CARTESIAN_POINT('Ctrl Pts',(-1.11977935566443,15.2,11.3757597078786));
#230116=CARTESIAN_POINT('Ctrl Pts',(-1.11768136063922,15.2,11.381623160384));
#230117=CARTESIAN_POINT('Ctrl Pts',(-1.11556583955181,15.2,11.3875000794646));
#230118=CARTESIAN_POINT('Ctrl Pts',(-1.11429652657653,15.2,11.3910262318097));
#230119=CARTESIAN_POINT('Ctrl Pts',(-1.1130209038578,15.2,11.3945572327229));
#230120=CARTESIAN_POINT('Ctrl Pts',(-1.11173896000396,15.2,11.3980930480291));
#230121=CARTESIAN_POINT('Ctrl Pts',(-1.110457016383,15.2,11.401628862693));
#230122=CARTESIAN_POINT('Ctrl Pts',(-1.10916875256239,15.2,11.4051694916149));
#230123=CARTESIAN_POINT('Ctrl Pts',(-1.10787415431722,15.2,11.4087148951115));
#230124=CARTESIAN_POINT('Ctrl Pts',(-1.10657955607204,15.2,11.4122602986081));
#230125=CARTESIAN_POINT('Ctrl Pts',(-1.10527862254071,15.2,11.4158104755162));
#230126=CARTESIAN_POINT('Ctrl Pts',(-1.10397133974891,15.2,11.4193653785282));
#230127=CARTESIAN_POINT('Ctrl Pts',(-1.10179253501675,15.2,11.4252902170968));
#230128=CARTESIAN_POINT('Ctrl Pts',(-1.09959608544472,15.2,11.431228170913));
#230129=CARTESIAN_POINT('Ctrl Pts',(-1.09738195536205,15.2,11.4371791166813));
#230130=CARTESIAN_POINT('Ctrl Pts',(-1.09605347736072,15.2,11.4407496840126));
#230131=CARTESIAN_POINT('Ctrl Pts',(-1.09471863524371,15.2,11.4443249343496));
#230132=CARTESIAN_POINT('Ctrl Pts',(-1.09337743000006,15.2,11.447904865));
#230133=CARTESIAN_POINT('Origin',(-5.66257110645729E-14,15.2,-1.77635683940025E-14));
#230134=CARTESIAN_POINT('',(-1.76496130700006,15.2,10.223773109));
#230135=CARTESIAN_POINT('',(-1.76496130700006,12.2,10.223773109));
#230136=CARTESIAN_POINT('',(-1.76496130700006,15.2,10.223773109));
#230137=CARTESIAN_POINT('Origin',(-5.66257110645729E-14,12.2,-1.77635683940025E-14));
#230138=CARTESIAN_POINT('Origin',(-5.66257110645729E-14,15.2,-1.77635683940025E-14));
#230139=CARTESIAN_POINT('Origin',(-5.66257110645729E-14,15.2,-1.77635683940025E-14));
#230140=CARTESIAN_POINT('',(-2.33718477800006,15.2,11.259998549));
#230141=CARTESIAN_POINT('',(-2.71145515300006,15.2,11.175777868));
#230142=CARTESIAN_POINT('Origin',(-5.66257110645729E-14,15.2,-1.77635683940025E-14));
#230143=CARTESIAN_POINT('',(-2.71145515300006,12.2,11.175777868));
#230144=CARTESIAN_POINT('',(-2.71145515300006,15.2,11.175777868));
#230145=CARTESIAN_POINT('',(-2.33718477800006,12.2,11.259998549));
#230146=CARTESIAN_POINT('Origin',(-5.66257110645729E-14,12.2,-1.77635683940025E-14));
#230147=CARTESIAN_POINT('',(-2.33718477800006,15.2,11.259998549));
#230148=CARTESIAN_POINT('Ctrl Pts',(-2.71145515300006,15.2,11.175777868));
#230149=CARTESIAN_POINT('Ctrl Pts',(-2.71145515300006,11.6,11.175777868));
#230150=CARTESIAN_POINT('Ctrl Pts',(-2.71161876900006,15.2,11.175030994));
#230151=CARTESIAN_POINT('Ctrl Pts',(-2.71161876900006,11.6,11.175030994));
#230152=CARTESIAN_POINT('Ctrl Pts',(-2.71194562400006,15.2,11.173537618));
#230153=CARTESIAN_POINT('Ctrl Pts',(-2.71194562400006,11.6,11.173537618));
#230154=CARTESIAN_POINT('Ctrl Pts',(-2.71243478100006,15.2,11.17129866));
#230155=CARTESIAN_POINT('Ctrl Pts',(-2.71243478100006,11.6,11.17129866));
#230156=CARTESIAN_POINT('Ctrl Pts',(-2.71308473600006,15.2,11.168315598));
#230157=CARTESIAN_POINT('Ctrl Pts',(-2.71308473600006,11.6,11.168315598));
#230158=CARTESIAN_POINT('Ctrl Pts',(-2.71389342500005,15.2,11.164590464));
#230159=CARTESIAN_POINT('Ctrl Pts',(-2.71389342500005,11.6,11.164590464));
#230160=CARTESIAN_POINT('Ctrl Pts',(-2.71469835900006,15.2,11.160869024));
#230161=CARTESIAN_POINT('Ctrl Pts',(-2.71469835900006,11.6,11.160869024));
#230162=CARTESIAN_POINT('Ctrl Pts',(-2.71549953800006,15.2,11.15715128));
#230163=CARTESIAN_POINT('Ctrl Pts',(-2.71549953800006,11.6,11.15715128));
#230164=CARTESIAN_POINT('Ctrl Pts',(-2.71629696700006,15.2,11.153437237));
#230165=CARTESIAN_POINT('Ctrl Pts',(-2.71629696700006,11.6,11.153437237));
#230166=CARTESIAN_POINT('Ctrl Pts',(-2.71709064500006,15.2,11.149726898));
#230167=CARTESIAN_POINT('Ctrl Pts',(-2.71709064500006,11.6,11.149726898));
#230168=CARTESIAN_POINT('Ctrl Pts',(-2.71788057600005,15.2,11.146020271));
#230169=CARTESIAN_POINT('Ctrl Pts',(-2.71788057600005,11.6,11.146020271));
#230170=CARTESIAN_POINT('Ctrl Pts',(-2.71866676600005,15.2,11.142317366));
#230171=CARTESIAN_POINT('Ctrl Pts',(-2.71866676600005,11.6,11.142317366));
#230172=CARTESIAN_POINT('Ctrl Pts',(-2.71944921900006,15.2,11.138618192));
#230173=CARTESIAN_POINT('Ctrl Pts',(-2.71944921900006,11.6,11.138618192));
#230174=CARTESIAN_POINT('Ctrl Pts',(-2.72022794000006,15.2,11.134922759));
#230175=CARTESIAN_POINT('Ctrl Pts',(-2.72022794000006,11.6,11.134922759));
#230176=CARTESIAN_POINT('Ctrl Pts',(-2.72100293300006,15.2,11.131231076));
#230177=CARTESIAN_POINT('Ctrl Pts',(-2.72100293300006,11.6,11.131231076));
#230178=CARTESIAN_POINT('Ctrl Pts',(-2.72177420400005,15.2,11.127543154));
#230179=CARTESIAN_POINT('Ctrl Pts',(-2.72177420400005,11.6,11.127543154));
#230180=CARTESIAN_POINT('Ctrl Pts',(-2.72254175800006,15.2,11.123859));
#230181=CARTESIAN_POINT('Ctrl Pts',(-2.72254175800006,11.6,11.123859));
#230182=CARTESIAN_POINT('Ctrl Pts',(-2.72330559700006,15.2,11.120178623));
#230183=CARTESIAN_POINT('Ctrl Pts',(-2.72330559700006,11.6,11.120178623));
#230184=CARTESIAN_POINT('Ctrl Pts',(-2.72406572400006,15.2,11.116502029));
#230185=CARTESIAN_POINT('Ctrl Pts',(-2.72406572400006,11.6,11.116502029));
#230186=CARTESIAN_POINT('Ctrl Pts',(-2.72482214500006,15.2,11.112829227));
#230187=CARTESIAN_POINT('Ctrl Pts',(-2.72482214500006,11.6,11.112829227));
#230188=CARTESIAN_POINT('Ctrl Pts',(-2.72557486200005,15.2,11.109160223));
#230189=CARTESIAN_POINT('Ctrl Pts',(-2.72557486200005,11.6,11.109160223));
#230190=CARTESIAN_POINT('Ctrl Pts',(-2.72632388100006,15.2,11.105495025));
#230191=CARTESIAN_POINT('Ctrl Pts',(-2.72632388100006,11.6,11.105495025));
#230192=CARTESIAN_POINT('Ctrl Pts',(-2.72706920300006,15.2,11.10183364));
#230193=CARTESIAN_POINT('Ctrl Pts',(-2.72706920300006,11.6,11.10183364));
#230194=CARTESIAN_POINT('Ctrl Pts',(-2.72781083400006,15.2,11.098176078));
#230195=CARTESIAN_POINT('Ctrl Pts',(-2.72781083400006,11.6,11.098176078));
#230196=CARTESIAN_POINT('Ctrl Pts',(-2.72854877900006,15.2,11.094522347));
#230197=CARTESIAN_POINT('Ctrl Pts',(-2.72854877900006,11.6,11.094522347));
#230198=CARTESIAN_POINT('Ctrl Pts',(-2.72928304000006,15.2,11.090872455));
#230199=CARTESIAN_POINT('Ctrl Pts',(-2.72928304000006,11.6,11.090872455));
#230200=CARTESIAN_POINT('Ctrl Pts',(-2.73001362300006,15.2,11.087226411));
#230201=CARTESIAN_POINT('Ctrl Pts',(-2.73001362300006,11.6,11.087226411));
#230202=CARTESIAN_POINT('Ctrl Pts',(-2.73074053200005,15.2,11.083584223));
#230203=CARTESIAN_POINT('Ctrl Pts',(-2.73074053200005,11.6,11.083584223));
#230204=CARTESIAN_POINT('Ctrl Pts',(-2.73146377200006,15.2,11.0799459));
#230205=CARTESIAN_POINT('Ctrl Pts',(-2.73146377200006,11.6,11.0799459));
#230206=CARTESIAN_POINT('Ctrl Pts',(-2.73218334500006,15.2,11.076311449));
#230207=CARTESIAN_POINT('Ctrl Pts',(-2.73218334500006,11.6,11.076311449));
#230208=CARTESIAN_POINT('Ctrl Pts',(-2.73289925700006,15.2,11.072680878));
#230209=CARTESIAN_POINT('Ctrl Pts',(-2.73289925700006,11.6,11.072680878));
#230210=CARTESIAN_POINT('Ctrl Pts',(-2.73361151100006,15.2,11.069054196));
#230211=CARTESIAN_POINT('Ctrl Pts',(-2.73361151100006,11.6,11.069054196));
#230212=CARTESIAN_POINT('Ctrl Pts',(-2.73432011200006,15.2,11.065431411));
#230213=CARTESIAN_POINT('Ctrl Pts',(-2.73432011200006,11.6,11.065431411));
#230214=CARTESIAN_POINT('Ctrl Pts',(-2.73502506400006,15.2,11.06181253));
#230215=CARTESIAN_POINT('Ctrl Pts',(-2.73502506400006,11.6,11.06181253));
#230216=CARTESIAN_POINT('Ctrl Pts',(-2.73572637100005,15.2,11.058197563));
#230217=CARTESIAN_POINT('Ctrl Pts',(-2.73572637100005,11.6,11.058197563));
#230218=CARTESIAN_POINT('Ctrl Pts',(-2.73642403700005,15.2,11.054586517));
#230219=CARTESIAN_POINT('Ctrl Pts',(-2.73642403700005,11.6,11.054586517));
#230220=CARTESIAN_POINT('Ctrl Pts',(-2.73711806800006,15.2,11.050979401));
#230221=CARTESIAN_POINT('Ctrl Pts',(-2.73711806800006,11.6,11.050979401));
#230222=CARTESIAN_POINT('Ctrl Pts',(-2.73780846600005,15.2,11.047376223));
#230223=CARTESIAN_POINT('Ctrl Pts',(-2.73780846600005,11.6,11.047376223));
#230224=CARTESIAN_POINT('Ctrl Pts',(-2.73849523700005,15.2,11.043776991));
#230225=CARTESIAN_POINT('Ctrl Pts',(-2.73849523700005,11.6,11.043776991));
#230226=CARTESIAN_POINT('Ctrl Pts',(-2.73917838500005,15.2,11.040181715));
#230227=CARTESIAN_POINT('Ctrl Pts',(-2.73917838500005,11.6,11.040181715));
#230228=CARTESIAN_POINT('Ctrl Pts',(-2.73985791300006,15.2,11.036590401));
#230229=CARTESIAN_POINT('Ctrl Pts',(-2.73985791300006,11.6,11.036590401));
#230230=CARTESIAN_POINT('Ctrl Pts',(-2.74053382800005,15.2,11.033003059));
#230231=CARTESIAN_POINT('Ctrl Pts',(-2.74053382800005,11.6,11.033003059));
#230232=CARTESIAN_POINT('Ctrl Pts',(-2.74120613200005,15.2,11.029419696));
#230233=CARTESIAN_POINT('Ctrl Pts',(-2.74120613200005,11.6,11.029419696));
#230234=CARTESIAN_POINT('Ctrl Pts',(-2.74187483100006,15.2,11.025840322));
#230235=CARTESIAN_POINT('Ctrl Pts',(-2.74187483100006,11.6,11.025840322));
#230236=CARTESIAN_POINT('Ctrl Pts',(-2.74253992800006,15.2,11.022264944));
#230237=CARTESIAN_POINT('Ctrl Pts',(-2.74253992800006,11.6,11.022264944));
#230238=CARTESIAN_POINT('Ctrl Pts',(-2.74320142800006,15.2,11.01869357));
#230239=CARTESIAN_POINT('Ctrl Pts',(-2.74320142800006,11.6,11.01869357));
#230240=CARTESIAN_POINT('Ctrl Pts',(-2.74385933600006,15.2,11.015126211));
#230241=CARTESIAN_POINT('Ctrl Pts',(-2.74385933600006,11.6,11.015126211));
#230242=CARTESIAN_POINT('Ctrl Pts',(-2.74451365600005,15.2,11.011562872));
#230243=CARTESIAN_POINT('Ctrl Pts',(-2.74451365600005,11.6,11.011562872));
#230244=CARTESIAN_POINT('Ctrl Pts',(-2.74516439300006,15.2,11.008003564));
#230245=CARTESIAN_POINT('Ctrl Pts',(-2.74516439300006,11.6,11.008003564));
#230246=CARTESIAN_POINT('Ctrl Pts',(-2.74581155000006,15.2,11.004448294));
#230247=CARTESIAN_POINT('Ctrl Pts',(-2.74581155000006,11.6,11.004448294));
#230248=CARTESIAN_POINT('Ctrl Pts',(-2.74645513200006,15.2,11.00089707));
#230249=CARTESIAN_POINT('Ctrl Pts',(-2.74645513200006,11.6,11.00089707));
#230250=CARTESIAN_POINT('Ctrl Pts',(-2.74709514500006,15.2,10.997349902));
#230251=CARTESIAN_POINT('Ctrl Pts',(-2.74709514500006,11.6,10.997349902));
#230252=CARTESIAN_POINT('Ctrl Pts',(-2.74773159200006,15.2,10.993806798));
#230253=CARTESIAN_POINT('Ctrl Pts',(-2.74773159200006,11.6,10.993806798));
#230254=CARTESIAN_POINT('Ctrl Pts',(-2.74836447800006,15.2,10.990267766));
#230255=CARTESIAN_POINT('Ctrl Pts',(-2.74836447800006,11.6,10.990267766));
#230256=CARTESIAN_POINT('Ctrl Pts',(-2.74899380800006,15.2,10.986732814));
#230257=CARTESIAN_POINT('Ctrl Pts',(-2.74899380800006,11.6,10.986732814));
#230258=CARTESIAN_POINT('Ctrl Pts',(-2.74961958600006,15.2,10.983201952));
#230259=CARTESIAN_POINT('Ctrl Pts',(-2.74961958600006,11.6,10.983201952));
#230260=CARTESIAN_POINT('Ctrl Pts',(-2.75024181600006,15.2,10.979675187));
#230261=CARTESIAN_POINT('Ctrl Pts',(-2.75024181600006,11.6,10.979675187));
#230262=CARTESIAN_POINT('Ctrl Pts',(-2.75086050500006,15.2,10.976152528));
#230263=CARTESIAN_POINT('Ctrl Pts',(-2.75086050500006,11.6,10.976152528));
#230264=CARTESIAN_POINT('Ctrl Pts',(-2.75147565400006,15.2,10.972633985));
#230265=CARTESIAN_POINT('Ctrl Pts',(-2.75147565400006,11.6,10.972633985));
#230266=CARTESIAN_POINT('Ctrl Pts',(-2.75208727000006,15.2,10.969119564));
#230267=CARTESIAN_POINT('Ctrl Pts',(-2.75208727000006,11.6,10.969119564));
#230268=CARTESIAN_POINT('Ctrl Pts',(-2.75269535800006,15.2,10.965609275));
#230269=CARTESIAN_POINT('Ctrl Pts',(-2.75269535800006,11.6,10.965609275));
#230270=CARTESIAN_POINT('Ctrl Pts',(-2.75329992200006,15.2,10.962103126));
#230271=CARTESIAN_POINT('Ctrl Pts',(-2.75329992200006,11.6,10.962103126));
#230272=CARTESIAN_POINT('Ctrl Pts',(-2.75390096500006,15.2,10.958601125));
#230273=CARTESIAN_POINT('Ctrl Pts',(-2.75390096500006,11.6,10.958601125));
#230274=CARTESIAN_POINT('Ctrl Pts',(-2.75449849500006,15.2,10.955103284));
#230275=CARTESIAN_POINT('Ctrl Pts',(-2.75449849500006,11.6,10.955103284));
#230276=CARTESIAN_POINT('Ctrl Pts',(-2.75509251400006,15.2,10.951609606));
#230277=CARTESIAN_POINT('Ctrl Pts',(-2.75509251400006,11.6,10.951609606));
#230278=CARTESIAN_POINT('Ctrl Pts',(-2.75568302800006,15.2,10.948120105));
#230279=CARTESIAN_POINT('Ctrl Pts',(-2.75568302800006,11.6,10.948120105));
#230280=CARTESIAN_POINT('Ctrl Pts',(-2.75627004200006,15.2,10.944634786));
#230281=CARTESIAN_POINT('Ctrl Pts',(-2.75627004200006,11.6,10.944634786));
#230282=CARTESIAN_POINT('Ctrl Pts',(-2.75685355900006,15.2,10.941153659));
#230283=CARTESIAN_POINT('Ctrl Pts',(-2.75685355900006,11.6,10.941153659));
#230284=CARTESIAN_POINT('Ctrl Pts',(-2.75743358600006,15.2,10.937676733));
#230285=CARTESIAN_POINT('Ctrl Pts',(-2.75743358600006,11.6,10.937676733));
#230286=CARTESIAN_POINT('Ctrl Pts',(-2.75801012600006,15.2,10.934204015));
#230287=CARTESIAN_POINT('Ctrl Pts',(-2.75801012600006,11.6,10.934204015));
#230288=CARTESIAN_POINT('Ctrl Pts',(-2.75858318400005,15.2,10.930735515));
#230289=CARTESIAN_POINT('Ctrl Pts',(-2.75858318400005,11.6,10.930735515));
#230290=CARTESIAN_POINT('Ctrl Pts',(-2.75915276600006,15.2,10.927271243));
#230291=CARTESIAN_POINT('Ctrl Pts',(-2.75915276600006,11.6,10.927271243));
#230292=CARTESIAN_POINT('Ctrl Pts',(-2.75971887700006,15.2,10.923811204));
#230293=CARTESIAN_POINT('Ctrl Pts',(-2.75971887700006,11.6,10.923811204));
#230294=CARTESIAN_POINT('Ctrl Pts',(-2.76028152000006,15.2,10.92035541));
#230295=CARTESIAN_POINT('Ctrl Pts',(-2.76028152000006,11.6,10.92035541));
#230296=CARTESIAN_POINT('Ctrl Pts',(-2.76084070100006,15.2,10.916903869));
#230297=CARTESIAN_POINT('Ctrl Pts',(-2.76084070100006,11.6,10.916903869));
#230298=CARTESIAN_POINT('Ctrl Pts',(-2.76139642500006,15.2,10.913456588));
#230299=CARTESIAN_POINT('Ctrl Pts',(-2.76139642500006,11.6,10.913456588));
#230300=CARTESIAN_POINT('Ctrl Pts',(-2.76194869600006,15.2,10.910013578));
#230301=CARTESIAN_POINT('Ctrl Pts',(-2.76194869600006,11.6,10.910013578));
#230302=CARTESIAN_POINT('Ctrl Pts',(-2.76249752100005,15.2,10.906574846));
#230303=CARTESIAN_POINT('Ctrl Pts',(-2.76249752100005,11.6,10.906574846));
#230304=CARTESIAN_POINT('Ctrl Pts',(-2.76304290200006,15.2,10.903140402));
#230305=CARTESIAN_POINT('Ctrl Pts',(-2.76304290200006,11.6,10.903140402));
#230306=CARTESIAN_POINT('Ctrl Pts',(-2.76358484700005,15.2,10.899710254));
#230307=CARTESIAN_POINT('Ctrl Pts',(-2.76358484700005,11.6,10.899710254));
#230308=CARTESIAN_POINT('Ctrl Pts',(-2.76412335700006,15.2,10.896284411));
#230309=CARTESIAN_POINT('Ctrl Pts',(-2.76412335700006,11.6,10.896284411));
#230310=CARTESIAN_POINT('Ctrl Pts',(-2.76465844200006,15.2,10.892862881));
#230311=CARTESIAN_POINT('Ctrl Pts',(-2.76465844200006,11.6,10.892862881));
#230312=CARTESIAN_POINT('Ctrl Pts',(-2.76519010400006,15.2,10.889445675));
#230313=CARTESIAN_POINT('Ctrl Pts',(-2.76519010400006,11.6,10.889445675));
#230314=CARTESIAN_POINT('Ctrl Pts',(-2.76571834700006,15.2,10.8860328));
#230315=CARTESIAN_POINT('Ctrl Pts',(-2.76571834700006,11.6,10.8860328));
#230316=CARTESIAN_POINT('Ctrl Pts',(-2.76624317800006,15.2,10.882624266));
#230317=CARTESIAN_POINT('Ctrl Pts',(-2.76624317800006,11.6,10.882624266));
#230318=CARTESIAN_POINT('Ctrl Pts',(-2.76676460200005,15.2,10.87922008));
#230319=CARTESIAN_POINT('Ctrl Pts',(-2.76676460200005,11.6,10.87922008));
#230320=CARTESIAN_POINT('Ctrl Pts',(-2.76728262300006,15.2,10.875820252));
#230321=CARTESIAN_POINT('Ctrl Pts',(-2.76728262300006,11.6,10.875820252));
#230322=CARTESIAN_POINT('Ctrl Pts',(-2.76779724800006,15.2,10.872424791));
#230323=CARTESIAN_POINT('Ctrl Pts',(-2.76779724800006,11.6,10.872424791));
#230324=CARTESIAN_POINT('Ctrl Pts',(-2.76830847900006,15.2,10.869033706));
#230325=CARTESIAN_POINT('Ctrl Pts',(-2.76830847900006,11.6,10.869033706));
#230326=CARTESIAN_POINT('Ctrl Pts',(-2.76881632300006,15.2,10.865647005));
#230327=CARTESIAN_POINT('Ctrl Pts',(-2.76881632300006,11.6,10.865647005));
#230328=CARTESIAN_POINT('Ctrl Pts',(-2.76932078600006,15.2,10.862264699));
#230329=CARTESIAN_POINT('Ctrl Pts',(-2.76932078600006,11.6,10.862264699));
#230330=CARTESIAN_POINT('Ctrl Pts',(-2.76982187200006,15.2,10.858886794));
#230331=CARTESIAN_POINT('Ctrl Pts',(-2.76982187200006,11.6,10.858886794));
#230332=CARTESIAN_POINT('Ctrl Pts',(-2.77031958500006,15.2,10.855513301));
#230333=CARTESIAN_POINT('Ctrl Pts',(-2.77031958500006,11.6,10.855513301));
#230334=CARTESIAN_POINT('Ctrl Pts',(-2.77081393200006,15.2,10.852144229));
#230335=CARTESIAN_POINT('Ctrl Pts',(-2.77081393200006,11.6,10.852144229));
#230336=CARTESIAN_POINT('Ctrl Pts',(-2.77130491800006,15.2,10.848779585));
#230337=CARTESIAN_POINT('Ctrl Pts',(-2.77130491800006,11.6,10.848779585));
#230338=CARTESIAN_POINT('Ctrl Pts',(-2.77179254800005,15.2,10.845419379));
#230339=CARTESIAN_POINT('Ctrl Pts',(-2.77179254800005,11.6,10.845419379));
#230340=CARTESIAN_POINT('Ctrl Pts',(-2.77227682700006,15.2,10.842063621));
#230341=CARTESIAN_POINT('Ctrl Pts',(-2.77227682700006,11.6,10.842063621));
#230342=CARTESIAN_POINT('Ctrl Pts',(-2.77275776000006,15.2,10.838712319));
#230343=CARTESIAN_POINT('Ctrl Pts',(-2.77275776000006,11.6,10.838712319));
#230344=CARTESIAN_POINT('Ctrl Pts',(-2.77323535300006,15.2,10.835365483));
#230345=CARTESIAN_POINT('Ctrl Pts',(-2.77323535300006,11.6,10.835365483));
#230346=CARTESIAN_POINT('Ctrl Pts',(-2.77370961000006,15.2,10.83202312));
#230347=CARTESIAN_POINT('Ctrl Pts',(-2.77370961000006,11.6,10.83202312));
#230348=CARTESIAN_POINT('Ctrl Pts',(-2.77418053800006,15.2,10.828685241));
#230349=CARTESIAN_POINT('Ctrl Pts',(-2.77418053800006,11.6,10.828685241));
#230350=CARTESIAN_POINT('Ctrl Pts',(-2.77464814200005,15.2,10.825351855));
#230351=CARTESIAN_POINT('Ctrl Pts',(-2.77464814200005,11.6,10.825351855));
#230352=CARTESIAN_POINT('Ctrl Pts',(-2.77511242500006,15.2,10.822022969));
#230353=CARTESIAN_POINT('Ctrl Pts',(-2.77511242500006,11.6,10.822022969));
#230354=CARTESIAN_POINT('Ctrl Pts',(-2.77557339600006,15.2,10.818698594));
#230355=CARTESIAN_POINT('Ctrl Pts',(-2.77557339600006,11.6,10.818698594));
#230356=CARTESIAN_POINT('Ctrl Pts',(-2.77603105800006,15.2,10.815378739));
#230357=CARTESIAN_POINT('Ctrl Pts',(-2.77603105800006,11.6,10.815378739));
#230358=CARTESIAN_POINT('Ctrl Pts',(-2.77648541700006,15.2,10.812063413));
#230359=CARTESIAN_POINT('Ctrl Pts',(-2.77648541700006,11.6,10.812063413));
#230360=CARTESIAN_POINT('Ctrl Pts',(-2.77693647800006,15.2,10.808752625));
#230361=CARTESIAN_POINT('Ctrl Pts',(-2.77693647800006,11.6,10.808752625));
#230362=CARTESIAN_POINT('Ctrl Pts',(-2.77738424800006,15.2,10.805446383));
#230363=CARTESIAN_POINT('Ctrl Pts',(-2.77738424800006,11.6,10.805446383));
#230364=CARTESIAN_POINT('Ctrl Pts',(-2.77782872900006,15.2,10.802144697));
#230365=CARTESIAN_POINT('Ctrl Pts',(-2.77782872900006,11.6,10.802144697));
#230366=CARTESIAN_POINT('Ctrl Pts',(-2.77826993000006,15.2,10.798847577));
#230367=CARTESIAN_POINT('Ctrl Pts',(-2.77826993000006,11.6,10.798847577));
#230368=CARTESIAN_POINT('Ctrl Pts',(-2.77870785500005,15.2,10.795555031));
#230369=CARTESIAN_POINT('Ctrl Pts',(-2.77870785500005,11.6,10.795555031));
#230370=CARTESIAN_POINT('Ctrl Pts',(-2.77914251100006,15.2,10.792267068));
#230371=CARTESIAN_POINT('Ctrl Pts',(-2.77914251100006,11.6,10.792267068));
#230372=CARTESIAN_POINT('Ctrl Pts',(-2.77957390000005,15.2,10.788983699));
#230373=CARTESIAN_POINT('Ctrl Pts',(-2.77957390000005,11.6,10.788983699));
#230374=CARTESIAN_POINT('Ctrl Pts',(-2.78000203100006,15.2,10.785704931));
#230375=CARTESIAN_POINT('Ctrl Pts',(-2.78000203100006,11.6,10.785704931));
#230376=CARTESIAN_POINT('Ctrl Pts',(-2.78042690800006,15.2,10.782430774));
#230377=CARTESIAN_POINT('Ctrl Pts',(-2.78042690800006,11.6,10.782430774));
#230378=CARTESIAN_POINT('Ctrl Pts',(-2.78084853700005,15.2,10.779161239));
#230379=CARTESIAN_POINT('Ctrl Pts',(-2.78084853700005,11.6,10.779161239));
#230380=CARTESIAN_POINT('Ctrl Pts',(-2.78126692300006,15.2,10.775896333));
#230381=CARTESIAN_POINT('Ctrl Pts',(-2.78126692300006,11.6,10.775896333));
#230382=CARTESIAN_POINT('Ctrl Pts',(-2.78168207300005,15.2,10.772636066));
#230383=CARTESIAN_POINT('Ctrl Pts',(-2.78168207300005,11.6,10.772636066));
#230384=CARTESIAN_POINT('Ctrl Pts',(-2.78209399200006,15.2,10.769380447));
#230385=CARTESIAN_POINT('Ctrl Pts',(-2.78209399200006,11.6,10.769380447));
#230386=CARTESIAN_POINT('Ctrl Pts',(-2.78250268400006,15.2,10.766129486));
#230387=CARTESIAN_POINT('Ctrl Pts',(-2.78250268400006,11.6,10.766129486));
#230388=CARTESIAN_POINT('Ctrl Pts',(-2.78290815600006,15.2,10.762883192));
#230389=CARTESIAN_POINT('Ctrl Pts',(-2.78290815600006,11.6,10.762883192));
#230390=CARTESIAN_POINT('Ctrl Pts',(-2.78331041400006,15.2,10.759641574));
#230391=CARTESIAN_POINT('Ctrl Pts',(-2.78331041400006,11.6,10.759641574));
#230392=CARTESIAN_POINT('Ctrl Pts',(-2.78370946300006,15.2,10.756404641));
#230393=CARTESIAN_POINT('Ctrl Pts',(-2.78370946300006,11.6,10.756404641));
#230394=CARTESIAN_POINT('Ctrl Pts',(-2.78410531000006,15.2,10.753172404));
#230395=CARTESIAN_POINT('Ctrl Pts',(-2.78410531000006,11.6,10.753172404));
#230396=CARTESIAN_POINT('Ctrl Pts',(-2.78449795900006,15.2,10.749944871));
#230397=CARTESIAN_POINT('Ctrl Pts',(-2.78449795900006,11.6,10.749944871));
#230398=CARTESIAN_POINT('Ctrl Pts',(-2.78488741700006,15.2,10.746722052));
#230399=CARTESIAN_POINT('Ctrl Pts',(-2.78488741700006,11.6,10.746722052));
#230400=CARTESIAN_POINT('Ctrl Pts',(-2.78527368900006,15.2,10.743503955));
#230401=CARTESIAN_POINT('Ctrl Pts',(-2.78527368900006,11.6,10.743503955));
#230402=CARTESIAN_POINT('Ctrl Pts',(-2.78565678100006,15.2,10.740290591));
#230403=CARTESIAN_POINT('Ctrl Pts',(-2.78565678100006,11.6,10.740290591));
#230404=CARTESIAN_POINT('Ctrl Pts',(-2.78603670000006,15.2,10.73708197));
#230405=CARTESIAN_POINT('Ctrl Pts',(-2.78603670000006,11.6,10.73708197));
#230406=CARTESIAN_POINT('Ctrl Pts',(-2.78641345100006,15.2,10.7338781));
#230407=CARTESIAN_POINT('Ctrl Pts',(-2.78641345100006,11.6,10.7338781));
#230408=CARTESIAN_POINT('Ctrl Pts',(-2.78678703800006,15.2,10.73067899));
#230409=CARTESIAN_POINT('Ctrl Pts',(-2.78678703800006,11.6,10.73067899));
#230410=CARTESIAN_POINT('Ctrl Pts',(-2.78715746900006,15.2,10.727484651));
#230411=CARTESIAN_POINT('Ctrl Pts',(-2.78715746900006,11.6,10.727484651));
#230412=CARTESIAN_POINT('Ctrl Pts',(-2.78752475100006,15.2,10.724295092));
#230413=CARTESIAN_POINT('Ctrl Pts',(-2.78752475100006,11.6,10.724295092));
#230414=CARTESIAN_POINT('Ctrl Pts',(-2.78788888700006,15.2,10.721110321));
#230415=CARTESIAN_POINT('Ctrl Pts',(-2.78788888700006,11.6,10.721110321));
#230416=CARTESIAN_POINT('Ctrl Pts',(-2.78824988500005,15.2,10.71793035));
#230417=CARTESIAN_POINT('Ctrl Pts',(-2.78824988500005,11.6,10.71793035));
#230418=CARTESIAN_POINT('Ctrl Pts',(-2.78860774900005,15.2,10.714755188));
#230419=CARTESIAN_POINT('Ctrl Pts',(-2.78860774900005,11.6,10.714755188));
#230420=CARTESIAN_POINT('Ctrl Pts',(-2.78896248700006,15.2,10.711584842));
#230421=CARTESIAN_POINT('Ctrl Pts',(-2.78896248700006,11.6,10.711584842));
#230422=CARTESIAN_POINT('Ctrl Pts',(-2.78931410500005,15.2,10.708419325));
#230423=CARTESIAN_POINT('Ctrl Pts',(-2.78931410500005,11.6,10.708419325));
#230424=CARTESIAN_POINT('Ctrl Pts',(-2.78966260700006,15.2,10.705258645));
#230425=CARTESIAN_POINT('Ctrl Pts',(-2.78966260700006,11.6,10.705258645));
#230426=CARTESIAN_POINT('Ctrl Pts',(-2.79000800100006,15.2,10.702102811));
#230427=CARTESIAN_POINT('Ctrl Pts',(-2.79000800100006,11.6,10.702102811));
#230428=CARTESIAN_POINT('Ctrl Pts',(-2.79035029200006,15.2,10.698951833));
#230429=CARTESIAN_POINT('Ctrl Pts',(-2.79035029200006,11.6,10.698951833));
#230430=CARTESIAN_POINT('Ctrl Pts',(-2.79068948600006,15.2,10.695805722));
#230431=CARTESIAN_POINT('Ctrl Pts',(-2.79068948600006,11.6,10.695805722));
#230432=CARTESIAN_POINT('Ctrl Pts',(-2.79102559000005,15.2,10.692664486));
#230433=CARTESIAN_POINT('Ctrl Pts',(-2.79102559000005,11.6,10.692664486));
#230434=CARTESIAN_POINT('Ctrl Pts',(-2.79135860900006,15.2,10.689528136));
#230435=CARTESIAN_POINT('Ctrl Pts',(-2.79135860900006,11.6,10.689528136));
#230436=CARTESIAN_POINT('Ctrl Pts',(-2.79168855100006,15.2,10.68639668));
#230437=CARTESIAN_POINT('Ctrl Pts',(-2.79168855100006,11.6,10.68639668));
#230438=CARTESIAN_POINT('Ctrl Pts',(-2.79201542000005,15.2,10.683270128));
#230439=CARTESIAN_POINT('Ctrl Pts',(-2.79201542000005,11.6,10.683270128));
#230440=CARTESIAN_POINT('Ctrl Pts',(-2.79233922300006,15.2,10.680148491));
#230441=CARTESIAN_POINT('Ctrl Pts',(-2.79233922300006,11.6,10.680148491));
#230442=CARTESIAN_POINT('Ctrl Pts',(-2.79265996700006,15.2,10.677031779));
#230443=CARTESIAN_POINT('Ctrl Pts',(-2.79265996700006,11.6,10.677031779));
#230444=CARTESIAN_POINT('Ctrl Pts',(-2.79297765700006,15.2,10.67392));
#230445=CARTESIAN_POINT('Ctrl Pts',(-2.79297765700006,11.6,10.67392));
#230446=CARTESIAN_POINT('Ctrl Pts',(-2.79329230000006,15.2,10.670813164));
#230447=CARTESIAN_POINT('Ctrl Pts',(-2.79329230000006,11.6,10.670813164));
#230448=CARTESIAN_POINT('Ctrl Pts',(-2.79360390200006,15.2,10.667711281));
#230449=CARTESIAN_POINT('Ctrl Pts',(-2.79360390200006,11.6,10.667711281));
#230450=CARTESIAN_POINT('Ctrl Pts',(-2.79391246900006,15.2,10.664614362));
#230451=CARTESIAN_POINT('Ctrl Pts',(-2.79391246900006,11.6,10.664614362));
#230452=CARTESIAN_POINT('Ctrl Pts',(-2.79421800800006,15.2,10.661522415));
#230453=CARTESIAN_POINT('Ctrl Pts',(-2.79421800800006,11.6,10.661522415));
#230454=CARTESIAN_POINT('Ctrl Pts',(-2.79452052500006,15.2,10.658435452));
#230455=CARTESIAN_POINT('Ctrl Pts',(-2.79452052500006,11.6,10.658435452));
#230456=CARTESIAN_POINT('Ctrl Pts',(-2.79482002600006,15.2,10.655353481));
#230457=CARTESIAN_POINT('Ctrl Pts',(-2.79482002600006,11.6,10.655353481));
#230458=CARTESIAN_POINT('Ctrl Pts',(-2.79511651700005,15.2,10.652276512));
#230459=CARTESIAN_POINT('Ctrl Pts',(-2.79511651700005,11.6,10.652276512));
#230460=CARTESIAN_POINT('Ctrl Pts',(-2.79541000600006,15.2,10.649204555));
#230461=CARTESIAN_POINT('Ctrl Pts',(-2.79541000600006,11.6,10.649204555));
#230462=CARTESIAN_POINT('Ctrl Pts',(-2.79570049800005,15.2,10.64613762));
#230463=CARTESIAN_POINT('Ctrl Pts',(-2.79570049800005,11.6,10.64613762));
#230464=CARTESIAN_POINT('Ctrl Pts',(-2.79598799900006,15.2,10.643075718));
#230465=CARTESIAN_POINT('Ctrl Pts',(-2.79598799900006,11.6,10.643075718));
#230466=CARTESIAN_POINT('Ctrl Pts',(-2.79627251800005,15.2,10.640018857));
#230467=CARTESIAN_POINT('Ctrl Pts',(-2.79627251800005,11.6,10.640018857));
#230468=CARTESIAN_POINT('Ctrl Pts',(-2.79655405900006,15.2,10.636967049));
#230469=CARTESIAN_POINT('Ctrl Pts',(-2.79655405900006,11.6,10.636967049));
#230470=CARTESIAN_POINT('Ctrl Pts',(-2.79683262900006,15.2,10.633920302));
#230471=CARTESIAN_POINT('Ctrl Pts',(-2.79683262900006,11.6,10.633920302));
#230472=CARTESIAN_POINT('Ctrl Pts',(-2.79710823600006,15.2,10.630878627));
#230473=CARTESIAN_POINT('Ctrl Pts',(-2.79710823600006,11.6,10.630878627));
#230474=CARTESIAN_POINT('Ctrl Pts',(-2.79738088300005,15.2,10.627842034));
#230475=CARTESIAN_POINT('Ctrl Pts',(-2.79738088300005,11.6,10.627842034));
#230476=CARTESIAN_POINT('Ctrl Pts',(-2.79765058100006,15.2,10.624810531));
#230477=CARTESIAN_POINT('Ctrl Pts',(-2.79765058100006,11.6,10.624810531));
#230478=CARTESIAN_POINT('Ctrl Pts',(-2.79791733400006,15.2,10.621784132));
#230479=CARTESIAN_POINT('Ctrl Pts',(-2.79791733400006,11.6,10.621784132));
#230480=CARTESIAN_POINT('Ctrl Pts',(-2.79818114900006,15.2,10.618762845));
#230481=CARTESIAN_POINT('Ctrl Pts',(-2.79818114900006,11.6,10.618762845));
#230482=CARTESIAN_POINT('Ctrl Pts',(-2.79844203300006,15.2,10.615746678));
#230483=CARTESIAN_POINT('Ctrl Pts',(-2.79844203300006,11.6,10.615746678));
#230484=CARTESIAN_POINT('Ctrl Pts',(-2.79869999200006,15.2,10.612735644));
#230485=CARTESIAN_POINT('Ctrl Pts',(-2.79869999200006,11.6,10.612735644));
#230486=CARTESIAN_POINT('Ctrl Pts',(-2.79895503300006,15.2,10.609729752));
#230487=CARTESIAN_POINT('Ctrl Pts',(-2.79895503300006,11.6,10.609729752));
#230488=CARTESIAN_POINT('Ctrl Pts',(-2.79920716400006,15.2,10.606729013));
#230489=CARTESIAN_POINT('Ctrl Pts',(-2.79920716400006,11.6,10.606729013));
#230490=CARTESIAN_POINT('Ctrl Pts',(-2.79945638900006,15.2,10.603733435));
#230491=CARTESIAN_POINT('Ctrl Pts',(-2.79945638900006,11.6,10.603733435));
#230492=CARTESIAN_POINT('Ctrl Pts',(-2.79970271700006,15.2,10.60074303));
#230493=CARTESIAN_POINT('Ctrl Pts',(-2.79970271700006,11.6,10.60074303));
#230494=CARTESIAN_POINT('Ctrl Pts',(-2.79994615400006,15.2,10.597757808));
#230495=CARTESIAN_POINT('Ctrl Pts',(-2.79994615400006,11.6,10.597757808));
#230496=CARTESIAN_POINT('Ctrl Pts',(-2.80018670700006,15.2,10.594777778));
#230497=CARTESIAN_POINT('Ctrl Pts',(-2.80018670700006,11.6,10.594777778));
#230498=CARTESIAN_POINT('Ctrl Pts',(-2.80042438200006,15.2,10.591802951));
#230499=CARTESIAN_POINT('Ctrl Pts',(-2.80042438200006,11.6,10.591802951));
#230500=CARTESIAN_POINT('Ctrl Pts',(-2.80065918600005,15.2,10.588833338));
#230501=CARTESIAN_POINT('Ctrl Pts',(-2.80065918600005,11.6,10.588833338));
#230502=CARTESIAN_POINT('Ctrl Pts',(-2.80089112800006,15.2,10.585868947));
#230503=CARTESIAN_POINT('Ctrl Pts',(-2.80089112800006,11.6,10.585868947));
#230504=CARTESIAN_POINT('Ctrl Pts',(-2.80112021200006,15.2,10.582909791));
#230505=CARTESIAN_POINT('Ctrl Pts',(-2.80112021200006,11.6,10.582909791));
#230506=CARTESIAN_POINT('Ctrl Pts',(-2.80134644700006,15.2,10.579955878));
#230507=CARTESIAN_POINT('Ctrl Pts',(-2.80134644700006,11.6,10.579955878));
#230508=CARTESIAN_POINT('Ctrl Pts',(-2.80156983900006,15.2,10.57700722));
#230509=CARTESIAN_POINT('Ctrl Pts',(-2.80156983900006,11.6,10.57700722));
#230510=CARTESIAN_POINT('Ctrl Pts',(-2.80179039400006,15.2,10.574063826));
#230511=CARTESIAN_POINT('Ctrl Pts',(-2.80179039400006,11.6,10.574063826));
#230512=CARTESIAN_POINT('Ctrl Pts',(-2.80200812100006,15.2,10.571125707));
#230513=CARTESIAN_POINT('Ctrl Pts',(-2.80200812100006,11.6,10.571125707));
#230514=CARTESIAN_POINT('Ctrl Pts',(-2.80222302600006,15.2,10.568192874));
#230515=CARTESIAN_POINT('Ctrl Pts',(-2.80222302600006,11.6,10.568192874));
#230516=CARTESIAN_POINT('Ctrl Pts',(-2.80243511500006,15.2,10.565265335));
#230517=CARTESIAN_POINT('Ctrl Pts',(-2.80243511500006,11.6,10.565265335));
#230518=CARTESIAN_POINT('Ctrl Pts',(-2.80264439700006,15.2,10.562343103));
#230519=CARTESIAN_POINT('Ctrl Pts',(-2.80264439700006,11.6,10.562343103));
#230520=CARTESIAN_POINT('Ctrl Pts',(-2.80285087800006,15.2,10.559426187));
#230521=CARTESIAN_POINT('Ctrl Pts',(-2.80285087800006,11.6,10.559426187));
#230522=CARTESIAN_POINT('Ctrl Pts',(-2.80305456500006,15.2,10.556514597));
#230523=CARTESIAN_POINT('Ctrl Pts',(-2.80305456500006,11.6,10.556514597));
#230524=CARTESIAN_POINT('Ctrl Pts',(-2.80325546600006,15.2,10.553608346));
#230525=CARTESIAN_POINT('Ctrl Pts',(-2.80325546600006,11.6,10.553608346));
#230526=CARTESIAN_POINT('Ctrl Pts',(-2.80345358700006,15.2,10.550707441));
#230527=CARTESIAN_POINT('Ctrl Pts',(-2.80345358700006,11.6,10.550707441));
#230528=CARTESIAN_POINT('Ctrl Pts',(-2.80364893600006,15.2,10.547811894));
#230529=CARTESIAN_POINT('Ctrl Pts',(-2.80364893600006,11.6,10.547811894));
#230530=CARTESIAN_POINT('Ctrl Pts',(-2.80384152000006,15.2,10.544921717));
#230531=CARTESIAN_POINT('Ctrl Pts',(-2.80384152000006,11.6,10.544921717));
#230532=CARTESIAN_POINT('Ctrl Pts',(-2.80403134500005,15.2,10.542036918));
#230533=CARTESIAN_POINT('Ctrl Pts',(-2.80403134500005,11.6,10.542036918));
#230534=CARTESIAN_POINT('Ctrl Pts',(-2.80421842000006,15.2,10.539157509));
#230535=CARTESIAN_POINT('Ctrl Pts',(-2.80421842000006,11.6,10.539157509));
#230536=CARTESIAN_POINT('Ctrl Pts',(-2.80440275200006,15.2,10.5362835));
#230537=CARTESIAN_POINT('Ctrl Pts',(-2.80440275200006,11.6,10.5362835));
#230538=CARTESIAN_POINT('Ctrl Pts',(-2.80458434800006,15.2,10.533414902));
#230539=CARTESIAN_POINT('Ctrl Pts',(-2.80458434800006,11.6,10.533414902));
#230540=CARTESIAN_POINT('Ctrl Pts',(-2.80476321500006,15.2,10.530551726));
#230541=CARTESIAN_POINT('Ctrl Pts',(-2.80476321500006,11.6,10.530551726));
#230542=CARTESIAN_POINT('Ctrl Pts',(-2.80493936200005,15.2,10.52769398));
#230543=CARTESIAN_POINT('Ctrl Pts',(-2.80493936200005,11.6,10.52769398));
#230544=CARTESIAN_POINT('Ctrl Pts',(-2.80511279300006,15.2,10.524841678));
#230545=CARTESIAN_POINT('Ctrl Pts',(-2.80511279300006,11.6,10.524841678));
#230546=CARTESIAN_POINT('Ctrl Pts',(-2.80528351900006,15.2,10.52199483));
#230547=CARTESIAN_POINT('Ctrl Pts',(-2.80528351900006,11.6,10.52199483));
#230548=CARTESIAN_POINT('Ctrl Pts',(-2.80545154500006,15.2,10.519153444));
#230549=CARTESIAN_POINT('Ctrl Pts',(-2.80545154500006,11.6,10.519153444));
#230550=CARTESIAN_POINT('Ctrl Pts',(-2.80561687900006,15.2,10.516317534));
#230551=CARTESIAN_POINT('Ctrl Pts',(-2.80561687900006,11.6,10.516317534));
#230552=CARTESIAN_POINT('Ctrl Pts',(-2.80577953000006,15.2,10.513487108));
#230553=CARTESIAN_POINT('Ctrl Pts',(-2.80577953000006,11.6,10.513487108));
#230554=CARTESIAN_POINT('Ctrl Pts',(-2.80593950400006,15.2,10.510662179));
#230555=CARTESIAN_POINT('Ctrl Pts',(-2.80593950400006,11.6,10.510662179));
#230556=CARTESIAN_POINT('Ctrl Pts',(-2.80609680800006,15.2,10.507842757));
#230557=CARTESIAN_POINT('Ctrl Pts',(-2.80609680800006,11.6,10.507842757));
#230558=CARTESIAN_POINT('Ctrl Pts',(-2.80625145000006,15.2,10.505028852));
#230559=CARTESIAN_POINT('Ctrl Pts',(-2.80625145000006,11.6,10.505028852));
#230560=CARTESIAN_POINT('Ctrl Pts',(-2.80640343900005,15.2,10.502220475));
#230561=CARTESIAN_POINT('Ctrl Pts',(-2.80640343900005,11.6,10.502220475));
#230562=CARTESIAN_POINT('Ctrl Pts',(-2.80655278100005,15.2,10.499417638));
#230563=CARTESIAN_POINT('Ctrl Pts',(-2.80655278100005,11.6,10.499417638));
#230564=CARTESIAN_POINT('Ctrl Pts',(-2.80669948500006,15.2,10.49662035));
#230565=CARTESIAN_POINT('Ctrl Pts',(-2.80669948500006,11.6,10.49662035));
#230566=CARTESIAN_POINT('Ctrl Pts',(-2.80684355800005,15.2,10.493828624));
#230567=CARTESIAN_POINT('Ctrl Pts',(-2.80684355800005,11.6,10.493828624));
#230568=CARTESIAN_POINT('Ctrl Pts',(-2.80698500600006,15.2,10.491042469));
#230569=CARTESIAN_POINT('Ctrl Pts',(-2.80698500600006,11.6,10.491042469));
#230570=CARTESIAN_POINT('Ctrl Pts',(-2.80712383900006,15.2,10.488261897));
#230571=CARTESIAN_POINT('Ctrl Pts',(-2.80712383900006,11.6,10.488261897));
#230572=CARTESIAN_POINT('Ctrl Pts',(-2.80726006500006,15.2,10.485486918));
#230573=CARTESIAN_POINT('Ctrl Pts',(-2.80726006500006,11.6,10.485486918));
#230574=CARTESIAN_POINT('Ctrl Pts',(-2.80739369000006,15.2,10.482717543));
#230575=CARTESIAN_POINT('Ctrl Pts',(-2.80739369000006,11.6,10.482717543));
#230576=CARTESIAN_POINT('Ctrl Pts',(-2.80752472300006,15.2,10.479953784));
#230577=CARTESIAN_POINT('Ctrl Pts',(-2.80752472300006,11.6,10.479953784));
#230578=CARTESIAN_POINT('Ctrl Pts',(-2.80765317100005,15.2,10.477195653));
#230579=CARTESIAN_POINT('Ctrl Pts',(-2.80765317100005,11.6,10.477195653));
#230580=CARTESIAN_POINT('Ctrl Pts',(-2.80777904200006,15.2,10.474443157));
#230581=CARTESIAN_POINT('Ctrl Pts',(-2.80777904200006,11.6,10.474443157));
#230582=CARTESIAN_POINT('Ctrl Pts',(-2.80790234500006,15.2,10.47169631));
#230583=CARTESIAN_POINT('Ctrl Pts',(-2.80790234500006,11.6,10.47169631));
#230584=CARTESIAN_POINT('Ctrl Pts',(-2.80802308700005,15.2,10.468955123));
#230585=CARTESIAN_POINT('Ctrl Pts',(-2.80802308700005,11.6,10.468955123));
#230586=CARTESIAN_POINT('Ctrl Pts',(-2.80814127600005,15.2,10.466219607));
#230587=CARTESIAN_POINT('Ctrl Pts',(-2.80814127600005,11.6,10.466219607));
#230588=CARTESIAN_POINT('Ctrl Pts',(-2.80825692000006,15.2,10.463489772));
#230589=CARTESIAN_POINT('Ctrl Pts',(-2.80825692000006,11.6,10.463489772));
#230590=CARTESIAN_POINT('Ctrl Pts',(-2.80837002600005,15.2,10.460765629));
#230591=CARTESIAN_POINT('Ctrl Pts',(-2.80837002600005,11.6,10.460765629));
#230592=CARTESIAN_POINT('Ctrl Pts',(-2.80848060400006,15.2,10.458047191));
#230593=CARTESIAN_POINT('Ctrl Pts',(-2.80848060400006,11.6,10.458047191));
#230594=CARTESIAN_POINT('Ctrl Pts',(-2.80858866100006,15.2,10.455334468));
#230595=CARTESIAN_POINT('Ctrl Pts',(-2.80858866100006,11.6,10.455334468));
#230596=CARTESIAN_POINT('Ctrl Pts',(-2.80869420500005,15.2,10.45262747));
#230597=CARTESIAN_POINT('Ctrl Pts',(-2.80869420500005,11.6,10.45262747));
#230598=CARTESIAN_POINT('Ctrl Pts',(-2.80879724400006,15.2,10.44992621));
#230599=CARTESIAN_POINT('Ctrl Pts',(-2.80879724400006,11.6,10.44992621));
#230600=CARTESIAN_POINT('Ctrl Pts',(-2.80889778700006,15.2,10.447230699));
#230601=CARTESIAN_POINT('Ctrl Pts',(-2.80889778700006,11.6,10.447230699));
#230602=CARTESIAN_POINT('Ctrl Pts',(-2.80899584100006,15.2,10.444540948));
#230603=CARTESIAN_POINT('Ctrl Pts',(-2.80899584100006,11.6,10.444540948));
#230604=CARTESIAN_POINT('Ctrl Pts',(-2.80909141500006,15.2,10.441856968));
#230605=CARTESIAN_POINT('Ctrl Pts',(-2.80909141500006,11.6,10.441856968));
#230606=CARTESIAN_POINT('Ctrl Pts',(-2.80918451700006,15.2,10.43917877));
#230607=CARTESIAN_POINT('Ctrl Pts',(-2.80918451700006,11.6,10.43917877));
#230608=CARTESIAN_POINT('Ctrl Pts',(-2.80927515500006,15.2,10.436506365));
#230609=CARTESIAN_POINT('Ctrl Pts',(-2.80927515500006,11.6,10.436506365));
#230610=CARTESIAN_POINT('Ctrl Pts',(-2.80936333800006,15.2,10.433839767));
#230611=CARTESIAN_POINT('Ctrl Pts',(-2.80936333800006,11.6,10.433839767));
#230612=CARTESIAN_POINT('Ctrl Pts',(-2.80944907400006,15.2,10.431178984));
#230613=CARTESIAN_POINT('Ctrl Pts',(-2.80944907400006,11.6,10.431178984));
#230614=CARTESIAN_POINT('Ctrl Pts',(-2.80953237000006,15.2,10.428524029));
#230615=CARTESIAN_POINT('Ctrl Pts',(-2.80953237000006,11.6,10.428524029));
#230616=CARTESIAN_POINT('Ctrl Pts',(-2.80961323600006,15.2,10.425874914));
#230617=CARTESIAN_POINT('Ctrl Pts',(-2.80961323600006,11.6,10.425874914));
#230618=CARTESIAN_POINT('Ctrl Pts',(-2.80969168100006,15.2,10.423231649));
#230619=CARTESIAN_POINT('Ctrl Pts',(-2.80969168100006,11.6,10.423231649));
#230620=CARTESIAN_POINT('Ctrl Pts',(-2.80976771100006,15.2,10.420594246));
#230621=CARTESIAN_POINT('Ctrl Pts',(-2.80976771100006,11.6,10.420594246));
#230622=CARTESIAN_POINT('Ctrl Pts',(-2.80984133800006,15.2,10.417962717));
#230623=CARTESIAN_POINT('Ctrl Pts',(-2.80984133800006,11.6,10.417962717));
#230624=CARTESIAN_POINT('Ctrl Pts',(-2.80991256600006,15.2,10.415337072));
#230625=CARTESIAN_POINT('Ctrl Pts',(-2.80991256600006,11.6,10.415337072));
#230626=CARTESIAN_POINT('Ctrl Pts',(-2.80998140700006,15.2,10.412717324));
#230627=CARTESIAN_POINT('Ctrl Pts',(-2.80998140700006,11.6,10.412717324));
#230628=CARTESIAN_POINT('Ctrl Pts',(-2.81004786900006,15.2,10.410103485));
#230629=CARTESIAN_POINT('Ctrl Pts',(-2.81004786900006,11.6,10.410103485));
#230630=CARTESIAN_POINT('Ctrl Pts',(-2.81011195900006,15.2,10.407495565));
#230631=CARTESIAN_POINT('Ctrl Pts',(-2.81011195900006,11.6,10.407495565));
#230632=CARTESIAN_POINT('Ctrl Pts',(-2.81017368600006,15.2,10.404893577));
#230633=CARTESIAN_POINT('Ctrl Pts',(-2.81017368600006,11.6,10.404893577));
#230634=CARTESIAN_POINT('Ctrl Pts',(-2.81023306000006,15.2,10.402297531));
#230635=CARTESIAN_POINT('Ctrl Pts',(-2.81023306000006,11.6,10.402297531));
#230636=CARTESIAN_POINT('Ctrl Pts',(-2.81029009000005,15.2,10.399707441));
#230637=CARTESIAN_POINT('Ctrl Pts',(-2.81029009000005,11.6,10.399707441));
#230638=CARTESIAN_POINT('Ctrl Pts',(-2.81034478200006,15.2,10.397123316));
#230639=CARTESIAN_POINT('Ctrl Pts',(-2.81034478200006,11.6,10.397123316));
#230640=CARTESIAN_POINT('Ctrl Pts',(-2.81039714700006,15.2,10.39454517));
#230641=CARTESIAN_POINT('Ctrl Pts',(-2.81039714700006,11.6,10.39454517));
#230642=CARTESIAN_POINT('Ctrl Pts',(-2.81044719400006,15.2,10.391973013));
#230643=CARTESIAN_POINT('Ctrl Pts',(-2.81044719400006,11.6,10.391973013));
#230644=CARTESIAN_POINT('Ctrl Pts',(-2.81049493100006,15.2,10.389406857));
#230645=CARTESIAN_POINT('Ctrl Pts',(-2.81049493100006,11.6,10.389406857));
#230646=CARTESIAN_POINT('Ctrl Pts',(-2.81054036600006,15.2,10.386846714));
#230647=CARTESIAN_POINT('Ctrl Pts',(-2.81054036600006,11.6,10.386846714));
#230648=CARTESIAN_POINT('Ctrl Pts',(-2.81058350900006,15.2,10.384292596));
#230649=CARTESIAN_POINT('Ctrl Pts',(-2.81058350900006,11.6,10.384292596));
#230650=CARTESIAN_POINT('Ctrl Pts',(-2.81062436900006,15.2,10.381744516));
#230651=CARTESIAN_POINT('Ctrl Pts',(-2.81062436900006,11.6,10.381744516));
#230652=CARTESIAN_POINT('Ctrl Pts',(-2.81066295400006,15.2,10.379202484));
#230653=CARTESIAN_POINT('Ctrl Pts',(-2.81066295400006,11.6,10.379202484));
#230654=CARTESIAN_POINT('Ctrl Pts',(-2.81069927400006,15.2,10.376666512));
#230655=CARTESIAN_POINT('Ctrl Pts',(-2.81069927400006,11.6,10.376666512));
#230656=CARTESIAN_POINT('Ctrl Pts',(-2.81073333700005,15.2,10.374136614));
#230657=CARTESIAN_POINT('Ctrl Pts',(-2.81073333700005,11.6,10.374136614));
#230658=CARTESIAN_POINT('Ctrl Pts',(-2.81076515300006,15.2,10.371612799));
#230659=CARTESIAN_POINT('Ctrl Pts',(-2.81076515300006,11.6,10.371612799));
#230660=CARTESIAN_POINT('Ctrl Pts',(-2.81079473100006,15.2,10.369095081));
#230661=CARTESIAN_POINT('Ctrl Pts',(-2.81079473100006,11.6,10.369095081));
#230662=CARTESIAN_POINT('Ctrl Pts',(-2.81082207900006,15.2,10.366583471));
#230663=CARTESIAN_POINT('Ctrl Pts',(-2.81082207900006,11.6,10.366583471));
#230664=CARTESIAN_POINT('Ctrl Pts',(-2.81084720700005,15.2,10.364077981));
#230665=CARTESIAN_POINT('Ctrl Pts',(-2.81084720700005,11.6,10.364077981));
#230666=CARTESIAN_POINT('Ctrl Pts',(-2.81087012500006,15.2,10.361578624));
#230667=CARTESIAN_POINT('Ctrl Pts',(-2.81087012500006,11.6,10.361578624));
#230668=CARTESIAN_POINT('Ctrl Pts',(-2.81089084000006,15.2,10.359085411));
#230669=CARTESIAN_POINT('Ctrl Pts',(-2.81089084000006,11.6,10.359085411));
#230670=CARTESIAN_POINT('Ctrl Pts',(-2.81090936200005,15.2,10.356598354));
#230671=CARTESIAN_POINT('Ctrl Pts',(-2.81090936200005,11.6,10.356598354));
#230672=CARTESIAN_POINT('Ctrl Pts',(-2.81092570200005,15.2,10.354117466));
#230673=CARTESIAN_POINT('Ctrl Pts',(-2.81092570200005,11.6,10.354117466));
#230674=CARTESIAN_POINT('Ctrl Pts',(-2.81093986900005,15.2,10.351642759));
#230675=CARTESIAN_POINT('Ctrl Pts',(-2.81093986900005,11.6,10.351642759));
#230676=CARTESIAN_POINT('Ctrl Pts',(-2.81095187000005,15.2,10.349174244));
#230677=CARTESIAN_POINT('Ctrl Pts',(-2.81095187000005,11.6,10.349174244));
#230678=CARTESIAN_POINT('Ctrl Pts',(-2.81096171500006,15.2,10.346711935));
#230679=CARTESIAN_POINT('Ctrl Pts',(-2.81096171500006,11.6,10.346711935));
#230680=CARTESIAN_POINT('Ctrl Pts',(-2.81096941600006,15.2,10.344255843));
#230681=CARTESIAN_POINT('Ctrl Pts',(-2.81096941600006,11.6,10.344255843));
#230682=CARTESIAN_POINT('Ctrl Pts',(-2.81097498000006,15.2,10.34180598));
#230683=CARTESIAN_POINT('Ctrl Pts',(-2.81097498000006,11.6,10.34180598));
#230684=CARTESIAN_POINT('Ctrl Pts',(-2.81097841700006,15.2,10.33936236));
#230685=CARTESIAN_POINT('Ctrl Pts',(-2.81097841700006,11.6,10.33936236));
#230686=CARTESIAN_POINT('Ctrl Pts',(-2.81097973600006,15.2,10.336924994));
#230687=CARTESIAN_POINT('Ctrl Pts',(-2.81097973600006,11.6,10.336924994));
#230688=CARTESIAN_POINT('Ctrl Pts',(-2.81097894800005,15.2,10.334493893));
#230689=CARTESIAN_POINT('Ctrl Pts',(-2.81097894800005,11.6,10.334493893));
#230690=CARTESIAN_POINT('Ctrl Pts',(-2.81097606100006,15.2,10.332069072));
#230691=CARTESIAN_POINT('Ctrl Pts',(-2.81097606100006,11.6,10.332069072));
#230692=CARTESIAN_POINT('Ctrl Pts',(-2.81097108600005,15.2,10.329650542));
#230693=CARTESIAN_POINT('Ctrl Pts',(-2.81097108600005,11.6,10.329650542));
#230694=CARTESIAN_POINT('Ctrl Pts',(-2.81096403200006,15.2,10.327238316));
#230695=CARTESIAN_POINT('Ctrl Pts',(-2.81096403200006,11.6,10.327238316));
#230696=CARTESIAN_POINT('Ctrl Pts',(-2.81095490900006,15.2,10.324832405));
#230697=CARTESIAN_POINT('Ctrl Pts',(-2.81095490900006,11.6,10.324832405));
#230698=CARTESIAN_POINT('Ctrl Pts',(-2.81094372600006,15.2,10.322432823));
#230699=CARTESIAN_POINT('Ctrl Pts',(-2.81094372600006,11.6,10.322432823));
#230700=CARTESIAN_POINT('Ctrl Pts',(-2.81093049400006,15.2,10.320039583));
#230701=CARTESIAN_POINT('Ctrl Pts',(-2.81093049400006,11.6,10.320039583));
#230702=CARTESIAN_POINT('Ctrl Pts',(-2.81091522100006,15.2,10.317652695));
#230703=CARTESIAN_POINT('Ctrl Pts',(-2.81091522100006,11.6,10.317652695));
#230704=CARTESIAN_POINT('Ctrl Pts',(-2.81089791700006,15.2,10.315272175));
#230705=CARTESIAN_POINT('Ctrl Pts',(-2.81089791700006,11.6,10.315272175));
#230706=CARTESIAN_POINT('Ctrl Pts',(-2.81087859400006,15.2,10.312898032));
#230707=CARTESIAN_POINT('Ctrl Pts',(-2.81087859400006,11.6,10.312898032));
#230708=CARTESIAN_POINT('Ctrl Pts',(-2.81085726200006,15.2,10.310530282));
#230709=CARTESIAN_POINT('Ctrl Pts',(-2.81085726200006,11.6,10.310530282));
#230710=CARTESIAN_POINT('Ctrl Pts',(-2.81083392800006,15.2,10.308168934));
#230711=CARTESIAN_POINT('Ctrl Pts',(-2.81083392800006,11.6,10.308168934));
#230712=CARTESIAN_POINT('Ctrl Pts',(-2.81080860300006,15.2,10.305814004));
#230713=CARTESIAN_POINT('Ctrl Pts',(-2.81080860300006,11.6,10.305814004));
#230714=CARTESIAN_POINT('Ctrl Pts',(-2.81078129900005,15.2,10.303465504));
#230715=CARTESIAN_POINT('Ctrl Pts',(-2.81078129900005,11.6,10.303465504));
#230716=CARTESIAN_POINT('Ctrl Pts',(-2.81075202400006,15.2,10.301123445));
#230717=CARTESIAN_POINT('Ctrl Pts',(-2.81075202400006,11.6,10.301123445));
#230718=CARTESIAN_POINT('Ctrl Pts',(-2.81072078900006,15.2,10.298787841));
#230719=CARTESIAN_POINT('Ctrl Pts',(-2.81072078900006,11.6,10.298787841));
#230720=CARTESIAN_POINT('Ctrl Pts',(-2.81068760400006,15.2,10.296458705));
#230721=CARTESIAN_POINT('Ctrl Pts',(-2.81068760400006,11.6,10.296458705));
#230722=CARTESIAN_POINT('Ctrl Pts',(-2.81065248000006,15.2,10.29413605));
#230723=CARTESIAN_POINT('Ctrl Pts',(-2.81065248000006,11.6,10.29413605));
#230724=CARTESIAN_POINT('Ctrl Pts',(-2.81061542500006,15.2,10.291819888));
#230725=CARTESIAN_POINT('Ctrl Pts',(-2.81061542500006,11.6,10.291819888));
#230726=CARTESIAN_POINT('Ctrl Pts',(-2.81057645100006,15.2,10.289510232));
#230727=CARTESIAN_POINT('Ctrl Pts',(-2.81057645100006,11.6,10.289510232));
#230728=CARTESIAN_POINT('Ctrl Pts',(-2.81053556900006,15.2,10.287207096));
#230729=CARTESIAN_POINT('Ctrl Pts',(-2.81053556900006,11.6,10.287207096));
#230730=CARTESIAN_POINT('Ctrl Pts',(-2.81049278700006,15.2,10.284910491));
#230731=CARTESIAN_POINT('Ctrl Pts',(-2.81049278700006,11.6,10.284910491));
#230732=CARTESIAN_POINT('Ctrl Pts',(-2.81044811600006,15.2,10.282620433));
#230733=CARTESIAN_POINT('Ctrl Pts',(-2.81044811600006,11.6,10.282620433));
#230734=CARTESIAN_POINT('Ctrl Pts',(-2.81040156900006,15.2,10.280336931));
#230735=CARTESIAN_POINT('Ctrl Pts',(-2.81040156900006,11.6,10.280336931));
#230736=CARTESIAN_POINT('Ctrl Pts',(-2.81035315300006,15.2,10.278060001));
#230737=CARTESIAN_POINT('Ctrl Pts',(-2.81035315300006,11.6,10.278060001));
#230738=CARTESIAN_POINT('Ctrl Pts',(-2.81030288100005,15.2,10.275789656));
#230739=CARTESIAN_POINT('Ctrl Pts',(-2.81030288100005,11.6,10.275789656));
#230740=CARTESIAN_POINT('Ctrl Pts',(-2.81025076100006,15.2,10.273525909));
#230741=CARTESIAN_POINT('Ctrl Pts',(-2.81025076100006,11.6,10.273525909));
#230742=CARTESIAN_POINT('Ctrl Pts',(-2.81019680700005,15.2,10.271268772));
#230743=CARTESIAN_POINT('Ctrl Pts',(-2.81019680700005,11.6,10.271268772));
#230744=CARTESIAN_POINT('Ctrl Pts',(-2.81014102700006,15.2,10.269018258));
#230745=CARTESIAN_POINT('Ctrl Pts',(-2.81014102700006,11.6,10.269018258));
#230746=CARTESIAN_POINT('Ctrl Pts',(-2.81008343200006,15.2,10.266774382));
#230747=CARTESIAN_POINT('Ctrl Pts',(-2.81008343200006,11.6,10.266774382));
#230748=CARTESIAN_POINT('Ctrl Pts',(-2.81002403300006,15.2,10.264537156));
#230749=CARTESIAN_POINT('Ctrl Pts',(-2.81002403300006,11.6,10.264537156));
#230750=CARTESIAN_POINT('Ctrl Pts',(-2.80996284200006,15.2,10.262306594));
#230751=CARTESIAN_POINT('Ctrl Pts',(-2.80996284200006,11.6,10.262306594));
#230752=CARTESIAN_POINT('Ctrl Pts',(-2.80989986700006,15.2,10.260082708));
#230753=CARTESIAN_POINT('Ctrl Pts',(-2.80989986700006,11.6,10.260082708));
#230754=CARTESIAN_POINT('Ctrl Pts',(-2.80983512200006,15.2,10.257865513));
#230755=CARTESIAN_POINT('Ctrl Pts',(-2.80983512200006,11.6,10.257865513));
#230756=CARTESIAN_POINT('Ctrl Pts',(-2.80976861600006,15.2,10.255655021));
#230757=CARTESIAN_POINT('Ctrl Pts',(-2.80976861600006,11.6,10.255655021));
#230758=CARTESIAN_POINT('Ctrl Pts',(-2.80970036000005,15.2,10.253451246));
#230759=CARTESIAN_POINT('Ctrl Pts',(-2.80970036000005,11.6,10.253451246));
#230760=CARTESIAN_POINT('Ctrl Pts',(-2.80963036400005,15.2,10.251254202));
#230761=CARTESIAN_POINT('Ctrl Pts',(-2.80963036400005,11.6,10.251254202));
#230762=CARTESIAN_POINT('Ctrl Pts',(-2.80955864200005,15.2,10.249063902));
#230763=CARTESIAN_POINT('Ctrl Pts',(-2.80955864200005,11.6,10.249063902));
#230764=CARTESIAN_POINT('Ctrl Pts',(-2.80948520300006,15.2,10.246880359));
#230765=CARTESIAN_POINT('Ctrl Pts',(-2.80948520300006,11.6,10.246880359));
#230766=CARTESIAN_POINT('Ctrl Pts',(-2.80941005800006,15.2,10.244703588));
#230767=CARTESIAN_POINT('Ctrl Pts',(-2.80941005800006,11.6,10.244703588));
#230768=CARTESIAN_POINT('Ctrl Pts',(-2.80933321800005,15.2,10.242533601));
#230769=CARTESIAN_POINT('Ctrl Pts',(-2.80933321800005,11.6,10.242533601));
#230770=CARTESIAN_POINT('Ctrl Pts',(-2.80925469500006,15.2,10.240370412));
#230771=CARTESIAN_POINT('Ctrl Pts',(-2.80925469500006,11.6,10.240370412));
#230772=CARTESIAN_POINT('Ctrl Pts',(-2.80917450000006,15.2,10.238214036));
#230773=CARTESIAN_POINT('Ctrl Pts',(-2.80917450000006,11.6,10.238214036));
#230774=CARTESIAN_POINT('Ctrl Pts',(-2.80909264400006,15.2,10.236064484));
#230775=CARTESIAN_POINT('Ctrl Pts',(-2.80909264400006,11.6,10.236064484));
#230776=CARTESIAN_POINT('Ctrl Pts',(-2.80900913900005,15.2,10.233921772));
#230777=CARTESIAN_POINT('Ctrl Pts',(-2.80900913900005,11.6,10.233921772));
#230778=CARTESIAN_POINT('Ctrl Pts',(-2.80892399400006,15.2,10.231785914));
#230779=CARTESIAN_POINT('Ctrl Pts',(-2.80892399400006,11.6,10.231785914));
#230780=CARTESIAN_POINT('Ctrl Pts',(-2.80883722400006,15.2,10.229656922));
#230781=CARTESIAN_POINT('Ctrl Pts',(-2.80883722400006,11.6,10.229656922));
#230782=CARTESIAN_POINT('Ctrl Pts',(-2.80874883800006,15.2,10.227534811));
#230783=CARTESIAN_POINT('Ctrl Pts',(-2.80874883800006,11.6,10.227534811));
#230784=CARTESIAN_POINT('Ctrl Pts',(-2.80865884800006,15.2,10.225419595));
#230785=CARTESIAN_POINT('Ctrl Pts',(-2.80865884800006,11.6,10.225419595));
#230786=CARTESIAN_POINT('Ctrl Pts',(-2.80856726600006,15.2,10.223311287));
#230787=CARTESIAN_POINT('Ctrl Pts',(-2.80856726600006,11.6,10.223311287));
#230788=CARTESIAN_POINT('Ctrl Pts',(-2.80847410200006,15.2,10.221209902));
#230789=CARTESIAN_POINT('Ctrl Pts',(-2.80847410200006,11.6,10.221209902));
#230790=CARTESIAN_POINT('Ctrl Pts',(-2.80837937000005,15.2,10.219115454));
#230791=CARTESIAN_POINT('Ctrl Pts',(-2.80837937000005,11.6,10.219115454));
#230792=CARTESIAN_POINT('Ctrl Pts',(-2.80828308100005,15.2,10.217027956));
#230793=CARTESIAN_POINT('Ctrl Pts',(-2.80828308100005,11.6,10.217027956));
#230794=CARTESIAN_POINT('Ctrl Pts',(-2.80818524500006,15.2,10.214947422));
#230795=CARTESIAN_POINT('Ctrl Pts',(-2.80818524500006,11.6,10.214947422));
#230796=CARTESIAN_POINT('Ctrl Pts',(-2.80808587600006,15.2,10.212873868));
#230797=CARTESIAN_POINT('Ctrl Pts',(-2.80808587600006,11.6,10.212873868));
#230798=CARTESIAN_POINT('Ctrl Pts',(-2.80798498400006,15.2,10.210807306));
#230799=CARTESIAN_POINT('Ctrl Pts',(-2.80798498400006,11.6,10.210807306));
#230800=CARTESIAN_POINT('Ctrl Pts',(-2.80788258200006,15.2,10.208747751));
#230801=CARTESIAN_POINT('Ctrl Pts',(-2.80788258200006,11.6,10.208747751));
#230802=CARTESIAN_POINT('Ctrl Pts',(-2.80777868100006,15.2,10.206695219));
#230803=CARTESIAN_POINT('Ctrl Pts',(-2.80777868100006,11.6,10.206695219));
#230804=CARTESIAN_POINT('Ctrl Pts',(-2.80767329400006,15.2,10.20464972));
#230805=CARTESIAN_POINT('Ctrl Pts',(-2.80767329400006,11.6,10.20464972));
#230806=CARTESIAN_POINT('Ctrl Pts',(-2.80756643200006,15.2,10.202611273));
#230807=CARTESIAN_POINT('Ctrl Pts',(-2.80756643200006,11.6,10.202611273));
#230808=CARTESIAN_POINT('Ctrl Pts',(-2.80745810900005,15.2,10.200579889));
#230809=CARTESIAN_POINT('Ctrl Pts',(-2.80745810900005,11.6,10.200579889));
#230810=CARTESIAN_POINT('Ctrl Pts',(-2.80734833500006,15.2,10.198555584));
#230811=CARTESIAN_POINT('Ctrl Pts',(-2.80734833500006,11.6,10.198555584));
#230812=CARTESIAN_POINT('Ctrl Pts',(-2.80723712200006,15.2,10.196538372));
#230813=CARTESIAN_POINT('Ctrl Pts',(-2.80723712200006,11.6,10.196538372));
#230814=CARTESIAN_POINT('Ctrl Pts',(-2.80712448400006,15.2,10.194528266));
#230815=CARTESIAN_POINT('Ctrl Pts',(-2.80712448400006,11.6,10.194528266));
#230816=CARTESIAN_POINT('Ctrl Pts',(-2.80701043200006,15.2,10.192525284));
#230817=CARTESIAN_POINT('Ctrl Pts',(-2.80701043200006,11.6,10.192525284));
#230818=CARTESIAN_POINT('Ctrl Pts',(-2.80689497900006,15.2,10.190529438));
#230819=CARTESIAN_POINT('Ctrl Pts',(-2.80689497900006,11.6,10.190529438));
#230820=CARTESIAN_POINT('Ctrl Pts',(-2.80677813600006,15.2,10.188540742));
#230821=CARTESIAN_POINT('Ctrl Pts',(-2.80677813600006,11.6,10.188540742));
#230822=CARTESIAN_POINT('Ctrl Pts',(-2.80665991800006,15.2,10.186559212));
#230823=CARTESIAN_POINT('Ctrl Pts',(-2.80665991800006,11.6,10.186559212));
#230824=CARTESIAN_POINT('Ctrl Pts',(-2.80654033400006,15.2,10.184584864));
#230825=CARTESIAN_POINT('Ctrl Pts',(-2.80654033400006,11.6,10.184584864));
#230826=CARTESIAN_POINT('Ctrl Pts',(-2.80641939900006,15.2,10.182617709));
#230827=CARTESIAN_POINT('Ctrl Pts',(-2.80641939900006,11.6,10.182617709));
#230828=CARTESIAN_POINT('Ctrl Pts',(-2.80629712500006,15.2,10.180657765));
#230829=CARTESIAN_POINT('Ctrl Pts',(-2.80629712500006,11.6,10.180657765));
#230830=CARTESIAN_POINT('Ctrl Pts',(-2.80617352500005,15.2,10.178705045));
#230831=CARTESIAN_POINT('Ctrl Pts',(-2.80617352500005,11.6,10.178705045));
#230832=CARTESIAN_POINT('Ctrl Pts',(-2.80604861100006,15.2,10.176759565));
#230833=CARTESIAN_POINT('Ctrl Pts',(-2.80604861100006,11.6,10.176759565));
#230834=CARTESIAN_POINT('Ctrl Pts',(-2.80592239500006,15.2,10.174821339));
#230835=CARTESIAN_POINT('Ctrl Pts',(-2.80592239500006,11.6,10.174821339));
#230836=CARTESIAN_POINT('Ctrl Pts',(-2.80579489100006,15.2,10.172890382));
#230837=CARTESIAN_POINT('Ctrl Pts',(-2.80579489100006,11.6,10.172890382));
#230838=CARTESIAN_POINT('Ctrl Pts',(-2.80566611200006,15.2,10.170966709));
#230839=CARTESIAN_POINT('Ctrl Pts',(-2.80566611200006,11.6,10.170966709));
#230840=CARTESIAN_POINT('Ctrl Pts',(-2.80553607000006,15.2,10.169050336));
#230841=CARTESIAN_POINT('Ctrl Pts',(-2.80553607000006,11.6,10.169050336));
#230842=CARTESIAN_POINT('Ctrl Pts',(-2.80540477700006,15.2,10.167141276));
#230843=CARTESIAN_POINT('Ctrl Pts',(-2.80540477700006,11.6,10.167141276));
#230844=CARTESIAN_POINT('Ctrl Pts',(-2.80527224900006,15.2,10.165239546));
#230845=CARTESIAN_POINT('Ctrl Pts',(-2.80527224900006,11.6,10.165239546));
#230846=CARTESIAN_POINT('Ctrl Pts',(-2.80513849700006,15.2,10.16334516));
#230847=CARTESIAN_POINT('Ctrl Pts',(-2.80513849700006,11.6,10.16334516));
#230848=CARTESIAN_POINT('Ctrl Pts',(-2.80500353400006,15.2,10.161458135));
#230849=CARTESIAN_POINT('Ctrl Pts',(-2.80500353400006,11.6,10.161458135));
#230850=CARTESIAN_POINT('Ctrl Pts',(-2.80486737300006,15.2,10.159578484));
#230851=CARTESIAN_POINT('Ctrl Pts',(-2.80486737300006,11.6,10.159578484));
#230852=CARTESIAN_POINT('Ctrl Pts',(-2.80473002900006,15.2,10.157706223));
#230853=CARTESIAN_POINT('Ctrl Pts',(-2.80473002900006,11.6,10.157706223));
#230854=CARTESIAN_POINT('Ctrl Pts',(-2.80459151300006,15.2,10.155841368));
#230855=CARTESIAN_POINT('Ctrl Pts',(-2.80459151300006,11.6,10.155841368));
#230856=CARTESIAN_POINT('Ctrl Pts',(-2.80445184000006,15.2,10.153983933));
#230857=CARTESIAN_POINT('Ctrl Pts',(-2.80445184000006,11.6,10.153983933));
#230858=CARTESIAN_POINT('Ctrl Pts',(-2.80431102200006,15.2,10.152133935));
#230859=CARTESIAN_POINT('Ctrl Pts',(-2.80431102200006,11.6,10.152133935));
#230860=CARTESIAN_POINT('Ctrl Pts',(-2.80416907300005,15.2,10.150291389));
#230861=CARTESIAN_POINT('Ctrl Pts',(-2.80416907300005,11.6,10.150291389));
#230862=CARTESIAN_POINT('Ctrl Pts',(-2.80402600700006,15.2,10.14845631));
#230863=CARTESIAN_POINT('Ctrl Pts',(-2.80402600700006,11.6,10.14845631));
#230864=CARTESIAN_POINT('Ctrl Pts',(-2.80388183800006,15.2,10.146628712));
#230865=CARTESIAN_POINT('Ctrl Pts',(-2.80388183800006,11.6,10.146628712));
#230866=CARTESIAN_POINT('Ctrl Pts',(-2.80373657700005,15.2,10.144808615));
#230867=CARTESIAN_POINT('Ctrl Pts',(-2.80373657700005,11.6,10.144808615));
#230868=CARTESIAN_POINT('Ctrl Pts',(-2.80359024100005,15.2,10.142996029));
#230869=CARTESIAN_POINT('Ctrl Pts',(-2.80359024100005,11.6,10.142996029));
#230870=CARTESIAN_POINT('Ctrl Pts',(-2.80344284000006,15.2,10.141190975));
#230871=CARTESIAN_POINT('Ctrl Pts',(-2.80344284000006,11.6,10.141190975));
#230872=CARTESIAN_POINT('Ctrl Pts',(-2.80329439200006,15.2,10.139393467));
#230873=CARTESIAN_POINT('Ctrl Pts',(-2.80329439200006,11.6,10.139393467));
#230874=CARTESIAN_POINT('Ctrl Pts',(-2.80314490700006,15.2,10.137603518));
#230875=CARTESIAN_POINT('Ctrl Pts',(-2.80314490700006,11.6,10.137603518));
#230876=CARTESIAN_POINT('Ctrl Pts',(-2.80299440200006,15.2,10.135821147));
#230877=CARTESIAN_POINT('Ctrl Pts',(-2.80299440200006,11.6,10.135821147));
#230878=CARTESIAN_POINT('Ctrl Pts',(-2.80284288900006,15.2,10.134046369));
#230879=CARTESIAN_POINT('Ctrl Pts',(-2.80284288900006,11.6,10.134046369));
#230880=CARTESIAN_POINT('Ctrl Pts',(-2.80269038200006,15.2,10.1322792));
#230881=CARTESIAN_POINT('Ctrl Pts',(-2.80269038200006,11.6,10.1322792));
#230882=CARTESIAN_POINT('Ctrl Pts',(-2.80253689600006,15.2,10.130519656));
#230883=CARTESIAN_POINT('Ctrl Pts',(-2.80253689600006,11.6,10.130519656));
#230884=CARTESIAN_POINT('Ctrl Pts',(-2.80238244500006,15.2,10.128767753));
#230885=CARTESIAN_POINT('Ctrl Pts',(-2.80238244500006,11.6,10.128767753));
#230886=CARTESIAN_POINT('Ctrl Pts',(-2.80222704300006,15.2,10.127023506));
#230887=CARTESIAN_POINT('Ctrl Pts',(-2.80222704300006,11.6,10.127023506));
#230888=CARTESIAN_POINT('Ctrl Pts',(-2.80207070500006,15.2,10.125286933));
#230889=CARTESIAN_POINT('Ctrl Pts',(-2.80207070500006,11.6,10.125286933));
#230890=CARTESIAN_POINT('Ctrl Pts',(-2.80191344400006,15.2,10.123558049));
#230891=CARTESIAN_POINT('Ctrl Pts',(-2.80191344400006,11.6,10.123558049));
#230892=CARTESIAN_POINT('Ctrl Pts',(-2.80175527400006,15.2,10.121836872));
#230893=CARTESIAN_POINT('Ctrl Pts',(-2.80175527400006,11.6,10.121836872));
#230894=CARTESIAN_POINT('Ctrl Pts',(-2.80159621100006,15.2,10.120123415));
#230895=CARTESIAN_POINT('Ctrl Pts',(-2.80159621100006,11.6,10.120123415));
#230896=CARTESIAN_POINT('Ctrl Pts',(-2.80143627000006,15.2,10.118417697));
#230897=CARTESIAN_POINT('Ctrl Pts',(-2.80143627000006,11.6,10.118417697));
#230898=CARTESIAN_POINT('Ctrl Pts',(-2.80127546300006,15.2,10.116719734));
#230899=CARTESIAN_POINT('Ctrl Pts',(-2.80127546300006,11.6,10.116719734));
#230900=CARTESIAN_POINT('Ctrl Pts',(-2.80111380600006,15.2,10.115029541));
#230901=CARTESIAN_POINT('Ctrl Pts',(-2.80111380600006,11.6,10.115029541));
#230902=CARTESIAN_POINT('Ctrl Pts',(-2.80095131400006,15.2,10.113347136));
#230903=CARTESIAN_POINT('Ctrl Pts',(-2.80095131400006,11.6,10.113347136));
#230904=CARTESIAN_POINT('Ctrl Pts',(-2.80078800200006,15.2,10.111672537));
#230905=CARTESIAN_POINT('Ctrl Pts',(-2.80078800200006,11.6,10.111672537));
#230906=CARTESIAN_POINT('Ctrl Pts',(-2.80062388500005,15.2,10.110005756));
#230907=CARTESIAN_POINT('Ctrl Pts',(-2.80062388500005,11.6,10.110005756));
#230908=CARTESIAN_POINT('Ctrl Pts',(-2.80045897700006,15.2,10.108346814));
#230909=CARTESIAN_POINT('Ctrl Pts',(-2.80045897700006,11.6,10.108346814));
#230910=CARTESIAN_POINT('Ctrl Pts',(-2.80029329300006,15.2,10.106695726));
#230911=CARTESIAN_POINT('Ctrl Pts',(-2.80029329300006,11.6,10.106695726));
#230912=CARTESIAN_POINT('Ctrl Pts',(-2.80012684900006,15.2,10.105052508));
#230913=CARTESIAN_POINT('Ctrl Pts',(-2.80012684900006,11.6,10.105052508));
#230914=CARTESIAN_POINT('Ctrl Pts',(-2.79995965900006,15.2,10.103417179));
#230915=CARTESIAN_POINT('Ctrl Pts',(-2.79995965900006,11.6,10.103417179));
#230916=CARTESIAN_POINT('Ctrl Pts',(-2.79979173800006,15.2,10.101789754));
#230917=CARTESIAN_POINT('Ctrl Pts',(-2.79979173800006,11.6,10.101789754));
#230918=CARTESIAN_POINT('Ctrl Pts',(-2.79962310200006,15.2,10.100170251));
#230919=CARTESIAN_POINT('Ctrl Pts',(-2.79962310200006,11.6,10.100170251));
#230920=CARTESIAN_POINT('Ctrl Pts',(-2.79945376700006,15.2,10.098558686));
#230921=CARTESIAN_POINT('Ctrl Pts',(-2.79945376700006,11.6,10.098558686));
#230922=CARTESIAN_POINT('Ctrl Pts',(-2.79928374700006,15.2,10.096955078));
#230923=CARTESIAN_POINT('Ctrl Pts',(-2.79928374700006,11.6,10.096955078));
#230924=CARTESIAN_POINT('Ctrl Pts',(-2.79911305800006,15.2,10.095359441));
#230925=CARTESIAN_POINT('Ctrl Pts',(-2.79911305800006,11.6,10.095359441));
#230926=CARTESIAN_POINT('Ctrl Pts',(-2.79894171600006,15.2,10.093771795));
#230927=CARTESIAN_POINT('Ctrl Pts',(-2.79894171600006,11.6,10.093771795));
#230928=CARTESIAN_POINT('Ctrl Pts',(-2.79876973600006,15.2,10.092192157));
#230929=CARTESIAN_POINT('Ctrl Pts',(-2.79876973600006,11.6,10.092192157));
#230930=CARTESIAN_POINT('Ctrl Pts',(-2.79859713300006,15.2,10.090620543));
#230931=CARTESIAN_POINT('Ctrl Pts',(-2.79859713300006,11.6,10.090620543));
#230932=CARTESIAN_POINT('Ctrl Pts',(-2.79842392400006,15.2,10.08905697));
#230933=CARTESIAN_POINT('Ctrl Pts',(-2.79842392400006,11.6,10.08905697));
#230934=CARTESIAN_POINT('Ctrl Pts',(-2.79825012400006,15.2,10.087501457));
#230935=CARTESIAN_POINT('Ctrl Pts',(-2.79825012400006,11.6,10.087501457));
#230936=CARTESIAN_POINT('Ctrl Pts',(-2.79807575000006,15.2,10.08595402));
#230937=CARTESIAN_POINT('Ctrl Pts',(-2.79807575000006,11.6,10.08595402));
#230938=CARTESIAN_POINT('Ctrl Pts',(-2.79790081600006,15.2,10.084414678));
#230939=CARTESIAN_POINT('Ctrl Pts',(-2.79790081600006,11.6,10.084414678));
#230940=CARTESIAN_POINT('Ctrl Pts',(-2.79772533900006,15.2,10.082883449));
#230941=CARTESIAN_POINT('Ctrl Pts',(-2.79772533900006,11.6,10.082883449));
#230942=CARTESIAN_POINT('Ctrl Pts',(-2.79754933700006,15.2,10.081360348));
#230943=CARTESIAN_POINT('Ctrl Pts',(-2.79754933700006,11.6,10.081360348));
#230944=CARTESIAN_POINT('Ctrl Pts',(-2.79737282200006,15.2,10.079845395));
#230945=CARTESIAN_POINT('Ctrl Pts',(-2.79737282200006,11.6,10.079845395));
#230946=CARTESIAN_POINT('Ctrl Pts',(-2.79719581400005,15.2,10.078338606));
#230947=CARTESIAN_POINT('Ctrl Pts',(-2.79719581400005,11.6,10.078338606));
#230948=CARTESIAN_POINT('Ctrl Pts',(-2.79701832900006,15.2,10.076840001));
#230949=CARTESIAN_POINT('Ctrl Pts',(-2.79701832900006,11.6,10.076840001));
#230950=CARTESIAN_POINT('Ctrl Pts',(-2.79684038000005,15.2,10.075349597));
#230951=CARTESIAN_POINT('Ctrl Pts',(-2.79684038000005,11.6,10.075349597));
#230952=CARTESIAN_POINT('Ctrl Pts',(-2.79666198700005,15.2,10.073867411));
#230953=CARTESIAN_POINT('Ctrl Pts',(-2.79666198700005,11.6,10.073867411));
#230954=CARTESIAN_POINT('Ctrl Pts',(-2.79648316500006,15.2,10.072393463));
#230955=CARTESIAN_POINT('Ctrl Pts',(-2.79648316500006,11.6,10.072393463));
#230956=CARTESIAN_POINT('Ctrl Pts',(-2.79630393100006,15.2,10.070927768));
#230957=CARTESIAN_POINT('Ctrl Pts',(-2.79630393100006,11.6,10.070927768));
#230958=CARTESIAN_POINT('Ctrl Pts',(-2.79612430200006,15.2,10.069470348));
#230959=CARTESIAN_POINT('Ctrl Pts',(-2.79612430200006,11.6,10.069470348));
#230960=CARTESIAN_POINT('Ctrl Pts',(-2.79594429400006,15.2,10.068021219));
#230961=CARTESIAN_POINT('Ctrl Pts',(-2.79594429400006,11.6,10.068021219));
#230962=CARTESIAN_POINT('Ctrl Pts',(-2.79576392500006,15.2,10.066580399));
#230963=CARTESIAN_POINT('Ctrl Pts',(-2.79576392500006,11.6,10.066580399));
#230964=CARTESIAN_POINT('Ctrl Pts',(-2.79558321100006,15.2,10.065147907));
#230965=CARTESIAN_POINT('Ctrl Pts',(-2.79558321100006,11.6,10.065147907));
#230966=CARTESIAN_POINT('Ctrl Pts',(-2.79540216900006,15.2,10.063723762));
#230967=CARTESIAN_POINT('Ctrl Pts',(-2.79540216900006,11.6,10.063723762));
#230968=CARTESIAN_POINT('Ctrl Pts',(-2.79522081700006,15.2,10.062307981));
#230969=CARTESIAN_POINT('Ctrl Pts',(-2.79522081700006,11.6,10.062307981));
#230970=CARTESIAN_POINT('Ctrl Pts',(-2.79503917100006,15.2,10.060900584));
#230971=CARTESIAN_POINT('Ctrl Pts',(-2.79503917100006,11.6,10.060900584));
#230972=CARTESIAN_POINT('Ctrl Pts',(-2.79485724900006,15.2,10.05950159));
#230973=CARTESIAN_POINT('Ctrl Pts',(-2.79485724900006,11.6,10.05950159));
#230974=CARTESIAN_POINT('Ctrl Pts',(-2.79467506800006,15.2,10.058111017));
#230975=CARTESIAN_POINT('Ctrl Pts',(-2.79467506800006,11.6,10.058111017));
#230976=CARTESIAN_POINT('Ctrl Pts',(-2.79449264500006,15.2,10.056728882));
#230977=CARTESIAN_POINT('Ctrl Pts',(-2.79449264500006,11.6,10.056728882));
#230978=CARTESIAN_POINT('Ctrl Pts',(-2.79431000000006,15.2,10.055355206));
#230979=CARTESIAN_POINT('Ctrl Pts',(-2.79431000000006,11.6,10.055355206));
#230980=CARTESIAN_POINT('Ctrl Pts',(-2.79412714700006,15.2,10.053990008));
#230981=CARTESIAN_POINT('Ctrl Pts',(-2.79412714700006,11.6,10.053990008));
#230982=CARTESIAN_POINT('Ctrl Pts',(-2.79394410600006,15.2,10.052633307));
#230983=CARTESIAN_POINT('Ctrl Pts',(-2.79394410600006,11.6,10.052633307));
#230984=CARTESIAN_POINT('Ctrl Pts',(-2.79376089400006,15.2,10.05128512));
#230985=CARTESIAN_POINT('Ctrl Pts',(-2.79376089400006,11.6,10.05128512));
#230986=CARTESIAN_POINT('Ctrl Pts',(-2.79357752900005,15.2,10.049945468));
#230987=CARTESIAN_POINT('Ctrl Pts',(-2.79357752900005,11.6,10.049945468));
#230988=CARTESIAN_POINT('Ctrl Pts',(-2.79339402900006,15.2,10.048614371));
#230989=CARTESIAN_POINT('Ctrl Pts',(-2.79339402900006,11.6,10.048614371));
#230990=CARTESIAN_POINT('Ctrl Pts',(-2.79321041200005,15.2,10.047291846));
#230991=CARTESIAN_POINT('Ctrl Pts',(-2.79321041200005,11.6,10.047291846));
#230992=CARTESIAN_POINT('Ctrl Pts',(-2.79302669600006,15.2,10.045977913));
#230993=CARTESIAN_POINT('Ctrl Pts',(-2.79302669600006,11.6,10.045977913));
#230994=CARTESIAN_POINT('Ctrl Pts',(-2.79284290000006,15.2,10.044672593));
#230995=CARTESIAN_POINT('Ctrl Pts',(-2.79284290000006,11.6,10.044672593));
#230996=CARTESIAN_POINT('Ctrl Pts',(-2.79265904100006,15.2,10.043375903));
#230997=CARTESIAN_POINT('Ctrl Pts',(-2.79265904100006,11.6,10.043375903));
#230998=CARTESIAN_POINT('Ctrl Pts',(-2.79247513800006,15.2,10.042087865));
#230999=CARTESIAN_POINT('Ctrl Pts',(-2.79247513800006,11.6,10.042087865));
#231000=CARTESIAN_POINT('Ctrl Pts',(-2.79229120900006,15.2,10.040808498));
#231001=CARTESIAN_POINT('Ctrl Pts',(-2.79229120900006,11.6,10.040808498));
#231002=CARTESIAN_POINT('Ctrl Pts',(-2.79210727300006,15.2,10.03953782));
#231003=CARTESIAN_POINT('Ctrl Pts',(-2.79210727300006,11.6,10.03953782));
#231004=CARTESIAN_POINT('Ctrl Pts',(-2.79192335000006,15.2,10.038275854));
#231005=CARTESIAN_POINT('Ctrl Pts',(-2.79192335000006,11.6,10.038275854));
#231006=CARTESIAN_POINT('Ctrl Pts',(-2.79173945700005,15.2,10.037022616));
#231007=CARTESIAN_POINT('Ctrl Pts',(-2.79173945700005,11.6,10.037022616));
#231008=CARTESIAN_POINT('Ctrl Pts',(-2.79155561200006,15.2,10.035778129));
#231009=CARTESIAN_POINT('Ctrl Pts',(-2.79155561200006,11.6,10.035778129));
#231010=CARTESIAN_POINT('Ctrl Pts',(-2.79137183700006,15.2,10.034542412));
#231011=CARTESIAN_POINT('Ctrl Pts',(-2.79137183700006,11.6,10.034542412));
#231012=CARTESIAN_POINT('Ctrl Pts',(-2.79118814900006,15.2,10.033315486));
#231013=CARTESIAN_POINT('Ctrl Pts',(-2.79118814900006,11.6,10.033315486));
#231014=CARTESIAN_POINT('Ctrl Pts',(-2.79100456600006,15.2,10.032097369));
#231015=CARTESIAN_POINT('Ctrl Pts',(-2.79100456600006,11.6,10.032097369));
#231016=CARTESIAN_POINT('Ctrl Pts',(-2.79082110900006,15.2,10.030888083));
#231017=CARTESIAN_POINT('Ctrl Pts',(-2.79082110900006,11.6,10.030888083));
#231018=CARTESIAN_POINT('Ctrl Pts',(-2.79063779700006,15.2,10.029687649));
#231019=CARTESIAN_POINT('Ctrl Pts',(-2.79063779700006,11.6,10.029687649));
#231020=CARTESIAN_POINT('Ctrl Pts',(-2.79045465000006,15.2,10.028496085));
#231021=CARTESIAN_POINT('Ctrl Pts',(-2.79045465000006,11.6,10.028496085));
#231022=CARTESIAN_POINT('Ctrl Pts',(-2.79027168600006,15.2,10.027313415));
#231023=CARTESIAN_POINT('Ctrl Pts',(-2.79027168600006,11.6,10.027313415));
#231024=CARTESIAN_POINT('Ctrl Pts',(-2.79008892600006,15.2,10.026139656));
#231025=CARTESIAN_POINT('Ctrl Pts',(-2.79008892600006,11.6,10.026139656));
#231026=CARTESIAN_POINT('Ctrl Pts',(-2.78990639000006,15.2,10.024974832));
#231027=CARTESIAN_POINT('Ctrl Pts',(-2.78990639000006,11.6,10.024974832));
#231028=CARTESIAN_POINT('Ctrl Pts',(-2.78972409600006,15.2,10.023818962));
#231029=CARTESIAN_POINT('Ctrl Pts',(-2.78972409600006,11.6,10.023818962));
#231030=CARTESIAN_POINT('Ctrl Pts',(-2.78954206500006,15.2,10.022672066));
#231031=CARTESIAN_POINT('Ctrl Pts',(-2.78954206500006,11.6,10.022672066));
#231032=CARTESIAN_POINT('Ctrl Pts',(-2.78936031700006,15.2,10.021534166));
#231033=CARTESIAN_POINT('Ctrl Pts',(-2.78936031700006,11.6,10.021534166));
#231034=CARTESIAN_POINT('Ctrl Pts',(-2.78917887200006,15.2,10.020405283));
#231035=CARTESIAN_POINT('Ctrl Pts',(-2.78917887200006,11.6,10.020405283));
#231036=CARTESIAN_POINT('Ctrl Pts',(-2.78899775000006,15.2,10.01928544));
#231037=CARTESIAN_POINT('Ctrl Pts',(-2.78899775000006,11.6,10.01928544));
#231038=CARTESIAN_POINT('Ctrl Pts',(-2.78881697200006,15.2,10.018174655));
#231039=CARTESIAN_POINT('Ctrl Pts',(-2.78881697200006,11.6,10.018174655));
#231040=CARTESIAN_POINT('Ctrl Pts',(-2.78863655900006,15.2,10.017072951));
#231041=CARTESIAN_POINT('Ctrl Pts',(-2.78863655900006,11.6,10.017072951));
#231042=CARTESIAN_POINT('Ctrl Pts',(-2.78845652900006,15.2,10.015980349));
#231043=CARTESIAN_POINT('Ctrl Pts',(-2.78845652900006,11.6,10.015980349));
#231044=CARTESIAN_POINT('Ctrl Pts',(-2.78827690500006,15.2,10.014896871));
#231045=CARTESIAN_POINT('Ctrl Pts',(-2.78827690500006,11.6,10.014896871));
#231046=CARTESIAN_POINT('Ctrl Pts',(-2.78809770700006,15.2,10.013822538));
#231047=CARTESIAN_POINT('Ctrl Pts',(-2.78809770700006,11.6,10.013822538));
#231048=CARTESIAN_POINT('Ctrl Pts',(-2.78791895500006,15.2,10.012757373));
#231049=CARTESIAN_POINT('Ctrl Pts',(-2.78791895500006,11.6,10.012757373));
#231050=CARTESIAN_POINT('Ctrl Pts',(-2.78774067200006,15.2,10.011701396));
#231051=CARTESIAN_POINT('Ctrl Pts',(-2.78774067200006,11.6,10.011701396));
#231052=CARTESIAN_POINT('Ctrl Pts',(-2.78756287800006,15.2,10.01065463));
#231053=CARTESIAN_POINT('Ctrl Pts',(-2.78756287800006,11.6,10.01065463));
#231054=CARTESIAN_POINT('Ctrl Pts',(-2.78738559300006,15.2,10.009617096));
#231055=CARTESIAN_POINT('Ctrl Pts',(-2.78738559300006,11.6,10.009617096));
#231056=CARTESIAN_POINT('Ctrl Pts',(-2.78720884000006,15.2,10.008588818));
#231057=CARTESIAN_POINT('Ctrl Pts',(-2.78720884000006,11.6,10.008588818));
#231058=CARTESIAN_POINT('Ctrl Pts',(-2.78703264000006,15.2,10.007569816));
#231059=CARTESIAN_POINT('Ctrl Pts',(-2.78703264000006,11.6,10.007569816));
#231060=CARTESIAN_POINT('Ctrl Pts',(-2.78685701500006,15.2,10.006560113));
#231061=CARTESIAN_POINT('Ctrl Pts',(-2.78685701500006,11.6,10.006560113));
#231062=CARTESIAN_POINT('Ctrl Pts',(-2.78668198600006,15.2,10.005559731));
#231063=CARTESIAN_POINT('Ctrl Pts',(-2.78668198600006,11.6,10.005559731));
#231064=CARTESIAN_POINT('Ctrl Pts',(-2.78650757400006,15.2,10.004568694));
#231065=CARTESIAN_POINT('Ctrl Pts',(-2.78650757400006,11.6,10.004568694));
#231066=CARTESIAN_POINT('Ctrl Pts',(-2.78633380200006,15.2,10.003587023));
#231067=CARTESIAN_POINT('Ctrl Pts',(-2.78633380200006,11.6,10.003587023));
#231068=CARTESIAN_POINT('Ctrl Pts',(-2.78616069100006,15.2,10.002614742));
#231069=CARTESIAN_POINT('Ctrl Pts',(-2.78616069100006,11.6,10.002614742));
#231070=CARTESIAN_POINT('Ctrl Pts',(-2.78598826500006,15.2,10.001651872));
#231071=CARTESIAN_POINT('Ctrl Pts',(-2.78598826500006,11.6,10.001651872));
#231072=CARTESIAN_POINT('Ctrl Pts',(-2.78581654500006,15.2,10.000698438));
#231073=CARTESIAN_POINT('Ctrl Pts',(-2.78581654500006,11.6,10.000698438));
#231074=CARTESIAN_POINT('Ctrl Pts',(-2.78564555300005,15.2,9.99975446099998));
#231075=CARTESIAN_POINT('Ctrl Pts',(-2.78564555300005,11.6,9.99975446099998));
#231076=CARTESIAN_POINT('Ctrl Pts',(-2.78547531100005,15.2,9.99881996499998));
#231077=CARTESIAN_POINT('Ctrl Pts',(-2.78547531100005,11.6,9.99881996499998));
#231078=CARTESIAN_POINT('Ctrl Pts',(-2.78530584400006,15.2,9.99789497199998));
#231079=CARTESIAN_POINT('Ctrl Pts',(-2.78530584400006,11.6,9.99789497199998));
#231080=CARTESIAN_POINT('Ctrl Pts',(-2.78513717300005,15.2,9.99697950799998));
#231081=CARTESIAN_POINT('Ctrl Pts',(-2.78513717300005,11.6,9.99697950799998));
#231082=CARTESIAN_POINT('Ctrl Pts',(-2.78497028700006,15.2,9.99607881099998));
#231083=CARTESIAN_POINT('Ctrl Pts',(-2.78497028700006,11.6,9.99607881099998));
#231084=CARTESIAN_POINT('Ctrl Pts',(-2.78483763600006,15.2,9.99536684699999));
#231085=CARTESIAN_POINT('Ctrl Pts',(-2.78483763600006,11.6,9.99536684699999));
#231086=CARTESIAN_POINT('Ctrl Pts',(-2.78473877000006,15.2,9.99483839999998));
#231087=CARTESIAN_POINT('Ctrl Pts',(-2.78473877000006,11.6,9.99483839999998));
#231088=CARTESIAN_POINT('Ctrl Pts',(-2.78467335000005,15.2,9.99448967799999));
#231089=CARTESIAN_POINT('Ctrl Pts',(-2.78467335000005,11.6,9.99448967799999));
#231090=CARTESIAN_POINT('Ctrl Pts',(-2.78464115900006,15.2,9.99431831799999));
#231091=CARTESIAN_POINT('Ctrl Pts',(-2.78464115900006,11.6,9.99431831799999));
#231092=CARTESIAN_POINT('',(-2.78464115900006,12.2,9.99431831699999));
#231093=CARTESIAN_POINT('',(-2.78464115900006,15.2,9.99431831699999));
#231094=CARTESIAN_POINT('',(-2.78464115900006,12.2,9.99431831699999));
#231095=CARTESIAN_POINT('Ctrl Pts',(-2.71145515300006,12.2,11.175777868));
#231096=CARTESIAN_POINT('Ctrl Pts',(-2.71281861996396,12.2,11.1695539166432));
#231097=CARTESIAN_POINT('Ctrl Pts',(-2.7141664268337,12.2,11.1633453605358));
#231098=CARTESIAN_POINT('Ctrl Pts',(-2.71549860045082,12.2,11.1571522052299));
#231099=CARTESIAN_POINT('Ctrl Pts',(-2.71629790459205,12.2,11.1534363121814));
#231100=CARTESIAN_POINT('Ctrl Pts',(-2.71709157984107,12.2,11.1497259665856));
#231101=CARTESIAN_POINT('Ctrl Pts',(-2.71787964073271,12.2,11.146021201495));
#231102=CARTESIAN_POINT('Ctrl Pts',(-2.71866770162435,12.2,11.1423164364044));
#231103=CARTESIAN_POINT('Ctrl Pts',(-2.71945015054306,12.2,11.1386172539523));
#231104=CARTESIAN_POINT('Ctrl Pts',(-2.72022700793199,12.2,11.1349236969193));
#231105=CARTESIAN_POINT('Ctrl Pts',(-2.72100386532092,12.2,11.1312301398863));
#231106=CARTESIAN_POINT('Ctrl Pts',(-2.72177513241023,12.2,11.1275422097697));
#231107=CARTESIAN_POINT('Ctrl Pts',(-2.7225408290915,12.2,11.1238599450277));
#231108=CARTESIAN_POINT('Ctrl Pts',(-2.72381699027332,12.2,11.1177228369014));
#231109=CARTESIAN_POINT('Ctrl Pts',(-2.72507767193107,12.2,11.1116014639427));
#231110=CARTESIAN_POINT('Ctrl Pts',(-2.72632295664715,12.2,11.1054959789837));
#231111=CARTESIAN_POINT('Ctrl Pts',(-2.72707012744965,12.2,11.1018326881415));
#231112=CARTESIAN_POINT('Ctrl Pts',(-2.72781175456561,12.2,11.0981751182142));
#231113=CARTESIAN_POINT('Ctrl Pts',(-2.72854785787295,12.2,11.0945233075544));
#231114=CARTESIAN_POINT('Ctrl Pts',(-2.72928396131402,12.2,11.0908714962312));
#231115=CARTESIAN_POINT('Ctrl Pts',(-2.73001453998686,12.2,11.0872254438013));
#231116=CARTESIAN_POINT('Ctrl Pts',(-2.73073961488315,12.2,11.0835851884397));
#231117=CARTESIAN_POINT('Ctrl Pts',(-2.73146468964772,12.2,11.0799449337394));
#231118=CARTESIAN_POINT('Ctrl Pts',(-2.73218425928759,12.2,11.0763104755055));
#231119=CARTESIAN_POINT('Ctrl Pts',(-2.7328983425945,12.2,11.0726818498462));
#231120=CARTESIAN_POINT('Ctrl Pts',(-2.73361242590142,12.2,11.0690532241869));
#231121=CARTESIAN_POINT('Ctrl Pts',(-2.73432102293977,12.2,11.0654304316483));
#231122=CARTESIAN_POINT('Ctrl Pts',(-2.73502415275073,12.2,11.0618135084717));
#231123=CARTESIAN_POINT('Ctrl Pts',(-2.73572728256168,12.2,11.058196585295));
#231124=CARTESIAN_POINT('Ctrl Pts',(-2.73642494497144,12.2,11.054585531722));
#231125=CARTESIAN_POINT('Ctrl Pts',(-2.73711715978279,12.2,11.0509803855032));
#231126=CARTESIAN_POINT('Ctrl Pts',(-2.73780937459415,12.2,11.0473752392845));
#231127=CARTESIAN_POINT('Ctrl Pts',(-2.73849614156669,12.2,11.0437760001283));
#231128=CARTESIAN_POINT('Ctrl Pts',(-2.73917747995907,12.2,11.040182705925));
#231129=CARTESIAN_POINT('Ctrl Pts',(-2.73985881835145,12.2,11.0365894117218));
#231130=CARTESIAN_POINT('Ctrl Pts',(-2.74053472872754,12.2,11.033002061668));
#231131=CARTESIAN_POINT('Ctrl Pts',(-2.74120523057892,12.2,11.0294206940057));
#231132=CARTESIAN_POINT('Ctrl Pts',(-2.7418757325521,12.2,11.0258393256927));
#231133=CARTESIAN_POINT('Ctrl Pts',(-2.74254082566543,12.2,11.0222639392731));
#231134=CARTESIAN_POINT('Ctrl Pts',(-2.74320053013557,12.2,11.0186945729218));
#231135=CARTESIAN_POINT('Ctrl Pts',(-2.74386023448586,12.2,11.0151252072191));
#231136=CARTESIAN_POINT('Ctrl Pts',(-2.74451455080071,12.2,11.0115618612429));
#231137=CARTESIAN_POINT('Ctrl Pts',(-2.74516349814226,12.2,11.0080045728201));
#231138=CARTESIAN_POINT('Ctrl Pts',(-2.74581244548382,12.2,11.0044472843973));
#231139=CARTESIAN_POINT('Ctrl Pts',(-2.74645602327657,12.2,11.0008960528176));
#231140=CARTESIAN_POINT('Ctrl Pts',(-2.74709425358624,12.2,10.9973509176136));
#231141=CARTESIAN_POINT('Ctrl Pts',(-2.74773248389591,12.2,10.9938057824097));
#231142=CARTESIAN_POINT('Ctrl Pts',(-2.74836536568956,12.2,10.9902667426383));
#231143=CARTESIAN_POINT('Ctrl Pts',(-2.7489929200001,12.2,10.9867338364749));
#231144=CARTESIAN_POINT('Ctrl Pts',(-2.74962047431063,12.2,10.9832009303116));
#231145=CARTESIAN_POINT('Ctrl Pts',(-2.75024270067137,12.2,10.9796741575564));
#231146=CARTESIAN_POINT('Ctrl Pts',(-2.75085961998276,12.2,10.9761535573505));
#231147=CARTESIAN_POINT('Ctrl Pts',(-2.75147653929415,12.2,10.9726329571445));
#231148=CARTESIAN_POINT('Ctrl Pts',(-2.75208815058921,12.2,10.9691185289715));
#231149=CARTESIAN_POINT('Ctrl Pts',(-2.75269447685958,12.2,10.9656103107647));
#231150=CARTESIAN_POINT('Ctrl Pts',(-2.75330080324009,12.2,10.9621020919207));
#231151=CARTESIAN_POINT('Ctrl Pts',(-2.7539018424941,12.2,10.9586000833784));
#231152=CARTESIAN_POINT('Ctrl Pts',(-2.7544976174133,12.2,10.9551043240796));
#231153=CARTESIAN_POINT('Ctrl Pts',(-2.75509339222427,12.2,10.9516085654158));
#231154=CARTESIAN_POINT('Ctrl Pts',(-2.75568390197257,12.2,10.9481190555728));
#231155=CARTESIAN_POINT('Ctrl Pts',(-2.75626916789661,12.2,10.9446358333177));
#231156=CARTESIAN_POINT('Ctrl Pts',(-2.75685443382064,12.2,10.9411526110627));
#231157=CARTESIAN_POINT('Ctrl Pts',(-2.757434456134,12.2,10.9376756771618));
#231158=CARTESIAN_POINT('Ctrl Pts',(-2.75800925557099,12.2,10.9342050691218));
#231159=CARTESIAN_POINT('Ctrl Pts',(-2.75858405500798,12.2,10.9307344610817));
#231160=CARTESIAN_POINT('Ctrl Pts',(-2.7591536326706,12.2,10.9272701807576));
#231161=CARTESIAN_POINT('Ctrl Pts',(-2.7597180100251,12.2,10.9238122652166));
#231162=CARTESIAN_POINT('Ctrl Pts',(-2.76028238737959,12.2,10.9203543496756));
#231163=CARTESIAN_POINT('Ctrl Pts',(-2.76084156377596,12.2,10.9169028007176));
#231164=CARTESIAN_POINT('Ctrl Pts',(-2.76139556171462,12.2,10.9134576560922));
#231165=CARTESIAN_POINT('Ctrl Pts',(-2.76194955965328,12.2,10.9100125114668));
#231166=CARTESIAN_POINT('Ctrl Pts',(-2.76249837945352,12.2,10.9065737720116));
#231167=CARTESIAN_POINT('Ctrl Pts',(-2.76304204283652,12.2,10.9031414766724));
#231168=CARTESIAN_POINT('Ctrl Pts',(-2.76358570621952,12.2,10.8997091813332));
#231169=CARTESIAN_POINT('Ctrl Pts',(-2.76412421241916,12.2,10.8962833298386));
#231170=CARTESIAN_POINT('Ctrl Pts',(-2.76465758615048,12.2,10.892863962712));
#231171=CARTESIAN_POINT('Ctrl Pts',(-2.76519095997869,12.2,10.8894445949642));
#231172=CARTESIAN_POINT('Ctrl Pts',(-2.76571919840546,12.2,10.8860317120682));
#231173=CARTESIAN_POINT('Ctrl Pts',(-2.76624232635579,12.2,10.8826253522824));
#231174=CARTESIAN_POINT('Ctrl Pts',(-2.7667654542111,12.2,10.8792189931153));
#231175=CARTESIAN_POINT('Ctrl Pts',(-2.76728347124166,12.2,10.8758191567896));
#231176=CARTESIAN_POINT('Ctrl Pts',(-2.76779639959758,12.2,10.8724258846218));
#231177=CARTESIAN_POINT('Ctrl Pts',(-2.7683093279535,12.2,10.8690326124541));
#231178=CARTESIAN_POINT('Ctrl Pts',(-2.76881716693322,12.2,10.8656459039727));
#231179=CARTESIAN_POINT('Ctrl Pts',(-2.76931994175055,12.2,10.8622657992885));
#231180=CARTESIAN_POINT('Ctrl Pts',(-2.76982271656787,12.2,10.8588856946044));
#231181=CARTESIAN_POINT('Ctrl Pts',(-2.77032042484861,12.2,10.8555121932127));
#231182=CARTESIAN_POINT('Ctrl Pts',(-2.77081309174964,12.2,10.852145336028));
#231183=CARTESIAN_POINT('Ctrl Pts',(-2.77130575865067,12.2,10.8487784788433));
#231184=CARTESIAN_POINT('Ctrl Pts',(-2.7717933840145,12.2,10.845418264511));
#231185=CARTESIAN_POINT('Ctrl Pts',(-2.77227599045574,12.2,10.8420647353823));
#231186=CARTESIAN_POINT('Ctrl Pts',(-2.77275859689697,12.2,10.8387112062535));
#231187=CARTESIAN_POINT('Ctrl Pts',(-2.77323618464688,12.2,10.8353643617576));
#231188=CARTESIAN_POINT('Ctrl Pts',(-2.77370877763039,12.2,10.8320242417114));
#231189=CARTESIAN_POINT('Ctrl Pts',(-2.77433890166564,12.2,10.8275707479119));
#231190=CARTESIAN_POINT('Ctrl Pts',(-2.77496014623938,12.2,10.8231292099251));
#231191=CARTESIAN_POINT('Ctrl Pts',(-2.77557256877551,12.2,10.8186997239969));
#231192=CARTESIAN_POINT('Ctrl Pts',(-2.77603188563588,12.2,10.8153776098526));
#231193=CARTESIAN_POINT('Ctrl Pts',(-2.77648623934728,12.2,10.8120622756645));
#231194=CARTESIAN_POINT('Ctrl Pts',(-2.77693565520801,12.2,10.8087537615196));
#231195=CARTESIAN_POINT('Ctrl Pts',(-2.77753487641009,12.2,10.8043424089258));
#231196=CARTESIAN_POINT('Ctrl Pts',(-2.77812531660605,12.2,10.7999431811761));
#231197=CARTESIAN_POINT('Ctrl Pts',(-2.77870703780353,12.2,10.7955561760493));
#231198=CARTESIAN_POINT('Ctrl Pts',(-2.77928875892175,12.2,10.7911691715203));
#231199=CARTESIAN_POINT('Ctrl Pts',(-2.77986175804667,12.2,10.7867943898008));
#231200=CARTESIAN_POINT('Ctrl Pts',(-2.78042609594554,12.2,10.7824319298234));
#231201=CARTESIAN_POINT('Ctrl Pts',(-2.7809904339213,12.2,10.7780694692515));
#231202=CARTESIAN_POINT('Ctrl Pts',(-2.78154611068692,12.2,10.7737193302587));
#231203=CARTESIAN_POINT('Ctrl Pts',(-2.78209318535443,12.2,10.7693816108623));
#231204=CARTESIAN_POINT('Ctrl Pts',(-2.7826402599474,12.2,10.7650438920568));
#231205=CARTESIAN_POINT('Ctrl Pts',(-2.78317873119667,12.2,10.7607185939203));
#231206=CARTESIAN_POINT('Ctrl Pts',(-2.78370866243169,12.2,10.7564058153276));
#231207=CARTESIAN_POINT('Ctrl Pts',(-2.78423859373891,12.2,10.7520930361473));
#231208=CARTESIAN_POINT('Ctrl Pts',(-2.78475998396732,12.2,10.747792777624));
#231209=CARTESIAN_POINT('Ctrl Pts',(-2.78527289405027,12.2,10.7435051378912));
#231210=CARTESIAN_POINT('Ctrl Pts',(-2.78578580406334,12.2,10.7392174987426));
#231211=CARTESIAN_POINT('Ctrl Pts',(-2.78629023610144,12.2,10.7349424814397));
#231212=CARTESIAN_POINT('Ctrl Pts',(-2.78678624891974,12.2,10.7306801833518));
#231213=CARTESIAN_POINT('Ctrl Pts',(-2.78728226180562,12.2,10.7264178846832));
#231214=CARTESIAN_POINT('Ctrl Pts',(-2.78776985954695,12.2,10.7221683065615));
#231215=CARTESIAN_POINT('Ctrl Pts',(-2.78824910157252,12.2,10.717931551887));
#231216=CARTESIAN_POINT('Ctrl Pts',(-2.7887283435328,12.2,10.7136947977898));
#231217=CARTESIAN_POINT('Ctrl Pts',(-2.78919923188086,12.2,10.7094708651316));
#231218=CARTESIAN_POINT('Ctrl Pts',(-2.78966182989945,12.2,10.7052598571968));
#231219=CARTESIAN_POINT('Ctrl Pts',(-2.79012442798107,12.2,10.7010488486882));
#231220=CARTESIAN_POINT('Ctrl Pts',(-2.79057873602685,12.2,10.696850763997));
#231221=CARTESIAN_POINT('Ctrl Pts',(-2.79102481877539,12.2,10.6926657074721));
#231222=CARTESIAN_POINT('Ctrl Pts',(-2.79147090146315,12.2,10.6884806515174));
#231223=CARTESIAN_POINT('Ctrl Pts',(-2.79190875953079,12.2,10.6843086209079));
#231224=CARTESIAN_POINT('Ctrl Pts',(-2.79233845816316,12.2,10.6801497229133));
#231225=CARTESIAN_POINT('Ctrl Pts',(-2.79276815685408,12.2,10.6759908243519));
#231226=CARTESIAN_POINT('Ctrl Pts',(-2.79318969651368,12.2,10.6718450558112));
#231227=CARTESIAN_POINT('Ctrl Pts',(-2.79360314325842,12.2,10.6677125219749));
#231228=CARTESIAN_POINT('Ctrl Pts',(-2.79401659000317,12.2,10.6635799881386));
#231229=CARTESIAN_POINT('Ctrl Pts',(-2.7944219447831,12.2,10.6594606899399));
#231230=CARTESIAN_POINT('Ctrl Pts',(-2.79481927358171,12.2,10.6553547308286));
#231231=CARTESIAN_POINT('Ctrl Pts',(-2.79531593449877,12.2,10.6502222827787));
#231232=CARTESIAN_POINT('Ctrl Pts',(-2.79580005608323,12.2,10.6451106764404));
#231233=CARTESIAN_POINT('Ctrl Pts',(-2.79627177346338,12.2,10.6400201208825));
#231234=CARTESIAN_POINT('Ctrl Pts',(-2.7966491474292,12.2,10.6359476757703));
#231235=CARTESIAN_POINT('Ctrl Pts',(-2.79701858150538,12.2,10.6318887028815));
#231236=CARTESIAN_POINT('Ctrl Pts',(-2.79738014569176,12.2,10.6278433065499));
#231237=CARTESIAN_POINT('Ctrl Pts',(-2.79774170987813,12.2,10.6237979102183));
#231238=CARTESIAN_POINT('Ctrl Pts',(-2.79809540574137,12.2,10.6197660935549));
#231239=CARTESIAN_POINT('Ctrl Pts',(-2.79844130181497,12.2,10.6157479605596));
#231240=CARTESIAN_POINT('Ctrl Pts',(-2.79878719784145,12.2,10.6117298281118));
#231241=CARTESIAN_POINT('Ctrl Pts',(-2.79912529522451,12.2,10.6077253823454));
#231242=CARTESIAN_POINT('Ctrl Pts',(-2.799455664698,12.2,10.6037347285596));
#231243=CARTESIAN_POINT('Ctrl Pts',(-2.79978603421651,12.2,10.5997440742302));
#231244=CARTESIAN_POINT('Ctrl Pts',(-2.80010867739129,12.2,10.5957672132572));
#231245=CARTESIAN_POINT('Ctrl Pts',(-2.80042366431242,12.2,10.5918042539));
#231246=CARTESIAN_POINT('Ctrl Pts',(-2.80073865119063,12.2,10.5878412950827));
#231247=CARTESIAN_POINT('Ctrl Pts',(-2.80104598424952,12.2,10.5838922378927));
#231248=CARTESIAN_POINT('Ctrl Pts',(-2.80134573622551,12.2,10.5799571920467));
#231249=CARTESIAN_POINT('Ctrl Pts',(-2.80172042622613,12.2,10.5750383843372));
#231250=CARTESIAN_POINT('Ctrl Pts',(-2.80208326965978,12.2,10.5701414696755));
#231251=CARTESIAN_POINT('Ctrl Pts',(-2.80243441320205,12.2,10.5652666620355));
#231252=CARTESIAN_POINT('Ctrl Pts',(-2.80271532805118,12.2,10.561366815711));
#231253=CARTESIAN_POINT('Ctrl Pts',(-2.80298875558372,12.2,10.5574811186609));
#231254=CARTESIAN_POINT('Ctrl Pts',(-2.80325477105531,12.2,10.5536096819799));
#231255=CARTESIAN_POINT('Ctrl Pts',(-2.80352078649065,12.2,10.5497382458264));
#231256=CARTESIAN_POINT('Ctrl Pts',(-2.80377938992731,12.2,10.5458810695954));
#231257=CARTESIAN_POINT('Ctrl Pts',(-2.80403065746281,12.2,10.5420382657976));
#231258=CARTESIAN_POINT('Ctrl Pts',(-2.80428192503253,12.2,10.5381954614761));
#231259=CARTESIAN_POINT('Ctrl Pts',(-2.80452585824305,12.2,10.534367030223));
#231260=CARTESIAN_POINT('Ctrl Pts',(-2.8047625349777,12.2,10.5305530832383));
#231261=CARTESIAN_POINT('Ctrl Pts',(-2.8049992116801,12.2,10.5267391367732));
#231262=CARTESIAN_POINT('Ctrl Pts',(-2.80522863103812,12.2,10.522939676158));
#231263=CARTESIAN_POINT('Ctrl Pts',(-2.80545087197613,12.2,10.5191548134992));
#231264=CARTESIAN_POINT('Ctrl Pts',(-2.80572867317135,12.2,10.514423734789));
#231265=CARTESIAN_POINT('Ctrl Pts',(-2.80599525983273,12.2,10.5097154677188));
#231266=CARTESIAN_POINT('Ctrl Pts',(-2.80625078670831,12.2,10.5050302343148));
#231267=CARTESIAN_POINT('Ctrl Pts',(-2.80645520821991,12.2,10.5012820473874));
#231268=CARTESIAN_POINT('Ctrl Pts',(-2.80665255356677,12.2,10.4975486028395));
#231269=CARTESIAN_POINT('Ctrl Pts',(-2.80684290179891,12.2,10.4938300164711));
#231270=CARTESIAN_POINT('Ctrl Pts',(-2.80703325000512,12.2,10.4901114306093));
#231271=CARTESIAN_POINT('Ctrl Pts',(-2.80721660240723,12.2,10.486407702086));
#231272=CARTESIAN_POINT('Ctrl Pts',(-2.80739304195778,12.2,10.4827189475353));
#231273=CARTESIAN_POINT('Ctrl Pts',(-2.80756948153236,12.2,10.479030192482));
#231274=CARTESIAN_POINT('Ctrl Pts',(-2.80773900726324,12.2,10.4753564130104));
#231275=CARTESIAN_POINT('Ctrl Pts',(-2.80790170477165,12.2,10.471697724701));
#231276=CARTESIAN_POINT('Ctrl Pts',(-2.8080644022579,12.2,10.46803903689));
#231277=CARTESIAN_POINT('Ctrl Pts',(-2.80822027035108,12.2,10.4643954415787));
#231278=CARTESIAN_POINT('Ctrl Pts',(-2.8083693939507,12.2,10.4607670558182));
#231279=CARTESIAN_POINT('Ctrl Pts',(-2.80851851757063,12.2,10.4571386695633));
#231280=CARTESIAN_POINT('Ctrl Pts',(-2.80866089775329,12.2,10.4535254935709));
#231281=CARTESIAN_POINT('Ctrl Pts',(-2.80879661998351,12.2,10.4499276472475));
#231282=CARTESIAN_POINT('Ctrl Pts',(-2.80893234219523,12.2,10.4463298014142));
#231283=CARTESIAN_POINT('Ctrl Pts',(-2.80906140671995,12.2,10.4427472858459));
#231284=CARTESIAN_POINT('Ctrl Pts',(-2.80918390098838,12.2,10.4391802188581));
#231285=CARTESIAN_POINT('Ctrl Pts',(-2.80930639527351,12.2,10.4356131513843));
#231286=CARTESIAN_POINT('Ctrl Pts',(-2.8094223200969,12.2,10.4320615346203));
#231287=CARTESIAN_POINT('Ctrl Pts',(-2.80953176249175,12.2,10.4285254889833));
#231288=CARTESIAN_POINT('Ctrl Pts',(-2.8096412048866,12.2,10.4249894433462));
#231289=CARTESIAN_POINT('Ctrl Pts',(-2.80974416743904,12.2,10.4214689690302));
#231290=CARTESIAN_POINT('Ctrl Pts',(-2.80984073833253,12.2,10.4179641874519));
#231291=CARTESIAN_POINT('Ctrl Pts',(-2.80996145192967,12.2,10.4135832111954));
#231292=CARTESIAN_POINT('Ctrl Pts',(-2.81007217891929,12.2,10.4092267559631));
#231293=CARTESIAN_POINT('Ctrl Pts',(-2.81017309772854,12.2,10.4048950630998));
#231294=CARTESIAN_POINT('Ctrl Pts',(-2.8102740165488,12.2,10.4005633697644));
#231295=CARTESIAN_POINT('Ctrl Pts',(-2.81036512871086,12.2,10.3962564396454));
#231296=CARTESIAN_POINT('Ctrl Pts',(-2.81044661648942,12.2,10.39197451381));
#231297=CARTESIAN_POINT('Ctrl Pts',(-2.81051180671583,12.2,10.388548972955));
#231298=CARTESIAN_POINT('Ctrl Pts',(-2.81057083593034,12.2,10.3851394349924));
#231299=CARTESIAN_POINT('Ctrl Pts',(-2.81062380026678,12.2,10.3817460280143));
#231300=CARTESIAN_POINT('Ctrl Pts',(-2.810676764596,12.2,10.3783526214986));
#231301=CARTESIAN_POINT('Ctrl Pts',(-2.81072366321001,12.2,10.3749753441125));
#231302=CARTESIAN_POINT('Ctrl Pts',(-2.81076459348505,12.2,10.3716143237745));
#231303=CARTESIAN_POINT('Ctrl Pts',(-2.81080552376568,12.2,10.3682533029785));
#231304=CARTESIAN_POINT('Ctrl Pts',(-2.81084048466238,12.2,10.3649085389119));
#231305=CARTESIAN_POINT('Ctrl Pts',(-2.81086957427508,12.2,10.3615801600082));
#231306=CARTESIAN_POINT('Ctrl Pts',(-2.81090593628897,12.2,10.3574196866054));
#231307=CARTESIAN_POINT('Ctrl Pts',(-2.81093312448892,12.2,10.3532848137552));
#231308=CARTESIAN_POINT('Ctrl Pts',(-2.81095133101675,12.2,10.3491757954727));
#231309=CARTESIAN_POINT('Ctrl Pts',(-2.81097317884937,12.2,10.3442449737128));
#231310=CARTESIAN_POINT('Ctrl Pts',(-2.81098209669121,12.2,10.3393513828899));
#231311=CARTESIAN_POINT('Ctrl Pts',(-2.81097842327522,12.2,10.3344954632314));
#231312=CARTESIAN_POINT('Ctrl Pts',(-2.81097536209512,12.2,10.3304488633689));
#231313=CARTESIAN_POINT('Ctrl Pts',(-2.8109635582398,12.2,10.3264284254738));
#231314=CARTESIAN_POINT('Ctrl Pts',(-2.81094321372636,12.2,10.3224344087363));
#231315=CARTESIAN_POINT('Ctrl Pts',(-2.81092286921291,12.2,10.3184403919987));
#231316=CARTESIAN_POINT('Ctrl Pts',(-2.81089398195202,12.2,10.3144727960815));
#231317=CARTESIAN_POINT('Ctrl Pts',(-2.81085676153579,12.2,10.3105318828162));
#231318=CARTESIAN_POINT('Ctrl Pts',(-2.81081954111956,12.2,10.3065909695509));
#231319=CARTESIAN_POINT('Ctrl Pts',(-2.81077398338366,12.2,10.3026767395475));
#231320=CARTESIAN_POINT('Ctrl Pts',(-2.81072030150844,12.2,10.298789458002));
#231321=CARTESIAN_POINT('Ctrl Pts',(-2.81066661963322,12.2,10.2949021764566));
#231322=CARTESIAN_POINT('Ctrl Pts',(-2.81060481270563,12.2,10.2910418444166));
#231323=CARTESIAN_POINT('Ctrl Pts',(-2.81053509402508,12.2,10.2872087287916));
#231324=CARTESIAN_POINT('Ctrl Pts',(-2.81046537534452,12.2,10.2833756131666));
#231325=CARTESIAN_POINT('Ctrl Pts',(-2.81038774418933,12.2,10.2795697137705));
#231326=CARTESIAN_POINT('Ctrl Pts',(-2.81030241905003,12.2,10.2757913054895));
#231327=CARTESIAN_POINT('Ctrl Pts',(-2.81021709391073,12.2,10.2720128972086));
#231328=CARTESIAN_POINT('Ctrl Pts',(-2.81012407523829,12.2,10.2682619765996));
#231329=CARTESIAN_POINT('Ctrl Pts',(-2.81002358496012,12.2,10.2645388217399));
#231330=CARTESIAN_POINT('Ctrl Pts',(-2.80992309468195,12.2,10.2608156668803));
#231331=CARTESIAN_POINT('Ctrl Pts',(-2.80981513335954,12.2,10.2571202757921));
#231332=CARTESIAN_POINT('Ctrl Pts',(-2.80969992502583,12.2,10.2534529285019));
#231333=CARTESIAN_POINT('Ctrl Pts',(-2.80958471669212,12.2,10.2497855812117));
#231334=CARTESIAN_POINT('Ctrl Pts',(-2.80946226480308,12.2,10.2461462782537));
#231335=CARTESIAN_POINT('Ctrl Pts',(-2.80933279722669,12.2,10.2425353000892));
#231336=CARTESIAN_POINT('Ctrl Pts',(-2.80920332965029,12.2,10.2389243219246));
#231337=CARTESIAN_POINT('Ctrl Pts',(-2.80906684851522,12.2,10.2353416698494));
#231338=CARTESIAN_POINT('Ctrl Pts',(-2.80892358768133,12.2,10.23178763006));
#231339=CARTESIAN_POINT('Ctrl Pts',(-2.80875167468692,12.2,10.2275227824678));
#231340=CARTESIAN_POINT('Ctrl Pts',(-2.8085699999856,12.2,10.2232991351234));
#231341=CARTESIAN_POINT('Ctrl Pts',(-2.80837898074165,12.2,10.2191171915063));
#231342=CARTESIAN_POINT('Ctrl Pts',(-2.80821979803257,12.2,10.2156322383655));
#231343=CARTESIAN_POINT('Ctrl Pts',(-2.80805412475578,12.2,10.2121762438355));
#231344=CARTESIAN_POINT('Ctrl Pts',(-2.80788220725546,12.2,10.208749506476));
#231345=CARTESIAN_POINT('Ctrl Pts',(-2.80771028975513,12.2,10.2053227691164));
#231346=CARTESIAN_POINT('Ctrl Pts',(-2.80753212928275,12.2,10.2019252859783));
#231347=CARTESIAN_POINT('Ctrl Pts',(-2.80734797525466,12.2,10.1985573570215));
#231348=CARTESIAN_POINT('Ctrl Pts',(-2.80709015963139,12.2,10.1938422567757));
#231349=CARTESIAN_POINT('Ctrl Pts',(-2.80682059910816,12.2,10.1891850798021));
#231350=CARTESIAN_POINT('Ctrl Pts',(-2.80653999625128,12.2,10.1845866627379));
#231351=CARTESIAN_POINT('Ctrl Pts',(-2.80629947948873,12.2,10.1806451619368));
#231352=CARTESIAN_POINT('Ctrl Pts',(-2.8060508531587,12.2,10.1767468304232));
#231353=CARTESIAN_POINT('Ctrl Pts',(-2.80579457222774,12.2,10.1728922027983));
#231354=CARTESIAN_POINT('Ctrl Pts',(-2.80553829132005,12.2,10.1690375755236));
#231355=CARTESIAN_POINT('Ctrl Pts',(-2.80527435617489,12.2,10.1652266519903));
#231356=CARTESIAN_POINT('Ctrl Pts',(-2.80500323451686,12.2,10.1614599785266));
#231357=CARTESIAN_POINT('Ctrl Pts',(-2.80473211285883,12.2,10.1576933050629));
#231358=CARTESIAN_POINT('Ctrl Pts',(-2.80445380643698,12.2,10.1539708785952));
#231359=CARTESIAN_POINT('Ctrl Pts',(-2.80416879378113,12.2,10.1502932561424));
#231360=CARTESIAN_POINT('Ctrl Pts',(-2.80388378109939,12.2,10.1466156333556));
#231361=CARTESIAN_POINT('Ctrl Pts',(-2.80359206356105,12.2,10.1429828111584));
#231362=CARTESIAN_POINT('Ctrl Pts',(-2.80329413277956,12.2,10.139395356453));
#231363=CARTESIAN_POINT('Ctrl Pts',(-2.80299620202515,12.2,10.1358079020734));
#231364=CARTESIAN_POINT('Ctrl Pts',(-2.80269205783048,12.2,10.1322658141479));
#231365=CARTESIAN_POINT('Ctrl Pts',(-2.8023822072584,12.2,10.1287696670249));
#231366=CARTESIAN_POINT('Ctrl Pts',(-2.80207235668633,12.2,10.1252735199019));
#231367=CARTESIAN_POINT('Ctrl Pts',(-2.80175679923515,12.2,10.1218233145367));
#231368=CARTESIAN_POINT('Ctrl Pts',(-2.80143605356441,12.2,10.1184196360709));
#231369=CARTESIAN_POINT('Ctrl Pts',(-2.80111530786454,12.2,10.1150159572961));
#231370=CARTESIAN_POINT('Ctrl Pts',(-2.80078937240736,12.2,10.1116588047413));
#231371=CARTESIAN_POINT('Ctrl Pts',(-2.80045878297236,12.2,10.1083487771475));
#231372=CARTESIAN_POINT('Ctrl Pts',(-2.80007309534324,12.2,10.104487078739));
#231373=CARTESIAN_POINT('Ctrl Pts',(-2.79968107048435,12.2,10.1006895201144));
#231374=CARTESIAN_POINT('Ctrl Pts',(-2.7992835797872,12.2,10.0969570711486));
#231375=CARTESIAN_POINT('Ctrl Pts',(-2.79894287343557,12.2,10.0937578288044));
#231376=CARTESIAN_POINT('Ctrl Pts',(-2.79859815189461,12.2,10.0906064231295));
#231377=CARTESIAN_POINT('Ctrl Pts',(-2.79824998044137,12.2,10.0875034757249));
#231378=CARTESIAN_POINT('Ctrl Pts',(-2.79790180901977,12.2,10.0844005286021));
#231379=CARTESIAN_POINT('Ctrl Pts',(-2.79755018529552,12.2,10.0813460427824));
#231380=CARTESIAN_POINT('Ctrl Pts',(-2.79719569472506,12.2,10.0783406519749));
#231381=CARTESIAN_POINT('Ctrl Pts',(-2.7968412041546,12.2,10.0753352611674));
#231382=CARTESIAN_POINT('Ctrl Pts',(-2.79648384147295,12.2,10.072378967257));
#231383=CARTESIAN_POINT('Ctrl Pts',(-2.79612420730151,12.2,10.0694724210479));
#231384=CARTESIAN_POINT('Ctrl Pts',(-2.79576457309741,12.2,10.0665658745747));
#231385=CARTESIAN_POINT('Ctrl Pts',(-2.79540266705536,12.2,10.0637090725018));
#231386=CARTESIAN_POINT('Ctrl Pts',(-2.7950391019521,12.2,10.0609026844357));
#231387=CARTESIAN_POINT('Ctrl Pts',(-2.79467553688187,12.2,10.0580962966244));
#231388=CARTESIAN_POINT('Ctrl Pts',(-2.79431031332991,12.2,10.0553403202792));
#231389=CARTESIAN_POINT('Ctrl Pts',(-2.79394406325822,12.2,10.052635435532));
#231390=CARTESIAN_POINT('Ctrl Pts',(-2.79357781318653,12.2,10.0499305507847));
#231391=CARTESIAN_POINT('Ctrl Pts',(-2.79321053627339,12.2,10.0472767573413));
#231392=CARTESIAN_POINT('Ctrl Pts',(-2.79284288428676,12.2,10.0446747506836));
#231393=CARTESIAN_POINT('Ctrl Pts',(-2.79247523226674,12.2,10.0420727437895));
#231394=CARTESIAN_POINT('Ctrl Pts',(-2.79210720367999,12.2,10.0395225250769));
#231395=CARTESIAN_POINT('Ctrl Pts',(-2.7917394689933,12.2,10.0370248034443));
#231396=CARTESIAN_POINT('Ctrl Pts',(-2.79137173434002,12.2,10.0345270820386));
#231397=CARTESIAN_POINT('Ctrl Pts',(-2.79100429403339,12.2,10.0320818608305));
#231398=CARTESIAN_POINT('Ctrl Pts',(-2.79063783821342,12.2,10.0296898664198));
#231399=CARTESIAN_POINT('Ctrl Pts',(-2.79027138239345,12.2,10.027297872009));
#231400=CARTESIAN_POINT('Ctrl Pts',(-2.78990591142341,12.2,10.0249591074523));
#231401=CARTESIAN_POINT('Ctrl Pts',(-2.78954213576989,12.2,10.0226743151163));
#231402=CARTESIAN_POINT('Ctrl Pts',(-2.78917836011637,12.2,10.0203895227803));
#231403=CARTESIAN_POINT('Ctrl Pts',(-2.78881628091801,12.2,10.0181587065701));
#231404=CARTESIAN_POINT('Ctrl Pts',(-2.78845663051425,12.2,10.0159826302288));
#231405=CARTESIAN_POINT('Ctrl Pts',(-2.78809698007782,12.2,10.0138065536898));
#231406=CARTESIAN_POINT('Ctrl Pts',(-2.7877397603166,12.2,10.0116852182978));
#231407=CARTESIAN_POINT('Ctrl Pts',(-2.7873857259641,12.2,10.0096194098542));
#231408=CARTESIAN_POINT('Ctrl Pts',(-2.78703169164377,12.2,10.0075536015983));
#231409=CARTESIAN_POINT('Ctrl Pts',(-2.78668084651418,12.2,10.0055433186638));
#231410=CARTESIAN_POINT('Ctrl Pts',(-2.7863339672752,12.2,10.0035893704758));
#231411=CARTESIAN_POINT('Ctrl Pts',(-2.7857574999564,12.2,10.0003421675693));
#231412=CARTESIAN_POINT('Ctrl Pts',(-2.78519199058759,12.2,9.99725051957323));
#231413=CARTESIAN_POINT('Ctrl Pts',(-2.78464115900006,12.2,9.99431831799999));
#231414=CARTESIAN_POINT('Ctrl Pts',(-2.78464115900006,15.2,9.99431831799999));
#231415=CARTESIAN_POINT('Ctrl Pts',(-2.78497102164681,15.2,9.9960742517439));
#231416=CARTESIAN_POINT('Ctrl Pts',(-2.7853061480725,15.2,9.99788737721449));
#231417=CARTESIAN_POINT('Ctrl Pts',(-2.78564574048785,15.2,9.99975683102847));
#231418=CARTESIAN_POINT('Ctrl Pts',(-2.78598697058949,15.2,10.0016353002937));
#231419=CARTESIAN_POINT('Ctrl Pts',(-2.78633270293049,15.2,10.0035706519564));
#231420=CARTESIAN_POINT('Ctrl Pts',(-2.78668214030053,15.2,10.0055620674177));
#231421=CARTESIAN_POINT('Ctrl Pts',(-2.78703157763883,15.2,10.007553482698));
#231422=CARTESIAN_POINT('Ctrl Pts',(-2.78738472059632,15.2,10.0096009594763));
#231423=CARTESIAN_POINT('Ctrl Pts',(-2.78774079425005,15.2,10.0117036987332));
#231424=CARTESIAN_POINT('Ctrl Pts',(-2.78809686790378,15.2,10.0138064379902));
#231425=CARTESIAN_POINT('Ctrl Pts',(-2.78845587543532,15.2,10.015964439659));
#231426=CARTESIAN_POINT('Ctrl Pts',(-2.78881706319012,15.2,10.0181769250193));
#231427=CARTESIAN_POINT('Ctrl Pts',(-2.78917825097771,15.2,10.0203894105806));
#231428=CARTESIAN_POINT('Ctrl Pts',(-2.78954162379485,15.2,10.0226563798811));
#231429=CARTESIAN_POINT('Ctrl Pts',(-2.78990645056482,15.2,10.0249770707612));
#231430=CARTESIAN_POINT('Ctrl Pts',(-2.79027127730165,15.2,10.0272977614305));
#231431=CARTESIAN_POINT('Ctrl Pts',(-2.79063756082855,15.2,10.0296721774031));
#231432=CARTESIAN_POINT('Ctrl Pts',(-2.79100459748355,15.2,10.0320995767427));
#231433=CARTESIAN_POINT('Ctrl Pts',(-2.79137163413856,15.2,10.0345269760823));
#231434=CARTESIAN_POINT('Ctrl Pts',(-2.79173942030171,15.2,10.0370073571481));
#231435=CARTESIAN_POINT('Ctrl Pts',(-2.79210727620501,15.2,10.0395399978038));
#231436=CARTESIAN_POINT('Ctrl Pts',(-2.79247513214172,15.2,10.0420726386895));
#231437=CARTESIAN_POINT('Ctrl Pts',(-2.79284305736179,15.2,10.0446575395651));
#231438=CARTESIAN_POINT('Ctrl Pts',(-2.79321038729843,15.2,10.0472939942956));
#231439=CARTESIAN_POINT('Ctrl Pts',(-2.7935777172017,15.2,10.0499304487866));
#231440=CARTESIAN_POINT('Ctrl Pts',(-2.79394445291664,15.2,10.0526184549133));
#231441=CARTESIAN_POINT('Ctrl Pts',(-2.79430994806997,15.2,10.0553573256494));
#231442=CARTESIAN_POINT('Ctrl Pts',(-2.79467544322331,15.2,10.0580961963854));
#231443=CARTESIAN_POINT('Ctrl Pts',(-2.79503970031006,15.2,10.060885930059));
#231444=CARTESIAN_POINT('Ctrl Pts',(-2.79540209146363,15.2,10.0637258528703));
#231445=CARTESIAN_POINT('Ctrl Pts',(-2.79576448261721,15.2,10.0665657756816));
#231446=CARTESIAN_POINT('Ctrl Pts',(-2.79612500880721,15.2,10.0694558861813));
#231447=CARTESIAN_POINT('Ctrl Pts',(-2.79648306196103,15.2,10.0723955259878));
#231448=CARTESIAN_POINT('Ctrl Pts',(-2.79684111514738,15.2,10.0753351660613));
#231449=CARTESIAN_POINT('Ctrl Pts',(-2.79719669448351,15.2,10.0783243339647));
#231450=CARTESIAN_POINT('Ctrl Pts',(-2.79754920883593,15.2,10.0813623851324));
#231451=CARTESIAN_POINT('Ctrl Pts',(-2.79790172315632,15.2,10.0844004360241));
#231452=CARTESIAN_POINT('Ctrl Pts',(-2.79825117216088,15.2,10.0874873693649));
#231453=CARTESIAN_POINT('Ctrl Pts',(-2.79859698148324,15.2,10.0906225532652));
#231454=CARTESIAN_POINT('Ctrl Pts',(-2.79900042571359,15.2,10.0942802680053));
#231455=CARTESIAN_POINT('Ctrl Pts',(-2.79939891254026,15.2,10.0980036552378));
#231456=CARTESIAN_POINT('Ctrl Pts',(-2.79979155926839,15.2,10.1017917346604));
#231457=CARTESIAN_POINT('Ctrl Pts',(-2.80012811358931,15.2,10.1050386597112));
#231458=CARTESIAN_POINT('Ctrl Pts',(-2.80046037415222,15.2,10.1083331142665));
#231459=CARTESIAN_POINT('Ctrl Pts',(-2.80078780072386,15.2,10.111674491393));
#231460=CARTESIAN_POINT('Ctrl Pts',(-2.80111522729551,15.2,10.1150158685195));
#231461=CARTESIAN_POINT('Ctrl Pts',(-2.80143782030164,15.2,10.1184041704702));
#231462=CARTESIAN_POINT('Ctrl Pts',(-2.80175505070715,15.2,10.1218388016755));
#231463=CARTESIAN_POINT('Ctrl Pts',(-2.80207228114147,15.2,10.1252734331929));
#231464=CARTESIAN_POINT('Ctrl Pts',(-2.80238414665863,15.2,10.1287543959148));
#231465=CARTESIAN_POINT('Ctrl Pts',(-2.80269013725838,15.2,10.1322811064423));
#231466=CARTESIAN_POINT('Ctrl Pts',(-2.80299612783034,15.2,10.1358078166494));
#231467=CARTESIAN_POINT('Ctrl Pts',(-2.80329624015926,15.2,10.1393802749717));
#231468=CARTESIAN_POINT('Ctrl Pts',(-2.8035899748166,15.2,10.1429979119399));
#231469=CARTESIAN_POINT('Ctrl Pts',(-2.80388370947394,15.2,10.1466155489081));
#231470=CARTESIAN_POINT('Ctrl Pts',(-2.80417106491254,15.2,10.1502783616335));
#231471=CARTESIAN_POINT('Ctrl Pts',(-2.80445155373616,15.2,10.1539857918291));
#231472=CARTESIAN_POINT('Ctrl Pts',(-2.80477879071402,15.2,10.1583111272819));
#231473=CARTESIAN_POINT('Ctrl Pts',(-2.8050966796604,15.2,10.1626971897311));
#231474=CARTESIAN_POINT('Ctrl Pts',(-2.80540446820828,15.2,10.1671431084732));
#231475=CARTESIAN_POINT('Ctrl Pts',(-2.80571225675616,15.2,10.1715890272153));
#231476=CARTESIAN_POINT('Ctrl Pts',(-2.8060099429316,15.2,10.1760947993178));
#231477=CARTESIAN_POINT('Ctrl Pts',(-2.8062967935051,15.2,10.1806595712383));
#231478=CARTESIAN_POINT('Ctrl Pts',(-2.80658364405628,15.2,10.1852243428035));
#231479=CARTESIAN_POINT('Ctrl Pts',(-2.8068596611745,15.2,10.1898481137241));
#231480=CARTESIAN_POINT('Ctrl Pts',(-2.80712413049203,15.2,10.1945300465125));
#231481=CARTESIAN_POINT('Ctrl Pts',(-2.80731303715918,15.2,10.1978742844268));
#231482=CARTESIAN_POINT('Ctrl Pts',(-2.80749605282088,15.2,10.2012481962405));
#231483=CARTESIAN_POINT('Ctrl Pts',(-2.80767292525193,15.2,10.2046514824881));
#231484=CARTESIAN_POINT('Ctrl Pts',(-2.80788517218078,15.2,10.2087354262079));
#231485=CARTESIAN_POINT('Ctrl Pts',(-2.80808857128242,15.2,10.2128616674821));
#231486=CARTESIAN_POINT('Ctrl Pts',(-2.80828269430216,15.2,10.2170296974199));
#231487=CARTESIAN_POINT('Ctrl Pts',(-2.80844446347646,15.2,10.2205030555121));
#231488=CARTESIAN_POINT('Ctrl Pts',(-2.80859979202005,15.2,10.2240054312428));
#231489=CARTESIAN_POINT('Ctrl Pts',(-2.80874843701951,15.2,10.2275365352035));
#231490=CARTESIAN_POINT('Ctrl Pts',(-2.80889708201897,15.2,10.2310676391641));
#231491=CARTESIAN_POINT('Ctrl Pts',(-2.80903904387386,15.2,10.2346274710503));
#231492=CARTESIAN_POINT('Ctrl Pts',(-2.80917408477607,15.2,10.2382157425109));
#231493=CARTESIAN_POINT('Ctrl Pts',(-2.80930912566356,15.2,10.2418040135805));
#231494=CARTESIAN_POINT('Ctrl Pts',(-2.80943724665241,15.2,10.2454207239672));
#231495=CARTESIAN_POINT('Ctrl Pts',(-2.80955821275092,15.2,10.2490655907898));
#231496=CARTESIAN_POINT('Ctrl Pts',(-2.80972756530992,15.2,10.2541684049772));
#231497=CARTESIAN_POINT('Ctrl Pts',(-2.80988289856849,15.2,10.2593264048552));
#231498=CARTESIAN_POINT('Ctrl Pts',(-2.81002358496012,15.2,10.2645388217399));
#231499=CARTESIAN_POINT('Ctrl Pts',(-2.81012407523829,15.2,10.2682619765996));
#231500=CARTESIAN_POINT('Ctrl Pts',(-2.81021709391073,15.2,10.2720128972086));
#231501=CARTESIAN_POINT('Ctrl Pts',(-2.81030241905003,15.2,10.2757913054895));
#231502=CARTESIAN_POINT('Ctrl Pts',(-2.81038774418933,15.2,10.2795697137705));
#231503=CARTESIAN_POINT('Ctrl Pts',(-2.81046537534452,15.2,10.2833756131666));
#231504=CARTESIAN_POINT('Ctrl Pts',(-2.81053509402508,15.2,10.2872087287916));
#231505=CARTESIAN_POINT('Ctrl Pts',(-2.81060481270563,15.2,10.2910418444166));
#231506=CARTESIAN_POINT('Ctrl Pts',(-2.81066661963322,15.2,10.2949021764565));
#231507=CARTESIAN_POINT('Ctrl Pts',(-2.81072030150844,15.2,10.298789458002));
#231508=CARTESIAN_POINT('Ctrl Pts',(-2.81077398338366,15.2,10.3026767395475));
#231509=CARTESIAN_POINT('Ctrl Pts',(-2.81081954111956,15.2,10.3065909695509));
#231510=CARTESIAN_POINT('Ctrl Pts',(-2.81085676153579,15.2,10.3105318828162));
#231511=CARTESIAN_POINT('Ctrl Pts',(-2.81090142603365,15.2,10.3152609785627));
#231512=CARTESIAN_POINT('Ctrl Pts',(-2.81093408968245,15.2,10.3200284964061));
#231513=CARTESIAN_POINT('Ctrl Pts',(-2.81095439401559,15.2,10.3248339869798));
#231514=CARTESIAN_POINT('Ctrl Pts',(-2.81097808240547,15.2,10.3304403929402));
#231515=CARTESIAN_POINT('Ctrl Pts',(-2.81098495125587,15.2,10.3360984795428));
#231516=CARTESIAN_POINT('Ctrl Pts',(-2.81097444824174,15.2,10.3418075407271));
#231517=CARTESIAN_POINT('Ctrl Pts',(-2.8109669460889,15.2,10.3458854415096));
#231518=CARTESIAN_POINT('Ctrl Pts',(-2.81095058234328,15.2,10.3499893506076));
#231519=CARTESIAN_POINT('Ctrl Pts',(-2.81092515873169,15.2,10.3541190115118));
#231520=CARTESIAN_POINT('Ctrl Pts',(-2.81089973512011,15.2,10.3582486724161));
#231521=CARTESIAN_POINT('Ctrl Pts',(-2.81086525538654,15.2,10.36240408635));
#231522=CARTESIAN_POINT('Ctrl Pts',(-2.81082152399716,15.2,10.3665850012818));
#231523=CARTESIAN_POINT('Ctrl Pts',(-2.81078653888852,15.2,10.3699297329539));
#231524=CARTESIAN_POINT('Ctrl Pts',(-2.8107456327715,15.2,10.3732907846882));
#231525=CARTESIAN_POINT('Ctrl Pts',(-2.81069870977352,15.2,10.3766680299683));
#231526=CARTESIAN_POINT('Ctrl Pts',(-2.81065178676915,15.2,10.3800452757085));
#231527=CARTESIAN_POINT('Ctrl Pts',(-2.81059884604604,15.2,10.3834387144058));
#231528=CARTESIAN_POINT('Ctrl Pts',(-2.81053979298686,15.2,10.3868482205371));
#231529=CARTESIAN_POINT('Ctrl Pts',(-2.81048073993573,15.2,10.3902577262039));
#231530=CARTESIAN_POINT('Ctrl Pts',(-2.81041557268305,15.2,10.3936832977703));
#231531=CARTESIAN_POINT('Ctrl Pts',(-2.81034420024508,15.2,10.3971248101539));
#231532=CARTESIAN_POINT('Ctrl Pts',(-2.81025498469032,15.2,10.4014267009851));
#231533=CARTESIAN_POINT('Ctrl Pts',(-2.81015607047853,15.2,10.4057534998181));
#231534=CARTESIAN_POINT('Ctrl Pts',(-2.81004727602934,15.2,10.4101049642699));
#231535=CARTESIAN_POINT('Ctrl Pts',(-2.80996024046524,15.2,10.413586136021));
#231536=CARTESIAN_POINT('Ctrl Pts',(-2.80986688240328,15.2,10.417083094467));
#231537=CARTESIAN_POINT('Ctrl Pts',(-2.8097671101752,15.2,10.4205957147706));
#231538=CARTESIAN_POINT('Ctrl Pts',(-2.8096423948969,15.2,10.4249864899107));
#231539=CARTESIAN_POINT('Ctrl Pts',(-2.80950765977441,15.2,10.4294017383725));
#231540=CARTESIAN_POINT('Ctrl Pts',(-2.80936272623221,15.2,10.4338412210821));
#231541=CARTESIAN_POINT('Ctrl Pts',(-2.80924677940793,15.2,10.4373928069594));
#231542=CARTESIAN_POINT('Ctrl Pts',(-2.80912430728355,15.2,10.4409599042343));
#231543=CARTESIAN_POINT('Ctrl Pts',(-2.80899522101044,15.2,10.4445423902302));
#231544=CARTESIAN_POINT('Ctrl Pts',(-2.80883386315588,15.2,10.4490204980911));
#231545=CARTESIAN_POINT('Ctrl Pts',(-2.80866217064472,15.2,10.4535226533442));
#231546=CARTESIAN_POINT('Ctrl Pts',(-2.80847997377027,15.2,10.4580486194541));
#231547=CARTESIAN_POINT('Ctrl Pts',(-2.80833421626276,15.2,10.4616693925393));
#231548=CARTESIAN_POINT('Ctrl Pts',(-2.80818173696834,15.2,10.4653054066736));
#231549=CARTESIAN_POINT('Ctrl Pts',(-2.808022448737,15.2,10.4689565410402));
#231550=CARTESIAN_POINT('Ctrl Pts',(-2.80786316052735,15.2,10.4726076749094));
#231551=CARTESIAN_POINT('Ctrl Pts',(-2.80769706494405,15.2,10.476273931598));
#231552=CARTESIAN_POINT('Ctrl Pts',(-2.80752407678348,15.2,10.4799551904242));
#231553=CARTESIAN_POINT('Ctrl Pts',(-2.8073078415651,15.2,10.484556764333));
#231554=CARTESIAN_POINT('Ctrl Pts',(-2.80708083707612,15.2,10.489181783764));
#231555=CARTESIAN_POINT('Ctrl Pts',(-2.80684290179891,15.2,10.4938300164711));
#231556=CARTESIAN_POINT('Ctrl Pts',(-2.8065573794507,15.2,10.4994078960236));
#231557=CARTESIAN_POINT('Ctrl Pts',(-2.80625611574221,15.2,10.505019206722));
#231558=CARTESIAN_POINT('Ctrl Pts',(-2.80593883647383,15.2,10.5106635563652));
#231559=CARTESIAN_POINT('Ctrl Pts',(-2.80567443712674,15.2,10.5153671802988));
#231560=CARTESIAN_POINT('Ctrl Pts',(-2.80539891531652,15.2,10.520093750965));
#231561=CARTESIAN_POINT('Ctrl Pts',(-2.8051121167376,15.2,10.5248430408621));
#231562=CARTESIAN_POINT('Ctrl Pts',(-2.80482531812741,15.2,10.5295923312768));
#231563=CARTESIAN_POINT('Ctrl Pts',(-2.80452724109519,15.2,10.5343643448414));
#231564=CARTESIAN_POINT('Ctrl Pts',(-2.80421773429056,15.2,10.5391588583812));
#231565=CARTESIAN_POINT('Ctrl Pts',(-2.80390822748595,15.2,10.543953371921));
#231566=CARTESIAN_POINT('Ctrl Pts',(-2.80358729037667,15.2,10.5487703863925));
#231567=CARTESIAN_POINT('Ctrl Pts',(-2.80325477105531,15.2,10.5536096819799));
#231568=CARTESIAN_POINT('Ctrl Pts',(-2.80298875558372,15.2,10.5574811186608));
#231569=CARTESIAN_POINT('Ctrl Pts',(-2.80271532805118,15.2,10.561366815711));
#231570=CARTESIAN_POINT('Ctrl Pts',(-2.80243441320205,15.2,10.5652666620355));
#231571=CARTESIAN_POINT('Ctrl Pts',(-2.80215349839119,15.2,10.5691665078288));
#231572=CARTESIAN_POINT('Ctrl Pts',(-2.80186509529851,15.2,10.5730805021414));
#231573=CARTESIAN_POINT('Ctrl Pts',(-2.80156912982347,15.2,10.5770085353744));
#231574=CARTESIAN_POINT('Ctrl Pts',(-2.80127316430811,15.2,10.5809365691426));
#231575=CARTESIAN_POINT('Ctrl Pts',(-2.80096963519882,15.2,10.5848786418107));
#231576=CARTESIAN_POINT('Ctrl Pts',(-2.80065847045821,15.2,10.5888346435443));
#231577=CARTESIAN_POINT('Ctrl Pts',(-2.80034730575999,15.2,10.5927906447388));
#231578=CARTESIAN_POINT('Ctrl Pts',(-2.80002850500653,15.2,10.5967605751396));
#231579=CARTESIAN_POINT('Ctrl Pts',(-2.7997019943118,15.2,10.6007443250903));
#231580=CARTESIAN_POINT('Ctrl Pts',(-2.79937548357257,15.2,10.6047280755837));
#231581=CARTESIAN_POINT('Ctrl Pts',(-2.7990412633604,15.2,10.6087256464091));
#231582=CARTESIAN_POINT('Ctrl Pts',(-2.79869926250842,15.2,10.6127369295166));
#231583=CARTESIAN_POINT('Ctrl Pts',(-2.79818626127706,15.2,10.6187538536314));
#231584=CARTESIAN_POINT('Ctrl Pts',(-2.79765575127205,15.2,10.6248016305437));
#231585=CARTESIAN_POINT('Ctrl Pts',(-2.79710749612651,15.2,10.6308798968207));
#231586=CARTESIAN_POINT('Ctrl Pts',(-2.79665061682196,15.2,10.6359451189023));
#231587=CARTESIAN_POINT('Ctrl Pts',(-2.79618141222916,15.2,10.6410315145312));
#231588=CARTESIAN_POINT('Ctrl Pts',(-2.79569975033096,15.2,10.6461388776321));
#231589=CARTESIAN_POINT('Ctrl Pts',(-2.7953144207914,15.2,10.6502247683355));
#231590=CARTESIAN_POINT('Ctrl Pts',(-2.79492111698961,15.2,10.6543240784612));
#231591=CARTESIAN_POINT('Ctrl Pts',(-2.7945197709672,15.2,10.6584367003529));
#231592=CARTESIAN_POINT('Ctrl Pts',(-2.79391775198827,15.2,10.6646056326302));
#231593=CARTESIAN_POINT('Ctrl Pts',(-2.79329763852748,15.2,10.6708045226549));
#231594=CARTESIAN_POINT('Ctrl Pts',(-2.79265920355147,15.2,10.6770330119273));
#231595=CARTESIAN_POINT('Ctrl Pts',(-2.79212717438547,15.2,10.6822234198429));
#231596=CARTESIAN_POINT('Ctrl Pts',(-2.79158242218066,15.2,10.6874343871012));
#231597=CARTESIAN_POINT('Ctrl Pts',(-2.79102481877539,15.2,10.6926657074721));
#231598=CARTESIAN_POINT('Ctrl Pts',(-2.79057873602686,15.2,10.6968507639969));
#231599=CARTESIAN_POINT('Ctrl Pts',(-2.79012442798107,15.2,10.7010488486882));
#231600=CARTESIAN_POINT('Ctrl Pts',(-2.78966182989945,15.2,10.7052598571968));
#231601=CARTESIAN_POINT('Ctrl Pts',(-2.78896793284005,15.2,10.7115763693859));
#231602=CARTESIAN_POINT('Ctrl Pts',(-2.78825538343487,15.2,10.7179219609055));
#231603=CARTESIAN_POINT('Ctrl Pts',(-2.78752396454142,15.2,10.7242962890362));
#231604=CARTESIAN_POINT('Ctrl Pts',(-2.78703635196794,15.2,10.7285458409303));
#231605=CARTESIAN_POINT('Ctrl Pts',(-2.7865403551988,15.2,10.7328081643545));
#231606=CARTESIAN_POINT('Ctrl Pts',(-2.78603590807423,15.2,10.7370831570593));
#231607=CARTESIAN_POINT('Ctrl Pts',(-2.78553146088093,15.2,10.7413581503466));
#231608=CARTESIAN_POINT('Ctrl Pts',(-2.78501856659518,15.2,10.7456458155822));
#231609=CARTESIAN_POINT('Ctrl Pts',(-2.78449716123343,15.2,10.7499460494833));
#231610=CARTESIAN_POINT('Ctrl Pts',(-2.78397575587167,15.2,10.7542462833843));
#231611=CARTESIAN_POINT('Ctrl Pts',(-2.78344583971171,15.2,10.7585590878035));
#231612=CARTESIAN_POINT('Ctrl Pts',(-2.78290735240371,15.2,10.7628843617071));
#231613=CARTESIAN_POINT('Ctrl Pts',(-2.78223424337876,15.2,10.7682909532027));
#231614=CARTESIAN_POINT('Ctrl Pts',(-2.78154773961424,15.2,10.7737170298384));
#231615=CARTESIAN_POINT('Ctrl Pts',(-2.78084772635831,15.2,10.7791623955627));
#231616=CARTESIAN_POINT('Ctrl Pts',(-2.78014771302609,15.2,10.7846077618805));
#231617=CARTESIAN_POINT('Ctrl Pts',(-2.77943418926074,15.2,10.7900724199398));
#231618=CARTESIAN_POINT('Ctrl Pts',(-2.77870703780353,15.2,10.7955561760493));
#231619=CARTESIAN_POINT('Ctrl Pts',(-2.77812531660606,15.2,10.799943181176));
#231620=CARTESIAN_POINT('Ctrl Pts',(-2.77753487641009,15.2,10.8043424089258));
#231621=CARTESIAN_POINT('Ctrl Pts',(-2.77693565520801,15.2,10.8087537615196));
#231622=CARTESIAN_POINT('Ctrl Pts',(-2.77618662874624,15.2,10.8142679519614));
#231623=CARTESIAN_POINT('Ctrl Pts',(-2.77542388508326,15.2,10.8198010883122));
#231624=CARTESIAN_POINT('Ctrl Pts',(-2.77464731174922,15.2,10.8253529803965));
#231625=CARTESIAN_POINT('Ctrl Pts',(-2.77402605313277,15.2,10.8297944937008));
#231626=CARTESIAN_POINT('Ctrl Pts',(-2.77339594292364,15.2,10.8342480107222));
#231627=CARTESIAN_POINT('Ctrl Pts',(-2.7727569250879,15.2,10.8387134347448));
#231628=CARTESIAN_POINT('Ctrl Pts',(-2.77227766160226,15.2,10.8420625035223));
#231629=CARTESIAN_POINT('Ctrl Pts',(-2.77179338738188,15.2,10.8454182705767));
#231630=CARTESIAN_POINT('Ctrl Pts',(-2.77130407889342,15.2,10.8487806952329));
#231631=CARTESIAN_POINT('Ctrl Pts',(-2.77081477049385,15.2,10.8521431192783));
#231632=CARTESIAN_POINT('Ctrl Pts',(-2.77032042864414,15.2,10.8555121994231));
#231633=CARTESIAN_POINT('Ctrl Pts',(-2.76982102867842,15.2,10.8588878976365));
#231634=CARTESIAN_POINT('Ctrl Pts',(-2.7693216287127,15.2,10.8622635958499));
#231635=CARTESIAN_POINT('Ctrl Pts',(-2.76881717020973,15.2,10.8656459103087));
#231636=CARTESIAN_POINT('Ctrl Pts',(-2.76830763218613,15.2,10.8690348023944));
#231637=CARTESIAN_POINT('Ctrl Pts',(-2.76762824818553,15.2,10.8735533249703));
#231638=CARTESIAN_POINT('Ctrl Pts',(-2.76693983013118,15.2,10.878083540266));
#231639=CARTESIAN_POINT('Ctrl Pts',(-2.7662423263558,15.2,10.8826253522824));
#231640=CARTESIAN_POINT('Ctrl Pts',(-2.7653704465653,15.2,10.8883026177669));
#231641=CARTESIAN_POINT('Ctrl Pts',(-2.76448436840411,15.2,10.8939980046414));
#231642=CARTESIAN_POINT('Ctrl Pts',(-2.76358398842956,15.2,10.8997113295784));
#231643=CARTESIAN_POINT('Ctrl Pts',(-2.76304376046446,15.2,10.9031393244161));
#231644=CARTESIAN_POINT('Ctrl Pts',(-2.76249838293274,15.2,10.906573776609));
#231645=CARTESIAN_POINT('Ctrl Pts',(-2.76194783457844,15.2,10.9100146467748));
#231646=CARTESIAN_POINT('Ctrl Pts',(-2.76139728612413,15.2,10.9134555175657));
#231647=CARTESIAN_POINT('Ctrl Pts',(-2.76084156691003,15.2,10.9169028066167));
#231648=CARTESIAN_POINT('Ctrl Pts',(-2.76028065436947,15.2,10.9203564739945));
#231649=CARTESIAN_POINT('Ctrl Pts',(-2.75953277115189,15.2,10.9249613627859));
#231650=CARTESIAN_POINT('Ctrl Pts',(-2.7587756547855,15.2,10.9295775919452));
#231651=CARTESIAN_POINT('Ctrl Pts',(-2.75800925557099,15.2,10.9342050691217));
#231652=CARTESIAN_POINT('Ctrl Pts',(-2.75705125647454,15.2,10.9399894160652));
#231653=CARTESIAN_POINT('Ctrl Pts',(-2.75607874934396,15.2,10.9457913356315));
#231654=CARTESIAN_POINT('Ctrl Pts',(-2.7550916377423,15.2,10.9516106501718));
#231655=CARTESIAN_POINT('Ctrl Pts',(-2.75430194841792,15.2,10.9562661020577));
#231656=CARTESIAN_POINT('Ctrl Pts',(-2.75350291196016,15.2,10.9609326860642));
#231657=CARTESIAN_POINT('Ctrl Pts',(-2.75269447685957,15.2,10.9656103107648));
#231658=CARTESIAN_POINT('Ctrl Pts',(-2.75208815058921,15.2,10.9691185289715));
#231659=CARTESIAN_POINT('Ctrl Pts',(-2.75147653929414,15.2,10.9726329571445));
#231660=CARTESIAN_POINT('Ctrl Pts',(-2.75085961998276,15.2,10.9761535573505));
#231661=CARTESIAN_POINT('Ctrl Pts',(-2.75003706093827,15.2,10.9808476907452));
#231662=CARTESIAN_POINT('Ctrl Pts',(-2.74920506689291,15.2,10.9855527972988));
#231663=CARTESIAN_POINT('Ctrl Pts',(-2.74836358912933,15.2,10.9902687852456));
#231664=CARTESIAN_POINT('Ctrl Pts',(-2.74752211125111,15.2,10.9949847738348));
#231665=CARTESIAN_POINT('Ctrl Pts',(-2.74667114958644,15.2,10.9997116435735));
#231666=CARTESIAN_POINT('Ctrl Pts',(-2.74581065625784,15.2,11.0044493055198));
#231667=CARTESIAN_POINT('Ctrl Pts',(-2.74516528632001,15.2,11.0080025516568));
#231668=CARTESIAN_POINT('Ctrl Pts',(-2.74451455336314,15.2,11.0115618678267));
#231669=CARTESIAN_POINT('Ctrl Pts',(-2.74385843900902,15.2,11.0151272160467));
#231670=CARTESIAN_POINT('Ctrl Pts',(-2.74320232465491,15.2,11.0186925642667));
#231671=CARTESIAN_POINT('Ctrl Pts',(-2.74254082889799,15.2,11.0222639453739));
#231672=CARTESIAN_POINT('Ctrl Pts',(-2.74187393058936,15.2,11.0258413206185));
#231673=CARTESIAN_POINT('Ctrl Pts',(-2.74120703228073,15.2,11.029418695863));
#231674=CARTESIAN_POINT('Ctrl Pts',(-2.74053473170581,15.2,11.033002066032));
#231675=CARTESIAN_POINT('Ctrl Pts',(-2.73985700985617,15.2,11.0365913931925));
#231676=CARTESIAN_POINT('Ctrl Pts',(-2.73917928788341,15.2,11.040180721005));
#231677=CARTESIAN_POINT('Ctrl Pts',(-2.73849614410079,15.2,11.0437760055275));
#231678=CARTESIAN_POINT('Ctrl Pts',(-2.73780755908331,15.2,11.0473772103017));
#231679=CARTESIAN_POINT('Ctrl Pts',(-2.73665991767939,15.2,11.0533792167321));
#231680=CARTESIAN_POINT('Ctrl Pts',(-2.73549716116342,15.2,11.0593976664086));
#231681=CARTESIAN_POINT('Ctrl Pts',(-2.73431919990417,15.2,11.0654323862356));
#231682=CARTESIAN_POINT('Ctrl Pts',(-2.73314123851652,15.2,11.0714671067204));
#231683=CARTESIAN_POINT('Ctrl Pts',(-2.73194807286801,15.2,11.0775180970522));
#231684=CARTESIAN_POINT('Ctrl Pts',(-2.73073961488316,15.2,11.0835851884397));
#231685=CARTESIAN_POINT('Ctrl Pts',(-2.73001453998687,15.2,11.0872254438013));
#231686=CARTESIAN_POINT('Ctrl Pts',(-2.72928396131402,15.2,11.0908714962312));
#231687=CARTESIAN_POINT('Ctrl Pts',(-2.72854785787295,15.2,11.0945233075544));
#231688=CARTESIAN_POINT('Ctrl Pts',(-2.72732101911654,15.2,11.1006096582117));
#231689=CARTESIAN_POINT('Ctrl Pts',(-2.72607883461512,15.2,11.1067120056901));
#231690=CARTESIAN_POINT('Ctrl Pts',(-2.72482121919792,15.2,11.1128301757163));
#231691=CARTESIAN_POINT('Ctrl Pts',(-2.72406664975569,15.2,11.1165010786657));
#231692=CARTESIAN_POINT('Ctrl Pts',(-2.72330652591187,15.2,11.1201776796168));
#231693=CARTESIAN_POINT('Ctrl Pts',(-2.7225408290915,15.2,11.1238599450277));
#231694=CARTESIAN_POINT('Ctrl Pts',(-2.72177513241023,15.2,11.1275422097697));
#231695=CARTESIAN_POINT('Ctrl Pts',(-2.72100386532091,15.2,11.1312301398864));
#231696=CARTESIAN_POINT('Ctrl Pts',(-2.72022700793199,15.2,11.1349236969193));
#231697=CARTESIAN_POINT('Ctrl Pts',(-2.71945015054306,15.2,11.1386172539523));
#231698=CARTESIAN_POINT('Ctrl Pts',(-2.71866770162434,15.2,11.1423164364044));
#231699=CARTESIAN_POINT('Ctrl Pts',(-2.71787964073271,15.2,11.146021201495));
#231700=CARTESIAN_POINT('Ctrl Pts',(-2.71709157984108,15.2,11.1497259665855));
#231701=CARTESIAN_POINT('Ctrl Pts',(-2.71629790459204,15.2,11.1534363121814));
#231702=CARTESIAN_POINT('Ctrl Pts',(-2.71549860045082,15.2,11.1571522052299));
#231703=CARTESIAN_POINT('Ctrl Pts',(-2.71416642683371,15.2,11.1633453605357));
#231704=CARTESIAN_POINT('Ctrl Pts',(-2.71281861996396,15.2,11.1695539166432));
#231705=CARTESIAN_POINT('Ctrl Pts',(-2.71145515300006,15.2,11.175777868));
#231706=CARTESIAN_POINT('Ctrl Pts',(-1.76496130700006,15.2,10.22377311));
#231707=CARTESIAN_POINT('Ctrl Pts',(-1.76496130700006,11.6,10.22377311));
#231708=CARTESIAN_POINT('Ctrl Pts',(-1.76500562500005,15.2,10.223941742));
#231709=CARTESIAN_POINT('Ctrl Pts',(-1.76500562500005,11.6,10.223941742));
#231710=CARTESIAN_POINT('Ctrl Pts',(-1.76509588900006,15.2,10.224284874));
#231711=CARTESIAN_POINT('Ctrl Pts',(-1.76509588900006,11.6,10.224284874));
#231712=CARTESIAN_POINT('Ctrl Pts',(-1.76523291900006,15.2,10.224804732));
#231713=CARTESIAN_POINT('Ctrl Pts',(-1.76523291900006,11.6,10.224804732));
#231714=CARTESIAN_POINT('Ctrl Pts',(-1.76541803300006,15.2,10.22550489));
#231715=CARTESIAN_POINT('Ctrl Pts',(-1.76541803300006,11.6,10.22550489));
#231716=CARTESIAN_POINT('Ctrl Pts',(-1.76565305800006,15.2,10.226390254));
#231717=CARTESIAN_POINT('Ctrl Pts',(-1.76565305800006,11.6,10.226390254));
#231718=CARTESIAN_POINT('Ctrl Pts',(-1.76589279600006,15.2,10.227289726));
#231719=CARTESIAN_POINT('Ctrl Pts',(-1.76589279600006,11.6,10.227289726));
#231720=CARTESIAN_POINT('Ctrl Pts',(-1.76613589400006,15.2,10.22819815));
#231721=CARTESIAN_POINT('Ctrl Pts',(-1.76613589400006,11.6,10.22819815));
#231722=CARTESIAN_POINT('Ctrl Pts',(-1.76638236600006,15.2,10.229115492));
#231723=CARTESIAN_POINT('Ctrl Pts',(-1.76638236600006,11.6,10.229115492));
#231724=CARTESIAN_POINT('Ctrl Pts',(-1.76663222000006,15.2,10.230041723));
#231725=CARTESIAN_POINT('Ctrl Pts',(-1.76663222000006,11.6,10.230041723));
#231726=CARTESIAN_POINT('Ctrl Pts',(-1.76688546700006,15.2,10.230976812));
#231727=CARTESIAN_POINT('Ctrl Pts',(-1.76688546700006,11.6,10.230976812));
#231728=CARTESIAN_POINT('Ctrl Pts',(-1.76714211800005,15.2,10.231920729));
#231729=CARTESIAN_POINT('Ctrl Pts',(-1.76714211800005,11.6,10.231920729));
#231730=CARTESIAN_POINT('Ctrl Pts',(-1.76740218300006,15.2,10.232873444));
#231731=CARTESIAN_POINT('Ctrl Pts',(-1.76740218300006,11.6,10.232873444));
#231732=CARTESIAN_POINT('Ctrl Pts',(-1.76766567100006,15.2,10.233834926));
#231733=CARTESIAN_POINT('Ctrl Pts',(-1.76766567100006,11.6,10.233834926));
#231734=CARTESIAN_POINT('Ctrl Pts',(-1.76793259300006,15.2,10.234805146));
#231735=CARTESIAN_POINT('Ctrl Pts',(-1.76793259300006,11.6,10.234805146));
#231736=CARTESIAN_POINT('Ctrl Pts',(-1.76820296100006,15.2,10.235784074));
#231737=CARTESIAN_POINT('Ctrl Pts',(-1.76820296100006,11.6,10.235784074));
#231738=CARTESIAN_POINT('Ctrl Pts',(-1.76847678200006,15.2,10.23677168));
#231739=CARTESIAN_POINT('Ctrl Pts',(-1.76847678200006,11.6,10.23677168));
#231740=CARTESIAN_POINT('Ctrl Pts',(-1.76875406800006,15.2,10.237767935));
#231741=CARTESIAN_POINT('Ctrl Pts',(-1.76875406800006,11.6,10.237767935));
#231742=CARTESIAN_POINT('Ctrl Pts',(-1.76903482800005,15.2,10.23877281));
#231743=CARTESIAN_POINT('Ctrl Pts',(-1.76903482800005,11.6,10.23877281));
#231744=CARTESIAN_POINT('Ctrl Pts',(-1.76931907200006,15.2,10.239786274));
#231745=CARTESIAN_POINT('Ctrl Pts',(-1.76931907200006,11.6,10.239786274));
#231746=CARTESIAN_POINT('Ctrl Pts',(-1.76960681100006,15.2,10.2408083));
#231747=CARTESIAN_POINT('Ctrl Pts',(-1.76960681100006,11.6,10.2408083));
#231748=CARTESIAN_POINT('Ctrl Pts',(-1.76989805200006,15.2,10.241838858));
#231749=CARTESIAN_POINT('Ctrl Pts',(-1.76989805200006,11.6,10.241838858));
#231750=CARTESIAN_POINT('Ctrl Pts',(-1.77019280700006,15.2,10.24287792));
#231751=CARTESIAN_POINT('Ctrl Pts',(-1.77019280700006,11.6,10.24287792));
#231752=CARTESIAN_POINT('Ctrl Pts',(-1.77049108600006,15.2,10.243925457));
#231753=CARTESIAN_POINT('Ctrl Pts',(-1.77049108600006,11.6,10.243925457));
#231754=CARTESIAN_POINT('Ctrl Pts',(-1.77079289700006,15.2,10.244981439));
#231755=CARTESIAN_POINT('Ctrl Pts',(-1.77079289700006,11.6,10.244981439));
#231756=CARTESIAN_POINT('Ctrl Pts',(-1.77109824900006,15.2,10.246045839));
#231757=CARTESIAN_POINT('Ctrl Pts',(-1.77109824900006,11.6,10.246045839));
#231758=CARTESIAN_POINT('Ctrl Pts',(-1.77140715400005,15.2,10.24711863));
#231759=CARTESIAN_POINT('Ctrl Pts',(-1.77140715400005,11.6,10.24711863));
#231760=CARTESIAN_POINT('Ctrl Pts',(-1.77171961900006,15.2,10.248199782));
#231761=CARTESIAN_POINT('Ctrl Pts',(-1.77171961900006,11.6,10.248199782));
#231762=CARTESIAN_POINT('Ctrl Pts',(-1.77203565500006,15.2,10.249289266));
#231763=CARTESIAN_POINT('Ctrl Pts',(-1.77203565500006,11.6,10.249289266));
#231764=CARTESIAN_POINT('Ctrl Pts',(-1.77235527000006,15.2,10.250387056));
#231765=CARTESIAN_POINT('Ctrl Pts',(-1.77235527000006,11.6,10.250387056));
#231766=CARTESIAN_POINT('Ctrl Pts',(-1.77267847400006,15.2,10.251493125));
#231767=CARTESIAN_POINT('Ctrl Pts',(-1.77267847400006,11.6,10.251493125));
#231768=CARTESIAN_POINT('Ctrl Pts',(-1.77300527500006,15.2,10.252607443));
#231769=CARTESIAN_POINT('Ctrl Pts',(-1.77300527500006,11.6,10.252607443));
#231770=CARTESIAN_POINT('Ctrl Pts',(-1.77333568300006,15.2,10.253729984));
#231771=CARTESIAN_POINT('Ctrl Pts',(-1.77333568300006,11.6,10.253729984));
#231772=CARTESIAN_POINT('Ctrl Pts',(-1.77366970800006,15.2,10.254860721));
#231773=CARTESIAN_POINT('Ctrl Pts',(-1.77366970800006,11.6,10.254860721));
#231774=CARTESIAN_POINT('Ctrl Pts',(-1.77400735800005,15.2,10.255999624));
#231775=CARTESIAN_POINT('Ctrl Pts',(-1.77400735800005,11.6,10.255999624));
#231776=CARTESIAN_POINT('Ctrl Pts',(-1.77434864200006,15.2,10.257146669));
#231777=CARTESIAN_POINT('Ctrl Pts',(-1.77434864200006,11.6,10.257146669));
#231778=CARTESIAN_POINT('Ctrl Pts',(-1.77469356900006,15.2,10.258301828));
#231779=CARTESIAN_POINT('Ctrl Pts',(-1.77469356900006,11.6,10.258301828));
#231780=CARTESIAN_POINT('Ctrl Pts',(-1.77504214700006,15.2,10.259465072));
#231781=CARTESIAN_POINT('Ctrl Pts',(-1.77504214700006,11.6,10.259465072));
#231782=CARTESIAN_POINT('Ctrl Pts',(-1.77539438600005,15.2,10.260636378));
#231783=CARTESIAN_POINT('Ctrl Pts',(-1.77539438600005,11.6,10.260636378));
#231784=CARTESIAN_POINT('Ctrl Pts',(-1.77575029400006,15.2,10.261815716));
#231785=CARTESIAN_POINT('Ctrl Pts',(-1.77575029400006,11.6,10.261815716));
#231786=CARTESIAN_POINT('Ctrl Pts',(-1.77610988000006,15.2,10.263003062));
#231787=CARTESIAN_POINT('Ctrl Pts',(-1.77610988000006,11.6,10.263003062));
#231788=CARTESIAN_POINT('Ctrl Pts',(-1.77647315400006,15.2,10.264198387));
#231789=CARTESIAN_POINT('Ctrl Pts',(-1.77647315400006,11.6,10.264198387));
#231790=CARTESIAN_POINT('Ctrl Pts',(-1.77684012100006,15.2,10.265401667));
#231791=CARTESIAN_POINT('Ctrl Pts',(-1.77684012100006,11.6,10.265401667));
#231792=CARTESIAN_POINT('Ctrl Pts',(-1.77721079300006,15.2,10.266612873));
#231793=CARTESIAN_POINT('Ctrl Pts',(-1.77721079300006,11.6,10.266612873));
#231794=CARTESIAN_POINT('Ctrl Pts',(-1.77758517500005,15.2,10.267831982));
#231795=CARTESIAN_POINT('Ctrl Pts',(-1.77758517500005,11.6,10.267831982));
#231796=CARTESIAN_POINT('Ctrl Pts',(-1.77796328000006,15.2,10.269058967));
#231797=CARTESIAN_POINT('Ctrl Pts',(-1.77796328000006,11.6,10.269058967));
#231798=CARTESIAN_POINT('Ctrl Pts',(-1.77834511300006,15.2,10.2702938));
#231799=CARTESIAN_POINT('Ctrl Pts',(-1.77834511300006,11.6,10.2702938));
#231800=CARTESIAN_POINT('Ctrl Pts',(-1.77873068400005,15.2,10.271536458));
#231801=CARTESIAN_POINT('Ctrl Pts',(-1.77873068400005,11.6,10.271536458));
#231802=CARTESIAN_POINT('Ctrl Pts',(-1.77911999900006,15.2,10.272786914));
#231803=CARTESIAN_POINT('Ctrl Pts',(-1.77911999900006,11.6,10.272786914));
#231804=CARTESIAN_POINT('Ctrl Pts',(-1.77951306900006,15.2,10.274045143));
#231805=CARTESIAN_POINT('Ctrl Pts',(-1.77951306900006,11.6,10.274045143));
#231806=CARTESIAN_POINT('Ctrl Pts',(-1.77990990000006,15.2,10.275311119));
#231807=CARTESIAN_POINT('Ctrl Pts',(-1.77990990000006,11.6,10.275311119));
#231808=CARTESIAN_POINT('Ctrl Pts',(-1.78031050100006,15.2,10.276584816));
#231809=CARTESIAN_POINT('Ctrl Pts',(-1.78031050100006,11.6,10.276584816));
#231810=CARTESIAN_POINT('Ctrl Pts',(-1.78071488100006,15.2,10.277866211));
#231811=CARTESIAN_POINT('Ctrl Pts',(-1.78071488100006,11.6,10.277866211));
#231812=CARTESIAN_POINT('Ctrl Pts',(-1.78112304700006,15.2,10.279155276));
#231813=CARTESIAN_POINT('Ctrl Pts',(-1.78112304700006,11.6,10.279155276));
#231814=CARTESIAN_POINT('Ctrl Pts',(-1.78153500600006,15.2,10.280451988));
#231815=CARTESIAN_POINT('Ctrl Pts',(-1.78153500600006,11.6,10.280451988));
#231816=CARTESIAN_POINT('Ctrl Pts',(-1.78195076800006,15.2,10.281756322));
#231817=CARTESIAN_POINT('Ctrl Pts',(-1.78195076800006,11.6,10.281756322));
#231818=CARTESIAN_POINT('Ctrl Pts',(-1.78237034000006,15.2,10.283068252));
#231819=CARTESIAN_POINT('Ctrl Pts',(-1.78237034000006,11.6,10.283068252));
#231820=CARTESIAN_POINT('Ctrl Pts',(-1.78279372900006,15.2,10.284387754));
#231821=CARTESIAN_POINT('Ctrl Pts',(-1.78279372900006,11.6,10.284387754));
#231822=CARTESIAN_POINT('Ctrl Pts',(-1.78322094500006,15.2,10.285714803));
#231823=CARTESIAN_POINT('Ctrl Pts',(-1.78322094500006,11.6,10.285714803));
#231824=CARTESIAN_POINT('Ctrl Pts',(-1.78365199300006,15.2,10.287049375));
#231825=CARTESIAN_POINT('Ctrl Pts',(-1.78365199300006,11.6,10.287049375));
#231826=CARTESIAN_POINT('Ctrl Pts',(-1.78408688300005,15.2,10.288391445));
#231827=CARTESIAN_POINT('Ctrl Pts',(-1.78408688300005,11.6,10.288391445));
#231828=CARTESIAN_POINT('Ctrl Pts',(-1.78452562100006,15.2,10.28974099));
#231829=CARTESIAN_POINT('Ctrl Pts',(-1.78452562100006,11.6,10.28974099));
#231830=CARTESIAN_POINT('Ctrl Pts',(-1.78496821700006,15.2,10.291097984));
#231831=CARTESIAN_POINT('Ctrl Pts',(-1.78496821700006,11.6,10.291097984));
#231832=CARTESIAN_POINT('Ctrl Pts',(-1.78541467400006,15.2,10.292462403));
#231833=CARTESIAN_POINT('Ctrl Pts',(-1.78541467400006,11.6,10.292462403));
#231834=CARTESIAN_POINT('Ctrl Pts',(-1.78586500500006,15.2,10.293834224));
#231835=CARTESIAN_POINT('Ctrl Pts',(-1.78586500500006,11.6,10.293834224));
#231836=CARTESIAN_POINT('Ctrl Pts',(-1.78631921400006,15.2,10.295213423));
#231837=CARTESIAN_POINT('Ctrl Pts',(-1.78631921400006,11.6,10.295213423));
#231838=CARTESIAN_POINT('Ctrl Pts',(-1.78677730900006,15.2,10.296599975));
#231839=CARTESIAN_POINT('Ctrl Pts',(-1.78677730900006,11.6,10.296599975));
#231840=CARTESIAN_POINT('Ctrl Pts',(-1.78723929800006,15.2,10.297993857));
#231841=CARTESIAN_POINT('Ctrl Pts',(-1.78723929800006,11.6,10.297993857));
#231842=CARTESIAN_POINT('Ctrl Pts',(-1.78770518700006,15.2,10.299395046));
#231843=CARTESIAN_POINT('Ctrl Pts',(-1.78770518700006,11.6,10.299395046));
#231844=CARTESIAN_POINT('Ctrl Pts',(-1.78817498600006,15.2,10.300803517));
#231845=CARTESIAN_POINT('Ctrl Pts',(-1.78817498600006,11.6,10.300803517));
#231846=CARTESIAN_POINT('Ctrl Pts',(-1.78864870100006,15.2,10.302219248));
#231847=CARTESIAN_POINT('Ctrl Pts',(-1.78864870100006,11.6,10.302219248));
#231848=CARTESIAN_POINT('Ctrl Pts',(-1.78912633700006,15.2,10.303642214));
#231849=CARTESIAN_POINT('Ctrl Pts',(-1.78912633700006,11.6,10.303642214));
#231850=CARTESIAN_POINT('Ctrl Pts',(-1.78960790600006,15.2,10.305072394));
#231851=CARTESIAN_POINT('Ctrl Pts',(-1.78960790600006,11.6,10.305072394));
#231852=CARTESIAN_POINT('Ctrl Pts',(-1.79009341000006,15.2,10.306509761));
#231853=CARTESIAN_POINT('Ctrl Pts',(-1.79009341000006,11.6,10.306509761));
#231854=CARTESIAN_POINT('Ctrl Pts',(-1.79058285800005,15.2,10.307954296));
#231855=CARTESIAN_POINT('Ctrl Pts',(-1.79058285800005,11.6,10.307954296));
#231856=CARTESIAN_POINT('Ctrl Pts',(-1.79107625800006,15.2,10.309405975));
#231857=CARTESIAN_POINT('Ctrl Pts',(-1.79107625800006,11.6,10.309405975));
#231858=CARTESIAN_POINT('Ctrl Pts',(-1.79157361700006,15.2,10.310864773));
#231859=CARTESIAN_POINT('Ctrl Pts',(-1.79157361700006,11.6,10.310864773));
#231860=CARTESIAN_POINT('Ctrl Pts',(-1.79207494100006,15.2,10.312330668));
#231861=CARTESIAN_POINT('Ctrl Pts',(-1.79207494100006,11.6,10.312330668));
#231862=CARTESIAN_POINT('Ctrl Pts',(-1.79258023800006,15.2,10.313803638));
#231863=CARTESIAN_POINT('Ctrl Pts',(-1.79258023800006,11.6,10.313803638));
#231864=CARTESIAN_POINT('Ctrl Pts',(-1.79308951300006,15.2,10.315283661));
#231865=CARTESIAN_POINT('Ctrl Pts',(-1.79308951300006,11.6,10.315283661));
#231866=CARTESIAN_POINT('Ctrl Pts',(-1.79360277400006,15.2,10.316770712));
#231867=CARTESIAN_POINT('Ctrl Pts',(-1.79360277400006,11.6,10.316770712));
#231868=CARTESIAN_POINT('Ctrl Pts',(-1.79412002900006,15.2,10.31826477));
#231869=CARTESIAN_POINT('Ctrl Pts',(-1.79412002900006,11.6,10.31826477));
#231870=CARTESIAN_POINT('Ctrl Pts',(-1.79464128300005,15.2,10.319765814));
#231871=CARTESIAN_POINT('Ctrl Pts',(-1.79464128300005,11.6,10.319765814));
#231872=CARTESIAN_POINT('Ctrl Pts',(-1.79516654300006,15.2,10.321273819));
#231873=CARTESIAN_POINT('Ctrl Pts',(-1.79516654300006,11.6,10.321273819));
#231874=CARTESIAN_POINT('Ctrl Pts',(-1.79569581700005,15.2,10.322788764));
#231875=CARTESIAN_POINT('Ctrl Pts',(-1.79569581700005,11.6,10.322788764));
#231876=CARTESIAN_POINT('Ctrl Pts',(-1.79622911000005,15.2,10.324310627));
#231877=CARTESIAN_POINT('Ctrl Pts',(-1.79622911000005,11.6,10.324310627));
#231878=CARTESIAN_POINT('Ctrl Pts',(-1.79676643100006,15.2,10.325839385));
#231879=CARTESIAN_POINT('Ctrl Pts',(-1.79676643100006,11.6,10.325839385));
#231880=CARTESIAN_POINT('Ctrl Pts',(-1.79730778400006,15.2,10.327375017));
#231881=CARTESIAN_POINT('Ctrl Pts',(-1.79730778400006,11.6,10.327375017));
#231882=CARTESIAN_POINT('Ctrl Pts',(-1.79785317600006,15.2,10.328917501));
#231883=CARTESIAN_POINT('Ctrl Pts',(-1.79785317600006,11.6,10.328917501));
#231884=CARTESIAN_POINT('Ctrl Pts',(-1.79840261400006,15.2,10.330466814));
#231885=CARTESIAN_POINT('Ctrl Pts',(-1.79840261400006,11.6,10.330466814));
#231886=CARTESIAN_POINT('Ctrl Pts',(-1.79895610500005,15.2,10.332022936));
#231887=CARTESIAN_POINT('Ctrl Pts',(-1.79895610500005,11.6,10.332022936));
#231888=CARTESIAN_POINT('Ctrl Pts',(-1.79951365500005,15.2,10.333585844));
#231889=CARTESIAN_POINT('Ctrl Pts',(-1.79951365500005,11.6,10.333585844));
#231890=CARTESIAN_POINT('Ctrl Pts',(-1.80007527000006,15.2,10.335155517));
#231891=CARTESIAN_POINT('Ctrl Pts',(-1.80007527000006,11.6,10.335155517));
#231892=CARTESIAN_POINT('Ctrl Pts',(-1.80064095700006,15.2,10.336731933));
#231893=CARTESIAN_POINT('Ctrl Pts',(-1.80064095700006,11.6,10.336731933));
#231894=CARTESIAN_POINT('Ctrl Pts',(-1.80121072300006,15.2,10.338315071));
#231895=CARTESIAN_POINT('Ctrl Pts',(-1.80121072300006,11.6,10.338315071));
#231896=CARTESIAN_POINT('Ctrl Pts',(-1.80178457200005,15.2,10.339904909));
#231897=CARTESIAN_POINT('Ctrl Pts',(-1.80178457200005,11.6,10.339904909));
#231898=CARTESIAN_POINT('Ctrl Pts',(-1.80236251100005,15.2,10.341501427));
#231899=CARTESIAN_POINT('Ctrl Pts',(-1.80236251100005,11.6,10.341501427));
#231900=CARTESIAN_POINT('Ctrl Pts',(-1.80294454800005,15.2,10.343104602));
#231901=CARTESIAN_POINT('Ctrl Pts',(-1.80294454800005,11.6,10.343104602));
#231902=CARTESIAN_POINT('Ctrl Pts',(-1.80353068700006,15.2,10.344714415));
#231903=CARTESIAN_POINT('Ctrl Pts',(-1.80353068700006,11.6,10.344714415));
#231904=CARTESIAN_POINT('Ctrl Pts',(-1.80412093600005,15.2,10.346330843));
#231905=CARTESIAN_POINT('Ctrl Pts',(-1.80412093600005,11.6,10.346330843));
#231906=CARTESIAN_POINT('Ctrl Pts',(-1.80471530000006,15.2,10.347953866));
#231907=CARTESIAN_POINT('Ctrl Pts',(-1.80471530000006,11.6,10.347953866));
#231908=CARTESIAN_POINT('Ctrl Pts',(-1.80531378500006,15.2,10.349583462));
#231909=CARTESIAN_POINT('Ctrl Pts',(-1.80531378500006,11.6,10.349583462));
#231910=CARTESIAN_POINT('Ctrl Pts',(-1.80591639800005,15.2,10.351219613));
#231911=CARTESIAN_POINT('Ctrl Pts',(-1.80591639800005,11.6,10.351219613));
#231912=CARTESIAN_POINT('Ctrl Pts',(-1.80652314300006,15.2,10.352862294));
#231913=CARTESIAN_POINT('Ctrl Pts',(-1.80652314300006,11.6,10.352862294));
#231914=CARTESIAN_POINT('Ctrl Pts',(-1.80713402800006,15.2,10.354511488));
#231915=CARTESIAN_POINT('Ctrl Pts',(-1.80713402800006,11.6,10.354511488));
#231916=CARTESIAN_POINT('Ctrl Pts',(-1.80774906000006,15.2,10.356167173));
#231917=CARTESIAN_POINT('Ctrl Pts',(-1.80774906000006,11.6,10.356167173));
#231918=CARTESIAN_POINT('Ctrl Pts',(-1.80836824100005,15.2,10.357829328));
#231919=CARTESIAN_POINT('Ctrl Pts',(-1.80836824100005,11.6,10.357829328));
#231920=CARTESIAN_POINT('Ctrl Pts',(-1.80899158000006,15.2,10.359497932));
#231921=CARTESIAN_POINT('Ctrl Pts',(-1.80899158000006,11.6,10.359497932));
#231922=CARTESIAN_POINT('Ctrl Pts',(-1.80961908100006,15.2,10.361172966));
#231923=CARTESIAN_POINT('Ctrl Pts',(-1.80961908100006,11.6,10.361172966));
#231924=CARTESIAN_POINT('Ctrl Pts',(-1.81025075100006,15.2,10.36285441));
#231925=CARTESIAN_POINT('Ctrl Pts',(-1.81025075100006,11.6,10.36285441));
#231926=CARTESIAN_POINT('Ctrl Pts',(-1.81088659600006,15.2,10.364542243));
#231927=CARTESIAN_POINT('Ctrl Pts',(-1.81088659600006,11.6,10.364542243));
#231928=CARTESIAN_POINT('Ctrl Pts',(-1.81152662100006,15.2,10.366236443));
#231929=CARTESIAN_POINT('Ctrl Pts',(-1.81152662100006,11.6,10.366236443));
#231930=CARTESIAN_POINT('Ctrl Pts',(-1.81217083200006,15.2,10.367936993));
#231931=CARTESIAN_POINT('Ctrl Pts',(-1.81217083200006,11.6,10.367936993));
#231932=CARTESIAN_POINT('Ctrl Pts',(-1.81281923400005,15.2,10.36964387));
#231933=CARTESIAN_POINT('Ctrl Pts',(-1.81281923400005,11.6,10.36964387));
#231934=CARTESIAN_POINT('Ctrl Pts',(-1.81347183300006,15.2,10.371357057));
#231935=CARTESIAN_POINT('Ctrl Pts',(-1.81347183300006,11.6,10.371357057));
#231936=CARTESIAN_POINT('Ctrl Pts',(-1.81412863500006,15.2,10.373076533));
#231937=CARTESIAN_POINT('Ctrl Pts',(-1.81412863500006,11.6,10.373076533));
#231938=CARTESIAN_POINT('Ctrl Pts',(-1.81478964600006,15.2,10.374802277));
#231939=CARTESIAN_POINT('Ctrl Pts',(-1.81478964600006,11.6,10.374802277));
#231940=CARTESIAN_POINT('Ctrl Pts',(-1.81545487000006,15.2,10.37653427));
#231941=CARTESIAN_POINT('Ctrl Pts',(-1.81545487000006,11.6,10.37653427));
#231942=CARTESIAN_POINT('Ctrl Pts',(-1.81612431400006,15.2,10.378272492));
#231943=CARTESIAN_POINT('Ctrl Pts',(-1.81612431400006,11.6,10.378272492));
#231944=CARTESIAN_POINT('Ctrl Pts',(-1.81679798300005,15.2,10.380016924));
#231945=CARTESIAN_POINT('Ctrl Pts',(-1.81679798300005,11.6,10.380016924));
#231946=CARTESIAN_POINT('Ctrl Pts',(-1.81747588200006,15.2,10.381767546));
#231947=CARTESIAN_POINT('Ctrl Pts',(-1.81747588200006,11.6,10.381767546));
#231948=CARTESIAN_POINT('Ctrl Pts',(-1.81815801700006,15.2,10.383524338));
#231949=CARTESIAN_POINT('Ctrl Pts',(-1.81815801700006,11.6,10.383524338));
#231950=CARTESIAN_POINT('Ctrl Pts',(-1.81884439400006,15.2,10.385287281));
#231951=CARTESIAN_POINT('Ctrl Pts',(-1.81884439400006,11.6,10.385287281));
#231952=CARTESIAN_POINT('Ctrl Pts',(-1.81953501600006,15.2,10.387056356));
#231953=CARTESIAN_POINT('Ctrl Pts',(-1.81953501600006,11.6,10.387056356));
#231954=CARTESIAN_POINT('Ctrl Pts',(-1.82022989100005,15.2,10.388831544));
#231955=CARTESIAN_POINT('Ctrl Pts',(-1.82022989100005,11.6,10.388831544));
#231956=CARTESIAN_POINT('Ctrl Pts',(-1.82092902200006,15.2,10.390612824));
#231957=CARTESIAN_POINT('Ctrl Pts',(-1.82092902200006,11.6,10.390612824));
#231958=CARTESIAN_POINT('Ctrl Pts',(-1.82163241600006,15.2,10.392400178));
#231959=CARTESIAN_POINT('Ctrl Pts',(-1.82163241600006,11.6,10.392400178));
#231960=CARTESIAN_POINT('Ctrl Pts',(-1.82234007900006,15.2,10.394193587));
#231961=CARTESIAN_POINT('Ctrl Pts',(-1.82234007900006,11.6,10.394193587));
#231962=CARTESIAN_POINT('Ctrl Pts',(-1.82305201300006,15.2,10.395993032));
#231963=CARTESIAN_POINT('Ctrl Pts',(-1.82305201300006,11.6,10.395993032));
#231964=CARTESIAN_POINT('Ctrl Pts',(-1.82376822600005,15.2,10.397798493));
#231965=CARTESIAN_POINT('Ctrl Pts',(-1.82376822600005,11.6,10.397798493));
#231966=CARTESIAN_POINT('Ctrl Pts',(-1.82448872100006,15.2,10.399609951));
#231967=CARTESIAN_POINT('Ctrl Pts',(-1.82448872100006,11.6,10.399609951));
#231968=CARTESIAN_POINT('Ctrl Pts',(-1.82521350600006,15.2,10.40142739));
#231969=CARTESIAN_POINT('Ctrl Pts',(-1.82521350600006,11.6,10.40142739));
#231970=CARTESIAN_POINT('Ctrl Pts',(-1.82594258300006,15.2,10.403250787));
#231971=CARTESIAN_POINT('Ctrl Pts',(-1.82594258300006,11.6,10.403250787));
#231972=CARTESIAN_POINT('Ctrl Pts',(-1.82667595900006,15.2,10.405080126));
#231973=CARTESIAN_POINT('Ctrl Pts',(-1.82667595900006,11.6,10.405080126));
#231974=CARTESIAN_POINT('Ctrl Pts',(-1.82741363900006,15.2,10.406915388));
#231975=CARTESIAN_POINT('Ctrl Pts',(-1.82741363900006,11.6,10.406915388));
#231976=CARTESIAN_POINT('Ctrl Pts',(-1.82815562700006,15.2,10.408756553));
#231977=CARTESIAN_POINT('Ctrl Pts',(-1.82815562700006,11.6,10.408756553));
#231978=CARTESIAN_POINT('Ctrl Pts',(-1.82890192700006,15.2,10.410603602));
#231979=CARTESIAN_POINT('Ctrl Pts',(-1.82890192700006,11.6,10.410603602));
#231980=CARTESIAN_POINT('Ctrl Pts',(-1.82965254700005,15.2,10.41245652));
#231981=CARTESIAN_POINT('Ctrl Pts',(-1.82965254700005,11.6,10.41245652));
#231982=CARTESIAN_POINT('Ctrl Pts',(-1.83040749000006,15.2,10.414315285));
#231983=CARTESIAN_POINT('Ctrl Pts',(-1.83040749000006,11.6,10.414315285));
#231984=CARTESIAN_POINT('Ctrl Pts',(-1.83116676100005,15.2,10.416179881));
#231985=CARTESIAN_POINT('Ctrl Pts',(-1.83116676100005,11.6,10.416179881));
#231986=CARTESIAN_POINT('Ctrl Pts',(-1.83193036600006,15.2,10.418050288));
#231987=CARTESIAN_POINT('Ctrl Pts',(-1.83193036600006,11.6,10.418050288));
#231988=CARTESIAN_POINT('Ctrl Pts',(-1.83269830800006,15.2,10.419926488));
#231989=CARTESIAN_POINT('Ctrl Pts',(-1.83269830800006,11.6,10.419926488));
#231990=CARTESIAN_POINT('Ctrl Pts',(-1.83347059200006,15.2,10.421808463));
#231991=CARTESIAN_POINT('Ctrl Pts',(-1.83347059200006,11.6,10.421808463));
#231992=CARTESIAN_POINT('Ctrl Pts',(-1.83424722500006,15.2,10.423696195));
#231993=CARTESIAN_POINT('Ctrl Pts',(-1.83424722500006,11.6,10.423696195));
#231994=CARTESIAN_POINT('Ctrl Pts',(-1.83502821000005,15.2,10.425589666));
#231995=CARTESIAN_POINT('Ctrl Pts',(-1.83502821000005,11.6,10.425589666));
#231996=CARTESIAN_POINT('Ctrl Pts',(-1.83581355100006,15.2,10.427488856));
#231997=CARTESIAN_POINT('Ctrl Pts',(-1.83581355100006,11.6,10.427488856));
#231998=CARTESIAN_POINT('Ctrl Pts',(-1.83660325400006,15.2,10.42939375));
#231999=CARTESIAN_POINT('Ctrl Pts',(-1.83660325400006,11.6,10.42939375));
#232000=CARTESIAN_POINT('Ctrl Pts',(-1.83739732400006,15.2,10.431304328));
#232001=CARTESIAN_POINT('Ctrl Pts',(-1.83739732400006,11.6,10.431304328));
#232002=CARTESIAN_POINT('Ctrl Pts',(-1.83819576400006,15.2,10.433220574));
#232003=CARTESIAN_POINT('Ctrl Pts',(-1.83819576400006,11.6,10.433220574));
#232004=CARTESIAN_POINT('Ctrl Pts',(-1.83899858000005,15.2,10.435142469));
#232005=CARTESIAN_POINT('Ctrl Pts',(-1.83899858000005,11.6,10.435142469));
#232006=CARTESIAN_POINT('Ctrl Pts',(-1.83980577600006,15.2,10.437069993));
#232007=CARTESIAN_POINT('Ctrl Pts',(-1.83980577600006,11.6,10.437069993));
#232008=CARTESIAN_POINT('Ctrl Pts',(-1.84061735700006,15.2,10.439003133));
#232009=CARTESIAN_POINT('Ctrl Pts',(-1.84061735700006,11.6,10.439003133));
#232010=CARTESIAN_POINT('Ctrl Pts',(-1.84143332700006,15.2,10.440941867));
#232011=CARTESIAN_POINT('Ctrl Pts',(-1.84143332700006,11.6,10.440941867));
#232012=CARTESIAN_POINT('Ctrl Pts',(-1.84225369100006,15.2,10.442886179));
#232013=CARTESIAN_POINT('Ctrl Pts',(-1.84225369100006,11.6,10.442886179));
#232014=CARTESIAN_POINT('Ctrl Pts',(-1.84307845300005,15.2,10.444836052));
#232015=CARTESIAN_POINT('Ctrl Pts',(-1.84307845300005,11.6,10.444836052));
#232016=CARTESIAN_POINT('Ctrl Pts',(-1.84390761700006,15.2,10.446791469));
#232017=CARTESIAN_POINT('Ctrl Pts',(-1.84390761700006,11.6,10.446791469));
#232018=CARTESIAN_POINT('Ctrl Pts',(-1.84474118900006,15.2,10.44875241));
#232019=CARTESIAN_POINT('Ctrl Pts',(-1.84474118900006,11.6,10.44875241));
#232020=CARTESIAN_POINT('Ctrl Pts',(-1.84557917400005,15.2,10.45071886));
#232021=CARTESIAN_POINT('Ctrl Pts',(-1.84557917400005,11.6,10.45071886));
#232022=CARTESIAN_POINT('Ctrl Pts',(-1.84642157300006,15.2,10.4526908));
#232023=CARTESIAN_POINT('Ctrl Pts',(-1.84642157300006,11.6,10.4526908));
#232024=CARTESIAN_POINT('Ctrl Pts',(-1.84726839200006,15.2,10.454668215));
#232025=CARTESIAN_POINT('Ctrl Pts',(-1.84726839200006,11.6,10.454668215));
#232026=CARTESIAN_POINT('Ctrl Pts',(-1.84811963700006,15.2,10.456651086));
#232027=CARTESIAN_POINT('Ctrl Pts',(-1.84811963700006,11.6,10.456651086));
#232028=CARTESIAN_POINT('Ctrl Pts',(-1.84897531000005,15.2,10.458639395));
#232029=CARTESIAN_POINT('Ctrl Pts',(-1.84897531000005,11.6,10.458639395));
#232030=CARTESIAN_POINT('Ctrl Pts',(-1.84983541700006,15.2,10.460633126));
#232031=CARTESIAN_POINT('Ctrl Pts',(-1.84983541700006,11.6,10.460633126));
#232032=CARTESIAN_POINT('Ctrl Pts',(-1.85069996000006,15.2,10.462632262));
#232033=CARTESIAN_POINT('Ctrl Pts',(-1.85069996000006,11.6,10.462632262));
#232034=CARTESIAN_POINT('Ctrl Pts',(-1.85156894600006,15.2,10.464636786));
#232035=CARTESIAN_POINT('Ctrl Pts',(-1.85156894600006,11.6,10.464636786));
#232036=CARTESIAN_POINT('Ctrl Pts',(-1.85244237800006,15.2,10.46664668));
#232037=CARTESIAN_POINT('Ctrl Pts',(-1.85244237800006,11.6,10.46664668));
#232038=CARTESIAN_POINT('Ctrl Pts',(-1.85332026000005,15.2,10.468661929));
#232039=CARTESIAN_POINT('Ctrl Pts',(-1.85332026000005,11.6,10.468661929));
#232040=CARTESIAN_POINT('Ctrl Pts',(-1.85420259600006,15.2,10.470682514));
#232041=CARTESIAN_POINT('Ctrl Pts',(-1.85420259600006,11.6,10.470682514));
#232042=CARTESIAN_POINT('Ctrl Pts',(-1.85508939000006,15.2,10.472708419));
#232043=CARTESIAN_POINT('Ctrl Pts',(-1.85508939000006,11.6,10.472708419));
#232044=CARTESIAN_POINT('Ctrl Pts',(-1.85598064800006,15.2,10.474739628));
#232045=CARTESIAN_POINT('Ctrl Pts',(-1.85598064800006,11.6,10.474739628));
#232046=CARTESIAN_POINT('Ctrl Pts',(-1.85687637100005,15.2,10.476776124));
#232047=CARTESIAN_POINT('Ctrl Pts',(-1.85687637100005,11.6,10.476776124));
#232048=CARTESIAN_POINT('Ctrl Pts',(-1.85777656600006,15.2,10.478817888));
#232049=CARTESIAN_POINT('Ctrl Pts',(-1.85777656600006,11.6,10.478817888));
#232050=CARTESIAN_POINT('Ctrl Pts',(-1.85868123400006,15.2,10.480864906));
#232051=CARTESIAN_POINT('Ctrl Pts',(-1.85868123400006,11.6,10.480864906));
#232052=CARTESIAN_POINT('Ctrl Pts',(-1.85959038200005,15.2,10.48291716));
#232053=CARTESIAN_POINT('Ctrl Pts',(-1.85959038200005,11.6,10.48291716));
#232054=CARTESIAN_POINT('Ctrl Pts',(-1.86050401200006,15.2,10.484974635));
#232055=CARTESIAN_POINT('Ctrl Pts',(-1.86050401200006,11.6,10.484974635));
#232056=CARTESIAN_POINT('Ctrl Pts',(-1.86142213000006,15.2,10.487037313));
#232057=CARTESIAN_POINT('Ctrl Pts',(-1.86142213000006,11.6,10.487037313));
#232058=CARTESIAN_POINT('Ctrl Pts',(-1.86234473700006,15.2,10.489105177));
#232059=CARTESIAN_POINT('Ctrl Pts',(-1.86234473700006,11.6,10.489105177));
#232060=CARTESIAN_POINT('Ctrl Pts',(-1.86327183900006,15.2,10.491178213));
#232061=CARTESIAN_POINT('Ctrl Pts',(-1.86327183900006,11.6,10.491178213));
#232062=CARTESIAN_POINT('Ctrl Pts',(-1.86420344100006,15.2,10.493256403));
#232063=CARTESIAN_POINT('Ctrl Pts',(-1.86420344100006,11.6,10.493256403));
#232064=CARTESIAN_POINT('Ctrl Pts',(-1.86513954500006,15.2,10.49533973));
#232065=CARTESIAN_POINT('Ctrl Pts',(-1.86513954500006,11.6,10.49533973));
#232066=CARTESIAN_POINT('Ctrl Pts',(-1.86608015400005,15.2,10.497428179));
#232067=CARTESIAN_POINT('Ctrl Pts',(-1.86608015400005,11.6,10.497428179));
#232068=CARTESIAN_POINT('Ctrl Pts',(-1.86702527300006,15.2,10.499521734));
#232069=CARTESIAN_POINT('Ctrl Pts',(-1.86702527300006,11.6,10.499521734));
#232070=CARTESIAN_POINT('Ctrl Pts',(-1.86797490700006,15.2,10.501620378));
#232071=CARTESIAN_POINT('Ctrl Pts',(-1.86797490700006,11.6,10.501620378));
#232072=CARTESIAN_POINT('Ctrl Pts',(-1.86892905800006,15.2,10.503724094));
#232073=CARTESIAN_POINT('Ctrl Pts',(-1.86892905800006,11.6,10.503724094));
#232074=CARTESIAN_POINT('Ctrl Pts',(-1.86988773000006,15.2,10.505832868));
#232075=CARTESIAN_POINT('Ctrl Pts',(-1.86988773000006,11.6,10.505832868));
#232076=CARTESIAN_POINT('Ctrl Pts',(-1.87085092800006,15.2,10.507946682));
#232077=CARTESIAN_POINT('Ctrl Pts',(-1.87085092800006,11.6,10.507946682));
#232078=CARTESIAN_POINT('Ctrl Pts',(-1.87181865400006,15.2,10.510065522));
#232079=CARTESIAN_POINT('Ctrl Pts',(-1.87181865400006,11.6,10.510065522));
#232080=CARTESIAN_POINT('Ctrl Pts',(-1.87279091300006,15.2,10.512189371));
#232081=CARTESIAN_POINT('Ctrl Pts',(-1.87279091300006,11.6,10.512189371));
#232082=CARTESIAN_POINT('Ctrl Pts',(-1.87376770900005,15.2,10.514318212));
#232083=CARTESIAN_POINT('Ctrl Pts',(-1.87376770900005,11.6,10.514318212));
#232084=CARTESIAN_POINT('Ctrl Pts',(-1.87474904500006,15.2,10.516452031));
#232085=CARTESIAN_POINT('Ctrl Pts',(-1.87474904500006,11.6,10.516452031));
#232086=CARTESIAN_POINT('Ctrl Pts',(-1.87573492300006,15.2,10.518590811));
#232087=CARTESIAN_POINT('Ctrl Pts',(-1.87573492300006,11.6,10.518590811));
#232088=CARTESIAN_POINT('Ctrl Pts',(-1.87672535000006,15.2,10.520734537));
#232089=CARTESIAN_POINT('Ctrl Pts',(-1.87672535000006,11.6,10.520734537));
#232090=CARTESIAN_POINT('Ctrl Pts',(-1.87772032700006,15.2,10.522883192));
#232091=CARTESIAN_POINT('Ctrl Pts',(-1.87772032700006,11.6,10.522883192));
#232092=CARTESIAN_POINT('Ctrl Pts',(-1.87871985800005,15.2,10.525036762));
#232093=CARTESIAN_POINT('Ctrl Pts',(-1.87871985800005,11.6,10.525036762));
#232094=CARTESIAN_POINT('Ctrl Pts',(-1.87972394600005,15.2,10.52719523));
#232095=CARTESIAN_POINT('Ctrl Pts',(-1.87972394600005,11.6,10.52719523));
#232096=CARTESIAN_POINT('Ctrl Pts',(-1.88073259700006,15.2,10.529358581));
#232097=CARTESIAN_POINT('Ctrl Pts',(-1.88073259700006,11.6,10.529358581));
#232098=CARTESIAN_POINT('Ctrl Pts',(-1.88174581300005,15.2,10.531526799));
#232099=CARTESIAN_POINT('Ctrl Pts',(-1.88174581300005,11.6,10.531526799));
#232100=CARTESIAN_POINT('Ctrl Pts',(-1.88276359700006,15.2,10.533699869));
#232101=CARTESIAN_POINT('Ctrl Pts',(-1.88276359700006,11.6,10.533699869));
#232102=CARTESIAN_POINT('Ctrl Pts',(-1.88378595300006,15.2,10.535877775));
#232103=CARTESIAN_POINT('Ctrl Pts',(-1.88378595300006,11.6,10.535877775));
#232104=CARTESIAN_POINT('Ctrl Pts',(-1.88481288500005,15.2,10.538060502));
#232105=CARTESIAN_POINT('Ctrl Pts',(-1.88481288500005,11.6,10.538060502));
#232106=CARTESIAN_POINT('Ctrl Pts',(-1.88584439500006,15.2,10.540248036));
#232107=CARTESIAN_POINT('Ctrl Pts',(-1.88584439500006,11.6,10.540248036));
#232108=CARTESIAN_POINT('Ctrl Pts',(-1.88688048700006,15.2,10.542440358));
#232109=CARTESIAN_POINT('Ctrl Pts',(-1.88688048700006,11.6,10.542440358));
#232110=CARTESIAN_POINT('Ctrl Pts',(-1.88792116500006,15.2,10.544637456));
#232111=CARTESIAN_POINT('Ctrl Pts',(-1.88792116500006,11.6,10.544637456));
#232112=CARTESIAN_POINT('Ctrl Pts',(-1.88896643100006,15.2,10.546839313));
#232113=CARTESIAN_POINT('Ctrl Pts',(-1.88896643100006,11.6,10.546839313));
#232114=CARTESIAN_POINT('Ctrl Pts',(-1.89001629100006,15.2,10.549045914));
#232115=CARTESIAN_POINT('Ctrl Pts',(-1.89001629100006,11.6,10.549045914));
#232116=CARTESIAN_POINT('Ctrl Pts',(-1.89107074600006,15.2,10.551257245));
#232117=CARTESIAN_POINT('Ctrl Pts',(-1.89107074600006,11.6,10.551257245));
#232118=CARTESIAN_POINT('Ctrl Pts',(-1.89212979900006,15.2,10.553473289));
#232119=CARTESIAN_POINT('Ctrl Pts',(-1.89212979900006,11.6,10.553473289));
#232120=CARTESIAN_POINT('Ctrl Pts',(-1.89319345500006,15.2,10.555694031));
#232121=CARTESIAN_POINT('Ctrl Pts',(-1.89319345500006,11.6,10.555694031));
#232122=CARTESIAN_POINT('Ctrl Pts',(-1.89426171700006,15.2,10.557919459));
#232123=CARTESIAN_POINT('Ctrl Pts',(-1.89426171700006,11.6,10.557919459));
#232124=CARTESIAN_POINT('Ctrl Pts',(-1.89533458700006,15.2,10.560149554));
#232125=CARTESIAN_POINT('Ctrl Pts',(-1.89533458700006,11.6,10.560149554));
#232126=CARTESIAN_POINT('Ctrl Pts',(-1.89641206900005,15.2,10.562384303));
#232127=CARTESIAN_POINT('Ctrl Pts',(-1.89641206900005,11.6,10.562384303));
#232128=CARTESIAN_POINT('Ctrl Pts',(-1.89749416700006,15.2,10.564623692));
#232129=CARTESIAN_POINT('Ctrl Pts',(-1.89749416700006,11.6,10.564623692));
#232130=CARTESIAN_POINT('Ctrl Pts',(-1.89858088300006,15.2,10.566867704));
#232131=CARTESIAN_POINT('Ctrl Pts',(-1.89858088300006,11.6,10.566867704));
#232132=CARTESIAN_POINT('Ctrl Pts',(-1.89967222000006,15.2,10.569116324));
#232133=CARTESIAN_POINT('Ctrl Pts',(-1.89967222000006,11.6,10.569116324));
#232134=CARTESIAN_POINT('Ctrl Pts',(-1.90076818200006,15.2,10.571369539));
#232135=CARTESIAN_POINT('Ctrl Pts',(-1.90076818200006,11.6,10.571369539));
#232136=CARTESIAN_POINT('Ctrl Pts',(-1.90186877100006,15.2,10.573627333));
#232137=CARTESIAN_POINT('Ctrl Pts',(-1.90186877100006,11.6,10.573627333));
#232138=CARTESIAN_POINT('Ctrl Pts',(-1.90297399300006,15.2,10.575889692));
#232139=CARTESIAN_POINT('Ctrl Pts',(-1.90297399300006,11.6,10.575889692));
#232140=CARTESIAN_POINT('Ctrl Pts',(-1.90408384600006,15.2,10.578156601));
#232141=CARTESIAN_POINT('Ctrl Pts',(-1.90408384600006,11.6,10.578156601));
#232142=CARTESIAN_POINT('Ctrl Pts',(-1.90519833900006,15.2,10.580428045));
#232143=CARTESIAN_POINT('Ctrl Pts',(-1.90519833900006,11.6,10.580428045));
#232144=CARTESIAN_POINT('Ctrl Pts',(-1.90631747000006,15.2,10.582704009));
#232145=CARTESIAN_POINT('Ctrl Pts',(-1.90631747000006,11.6,10.582704009));
#232146=CARTESIAN_POINT('Ctrl Pts',(-1.90744124500006,15.2,10.584984479));
#232147=CARTESIAN_POINT('Ctrl Pts',(-1.90744124500006,11.6,10.584984479));
#232148=CARTESIAN_POINT('Ctrl Pts',(-1.90856966700006,15.2,10.587269441));
#232149=CARTESIAN_POINT('Ctrl Pts',(-1.90856966700006,11.6,10.587269441));
#232150=CARTESIAN_POINT('Ctrl Pts',(-1.90970273800006,15.2,10.589558879));
#232151=CARTESIAN_POINT('Ctrl Pts',(-1.90970273800006,11.6,10.589558879));
#232152=CARTESIAN_POINT('Ctrl Pts',(-1.91084046000006,15.2,10.591852781));
#232153=CARTESIAN_POINT('Ctrl Pts',(-1.91084046000006,11.6,10.591852781));
#232154=CARTESIAN_POINT('Ctrl Pts',(-1.91198283900006,15.2,10.594151129));
#232155=CARTESIAN_POINT('Ctrl Pts',(-1.91198283900006,11.6,10.594151129));
#232156=CARTESIAN_POINT('Ctrl Pts',(-1.91312987400006,15.2,10.596453911));
#232157=CARTESIAN_POINT('Ctrl Pts',(-1.91312987400006,11.6,10.596453911));
#232158=CARTESIAN_POINT('Ctrl Pts',(-1.91428157100006,15.2,10.598761112));
#232159=CARTESIAN_POINT('Ctrl Pts',(-1.91428157100006,11.6,10.598761112));
#232160=CARTESIAN_POINT('Ctrl Pts',(-1.91543793200006,15.2,10.601072718));
#232161=CARTESIAN_POINT('Ctrl Pts',(-1.91543793200006,11.6,10.601072718));
#232162=CARTESIAN_POINT('Ctrl Pts',(-1.91659896000006,15.2,10.603388714));
#232163=CARTESIAN_POINT('Ctrl Pts',(-1.91659896000006,11.6,10.603388714));
#232164=CARTESIAN_POINT('Ctrl Pts',(-1.91776465700006,15.2,10.605709086));
#232165=CARTESIAN_POINT('Ctrl Pts',(-1.91776465700006,11.6,10.605709086));
#232166=CARTESIAN_POINT('Ctrl Pts',(-1.91893502800006,15.2,10.608033819));
#232167=CARTESIAN_POINT('Ctrl Pts',(-1.91893502800006,11.6,10.608033819));
#232168=CARTESIAN_POINT('Ctrl Pts',(-1.92011007300006,15.2,10.610362901));
#232169=CARTESIAN_POINT('Ctrl Pts',(-1.92011007300006,11.6,10.610362901));
#232170=CARTESIAN_POINT('Ctrl Pts',(-1.92128979700006,15.2,10.612696316));
#232171=CARTESIAN_POINT('Ctrl Pts',(-1.92128979700006,11.6,10.612696316));
#232172=CARTESIAN_POINT('Ctrl Pts',(-1.92247420100006,15.2,10.615034051));
#232173=CARTESIAN_POINT('Ctrl Pts',(-1.92247420100006,11.6,10.615034051));
#232174=CARTESIAN_POINT('Ctrl Pts',(-1.92366329000006,15.2,10.617376091));
#232175=CARTESIAN_POINT('Ctrl Pts',(-1.92366329000006,11.6,10.617376091));
#232176=CARTESIAN_POINT('Ctrl Pts',(-1.92485706500006,15.2,10.619722422));
#232177=CARTESIAN_POINT('Ctrl Pts',(-1.92485706500006,11.6,10.619722422));
#232178=CARTESIAN_POINT('Ctrl Pts',(-1.92605552900006,15.2,10.62207303));
#232179=CARTESIAN_POINT('Ctrl Pts',(-1.92605552900006,11.6,10.62207303));
#232180=CARTESIAN_POINT('Ctrl Pts',(-1.92725868600006,15.2,10.624427901));
#232181=CARTESIAN_POINT('Ctrl Pts',(-1.92725868600006,11.6,10.624427901));
#232182=CARTESIAN_POINT('Ctrl Pts',(-1.92846653700005,15.2,10.626787021));
#232183=CARTESIAN_POINT('Ctrl Pts',(-1.92846653700005,11.6,10.626787021));
#232184=CARTESIAN_POINT('Ctrl Pts',(-1.92967908600005,15.2,10.629150376));
#232185=CARTESIAN_POINT('Ctrl Pts',(-1.92967908600005,11.6,10.629150376));
#232186=CARTESIAN_POINT('Ctrl Pts',(-1.93089633400006,15.2,10.631517953));
#232187=CARTESIAN_POINT('Ctrl Pts',(-1.93089633400006,11.6,10.631517953));
#232188=CARTESIAN_POINT('Ctrl Pts',(-1.93211828500006,15.2,10.633889738));
#232189=CARTESIAN_POINT('Ctrl Pts',(-1.93211828500006,11.6,10.633889738));
#232190=CARTESIAN_POINT('Ctrl Pts',(-1.93334494300006,15.2,10.636265716));
#232191=CARTESIAN_POINT('Ctrl Pts',(-1.93334494300006,11.6,10.636265716));
#232192=CARTESIAN_POINT('Ctrl Pts',(-1.93457630800005,15.2,10.638645874));
#232193=CARTESIAN_POINT('Ctrl Pts',(-1.93457630800005,11.6,10.638645874));
#232194=CARTESIAN_POINT('Ctrl Pts',(-1.93581238400005,15.2,10.641030198));
#232195=CARTESIAN_POINT('Ctrl Pts',(-1.93581238400005,11.6,10.641030198));
#232196=CARTESIAN_POINT('Ctrl Pts',(-1.93705317300006,15.2,10.643418674));
#232197=CARTESIAN_POINT('Ctrl Pts',(-1.93705317300006,11.6,10.643418674));
#232198=CARTESIAN_POINT('Ctrl Pts',(-1.93829867700006,15.2,10.645811289));
#232199=CARTESIAN_POINT('Ctrl Pts',(-1.93829867700006,11.6,10.645811289));
#232200=CARTESIAN_POINT('Ctrl Pts',(-1.93954890100006,15.2,10.648208029));
#232201=CARTESIAN_POINT('Ctrl Pts',(-1.93954890100006,11.6,10.648208029));
#232202=CARTESIAN_POINT('Ctrl Pts',(-1.94080384500006,15.2,10.650608881));
#232203=CARTESIAN_POINT('Ctrl Pts',(-1.94080384500006,11.6,10.650608881));
#232204=CARTESIAN_POINT('Ctrl Pts',(-1.94206351300006,15.2,10.65301383));
#232205=CARTESIAN_POINT('Ctrl Pts',(-1.94206351300006,11.6,10.65301383));
#232206=CARTESIAN_POINT('Ctrl Pts',(-1.94332790700006,15.2,10.655422863));
#232207=CARTESIAN_POINT('Ctrl Pts',(-1.94332790700006,11.6,10.655422863));
#232208=CARTESIAN_POINT('Ctrl Pts',(-1.94459703000006,15.2,10.657835968));
#232209=CARTESIAN_POINT('Ctrl Pts',(-1.94459703000006,11.6,10.657835968));
#232210=CARTESIAN_POINT('Ctrl Pts',(-1.94587088300006,15.2,10.66025313));
#232211=CARTESIAN_POINT('Ctrl Pts',(-1.94587088300006,11.6,10.66025313));
#232212=CARTESIAN_POINT('Ctrl Pts',(-1.94714947000006,15.2,10.662674335));
#232213=CARTESIAN_POINT('Ctrl Pts',(-1.94714947000006,11.6,10.662674335));
#232214=CARTESIAN_POINT('Ctrl Pts',(-1.94843279200006,15.2,10.665099571));
#232215=CARTESIAN_POINT('Ctrl Pts',(-1.94843279200006,11.6,10.665099571));
#232216=CARTESIAN_POINT('Ctrl Pts',(-1.94972085400006,15.2,10.667528824));
#232217=CARTESIAN_POINT('Ctrl Pts',(-1.94972085400006,11.6,10.667528824));
#232218=CARTESIAN_POINT('Ctrl Pts',(-1.95101365600005,15.2,10.669962079));
#232219=CARTESIAN_POINT('Ctrl Pts',(-1.95101365600005,11.6,10.669962079));
#232220=CARTESIAN_POINT('Ctrl Pts',(-1.95231120100006,15.2,10.672399326));
#232221=CARTESIAN_POINT('Ctrl Pts',(-1.95231120100006,11.6,10.672399326));
#232222=CARTESIAN_POINT('Ctrl Pts',(-1.95361349100006,15.2,10.674840549));
#232223=CARTESIAN_POINT('Ctrl Pts',(-1.95361349100006,11.6,10.674840549));
#232224=CARTESIAN_POINT('Ctrl Pts',(-1.95492053000006,15.2,10.677285737));
#232225=CARTESIAN_POINT('Ctrl Pts',(-1.95492053000006,11.6,10.677285737));
#232226=CARTESIAN_POINT('Ctrl Pts',(-1.95623231900006,15.2,10.679734874));
#232227=CARTESIAN_POINT('Ctrl Pts',(-1.95623231900006,11.6,10.679734874));
#232228=CARTESIAN_POINT('Ctrl Pts',(-1.95754886100006,15.2,10.682187949));
#232229=CARTESIAN_POINT('Ctrl Pts',(-1.95754886100006,11.6,10.682187949));
#232230=CARTESIAN_POINT('Ctrl Pts',(-1.95887015700006,15.2,10.684644947));
#232231=CARTESIAN_POINT('Ctrl Pts',(-1.95887015700006,11.6,10.684644947));
#232232=CARTESIAN_POINT('Ctrl Pts',(-1.96019621100006,15.2,10.687105857));
#232233=CARTESIAN_POINT('Ctrl Pts',(-1.96019621100006,11.6,10.687105857));
#232234=CARTESIAN_POINT('Ctrl Pts',(-1.96152702400005,15.2,10.689570664));
#232235=CARTESIAN_POINT('Ctrl Pts',(-1.96152702400005,11.6,10.689570664));
#232236=CARTESIAN_POINT('Ctrl Pts',(-1.96286259900006,15.2,10.692039356));
#232237=CARTESIAN_POINT('Ctrl Pts',(-1.96286259900006,11.6,10.692039356));
#232238=CARTESIAN_POINT('Ctrl Pts',(-1.96420293800006,15.2,10.69451192));
#232239=CARTESIAN_POINT('Ctrl Pts',(-1.96420293800006,11.6,10.69451192));
#232240=CARTESIAN_POINT('Ctrl Pts',(-1.96554804400006,15.2,10.696988341));
#232241=CARTESIAN_POINT('Ctrl Pts',(-1.96554804400006,11.6,10.696988341));
#232242=CARTESIAN_POINT('Ctrl Pts',(-1.96689791800006,15.2,10.699468609));
#232243=CARTESIAN_POINT('Ctrl Pts',(-1.96689791800006,11.6,10.699468609));
#232244=CARTESIAN_POINT('Ctrl Pts',(-1.96825256200006,15.2,10.701952709));
#232245=CARTESIAN_POINT('Ctrl Pts',(-1.96825256200006,11.6,10.701952709));
#232246=CARTESIAN_POINT('Ctrl Pts',(-1.96961198100006,15.2,10.704440629));
#232247=CARTESIAN_POINT('Ctrl Pts',(-1.96961198100006,11.6,10.704440629));
#232248=CARTESIAN_POINT('Ctrl Pts',(-1.97097617400006,15.2,10.706932356));
#232249=CARTESIAN_POINT('Ctrl Pts',(-1.97097617400006,11.6,10.706932356));
#232250=CARTESIAN_POINT('Ctrl Pts',(-1.97234514400006,15.2,10.709427877));
#232251=CARTESIAN_POINT('Ctrl Pts',(-1.97234514400006,11.6,10.709427877));
#232252=CARTESIAN_POINT('Ctrl Pts',(-1.97371889400005,15.2,10.711927178));
#232253=CARTESIAN_POINT('Ctrl Pts',(-1.97371889400005,11.6,10.711927178));
#232254=CARTESIAN_POINT('Ctrl Pts',(-1.97509742500006,15.2,10.714430247));
#232255=CARTESIAN_POINT('Ctrl Pts',(-1.97509742500006,11.6,10.714430247));
#232256=CARTESIAN_POINT('Ctrl Pts',(-1.97648074000006,15.2,10.716937072));
#232257=CARTESIAN_POINT('Ctrl Pts',(-1.97648074000006,11.6,10.716937072));
#232258=CARTESIAN_POINT('Ctrl Pts',(-1.97786884200006,15.2,10.719447641));
#232259=CARTESIAN_POINT('Ctrl Pts',(-1.97786884200006,11.6,10.719447641));
#232260=CARTESIAN_POINT('Ctrl Pts',(-1.97926173100006,15.2,10.721961938));
#232261=CARTESIAN_POINT('Ctrl Pts',(-1.97926173100006,11.6,10.721961938));
#232262=CARTESIAN_POINT('Ctrl Pts',(-1.98065941000006,15.2,10.724479953));
#232263=CARTESIAN_POINT('Ctrl Pts',(-1.98065941000006,11.6,10.724479953));
#232264=CARTESIAN_POINT('Ctrl Pts',(-1.98206188100006,15.2,10.727001672));
#232265=CARTESIAN_POINT('Ctrl Pts',(-1.98206188100006,11.6,10.727001672));
#232266=CARTESIAN_POINT('Ctrl Pts',(-1.98346914700006,15.2,10.729527083));
#232267=CARTESIAN_POINT('Ctrl Pts',(-1.98346914700006,11.6,10.729527083));
#232268=CARTESIAN_POINT('Ctrl Pts',(-1.98488120800006,15.2,10.732056173));
#232269=CARTESIAN_POINT('Ctrl Pts',(-1.98488120800006,11.6,10.732056173));
#232270=CARTESIAN_POINT('Ctrl Pts',(-1.98629806800006,15.2,10.73458893));
#232271=CARTESIAN_POINT('Ctrl Pts',(-1.98629806800006,11.6,10.73458893));
#232272=CARTESIAN_POINT('Ctrl Pts',(-1.98771972900006,15.2,10.737125342));
#232273=CARTESIAN_POINT('Ctrl Pts',(-1.98771972900006,11.6,10.737125342));
#232274=CARTESIAN_POINT('Ctrl Pts',(-1.98914619100006,15.2,10.739665394));
#232275=CARTESIAN_POINT('Ctrl Pts',(-1.98914619100006,11.6,10.739665394));
#232276=CARTESIAN_POINT('Ctrl Pts',(-1.99057745700005,15.2,10.742209076));
#232277=CARTESIAN_POINT('Ctrl Pts',(-1.99057745700005,11.6,10.742209076));
#232278=CARTESIAN_POINT('Ctrl Pts',(-1.99201353000006,15.2,10.744756373));
#232279=CARTESIAN_POINT('Ctrl Pts',(-1.99201353000006,11.6,10.744756373));
#232280=CARTESIAN_POINT('Ctrl Pts',(-1.99345441100006,15.2,10.747307276));
#232281=CARTESIAN_POINT('Ctrl Pts',(-1.99345441100006,11.6,10.747307276));
#232282=CARTESIAN_POINT('Ctrl Pts',(-1.99490010200006,15.2,10.74986177));
#232283=CARTESIAN_POINT('Ctrl Pts',(-1.99490010200006,11.6,10.74986177));
#232284=CARTESIAN_POINT('Ctrl Pts',(-1.99635060500006,15.2,10.752419843));
#232285=CARTESIAN_POINT('Ctrl Pts',(-1.99635060500006,11.6,10.752419843));
#232286=CARTESIAN_POINT('Ctrl Pts',(-1.99780592300006,15.2,10.754981483));
#232287=CARTESIAN_POINT('Ctrl Pts',(-1.99780592300006,11.6,10.754981483));
#232288=CARTESIAN_POINT('Ctrl Pts',(-1.99926605600006,15.2,10.757546678));
#232289=CARTESIAN_POINT('Ctrl Pts',(-1.99926605600006,11.6,10.757546678));
#232290=CARTESIAN_POINT('Ctrl Pts',(-2.00073100600005,15.2,10.760115415));
#232291=CARTESIAN_POINT('Ctrl Pts',(-2.00073100600005,11.6,10.760115415));
#232292=CARTESIAN_POINT('Ctrl Pts',(-2.00220077600005,15.2,10.762687682));
#232293=CARTESIAN_POINT('Ctrl Pts',(-2.00220077600005,11.6,10.762687682));
#232294=CARTESIAN_POINT('Ctrl Pts',(-2.00367536800006,15.2,10.765263466));
#232295=CARTESIAN_POINT('Ctrl Pts',(-2.00367536800006,11.6,10.765263466));
#232296=CARTESIAN_POINT('Ctrl Pts',(-2.00515478300006,15.2,10.767842757));
#232297=CARTESIAN_POINT('Ctrl Pts',(-2.00515478300006,11.6,10.767842757));
#232298=CARTESIAN_POINT('Ctrl Pts',(-2.00663902300006,15.2,10.770425539));
#232299=CARTESIAN_POINT('Ctrl Pts',(-2.00663902300006,11.6,10.770425539));
#232300=CARTESIAN_POINT('Ctrl Pts',(-2.00812809100006,15.2,10.773011804));
#232301=CARTESIAN_POINT('Ctrl Pts',(-2.00812809100006,11.6,10.773011804));
#232302=CARTESIAN_POINT('Ctrl Pts',(-2.00962198600006,15.2,10.775601537));
#232303=CARTESIAN_POINT('Ctrl Pts',(-2.00962198600006,11.6,10.775601537));
#232304=CARTESIAN_POINT('Ctrl Pts',(-2.01112071300006,15.2,10.778194727));
#232305=CARTESIAN_POINT('Ctrl Pts',(-2.01112071300006,11.6,10.778194727));
#232306=CARTESIAN_POINT('Ctrl Pts',(-2.01262427200006,15.2,10.780791361));
#232307=CARTESIAN_POINT('Ctrl Pts',(-2.01262427200006,11.6,10.780791361));
#232308=CARTESIAN_POINT('Ctrl Pts',(-2.01413266500006,15.2,10.783391429));
#232309=CARTESIAN_POINT('Ctrl Pts',(-2.01413266500006,11.6,10.783391429));
#232310=CARTESIAN_POINT('Ctrl Pts',(-2.01564589300005,15.2,10.785994916));
#232311=CARTESIAN_POINT('Ctrl Pts',(-2.01564589300005,11.6,10.785994916));
#232312=CARTESIAN_POINT('Ctrl Pts',(-2.01716396000006,15.2,10.788601812));
#232313=CARTESIAN_POINT('Ctrl Pts',(-2.01716396000006,11.6,10.788601812));
#232314=CARTESIAN_POINT('Ctrl Pts',(-2.01868686500006,15.2,10.791212105));
#232315=CARTESIAN_POINT('Ctrl Pts',(-2.01868686500006,11.6,10.791212105));
#232316=CARTESIAN_POINT('Ctrl Pts',(-2.02021461200005,15.2,10.793825782));
#232317=CARTESIAN_POINT('Ctrl Pts',(-2.02021461200005,11.6,10.793825782));
#232318=CARTESIAN_POINT('Ctrl Pts',(-2.02174720100006,15.2,10.796442831));
#232319=CARTESIAN_POINT('Ctrl Pts',(-2.02174720100006,11.6,10.796442831));
#232320=CARTESIAN_POINT('Ctrl Pts',(-2.02328463500006,15.2,10.799063242));
#232321=CARTESIAN_POINT('Ctrl Pts',(-2.02328463500006,11.6,10.799063242));
#232322=CARTESIAN_POINT('Ctrl Pts',(-2.02482691500005,15.2,10.801687001));
#232323=CARTESIAN_POINT('Ctrl Pts',(-2.02482691500005,11.6,10.801687001));
#232324=CARTESIAN_POINT('Ctrl Pts',(-2.02637404300006,15.2,10.804314096));
#232325=CARTESIAN_POINT('Ctrl Pts',(-2.02637404300006,11.6,10.804314096));
#232326=CARTESIAN_POINT('Ctrl Pts',(-2.02792601900006,15.2,10.806944517));
#232327=CARTESIAN_POINT('Ctrl Pts',(-2.02792601900006,11.6,10.806944517));
#232328=CARTESIAN_POINT('Ctrl Pts',(-2.02948284700006,15.2,10.809578251));
#232329=CARTESIAN_POINT('Ctrl Pts',(-2.02948284700006,11.6,10.809578251));
#232330=CARTESIAN_POINT('Ctrl Pts',(-2.03104452800006,15.2,10.812215286));
#232331=CARTESIAN_POINT('Ctrl Pts',(-2.03104452800006,11.6,10.812215286));
#232332=CARTESIAN_POINT('Ctrl Pts',(-2.03261106300006,15.2,10.814855612));
#232333=CARTESIAN_POINT('Ctrl Pts',(-2.03261106300006,11.6,10.814855612));
#232334=CARTESIAN_POINT('Ctrl Pts',(-2.03418245300006,15.2,10.817499214));
#232335=CARTESIAN_POINT('Ctrl Pts',(-2.03418245300006,11.6,10.817499214));
#232336=CARTESIAN_POINT('Ctrl Pts',(-2.03575870100006,15.2,10.820146084));
#232337=CARTESIAN_POINT('Ctrl Pts',(-2.03575870100006,11.6,10.820146084));
#232338=CARTESIAN_POINT('Ctrl Pts',(-2.03733980800005,15.2,10.822796206));
#232339=CARTESIAN_POINT('Ctrl Pts',(-2.03733980800005,11.6,10.822796206));
#232340=CARTESIAN_POINT('Ctrl Pts',(-2.03892577600006,15.2,10.825449573));
#232341=CARTESIAN_POINT('Ctrl Pts',(-2.03892577600006,11.6,10.825449573));
#232342=CARTESIAN_POINT('Ctrl Pts',(-2.04051660600005,15.2,10.828106169));
#232343=CARTESIAN_POINT('Ctrl Pts',(-2.04051660600005,11.6,10.828106169));
#232344=CARTESIAN_POINT('Ctrl Pts',(-2.04211229900006,15.2,10.830765987));
#232345=CARTESIAN_POINT('Ctrl Pts',(-2.04211229900006,11.6,10.830765987));
#232346=CARTESIAN_POINT('Ctrl Pts',(-2.04371285800006,15.2,10.83342901));
#232347=CARTESIAN_POINT('Ctrl Pts',(-2.04371285800006,11.6,10.83342901));
#232348=CARTESIAN_POINT('Ctrl Pts',(-2.04531828300006,15.2,10.836095231));
#232349=CARTESIAN_POINT('Ctrl Pts',(-2.04531828300006,11.6,10.836095231));
#232350=CARTESIAN_POINT('Ctrl Pts',(-2.04692857600006,15.2,10.838764637));
#232351=CARTESIAN_POINT('Ctrl Pts',(-2.04692857600006,11.6,10.838764637));
#232352=CARTESIAN_POINT('Ctrl Pts',(-2.04854373900006,15.2,10.841437215));
#232353=CARTESIAN_POINT('Ctrl Pts',(-2.04854373900006,11.6,10.841437215));
#232354=CARTESIAN_POINT('Ctrl Pts',(-2.05016377400006,15.2,10.844112956));
#232355=CARTESIAN_POINT('Ctrl Pts',(-2.05016377400006,11.6,10.844112956));
#232356=CARTESIAN_POINT('Ctrl Pts',(-2.05178868100006,15.2,10.846791846));
#232357=CARTESIAN_POINT('Ctrl Pts',(-2.05178868100006,11.6,10.846791846));
#232358=CARTESIAN_POINT('Ctrl Pts',(-2.05341846200006,15.2,10.849473875));
#232359=CARTESIAN_POINT('Ctrl Pts',(-2.05341846200006,11.6,10.849473875));
#232360=CARTESIAN_POINT('Ctrl Pts',(-2.05505311800006,15.2,10.852159031));
#232361=CARTESIAN_POINT('Ctrl Pts',(-2.05505311800006,11.6,10.852159031));
#232362=CARTESIAN_POINT('Ctrl Pts',(-2.05669265100005,15.2,10.854847304));
#232363=CARTESIAN_POINT('Ctrl Pts',(-2.05669265100005,11.6,10.854847304));
#232364=CARTESIAN_POINT('Ctrl Pts',(-2.05833706300006,15.2,10.857538681));
#232365=CARTESIAN_POINT('Ctrl Pts',(-2.05833706300006,11.6,10.857538681));
#232366=CARTESIAN_POINT('Ctrl Pts',(-2.05998635400006,15.2,10.86023315));
#232367=CARTESIAN_POINT('Ctrl Pts',(-2.05998635400006,11.6,10.86023315));
#232368=CARTESIAN_POINT('Ctrl Pts',(-2.06164052600006,15.2,10.862930701));
#232369=CARTESIAN_POINT('Ctrl Pts',(-2.06164052600006,11.6,10.862930701));
#232370=CARTESIAN_POINT('Ctrl Pts',(-2.06329958100006,15.2,10.865631324));
#232371=CARTESIAN_POINT('Ctrl Pts',(-2.06329958100006,11.6,10.865631324));
#232372=CARTESIAN_POINT('Ctrl Pts',(-2.06496352000006,15.2,10.868335004));
#232373=CARTESIAN_POINT('Ctrl Pts',(-2.06496352000006,11.6,10.868335004));
#232374=CARTESIAN_POINT('Ctrl Pts',(-2.06663234400006,15.2,10.871041733));
#232375=CARTESIAN_POINT('Ctrl Pts',(-2.06663234400006,11.6,10.871041733));
#232376=CARTESIAN_POINT('Ctrl Pts',(-2.06830605500006,15.2,10.873751498));
#232377=CARTESIAN_POINT('Ctrl Pts',(-2.06830605500006,11.6,10.873751498));
#232378=CARTESIAN_POINT('Ctrl Pts',(-2.06998465300006,15.2,10.876464289));
#232379=CARTESIAN_POINT('Ctrl Pts',(-2.06998465300006,11.6,10.876464289));
#232380=CARTESIAN_POINT('Ctrl Pts',(-2.07166814000006,15.2,10.879180095));
#232381=CARTESIAN_POINT('Ctrl Pts',(-2.07166814000006,11.6,10.879180095));
#232382=CARTESIAN_POINT('Ctrl Pts',(-2.07335651800005,15.2,10.881898902));
#232383=CARTESIAN_POINT('Ctrl Pts',(-2.07335651800005,11.6,10.881898902));
#232384=CARTESIAN_POINT('Ctrl Pts',(-2.07504978800006,15.2,10.884620702));
#232385=CARTESIAN_POINT('Ctrl Pts',(-2.07504978800006,11.6,10.884620702));
#232386=CARTESIAN_POINT('Ctrl Pts',(-2.07674795100006,15.2,10.887345482));
#232387=CARTESIAN_POINT('Ctrl Pts',(-2.07674795100006,11.6,10.887345482));
#232388=CARTESIAN_POINT('Ctrl Pts',(-2.07845100800006,15.2,10.890073232));
#232389=CARTESIAN_POINT('Ctrl Pts',(-2.07845100800006,11.6,10.890073232));
#232390=CARTESIAN_POINT('Ctrl Pts',(-2.08015896100005,15.2,10.892803939));
#232391=CARTESIAN_POINT('Ctrl Pts',(-2.08015896100005,11.6,10.892803939));
#232392=CARTESIAN_POINT('Ctrl Pts',(-2.08187181100006,15.2,10.895537595));
#232393=CARTESIAN_POINT('Ctrl Pts',(-2.08187181100006,11.6,10.895537595));
#232394=CARTESIAN_POINT('Ctrl Pts',(-2.08358955800006,15.2,10.898274187));
#232395=CARTESIAN_POINT('Ctrl Pts',(-2.08358955800006,11.6,10.898274187));
#232396=CARTESIAN_POINT('Ctrl Pts',(-2.08531220600006,15.2,10.901013704));
#232397=CARTESIAN_POINT('Ctrl Pts',(-2.08531220600006,11.6,10.901013704));
#232398=CARTESIAN_POINT('Ctrl Pts',(-2.08703975300006,15.2,10.903756135));
#232399=CARTESIAN_POINT('Ctrl Pts',(-2.08703975300006,11.6,10.903756135));
#232400=CARTESIAN_POINT('Ctrl Pts',(-2.08877220300006,15.2,10.906501469));
#232401=CARTESIAN_POINT('Ctrl Pts',(-2.08877220300006,11.6,10.906501469));
#232402=CARTESIAN_POINT('Ctrl Pts',(-2.09050955500006,15.2,10.909249696));
#232403=CARTESIAN_POINT('Ctrl Pts',(-2.09050955500006,11.6,10.909249696));
#232404=CARTESIAN_POINT('Ctrl Pts',(-2.09225181300006,15.2,10.912000804));
#232405=CARTESIAN_POINT('Ctrl Pts',(-2.09225181300006,11.6,10.912000804));
#232406=CARTESIAN_POINT('Ctrl Pts',(-2.09399897400006,15.2,10.914754782));
#232407=CARTESIAN_POINT('Ctrl Pts',(-2.09399897400006,11.6,10.914754782));
#232408=CARTESIAN_POINT('Ctrl Pts',(-2.09575104200006,15.2,10.91751162));
#232409=CARTESIAN_POINT('Ctrl Pts',(-2.09575104200006,11.6,10.91751162));
#232410=CARTESIAN_POINT('Ctrl Pts',(-2.09750801800006,15.2,10.920271306));
#232411=CARTESIAN_POINT('Ctrl Pts',(-2.09750801800006,11.6,10.920271306));
#232412=CARTESIAN_POINT('Ctrl Pts',(-2.09926990300006,15.2,10.923033831));
#232413=CARTESIAN_POINT('Ctrl Pts',(-2.09926990300006,11.6,10.923033831));
#232414=CARTESIAN_POINT('Ctrl Pts',(-2.10103669800006,15.2,10.925799181));
#232415=CARTESIAN_POINT('Ctrl Pts',(-2.10103669800006,11.6,10.925799181));
#232416=CARTESIAN_POINT('Ctrl Pts',(-2.10280840300006,15.2,10.928567349));
#232417=CARTESIAN_POINT('Ctrl Pts',(-2.10280840300006,11.6,10.928567349));
#232418=CARTESIAN_POINT('Ctrl Pts',(-2.10458502100006,15.2,10.931338321));
#232419=CARTESIAN_POINT('Ctrl Pts',(-2.10458502100006,11.6,10.931338321));
#232420=CARTESIAN_POINT('Ctrl Pts',(-2.10636655200005,15.2,10.934112088));
#232421=CARTESIAN_POINT('Ctrl Pts',(-2.10636655200005,11.6,10.934112088));
#232422=CARTESIAN_POINT('Ctrl Pts',(-2.10815299700006,15.2,10.936888639));
#232423=CARTESIAN_POINT('Ctrl Pts',(-2.10815299700006,11.6,10.936888639));
#232424=CARTESIAN_POINT('Ctrl Pts',(-2.10994435800006,15.2,10.939667962));
#232425=CARTESIAN_POINT('Ctrl Pts',(-2.10994435800006,11.6,10.939667962));
#232426=CARTESIAN_POINT('Ctrl Pts',(-2.11174063500006,15.2,10.942450048));
#232427=CARTESIAN_POINT('Ctrl Pts',(-2.11174063500006,11.6,10.942450048));
#232428=CARTESIAN_POINT('Ctrl Pts',(-2.11354183000006,15.2,10.945234886));
#232429=CARTESIAN_POINT('Ctrl Pts',(-2.11354183000006,11.6,10.945234886));
#232430=CARTESIAN_POINT('Ctrl Pts',(-2.11534794300006,15.2,10.948022464));
#232431=CARTESIAN_POINT('Ctrl Pts',(-2.11534794300006,11.6,10.948022464));
#232432=CARTESIAN_POINT('Ctrl Pts',(-2.11715897500006,15.2,10.950812773));
#232433=CARTESIAN_POINT('Ctrl Pts',(-2.11715897500006,11.6,10.950812773));
#232434=CARTESIAN_POINT('Ctrl Pts',(-2.11897492800006,15.2,10.953605801));
#232435=CARTESIAN_POINT('Ctrl Pts',(-2.11897492800006,11.6,10.953605801));
#232436=CARTESIAN_POINT('Ctrl Pts',(-2.12079580400005,15.2,10.956401538));
#232437=CARTESIAN_POINT('Ctrl Pts',(-2.12079580400005,11.6,10.956401538));
#232438=CARTESIAN_POINT('Ctrl Pts',(-2.12262160100006,15.2,10.959199973));
#232439=CARTESIAN_POINT('Ctrl Pts',(-2.12262160100006,11.6,10.959199973));
#232440=CARTESIAN_POINT('Ctrl Pts',(-2.12445232200006,15.2,10.962001097));
#232441=CARTESIAN_POINT('Ctrl Pts',(-2.12445232200006,11.6,10.962001097));
#232442=CARTESIAN_POINT('Ctrl Pts',(-2.12628796700006,15.2,10.964804897));
#232443=CARTESIAN_POINT('Ctrl Pts',(-2.12628796700006,11.6,10.964804897));
#232444=CARTESIAN_POINT('Ctrl Pts',(-2.12812853900005,15.2,10.967611364));
#232445=CARTESIAN_POINT('Ctrl Pts',(-2.12812853900005,11.6,10.967611364));
#232446=CARTESIAN_POINT('Ctrl Pts',(-2.12997403700005,15.2,10.970420488));
#232447=CARTESIAN_POINT('Ctrl Pts',(-2.12997403700005,11.6,10.970420488));
#232448=CARTESIAN_POINT('Ctrl Pts',(-2.13182446200006,15.2,10.973232257));
#232449=CARTESIAN_POINT('Ctrl Pts',(-2.13182446200006,11.6,10.973232257));
#232450=CARTESIAN_POINT('Ctrl Pts',(-2.13367981500005,15.2,10.976046662));
#232451=CARTESIAN_POINT('Ctrl Pts',(-2.13367981500005,11.6,10.976046662));
#232452=CARTESIAN_POINT('Ctrl Pts',(-2.13554009800006,15.2,10.978863691));
#232453=CARTESIAN_POINT('Ctrl Pts',(-2.13554009800006,11.6,10.978863691));
#232454=CARTESIAN_POINT('Ctrl Pts',(-2.13740531100005,15.2,10.981683335));
#232455=CARTESIAN_POINT('Ctrl Pts',(-2.13740531100005,11.6,10.981683335));
#232456=CARTESIAN_POINT('Ctrl Pts',(-2.13927545500006,15.2,10.984505582));
#232457=CARTESIAN_POINT('Ctrl Pts',(-2.13927545500006,11.6,10.984505582));
#232458=CARTESIAN_POINT('Ctrl Pts',(-2.14115053100006,15.2,10.987330423));
#232459=CARTESIAN_POINT('Ctrl Pts',(-2.14115053100006,11.6,10.987330423));
#232460=CARTESIAN_POINT('Ctrl Pts',(-2.14303054100006,15.2,10.990157848));
#232461=CARTESIAN_POINT('Ctrl Pts',(-2.14303054100006,11.6,10.990157848));
#232462=CARTESIAN_POINT('Ctrl Pts',(-2.14491548400006,15.2,10.992987845));
#232463=CARTESIAN_POINT('Ctrl Pts',(-2.14491548400006,11.6,10.992987845));
#232464=CARTESIAN_POINT('Ctrl Pts',(-2.14680536100006,15.2,10.995820404));
#232465=CARTESIAN_POINT('Ctrl Pts',(-2.14680536100006,11.6,10.995820404));
#232466=CARTESIAN_POINT('Ctrl Pts',(-2.14870017400006,15.2,10.998655516));
#232467=CARTESIAN_POINT('Ctrl Pts',(-2.14870017400006,11.6,10.998655516));
#232468=CARTESIAN_POINT('Ctrl Pts',(-2.15059992400006,15.2,11.00149317));
#232469=CARTESIAN_POINT('Ctrl Pts',(-2.15059992400006,11.6,11.00149317));
#232470=CARTESIAN_POINT('Ctrl Pts',(-2.15250461100006,15.2,11.004333354));
#232471=CARTESIAN_POINT('Ctrl Pts',(-2.15250461100006,11.6,11.004333354));
#232472=CARTESIAN_POINT('Ctrl Pts',(-2.15441423500006,15.2,11.007176061));
#232473=CARTESIAN_POINT('Ctrl Pts',(-2.15441423500006,11.6,11.007176061));
#232474=CARTESIAN_POINT('Ctrl Pts',(-2.15632879900005,15.2,11.010021279));
#232475=CARTESIAN_POINT('Ctrl Pts',(-2.15632879900005,11.6,11.010021279));
#232476=CARTESIAN_POINT('Ctrl Pts',(-2.15824830200006,15.2,11.012868997));
#232477=CARTESIAN_POINT('Ctrl Pts',(-2.15824830200006,11.6,11.012868997));
#232478=CARTESIAN_POINT('Ctrl Pts',(-2.16017274700006,15.2,11.015719206));
#232479=CARTESIAN_POINT('Ctrl Pts',(-2.16017274700006,11.6,11.015719206));
#232480=CARTESIAN_POINT('Ctrl Pts',(-2.16210213200006,15.2,11.018571894));
#232481=CARTESIAN_POINT('Ctrl Pts',(-2.16210213200006,11.6,11.018571894));
#232482=CARTESIAN_POINT('Ctrl Pts',(-2.16403645900006,15.2,11.021427054));
#232483=CARTESIAN_POINT('Ctrl Pts',(-2.16403645900006,11.6,11.021427054));
#232484=CARTESIAN_POINT('Ctrl Pts',(-2.16597572900006,15.2,11.024284674));
#232485=CARTESIAN_POINT('Ctrl Pts',(-2.16597572900006,11.6,11.024284674));
#232486=CARTESIAN_POINT('Ctrl Pts',(-2.16791994200006,15.2,11.027144743));
#232487=CARTESIAN_POINT('Ctrl Pts',(-2.16791994200006,11.6,11.027144743));
#232488=CARTESIAN_POINT('Ctrl Pts',(-2.16986910100006,15.2,11.030007253));
#232489=CARTESIAN_POINT('Ctrl Pts',(-2.16986910100006,11.6,11.030007253));
#232490=CARTESIAN_POINT('Ctrl Pts',(-2.17182320400005,15.2,11.032872191));
#232491=CARTESIAN_POINT('Ctrl Pts',(-2.17182320400005,11.6,11.032872191));
#232492=CARTESIAN_POINT('Ctrl Pts',(-2.17378225200005,15.2,11.03573955));
#232493=CARTESIAN_POINT('Ctrl Pts',(-2.17378225200005,11.6,11.03573955));
#232494=CARTESIAN_POINT('Ctrl Pts',(-2.17574624800006,15.2,11.038609318));
#232495=CARTESIAN_POINT('Ctrl Pts',(-2.17574624800006,11.6,11.038609318));
#232496=CARTESIAN_POINT('Ctrl Pts',(-2.17771519000005,15.2,11.041481486));
#232497=CARTESIAN_POINT('Ctrl Pts',(-2.17771519000005,11.6,11.041481486));
#232498=CARTESIAN_POINT('Ctrl Pts',(-2.17968908100006,15.2,11.044356044));
#232499=CARTESIAN_POINT('Ctrl Pts',(-2.17968908100006,11.6,11.044356044));
#232500=CARTESIAN_POINT('Ctrl Pts',(-2.18166792000006,15.2,11.047232981));
#232501=CARTESIAN_POINT('Ctrl Pts',(-2.18166792000006,11.6,11.047232981));
#232502=CARTESIAN_POINT('Ctrl Pts',(-2.18365170900006,15.2,11.050112287));
#232503=CARTESIAN_POINT('Ctrl Pts',(-2.18365170900006,11.6,11.050112287));
#232504=CARTESIAN_POINT('Ctrl Pts',(-2.18564044700006,15.2,11.052993953));
#232505=CARTESIAN_POINT('Ctrl Pts',(-2.18564044700006,11.6,11.052993953));
#232506=CARTESIAN_POINT('Ctrl Pts',(-2.18763413600006,15.2,11.05587797));
#232507=CARTESIAN_POINT('Ctrl Pts',(-2.18763413600006,11.6,11.05587797));
#232508=CARTESIAN_POINT('Ctrl Pts',(-2.18963277800006,15.2,11.058764325));
#232509=CARTESIAN_POINT('Ctrl Pts',(-2.18963277800006,11.6,11.058764325));
#232510=CARTESIAN_POINT('Ctrl Pts',(-2.19163637000006,15.2,11.06165301));
#232511=CARTESIAN_POINT('Ctrl Pts',(-2.19163637000006,11.6,11.06165301));
#232512=CARTESIAN_POINT('Ctrl Pts',(-2.19364491500006,15.2,11.064544015));
#232513=CARTESIAN_POINT('Ctrl Pts',(-2.19364491500006,11.6,11.064544015));
#232514=CARTESIAN_POINT('Ctrl Pts',(-2.19565841400006,15.2,11.06743733));
#232515=CARTESIAN_POINT('Ctrl Pts',(-2.19565841400006,11.6,11.06743733));
#232516=CARTESIAN_POINT('Ctrl Pts',(-2.19767686600005,15.2,11.070332946));
#232517=CARTESIAN_POINT('Ctrl Pts',(-2.19767686600005,11.6,11.070332946));
#232518=CARTESIAN_POINT('Ctrl Pts',(-2.19970027200006,15.2,11.073230851));
#232519=CARTESIAN_POINT('Ctrl Pts',(-2.19970027200006,11.6,11.073230851));
#232520=CARTESIAN_POINT('Ctrl Pts',(-2.20172863400005,15.2,11.076131037));
#232521=CARTESIAN_POINT('Ctrl Pts',(-2.20172863400005,11.6,11.076131037));
#232522=CARTESIAN_POINT('Ctrl Pts',(-2.20376195100005,15.2,11.079033494));
#232523=CARTESIAN_POINT('Ctrl Pts',(-2.20376195100005,11.6,11.079033494));
#232524=CARTESIAN_POINT('Ctrl Pts',(-2.20580022500006,15.2,11.081938211));
#232525=CARTESIAN_POINT('Ctrl Pts',(-2.20580022500006,11.6,11.081938211));
#232526=CARTESIAN_POINT('Ctrl Pts',(-2.20784345600006,15.2,11.08484518));
#232527=CARTESIAN_POINT('Ctrl Pts',(-2.20784345600006,11.6,11.08484518));
#232528=CARTESIAN_POINT('Ctrl Pts',(-2.20989164400006,15.2,11.08775439));
#232529=CARTESIAN_POINT('Ctrl Pts',(-2.20989164400006,11.6,11.08775439));
#232530=CARTESIAN_POINT('Ctrl Pts',(-2.21194479000005,15.2,11.090665832));
#232531=CARTESIAN_POINT('Ctrl Pts',(-2.21194479000005,11.6,11.090665832));
#232532=CARTESIAN_POINT('Ctrl Pts',(-2.21400289400006,15.2,11.093579495));
#232533=CARTESIAN_POINT('Ctrl Pts',(-2.21400289400006,11.6,11.093579495));
#232534=CARTESIAN_POINT('Ctrl Pts',(-2.21606595800006,15.2,11.09649537));
#232535=CARTESIAN_POINT('Ctrl Pts',(-2.21606595800006,11.6,11.09649537));
#232536=CARTESIAN_POINT('Ctrl Pts',(-2.21813398100006,15.2,11.099413448));
#232537=CARTESIAN_POINT('Ctrl Pts',(-2.21813398100006,11.6,11.099413448));
#232538=CARTESIAN_POINT('Ctrl Pts',(-2.22020696400006,15.2,11.102333719));
#232539=CARTESIAN_POINT('Ctrl Pts',(-2.22020696400006,11.6,11.102333719));
#232540=CARTESIAN_POINT('Ctrl Pts',(-2.22228490800005,15.2,11.105256173));
#232541=CARTESIAN_POINT('Ctrl Pts',(-2.22228490800005,11.6,11.105256173));
#232542=CARTESIAN_POINT('Ctrl Pts',(-2.22436781300006,15.2,11.1081808));
#232543=CARTESIAN_POINT('Ctrl Pts',(-2.22436781300006,11.6,11.1081808));
#232544=CARTESIAN_POINT('Ctrl Pts',(-2.22645567900006,15.2,11.111107592));
#232545=CARTESIAN_POINT('Ctrl Pts',(-2.22645567900006,11.6,11.111107592));
#232546=CARTESIAN_POINT('Ctrl Pts',(-2.22854850800006,15.2,11.114036538));
#232547=CARTESIAN_POINT('Ctrl Pts',(-2.22854850800006,11.6,11.114036538));
#232548=CARTESIAN_POINT('Ctrl Pts',(-2.23064629900006,15.2,11.116967628));
#232549=CARTESIAN_POINT('Ctrl Pts',(-2.23064629900006,11.6,11.116967628));
#232550=CARTESIAN_POINT('Ctrl Pts',(-2.23274905300006,15.2,11.119900853));
#232551=CARTESIAN_POINT('Ctrl Pts',(-2.23274905300006,11.6,11.119900853));
#232552=CARTESIAN_POINT('Ctrl Pts',(-2.23485677000005,15.2,11.122836203));
#232553=CARTESIAN_POINT('Ctrl Pts',(-2.23485677000005,11.6,11.122836203));
#232554=CARTESIAN_POINT('Ctrl Pts',(-2.23696945300006,15.2,11.12577367));
#232555=CARTESIAN_POINT('Ctrl Pts',(-2.23696945300006,11.6,11.12577367));
#232556=CARTESIAN_POINT('Ctrl Pts',(-2.23908709900006,15.2,11.128713244));
#232557=CARTESIAN_POINT('Ctrl Pts',(-2.23908709900006,11.6,11.128713244));
#232558=CARTESIAN_POINT('Ctrl Pts',(-2.24120971000006,15.2,11.131654913));
#232559=CARTESIAN_POINT('Ctrl Pts',(-2.24120971000006,11.6,11.131654913));
#232560=CARTESIAN_POINT('Ctrl Pts',(-2.24333728600006,15.2,11.134598672));
#232561=CARTESIAN_POINT('Ctrl Pts',(-2.24333728600006,11.6,11.134598672));
#232562=CARTESIAN_POINT('Ctrl Pts',(-2.24546982700006,15.2,11.137544507));
#232563=CARTESIAN_POINT('Ctrl Pts',(-2.24546982700006,11.6,11.137544507));
#232564=CARTESIAN_POINT('Ctrl Pts',(-2.24760733500006,15.2,11.140492411));
#232565=CARTESIAN_POINT('Ctrl Pts',(-2.24760733500006,11.6,11.140492411));
#232566=CARTESIAN_POINT('Ctrl Pts',(-2.24974981000006,15.2,11.143442374));
#232567=CARTESIAN_POINT('Ctrl Pts',(-2.24974981000006,11.6,11.143442374));
#232568=CARTESIAN_POINT('Ctrl Pts',(-2.25189725100006,15.2,11.146394387));
#232569=CARTESIAN_POINT('Ctrl Pts',(-2.25189725100006,11.6,11.146394387));
#232570=CARTESIAN_POINT('Ctrl Pts',(-2.25404966000006,15.2,11.14934844));
#232571=CARTESIAN_POINT('Ctrl Pts',(-2.25404966000006,11.6,11.14934844));
#232572=CARTESIAN_POINT('Ctrl Pts',(-2.25620703600006,15.2,11.152304525));
#232573=CARTESIAN_POINT('Ctrl Pts',(-2.25620703600006,11.6,11.152304525));
#232574=CARTESIAN_POINT('Ctrl Pts',(-2.25836938000006,15.2,11.15526263));
#232575=CARTESIAN_POINT('Ctrl Pts',(-2.25836938000006,11.6,11.15526263));
#232576=CARTESIAN_POINT('Ctrl Pts',(-2.26053669300006,15.2,11.158222748));
#232577=CARTESIAN_POINT('Ctrl Pts',(-2.26053669300006,11.6,11.158222748));
#232578=CARTESIAN_POINT('Ctrl Pts',(-2.26270897400005,15.2,11.161184868));
#232579=CARTESIAN_POINT('Ctrl Pts',(-2.26270897400005,11.6,11.161184868));
#232580=CARTESIAN_POINT('Ctrl Pts',(-2.26488622500006,15.2,11.164148983));
#232581=CARTESIAN_POINT('Ctrl Pts',(-2.26488622500006,11.6,11.164148983));
#232582=CARTESIAN_POINT('Ctrl Pts',(-2.26706844500006,15.2,11.16711508));
#232583=CARTESIAN_POINT('Ctrl Pts',(-2.26706844500006,11.6,11.16711508));
#232584=CARTESIAN_POINT('Ctrl Pts',(-2.26925563400005,15.2,11.170083153));
#232585=CARTESIAN_POINT('Ctrl Pts',(-2.26925563400005,11.6,11.170083153));
#232586=CARTESIAN_POINT('Ctrl Pts',(-2.27144779400006,15.2,11.173053191));
#232587=CARTESIAN_POINT('Ctrl Pts',(-2.27144779400006,11.6,11.173053191));
#232588=CARTESIAN_POINT('Ctrl Pts',(-2.27364492400006,15.2,11.176025185));
#232589=CARTESIAN_POINT('Ctrl Pts',(-2.27364492400006,11.6,11.176025185));
#232590=CARTESIAN_POINT('Ctrl Pts',(-2.27584702400006,15.2,11.178999126));
#232591=CARTESIAN_POINT('Ctrl Pts',(-2.27584702400006,11.6,11.178999126));
#232592=CARTESIAN_POINT('Ctrl Pts',(-2.27805409600006,15.2,11.181975005));
#232593=CARTESIAN_POINT('Ctrl Pts',(-2.27805409600006,11.6,11.181975005));
#232594=CARTESIAN_POINT('Ctrl Pts',(-2.28026613900006,15.2,11.184952813));
#232595=CARTESIAN_POINT('Ctrl Pts',(-2.28026613900006,11.6,11.184952813));
#232596=CARTESIAN_POINT('Ctrl Pts',(-2.28248315300006,15.2,11.187932541));
#232597=CARTESIAN_POINT('Ctrl Pts',(-2.28248315300006,11.6,11.187932541));
#232598=CARTESIAN_POINT('Ctrl Pts',(-2.28470513900006,15.2,11.19091418));
#232599=CARTESIAN_POINT('Ctrl Pts',(-2.28470513900006,11.6,11.19091418));
#232600=CARTESIAN_POINT('Ctrl Pts',(-2.28693209700006,15.2,11.193897718));
#232601=CARTESIAN_POINT('Ctrl Pts',(-2.28693209700006,11.6,11.193897718));
#232602=CARTESIAN_POINT('Ctrl Pts',(-2.28916402800006,15.2,11.19688315));
#232603=CARTESIAN_POINT('Ctrl Pts',(-2.28916402800006,11.6,11.19688315));
#232604=CARTESIAN_POINT('Ctrl Pts',(-2.29140093100006,15.2,11.199870463));
#232605=CARTESIAN_POINT('Ctrl Pts',(-2.29140093100006,11.6,11.199870463));
#232606=CARTESIAN_POINT('Ctrl Pts',(-2.29364280600006,15.2,11.202859649));
#232607=CARTESIAN_POINT('Ctrl Pts',(-2.29364280600006,11.6,11.202859649));
#232608=CARTESIAN_POINT('Ctrl Pts',(-2.29588965500006,15.2,11.205850699));
#232609=CARTESIAN_POINT('Ctrl Pts',(-2.29588965500006,11.6,11.205850699));
#232610=CARTESIAN_POINT('Ctrl Pts',(-2.29814147700006,15.2,11.208843603));
#232611=CARTESIAN_POINT('Ctrl Pts',(-2.29814147700006,11.6,11.208843603));
#232612=CARTESIAN_POINT('Ctrl Pts',(-2.30039827300006,15.2,11.211838352));
#232613=CARTESIAN_POINT('Ctrl Pts',(-2.30039827300006,11.6,11.211838352));
#232614=CARTESIAN_POINT('Ctrl Pts',(-2.30266004300006,15.2,11.214834939));
#232615=CARTESIAN_POINT('Ctrl Pts',(-2.30266004300006,11.6,11.214834939));
#232616=CARTESIAN_POINT('Ctrl Pts',(-2.30492678500006,15.2,11.217833355));
#232617=CARTESIAN_POINT('Ctrl Pts',(-2.30492678500006,11.6,11.217833355));
#232618=CARTESIAN_POINT('Ctrl Pts',(-2.30719850200006,15.2,11.220833594));
#232619=CARTESIAN_POINT('Ctrl Pts',(-2.30719850200006,11.6,11.220833594));
#232620=CARTESIAN_POINT('Ctrl Pts',(-2.30947519300006,15.2,11.223835644));
#232621=CARTESIAN_POINT('Ctrl Pts',(-2.30947519300006,11.6,11.223835644));
#232622=CARTESIAN_POINT('Ctrl Pts',(-2.31175685900006,15.2,11.226839497));
#232623=CARTESIAN_POINT('Ctrl Pts',(-2.31175685900006,11.6,11.226839497));
#232624=CARTESIAN_POINT('Ctrl Pts',(-2.31404349900005,15.2,11.229845144));
#232625=CARTESIAN_POINT('Ctrl Pts',(-2.31404349900005,11.6,11.229845144));
#232626=CARTESIAN_POINT('Ctrl Pts',(-2.31633511400006,15.2,11.232852573));
#232627=CARTESIAN_POINT('Ctrl Pts',(-2.31633511400006,11.6,11.232852573));
#232628=CARTESIAN_POINT('Ctrl Pts',(-2.31863170400006,15.2,11.23586177));
#232629=CARTESIAN_POINT('Ctrl Pts',(-2.31863170400006,11.6,11.23586177));
#232630=CARTESIAN_POINT('Ctrl Pts',(-2.32093326800006,15.2,11.238872729));
#232631=CARTESIAN_POINT('Ctrl Pts',(-2.32093326800006,11.6,11.238872729));
#232632=CARTESIAN_POINT('Ctrl Pts',(-2.32323980900006,15.2,11.241885437));
#232633=CARTESIAN_POINT('Ctrl Pts',(-2.32323980900006,11.6,11.241885437));
#232634=CARTESIAN_POINT('Ctrl Pts',(-2.32555132500006,15.2,11.244899888));
#232635=CARTESIAN_POINT('Ctrl Pts',(-2.32555132500006,11.6,11.244899888));
#232636=CARTESIAN_POINT('Ctrl Pts',(-2.32786781600006,15.2,11.247916073));
#232637=CARTESIAN_POINT('Ctrl Pts',(-2.32786781600006,11.6,11.247916073));
#232638=CARTESIAN_POINT('Ctrl Pts',(-2.33018928300006,15.2,11.250933991));
#232639=CARTESIAN_POINT('Ctrl Pts',(-2.33018928300006,11.6,11.250933991));
#232640=CARTESIAN_POINT('Ctrl Pts',(-2.33251572500006,15.2,11.253953638));
#232641=CARTESIAN_POINT('Ctrl Pts',(-2.33251572500006,11.6,11.253953638));
#232642=CARTESIAN_POINT('Ctrl Pts',(-2.33438085900006,15.2,11.256370738));
#232643=CARTESIAN_POINT('Ctrl Pts',(-2.33438085900006,11.6,11.256370738));
#232644=CARTESIAN_POINT('Ctrl Pts',(-2.33578194800006,15.2,11.258184341));
#232645=CARTESIAN_POINT('Ctrl Pts',(-2.33578194800006,11.6,11.258184341));
#232646=CARTESIAN_POINT('Ctrl Pts',(-2.33671700200006,15.2,11.259393755));
#232647=CARTESIAN_POINT('Ctrl Pts',(-2.33671700200006,11.6,11.259393755));
#232648=CARTESIAN_POINT('Ctrl Pts',(-2.33718477800006,15.2,11.259998549));
#232649=CARTESIAN_POINT('Ctrl Pts',(-2.33718477800006,11.6,11.259998549));
#232650=CARTESIAN_POINT('Ctrl Pts',(-1.76496130700006,15.2,10.22377311));
#232651=CARTESIAN_POINT('Ctrl Pts',(-1.76541543493207,15.2,10.2255010873779));
#232652=CARTESIAN_POINT('Ctrl Pts',(-1.76588926591707,15.2,10.2272829938834));
#232653=CARTESIAN_POINT('Ctrl Pts',(-1.76638321147092,15.2,10.2291177140323));
#232654=CARTESIAN_POINT('Ctrl Pts',(-1.76687953907992,15.2,10.2309612821291));
#232655=CARTESIAN_POINT('Ctrl Pts',(-1.76739616286972,15.2,10.2328581799819));
#232656=CARTESIAN_POINT('Ctrl Pts',(-1.76793345451038,15.2,10.2348073231886));
#232657=CARTESIAN_POINT('Ctrl Pts',(-1.76847074610224,15.2,10.2367564662182));
#232658=CARTESIAN_POINT('Ctrl Pts',(-1.76902870497939,15.2,10.2387578539245));
#232659=CARTESIAN_POINT('Ctrl Pts',(-1.76960768654168,15.2,10.2408104330166));
#232660=CARTESIAN_POINT('Ctrl Pts',(-1.77018666810398,15.2,10.2428630121086));
#232661=CARTESIAN_POINT('Ctrl Pts',(-1.77078667246607,15.2,10.2449667819402));
#232662=CARTESIAN_POINT('Ctrl Pts',(-1.77140804397329,15.2,10.24712072005));
#232663=CARTESIAN_POINT('Ctrl Pts',(-1.77202941553697,15.2,10.2492746583554));
#232664=CARTESIAN_POINT('Ctrl Pts',(-1.77267215276809,15.2,10.2514787598444));
#232665=CARTESIAN_POINT('Ctrl Pts',(-1.77333658730578,15.2,10.2537320332205));
#232666=CARTESIAN_POINT('Ctrl Pts',(-1.77400102178312,15.2,10.255985306392));
#232667=CARTESIAN_POINT('Ctrl Pts',(-1.77468715486446,15.2,10.2582877466256));
#232668=CARTESIAN_POINT('Ctrl Pts',(-1.77539530325867,15.2,10.260638386051));
#232669=CARTESIAN_POINT('Ctrl Pts',(-1.77610345165288,15.2,10.2629890254764));
#232670=CARTESIAN_POINT('Ctrl Pts',(-1.77683361717075,15.2,10.2653878615328));
#232671=CARTESIAN_POINT('Ctrl Pts',(-1.77758610564243,15.2,10.2678339508585));
#232672=CARTESIAN_POINT('Ctrl Pts',(-1.77833859418247,15.2,10.2702800404063));
#232673=CARTESIAN_POINT('Ctrl Pts',(-1.77911340904196,15.2,10.2727733804935));
#232674=CARTESIAN_POINT('Ctrl Pts',(-1.77991084258694,15.2,10.2753130495517));
#232675=CARTESIAN_POINT('Ctrl Pts',(-1.7807082760595,15.2,10.2778527183792));
#232676=CARTESIAN_POINT('Ctrl Pts',(-1.78152833193401,15.2,10.2804387173121));
#232677=CARTESIAN_POINT('Ctrl Pts',(-1.78237129432105,15.2,10.2830701451352));
#232678=CARTESIAN_POINT('Ctrl Pts',(-1.7832142567081,15.2,10.2857015729583));
#232679=CARTESIAN_POINT('Ctrl Pts',(-1.78408012798497,15.2,10.2883784311276));
#232680=CARTESIAN_POINT('Ctrl Pts',(-1.78496918228499,15.2,10.2910998401101));
#232681=CARTESIAN_POINT('Ctrl Pts',(-1.78585823658502,15.2,10.2938212490926));
#232682=CARTESIAN_POINT('Ctrl Pts',(-1.78677047506695,15.2,10.2965872102404));
#232683=CARTESIAN_POINT('Ctrl Pts',(-1.7877061643647,15.2,10.2993968662187));
#232684=CARTESIAN_POINT('Ctrl Pts',(-1.7887978019354,15.2,10.3026747983635));
#232685=CARTESIAN_POINT('Ctrl Pts',(-1.78992136090724,15.2,10.3060122026356));
#232686=CARTESIAN_POINT('Ctrl Pts',(-1.79107724768775,15.2,10.3094077546164));
#232687=CARTESIAN_POINT('Ctrl Pts',(-1.79223313446825,15.2,10.3128033065971));
#232688=CARTESIAN_POINT('Ctrl Pts',(-1.79342135008691,15.2,10.3162570016962));
#232689=CARTESIAN_POINT('Ctrl Pts',(-1.79464228456548,15.2,10.3197675544474));
#232690=CARTESIAN_POINT('Ctrl Pts',(-1.79568879977852,15.2,10.3227765995066));
#232691=CARTESIAN_POINT('Ctrl Pts',(-1.79675935631462,15.2,10.325827414804));
#232692=CARTESIAN_POINT('Ctrl Pts',(-1.79785418744045,15.2,10.3289192081066));
#232693=CARTESIAN_POINT('Ctrl Pts',(-1.79913149048688,15.2,10.3325263004801));
#232694=CARTESIAN_POINT('Ctrl Pts',(-1.80044184035678,15.2,10.3361891677487));
#232695=CARTESIAN_POINT('Ctrl Pts',(-1.80178559450887,15.2,10.3399065789764));
#232696=CARTESIAN_POINT('Ctrl Pts',(-1.8029373837223,15.2,10.3430929312918));
#232697=CARTESIAN_POINT('Ctrl Pts',(-1.80411371803772,15.2,10.3463193572175));
#232698=CARTESIAN_POINT('Ctrl Pts',(-1.80531481690965,15.2,10.3495851005138));
#232699=CARTESIAN_POINT('Ctrl Pts',(-1.80651591589069,15.2,10.3528508441067));
#232700=CARTESIAN_POINT('Ctrl Pts',(-1.80774177967481,15.2,10.3561559049212));
#232701=CARTESIAN_POINT('Ctrl Pts',(-1.80899262066136,15.2,10.359499539856));
#232702=CARTESIAN_POINT('Ctrl Pts',(-1.81045193497523,15.2,10.3634004468245));
#232703=CARTESIAN_POINT('Ctrl Pts',(-1.81194524810849,15.2,10.3673538598976));
#232704=CARTESIAN_POINT('Ctrl Pts',(-1.81347288367876,15.2,10.371358629063));
#232705=CARTESIAN_POINT('Ctrl Pts',(-1.81478228574905,15.2,10.3747912887485));
#232706=CARTESIAN_POINT('Ctrl Pts',(-1.81611690607242,15.2,10.3782616779469));
#232707=CARTESIAN_POINT('Ctrl Pts',(-1.81747694114826,15.2,10.3817690888906));
#232708=CARTESIAN_POINT('Ctrl Pts',(-1.81883697610056,15.2,10.3852764995156));
#232709=CARTESIAN_POINT('Ctrl Pts',(-1.82022242567718,15.2,10.3888209322404));
#232710=CARTESIAN_POINT('Ctrl Pts',(-1.82163348329369,15.2,10.3924016919452));
#232711=CARTESIAN_POINT('Ctrl Pts',(-1.82327971726508,15.2,10.396579245151));
#232712=CARTESIAN_POINT('Ctrl Pts',(-1.82496080224826,15.2,10.40080624303));
#232713=CARTESIAN_POINT('Ctrl Pts',(-1.82667703515203,15.2,10.405081607141));
#232714=CARTESIAN_POINT('Ctrl Pts',(-1.82814809185033,15.2,10.4087462047603));
#232715=CARTESIAN_POINT('Ctrl Pts',(-1.82964496786233,15.2,10.4124463342712));
#232716=CARTESIAN_POINT('Ctrl Pts',(-1.83116784455811,15.2,10.4161813339703));
#232717=CARTESIAN_POINT('Ctrl Pts',(-1.83243690851737,15.2,10.4192938338326));
#232718=CARTESIAN_POINT('Ctrl Pts',(-1.83372402674008,15.2,10.4224305475944));
#232719=CARTESIAN_POINT('Ctrl Pts',(-1.83502929910215,15.2,10.4255910959984));
#232720=CARTESIAN_POINT('Ctrl Pts',(-1.83633457146423,15.2,10.4287516444025));
#232721=CARTESIAN_POINT('Ctrl Pts',(-1.8376579978042,15.2,10.4319360296438));
#232722=CARTESIAN_POINT('Ctrl Pts',(-1.83899967516415,15.2,10.4351438766807));
#232723=CARTESIAN_POINT('Ctrl Pts',(-1.8406096879376,15.2,10.4389932929851));
#232724=CARTESIAN_POINT('Ctrl Pts',(-1.84224598213541,15.2,10.4428764951005));
#232725=CARTESIAN_POINT('Ctrl Pts',(-1.84390871899168,15.2,10.4467928500416));
#232726=CARTESIAN_POINT('Ctrl Pts',(-1.84529433308891,15.2,10.4500564792777));
#232727=CARTESIAN_POINT('Ctrl Pts',(-1.84669831180539,15.2,10.4533431311977));
#232728=CARTESIAN_POINT('Ctrl Pts',(-1.84812074403412,15.2,10.4566524455184));
#232729=CARTESIAN_POINT('Ctrl Pts',(-1.84954317626286,15.2,10.4599617598391));
#232730=CARTESIAN_POINT('Ctrl Pts',(-1.85098406170572,15.2,10.4632937354628));
#232731=CARTESIAN_POINT('Ctrl Pts',(-1.85244349059557,15.2,10.4666480189361));
#232732=CARTESIAN_POINT('Ctrl Pts',(-1.8539029194854,15.2,10.4700023024094));
#232733=CARTESIAN_POINT('Ctrl Pts',(-1.85538089015814,15.2,10.4733788935545));
#232734=CARTESIAN_POINT('Ctrl Pts',(-1.856877489048,15.2,10.476777441264));
#232735=CARTESIAN_POINT('Ctrl Pts',(-1.85837408793786,15.2,10.4801759889735));
#232736=CARTESIAN_POINT('Ctrl Pts',(-1.8598893144058,15.2,10.4835964935706));
#232737=CARTESIAN_POINT('Ctrl Pts',(-1.86142325246981,15.2,10.4870386099246));
#232738=CARTESIAN_POINT('Ctrl Pts',(-1.86357076562567,15.2,10.49185757252));
#232739=CARTESIAN_POINT('Ctrl Pts',(-1.86575495311634,15.2,10.4967188955553));
#232740=CARTESIAN_POINT('Ctrl Pts',(-1.86797603605917,15.2,10.5016216455669));
#232741=CARTESIAN_POINT('Ctrl Pts',(-1.86956252397429,15.2,10.505123610079));
#232742=CARTESIAN_POINT('Ctrl Pts',(-1.87116783398727,15.2,10.5086467122575));
#232743=CARTESIAN_POINT('Ctrl Pts',(-1.87279204705319,15.2,10.5121906186136));
#232744=CARTESIAN_POINT('Ctrl Pts',(-1.87441626011912,15.2,10.5157345249697));
#232745=CARTESIAN_POINT('Ctrl Pts',(-1.87605937489797,15.2,10.5192992351444));
#232746=CARTESIAN_POINT('Ctrl Pts',(-1.87772146538309,15.2,10.5228844204906));
#232747=CARTESIAN_POINT('Ctrl Pts',(-1.87938355586821,15.2,10.5264696058367));
#232748=CARTESIAN_POINT('Ctrl Pts',(-1.8810646226677,15.2,10.5300752665917));
#232749=CARTESIAN_POINT('Ctrl Pts',(-1.88276473988894,15.2,10.5337010777713));
#232750=CARTESIAN_POINT('Ctrl Pts',(-1.88446485711018,15.2,10.5373268889508));
#232751=CARTESIAN_POINT('Ctrl Pts',(-1.88618402469853,15.2,10.5409728519169));
#232752=CARTESIAN_POINT('Ctrl Pts',(-1.88792231191978,15.2,10.544638645527));
#232753=CARTESIAN_POINT('Ctrl Pts',(-1.88966059914102,15.2,10.5483044391371));
#232754=CARTESIAN_POINT('Ctrl Pts',(-1.89141800780214,15.2,10.5519900629089));
#232755=CARTESIAN_POINT('Ctrl Pts',(-1.89319460649071,15.2,10.5556952024396));
#232756=CARTESIAN_POINT('Ctrl Pts',(-1.89497120517928,15.2,10.5594003419703));
#232757=CARTESIAN_POINT('Ctrl Pts',(-1.89676699360556,15.2,10.5631249979611));
#232758=CARTESIAN_POINT('Ctrl Pts',(-1.89858203825834,15.2,10.5668688560166));
#232759=CARTESIAN_POINT('Ctrl Pts',(-1.9000340740597,15.2,10.5698639426243));
#232760=CARTESIAN_POINT('Ctrl Pts',(-1.90149843394584,15.2,10.5728713194945));
#232761=CARTESIAN_POINT('Ctrl Pts',(-1.90297515108312,15.2,10.5758908299936));
#232762=CARTESIAN_POINT('Ctrl Pts',(-1.90445186801919,15.2,10.5789103400813));
#232763=CARTESIAN_POINT('Ctrl Pts',(-1.90594094191218,15.2,10.5819419825496));
#232764=CARTESIAN_POINT('Ctrl Pts',(-1.90744240674066,15.2,10.5849856019812));
#232765=CARTESIAN_POINT('Ctrl Pts',(-1.90894387177371,15.2,10.5880292218275));
#232766=CARTESIAN_POINT('Ctrl Pts',(-1.91045772694566,15.2,10.5910848193081));
#232767=CARTESIAN_POINT('Ctrl Pts',(-1.9119840033079,15.2,10.5941522379765));
#232768=CARTESIAN_POINT('Ctrl Pts',(-1.91351027946217,15.2,10.5972196562269));
#232769=CARTESIAN_POINT('Ctrl Pts',(-1.91504897688702,15.2,10.6002988976035));
#232770=CARTESIAN_POINT('Ctrl Pts',(-1.91660012714832,15.2,10.603389807739));
#232771=CARTESIAN_POINT('Ctrl Pts',(-1.91815127762096,15.2,10.6064807182957));
#232772=CARTESIAN_POINT('Ctrl Pts',(-1.91971488142971,15.2,10.6095832976644));
#232773=CARTESIAN_POINT('Ctrl Pts',(-1.92129096726211,15.2,10.6126973964352));
#232774=CARTESIAN_POINT('Ctrl Pts',(-1.92326107444525,15.2,10.6165900196865));
#232775=CARTESIAN_POINT('Ctrl Pts',(-1.92525068610564,15.2,10.6205006398734));
#232776=CARTESIAN_POINT('Ctrl Pts',(-1.92725985978782,15.2,10.6244289637638));
#232777=CARTESIAN_POINT('Ctrl Pts',(-1.92926903347,15.2,10.6283572876542));
#232778=CARTESIAN_POINT('Ctrl Pts',(-1.93129776727192,15.2,10.632303316717));
#232779=CARTESIAN_POINT('Ctrl Pts',(-1.93334612005127,15.2,10.63626676151));
#232780=CARTESIAN_POINT('Ctrl Pts',(-1.93498480214079,15.2,10.6394375170853));
#232781=CARTESIAN_POINT('Ctrl Pts',(-1.93663603814127,15.2,10.6426194186693));
#232782=CARTESIAN_POINT('Ctrl Pts',(-1.93829985695721,15.2,10.6458123202561));
#232783=CARTESIAN_POINT('Ctrl Pts',(-1.93996367599985,15.2,10.6490052222779));
#232784=CARTESIAN_POINT('Ctrl Pts',(-1.9416400778606,15.2,10.6522091241576));
#232785=CARTESIAN_POINT('Ctrl Pts',(-1.9433290895095,15.2,10.6554238815006));
#232786=CARTESIAN_POINT('Ctrl Pts',(-1.94501810092827,15.2,10.6586386384055));
#232787=CARTESIAN_POINT('Ctrl Pts',(-1.94671972068151,15.2,10.6618642508535));
#232788=CARTESIAN_POINT('Ctrl Pts',(-1.94843397681832,15.2,10.6651005749771));
#232789=CARTESIAN_POINT('Ctrl Pts',(-1.95014823318869,15.2,10.6683368995417));
#232790=CARTESIAN_POINT('Ctrl Pts',(-1.95187512535022,15.2,10.6715839345065));
#232791=CARTESIAN_POINT('Ctrl Pts',(-1.9536146784775,15.2,10.674841540681));
#232792=CARTESIAN_POINT('Ctrl Pts',(-1.95578911976809,15.2,10.6789135481773));
#232793=CARTESIAN_POINT('Ctrl Pts',(-1.95798334494354,15.2,10.6830020695188));
#232794=CARTESIAN_POINT('Ctrl Pts',(-1.96019740105628,15.2,10.6871068318119));
#232795=CARTESIAN_POINT('Ctrl Pts',(-1.96196864580168,15.2,10.6903906413778));
#232796=CARTESIAN_POINT('Ctrl Pts',(-1.96375258250929,15.2,10.6936848447646));
#232797=CARTESIAN_POINT('Ctrl Pts',(-1.96554923586158,15.2,10.6969893024382));
#232798=CARTESIAN_POINT('Ctrl Pts',(-1.96734588945867,15.2,10.7002937605621));
#232799=CARTESIAN_POINT('Ctrl Pts',(-1.96915525932304,15.2,10.7036084741259));
#232800=CARTESIAN_POINT('Ctrl Pts',(-1.97097736851447,15.2,10.7069333049741));
#232801=CARTESIAN_POINT('Ctrl Pts',(-1.97279947745765,15.2,10.7102581353693));
#232802=CARTESIAN_POINT('Ctrl Pts',(-1.97463432522597,15.2,10.7135930801896));
#232803=CARTESIAN_POINT('Ctrl Pts',(-1.97648193657408,15.2,10.7169380076933));
#232804=CARTESIAN_POINT('Ctrl Pts',(-1.97832954817392,15.2,10.7202829356526));
#232805=CARTESIAN_POINT('Ctrl Pts',(-1.98018992160868,15.2,10.7236378431383));
#232806=CARTESIAN_POINT('Ctrl Pts',(-1.98206307987825,15.2,10.7270025952668));
#232807=CARTESIAN_POINT('Ctrl Pts',(-1.98534110646718,15.2,10.7328909108039));
#232808=CARTESIAN_POINT('Ctrl Pts',(-1.98865828528117,15.2,10.7388093765999));
#232809=CARTESIAN_POINT('Ctrl Pts',(-1.99201473169475,15.2,10.7447572738942));
#232810=CARTESIAN_POINT('Ctrl Pts',(-1.99441219356806,15.2,10.7490057722262));
#232811=CARTESIAN_POINT('Ctrl Pts',(-1.99682969042726,15.2,10.7532692880193));
#232812=CARTESIAN_POINT('Ctrl Pts',(-1.99926725993951,15.2,10.7575475629487));
#232813=CARTESIAN_POINT('Ctrl Pts',(-2.00121731565559,15.2,10.7609701830787));
#232814=CARTESIAN_POINT('Ctrl Pts',(-2.00318021886519,15.2,10.7644022489491));
#232815=CARTESIAN_POINT('Ctrl Pts',(-2.00515598925969,15.2,10.767843629819));
#232816=CARTESIAN_POINT('Ctrl Pts',(-2.00762570211822,15.2,10.7721453556719));
#232817=CARTESIAN_POINT('Ctrl Pts',(-2.01011552044656,15.2,10.776461636477));
#232818=CARTESIAN_POINT('Ctrl Pts',(-2.01262548065595,15.2,10.7807922197416));
#232819=CARTESIAN_POINT('Ctrl Pts',(-2.01513544086535,15.2,10.7851228030062));
#232820=CARTESIAN_POINT('Ctrl Pts',(-2.01766554248254,15.2,10.7894676884955));
#232821=CARTESIAN_POINT('Ctrl Pts',(-2.02021582269191,15.2,10.7938266253018));
#232822=CARTESIAN_POINT('Ctrl Pts',(-2.02327615883198,15.2,10.7990573492793));
#232823=CARTESIAN_POINT('Ctrl Pts',(-2.02636555102808,15.2,10.8043083090051));
#232824=CARTESIAN_POINT('Ctrl Pts',(-2.02948406008016,15.2,10.8095790759794));
#232825=CARTESIAN_POINT('Ctrl Pts',(-2.03208281771799,15.2,10.8139713819509));
#232826=CARTESIAN_POINT('Ctrl Pts',(-2.0347017938533,15.2,10.8183774445831));
#232827=CARTESIAN_POINT('Ctrl Pts',(-2.03734102324024,15.2,10.8227970171725));
#232828=CARTESIAN_POINT('Ctrl Pts',(-2.03945240686485,15.2,10.8263326754368));
#232829=CARTESIAN_POINT('Ctrl Pts',(-2.04157675197055,15.2,10.8298769816141));
#232830=CARTESIAN_POINT('Ctrl Pts',(-2.04371407486613,15.2,10.8334298100308));
#232831=CARTESIAN_POINT('Ctrl Pts',(-2.04638572833999,15.2,10.8378708453097));
#232832=CARTESIAN_POINT('Ctrl Pts',(-2.04907765963643,15.2,10.8423252003443));
#232833=CARTESIAN_POINT('Ctrl Pts',(-2.05178989984644,15.2,10.8467926313176));
#232834=CARTESIAN_POINT('Ctrl Pts',(-2.05395969183708,15.2,10.8503665758041));
#232835=CARTESIAN_POINT('Ctrl Pts',(-2.05614248082365,15.2,10.8539488915136));
#232836=CARTESIAN_POINT('Ctrl Pts',(-2.05833828276517,15.2,10.8575394540142));
#232837=CARTESIAN_POINT('Ctrl Pts',(-2.06053408500586,15.2,10.8611300170039));
#232838=CARTESIAN_POINT('Ctrl Pts',(-2.0627428993325,15.2,10.8647288284339));
#232839=CARTESIAN_POINT('Ctrl Pts',(-2.06496474162162,15.2,10.868335766798));
#232840=CARTESIAN_POINT('Ctrl Pts',(-2.06718658360801,15.2,10.8719427046707));
#232841=CARTESIAN_POINT('Ctrl Pts',(-2.069421452576,15.2,10.8755577711895));
#232842=CARTESIAN_POINT('Ctrl Pts',(-2.07166936255802,15.2,10.8791808450038));
#232843=CARTESIAN_POINT('Ctrl Pts',(-2.07391727284633,15.2,10.8828039193119));
#232844=CARTESIAN_POINT('Ctrl Pts',(-2.07617822524971,15.2,10.8864350012722));
#232845=CARTESIAN_POINT('Ctrl Pts',(-2.07845223232172,15.2,10.8900739718197));
#232846=CARTESIAN_POINT('Ctrl Pts',(-2.08129474100681,15.2,10.8946226847561));
#232847=CARTESIAN_POINT('Ctrl Pts',(-2.08415764804215,15.2,10.8991837253138));
#232848=CARTESIAN_POINT('Ctrl Pts',(-2.08704097908548,15.2,10.9037568613565));
#232849=CARTESIAN_POINT('Ctrl Pts',(-2.08934764373158,15.2,10.9074153698915));
#232850=CARTESIAN_POINT('Ctrl Pts',(-2.09166738111486,15.2,10.9110816208727));
#232851=CARTESIAN_POINT('Ctrl Pts',(-2.09400020053442,15.2,10.914755496683));
#232852=CARTESIAN_POINT('Ctrl Pts',(-2.09633302027183,15.2,10.9184293729939));
#232853=CARTESIAN_POINT('Ctrl Pts',(-2.09867892545317,15.2,10.9221108747576));
#232854=CARTESIAN_POINT('Ctrl Pts',(-2.10103792586738,15.2,10.925799885977));
#232855=CARTESIAN_POINT('Ctrl Pts',(-2.10339692596018,15.2,10.9294888966937));
#232856=CARTESIAN_POINT('Ctrl Pts',(-2.1057690218732,15.2,10.9331854171922));
#232857=CARTESIAN_POINT('Ctrl Pts',(-2.10815422578847,15.2,10.9368893317222));
#232858=CARTESIAN_POINT('Ctrl Pts',(-2.11053943002873,15.2,10.940593246757));
#232859=CARTESIAN_POINT('Ctrl Pts',(-2.11293774265664,15.2,10.9443045566592));
#232860=CARTESIAN_POINT('Ctrl Pts',(-2.1153491729556,15.2,10.948023147029));
#232861=CARTESIAN_POINT('Ctrl Pts',(-2.11836346066501,15.2,10.952671384738));
#232862=CARTESIAN_POINT('Ctrl Pts',(-2.12139824801735,15.2,10.9573309978692));
#232863=CARTESIAN_POINT('Ctrl Pts',(-2.12445355337975,15.2,10.9620017665755));
#232864=CARTESIAN_POINT('Ctrl Pts',(-2.12689779746986,15.2,10.9657383812351));
#232865=CARTESIAN_POINT('Ctrl Pts',(-2.12935517517598,15.2,10.9694821344755));
#232866=CARTESIAN_POINT('Ctrl Pts',(-2.1318256938065,15.2,10.9732329156684));
#232867=CARTESIAN_POINT('Ctrl Pts',(-2.13367858286354,15.2,10.9760460016909));
#232868=CARTESIAN_POINT('Ctrl Pts',(-2.13553886482839,15.2,10.978863040638));
#232869=CARTESIAN_POINT('Ctrl Pts',(-2.13740654334285,15.2,10.98168398516));
#232870=CARTESIAN_POINT('Ctrl Pts',(-2.13927422219661,15.2,10.9845049301944));
#232871=CARTESIAN_POINT('Ctrl Pts',(-2.14114929790246,15.2,10.9873297811383));
#232872=CARTESIAN_POINT('Ctrl Pts',(-2.14303177467706,15.2,10.9901584916333));
#232873=CARTESIAN_POINT('Ctrl Pts',(-2.14554174313989,15.2,10.9939301047701));
#232874=CARTESIAN_POINT('Ctrl Pts',(-2.14806486711083,15.2,10.9977085785536));
#232875=CARTESIAN_POINT('Ctrl Pts',(-2.15060115824828,15.2,11.0014938025391));
#232876=CARTESIAN_POINT('Ctrl Pts',(-2.15250337668776,15.2,11.0043327206571));
#232877=CARTESIAN_POINT('Ctrl Pts',(-2.15441300006148,15.2,11.0071754366435));
#232878=CARTESIAN_POINT('Ctrl Pts',(-2.15633003357451,15.2,11.0100219037064));
#232879=CARTESIAN_POINT('Ctrl Pts',(-2.15888607849072,15.2,11.0138171934684));
#232880=CARTESIAN_POINT('Ctrl Pts',(-2.16145529675576,15.2,11.0176191503895));
#232881=CARTESIAN_POINT('Ctrl Pts',(-2.16403769495292,15.2,11.0214276693197));
#232882=CARTESIAN_POINT('Ctrl Pts',(-2.16597449342487,15.2,11.0242840582579));
#232883=CARTESIAN_POINT('Ctrl Pts',(-2.16791870613044,15.2,11.0271441369769));
#232884=CARTESIAN_POINT('Ctrl Pts',(-2.16987033702679,15.2,11.0300078600526));
#232885=CARTESIAN_POINT('Ctrl Pts',(-2.17182196792315,15.2,11.0328715831283));
#232886=CARTESIAN_POINT('Ctrl Pts',(-2.17378101556077,15.2,11.035738950872));
#232887=CARTESIAN_POINT('Ctrl Pts',(-2.17574748453989,15.2,11.038609917989));
#232888=CARTESIAN_POINT('Ctrl Pts',(-2.17771395351902,15.2,11.0414808851061));
#232889=CARTESIAN_POINT('Ctrl Pts',(-2.17968784329013,15.2,11.0443554523412));
#232890=CARTESIAN_POINT('Ctrl Pts',(-2.18166915725917,15.2,11.0472335729446));
#232891=CARTESIAN_POINT('Ctrl Pts',(-2.18365047122821,15.2,11.0501116935481));
#232892=CARTESIAN_POINT('Ctrl Pts',(-2.1856392083884,15.2,11.052993368893));
#232893=CARTESIAN_POINT('Ctrl Pts',(-2.18763537377317,15.2,11.0558785539126));
#232894=CARTESIAN_POINT('Ctrl Pts',(-2.18963153952058,15.2,11.0587637394565));
#232895=CARTESIAN_POINT('Ctrl Pts',(-2.19163513162849,15.2,11.0616524335097));
#232896=CARTESIAN_POINT('Ctrl Pts',(-2.19364615392175,15.2,11.0645445931388));
#232897=CARTESIAN_POINT('Ctrl Pts',(-2.19565717584967,15.2,11.0674367522425));
#232898=CARTESIAN_POINT('Ctrl Pts',(-2.1976756272969,15.2,11.0703323770043));
#232899=CARTESIAN_POINT('Ctrl Pts',(-2.19970151136704,15.2,11.0732314217942));
#232900=CARTESIAN_POINT('Ctrl Pts',(-2.20240269000454,15.2,11.0770968146719));
#232901=CARTESIAN_POINT('Ctrl Pts',(-2.20511708253712,15.2,11.0809682887116));
#232902=CARTESIAN_POINT('Ctrl Pts',(-2.20784469503548,15.2,11.0848457399497));
#232903=CARTESIAN_POINT('Ctrl Pts',(-2.20989040450217,15.2,11.0877538285104));
#232904=CARTESIAN_POINT('Ctrl Pts',(-2.21194354956001,15.2,11.0906652792209));
#232905=CARTESIAN_POINT('Ctrl Pts',(-2.21400413352581,15.2,11.0935800473646));
#232906=CARTESIAN_POINT('Ctrl Pts',(-2.21675157906309,15.2,11.0974664052425));
#232907=CARTESIAN_POINT('Ctrl Pts',(-2.21951224876549,15.2,11.1013586630542));
#232908=CARTESIAN_POINT('Ctrl Pts',(-2.22228614825,15.2,11.1052567162666));
#232909=CARTESIAN_POINT('Ctrl Pts',(-2.22436657267441,15.2,11.1081802559104));
#232910=CARTESIAN_POINT('Ctrl Pts',(-2.22645443836519,15.2,11.1111070565874));
#232911=CARTESIAN_POINT('Ctrl Pts',(-2.22854974828841,15.2,11.114037073689));
#232912=CARTESIAN_POINT('Ctrl Pts',(-2.23064505821163,15.2,11.1169670907906));
#232913=CARTESIAN_POINT('Ctrl Pts',(-2.23274781101391,15.2,11.1199003238756));
#232914=CARTESIAN_POINT('Ctrl Pts',(-2.23485801104179,15.2,11.1228367316652));
#232915=CARTESIAN_POINT('Ctrl Pts',(-2.23696821106968,15.2,11.1257731394548));
#232916=CARTESIAN_POINT('Ctrl Pts',(-2.23908585736497,15.2,11.1287127216825));
#232917=CARTESIAN_POINT('Ctrl Pts',(-2.24121095078674,15.2,11.1316554347835));
#232918=CARTESIAN_POINT('Ctrl Pts',(-2.2440444089398,15.2,11.1355790526078));
#232919=CARTESIAN_POINT('Ctrl Pts',(-2.24689110731358,15.2,11.1395082366661));
#232920=CARTESIAN_POINT('Ctrl Pts',(-2.249751051525,15.2,11.1434428864916));
#232921=CARTESIAN_POINT('Ctrl Pts',(-2.25189600948873,15.2,11.1463938735927));
#232922=CARTESIAN_POINT('Ctrl Pts',(-2.2540484177605,15.2,11.1493479356187));
#232923=CARTESIAN_POINT('Ctrl Pts',(-2.2562082777647,15.2,11.1523050297194));
#232924=CARTESIAN_POINT('Ctrl Pts',(-2.25836813776891,15.2,11.15526212382));
#232925=CARTESIAN_POINT('Ctrl Pts',(-2.2605354499839,15.2,11.15822224942));
#232926=CARTESIAN_POINT('Ctrl Pts',(-2.26271021605431,15.2,11.1611853661267));
#232927=CARTESIAN_POINT('Ctrl Pts',(-2.26633482630336,15.2,11.1661238941506));
#232928=CARTESIAN_POINT('Ctrl Pts',(-2.26998014113926,15.2,11.1710707268431));
#232929=CARTESIAN_POINT('Ctrl Pts',(-2.27364616627703,15.2,11.176025671426));
#232930=CARTESIAN_POINT('Ctrl Pts',(-2.27657898654709,15.2,11.1799896273083));
#232931=CARTESIAN_POINT('Ctrl Pts',(-2.2795250626827,15.2,11.183958775333));
#232932=CARTESIAN_POINT('Ctrl Pts',(-2.28248439623372,15.2,11.1879330190499));
#232933=CARTESIAN_POINT('Ctrl Pts',(-2.28470389619538,15.2,11.1909137015668));
#232934=CARTESIAN_POINT('Ctrl Pts',(-2.28693085412303,15.2,11.1938972487643));
#232935=CARTESIAN_POINT('Ctrl Pts',(-2.28916527101038,15.2,11.1968836202944));
#232936=CARTESIAN_POINT('Ctrl Pts',(-2.29139968789772,15.2,11.1998699918244));
#232937=CARTESIAN_POINT('Ctrl Pts',(-2.29364156283617,15.2,11.2028591863924));
#232938=CARTESIAN_POINT('Ctrl Pts',(-2.29589089826463,15.2,11.2058511625056));
#232939=CARTESIAN_POINT('Ctrl Pts',(-2.29889001244167,15.2,11.2098404643522));
#232940=CARTESIAN_POINT('Ctrl Pts',(-2.30190238960067,15.2,11.213834708802));
#232941=CARTESIAN_POINT('Ctrl Pts',(-2.30492802921138,15.2,11.2178338113538));
#232942=CARTESIAN_POINT('Ctrl Pts',(-2.30719725871329,15.2,11.2208331379952));
#232943=CARTESIAN_POINT('Ctrl Pts',(-2.30947394984811,15.2,11.2238351967865));
#232944=CARTESIAN_POINT('Ctrl Pts',(-2.31175810276576,15.2,11.2268399458025));
#232945=CARTESIAN_POINT('Ctrl Pts',(-2.31404225568342,15.2,11.2298446948186));
#232946=CARTESIAN_POINT('Ctrl Pts',(-2.31633387052517,15.2,11.2328521333317));
#232947=CARTESIAN_POINT('Ctrl Pts',(-2.31863294753543,15.2,11.2358622104444));
#232948=CARTESIAN_POINT('Ctrl Pts',(-2.3209320245457,15.2,11.238872287557));
#232949=CARTESIAN_POINT('Ctrl Pts',(-2.32323856528819,15.2,11.2418850040765));
#232950=CARTESIAN_POINT('Ctrl Pts',(-2.32555256875624,15.2,11.2449003215639));
#232951=CARTESIAN_POINT('Ctrl Pts',(-2.32940924134313,15.2,11.2499258508922));
#232952=CARTESIAN_POINT('Ctrl Pts',(-2.33328664381693,15.2,11.2549585979013));
#232953=CARTESIAN_POINT('Ctrl Pts',(-2.33718477800005,15.2,11.259998549));
#232954=CARTESIAN_POINT('Ctrl Pts',(-1.76496130700006,12.2,10.22377311));
#232955=CARTESIAN_POINT('Ctrl Pts',(-1.76541543493207,12.2,10.2255010873779));
#232956=CARTESIAN_POINT('Ctrl Pts',(-1.76588926591707,12.2,10.2272829938834));
#232957=CARTESIAN_POINT('Ctrl Pts',(-1.76638321147092,12.2,10.2291177140323));
#232958=CARTESIAN_POINT('Ctrl Pts',(-1.76687953907992,12.2,10.2309612821291));
#232959=CARTESIAN_POINT('Ctrl Pts',(-1.76739616286972,12.2,10.2328581799819));
#232960=CARTESIAN_POINT('Ctrl Pts',(-1.76793345451038,12.2,10.2348073231886));
#232961=CARTESIAN_POINT('Ctrl Pts',(-1.76847074610224,12.2,10.2367564662182));
#232962=CARTESIAN_POINT('Ctrl Pts',(-1.76902870497939,12.2,10.2387578539245));
#232963=CARTESIAN_POINT('Ctrl Pts',(-1.76960768654168,12.2,10.2408104330166));
#232964=CARTESIAN_POINT('Ctrl Pts',(-1.77018666810398,12.2,10.2428630121086));
#232965=CARTESIAN_POINT('Ctrl Pts',(-1.77078667246607,12.2,10.2449667819402));
#232966=CARTESIAN_POINT('Ctrl Pts',(-1.77140804397329,12.2,10.24712072005));
#232967=CARTESIAN_POINT('Ctrl Pts',(-1.77202941553697,12.2,10.2492746583554));
#232968=CARTESIAN_POINT('Ctrl Pts',(-1.77267215276809,12.2,10.2514787598444));
#232969=CARTESIAN_POINT('Ctrl Pts',(-1.77333658730578,12.2,10.2537320332205));
#232970=CARTESIAN_POINT('Ctrl Pts',(-1.77400102178312,12.2,10.255985306392));
#232971=CARTESIAN_POINT('Ctrl Pts',(-1.77468715486446,12.2,10.2582877466256));
#232972=CARTESIAN_POINT('Ctrl Pts',(-1.77539530325867,12.2,10.260638386051));
#232973=CARTESIAN_POINT('Ctrl Pts',(-1.77610345165288,12.2,10.2629890254764));
#232974=CARTESIAN_POINT('Ctrl Pts',(-1.77683361717075,12.2,10.2653878615328));
#232975=CARTESIAN_POINT('Ctrl Pts',(-1.77758610564243,12.2,10.2678339508585));
#232976=CARTESIAN_POINT('Ctrl Pts',(-1.77833859418247,12.2,10.2702800404063));
#232977=CARTESIAN_POINT('Ctrl Pts',(-1.77911340904195,12.2,10.2727733804935));
#232978=CARTESIAN_POINT('Ctrl Pts',(-1.77991084258694,12.2,10.2753130495517));
#232979=CARTESIAN_POINT('Ctrl Pts',(-1.7807082760595,12.2,10.2778527183792));
#232980=CARTESIAN_POINT('Ctrl Pts',(-1.78152833193401,12.2,10.2804387173121));
#232981=CARTESIAN_POINT('Ctrl Pts',(-1.78237129432105,12.2,10.2830701451352));
#232982=CARTESIAN_POINT('Ctrl Pts',(-1.7832142567081,12.2,10.2857015729583));
#232983=CARTESIAN_POINT('Ctrl Pts',(-1.78408012798497,12.2,10.2883784311276));
#232984=CARTESIAN_POINT('Ctrl Pts',(-1.78496918228499,12.2,10.2910998401101));
#232985=CARTESIAN_POINT('Ctrl Pts',(-1.78585823658502,12.2,10.2938212490926));
#232986=CARTESIAN_POINT('Ctrl Pts',(-1.78677047506695,12.2,10.2965872102404));
#232987=CARTESIAN_POINT('Ctrl Pts',(-1.7877061643647,12.2,10.2993968662187));
#232988=CARTESIAN_POINT('Ctrl Pts',(-1.7887978019354,12.2,10.3026747983635));
#232989=CARTESIAN_POINT('Ctrl Pts',(-1.78992136090724,12.2,10.3060122026356));
#232990=CARTESIAN_POINT('Ctrl Pts',(-1.79107724768775,12.2,10.3094077546164));
#232991=CARTESIAN_POINT('Ctrl Pts',(-1.79223313446825,12.2,10.3128033065971));
#232992=CARTESIAN_POINT('Ctrl Pts',(-1.79342135008691,12.2,10.3162570016962));
#232993=CARTESIAN_POINT('Ctrl Pts',(-1.79464228456549,12.2,10.3197675544474));
#232994=CARTESIAN_POINT('Ctrl Pts',(-1.79568879977852,12.2,10.3227765995066));
#232995=CARTESIAN_POINT('Ctrl Pts',(-1.79675935631462,12.2,10.325827414804));
#232996=CARTESIAN_POINT('Ctrl Pts',(-1.79785418744044,12.2,10.3289192081066));
#232997=CARTESIAN_POINT('Ctrl Pts',(-1.79894901866572,12.2,10.3320110016899));
#232998=CARTESIAN_POINT('Ctrl Pts',(-1.80006812791901,12.2,10.3351437736868));
#232999=CARTESIAN_POINT('Ctrl Pts',(-1.80121174389967,12.2,10.3383167463624));
#233000=CARTESIAN_POINT('Ctrl Pts',(-1.80235535977646,12.2,10.3414897187499));
#233001=CARTESIAN_POINT('Ctrl Pts',(-1.80352348028237,12.2,10.3447028939104));
#233002=CARTESIAN_POINT('Ctrl Pts',(-1.80471633032346,12.2,10.3479555094607));
#233003=CARTESIAN_POINT('Ctrl Pts',(-1.80590918036456,12.2,10.351208125011));
#233004=CARTESIAN_POINT('Ctrl Pts',(-1.80712675935363,12.2,10.3545001845413));
#233005=CARTESIAN_POINT('Ctrl Pts',(-1.80836928039073,12.2,10.3578309400852));
#233006=CARTESIAN_POINT('Ctrl Pts',(-1.80961180142783,12.2,10.3611616956292));
#233007=CARTESIAN_POINT('Ctrl Pts',(-1.81087926574946,12.2,10.3645311508882));
#233008=CARTESIAN_POINT('Ctrl Pts',(-1.81217187961746,12.2,10.3679385744285));
#233009=CARTESIAN_POINT('Ctrl Pts',(-1.81346449360286,12.2,10.3713459982783));
#233010=CARTESIAN_POINT('Ctrl Pts',(-1.81478225641568,12.2,10.3747913937401));
#233011=CARTESIAN_POINT('Ctrl Pts',(-1.81612537032332,12.2,10.3782740446815));
#233012=CARTESIAN_POINT('Ctrl Pts',(-1.81746848410895,12.2,10.3817566953066));
#233013=CARTESIAN_POINT('Ctrl Pts',(-1.81883694824376,12.2,10.3852766023865));
#233014=CARTESIAN_POINT('Ctrl Pts',(-1.82023095503271,12.2,10.3888330670233));
#233015=CARTESIAN_POINT('Ctrl Pts',(-1.82162496182165,12.2,10.3923895316601));
#233016=CARTESIAN_POINT('Ctrl Pts',(-1.8230445125134,12.2,10.3959825521803));
#233017=CARTESIAN_POINT('Ctrl Pts',(-1.82448979329248,12.2,10.3996114457961));
#233018=CARTESIAN_POINT('Ctrl Pts',(-1.82593507420284,12.2,10.4032403397414));
#233019=CARTESIAN_POINT('Ctrl Pts',(-1.82740608602869,12.2,10.4069051052444));
#233020=CARTESIAN_POINT('Ctrl Pts',(-1.82890300710321,12.2,10.4106050695496));
#233021=CARTESIAN_POINT('Ctrl Pts',(-1.83015044126398,12.2,10.4136883729692));
#233022=CARTESIAN_POINT('Ctrl Pts',(-1.83141587118312,12.2,10.4167961221577));
#233023=CARTESIAN_POINT('Ctrl Pts',(-1.83269939368457,12.2,10.4199279321596));
#233024=CARTESIAN_POINT('Ctrl Pts',(-1.83398291618601,12.2,10.4230597421614));
#233025=CARTESIAN_POINT('Ctrl Pts',(-1.83528453451561,12.2,10.4262156139472));
#233026=CARTESIAN_POINT('Ctrl Pts',(-1.83660434590599,12.2,10.4293951714492));
#233027=CARTESIAN_POINT('Ctrl Pts',(-1.83792415715251,12.2,10.4325747286046));
#233028=CARTESIAN_POINT('Ctrl Pts',(-1.83926216110527,12.2,10.4357779724537));
#233029=CARTESIAN_POINT('Ctrl Pts',(-1.84061845408095,12.2,10.4390045311279));
#233030=CARTESIAN_POINT('Ctrl Pts',(-1.84197474720446,12.2,10.4422310901538));
#233031=CARTESIAN_POINT('Ctrl Pts',(-1.84334932745266,12.2,10.4454809633182));
#233032=CARTESIAN_POINT('Ctrl Pts',(-1.84474229203447,12.2,10.4487537867885));
#233033=CARTESIAN_POINT('Ctrl Pts',(-1.84613525661629,12.2,10.4520266102588));
#233034=CARTESIAN_POINT('Ctrl Pts',(-1.8475466010084,12.2,10.4553223855673));
#233035=CARTESIAN_POINT('Ctrl Pts',(-1.84897641830076,12.2,10.4586407501065));
#233036=CARTESIAN_POINT('Ctrl Pts',(-1.85069219914511,12.2,10.4626227877705));
#233037=CARTESIAN_POINT('Ctrl Pts',(-1.85243457977794,12.2,10.466637356885));
#233038=CARTESIAN_POINT('Ctrl Pts',(-1.85420371070952,12.2,10.470683844441));
#233039=CARTESIAN_POINT('Ctrl Pts',(-1.85567798640548,12.2,10.4740559172206));
#233040=CARTESIAN_POINT('Ctrl Pts',(-1.85717084019619,12.2,10.4774501577616));
#233041=CARTESIAN_POINT('Ctrl Pts',(-1.85868235415605,12.2,10.4808662154718));
#233042=CARTESIAN_POINT('Ctrl Pts',(-1.86019386795117,12.2,10.4842822728095));
#233043=CARTESIAN_POINT('Ctrl Pts',(-1.86172404345668,12.2,10.4877201488652));
#233044=CARTESIAN_POINT('Ctrl Pts',(-1.86327296377242,12.2,10.4911795010558));
#233045=CARTESIAN_POINT('Ctrl Pts',(-1.86482188425699,12.2,10.4946388536235));
#233046=CARTESIAN_POINT('Ctrl Pts',(-1.86638954814405,12.2,10.4981196810547));
#233047=CARTESIAN_POINT('Ctrl Pts',(-1.86797603605917,12.2,10.5016216455669));
#233048=CARTESIAN_POINT('Ctrl Pts',(-1.86956252397429,12.2,10.505123610079));
#233049=CARTESIAN_POINT('Ctrl Pts',(-1.87116783398727,12.2,10.5086467122575));
#233050=CARTESIAN_POINT('Ctrl Pts',(-1.87279204705319,12.2,10.5121906186136));
#233051=CARTESIAN_POINT('Ctrl Pts',(-1.87441626011912,12.2,10.5157345249697));
#233052=CARTESIAN_POINT('Ctrl Pts',(-1.87605937489797,12.2,10.5192992351444));
#233053=CARTESIAN_POINT('Ctrl Pts',(-1.87772146538309,12.2,10.5228844204906));
#233054=CARTESIAN_POINT('Ctrl Pts',(-1.87938355586821,12.2,10.5264696058367));
#233055=CARTESIAN_POINT('Ctrl Pts',(-1.8810646226677,12.2,10.5300752665917));
#233056=CARTESIAN_POINT('Ctrl Pts',(-1.88276473988894,12.2,10.5337010777713));
#233057=CARTESIAN_POINT('Ctrl Pts',(-1.88446485711018,12.2,10.5373268889508));
#233058=CARTESIAN_POINT('Ctrl Pts',(-1.88618402469853,12.2,10.5409728519169));
#233059=CARTESIAN_POINT('Ctrl Pts',(-1.88792231191978,12.2,10.544638645527));
#233060=CARTESIAN_POINT('Ctrl Pts',(-1.88966059914102,12.2,10.5483044391371));
#233061=CARTESIAN_POINT('Ctrl Pts',(-1.89141800780214,12.2,10.5519900629089));
#233062=CARTESIAN_POINT('Ctrl Pts',(-1.89319460649071,12.2,10.5556952024396));
#233063=CARTESIAN_POINT('Ctrl Pts',(-1.89497120517928,12.2,10.5594003419703));
#233064=CARTESIAN_POINT('Ctrl Pts',(-1.89676699360556,12.2,10.5631249979611));
#233065=CARTESIAN_POINT('Ctrl Pts',(-1.89858203825834,12.2,10.5668688560166));
#233066=CARTESIAN_POINT('Ctrl Pts',(-1.9000340740597,12.2,10.5698639426243));
#233067=CARTESIAN_POINT('Ctrl Pts',(-1.90149843394584,12.2,10.5728713194945));
#233068=CARTESIAN_POINT('Ctrl Pts',(-1.90297515108312,12.2,10.5758908299936));
#233069=CARTESIAN_POINT('Ctrl Pts',(-1.90445186801919,12.2,10.5789103400813));
#233070=CARTESIAN_POINT('Ctrl Pts',(-1.90594094191218,12.2,10.5819419825496));
#233071=CARTESIAN_POINT('Ctrl Pts',(-1.90744240674066,12.2,10.5849856019812));
#233072=CARTESIAN_POINT('Ctrl Pts',(-1.90894387177371,12.2,10.5880292218275));
#233073=CARTESIAN_POINT('Ctrl Pts',(-1.91045772694566,12.2,10.5910848193081));
#233074=CARTESIAN_POINT('Ctrl Pts',(-1.9119840033079,12.2,10.5941522379765));
#233075=CARTESIAN_POINT('Ctrl Pts',(-1.91351027946217,12.2,10.5972196562269));
#233076=CARTESIAN_POINT('Ctrl Pts',(-1.91504897688702,12.2,10.6002988976035));
#233077=CARTESIAN_POINT('Ctrl Pts',(-1.91660012714832,12.2,10.603389807739));
#233078=CARTESIAN_POINT('Ctrl Pts',(-1.91815127762096,12.2,10.6064807182957));
#233079=CARTESIAN_POINT('Ctrl Pts',(-1.91971488142971,12.2,10.6095832976644));
#233080=CARTESIAN_POINT('Ctrl Pts',(-1.92129096726211,12.2,10.6126973964352));
#233081=CARTESIAN_POINT('Ctrl Pts',(-1.92286705287978,12.2,10.6158114947817));
#233082=CARTESIAN_POINT('Ctrl Pts',(-1.9244556212815,12.2,10.6189371113063));
#233083=CARTESIAN_POINT('Ctrl Pts',(-1.92605670209424,12.2,10.6220740954936));
#233084=CARTESIAN_POINT('Ctrl Pts',(-1.92765778312512,12.2,10.6252110801083));
#233085=CARTESIAN_POINT('Ctrl Pts',(-1.92927137668249,12.2,10.6283594320215));
#233086=CARTESIAN_POINT('Ctrl Pts',(-1.93089750988305,12.2,10.63151900525));
#233087=CARTESIAN_POINT('Ctrl Pts',(-1.93252364286205,12.2,10.634678578048));
#233088=CARTESIAN_POINT('Ctrl Pts',(-1.93416231850852,12.2,10.6378493704821));
#233089=CARTESIAN_POINT('Ctrl Pts',(-1.93581356201047,12.2,10.6410312355466));
#233090=CARTESIAN_POINT('Ctrl Pts',(-1.93829042760087,12.2,10.6458040337937));
#233091=CARTESIAN_POINT('Ctrl Pts',(-1.94079557203615,12.2,10.6506017454861));
#233092=CARTESIAN_POINT('Ctrl Pts',(-1.9433290895095,12.2,10.6554238815006));
#233093=CARTESIAN_POINT('Ctrl Pts',(-1.94501810092827,12.2,10.6586386384055));
#233094=CARTESIAN_POINT('Ctrl Pts',(-1.94671972068151,12.2,10.6618642508535));
#233095=CARTESIAN_POINT('Ctrl Pts',(-1.94843397681832,12.2,10.6651005749771));
#233096=CARTESIAN_POINT('Ctrl Pts',(-1.95014823318869,12.2,10.6683368995417));
#233097=CARTESIAN_POINT('Ctrl Pts',(-1.95187512535022,12.2,10.6715839345065));
#233098=CARTESIAN_POINT('Ctrl Pts',(-1.9536146784775,12.2,10.674841540681));
#233099=CARTESIAN_POINT('Ctrl Pts',(-1.95535423136776,12.2,10.6780991464118));
#233100=CARTESIAN_POINT('Ctrl Pts',(-1.95710644619818,12.2,10.6813673210785));
#233101=CARTESIAN_POINT('Ctrl Pts',(-1.95887134633085,12.2,10.6846459246987));
#233102=CARTESIAN_POINT('Ctrl Pts',(-1.96107747167705,12.2,10.688744179559));
#233103=CARTESIAN_POINT('Ctrl Pts',(-1.96330341898762,12.2,10.6928587300085));
#233104=CARTESIAN_POINT('Ctrl Pts',(-1.96554923586158,12.2,10.6969893024382));
#233105=CARTESIAN_POINT('Ctrl Pts',(-1.96734588945867,12.2,10.7002937605621));
#233106=CARTESIAN_POINT('Ctrl Pts',(-1.96915525932304,12.2,10.7036084741259));
#233107=CARTESIAN_POINT('Ctrl Pts',(-1.97097736851447,12.2,10.7069333049741));
#233108=CARTESIAN_POINT('Ctrl Pts',(-1.97279947745765,12.2,10.7102581353693));
#233109=CARTESIAN_POINT('Ctrl Pts',(-1.97463432522597,12.2,10.7135930801896));
#233110=CARTESIAN_POINT('Ctrl Pts',(-1.97648193657408,12.2,10.7169380076933));
#233111=CARTESIAN_POINT('Ctrl Pts',(-1.97832954817392,12.2,10.7202829356526));
#233112=CARTESIAN_POINT('Ctrl Pts',(-1.98018992160868,12.2,10.7236378431383));
#233113=CARTESIAN_POINT('Ctrl Pts',(-1.98206307987825,12.2,10.7270025952668));
#233114=CARTESIAN_POINT('Ctrl Pts',(-1.98393623789261,12.2,10.7303673469368));
#233115=CARTESIAN_POINT('Ctrl Pts',(-1.9858221802277,12.2,10.7337419437146));
#233116=CARTESIAN_POINT('Ctrl Pts',(-1.98772092899955,12.2,10.7371262515506));
#233117=CARTESIAN_POINT('Ctrl Pts',(-1.98961967803012,12.2,10.7405105598477));
#233118=CARTESIAN_POINT('Ctrl Pts',(-1.99153123199617,12.2,10.7439045773672));
#233119=CARTESIAN_POINT('Ctrl Pts',(-1.99345561365745,12.2,10.7473081740533));
#233120=CARTESIAN_POINT('Ctrl Pts',(-1.99537999505653,12.2,10.7507117702757));
#233121=CARTESIAN_POINT('Ctrl Pts',(-1.99731720448912,12.2,10.754124943285));
#233122=CARTESIAN_POINT('Ctrl Pts',(-1.99926725993951,12.2,10.7575475629487));
#233123=CARTESIAN_POINT('Ctrl Pts',(-2.00121731565559,12.2,10.7609701830787));
#233124=CARTESIAN_POINT('Ctrl Pts',(-2.0031802188652,12.2,10.7644022489491));
#233125=CARTESIAN_POINT('Ctrl Pts',(-2.00515598925969,12.2,10.767843629819));
#233126=CARTESIAN_POINT('Ctrl Pts',(-2.00713175938499,12.2,10.77128501022));
#233127=CARTESIAN_POINT('Ctrl Pts',(-2.00912039674324,12.2,10.7747357063541));
#233128=CARTESIAN_POINT('Ctrl Pts',(-2.01112192068943,12.2,10.7781955874593));
#233129=CARTESIAN_POINT('Ctrl Pts',(-2.01312344490833,12.2,10.7816554690358));
#233130=CARTESIAN_POINT('Ctrl Pts',(-2.01513785459787,12.2,10.785124536441));
#233131=CARTESIAN_POINT('Ctrl Pts',(-2.01716516954166,12.2,10.7886026612416));
#233132=CARTESIAN_POINT('Ctrl Pts',(-2.01919248448546,12.2,10.7920807860422));
#233133=CARTESIAN_POINT('Ctrl Pts',(-2.0212327038975,12.2,10.7955679675079));
#233134=CARTESIAN_POINT('Ctrl Pts',(-2.02328584684403,12.2,10.7990640795882));
#233135=CARTESIAN_POINT('Ctrl Pts',(-2.02533898951083,12.2,10.8025601911922));
#233136=CARTESIAN_POINT('Ctrl Pts',(-2.02740505413986,12.2,10.8060652314895));
#233137=CARTESIAN_POINT('Ctrl Pts',(-2.02948406008016,12.2,10.8095790759794));
#233138=CARTESIAN_POINT('Ctrl Pts',(-2.03156306630373,12.2,10.8130929209481));
#233139=CARTESIAN_POINT('Ctrl Pts',(-2.03365501234282,12.2,10.8166155704955));
#233140=CARTESIAN_POINT('Ctrl Pts',(-2.03575991606385,12.2,10.8201468975874));
#233141=CARTESIAN_POINT('Ctrl Pts',(-2.03786481949808,12.2,10.8236782241982));
#233142=CARTESIAN_POINT('Ctrl Pts',(-2.03998268064264,12.2,10.8272182290006));
#233143=CARTESIAN_POINT('Ctrl Pts',(-2.04211351530094,12.2,10.8307667880433));
#233144=CARTESIAN_POINT('Ctrl Pts',(-2.04424435024956,12.2,10.8343153475695));
#233145=CARTESIAN_POINT('Ctrl Pts',(-2.04638815826361,12.2,10.8378724610828));
#233146=CARTESIAN_POINT('Ctrl Pts',(-2.04854495715978,12.2,10.8414380059998));
#233147=CARTESIAN_POINT('Ctrl Pts',(-2.05070175576209,12.2,10.8450035504311));
#233148=CARTESIAN_POINT('Ctrl Pts',(-2.05287154411498,12.2,10.8485775250976));
#233149=CARTESIAN_POINT('Ctrl Pts',(-2.05505433693334,12.2,10.8521598097052));
#233150=CARTESIAN_POINT('Ctrl Pts',(-2.05723713004911,12.2,10.8557420948009));
#233151=CARTESIAN_POINT('Ctrl Pts',(-2.05943292863447,12.2,10.8593326877781));
#233152=CARTESIAN_POINT('Ctrl Pts',(-2.06164174692237,12.2,10.8629314692526));
#233153=CARTESIAN_POINT('Ctrl Pts',(-2.06385056490931,12.2,10.8665302502367));
#233154=CARTESIAN_POINT('Ctrl Pts',(-2.06607240380753,12.2,10.8701372180303));
#233155=CARTESIAN_POINT('Ctrl Pts',(-2.06830727640128,12.2,10.8737522539006));
#233156=CARTESIAN_POINT('Ctrl Pts',(-2.07054214929953,12.2,10.8773672902634));
#233157=CARTESIAN_POINT('Ctrl Pts',(-2.07279005567357,12.2,10.8809903947575));
#233158=CARTESIAN_POINT('Ctrl Pts',(-2.07505101125155,12.2,10.8846214470274));
#233159=CARTESIAN_POINT('Ctrl Pts',(-2.07787720556999,12.2,10.8891602621175));
#233160=CARTESIAN_POINT('Ctrl Pts',(-2.08072378741435,12.2,10.893711495909));
#233161=CARTESIAN_POINT('Ctrl Pts',(-2.08359078338763,12.2,10.8982749185485));
#233162=CARTESIAN_POINT('Ctrl Pts',(-2.08588437997875,12.2,10.9019256563616));
#233163=CARTESIAN_POINT('Ctrl Pts',(-2.0881910411978,12.2,10.9055841939038));
#233164=CARTESIAN_POINT('Ctrl Pts',(-2.0905107810624,12.2,10.9092504156589));
#233165=CARTESIAN_POINT('Ctrl Pts',(-2.09283052124306,12.2,10.9129166379135));
#233166=CARTESIAN_POINT('Ctrl Pts',(-2.09516333766861,12.2,10.9165905427712));
#233167=CARTESIAN_POINT('Ctrl Pts',(-2.09750924525161,12.2,10.9202720157108));
#233168=CARTESIAN_POINT('Ctrl Pts',(-2.09985515251497,12.2,10.9239534881488));
#233169=CARTESIAN_POINT('Ctrl Pts',(-2.10221414967688,12.2,10.9276425278763));
#233170=CARTESIAN_POINT('Ctrl Pts',(-2.1045862488705,12.2,10.9313390191289));
#233171=CARTESIAN_POINT('Ctrl Pts',(-2.10695834838733,12.2,10.9350355108852));
#233172=CARTESIAN_POINT('Ctrl Pts',(-2.10934354957487,12.2,10.9387394544005));
#233173=CARTESIAN_POINT('Ctrl Pts',(-2.11174186448333,12.2,10.9424507359916));
#233174=CARTESIAN_POINT('Ctrl Pts',(-2.11414017939179,12.2,10.9461620175827));
#233175=CARTESIAN_POINT('Ctrl Pts',(-2.11655160631296,12.2,10.9498806364804));
#233176=CARTESIAN_POINT('Ctrl Pts',(-2.11897615911309,12.2,10.9536064788508));
#233177=CARTESIAN_POINT('Ctrl Pts',(-2.12079457354802,12.2,10.9564008603748));
#233178=CARTESIAN_POINT('Ctrl Pts',(-2.12262037022891,12.2,10.9591993054536));
#233179=CARTESIAN_POINT('Ctrl Pts',(-2.12445355337975,12.2,10.9620017665755));
#233180=CARTESIAN_POINT('Ctrl Pts',(-2.12689779746986,12.2,10.9657383812351));
#233181=CARTESIAN_POINT('Ctrl Pts',(-2.12935517517598,12.2,10.9694821344755));
#233182=CARTESIAN_POINT('Ctrl Pts',(-2.1318256938065,12.2,10.9732329156684));
#233183=CARTESIAN_POINT('Ctrl Pts',(-2.13367858286354,12.2,10.9760460016909));
#233184=CARTESIAN_POINT('Ctrl Pts',(-2.13553886482839,12.2,10.978863040638));
#233185=CARTESIAN_POINT('Ctrl Pts',(-2.13740654334285,12.2,10.98168398516));
#233186=CARTESIAN_POINT('Ctrl Pts',(-2.13927422219661,12.2,10.9845049301944));
#233187=CARTESIAN_POINT('Ctrl Pts',(-2.14114929790246,12.2,10.9873297811383));
#233188=CARTESIAN_POINT('Ctrl Pts',(-2.14303177467706,12.2,10.9901584916333));
#233189=CARTESIAN_POINT('Ctrl Pts',(-2.14554174313989,12.2,10.9939301047701));
#233190=CARTESIAN_POINT('Ctrl Pts',(-2.14806486711083,12.2,10.9977085785536));
#233191=CARTESIAN_POINT('Ctrl Pts',(-2.15060115824828,12.2,11.0014938025391));
#233192=CARTESIAN_POINT('Ctrl Pts',(-2.15250337668776,12.2,11.0043327206571));
#233193=CARTESIAN_POINT('Ctrl Pts',(-2.15441300006148,12.2,11.0071754366435));
#233194=CARTESIAN_POINT('Ctrl Pts',(-2.1563300335745,12.2,11.0100219037064));
#233195=CARTESIAN_POINT('Ctrl Pts',(-2.15824706708753,12.2,11.0128683707693));
#233196=CARTESIAN_POINT('Ctrl Pts',(-2.16017151101673,12.2,11.015718588232));
#233197=CARTESIAN_POINT('Ctrl Pts',(-2.16210336707053,12.2,11.0185725113361));
#233198=CARTESIAN_POINT('Ctrl Pts',(-2.16403522347529,12.2,11.0214264349587));
#233199=CARTESIAN_POINT('Ctrl Pts',(-2.16597449255711,12.2,11.0242840647907));
#233200=CARTESIAN_POINT('Ctrl Pts',(-2.16792117888273,12.2,11.0271453538321));
#233201=CARTESIAN_POINT('Ctrl Pts',(-2.16986786485471,12.2,11.0300066423537));
#233202=CARTESIAN_POINT('Ctrl Pts',(-2.17182196726869,12.2,11.0328715901655));
#233203=CARTESIAN_POINT('Ctrl Pts',(-2.17378348933792,12.2,11.03574015283));
#233204=CARTESIAN_POINT('Ctrl Pts',(-2.17639885197811,12.2,11.0395649028756));
#233205=CARTESIAN_POINT('Ctrl Pts',(-2.17902740542042,12.2,11.043396078981));
#233206=CARTESIAN_POINT('Ctrl Pts',(-2.18166915725917,12.2,11.0472335729446));
#233207=CARTESIAN_POINT('Ctrl Pts',(-2.18365047122821,12.2,11.0501116935481));
#233208=CARTESIAN_POINT('Ctrl Pts',(-2.18563920838841,12.2,11.052993368893));
#233209=CARTESIAN_POINT('Ctrl Pts',(-2.18763537377318,12.2,11.0558785539127));
#233210=CARTESIAN_POINT('Ctrl Pts',(-2.18963153952059,12.2,11.0587637394565));
#233211=CARTESIAN_POINT('Ctrl Pts',(-2.19163513162849,12.2,11.0616524335097));
#233212=CARTESIAN_POINT('Ctrl Pts',(-2.19364615392175,12.2,11.0645445931388));
#233213=CARTESIAN_POINT('Ctrl Pts',(-2.19565717584967,12.2,11.0674367522425));
#233214=CARTESIAN_POINT('Ctrl Pts',(-2.1976756272969,12.2,11.0703323770043));
#233215=CARTESIAN_POINT('Ctrl Pts',(-2.19970151136704,12.2,11.0732314217942));
#233216=CARTESIAN_POINT('Ctrl Pts',(-2.20240269000454,12.2,11.0770968146719));
#233217=CARTESIAN_POINT('Ctrl Pts',(-2.20511708253712,12.2,11.0809682887116));
#233218=CARTESIAN_POINT('Ctrl Pts',(-2.20784469503548,12.2,11.0848457399497));
#233219=CARTESIAN_POINT('Ctrl Pts',(-2.20989040450216,12.2,11.0877538285104));
#233220=CARTESIAN_POINT('Ctrl Pts',(-2.21194354956001,12.2,11.0906652792209));
#233221=CARTESIAN_POINT('Ctrl Pts',(-2.21400413352581,12.2,11.0935800473646));
#233222=CARTESIAN_POINT('Ctrl Pts',(-2.21606471786595,12.2,11.0964948160377));
#233223=CARTESIAN_POINT('Ctrl Pts',(-2.21813274084982,12.2,11.0994129032952));
#233224=CARTESIAN_POINT('Ctrl Pts',(-2.22020820469413,12.2,11.1023342653868));
#233225=CARTESIAN_POINT('Ctrl Pts',(-2.22228366816139,12.2,11.1052556269478));
#233226=CARTESIAN_POINT('Ctrl Pts',(-2.2243665724866,12.2,11.1081802628086));
#233227=CARTESIAN_POINT('Ctrl Pts',(-2.22645691995298,12.2,11.1111081308275));
#233228=CARTESIAN_POINT('Ctrl Pts',(-2.22854726741935,12.2,11.1140359988464));
#233229=CARTESIAN_POINT('Ctrl Pts',(-2.23064505821883,12.2,11.1169670976126));
#233230=CARTESIAN_POINT('Ctrl Pts',(-2.23275029377692,12.2,11.1199013842693));
#233231=CARTESIAN_POINT('Ctrl Pts',(-2.23555727439356,12.2,11.1238137663006));
#233232=CARTESIAN_POINT('Ctrl Pts',(-2.23837749301974,12.2,11.1277318174937));
#233233=CARTESIAN_POINT('Ctrl Pts',(-2.24121095078674,12.2,11.1316554347835));
#233234=CARTESIAN_POINT('Ctrl Pts',(-2.24333604459456,12.2,11.134598148419));
#233235=CARTESIAN_POINT('Ctrl Pts',(-2.24546858543782,12.2,11.1375439932638));
#233236=CARTESIAN_POINT('Ctrl Pts',(-2.2476085772082,12.2,11.1404929264012));
#233237=CARTESIAN_POINT('Ctrl Pts',(-2.25046189892076,12.2,11.1444248363581));
#233238=CARTESIAN_POINT('Ctrl Pts',(-2.25332846455655,12.2,11.1483622377643));
#233239=CARTESIAN_POINT('Ctrl Pts',(-2.25620827776471,12.2,11.1523050297194));
#233240=CARTESIAN_POINT('Ctrl Pts',(-2.25836813776891,12.2,11.15526212382));
#233241=CARTESIAN_POINT('Ctrl Pts',(-2.2605354499839,12.2,11.15822224942));
#233242=CARTESIAN_POINT('Ctrl Pts',(-2.26271021605431,12.2,11.1611853661267));
#233243=CARTESIAN_POINT('Ctrl Pts',(-2.26488498212472,12.2,11.1641484828334));
#233244=CARTESIAN_POINT('Ctrl Pts',(-2.26706720178658,12.2,11.167114589061));
#233245=CARTESIAN_POINT('Ctrl Pts',(-2.26925687624766,12.2,11.1700836436194));
#233246=CARTESIAN_POINT('Ctrl Pts',(-2.27144655110652,12.2,11.1730526987171));
#233247=CARTESIAN_POINT('Ctrl Pts',(-2.27364368109253,12.2,11.1760247014658));
#233248=CARTESIAN_POINT('Ctrl Pts',(-2.27584826745561,12.2,11.1789996111485));
#233249=CARTESIAN_POINT('Ctrl Pts',(-2.27805285341819,12.2,11.1819745202908));
#233250=CARTESIAN_POINT('Ctrl Pts',(-2.28026489627206,12.2,11.184952336533));
#233251=CARTESIAN_POINT('Ctrl Pts',(-2.28248439623372,12.2,11.1879330190499));
#233252=CARTESIAN_POINT('Ctrl Pts',(-2.28470389619538,12.2,11.1909137015668));
#233253=CARTESIAN_POINT('Ctrl Pts',(-2.28693085412303,12.2,11.1938972487643));
#233254=CARTESIAN_POINT('Ctrl Pts',(-2.28916527101038,12.2,11.1968836202944));
#233255=CARTESIAN_POINT('Ctrl Pts',(-2.29139968789772,12.2,11.1998699918244));
#233256=CARTESIAN_POINT('Ctrl Pts',(-2.29364156283617,12.2,11.2028591863924));
#233257=CARTESIAN_POINT('Ctrl Pts',(-2.29589089826463,12.2,11.2058511625056));
#233258=CARTESIAN_POINT('Ctrl Pts',(-2.2981402336931,12.2,11.2088431386188));
#233259=CARTESIAN_POINT('Ctrl Pts',(-2.30039702983625,12.2,11.2118378951825));
#233260=CARTESIAN_POINT('Ctrl Pts',(-2.30266128579499,12.2,11.2148353959483));
#233261=CARTESIAN_POINT('Ctrl Pts',(-2.30492554175372,12.2,11.2178328967141));
#233262=CARTESIAN_POINT('Ctrl Pts',(-2.3071972578203,12.2,11.2208331434048));
#233263=CARTESIAN_POINT('Ctrl Pts',(-2.30947643623649,12.2,11.223836094087));
#233264=CARTESIAN_POINT('Ctrl Pts',(-2.31175561506672,12.2,11.2268390453147));
#233265=CARTESIAN_POINT('Ctrl Pts',(-2.31404225544904,12.2,11.2298447031182));
#233266=CARTESIAN_POINT('Ctrl Pts',(-2.31633635824179,12.2,11.2328530157224));
#233267=CARTESIAN_POINT('Ctrl Pts',(-2.31939516127085,12.2,11.2368640982839));
#233268=CARTESIAN_POINT('Ctrl Pts',(-2.32246723093896,12.2,11.2408798984299));
#233269=CARTESIAN_POINT('Ctrl Pts',(-2.32555256875624,12.2,11.2449003215639));
#233270=CARTESIAN_POINT('Ctrl Pts',(-2.32940924134313,12.2,11.2499258508922));
#233271=CARTESIAN_POINT('Ctrl Pts',(-2.33328664381693,12.2,11.2549585979013));
#233272=CARTESIAN_POINT('Ctrl Pts',(-2.33718477800005,12.2,11.259998549));
#233273=CARTESIAN_POINT('Origin',(-5.66257110645729E-14,15.2,-1.77635683940025E-14));
#233274=CARTESIAN_POINT('',(-3.20199116200006,15.2,9.86852965799999));
#233275=CARTESIAN_POINT('',(-3.20199116200006,12.2,9.86852965799999));
#233276=CARTESIAN_POINT('',(-3.20199116200006,15.2,9.86852965799999));
#233277=CARTESIAN_POINT('Origin',(-5.66257110645729E-14,12.2,-1.77635683940025E-14));
#233278=CARTESIAN_POINT('Origin',(-5.66257110645729E-14,15.2,-1.77635683940025E-14));
#233279=CARTESIAN_POINT('Origin',(-5.66257110645729E-14,15.2,-1.77635683940025E-14));
#233280=CARTESIAN_POINT('',(-3.91586047956408,15.2,10.8127719253567));
#233281=CARTESIAN_POINT('',(-4.27433547000006,15.2,10.676144262));
#233282=CARTESIAN_POINT('Origin',(-5.66257110645729E-14,15.2,-1.77635683940025E-14));
#233283=CARTESIAN_POINT('',(-4.27433547000006,12.2,10.676144262));
#233284=CARTESIAN_POINT('',(-4.27433547000006,15.2,10.676144262));
#233285=CARTESIAN_POINT('',(-3.91586047956408,12.2,10.8127719253567));
#233286=CARTESIAN_POINT('Origin',(-5.66257110645729E-14,12.2,-1.77635683940025E-14));
#233287=CARTESIAN_POINT('',(-3.91586048000006,15.2,10.812771926));
#233288=CARTESIAN_POINT('Ctrl Pts',(-3.20199116200006,15.2,9.86852965799999));
#233289=CARTESIAN_POINT('Ctrl Pts',(-3.20199116200006,11.6,9.86852965799999));
#233290=CARTESIAN_POINT('Ctrl Pts',(-3.20205902800006,15.2,9.86869026699999));
#233291=CARTESIAN_POINT('Ctrl Pts',(-3.20205902800006,11.6,9.86869026699999));
#233292=CARTESIAN_POINT('Ctrl Pts',(-3.20219720700006,15.2,9.86901705999998));
#233293=CARTESIAN_POINT('Ctrl Pts',(-3.20219720700006,11.6,9.86901705999998));
#233294=CARTESIAN_POINT('Ctrl Pts',(-3.20240682500006,15.2,9.86951212499999));
#233295=CARTESIAN_POINT('Ctrl Pts',(-3.20240682500006,11.6,9.86951212499999));
#233296=CARTESIAN_POINT('Ctrl Pts',(-3.20268969700006,15.2,9.87017881299998));
#233297=CARTESIAN_POINT('Ctrl Pts',(-3.20268969700006,11.6,9.87017881299998));
#233298=CARTESIAN_POINT('Ctrl Pts',(-3.20304833100006,15.2,9.87102171699998));
#233299=CARTESIAN_POINT('Ctrl Pts',(-3.20304833100006,11.6,9.87102171699998));
#233300=CARTESIAN_POINT('Ctrl Pts',(-3.20341363700006,15.2,9.87187791599998));
#233301=CARTESIAN_POINT('Ctrl Pts',(-3.20341363700006,11.6,9.87187791599998));
#233302=CARTESIAN_POINT('Ctrl Pts',(-3.20378354400006,15.2,9.87274249599999));
#233303=CARTESIAN_POINT('Ctrl Pts',(-3.20378354400006,11.6,9.87274249599999));
#233304=CARTESIAN_POINT('Ctrl Pts',(-3.20415805700006,15.2,9.87361542499999));
#233305=CARTESIAN_POINT('Ctrl Pts',(-3.20415805700006,11.6,9.87361542499999));
#233306=CARTESIAN_POINT('Ctrl Pts',(-3.20453718500006,15.2,9.87449666999998));
#233307=CARTESIAN_POINT('Ctrl Pts',(-3.20453718500006,11.6,9.87449666999998));
#233308=CARTESIAN_POINT('Ctrl Pts',(-3.20492093100006,15.2,9.87538620099999));
#233309=CARTESIAN_POINT('Ctrl Pts',(-3.20492093100006,11.6,9.87538620099999));
#233310=CARTESIAN_POINT('Ctrl Pts',(-3.20530930300006,15.2,9.87628398499999));
#233311=CARTESIAN_POINT('Ctrl Pts',(-3.20530930300006,11.6,9.87628398499999));
#233312=CARTESIAN_POINT('Ctrl Pts',(-3.20570230600006,15.2,9.87718999099998));
#233313=CARTESIAN_POINT('Ctrl Pts',(-3.20570230600006,11.6,9.87718999099998));
#233314=CARTESIAN_POINT('Ctrl Pts',(-3.20609994600006,15.2,9.87810418899999));
#233315=CARTESIAN_POINT('Ctrl Pts',(-3.20609994600006,11.6,9.87810418899999));
#233316=CARTESIAN_POINT('Ctrl Pts',(-3.20650222800006,15.2,9.87902654599999));
#233317=CARTESIAN_POINT('Ctrl Pts',(-3.20650222800006,11.6,9.87902654599999));
#233318=CARTESIAN_POINT('Ctrl Pts',(-3.20690915900005,15.2,9.87995703299998));
#233319=CARTESIAN_POINT('Ctrl Pts',(-3.20690915900005,11.6,9.87995703299998));
#233320=CARTESIAN_POINT('Ctrl Pts',(-3.20732074500006,15.2,9.88089561799999));
#233321=CARTESIAN_POINT('Ctrl Pts',(-3.20732074500006,11.6,9.88089561799999));
#233322=CARTESIAN_POINT('Ctrl Pts',(-3.20773698900005,15.2,9.88184226999999));
#233323=CARTESIAN_POINT('Ctrl Pts',(-3.20773698900005,11.6,9.88184226999999));
#233324=CARTESIAN_POINT('Ctrl Pts',(-3.20815790100006,15.2,9.88279695899998));
#233325=CARTESIAN_POINT('Ctrl Pts',(-3.20815790100006,11.6,9.88279695899998));
#233326=CARTESIAN_POINT('Ctrl Pts',(-3.20858348200006,15.2,9.88375965699999));
#233327=CARTESIAN_POINT('Ctrl Pts',(-3.20858348200006,11.6,9.88375965699999));
#233328=CARTESIAN_POINT('Ctrl Pts',(-3.20901374100006,15.2,9.88473032999998));
#233329=CARTESIAN_POINT('Ctrl Pts',(-3.20901374100006,11.6,9.88473032999998));
#233330=CARTESIAN_POINT('Ctrl Pts',(-3.20944868300006,15.2,9.88570895099999));
#233331=CARTESIAN_POINT('Ctrl Pts',(-3.20944868300006,11.6,9.88570895099999));
#233332=CARTESIAN_POINT('Ctrl Pts',(-3.20988831200005,15.2,9.88669548899999));
#233333=CARTESIAN_POINT('Ctrl Pts',(-3.20988831200005,11.6,9.88669548899999));
#233334=CARTESIAN_POINT('Ctrl Pts',(-3.21033263400006,15.2,9.88768991299998));
#233335=CARTESIAN_POINT('Ctrl Pts',(-3.21033263400006,11.6,9.88768991299998));
#233336=CARTESIAN_POINT('Ctrl Pts',(-3.21078165500006,15.2,9.88869219599999));
#233337=CARTESIAN_POINT('Ctrl Pts',(-3.21078165500006,11.6,9.88869219599999));
#233338=CARTESIAN_POINT('Ctrl Pts',(-3.21123538000006,15.2,9.88970230599998));
#233339=CARTESIAN_POINT('Ctrl Pts',(-3.21123538000006,11.6,9.88970230599998));
#233340=CARTESIAN_POINT('Ctrl Pts',(-3.21169381300006,15.2,9.89072021499998));
#233341=CARTESIAN_POINT('Ctrl Pts',(-3.21169381300006,11.6,9.89072021499998));
#233342=CARTESIAN_POINT('Ctrl Pts',(-3.21215696200006,15.2,9.89174589399998));
#233343=CARTESIAN_POINT('Ctrl Pts',(-3.21215696200006,11.6,9.89174589399998));
#233344=CARTESIAN_POINT('Ctrl Pts',(-3.21262483100006,15.2,9.89277931299998));
#233345=CARTESIAN_POINT('Ctrl Pts',(-3.21262483100006,11.6,9.89277931299998));
#233346=CARTESIAN_POINT('Ctrl Pts',(-3.21309742500006,15.2,9.89382044299998));
#233347=CARTESIAN_POINT('Ctrl Pts',(-3.21309742500006,11.6,9.89382044299998));
#233348=CARTESIAN_POINT('Ctrl Pts',(-3.21357474800006,15.2,9.89486925699998));
#233349=CARTESIAN_POINT('Ctrl Pts',(-3.21357474800006,11.6,9.89486925699998));
#233350=CARTESIAN_POINT('Ctrl Pts',(-3.21405680800006,15.2,9.89592572399999));
#233351=CARTESIAN_POINT('Ctrl Pts',(-3.21405680800006,11.6,9.89592572399999));
#233352=CARTESIAN_POINT('Ctrl Pts',(-3.21454360800006,15.2,9.89698981699998));
#233353=CARTESIAN_POINT('Ctrl Pts',(-3.21454360800006,11.6,9.89698981699998));
#233354=CARTESIAN_POINT('Ctrl Pts',(-3.21503515400006,15.2,9.89806150699999));
#233355=CARTESIAN_POINT('Ctrl Pts',(-3.21503515400006,11.6,9.89806150699999));
#233356=CARTESIAN_POINT('Ctrl Pts',(-3.21553144900005,15.2,9.89914076599998));
#233357=CARTESIAN_POINT('Ctrl Pts',(-3.21553144900005,11.6,9.89914076599998));
#233358=CARTESIAN_POINT('Ctrl Pts',(-3.21603250100006,15.2,9.90022756599998));
#233359=CARTESIAN_POINT('Ctrl Pts',(-3.21603250100006,11.6,9.90022756599998));
#233360=CARTESIAN_POINT('Ctrl Pts',(-3.21653831300006,15.2,9.90132187799999));
#233361=CARTESIAN_POINT('Ctrl Pts',(-3.21653831300006,11.6,9.90132187799999));
#233362=CARTESIAN_POINT('Ctrl Pts',(-3.21704889000006,15.2,9.90242367599999));
#233363=CARTESIAN_POINT('Ctrl Pts',(-3.21704889000006,11.6,9.90242367599999));
#233364=CARTESIAN_POINT('Ctrl Pts',(-3.21756423800006,15.2,9.90353292999998));
#233365=CARTESIAN_POINT('Ctrl Pts',(-3.21756423800006,11.6,9.90353292999998));
#233366=CARTESIAN_POINT('Ctrl Pts',(-3.21808436100006,15.2,9.90464961299999));
#233367=CARTESIAN_POINT('Ctrl Pts',(-3.21808436100006,11.6,9.90464961299999));
#233368=CARTESIAN_POINT('Ctrl Pts',(-3.21860926400006,15.2,9.90577369899999));
#233369=CARTESIAN_POINT('Ctrl Pts',(-3.21860926400006,11.6,9.90577369899999));
#233370=CARTESIAN_POINT('Ctrl Pts',(-3.21913895200006,15.2,9.90690515799999));
#233371=CARTESIAN_POINT('Ctrl Pts',(-3.21913895200006,11.6,9.90690515799999));
#233372=CARTESIAN_POINT('Ctrl Pts',(-3.21967342800006,15.2,9.90804396499998));
#233373=CARTESIAN_POINT('Ctrl Pts',(-3.21967342800006,11.6,9.90804396499998));
#233374=CARTESIAN_POINT('Ctrl Pts',(-3.22021270000006,15.2,9.90919009099999));
#233375=CARTESIAN_POINT('Ctrl Pts',(-3.22021270000006,11.6,9.90919009099999));
#233376=CARTESIAN_POINT('Ctrl Pts',(-3.22075677000006,15.2,9.91034351099999));
#233377=CARTESIAN_POINT('Ctrl Pts',(-3.22075677000006,11.6,9.91034351099999));
#233378=CARTESIAN_POINT('Ctrl Pts',(-3.22130564400006,15.2,9.91150419699999));
#233379=CARTESIAN_POINT('Ctrl Pts',(-3.22130564400006,11.6,9.91150419699999));
#233380=CARTESIAN_POINT('Ctrl Pts',(-3.22185932500005,15.2,9.91267212099999));
#233381=CARTESIAN_POINT('Ctrl Pts',(-3.22185932500005,11.6,9.91267212099999));
#233382=CARTESIAN_POINT('Ctrl Pts',(-3.22241782000006,15.2,9.91384725799998));
#233383=CARTESIAN_POINT('Ctrl Pts',(-3.22241782000006,11.6,9.91384725799998));
#233384=CARTESIAN_POINT('Ctrl Pts',(-3.22298113100006,15.2,9.91502958099998));
#233385=CARTESIAN_POINT('Ctrl Pts',(-3.22298113100006,11.6,9.91502958099998));
#233386=CARTESIAN_POINT('Ctrl Pts',(-3.22354926400005,15.2,9.91621906299999));
#233387=CARTESIAN_POINT('Ctrl Pts',(-3.22354926400005,11.6,9.91621906299999));
#233388=CARTESIAN_POINT('Ctrl Pts',(-3.22412222300006,15.2,9.91741567799998));
#233389=CARTESIAN_POINT('Ctrl Pts',(-3.22412222300006,11.6,9.91741567799998));
#233390=CARTESIAN_POINT('Ctrl Pts',(-3.22470001300006,15.2,9.91861939899999));
#233391=CARTESIAN_POINT('Ctrl Pts',(-3.22470001300006,11.6,9.91861939899999));
#233392=CARTESIAN_POINT('Ctrl Pts',(-3.22528263900006,15.2,9.91983020199999));
#233393=CARTESIAN_POINT('Ctrl Pts',(-3.22528263900006,11.6,9.91983020199999));
#233394=CARTESIAN_POINT('Ctrl Pts',(-3.22587010200006,15.2,9.92104805799999));
#233395=CARTESIAN_POINT('Ctrl Pts',(-3.22587010200006,11.6,9.92104805799999));
#233396=CARTESIAN_POINT('Ctrl Pts',(-3.22646241000006,15.2,9.92227294299998));
#233397=CARTESIAN_POINT('Ctrl Pts',(-3.22646241000006,11.6,9.92227294299998));
#233398=CARTESIAN_POINT('Ctrl Pts',(-3.22705956700006,15.2,9.92350483199999));
#233399=CARTESIAN_POINT('Ctrl Pts',(-3.22705956700006,11.6,9.92350483199999));
#233400=CARTESIAN_POINT('Ctrl Pts',(-3.22766157600006,15.2,9.92474369799999));
#233401=CARTESIAN_POINT('Ctrl Pts',(-3.22766157600006,11.6,9.92474369799999));
#233402=CARTESIAN_POINT('Ctrl Pts',(-3.22826843900006,15.2,9.92598951399999));
#233403=CARTESIAN_POINT('Ctrl Pts',(-3.22826843900006,11.6,9.92598951399999));
#233404=CARTESIAN_POINT('Ctrl Pts',(-3.22888016500006,15.2,9.92724225699998));
#233405=CARTESIAN_POINT('Ctrl Pts',(-3.22888016500006,11.6,9.92724225699998));
#233406=CARTESIAN_POINT('Ctrl Pts',(-3.22949675600006,15.2,9.92850189999999));
#233407=CARTESIAN_POINT('Ctrl Pts',(-3.22949675600006,11.6,9.92850189999999));
#233408=CARTESIAN_POINT('Ctrl Pts',(-3.23011821600006,15.2,9.92976841899999));
#233409=CARTESIAN_POINT('Ctrl Pts',(-3.23011821600006,11.6,9.92976841899999));
#233410=CARTESIAN_POINT('Ctrl Pts',(-3.23074454800006,15.2,9.93104178799998));
#233411=CARTESIAN_POINT('Ctrl Pts',(-3.23074454800006,11.6,9.93104178799998));
#233412=CARTESIAN_POINT('Ctrl Pts',(-3.23137575800006,15.2,9.93232198199999));
#233413=CARTESIAN_POINT('Ctrl Pts',(-3.23137575800006,11.6,9.93232198199999));
#233414=CARTESIAN_POINT('Ctrl Pts',(-3.23201185000006,15.2,9.93360897599998));
#233415=CARTESIAN_POINT('Ctrl Pts',(-3.23201185000006,11.6,9.93360897599998));
#233416=CARTESIAN_POINT('Ctrl Pts',(-3.23265282700006,15.2,9.93490274499998));
#233417=CARTESIAN_POINT('Ctrl Pts',(-3.23265282700006,11.6,9.93490274499998));
#233418=CARTESIAN_POINT('Ctrl Pts',(-3.23329869300006,15.2,9.93620326399999));
#233419=CARTESIAN_POINT('Ctrl Pts',(-3.23329869300006,11.6,9.93620326399999));
#233420=CARTESIAN_POINT('Ctrl Pts',(-3.23394945200006,15.2,9.93751050999998));
#233421=CARTESIAN_POINT('Ctrl Pts',(-3.23394945200006,11.6,9.93751050999998));
#233422=CARTESIAN_POINT('Ctrl Pts',(-3.23460510900006,15.2,9.93882445699998));
#233423=CARTESIAN_POINT('Ctrl Pts',(-3.23460510900006,11.6,9.93882445699998));
#233424=CARTESIAN_POINT('Ctrl Pts',(-3.23526566700005,15.2,9.94014507999999));
#233425=CARTESIAN_POINT('Ctrl Pts',(-3.23526566700005,11.6,9.94014507999999));
#233426=CARTESIAN_POINT('Ctrl Pts',(-3.23593113000006,15.2,9.94147235599998));
#233427=CARTESIAN_POINT('Ctrl Pts',(-3.23593113000006,11.6,9.94147235599998));
#233428=CARTESIAN_POINT('Ctrl Pts',(-3.23660150200006,15.2,9.94280625999998));
#233429=CARTESIAN_POINT('Ctrl Pts',(-3.23660150200006,11.6,9.94280625999998));
#233430=CARTESIAN_POINT('Ctrl Pts',(-3.23727678700005,15.2,9.94414676799998));
#233431=CARTESIAN_POINT('Ctrl Pts',(-3.23727678700005,11.6,9.94414676799998));
#233432=CARTESIAN_POINT('Ctrl Pts',(-3.23795698800006,15.2,9.94549385599999));
#233433=CARTESIAN_POINT('Ctrl Pts',(-3.23795698800006,11.6,9.94549385599999));
#233434=CARTESIAN_POINT('Ctrl Pts',(-3.23864211000005,15.2,9.94684749899999));
#233435=CARTESIAN_POINT('Ctrl Pts',(-3.23864211000005,11.6,9.94684749899999));
#233436=CARTESIAN_POINT('Ctrl Pts',(-3.23933215600006,15.2,9.94820767499998));
#233437=CARTESIAN_POINT('Ctrl Pts',(-3.23933215600006,11.6,9.94820767499998));
#233438=CARTESIAN_POINT('Ctrl Pts',(-3.24002712900006,15.2,9.94957435799999));
#233439=CARTESIAN_POINT('Ctrl Pts',(-3.24002712900006,11.6,9.94957435799999));
#233440=CARTESIAN_POINT('Ctrl Pts',(-3.24072703400006,15.2,9.95094752699998));
#233441=CARTESIAN_POINT('Ctrl Pts',(-3.24072703400006,11.6,9.95094752699998));
#233442=CARTESIAN_POINT('Ctrl Pts',(-3.24143187300006,15.2,9.95232715499998));
#233443=CARTESIAN_POINT('Ctrl Pts',(-3.24143187300006,11.6,9.95232715499998));
#233444=CARTESIAN_POINT('Ctrl Pts',(-3.24214165200006,15.2,9.95371322199999));
#233445=CARTESIAN_POINT('Ctrl Pts',(-3.24214165200006,11.6,9.95371322199999));
#233446=CARTESIAN_POINT('Ctrl Pts',(-3.24285637300005,15.2,9.95510570299999));
#233447=CARTESIAN_POINT('Ctrl Pts',(-3.24285637300005,11.6,9.95510570299999));
#233448=CARTESIAN_POINT('Ctrl Pts',(-3.24357604000005,15.2,9.95650457299998));
#233449=CARTESIAN_POINT('Ctrl Pts',(-3.24357604000005,11.6,9.95650457299998));
#233450=CARTESIAN_POINT('Ctrl Pts',(-3.24430065600006,15.2,9.95790981099999));
#233451=CARTESIAN_POINT('Ctrl Pts',(-3.24430065600006,11.6,9.95790981099999));
#233452=CARTESIAN_POINT('Ctrl Pts',(-3.24503022600005,15.2,9.95932139299999));
#233453=CARTESIAN_POINT('Ctrl Pts',(-3.24503022600005,11.6,9.95932139299999));
#233454=CARTESIAN_POINT('Ctrl Pts',(-3.24576475100006,15.2,9.96073929699998));
#233455=CARTESIAN_POINT('Ctrl Pts',(-3.24576475100006,11.6,9.96073929699998));
#233456=CARTESIAN_POINT('Ctrl Pts',(-3.24650423700006,15.2,9.96216349899999));
#233457=CARTESIAN_POINT('Ctrl Pts',(-3.24650423700006,11.6,9.96216349899999));
#233458=CARTESIAN_POINT('Ctrl Pts',(-3.24724868600006,15.2,9.96359397599999));
#233459=CARTESIAN_POINT('Ctrl Pts',(-3.24724868600006,11.6,9.96359397599999));
#233460=CARTESIAN_POINT('Ctrl Pts',(-3.24799810100005,15.2,9.96503070499998));
#233461=CARTESIAN_POINT('Ctrl Pts',(-3.24799810100005,11.6,9.96503070499998));
#233462=CARTESIAN_POINT('Ctrl Pts',(-3.24875248700006,15.2,9.96647366399999));
#233463=CARTESIAN_POINT('Ctrl Pts',(-3.24875248700006,11.6,9.96647366399999));
#233464=CARTESIAN_POINT('Ctrl Pts',(-3.24951184600006,15.2,9.96792282999999));
#233465=CARTESIAN_POINT('Ctrl Pts',(-3.24951184600006,11.6,9.96792282999999));
#233466=CARTESIAN_POINT('Ctrl Pts',(-3.25027618200005,15.2,9.96937817999999));
#233467=CARTESIAN_POINT('Ctrl Pts',(-3.25027618200005,11.6,9.96937817999999));
#233468=CARTESIAN_POINT('Ctrl Pts',(-3.25104550000006,15.2,9.97083969299998));
#233469=CARTESIAN_POINT('Ctrl Pts',(-3.25104550000006,11.6,9.97083969299998));
#233470=CARTESIAN_POINT('Ctrl Pts',(-3.25181979900006,15.2,9.97230734499999));
#233471=CARTESIAN_POINT('Ctrl Pts',(-3.25181979900006,11.6,9.97230734499999));
#233472=CARTESIAN_POINT('Ctrl Pts',(-3.25259908600006,15.2,9.97378111499999));
#233473=CARTESIAN_POINT('Ctrl Pts',(-3.25259908600006,11.6,9.97378111499999));
#233474=CARTESIAN_POINT('Ctrl Pts',(-3.25338336200006,15.2,9.97526097899998));
#233475=CARTESIAN_POINT('Ctrl Pts',(-3.25338336200006,11.6,9.97526097899998));
#233476=CARTESIAN_POINT('Ctrl Pts',(-3.25417263200006,15.2,9.97674691699999));
#233477=CARTESIAN_POINT('Ctrl Pts',(-3.25417263200006,11.6,9.97674691699999));
#233478=CARTESIAN_POINT('Ctrl Pts',(-3.25496689700006,15.2,9.97823890599999));
#233479=CARTESIAN_POINT('Ctrl Pts',(-3.25496689700006,11.6,9.97823890599999));
#233480=CARTESIAN_POINT('Ctrl Pts',(-3.25576616300005,15.2,9.97973692499999));
#233481=CARTESIAN_POINT('Ctrl Pts',(-3.25576616300005,11.6,9.97973692499999));
#233482=CARTESIAN_POINT('Ctrl Pts',(-3.25657043100006,15.2,9.98124094999999));
#233483=CARTESIAN_POINT('Ctrl Pts',(-3.25657043100006,11.6,9.98124094999999));
#233484=CARTESIAN_POINT('Ctrl Pts',(-3.25737970400006,15.2,9.98275095999999));
#233485=CARTESIAN_POINT('Ctrl Pts',(-3.25737970400006,11.6,9.98275095999999));
#233486=CARTESIAN_POINT('Ctrl Pts',(-3.25819398700005,15.2,9.98426693399999));
#233487=CARTESIAN_POINT('Ctrl Pts',(-3.25819398700005,11.6,9.98426693399999));
#233488=CARTESIAN_POINT('Ctrl Pts',(-3.25901328200006,15.2,9.98578885099998));
#233489=CARTESIAN_POINT('Ctrl Pts',(-3.25901328200006,11.6,9.98578885099998));
#233490=CARTESIAN_POINT('Ctrl Pts',(-3.25983759100006,15.2,9.98731668699998));
#233491=CARTESIAN_POINT('Ctrl Pts',(-3.25983759100006,11.6,9.98731668699998));
#233492=CARTESIAN_POINT('Ctrl Pts',(-3.26066691700006,15.2,9.98885042199999));
#233493=CARTESIAN_POINT('Ctrl Pts',(-3.26066691700006,11.6,9.98885042199999));
#233494=CARTESIAN_POINT('Ctrl Pts',(-3.26150126600006,15.2,9.99039003499998));
#233495=CARTESIAN_POINT('Ctrl Pts',(-3.26150126600006,11.6,9.99039003499998));
#233496=CARTESIAN_POINT('Ctrl Pts',(-3.26234063800006,15.2,9.99193550399998));
#233497=CARTESIAN_POINT('Ctrl Pts',(-3.26234063800006,11.6,9.99193550399998));
#233498=CARTESIAN_POINT('Ctrl Pts',(-3.26318503700006,15.2,9.99348680799999));
#233499=CARTESIAN_POINT('Ctrl Pts',(-3.26318503700006,11.6,9.99348680799999));
#233500=CARTESIAN_POINT('Ctrl Pts',(-3.26403446500006,15.2,9.99504392599999));
#233501=CARTESIAN_POINT('Ctrl Pts',(-3.26403446500006,11.6,9.99504392599999));
#233502=CARTESIAN_POINT('Ctrl Pts',(-3.26488892700006,15.2,9.99660683599998));
#233503=CARTESIAN_POINT('Ctrl Pts',(-3.26488892700006,11.6,9.99660683599998));
#233504=CARTESIAN_POINT('Ctrl Pts',(-3.26574842300006,15.2,9.99817551799998));
#233505=CARTESIAN_POINT('Ctrl Pts',(-3.26574842300006,11.6,9.99817551799998));
#233506=CARTESIAN_POINT('Ctrl Pts',(-3.26661295800006,15.2,9.99974995199998));
#233507=CARTESIAN_POINT('Ctrl Pts',(-3.26661295800006,11.6,9.99974995199998));
#233508=CARTESIAN_POINT('Ctrl Pts',(-3.26748253400006,15.2,10.001330114));
#233509=CARTESIAN_POINT('Ctrl Pts',(-3.26748253400006,11.6,10.001330114));
#233510=CARTESIAN_POINT('Ctrl Pts',(-3.26835715400006,15.2,10.002915986));
#233511=CARTESIAN_POINT('Ctrl Pts',(-3.26835715400006,11.6,10.002915986));
#233512=CARTESIAN_POINT('Ctrl Pts',(-3.26923682100006,15.2,10.004507545));
#233513=CARTESIAN_POINT('Ctrl Pts',(-3.26923682100006,11.6,10.004507545));
#233514=CARTESIAN_POINT('Ctrl Pts',(-3.27012153800006,15.2,10.006104772));
#233515=CARTESIAN_POINT('Ctrl Pts',(-3.27012153800006,11.6,10.006104772));
#233516=CARTESIAN_POINT('Ctrl Pts',(-3.27101130700005,15.2,10.007707647));
#233517=CARTESIAN_POINT('Ctrl Pts',(-3.27101130700005,11.6,10.007707647));
#233518=CARTESIAN_POINT('Ctrl Pts',(-3.27190613100006,15.2,10.009316147));
#233519=CARTESIAN_POINT('Ctrl Pts',(-3.27190613100006,11.6,10.009316147));
#233520=CARTESIAN_POINT('Ctrl Pts',(-3.27280601300005,15.2,10.010930254));
#233521=CARTESIAN_POINT('Ctrl Pts',(-3.27280601300005,11.6,10.010930254));
#233522=CARTESIAN_POINT('Ctrl Pts',(-3.27371095400005,15.2,10.012549946));
#233523=CARTESIAN_POINT('Ctrl Pts',(-3.27371095400005,11.6,10.012549946));
#233524=CARTESIAN_POINT('Ctrl Pts',(-3.27462095900006,15.2,10.014175204));
#233525=CARTESIAN_POINT('Ctrl Pts',(-3.27462095900006,11.6,10.014175204));
#233526=CARTESIAN_POINT('Ctrl Pts',(-3.27553603000006,15.2,10.015806007));
#233527=CARTESIAN_POINT('Ctrl Pts',(-3.27553603000006,11.6,10.015806007));
#233528=CARTESIAN_POINT('Ctrl Pts',(-3.27645616800006,15.2,10.017442335));
#233529=CARTESIAN_POINT('Ctrl Pts',(-3.27645616800006,11.6,10.017442335));
#233530=CARTESIAN_POINT('Ctrl Pts',(-3.27738137700006,15.2,10.019084167));
#233531=CARTESIAN_POINT('Ctrl Pts',(-3.27738137700006,11.6,10.019084167));
#233532=CARTESIAN_POINT('Ctrl Pts',(-3.27831166000006,15.2,10.020731485));
#233533=CARTESIAN_POINT('Ctrl Pts',(-3.27831166000006,11.6,10.020731485));
#233534=CARTESIAN_POINT('Ctrl Pts',(-3.27924701900006,15.2,10.022384268));
#233535=CARTESIAN_POINT('Ctrl Pts',(-3.27924701900006,11.6,10.022384268));
#233536=CARTESIAN_POINT('Ctrl Pts',(-3.28018745600006,15.2,10.024042496));
#233537=CARTESIAN_POINT('Ctrl Pts',(-3.28018745600006,11.6,10.024042496));
#233538=CARTESIAN_POINT('Ctrl Pts',(-3.28113297400006,15.2,10.025706148));
#233539=CARTESIAN_POINT('Ctrl Pts',(-3.28113297400006,11.6,10.025706148));
#233540=CARTESIAN_POINT('Ctrl Pts',(-3.28208357600006,15.2,10.027375206));
#233541=CARTESIAN_POINT('Ctrl Pts',(-3.28208357600006,11.6,10.027375206));
#233542=CARTESIAN_POINT('Ctrl Pts',(-3.28303926400006,15.2,10.02904965));
#233543=CARTESIAN_POINT('Ctrl Pts',(-3.28303926400006,11.6,10.02904965));
#233544=CARTESIAN_POINT('Ctrl Pts',(-3.28400003900006,15.2,10.03072946));
#233545=CARTESIAN_POINT('Ctrl Pts',(-3.28400003900006,11.6,10.03072946));
#233546=CARTESIAN_POINT('Ctrl Pts',(-3.28496590600006,15.2,10.032414616));
#233547=CARTESIAN_POINT('Ctrl Pts',(-3.28496590600006,11.6,10.032414616));
#233548=CARTESIAN_POINT('Ctrl Pts',(-3.28593686500006,15.2,10.0341051));
#233549=CARTESIAN_POINT('Ctrl Pts',(-3.28593686500006,11.6,10.0341051));
#233550=CARTESIAN_POINT('Ctrl Pts',(-3.28691292000005,15.2,10.035800891));
#233551=CARTESIAN_POINT('Ctrl Pts',(-3.28691292000005,11.6,10.035800891));
#233552=CARTESIAN_POINT('Ctrl Pts',(-3.28789407300006,15.2,10.037501971));
#233553=CARTESIAN_POINT('Ctrl Pts',(-3.28789407300006,11.6,10.037501971));
#233554=CARTESIAN_POINT('Ctrl Pts',(-3.28888032700006,15.2,10.03920832));
#233555=CARTESIAN_POINT('Ctrl Pts',(-3.28888032700006,11.6,10.03920832));
#233556=CARTESIAN_POINT('Ctrl Pts',(-3.28987168300006,15.2,10.040919918));
#233557=CARTESIAN_POINT('Ctrl Pts',(-3.28987168300006,11.6,10.040919918));
#233558=CARTESIAN_POINT('Ctrl Pts',(-3.29086814400006,15.2,10.042636747));
#233559=CARTESIAN_POINT('Ctrl Pts',(-3.29086814400006,11.6,10.042636747));
#233560=CARTESIAN_POINT('Ctrl Pts',(-3.29186971100006,15.2,10.044358787));
#233561=CARTESIAN_POINT('Ctrl Pts',(-3.29186971100006,11.6,10.044358787));
#233562=CARTESIAN_POINT('Ctrl Pts',(-3.29287638800006,15.2,10.046086019));
#233563=CARTESIAN_POINT('Ctrl Pts',(-3.29287638800006,11.6,10.046086019));
#233564=CARTESIAN_POINT('Ctrl Pts',(-3.29388817700006,15.2,10.047818426));
#233565=CARTESIAN_POINT('Ctrl Pts',(-3.29388817700006,11.6,10.047818426));
#233566=CARTESIAN_POINT('Ctrl Pts',(-3.29490507900006,15.2,10.049555987));
#233567=CARTESIAN_POINT('Ctrl Pts',(-3.29490507900006,11.6,10.049555987));
#233568=CARTESIAN_POINT('Ctrl Pts',(-3.29592709800006,15.2,10.051298683));
#233569=CARTESIAN_POINT('Ctrl Pts',(-3.29592709800006,11.6,10.051298683));
#233570=CARTESIAN_POINT('Ctrl Pts',(-3.29695423400006,15.2,10.053046497));
#233571=CARTESIAN_POINT('Ctrl Pts',(-3.29695423400006,11.6,10.053046497));
#233572=CARTESIAN_POINT('Ctrl Pts',(-3.29798649200006,15.2,10.054799409));
#233573=CARTESIAN_POINT('Ctrl Pts',(-3.29798649200006,11.6,10.054799409));
#233574=CARTESIAN_POINT('Ctrl Pts',(-3.29902387100006,15.2,10.0565574));
#233575=CARTESIAN_POINT('Ctrl Pts',(-3.29902387100006,11.6,10.0565574));
#233576=CARTESIAN_POINT('Ctrl Pts',(-3.30006637500006,15.2,10.058320453));
#233577=CARTESIAN_POINT('Ctrl Pts',(-3.30006637500006,11.6,10.058320453));
#233578=CARTESIAN_POINT('Ctrl Pts',(-3.30111400600006,15.2,10.060088547));
#233579=CARTESIAN_POINT('Ctrl Pts',(-3.30111400600006,11.6,10.060088547));
#233580=CARTESIAN_POINT('Ctrl Pts',(-3.30216676600006,15.2,10.061861665));
#233581=CARTESIAN_POINT('Ctrl Pts',(-3.30216676600006,11.6,10.061861665));
#233582=CARTESIAN_POINT('Ctrl Pts',(-3.30322465700006,15.2,10.063639789));
#233583=CARTESIAN_POINT('Ctrl Pts',(-3.30322465700006,11.6,10.063639789));
#233584=CARTESIAN_POINT('Ctrl Pts',(-3.30428768000006,15.2,10.065422899));
#233585=CARTESIAN_POINT('Ctrl Pts',(-3.30428768000006,11.6,10.065422899));
#233586=CARTESIAN_POINT('Ctrl Pts',(-3.30535583900006,15.2,10.067210979));
#233587=CARTESIAN_POINT('Ctrl Pts',(-3.30535583900006,11.6,10.067210979));
#233588=CARTESIAN_POINT('Ctrl Pts',(-3.30642913400006,15.2,10.069004009));
#233589=CARTESIAN_POINT('Ctrl Pts',(-3.30642913400006,11.6,10.069004009));
#233590=CARTESIAN_POINT('Ctrl Pts',(-3.30750756900006,15.2,10.070801971));
#233591=CARTESIAN_POINT('Ctrl Pts',(-3.30750756900006,11.6,10.070801971));
#233592=CARTESIAN_POINT('Ctrl Pts',(-3.30859114400006,15.2,10.072604847));
#233593=CARTESIAN_POINT('Ctrl Pts',(-3.30859114400006,11.6,10.072604847));
#233594=CARTESIAN_POINT('Ctrl Pts',(-3.30967986300006,15.2,10.07441262));
#233595=CARTESIAN_POINT('Ctrl Pts',(-3.30967986300006,11.6,10.07441262));
#233596=CARTESIAN_POINT('Ctrl Pts',(-3.31077372600005,15.2,10.07622527));
#233597=CARTESIAN_POINT('Ctrl Pts',(-3.31077372600005,11.6,10.07622527));
#233598=CARTESIAN_POINT('Ctrl Pts',(-3.31187273500006,15.2,10.078042781));
#233599=CARTESIAN_POINT('Ctrl Pts',(-3.31187273500006,11.6,10.078042781));
#233600=CARTESIAN_POINT('Ctrl Pts',(-3.31297689300006,15.2,10.079865133));
#233601=CARTESIAN_POINT('Ctrl Pts',(-3.31297689300006,11.6,10.079865133));
#233602=CARTESIAN_POINT('Ctrl Pts',(-3.31408620300006,15.2,10.081692309));
#233603=CARTESIAN_POINT('Ctrl Pts',(-3.31408620300006,11.6,10.081692309));
#233604=CARTESIAN_POINT('Ctrl Pts',(-3.31520066400006,15.2,10.083524292));
#233605=CARTESIAN_POINT('Ctrl Pts',(-3.31520066400006,11.6,10.083524292));
#233606=CARTESIAN_POINT('Ctrl Pts',(-3.31632027900006,15.2,10.085361064));
#233607=CARTESIAN_POINT('Ctrl Pts',(-3.31632027900006,11.6,10.085361064));
#233608=CARTESIAN_POINT('Ctrl Pts',(-3.31744505100006,15.2,10.087202607));
#233609=CARTESIAN_POINT('Ctrl Pts',(-3.31744505100006,11.6,10.087202607));
#233610=CARTESIAN_POINT('Ctrl Pts',(-3.31857498100006,15.2,10.089048904));
#233611=CARTESIAN_POINT('Ctrl Pts',(-3.31857498100006,11.6,10.089048904));
#233612=CARTESIAN_POINT('Ctrl Pts',(-3.31971007100006,15.2,10.090899936));
#233613=CARTESIAN_POINT('Ctrl Pts',(-3.31971007100006,11.6,10.090899936));
#233614=CARTESIAN_POINT('Ctrl Pts',(-3.32085032200006,15.2,10.092755686));
#233615=CARTESIAN_POINT('Ctrl Pts',(-3.32085032200006,11.6,10.092755686));
#233616=CARTESIAN_POINT('Ctrl Pts',(-3.32199573600006,15.2,10.094616137));
#233617=CARTESIAN_POINT('Ctrl Pts',(-3.32199573600006,11.6,10.094616137));
#233618=CARTESIAN_POINT('Ctrl Pts',(-3.32314631600005,15.2,10.096481272));
#233619=CARTESIAN_POINT('Ctrl Pts',(-3.32314631600005,11.6,10.096481272));
#233620=CARTESIAN_POINT('Ctrl Pts',(-3.32430206100006,15.2,10.098351073));
#233621=CARTESIAN_POINT('Ctrl Pts',(-3.32430206100006,11.6,10.098351073));
#233622=CARTESIAN_POINT('Ctrl Pts',(-3.32546297600006,15.2,10.100225521));
#233623=CARTESIAN_POINT('Ctrl Pts',(-3.32546297600006,11.6,10.100225521));
#233624=CARTESIAN_POINT('Ctrl Pts',(-3.32662906000006,15.2,10.102104602));
#233625=CARTESIAN_POINT('Ctrl Pts',(-3.32662906000006,11.6,10.102104602));
#233626=CARTESIAN_POINT('Ctrl Pts',(-3.32780031700006,15.2,10.103988296));
#233627=CARTESIAN_POINT('Ctrl Pts',(-3.32780031700006,11.6,10.103988296));
#233628=CARTESIAN_POINT('Ctrl Pts',(-3.32897674600006,15.2,10.105876588));
#233629=CARTESIAN_POINT('Ctrl Pts',(-3.32897674600006,11.6,10.105876588));
#233630=CARTESIAN_POINT('Ctrl Pts',(-3.33015835200006,15.2,10.107769459));
#233631=CARTESIAN_POINT('Ctrl Pts',(-3.33015835200006,11.6,10.107769459));
#233632=CARTESIAN_POINT('Ctrl Pts',(-3.33134513300006,15.2,10.109666894));
#233633=CARTESIAN_POINT('Ctrl Pts',(-3.33134513300006,11.6,10.109666894));
#233634=CARTESIAN_POINT('Ctrl Pts',(-3.33253709400006,15.2,10.111568874));
#233635=CARTESIAN_POINT('Ctrl Pts',(-3.33253709400006,11.6,10.111568874));
#233636=CARTESIAN_POINT('Ctrl Pts',(-3.33373423400006,15.2,10.113475383));
#233637=CARTESIAN_POINT('Ctrl Pts',(-3.33373423400006,11.6,10.113475383));
#233638=CARTESIAN_POINT('Ctrl Pts',(-3.33493655500006,15.2,10.115386405));
#233639=CARTESIAN_POINT('Ctrl Pts',(-3.33493655500006,11.6,10.115386405));
#233640=CARTESIAN_POINT('Ctrl Pts',(-3.33614406000006,15.2,10.11730192));
#233641=CARTESIAN_POINT('Ctrl Pts',(-3.33614406000006,11.6,10.11730192));
#233642=CARTESIAN_POINT('Ctrl Pts',(-3.33735675000006,15.2,10.119221915));
#233643=CARTESIAN_POINT('Ctrl Pts',(-3.33735675000006,11.6,10.119221915));
#233644=CARTESIAN_POINT('Ctrl Pts',(-3.33857462500006,15.2,10.121146371));
#233645=CARTESIAN_POINT('Ctrl Pts',(-3.33857462500006,11.6,10.121146371));
#233646=CARTESIAN_POINT('Ctrl Pts',(-3.33979768900006,15.2,10.123075272));
#233647=CARTESIAN_POINT('Ctrl Pts',(-3.33979768900006,11.6,10.123075272));
#233648=CARTESIAN_POINT('Ctrl Pts',(-3.34102594100006,15.2,10.125008601));
#233649=CARTESIAN_POINT('Ctrl Pts',(-3.34102594100006,11.6,10.125008601));
#233650=CARTESIAN_POINT('Ctrl Pts',(-3.34225938500006,15.2,10.126946342));
#233651=CARTESIAN_POINT('Ctrl Pts',(-3.34225938500006,11.6,10.126946342));
#233652=CARTESIAN_POINT('Ctrl Pts',(-3.34349802100005,15.2,10.128888478));
#233653=CARTESIAN_POINT('Ctrl Pts',(-3.34349802100005,11.6,10.128888478));
#233654=CARTESIAN_POINT('Ctrl Pts',(-3.34474185000006,15.2,10.130834991));
#233655=CARTESIAN_POINT('Ctrl Pts',(-3.34474185000006,11.6,10.130834991));
#233656=CARTESIAN_POINT('Ctrl Pts',(-3.34599087400006,15.2,10.132785868));
#233657=CARTESIAN_POINT('Ctrl Pts',(-3.34599087400006,11.6,10.132785868));
#233658=CARTESIAN_POINT('Ctrl Pts',(-3.34724509500006,15.2,10.134741089));
#233659=CARTESIAN_POINT('Ctrl Pts',(-3.34724509500006,11.6,10.134741089));
#233660=CARTESIAN_POINT('Ctrl Pts',(-3.34850451400006,15.2,10.13670064));
#233661=CARTESIAN_POINT('Ctrl Pts',(-3.34850451400006,11.6,10.13670064));
#233662=CARTESIAN_POINT('Ctrl Pts',(-3.34976913200005,15.2,10.138664505));
#233663=CARTESIAN_POINT('Ctrl Pts',(-3.34976913200005,11.6,10.138664505));
#233664=CARTESIAN_POINT('Ctrl Pts',(-3.35103895100006,15.2,10.140632665));
#233665=CARTESIAN_POINT('Ctrl Pts',(-3.35103895100006,11.6,10.140632665));
#233666=CARTESIAN_POINT('Ctrl Pts',(-3.35231397200006,15.2,10.142605106));
#233667=CARTESIAN_POINT('Ctrl Pts',(-3.35231397200006,11.6,10.142605106));
#233668=CARTESIAN_POINT('Ctrl Pts',(-3.35359419600006,15.2,10.144581811));
#233669=CARTESIAN_POINT('Ctrl Pts',(-3.35359419600006,11.6,10.144581811));
#233670=CARTESIAN_POINT('Ctrl Pts',(-3.35487962600005,15.2,10.146562764));
#233671=CARTESIAN_POINT('Ctrl Pts',(-3.35487962600005,11.6,10.146562764));
#233672=CARTESIAN_POINT('Ctrl Pts',(-3.35617026000006,15.2,10.14854795));
#233673=CARTESIAN_POINT('Ctrl Pts',(-3.35617026000006,11.6,10.14854795));
#233674=CARTESIAN_POINT('Ctrl Pts',(-3.35746610300005,15.2,10.150537351));
#233675=CARTESIAN_POINT('Ctrl Pts',(-3.35746610300005,11.6,10.150537351));
#233676=CARTESIAN_POINT('Ctrl Pts',(-3.35876715400006,15.2,10.152530952));
#233677=CARTESIAN_POINT('Ctrl Pts',(-3.35876715400006,11.6,10.152530952));
#233678=CARTESIAN_POINT('Ctrl Pts',(-3.36007341500005,15.2,10.154528737));
#233679=CARTESIAN_POINT('Ctrl Pts',(-3.36007341500005,11.6,10.154528737));
#233680=CARTESIAN_POINT('Ctrl Pts',(-3.36138488700006,15.2,10.156530691));
#233681=CARTESIAN_POINT('Ctrl Pts',(-3.36138488700006,11.6,10.156530691));
#233682=CARTESIAN_POINT('Ctrl Pts',(-3.36270157200006,15.2,10.158536796));
#233683=CARTESIAN_POINT('Ctrl Pts',(-3.36270157200006,11.6,10.158536796));
#233684=CARTESIAN_POINT('Ctrl Pts',(-3.36402347000006,15.2,10.160547038));
#233685=CARTESIAN_POINT('Ctrl Pts',(-3.36402347000006,11.6,10.160547038));
#233686=CARTESIAN_POINT('Ctrl Pts',(-3.36535058300006,15.2,10.162561401));
#233687=CARTESIAN_POINT('Ctrl Pts',(-3.36535058300006,11.6,10.162561401));
#233688=CARTESIAN_POINT('Ctrl Pts',(-3.36668291200006,15.2,10.164579868));
#233689=CARTESIAN_POINT('Ctrl Pts',(-3.36668291200006,11.6,10.164579868));
#233690=CARTESIAN_POINT('Ctrl Pts',(-3.36802045900006,15.2,10.166602425));
#233691=CARTESIAN_POINT('Ctrl Pts',(-3.36802045900006,11.6,10.166602425));
#233692=CARTESIAN_POINT('Ctrl Pts',(-3.36936322400006,15.2,10.168629055));
#233693=CARTESIAN_POINT('Ctrl Pts',(-3.36936322400006,11.6,10.168629055));
#233694=CARTESIAN_POINT('Ctrl Pts',(-3.37071120800006,15.2,10.170659744));
#233695=CARTESIAN_POINT('Ctrl Pts',(-3.37071120800006,11.6,10.170659744));
#233696=CARTESIAN_POINT('Ctrl Pts',(-3.37206441300005,15.2,10.172694474));
#233697=CARTESIAN_POINT('Ctrl Pts',(-3.37206441300005,11.6,10.172694474));
#233698=CARTESIAN_POINT('Ctrl Pts',(-3.37342284100006,15.2,10.174733231));
#233699=CARTESIAN_POINT('Ctrl Pts',(-3.37342284100006,11.6,10.174733231));
#233700=CARTESIAN_POINT('Ctrl Pts',(-3.37478649100006,15.2,10.176776001));
#233701=CARTESIAN_POINT('Ctrl Pts',(-3.37478649100006,11.6,10.176776001));
#233702=CARTESIAN_POINT('Ctrl Pts',(-3.37615536500006,15.2,10.178822766));
#233703=CARTESIAN_POINT('Ctrl Pts',(-3.37615536500006,11.6,10.178822766));
#233704=CARTESIAN_POINT('Ctrl Pts',(-3.37752946400005,15.2,10.180873512));
#233705=CARTESIAN_POINT('Ctrl Pts',(-3.37752946400005,11.6,10.180873512));
#233706=CARTESIAN_POINT('Ctrl Pts',(-3.37890879000006,15.2,10.182928223));
#233707=CARTESIAN_POINT('Ctrl Pts',(-3.37890879000006,11.6,10.182928223));
#233708=CARTESIAN_POINT('Ctrl Pts',(-3.38029334200006,15.2,10.184986884));
#233709=CARTESIAN_POINT('Ctrl Pts',(-3.38029334200006,11.6,10.184986884));
#233710=CARTESIAN_POINT('Ctrl Pts',(-3.38168312400006,15.2,10.18704948));
#233711=CARTESIAN_POINT('Ctrl Pts',(-3.38168312400006,11.6,10.18704948));
#233712=CARTESIAN_POINT('Ctrl Pts',(-3.38307813500006,15.2,10.189115995));
#233713=CARTESIAN_POINT('Ctrl Pts',(-3.38307813500006,11.6,10.189115995));
#233714=CARTESIAN_POINT('Ctrl Pts',(-3.38447837600006,15.2,10.191186415));
#233715=CARTESIAN_POINT('Ctrl Pts',(-3.38447837600006,11.6,10.191186415));
#233716=CARTESIAN_POINT('Ctrl Pts',(-3.38588384900006,15.2,10.193260723));
#233717=CARTESIAN_POINT('Ctrl Pts',(-3.38588384900006,11.6,10.193260723));
#233718=CARTESIAN_POINT('Ctrl Pts',(-3.38729455300005,15.2,10.195338907));
#233719=CARTESIAN_POINT('Ctrl Pts',(-3.38729455300005,11.6,10.195338907));
#233720=CARTESIAN_POINT('Ctrl Pts',(-3.38871049200006,15.2,10.197420948));
#233721=CARTESIAN_POINT('Ctrl Pts',(-3.38871049200006,11.6,10.197420948));
#233722=CARTESIAN_POINT('Ctrl Pts',(-3.39013166400006,15.2,10.199506834));
#233723=CARTESIAN_POINT('Ctrl Pts',(-3.39013166400006,11.6,10.199506834));
#233724=CARTESIAN_POINT('Ctrl Pts',(-3.39155807300005,15.2,10.20159655));
#233725=CARTESIAN_POINT('Ctrl Pts',(-3.39155807300005,11.6,10.20159655));
#233726=CARTESIAN_POINT('Ctrl Pts',(-3.39298971700006,15.2,10.203690079));
#233727=CARTESIAN_POINT('Ctrl Pts',(-3.39298971700006,11.6,10.203690079));
#233728=CARTESIAN_POINT('Ctrl Pts',(-3.39442659800006,15.2,10.205787407));
#233729=CARTESIAN_POINT('Ctrl Pts',(-3.39442659800006,11.6,10.205787407));
#233730=CARTESIAN_POINT('Ctrl Pts',(-3.39586871900006,15.2,10.207888521));
#233731=CARTESIAN_POINT('Ctrl Pts',(-3.39586871900006,11.6,10.207888521));
#233732=CARTESIAN_POINT('Ctrl Pts',(-3.39731607700006,15.2,10.209993403));
#233733=CARTESIAN_POINT('Ctrl Pts',(-3.39731607700006,11.6,10.209993403));
#233734=CARTESIAN_POINT('Ctrl Pts',(-3.39876867500006,15.2,10.21210204));
#233735=CARTESIAN_POINT('Ctrl Pts',(-3.39876867500006,11.6,10.21210204));
#233736=CARTESIAN_POINT('Ctrl Pts',(-3.40022651400006,15.2,10.214214418));
#233737=CARTESIAN_POINT('Ctrl Pts',(-3.40022651400006,11.6,10.214214418));
#233738=CARTESIAN_POINT('Ctrl Pts',(-3.40168959500006,15.2,10.21633052));
#233739=CARTESIAN_POINT('Ctrl Pts',(-3.40168959500006,11.6,10.21633052));
#233740=CARTESIAN_POINT('Ctrl Pts',(-3.40315791900006,15.2,10.218450334));
#233741=CARTESIAN_POINT('Ctrl Pts',(-3.40315791900006,11.6,10.218450334));
#233742=CARTESIAN_POINT('Ctrl Pts',(-3.40463148500006,15.2,10.220573844));
#233743=CARTESIAN_POINT('Ctrl Pts',(-3.40463148500006,11.6,10.220573844));
#233744=CARTESIAN_POINT('Ctrl Pts',(-3.40611029600006,15.2,10.222701035));
#233745=CARTESIAN_POINT('Ctrl Pts',(-3.40611029600006,11.6,10.222701035));
#233746=CARTESIAN_POINT('Ctrl Pts',(-3.40759435200006,15.2,10.224831892));
#233747=CARTESIAN_POINT('Ctrl Pts',(-3.40759435200006,11.6,10.224831892));
#233748=CARTESIAN_POINT('Ctrl Pts',(-3.40908365400006,15.2,10.226966403));
#233749=CARTESIAN_POINT('Ctrl Pts',(-3.40908365400006,11.6,10.226966403));
#233750=CARTESIAN_POINT('Ctrl Pts',(-3.41057820200006,15.2,10.229104551));
#233751=CARTESIAN_POINT('Ctrl Pts',(-3.41057820200006,11.6,10.229104551));
#233752=CARTESIAN_POINT('Ctrl Pts',(-3.41207799700005,15.2,10.231246324));
#233753=CARTESIAN_POINT('Ctrl Pts',(-3.41207799700005,11.6,10.231246324));
#233754=CARTESIAN_POINT('Ctrl Pts',(-3.41358304100006,15.2,10.233391705));
#233755=CARTESIAN_POINT('Ctrl Pts',(-3.41358304100006,11.6,10.233391705));
#233756=CARTESIAN_POINT('Ctrl Pts',(-3.41509333200006,15.2,10.235540681));
#233757=CARTESIAN_POINT('Ctrl Pts',(-3.41509333200006,11.6,10.235540681));
#233758=CARTESIAN_POINT('Ctrl Pts',(-3.41660887500006,15.2,10.237693238));
#233759=CARTESIAN_POINT('Ctrl Pts',(-3.41660887500006,11.6,10.237693238));
#233760=CARTESIAN_POINT('Ctrl Pts',(-3.41812966600005,15.2,10.239849361));
#233761=CARTESIAN_POINT('Ctrl Pts',(-3.41812966600005,11.6,10.239849361));
#233762=CARTESIAN_POINT('Ctrl Pts',(-3.41965570900005,15.2,10.242009036));
#233763=CARTESIAN_POINT('Ctrl Pts',(-3.41965570900005,11.6,10.242009036));
#233764=CARTESIAN_POINT('Ctrl Pts',(-3.42118700500006,15.2,10.244172248));
#233765=CARTESIAN_POINT('Ctrl Pts',(-3.42118700500006,11.6,10.244172248));
#233766=CARTESIAN_POINT('Ctrl Pts',(-3.42272355100006,15.2,10.246338985));
#233767=CARTESIAN_POINT('Ctrl Pts',(-3.42272355100006,11.6,10.246338985));
#233768=CARTESIAN_POINT('Ctrl Pts',(-3.42426535200006,15.2,10.24850923));
#233769=CARTESIAN_POINT('Ctrl Pts',(-3.42426535200006,11.6,10.24850923));
#233770=CARTESIAN_POINT('Ctrl Pts',(-3.42581240600006,15.2,10.250682971));
#233771=CARTESIAN_POINT('Ctrl Pts',(-3.42581240600006,11.6,10.250682971));
#233772=CARTESIAN_POINT('Ctrl Pts',(-3.42736471300006,15.2,10.252860194));
#233773=CARTESIAN_POINT('Ctrl Pts',(-3.42736471300006,11.6,10.252860194));
#233774=CARTESIAN_POINT('Ctrl Pts',(-3.42892227700006,15.2,10.255040884));
#233775=CARTESIAN_POINT('Ctrl Pts',(-3.42892227700006,11.6,10.255040884));
#233776=CARTESIAN_POINT('Ctrl Pts',(-3.43048509600006,15.2,10.257225026));
#233777=CARTESIAN_POINT('Ctrl Pts',(-3.43048509600006,11.6,10.257225026));
#233778=CARTESIAN_POINT('Ctrl Pts',(-3.43205317100006,15.2,10.25941261));
#233779=CARTESIAN_POINT('Ctrl Pts',(-3.43205317100006,11.6,10.25941261));
#233780=CARTESIAN_POINT('Ctrl Pts',(-3.43362650400006,15.2,10.261603617));
#233781=CARTESIAN_POINT('Ctrl Pts',(-3.43362650400006,11.6,10.261603617));
#233782=CARTESIAN_POINT('Ctrl Pts',(-3.43520509300005,15.2,10.263798037));
#233783=CARTESIAN_POINT('Ctrl Pts',(-3.43520509300005,11.6,10.263798037));
#233784=CARTESIAN_POINT('Ctrl Pts',(-3.43678894100006,15.2,10.265995854));
#233785=CARTESIAN_POINT('Ctrl Pts',(-3.43678894100006,11.6,10.265995854));
#233786=CARTESIAN_POINT('Ctrl Pts',(-3.43837804700006,15.2,10.268197055));
#233787=CARTESIAN_POINT('Ctrl Pts',(-3.43837804700006,11.6,10.268197055));
#233788=CARTESIAN_POINT('Ctrl Pts',(-3.43997241300006,15.2,10.270401626));
#233789=CARTESIAN_POINT('Ctrl Pts',(-3.43997241300006,11.6,10.270401626));
#233790=CARTESIAN_POINT('Ctrl Pts',(-3.44157203800005,15.2,10.272609554));
#233791=CARTESIAN_POINT('Ctrl Pts',(-3.44157203800005,11.6,10.272609554));
#233792=CARTESIAN_POINT('Ctrl Pts',(-3.44317692300006,15.2,10.274820823));
#233793=CARTESIAN_POINT('Ctrl Pts',(-3.44317692300006,11.6,10.274820823));
#233794=CARTESIAN_POINT('Ctrl Pts',(-3.44478706900006,15.2,10.277035423));
#233795=CARTESIAN_POINT('Ctrl Pts',(-3.44478706900006,11.6,10.277035423));
#233796=CARTESIAN_POINT('Ctrl Pts',(-3.44640247700006,15.2,10.279253337));
#233797=CARTESIAN_POINT('Ctrl Pts',(-3.44640247700006,11.6,10.279253337));
#233798=CARTESIAN_POINT('Ctrl Pts',(-3.44802314600006,15.2,10.281474554));
#233799=CARTESIAN_POINT('Ctrl Pts',(-3.44802314600006,11.6,10.281474554));
#233800=CARTESIAN_POINT('Ctrl Pts',(-3.44964907800006,15.2,10.283699057));
#233801=CARTESIAN_POINT('Ctrl Pts',(-3.44964907800006,11.6,10.283699057));
#233802=CARTESIAN_POINT('Ctrl Pts',(-3.45128027200006,15.2,10.285926836));
#233803=CARTESIAN_POINT('Ctrl Pts',(-3.45128027200006,11.6,10.285926836));
#233804=CARTESIAN_POINT('Ctrl Pts',(-3.45291672900006,15.2,10.288157876));
#233805=CARTESIAN_POINT('Ctrl Pts',(-3.45291672900006,11.6,10.288157876));
#233806=CARTESIAN_POINT('Ctrl Pts',(-3.45455845100005,15.2,10.290392165));
#233807=CARTESIAN_POINT('Ctrl Pts',(-3.45455845100005,11.6,10.290392165));
#233808=CARTESIAN_POINT('Ctrl Pts',(-3.45620543600006,15.2,10.292629685));
#233809=CARTESIAN_POINT('Ctrl Pts',(-3.45620543600006,11.6,10.292629685));
#233810=CARTESIAN_POINT('Ctrl Pts',(-3.45785768600006,15.2,10.294870428));
#233811=CARTESIAN_POINT('Ctrl Pts',(-3.45785768600006,11.6,10.294870428));
#233812=CARTESIAN_POINT('Ctrl Pts',(-3.45951520100006,15.2,10.297114378));
#233813=CARTESIAN_POINT('Ctrl Pts',(-3.45951520100006,11.6,10.297114378));
#233814=CARTESIAN_POINT('Ctrl Pts',(-3.46117798100006,15.2,10.299361522));
#233815=CARTESIAN_POINT('Ctrl Pts',(-3.46117798100006,11.6,10.299361522));
#233816=CARTESIAN_POINT('Ctrl Pts',(-3.46284602800006,15.2,10.301611847));
#233817=CARTESIAN_POINT('Ctrl Pts',(-3.46284602800006,11.6,10.301611847));
#233818=CARTESIAN_POINT('Ctrl Pts',(-3.46451934000005,15.2,10.303865339));
#233819=CARTESIAN_POINT('Ctrl Pts',(-3.46451934000005,11.6,10.303865339));
#233820=CARTESIAN_POINT('Ctrl Pts',(-3.46619791900005,15.2,10.306121985));
#233821=CARTESIAN_POINT('Ctrl Pts',(-3.46619791900005,11.6,10.306121985));
#233822=CARTESIAN_POINT('Ctrl Pts',(-3.46788176500006,15.2,10.308381772));
#233823=CARTESIAN_POINT('Ctrl Pts',(-3.46788176500006,11.6,10.308381772));
#233824=CARTESIAN_POINT('Ctrl Pts',(-3.46957087800006,15.2,10.310644686));
#233825=CARTESIAN_POINT('Ctrl Pts',(-3.46957087800006,11.6,10.310644686));
#233826=CARTESIAN_POINT('Ctrl Pts',(-3.47126525900006,15.2,10.312910717));
#233827=CARTESIAN_POINT('Ctrl Pts',(-3.47126525900006,11.6,10.312910717));
#233828=CARTESIAN_POINT('Ctrl Pts',(-3.47296490800006,15.2,10.315179848));
#233829=CARTESIAN_POINT('Ctrl Pts',(-3.47296490800006,11.6,10.315179848));
#233830=CARTESIAN_POINT('Ctrl Pts',(-3.47466982500006,15.2,10.317452067));
#233831=CARTESIAN_POINT('Ctrl Pts',(-3.47466982500006,11.6,10.317452067));
#233832=CARTESIAN_POINT('Ctrl Pts',(-3.47638001000006,15.2,10.319727363));
#233833=CARTESIAN_POINT('Ctrl Pts',(-3.47638001000006,11.6,10.319727363));
#233834=CARTESIAN_POINT('Ctrl Pts',(-3.47809546500006,15.2,10.322005719));
#233835=CARTESIAN_POINT('Ctrl Pts',(-3.47809546500006,11.6,10.322005719));
#233836=CARTESIAN_POINT('Ctrl Pts',(-3.47981618900006,15.2,10.324287126));
#233837=CARTESIAN_POINT('Ctrl Pts',(-3.47981618900006,11.6,10.324287126));
#233838=CARTESIAN_POINT('Ctrl Pts',(-3.48154218300006,15.2,10.326571569));
#233839=CARTESIAN_POINT('Ctrl Pts',(-3.48154218300006,11.6,10.326571569));
#233840=CARTESIAN_POINT('Ctrl Pts',(-3.48327344600006,15.2,10.328859035));
#233841=CARTESIAN_POINT('Ctrl Pts',(-3.48327344600006,11.6,10.328859035));
#233842=CARTESIAN_POINT('Ctrl Pts',(-3.48500997900006,15.2,10.331149512));
#233843=CARTESIAN_POINT('Ctrl Pts',(-3.48500997900006,11.6,10.331149512));
#233844=CARTESIAN_POINT('Ctrl Pts',(-3.48675178200006,15.2,10.333442987));
#233845=CARTESIAN_POINT('Ctrl Pts',(-3.48675178200006,11.6,10.333442987));
#233846=CARTESIAN_POINT('Ctrl Pts',(-3.48849885700006,15.2,10.335739446));
#233847=CARTESIAN_POINT('Ctrl Pts',(-3.48849885700006,11.6,10.335739446));
#233848=CARTESIAN_POINT('Ctrl Pts',(-3.49025120200006,15.2,10.338038877));
#233849=CARTESIAN_POINT('Ctrl Pts',(-3.49025120200006,11.6,10.338038877));
#233850=CARTESIAN_POINT('Ctrl Pts',(-3.49200881900006,15.2,10.340341268));
#233851=CARTESIAN_POINT('Ctrl Pts',(-3.49200881900006,11.6,10.340341268));
#233852=CARTESIAN_POINT('Ctrl Pts',(-3.49377170500006,15.2,10.342646605));
#233853=CARTESIAN_POINT('Ctrl Pts',(-3.49377170500006,11.6,10.342646605));
#233854=CARTESIAN_POINT('Ctrl Pts',(-3.49553986400006,15.2,10.344954876));
#233855=CARTESIAN_POINT('Ctrl Pts',(-3.49553986400006,11.6,10.344954876));
#233856=CARTESIAN_POINT('Ctrl Pts',(-3.49731329400006,15.2,10.347266067));
#233857=CARTESIAN_POINT('Ctrl Pts',(-3.49731329400006,11.6,10.347266067));
#233858=CARTESIAN_POINT('Ctrl Pts',(-3.49909199600006,15.2,10.349580167));
#233859=CARTESIAN_POINT('Ctrl Pts',(-3.49909199600006,11.6,10.349580167));
#233860=CARTESIAN_POINT('Ctrl Pts',(-3.50087597000006,15.2,10.351897163));
#233861=CARTESIAN_POINT('Ctrl Pts',(-3.50087597000006,11.6,10.351897163));
#233862=CARTESIAN_POINT('Ctrl Pts',(-3.50266521700005,15.2,10.354217043));
#233863=CARTESIAN_POINT('Ctrl Pts',(-3.50266521700005,11.6,10.354217043));
#233864=CARTESIAN_POINT('Ctrl Pts',(-3.50445973500006,15.2,10.356539792));
#233865=CARTESIAN_POINT('Ctrl Pts',(-3.50445973500006,11.6,10.356539792));
#233866=CARTESIAN_POINT('Ctrl Pts',(-3.50625952600006,15.2,10.3588654));
#233867=CARTESIAN_POINT('Ctrl Pts',(-3.50625952600006,11.6,10.3588654));
#233868=CARTESIAN_POINT('Ctrl Pts',(-3.50806458900006,15.2,10.361193853));
#233869=CARTESIAN_POINT('Ctrl Pts',(-3.50806458900006,11.6,10.361193853));
#233870=CARTESIAN_POINT('Ctrl Pts',(-3.50987492600006,15.2,10.363525139));
#233871=CARTESIAN_POINT('Ctrl Pts',(-3.50987492600006,11.6,10.363525139));
#233872=CARTESIAN_POINT('Ctrl Pts',(-3.51169053400006,15.2,10.365859245));
#233873=CARTESIAN_POINT('Ctrl Pts',(-3.51169053400006,11.6,10.365859245));
#233874=CARTESIAN_POINT('Ctrl Pts',(-3.51351141600006,15.2,10.36819616));
#233875=CARTESIAN_POINT('Ctrl Pts',(-3.51351141600006,11.6,10.36819616));
#233876=CARTESIAN_POINT('Ctrl Pts',(-3.51533757100006,15.2,10.370535871));
#233877=CARTESIAN_POINT('Ctrl Pts',(-3.51533757100006,11.6,10.370535871));
#233878=CARTESIAN_POINT('Ctrl Pts',(-3.51716899900006,15.2,10.372878364));
#233879=CARTESIAN_POINT('Ctrl Pts',(-3.51716899900006,11.6,10.372878364));
#233880=CARTESIAN_POINT('Ctrl Pts',(-3.51900570000006,15.2,10.375223629));
#233881=CARTESIAN_POINT('Ctrl Pts',(-3.51900570000006,11.6,10.375223629));
#233882=CARTESIAN_POINT('Ctrl Pts',(-3.52084767500005,15.2,10.377571653));
#233883=CARTESIAN_POINT('Ctrl Pts',(-3.52084767500005,11.6,10.377571653));
#233884=CARTESIAN_POINT('Ctrl Pts',(-3.52269492200006,15.2,10.379922423));
#233885=CARTESIAN_POINT('Ctrl Pts',(-3.52269492200006,11.6,10.379922423));
#233886=CARTESIAN_POINT('Ctrl Pts',(-3.52454744400006,15.2,10.382275926));
#233887=CARTESIAN_POINT('Ctrl Pts',(-3.52454744400006,11.6,10.382275926));
#233888=CARTESIAN_POINT('Ctrl Pts',(-3.52640523800006,15.2,10.384632152));
#233889=CARTESIAN_POINT('Ctrl Pts',(-3.52640523800006,11.6,10.384632152));
#233890=CARTESIAN_POINT('Ctrl Pts',(-3.52826830500006,15.2,10.386991087));
#233891=CARTESIAN_POINT('Ctrl Pts',(-3.52826830500006,11.6,10.386991087));
#233892=CARTESIAN_POINT('Ctrl Pts',(-3.53013664600006,15.2,10.389352721));
#233893=CARTESIAN_POINT('Ctrl Pts',(-3.53013664600006,11.6,10.389352721));
#233894=CARTESIAN_POINT('Ctrl Pts',(-3.53201026100006,15.2,10.391717039));
#233895=CARTESIAN_POINT('Ctrl Pts',(-3.53201026100006,11.6,10.391717039));
#233896=CARTESIAN_POINT('Ctrl Pts',(-3.53388914900005,15.2,10.39408403));
#233897=CARTESIAN_POINT('Ctrl Pts',(-3.53388914900005,11.6,10.39408403));
#233898=CARTESIAN_POINT('Ctrl Pts',(-3.53577331100006,15.2,10.396453683));
#233899=CARTESIAN_POINT('Ctrl Pts',(-3.53577331100006,11.6,10.396453683));
#233900=CARTESIAN_POINT('Ctrl Pts',(-3.53766274500006,15.2,10.398825984));
#233901=CARTESIAN_POINT('Ctrl Pts',(-3.53766274500006,11.6,10.398825984));
#233902=CARTESIAN_POINT('Ctrl Pts',(-3.53955745300006,15.2,10.401200923));
#233903=CARTESIAN_POINT('Ctrl Pts',(-3.53955745300006,11.6,10.401200923));
#233904=CARTESIAN_POINT('Ctrl Pts',(-3.54145743500006,15.2,10.403578487));
#233905=CARTESIAN_POINT('Ctrl Pts',(-3.54145743500006,11.6,10.403578487));
#233906=CARTESIAN_POINT('Ctrl Pts',(-3.54336269000005,15.2,10.405958664));
#233907=CARTESIAN_POINT('Ctrl Pts',(-3.54336269000005,11.6,10.405958664));
#233908=CARTESIAN_POINT('Ctrl Pts',(-3.54527321800005,15.2,10.408341441));
#233909=CARTESIAN_POINT('Ctrl Pts',(-3.54527321800005,11.6,10.408341441));
#233910=CARTESIAN_POINT('Ctrl Pts',(-3.54718901800006,15.2,10.410726808));
#233911=CARTESIAN_POINT('Ctrl Pts',(-3.54718901800006,11.6,10.410726808));
#233912=CARTESIAN_POINT('Ctrl Pts',(-3.54911009300006,15.2,10.413114752));
#233913=CARTESIAN_POINT('Ctrl Pts',(-3.54911009300006,11.6,10.413114752));
#233914=CARTESIAN_POINT('Ctrl Pts',(-3.55103644000006,15.2,10.415505261));
#233915=CARTESIAN_POINT('Ctrl Pts',(-3.55103644000006,11.6,10.415505261));
#233916=CARTESIAN_POINT('Ctrl Pts',(-3.55296806000006,15.2,10.417898323));
#233917=CARTESIAN_POINT('Ctrl Pts',(-3.55296806000006,11.6,10.417898323));
#233918=CARTESIAN_POINT('Ctrl Pts',(-3.55490495300006,15.2,10.420293927));
#233919=CARTESIAN_POINT('Ctrl Pts',(-3.55490495300006,11.6,10.420293927));
#233920=CARTESIAN_POINT('Ctrl Pts',(-3.55684711800006,15.2,10.422692061));
#233921=CARTESIAN_POINT('Ctrl Pts',(-3.55684711800006,11.6,10.422692061));
#233922=CARTESIAN_POINT('Ctrl Pts',(-3.55879455700006,15.2,10.425092713));
#233923=CARTESIAN_POINT('Ctrl Pts',(-3.55879455700006,11.6,10.425092713));
#233924=CARTESIAN_POINT('Ctrl Pts',(-3.56074726700006,15.2,10.427495872));
#233925=CARTESIAN_POINT('Ctrl Pts',(-3.56074726700006,11.6,10.427495872));
#233926=CARTESIAN_POINT('Ctrl Pts',(-3.56270525100006,15.2,10.429901523));
#233927=CARTESIAN_POINT('Ctrl Pts',(-3.56270525100006,11.6,10.429901523));
#233928=CARTESIAN_POINT('Ctrl Pts',(-3.56466850500006,15.2,10.432309659));
#233929=CARTESIAN_POINT('Ctrl Pts',(-3.56466850500006,11.6,10.432309659));
#233930=CARTESIAN_POINT('Ctrl Pts',(-3.56663703300006,15.2,10.434720265));
#233931=CARTESIAN_POINT('Ctrl Pts',(-3.56663703300006,11.6,10.434720265));
#233932=CARTESIAN_POINT('Ctrl Pts',(-3.56861083200006,15.2,10.437133332));
#233933=CARTESIAN_POINT('Ctrl Pts',(-3.56861083200006,11.6,10.437133332));
#233934=CARTESIAN_POINT('Ctrl Pts',(-3.57058990200006,15.2,10.439548846));
#233935=CARTESIAN_POINT('Ctrl Pts',(-3.57058990200006,11.6,10.439548846));
#233936=CARTESIAN_POINT('Ctrl Pts',(-3.57257424400006,15.2,10.441966796));
#233937=CARTESIAN_POINT('Ctrl Pts',(-3.57257424400006,11.6,10.441966796));
#233938=CARTESIAN_POINT('Ctrl Pts',(-3.57456385800006,15.2,10.44438717));
#233939=CARTESIAN_POINT('Ctrl Pts',(-3.57456385800006,11.6,10.44438717));
#233940=CARTESIAN_POINT('Ctrl Pts',(-3.57655874300006,15.2,10.446809958));
#233941=CARTESIAN_POINT('Ctrl Pts',(-3.57655874300006,11.6,10.446809958));
#233942=CARTESIAN_POINT('Ctrl Pts',(-3.57855889700006,15.2,10.449235148));
#233943=CARTESIAN_POINT('Ctrl Pts',(-3.57855889700006,11.6,10.449235148));
#233944=CARTESIAN_POINT('Ctrl Pts',(-3.58056432400006,15.2,10.451662728));
#233945=CARTESIAN_POINT('Ctrl Pts',(-3.58056432400006,11.6,10.451662728));
#233946=CARTESIAN_POINT('Ctrl Pts',(-3.58257502000006,15.2,10.454092686));
#233947=CARTESIAN_POINT('Ctrl Pts',(-3.58257502000006,11.6,10.454092686));
#233948=CARTESIAN_POINT('Ctrl Pts',(-3.58459098700005,15.2,10.456525011));
#233949=CARTESIAN_POINT('Ctrl Pts',(-3.58459098700005,11.6,10.456525011));
#233950=CARTESIAN_POINT('Ctrl Pts',(-3.58661222400006,15.2,10.458959692));
#233951=CARTESIAN_POINT('Ctrl Pts',(-3.58661222400006,11.6,10.458959692));
#233952=CARTESIAN_POINT('Ctrl Pts',(-3.58863873100006,15.2,10.461396717));
#233953=CARTESIAN_POINT('Ctrl Pts',(-3.58863873100006,11.6,10.461396717));
#233954=CARTESIAN_POINT('Ctrl Pts',(-3.59067050700006,15.2,10.463836075));
#233955=CARTESIAN_POINT('Ctrl Pts',(-3.59067050700006,11.6,10.463836075));
#233956=CARTESIAN_POINT('Ctrl Pts',(-3.59270755300006,15.2,10.466277755));
#233957=CARTESIAN_POINT('Ctrl Pts',(-3.59270755300006,11.6,10.466277755));
#233958=CARTESIAN_POINT('Ctrl Pts',(-3.59474986600006,15.2,10.468721746));
#233959=CARTESIAN_POINT('Ctrl Pts',(-3.59474986600006,11.6,10.468721746));
#233960=CARTESIAN_POINT('Ctrl Pts',(-3.59679745000006,15.2,10.471168035));
#233961=CARTESIAN_POINT('Ctrl Pts',(-3.59679745000006,11.6,10.471168035));
#233962=CARTESIAN_POINT('Ctrl Pts',(-3.59885030100005,15.2,10.473616611));
#233963=CARTESIAN_POINT('Ctrl Pts',(-3.59885030100005,11.6,10.473616611));
#233964=CARTESIAN_POINT('Ctrl Pts',(-3.60090842000006,15.2,10.476067465));
#233965=CARTESIAN_POINT('Ctrl Pts',(-3.60090842000006,11.6,10.476067465));
#233966=CARTESIAN_POINT('Ctrl Pts',(-3.60297180800006,15.2,10.478520583));
#233967=CARTESIAN_POINT('Ctrl Pts',(-3.60297180800006,11.6,10.478520583));
#233968=CARTESIAN_POINT('Ctrl Pts',(-3.60504046200006,15.2,10.480975954));
#233969=CARTESIAN_POINT('Ctrl Pts',(-3.60504046200006,11.6,10.480975954));
#233970=CARTESIAN_POINT('Ctrl Pts',(-3.60711438400006,15.2,10.48343357));
#233971=CARTESIAN_POINT('Ctrl Pts',(-3.60711438400006,11.6,10.48343357));
#233972=CARTESIAN_POINT('Ctrl Pts',(-3.60919357400006,15.2,10.485893416));
#233973=CARTESIAN_POINT('Ctrl Pts',(-3.60919357400006,11.6,10.485893416));
#233974=CARTESIAN_POINT('Ctrl Pts',(-3.61127802800006,15.2,10.488355482));
#233975=CARTESIAN_POINT('Ctrl Pts',(-3.61127802800006,11.6,10.488355482));
#233976=CARTESIAN_POINT('Ctrl Pts',(-3.61336775000006,15.2,10.490819758));
#233977=CARTESIAN_POINT('Ctrl Pts',(-3.61336775000006,11.6,10.490819758));
#233978=CARTESIAN_POINT('Ctrl Pts',(-3.61546273700006,15.2,10.493286233));
#233979=CARTESIAN_POINT('Ctrl Pts',(-3.61546273700006,11.6,10.493286233));
#233980=CARTESIAN_POINT('Ctrl Pts',(-3.61756298900006,15.2,10.495754894));
#233981=CARTESIAN_POINT('Ctrl Pts',(-3.61756298900006,11.6,10.495754894));
#233982=CARTESIAN_POINT('Ctrl Pts',(-3.61966850700006,15.2,10.498225732));
#233983=CARTESIAN_POINT('Ctrl Pts',(-3.61966850700006,11.6,10.498225732));
#233984=CARTESIAN_POINT('Ctrl Pts',(-3.62177928800006,15.2,10.500698735));
#233985=CARTESIAN_POINT('Ctrl Pts',(-3.62177928800006,11.6,10.500698735));
#233986=CARTESIAN_POINT('Ctrl Pts',(-3.62389533500005,15.2,10.503173891));
#233987=CARTESIAN_POINT('Ctrl Pts',(-3.62389533500005,11.6,10.503173891));
#233988=CARTESIAN_POINT('Ctrl Pts',(-3.62601664500006,15.2,10.505651191));
#233989=CARTESIAN_POINT('Ctrl Pts',(-3.62601664500006,11.6,10.505651191));
#233990=CARTESIAN_POINT('Ctrl Pts',(-3.62814321900006,15.2,10.508130623));
#233991=CARTESIAN_POINT('Ctrl Pts',(-3.62814321900006,11.6,10.508130623));
#233992=CARTESIAN_POINT('Ctrl Pts',(-3.63027505500006,15.2,10.510612176));
#233993=CARTESIAN_POINT('Ctrl Pts',(-3.63027505500006,11.6,10.510612176));
#233994=CARTESIAN_POINT('Ctrl Pts',(-3.63241215500006,15.2,10.513095839));
#233995=CARTESIAN_POINT('Ctrl Pts',(-3.63241215500006,11.6,10.513095839));
#233996=CARTESIAN_POINT('Ctrl Pts',(-3.63455451700006,15.2,10.515581602));
#233997=CARTESIAN_POINT('Ctrl Pts',(-3.63455451700006,11.6,10.515581602));
#233998=CARTESIAN_POINT('Ctrl Pts',(-3.63670214100006,15.2,10.518069453));
#233999=CARTESIAN_POINT('Ctrl Pts',(-3.63670214100006,11.6,10.518069453));
#234000=CARTESIAN_POINT('Ctrl Pts',(-3.63885502600006,15.2,10.520559382));
#234001=CARTESIAN_POINT('Ctrl Pts',(-3.63885502600006,11.6,10.520559382));
#234002=CARTESIAN_POINT('Ctrl Pts',(-3.64101317200006,15.2,10.523051378));
#234003=CARTESIAN_POINT('Ctrl Pts',(-3.64101317200006,11.6,10.523051378));
#234004=CARTESIAN_POINT('Ctrl Pts',(-3.64317657800005,15.2,10.525545429));
#234005=CARTESIAN_POINT('Ctrl Pts',(-3.64317657800005,11.6,10.525545429));
#234006=CARTESIAN_POINT('Ctrl Pts',(-3.64534524400006,15.2,10.528041525));
#234007=CARTESIAN_POINT('Ctrl Pts',(-3.64534524400006,11.6,10.528041525));
#234008=CARTESIAN_POINT('Ctrl Pts',(-3.64751916900006,15.2,10.530539657));
#234009=CARTESIAN_POINT('Ctrl Pts',(-3.64751916900006,11.6,10.530539657));
#234010=CARTESIAN_POINT('Ctrl Pts',(-3.64969835400006,15.2,10.533039813));
#234011=CARTESIAN_POINT('Ctrl Pts',(-3.64969835400006,11.6,10.533039813));
#234012=CARTESIAN_POINT('Ctrl Pts',(-3.65188279700006,15.2,10.53554198));
#234013=CARTESIAN_POINT('Ctrl Pts',(-3.65188279700006,11.6,10.53554198));
#234014=CARTESIAN_POINT('Ctrl Pts',(-3.65407249900006,15.2,10.538046151));
#234015=CARTESIAN_POINT('Ctrl Pts',(-3.65407249900006,11.6,10.538046151));
#234016=CARTESIAN_POINT('Ctrl Pts',(-3.65626745700006,15.2,10.540552313));
#234017=CARTESIAN_POINT('Ctrl Pts',(-3.65626745700006,11.6,10.540552313));
#234018=CARTESIAN_POINT('Ctrl Pts',(-3.65846767300006,15.2,10.543060457));
#234019=CARTESIAN_POINT('Ctrl Pts',(-3.65846767300006,11.6,10.543060457));
#234020=CARTESIAN_POINT('Ctrl Pts',(-3.66067314500006,15.2,10.54557057));
#234021=CARTESIAN_POINT('Ctrl Pts',(-3.66067314500006,11.6,10.54557057));
#234022=CARTESIAN_POINT('Ctrl Pts',(-3.66288387400005,15.2,10.548082643));
#234023=CARTESIAN_POINT('Ctrl Pts',(-3.66288387400005,11.6,10.548082643));
#234024=CARTESIAN_POINT('Ctrl Pts',(-3.66509985800006,15.2,10.550596665));
#234025=CARTESIAN_POINT('Ctrl Pts',(-3.66509985800006,11.6,10.550596665));
#234026=CARTESIAN_POINT('Ctrl Pts',(-3.66732109600005,15.2,10.553112627));
#234027=CARTESIAN_POINT('Ctrl Pts',(-3.66732109600005,11.6,10.553112627));
#234028=CARTESIAN_POINT('Ctrl Pts',(-3.66954759000006,15.2,10.555630515));
#234029=CARTESIAN_POINT('Ctrl Pts',(-3.66954759000006,11.6,10.555630515));
#234030=CARTESIAN_POINT('Ctrl Pts',(-3.67177933600006,15.2,10.558150322));
#234031=CARTESIAN_POINT('Ctrl Pts',(-3.67177933600006,11.6,10.558150322));
#234032=CARTESIAN_POINT('Ctrl Pts',(-3.67401633700006,15.2,10.560672036));
#234033=CARTESIAN_POINT('Ctrl Pts',(-3.67401633700006,11.6,10.560672036));
#234034=CARTESIAN_POINT('Ctrl Pts',(-3.67625858900006,15.2,10.563195645));
#234035=CARTESIAN_POINT('Ctrl Pts',(-3.67625858900006,11.6,10.563195645));
#234036=CARTESIAN_POINT('Ctrl Pts',(-3.67850609400006,15.2,10.565721141));
#234037=CARTESIAN_POINT('Ctrl Pts',(-3.67850609400006,11.6,10.565721141));
#234038=CARTESIAN_POINT('Ctrl Pts',(-3.68075885100006,15.2,10.568248513));
#234039=CARTESIAN_POINT('Ctrl Pts',(-3.68075885100006,11.6,10.568248513));
#234040=CARTESIAN_POINT('Ctrl Pts',(-3.68301685900006,15.2,10.570777751));
#234041=CARTESIAN_POINT('Ctrl Pts',(-3.68301685900006,11.6,10.570777751));
#234042=CARTESIAN_POINT('Ctrl Pts',(-3.68528011600006,15.2,10.573308843));
#234043=CARTESIAN_POINT('Ctrl Pts',(-3.68528011600006,11.6,10.573308843));
#234044=CARTESIAN_POINT('Ctrl Pts',(-3.68754862400006,15.2,10.575841779));
#234045=CARTESIAN_POINT('Ctrl Pts',(-3.68754862400006,11.6,10.575841779));
#234046=CARTESIAN_POINT('Ctrl Pts',(-3.68982238000005,15.2,10.57837655));
#234047=CARTESIAN_POINT('Ctrl Pts',(-3.68982238000005,11.6,10.57837655));
#234048=CARTESIAN_POINT('Ctrl Pts',(-3.69210138500006,15.2,10.580913144));
#234049=CARTESIAN_POINT('Ctrl Pts',(-3.69210138500006,11.6,10.580913144));
#234050=CARTESIAN_POINT('Ctrl Pts',(-3.69438563800006,15.2,10.583451552));
#234051=CARTESIAN_POINT('Ctrl Pts',(-3.69438563800006,11.6,10.583451552));
#234052=CARTESIAN_POINT('Ctrl Pts',(-3.69667513900006,15.2,10.585991762));
#234053=CARTESIAN_POINT('Ctrl Pts',(-3.69667513900006,11.6,10.585991762));
#234054=CARTESIAN_POINT('Ctrl Pts',(-3.69896988600006,15.2,10.588533766));
#234055=CARTESIAN_POINT('Ctrl Pts',(-3.69896988600006,11.6,10.588533766));
#234056=CARTESIAN_POINT('Ctrl Pts',(-3.70126987900006,15.2,10.591077552));
#234057=CARTESIAN_POINT('Ctrl Pts',(-3.70126987900006,11.6,10.591077552));
#234058=CARTESIAN_POINT('Ctrl Pts',(-3.70357511700006,15.2,10.593623111));
#234059=CARTESIAN_POINT('Ctrl Pts',(-3.70357511700006,11.6,10.593623111));
#234060=CARTESIAN_POINT('Ctrl Pts',(-3.70588560000006,15.2,10.596170432));
#234061=CARTESIAN_POINT('Ctrl Pts',(-3.70588560000006,11.6,10.596170432));
#234062=CARTESIAN_POINT('Ctrl Pts',(-3.70820132700006,15.2,10.598719505));
#234063=CARTESIAN_POINT('Ctrl Pts',(-3.70820132700006,11.6,10.598719505));
#234064=CARTESIAN_POINT('Ctrl Pts',(-3.71052229700005,15.2,10.60127032));
#234065=CARTESIAN_POINT('Ctrl Pts',(-3.71052229700005,11.6,10.60127032));
#234066=CARTESIAN_POINT('Ctrl Pts',(-3.71284850900006,15.2,10.603822866));
#234067=CARTESIAN_POINT('Ctrl Pts',(-3.71284850900006,11.6,10.603822866));
#234068=CARTESIAN_POINT('Ctrl Pts',(-3.71517996400006,15.2,10.606377133));
#234069=CARTESIAN_POINT('Ctrl Pts',(-3.71517996400006,11.6,10.606377133));
#234070=CARTESIAN_POINT('Ctrl Pts',(-3.71751666100006,15.2,10.608933113));
#234071=CARTESIAN_POINT('Ctrl Pts',(-3.71751666100006,11.6,10.608933113));
#234072=CARTESIAN_POINT('Ctrl Pts',(-3.71985859700006,15.2,10.611490792));
#234073=CARTESIAN_POINT('Ctrl Pts',(-3.71985859700006,11.6,10.611490792));
#234074=CARTESIAN_POINT('Ctrl Pts',(-3.72220577200006,15.2,10.614050164));
#234075=CARTESIAN_POINT('Ctrl Pts',(-3.72220577200006,11.6,10.614050164));
#234076=CARTESIAN_POINT('Ctrl Pts',(-3.72455818800006,15.2,10.616611217));
#234077=CARTESIAN_POINT('Ctrl Pts',(-3.72455818800006,11.6,10.616611217));
#234078=CARTESIAN_POINT('Ctrl Pts',(-3.72691584200005,15.2,10.619173941));
#234079=CARTESIAN_POINT('Ctrl Pts',(-3.72691584200005,11.6,10.619173941));
#234080=CARTESIAN_POINT('Ctrl Pts',(-3.72927873300006,15.2,10.621738325));
#234081=CARTESIAN_POINT('Ctrl Pts',(-3.72927873300006,11.6,10.621738325));
#234082=CARTESIAN_POINT('Ctrl Pts',(-3.73164686200006,15.2,10.624304361));
#234083=CARTESIAN_POINT('Ctrl Pts',(-3.73164686200006,11.6,10.624304361));
#234084=CARTESIAN_POINT('Ctrl Pts',(-3.73402022600006,15.2,10.626872037));
#234085=CARTESIAN_POINT('Ctrl Pts',(-3.73402022600006,11.6,10.626872037));
#234086=CARTESIAN_POINT('Ctrl Pts',(-3.73639882600005,15.2,10.629441345));
#234087=CARTESIAN_POINT('Ctrl Pts',(-3.73639882600005,11.6,10.629441345));
#234088=CARTESIAN_POINT('Ctrl Pts',(-3.73878266100006,15.2,10.632012275));
#234089=CARTESIAN_POINT('Ctrl Pts',(-3.73878266100006,11.6,10.632012275));
#234090=CARTESIAN_POINT('Ctrl Pts',(-3.74117172900006,15.2,10.634584815));
#234091=CARTESIAN_POINT('Ctrl Pts',(-3.74117172900006,11.6,10.634584815));
#234092=CARTESIAN_POINT('Ctrl Pts',(-3.74356603100006,15.2,10.637158957));
#234093=CARTESIAN_POINT('Ctrl Pts',(-3.74356603100006,11.6,10.637158957));
#234094=CARTESIAN_POINT('Ctrl Pts',(-3.74596556400006,15.2,10.63973469));
#234095=CARTESIAN_POINT('Ctrl Pts',(-3.74596556400006,11.6,10.63973469));
#234096=CARTESIAN_POINT('Ctrl Pts',(-3.74837033000006,15.2,10.642312005));
#234097=CARTESIAN_POINT('Ctrl Pts',(-3.74837033000006,11.6,10.642312005));
#234098=CARTESIAN_POINT('Ctrl Pts',(-3.75078032700006,15.2,10.644890891));
#234099=CARTESIAN_POINT('Ctrl Pts',(-3.75078032700006,11.6,10.644890891));
#234100=CARTESIAN_POINT('Ctrl Pts',(-3.75319555300006,15.2,10.647471339));
#234101=CARTESIAN_POINT('Ctrl Pts',(-3.75319555300006,11.6,10.647471339));
#234102=CARTESIAN_POINT('Ctrl Pts',(-3.75561600800006,15.2,10.650053339));
#234103=CARTESIAN_POINT('Ctrl Pts',(-3.75561600800006,11.6,10.650053339));
#234104=CARTESIAN_POINT('Ctrl Pts',(-3.75804169300006,15.2,10.652636882));
#234105=CARTESIAN_POINT('Ctrl Pts',(-3.75804169300006,11.6,10.652636882));
#234106=CARTESIAN_POINT('Ctrl Pts',(-3.76047260500005,15.2,10.655221957));
#234107=CARTESIAN_POINT('Ctrl Pts',(-3.76047260500005,11.6,10.655221957));
#234108=CARTESIAN_POINT('Ctrl Pts',(-3.76290874200006,15.2,10.657808555));
#234109=CARTESIAN_POINT('Ctrl Pts',(-3.76290874200006,11.6,10.657808555));
#234110=CARTESIAN_POINT('Ctrl Pts',(-3.76535010600006,15.2,10.660396666));
#234111=CARTESIAN_POINT('Ctrl Pts',(-3.76535010600006,11.6,10.660396666));
#234112=CARTESIAN_POINT('Ctrl Pts',(-3.76779669600006,15.2,10.66298628));
#234113=CARTESIAN_POINT('Ctrl Pts',(-3.76779669600006,11.6,10.66298628));
#234114=CARTESIAN_POINT('Ctrl Pts',(-3.77024850900006,15.2,10.665577388));
#234115=CARTESIAN_POINT('Ctrl Pts',(-3.77024850900006,11.6,10.665577388));
#234116=CARTESIAN_POINT('Ctrl Pts',(-3.77270554500006,15.2,10.66816998));
#234117=CARTESIAN_POINT('Ctrl Pts',(-3.77270554500006,11.6,10.66816998));
#234118=CARTESIAN_POINT('Ctrl Pts',(-3.77516780600006,15.2,10.670764045));
#234119=CARTESIAN_POINT('Ctrl Pts',(-3.77516780600006,11.6,10.670764045));
#234120=CARTESIAN_POINT('Ctrl Pts',(-3.77763528700005,15.2,10.673359576));
#234121=CARTESIAN_POINT('Ctrl Pts',(-3.77763528700005,11.6,10.673359576));
#234122=CARTESIAN_POINT('Ctrl Pts',(-3.78010798800006,15.2,10.67595656));
#234123=CARTESIAN_POINT('Ctrl Pts',(-3.78010798800006,11.6,10.67595656));
#234124=CARTESIAN_POINT('Ctrl Pts',(-3.78258591000006,15.2,10.678554992));
#234125=CARTESIAN_POINT('Ctrl Pts',(-3.78258591000006,11.6,10.678554992));
#234126=CARTESIAN_POINT('Ctrl Pts',(-3.78506905100005,15.2,10.681154858));
#234127=CARTESIAN_POINT('Ctrl Pts',(-3.78506905100005,11.6,10.681154858));
#234128=CARTESIAN_POINT('Ctrl Pts',(-3.78755741000006,15.2,10.68375615));
#234129=CARTESIAN_POINT('Ctrl Pts',(-3.78755741000006,11.6,10.68375615));
#234130=CARTESIAN_POINT('Ctrl Pts',(-3.79005098600006,15.2,10.686358859));
#234131=CARTESIAN_POINT('Ctrl Pts',(-3.79005098600006,11.6,10.686358859));
#234132=CARTESIAN_POINT('Ctrl Pts',(-3.79254977900006,15.2,10.688962975));
#234133=CARTESIAN_POINT('Ctrl Pts',(-3.79254977900006,11.6,10.688962975));
#234134=CARTESIAN_POINT('Ctrl Pts',(-3.79505378700006,15.2,10.691568489));
#234135=CARTESIAN_POINT('Ctrl Pts',(-3.79505378700006,11.6,10.691568489));
#234136=CARTESIAN_POINT('Ctrl Pts',(-3.79756300900006,15.2,10.69417539));
#234137=CARTESIAN_POINT('Ctrl Pts',(-3.79756300900006,11.6,10.69417539));
#234138=CARTESIAN_POINT('Ctrl Pts',(-3.80007744600006,15.2,10.696783671));
#234139=CARTESIAN_POINT('Ctrl Pts',(-3.80007744600006,11.6,10.696783671));
#234140=CARTESIAN_POINT('Ctrl Pts',(-3.80259709500006,15.2,10.69939332));
#234141=CARTESIAN_POINT('Ctrl Pts',(-3.80259709500006,11.6,10.69939332));
#234142=CARTESIAN_POINT('Ctrl Pts',(-3.80512195600006,15.2,10.702004329));
#234143=CARTESIAN_POINT('Ctrl Pts',(-3.80512195600006,11.6,10.702004329));
#234144=CARTESIAN_POINT('Ctrl Pts',(-3.80765202800006,15.2,10.704616688));
#234145=CARTESIAN_POINT('Ctrl Pts',(-3.80765202800006,11.6,10.704616688));
#234146=CARTESIAN_POINT('Ctrl Pts',(-3.81018731000006,15.2,10.707230387));
#234147=CARTESIAN_POINT('Ctrl Pts',(-3.81018731000006,11.6,10.707230387));
#234148=CARTESIAN_POINT('Ctrl Pts',(-3.81272780000006,15.2,10.709845418));
#234149=CARTESIAN_POINT('Ctrl Pts',(-3.81272780000006,11.6,10.709845418));
#234150=CARTESIAN_POINT('Ctrl Pts',(-3.81527349900006,15.2,10.712461771));
#234151=CARTESIAN_POINT('Ctrl Pts',(-3.81527349900006,11.6,10.712461771));
#234152=CARTESIAN_POINT('Ctrl Pts',(-3.81782440500006,15.2,10.715079436));
#234153=CARTESIAN_POINT('Ctrl Pts',(-3.81782440500006,11.6,10.715079436));
#234154=CARTESIAN_POINT('Ctrl Pts',(-3.82038051600006,15.2,10.717698406));
#234155=CARTESIAN_POINT('Ctrl Pts',(-3.82038051600006,11.6,10.717698406));
#234156=CARTESIAN_POINT('Ctrl Pts',(-3.82294183300006,15.2,10.720318668));
#234157=CARTESIAN_POINT('Ctrl Pts',(-3.82294183300006,11.6,10.720318668));
#234158=CARTESIAN_POINT('Ctrl Pts',(-3.82550835500005,15.2,10.722940216));
#234159=CARTESIAN_POINT('Ctrl Pts',(-3.82550835500005,11.6,10.722940216));
#234160=CARTESIAN_POINT('Ctrl Pts',(-3.82808007900006,15.2,10.725563037));
#234161=CARTESIAN_POINT('Ctrl Pts',(-3.82808007900006,11.6,10.725563037));
#234162=CARTESIAN_POINT('Ctrl Pts',(-3.83065700500006,15.2,10.728187127));
#234163=CARTESIAN_POINT('Ctrl Pts',(-3.83065700500006,11.6,10.728187127));
#234164=CARTESIAN_POINT('Ctrl Pts',(-3.83323913400006,15.2,10.730812472));
#234165=CARTESIAN_POINT('Ctrl Pts',(-3.83323913400006,11.6,10.730812472));
#234166=CARTESIAN_POINT('Ctrl Pts',(-3.83582646100006,15.2,10.733439064));
#234167=CARTESIAN_POINT('Ctrl Pts',(-3.83582646100006,11.6,10.733439064));
#234168=CARTESIAN_POINT('Ctrl Pts',(-3.83841898900006,15.2,10.736066894));
#234169=CARTESIAN_POINT('Ctrl Pts',(-3.83841898900006,11.6,10.736066894));
#234170=CARTESIAN_POINT('Ctrl Pts',(-3.84101671400006,15.2,10.738695954));
#234171=CARTESIAN_POINT('Ctrl Pts',(-3.84101671400006,11.6,10.738695954));
#234172=CARTESIAN_POINT('Ctrl Pts',(-3.84361963500006,15.2,10.741326232));
#234173=CARTESIAN_POINT('Ctrl Pts',(-3.84361963500006,11.6,10.741326232));
#234174=CARTESIAN_POINT('Ctrl Pts',(-3.84622775400006,15.2,10.743957722));
#234175=CARTESIAN_POINT('Ctrl Pts',(-3.84622775400006,11.6,10.743957722));
#234176=CARTESIAN_POINT('Ctrl Pts',(-3.84884106800006,15.2,10.746590414));
#234177=CARTESIAN_POINT('Ctrl Pts',(-3.84884106800006,11.6,10.746590414));
#234178=CARTESIAN_POINT('Ctrl Pts',(-3.85145957500006,15.2,10.749224298));
#234179=CARTESIAN_POINT('Ctrl Pts',(-3.85145957500006,11.6,10.749224298));
#234180=CARTESIAN_POINT('Ctrl Pts',(-3.85408327600006,15.2,10.751859366));
#234181=CARTESIAN_POINT('Ctrl Pts',(-3.85408327600006,11.6,10.751859366));
#234182=CARTESIAN_POINT('Ctrl Pts',(-3.85671217000006,15.2,10.754495608));
#234183=CARTESIAN_POINT('Ctrl Pts',(-3.85671217000006,11.6,10.754495608));
#234184=CARTESIAN_POINT('Ctrl Pts',(-3.85934625300006,15.2,10.757133016));
#234185=CARTESIAN_POINT('Ctrl Pts',(-3.85934625300006,11.6,10.757133016));
#234186=CARTESIAN_POINT('Ctrl Pts',(-3.86198552700006,15.2,10.759771578));
#234187=CARTESIAN_POINT('Ctrl Pts',(-3.86198552700006,11.6,10.759771578));
#234188=CARTESIAN_POINT('Ctrl Pts',(-3.86462998900006,15.2,10.762411286));
#234189=CARTESIAN_POINT('Ctrl Pts',(-3.86462998900006,11.6,10.762411286));
#234190=CARTESIAN_POINT('Ctrl Pts',(-3.86727963900006,15.2,10.765052131));
#234191=CARTESIAN_POINT('Ctrl Pts',(-3.86727963900006,11.6,10.765052131));
#234192=CARTESIAN_POINT('Ctrl Pts',(-3.86993447500006,15.2,10.767694103));
#234193=CARTESIAN_POINT('Ctrl Pts',(-3.86993447500006,11.6,10.767694103));
#234194=CARTESIAN_POINT('Ctrl Pts',(-3.87259449700006,15.2,10.770337195));
#234195=CARTESIAN_POINT('Ctrl Pts',(-3.87259449700006,11.6,10.770337195));
#234196=CARTESIAN_POINT('Ctrl Pts',(-3.87525970400006,15.2,10.772981399));
#234197=CARTESIAN_POINT('Ctrl Pts',(-3.87525970400006,11.6,10.772981399));
#234198=CARTESIAN_POINT('Ctrl Pts',(-3.87793009300006,15.2,10.775626704));
#234199=CARTESIAN_POINT('Ctrl Pts',(-3.87793009300006,11.6,10.775626704));
#234200=CARTESIAN_POINT('Ctrl Pts',(-3.88060566700006,15.2,10.778273105));
#234201=CARTESIAN_POINT('Ctrl Pts',(-3.88060566700006,11.6,10.778273105));
#234202=CARTESIAN_POINT('Ctrl Pts',(-3.88328642000006,15.2,10.780920592));
#234203=CARTESIAN_POINT('Ctrl Pts',(-3.88328642000006,11.6,10.780920592));
#234204=CARTESIAN_POINT('Ctrl Pts',(-3.88597235500006,15.2,10.783569156));
#234205=CARTESIAN_POINT('Ctrl Pts',(-3.88597235500006,11.6,10.783569156));
#234206=CARTESIAN_POINT('Ctrl Pts',(-3.88866346800006,15.2,10.786218787));
#234207=CARTESIAN_POINT('Ctrl Pts',(-3.88866346800006,11.6,10.786218787));
#234208=CARTESIAN_POINT('Ctrl Pts',(-3.89135975900006,15.2,10.788869473));
#234209=CARTESIAN_POINT('Ctrl Pts',(-3.89135975900006,11.6,10.788869473));
#234210=CARTESIAN_POINT('Ctrl Pts',(-3.89406122700006,15.2,10.791521203));
#234211=CARTESIAN_POINT('Ctrl Pts',(-3.89406122700006,11.6,10.791521203));
#234212=CARTESIAN_POINT('Ctrl Pts',(-3.89676786900006,15.2,10.794173967));
#234213=CARTESIAN_POINT('Ctrl Pts',(-3.89676786900006,11.6,10.794173967));
#234214=CARTESIAN_POINT('Ctrl Pts',(-3.89947968600006,15.2,10.796827755));
#234215=CARTESIAN_POINT('Ctrl Pts',(-3.89947968600006,11.6,10.796827755));
#234216=CARTESIAN_POINT('Ctrl Pts',(-3.90219667500006,15.2,10.79948256));
#234217=CARTESIAN_POINT('Ctrl Pts',(-3.90219667500006,11.6,10.79948256));
#234218=CARTESIAN_POINT('Ctrl Pts',(-3.90491883500006,15.2,10.802138374));
#234219=CARTESIAN_POINT('Ctrl Pts',(-3.90491883500006,11.6,10.802138374));
#234220=CARTESIAN_POINT('Ctrl Pts',(-3.90764616700006,15.2,10.804795194));
#234221=CARTESIAN_POINT('Ctrl Pts',(-3.90764616700006,11.6,10.804795194));
#234222=CARTESIAN_POINT('Ctrl Pts',(-3.91037867000006,15.2,10.807453019));
#234223=CARTESIAN_POINT('Ctrl Pts',(-3.91037867000006,11.6,10.807453019));
#234224=CARTESIAN_POINT('Ctrl Pts',(-3.91256880800006,15.2,10.80958008));
#234225=CARTESIAN_POINT('Ctrl Pts',(-3.91256880800006,11.6,10.80958008));
#234226=CARTESIAN_POINT('Ctrl Pts',(-3.91421373900006,15.2,10.811175828));
#234227=CARTESIAN_POINT('Ctrl Pts',(-3.91421373900006,11.6,10.811175828));
#234228=CARTESIAN_POINT('Ctrl Pts',(-3.91531139400006,15.2,10.81223986));
#234229=CARTESIAN_POINT('Ctrl Pts',(-3.91531139400006,11.6,10.81223986));
#234230=CARTESIAN_POINT('Ctrl Pts',(-3.91586047900006,15.2,10.812771925));
#234231=CARTESIAN_POINT('Ctrl Pts',(-3.91586047900006,11.6,10.812771925));
#234232=CARTESIAN_POINT('Ctrl Pts',(-3.20199116200006,15.2,9.86852965799999));
#234233=CARTESIAN_POINT('Ctrl Pts',(-3.20268658144428,15.2,9.87017541023993));
#234234=CARTESIAN_POINT('Ctrl Pts',(-3.20340918557853,15.2,9.8718717538802));
#234235=CARTESIAN_POINT('Ctrl Pts',(-3.20415921061787,15.2,9.87361750383371));
#234236=CARTESIAN_POINT('Ctrl Pts',(-3.20491285265707,15.2,9.87537167267594));
#234237=CARTESIAN_POINT('Ctrl Pts',(-3.20569417615054,15.2,9.87717573954122));
#234238=CARTESIAN_POINT('Ctrl Pts',(-3.20650339032002,15.2,9.87902857865426));
#234239=CARTESIAN_POINT('Ctrl Pts',(-3.207312604416,15.2,9.880881417599));
#234240=CARTESIAN_POINT('Ctrl Pts',(-3.20814971002311,15.2,9.88278302787072));
#234241=CARTESIAN_POINT('Ctrl Pts',(-3.20901491174167,15.2,9.88473231696656));
#234242=CARTESIAN_POINT('Ctrl Pts',(-3.20988011346024,15.2,9.88668160606242));
#234243=CARTESIAN_POINT('Ctrl Pts',(-3.21077340886668,15.2,9.88867857418553));
#234244=CARTESIAN_POINT('Ctrl Pts',(-3.21169499187759,15.2,9.89072215729398));
#234245=CARTESIAN_POINT('Ctrl Pts',(-3.2126165749722,15.2,9.89276574058806));
#234246=CARTESIAN_POINT('Ctrl Pts',(-3.21356644777639,15.2,9.89485593812154));
#234247=CARTESIAN_POINT('Ctrl Pts',(-3.21454479458166,15.2,9.89699171649106));
#234248=CARTESIAN_POINT('Ctrl Pts',(-3.21552314129806,15.2,9.89912749466659));
#234249=CARTESIAN_POINT('Ctrl Pts',(-3.21652996004167,15.2,9.9013088547466));
#234250=CARTESIAN_POINT('Ctrl Pts',(-3.21756543175881,15.2,9.90353478725925));
#234251=CARTESIAN_POINT('Ctrl Pts',(-3.21860090347595,15.2,9.9057607197719));
#234252=CARTESIAN_POINT('Ctrl Pts',(-3.21966502620654,15.2,9.90803122612666));
#234253=CARTESIAN_POINT('Ctrl Pts',(-3.22075797091556,15.2,9.91034532737397));
#234254=CARTESIAN_POINT('Ctrl Pts',(-3.22185091572386,15.2,9.91265942883149));
#234255=CARTESIAN_POINT('Ctrl Pts',(-3.22297268097742,15.2,9.91501712290282));
#234256=CARTESIAN_POINT('Ctrl Pts',(-3.22412343087545,15.2,9.91741745478656));
#234257=CARTESIAN_POINT('Ctrl Pts',(-3.22527418066896,15.2,9.91981778645227));
#234258=CARTESIAN_POINT('Ctrl Pts',(-3.22645391675033,15.2,9.92226075792395));
#234259=CARTESIAN_POINT('Ctrl Pts',(-3.22766278962435,15.2,9.92474543566884));
#234260=CARTESIAN_POINT('Ctrl Pts',(-3.22887166249837,15.2,9.92723011341373));
#234261=CARTESIAN_POINT('Ctrl Pts',(-3.23010967588672,15.2,9.9297564981219));
#234262=CARTESIAN_POINT('Ctrl Pts',(-3.23137697842272,15.2,9.93232368186017));
#234263=CARTESIAN_POINT('Ctrl Pts',(-3.23264428095873,15.2,9.93489086559843));
#234264=CARTESIAN_POINT('Ctrl Pts',(-3.23394087148897,15.2,9.93749884804353));
#234265=CARTESIAN_POINT('Ctrl Pts',(-3.23526689310548,15.2,9.94014674294464));
#234266=CARTESIAN_POINT('Ctrl Pts',(-3.23659291484242,15.2,9.94279463808627));
#234267=CARTESIAN_POINT('Ctrl Pts',(-3.23794836809883,15.2,9.94548244670671));
#234268=CARTESIAN_POINT('Ctrl Pts',(-3.23933338784228,15.2,9.94820930194036));
#234269=CARTESIAN_POINT('Ctrl Pts',(-3.24071840745992,15.2,9.95093615692632));
#234270=CARTESIAN_POINT('Ctrl Pts',(-3.24213299364533,15.2,9.95370206081286));
#234271=CARTESIAN_POINT('Ctrl Pts',(-3.24357727726601,15.2,9.95650616497364));
#234272=CARTESIAN_POINT('Ctrl Pts',(-3.2450215608867,15.2,9.95931026913442));
#234273=CARTESIAN_POINT('Ctrl Pts',(-3.24649554203443,15.2,9.96215257803488));
#234274=CARTESIAN_POINT('Ctrl Pts',(-3.2479993435611,15.2,9.96503226217771));
#234275=CARTESIAN_POINT('Ctrl Pts',(-3.24950314522436,15.2,9.96791194658211));
#234276=CARTESIAN_POINT('Ctrl Pts',(-3.25103676978215,15.2,9.97082900819847));
#234277=CARTESIAN_POINT('Ctrl Pts',(-3.25260033336868,15.2,9.97378263869438));
#234278=CARTESIAN_POINT('Ctrl Pts',(-3.25416389681318,15.2,9.97673626892201));
#234279=CARTESIAN_POINT('Ctrl Pts',(-3.25575739994263,15.2,9.97972647059485));
#234280=CARTESIAN_POINT('Ctrl Pts',(-3.25738095647427,15.2,9.98275245099855));
#234281=CARTESIAN_POINT('Ctrl Pts',(-3.2592751058595,15.2,9.98628276165277));
#234282=CARTESIAN_POINT('Ctrl Pts',(-3.26121016215456,15.2,9.98986177345009));
#234283=CARTESIAN_POINT('Ctrl Pts',(-3.26318629436744,15.2,9.99348826166115));
#234284=CARTESIAN_POINT('Ctrl Pts',(-3.26488012189057,15.2,9.99659667996642));
#234285=CARTESIAN_POINT('Ctrl Pts',(-3.26660412830504,15.2,9.99973998038289));
#234286=CARTESIAN_POINT('Ctrl Pts',(-3.26835841574921,15.2,10.0029174077818));
#234287=CARTESIAN_POINT('Ctrl Pts',(-3.27011270319338,15.2,10.0060948351807));
#234288=CARTESIAN_POINT('Ctrl Pts',(-3.27189727326186,15.2,10.0093063905831));
#234289=CARTESIAN_POINT('Ctrl Pts',(-3.27371221977718,15.2,10.0125513371296));
#234290=CARTESIAN_POINT('Ctrl Pts',(-3.27552716645736,15.2,10.0157962839708));
#234291=CARTESIAN_POINT('Ctrl Pts',(-3.27737249207549,15.2,10.0190746216309));
#234292=CARTESIAN_POINT('Ctrl Pts',(-3.27924828868987,15.2,10.022385629562));
#234293=CARTESIAN_POINT('Ctrl Pts',(-3.28112408513387,15.2,10.0256966371923));
#234294=CARTESIAN_POINT('Ctrl Pts',(-3.28303035277037,15.2,10.0290403113476));
#234295=CARTESIAN_POINT('Ctrl Pts',(-3.28496717903333,15.2,10.0324159479749));
#234296=CARTESIAN_POINT('Ctrl Pts',(-3.28690400529629,15.2,10.0357915846023));
#234297=CARTESIAN_POINT('Ctrl Pts',(-3.28887139188969,15.2,10.0391991836307));
#234298=CARTESIAN_POINT('Ctrl Pts',(-3.29086942033179,15.2,10.0426380494257));
#234299=CARTESIAN_POINT('Ctrl Pts',(-3.29253444409405,15.2,10.0455037710257));
#234300=CARTESIAN_POINT('Ctrl Pts',(-3.29422074766736,15.2,10.0483912065221));
#234301=CARTESIAN_POINT('Ctrl Pts',(-3.29592837718012,15.2,10.0512999622848));
#234302=CARTESIAN_POINT('Ctrl Pts',(-3.29763600669288,15.2,10.0542087180476));
#234303=CARTESIAN_POINT('Ctrl Pts',(-3.29936496202567,15.2,10.0571387952304));
#234304=CARTESIAN_POINT('Ctrl Pts',(-3.30111528813566,15.2,10.0600898027987));
#234305=CARTESIAN_POINT('Ctrl Pts',(-3.30286561424566,15.2,10.0630408103671));
#234306=CARTESIAN_POINT('Ctrl Pts',(-3.3046373103465,15.2,10.0660127511514));
#234307=CARTESIAN_POINT('Ctrl Pts',(-3.3064304189657,15.2,10.0690052419983));
#234308=CARTESIAN_POINT('Ctrl Pts',(-3.3082235275849,15.2,10.0719977328452));
#234309=CARTESIAN_POINT('Ctrl Pts',(-3.31003804933333,15.2,10.0750107746777));
#234310=CARTESIAN_POINT('Ctrl Pts',(-3.31187402225,15.2,10.0780439912749));
#234311=CARTESIAN_POINT('Ctrl Pts',(-3.31370999516666,15.2,10.0810772078721));
#234312=CARTESIAN_POINT('Ctrl Pts',(-3.31556742195911,15.2,10.0841305979709));
#234313=CARTESIAN_POINT('Ctrl Pts',(-3.31744634050936,15.2,10.0872037954849));
#234314=CARTESIAN_POINT('Ctrl Pts',(-3.31932525905961,15.2,10.0902769929989));
#234315=CARTESIAN_POINT('Ctrl Pts',(-3.32122566964693,15.2,10.0933699945971));
#234316=CARTESIAN_POINT('Ctrl Pts',(-3.32314760742583,15.2,10.0964824386953));
#234317=CARTESIAN_POINT('Ctrl Pts',(-3.32506954520472,15.2,10.0995948827935));
#234318=CARTESIAN_POINT('Ctrl Pts',(-3.3270130109442,15.2,10.1027267661829));
#234319=CARTESIAN_POINT('Ctrl Pts',(-3.32897804032031,15.2,10.1058777329895));
#234320=CARTESIAN_POINT('Ctrl Pts',(-3.33094306969641,15.2,10.109028699796));
#234321=CARTESIAN_POINT('Ctrl Pts',(-3.33292966250359,15.2,10.1121987499762));
#234322=CARTESIAN_POINT('Ctrl Pts',(-3.33493785121653,15.2,10.1153875286785));
#234323=CARTESIAN_POINT('Ctrl Pts',(-3.33694603992947,15.2,10.1185763073808));
#234324=CARTESIAN_POINT('Ctrl Pts',(-3.33897582562212,15.2,10.1217838150371));
#234325=CARTESIAN_POINT('Ctrl Pts',(-3.341027239235,15.2,10.1250097044136));
#234326=CARTESIAN_POINT('Ctrl Pts',(-3.34307865284788,15.2,10.12823559379));
#234327=CARTESIAN_POINT('Ctrl Pts',(-3.34515169463332,15.2,10.1314798639918));
#234328=CARTESIAN_POINT('Ctrl Pts',(-3.347246394774,15.2,10.13474217191));
#234329=CARTESIAN_POINT('Ctrl Pts',(-3.34934109468635,15.2,10.1380044794726));
#234330=CARTESIAN_POINT('Ctrl Pts',(-3.35145745234407,15.2,10.1412848267573));
#234331=CARTESIAN_POINT('Ctrl Pts',(-3.35359549717868,15.2,10.1445828725769));
#234332=CARTESIAN_POINT('Ctrl Pts',(-3.35573354224635,15.2,10.147880918756));
#234333=CARTESIAN_POINT('Ctrl Pts',(-3.35789327309978,15.2,10.1511966652487));
#234334=CARTESIAN_POINT('Ctrl Pts',(-3.36007471747301,15.2,10.154529778789));
#234335=CARTESIAN_POINT('Ctrl Pts',(-3.36225616184624,15.2,10.1578628923292));
#234336=CARTESIAN_POINT('Ctrl Pts',(-3.36445931938858,15.2,10.1612133721887));
#234337=CARTESIAN_POINT('Ctrl Pts',(-3.36668421619232,15.2,10.1645808900345));
#234338=CARTESIAN_POINT('Ctrl Pts',(-3.36890911299606,15.2,10.1679484078802));
#234339=CARTESIAN_POINT('Ctrl Pts',(-3.37115574774714,15.2,10.1713329633753));
#234340=CARTESIAN_POINT('Ctrl Pts',(-3.37342414626175,15.2,10.1747342338218));
#234341=CARTESIAN_POINT('Ctrl Pts',(-3.37569254477636,15.2,10.1781355042684));
#234342=CARTESIAN_POINT('Ctrl Pts',(-3.37798270410007,15.2,10.1815534888374));
#234343=CARTESIAN_POINT('Ctrl Pts',(-3.38029464930727,15.2,10.1849878675171));
#234344=CARTESIAN_POINT('Ctrl Pts',(-3.38260659451446,15.2,10.1884222461968));
#234345=CARTESIAN_POINT('Ctrl Pts',(-3.38494032557501,15.2,10.1918730190686));
#234346=CARTESIAN_POINT('Ctrl Pts',(-3.38729586154608,15.2,10.1953398710816));
#234347=CARTESIAN_POINT('Ctrl Pts',(-3.38918029042563,15.2,10.1981133528432));
#234348=CARTESIAN_POINT('Ctrl Pts',(-3.39107867605716,15.2,10.2008971257044));
#234349=CARTESIAN_POINT('Ctrl Pts',(-3.39299102653591,15.2,10.2036910291637));
#234350=CARTESIAN_POINT('Ctrl Pts',(-3.39538146450407,15.2,10.2071834082976));
#234351=CARTESIAN_POINT('Ctrl Pts',(-3.39779372467773,15.2,10.2106916181818));
#234352=CARTESIAN_POINT('Ctrl Pts',(-3.40022782481839,15.2,10.2142153495025));
#234353=CARTESIAN_POINT('Ctrl Pts',(-3.40217510477173,15.2,10.2170343343286));
#234354=CARTESIAN_POINT('Ctrl Pts',(-3.40413636253717,15.2,10.219863254359));
#234355=CARTESIAN_POINT('Ctrl Pts',(-3.40611160709699,15.2,10.222701951293));
#234356=CARTESIAN_POINT('Ctrl Pts',(-3.40808685192593,15.2,10.2255406486137));
#234357=CARTESIAN_POINT('Ctrl Pts',(-3.41007608329694,15.2,10.2283891251486));
#234358=CARTESIAN_POINT('Ctrl Pts',(-3.41207930950743,15.2,10.2312472264481));
#234359=CARTESIAN_POINT('Ctrl Pts',(-3.41408253544497,15.2,10.234105327358));
#234360=CARTESIAN_POINT('Ctrl Pts',(-3.41609975603161,15.2,10.2369730519368));
#234361=CARTESIAN_POINT('Ctrl Pts',(-3.41813097880908,15.2,10.2398502487565));
#234362=CARTESIAN_POINT('Ctrl Pts',(-3.42016220186329,15.2,10.2427274459682));
#234363=CARTESIAN_POINT('Ctrl Pts',(-3.42220742876644,15.2,10.2456141148395));
#234364=CARTESIAN_POINT('Ctrl Pts',(-3.42426666543514,15.2,10.2485101042201));
#234365=CARTESIAN_POINT('Ctrl Pts',(-3.42632590182327,15.2,10.2514060932062));
#234366=CARTESIAN_POINT('Ctrl Pts',(-3.42839914693979,15.2,10.2543114037067));
#234367=CARTESIAN_POINT('Ctrl Pts',(-3.43048640970553,15.2,10.2572258860021));
#234368=CARTESIAN_POINT('Ctrl Pts',(-3.43257367275567,15.2,10.2601403686946));
#234369=CARTESIAN_POINT('Ctrl Pts',(-3.43467495285964,15.2,10.2630640229044));
#234370=CARTESIAN_POINT('Ctrl Pts',(-3.43679025569806,15.2,10.2659967002314));
#234371=CARTESIAN_POINT('Ctrl Pts',(-3.43890555824827,15.2,10.268929377159));
#234372=CARTESIAN_POINT('Ctrl Pts',(-3.44103488396512,15.2,10.271871077618));
#234373=CARTESIAN_POINT('Ctrl Pts',(-3.44317823789957,15.2,10.2748216552092));
#234374=CARTESIAN_POINT('Ctrl Pts',(-3.44532159212606,15.2,10.2777722332024));
#234375=CARTESIAN_POINT('Ctrl Pts',(-3.44747897605656,15.2,10.2807316891739));
#234376=CARTESIAN_POINT('Ctrl Pts',(-3.44965039351815,15.2,10.2836998759603));
#234377=CARTESIAN_POINT('Ctrl Pts',(-3.45345037392799,15.2,10.2888942026342));
#234378=CARTESIAN_POINT('Ctrl Pts',(-3.45729333318342,15.2,10.294115273107));
#234379=CARTESIAN_POINT('Ctrl Pts',(-3.46117929807973,15.2,10.2993623177318));
#234380=CARTESIAN_POINT('Ctrl Pts',(-3.46339984923295,15.2,10.3023606286542));
#234381=CARTESIAN_POINT('Ctrl Pts',(-3.4656344423705,15.2,10.3053674211172));
#234382=CARTESIAN_POINT('Ctrl Pts',(-3.46788308157464,15.2,10.3083825535369));
#234383=CARTESIAN_POINT('Ctrl Pts',(-3.47181820056487,15.2,10.3136590357848));
#234384=CARTESIAN_POINT('Ctrl Pts',(-3.47579633560707,15.2,10.3189610629039));
#234385=CARTESIAN_POINT('Ctrl Pts',(-3.47981750667132,15.2,10.3242878852655));
#234386=CARTESIAN_POINT('Ctrl Pts',(-3.4821153184844,15.2,10.3273317834617));
#234387=CARTESIAN_POINT('Ctrl Pts',(-3.4844271811113,15.2,10.3303837782117));
#234388=CARTESIAN_POINT('Ctrl Pts',(-3.48675309958638,15.2,10.3334437325163));
#234389=CARTESIAN_POINT('Ctrl Pts',(-3.48907901837838,15.2,10.3365036872378));
#234390=CARTESIAN_POINT('Ctrl Pts',(-3.49141899295146,15.2,10.3395716010815));
#234391=CARTESIAN_POINT('Ctrl Pts',(-3.49377302320161,15.2,10.3426473384854));
#234392=CARTESIAN_POINT('Ctrl Pts',(-3.49671556085393,15.2,10.3464920100307));
#234393=CARTESIAN_POINT('Ctrl Pts',(-3.49968006414432,15.2,10.3503489047802));
#234394=CARTESIAN_POINT('Ctrl Pts',(-3.50266653497879,15.2,10.3542177605447));
#234395=CARTESIAN_POINT('Ctrl Pts',(-3.50505571145104,15.2,10.3573128449033));
#234396=CARTESIAN_POINT('Ctrl Pts',(-3.50745894693715,15.2,10.3604155837631));
#234397=CARTESIAN_POINT('Ctrl Pts',(-3.50987624340478,15.2,10.3635258435081));
#234398=CARTESIAN_POINT('Ctrl Pts',(-3.51229354020176,15.2,10.3666361036768));
#234399=CARTESIAN_POINT('Ctrl Pts',(-3.51472489772667,15.2,10.3697538860703));
#234400=CARTESIAN_POINT('Ctrl Pts',(-3.51717031726001,15.2,10.3728790569771));
#234401=CARTESIAN_POINT('Ctrl Pts',(-3.51961573646016,15.2,10.3760042274581));
#234402=CARTESIAN_POINT('Ctrl Pts',(-3.52207521794367,15.2,10.3791367884607));
#234403=CARTESIAN_POINT('Ctrl Pts',(-3.52454876162892,15.2,10.3822766062033));
#234404=CARTESIAN_POINT('Ctrl Pts',(-3.52764069148824,15.2,10.3862013787023));
#234405=CARTESIAN_POINT('Ctrl Pts',(-3.5307545921361,15.2,10.3901374933624));
#234406=CARTESIAN_POINT('Ctrl Pts',(-3.53389046706483,15.2,10.3940846949587));
#234407=CARTESIAN_POINT('Ctrl Pts',(-3.53702634199355,15.2,10.3980318965549));
#234408=CARTESIAN_POINT('Ctrl Pts',(-3.54018418873035,15.2,10.4019901867706));
#234409=CARTESIAN_POINT('Ctrl Pts',(-3.54336400782575,15.2,10.4059593135058));
#234410=CARTESIAN_POINT('Ctrl Pts',(-3.54654382692116,15.2,10.409928440241));
#234411=CARTESIAN_POINT('Ctrl Pts',(-3.54974561694407,15.2,10.413908404427));
#234412=CARTESIAN_POINT('Ctrl Pts',(-3.55296937786751,15.2,10.4178989580284));
#234413=CARTESIAN_POINT('Ctrl Pts',(-3.55619313879095,15.2,10.4218895116298));
#234414=CARTESIAN_POINT('Ctrl Pts',(-3.55943887002089,15.2,10.4258906562826));
#234415=CARTESIAN_POINT('Ctrl Pts',(-3.5627065683531,15.2,10.429902143921));
#234416=CARTESIAN_POINT('Ctrl Pts',(-3.56532072716133,15.2,10.4331113342066));
#234417=CARTESIAN_POINT('Ctrl Pts',(-3.56794894534067,15.2,10.4363271470235));
#234418=CARTESIAN_POINT('Ctrl Pts',(-3.5705912202078,15.2,10.4395494552551));
#234419=CARTESIAN_POINT('Ctrl Pts',(-3.57323349471492,15.2,10.4427717630476));
#234420=CARTESIAN_POINT('Ctrl Pts',(-3.57588982754871,15.2,10.4460005664673));
#234421=CARTESIAN_POINT('Ctrl Pts',(-3.57856021479592,15.2,10.4492357450305));
#234422=CARTESIAN_POINT('Ctrl Pts',(-3.58123060240697,15.2,10.4524709240346));
#234423=CARTESIAN_POINT('Ctrl Pts',(-3.58391504561995,15.2,10.4557124753742));
#234424=CARTESIAN_POINT('Ctrl Pts',(-3.58661354171241,15.2,10.4589602782739));
#234425=CARTESIAN_POINT('Ctrl Pts',(-3.58931203743721,15.2,10.462208080731));
#234426=CARTESIAN_POINT('Ctrl Pts',(-3.59202458546188,15.2,10.4654621349174));
#234427=CARTESIAN_POINT('Ctrl Pts',(-3.59475118323754,15.2,10.4687223199836));
#234428=CARTESIAN_POINT('Ctrl Pts',(-3.5974777813847,15.2,10.471982505494));
#234429=CARTESIAN_POINT('Ctrl Pts',(-3.60021842976976,15.2,10.4752488211395));
#234430=CARTESIAN_POINT('Ctrl Pts',(-3.60297312454355,15.2,10.4785211462772));
#234431=CARTESIAN_POINT('Ctrl Pts',(-3.60572781894201,15.2,10.481793470969));
#234432=CARTESIAN_POINT('Ctrl Pts',(-3.6084965606601,15.2,10.4850718073905));
#234433=CARTESIAN_POINT('Ctrl Pts',(-3.61127934448668,15.2,10.4883560339547));
#234434=CARTESIAN_POINT('Ctrl Pts',(-3.61475782455427,15.2,10.4924613174955));
#234435=CARTESIAN_POINT('Ctrl Pts',(-3.61825824732444,15.2,10.4965758083614));
#234436=CARTESIAN_POINT('Ctrl Pts',(-3.62178060398928,15.2,10.5006992727356));
#234437=CARTESIAN_POINT('Ctrl Pts',(-3.62459848947474,15.2,10.5039980444148));
#234438=CARTESIAN_POINT('Ctrl Pts',(-3.62743041346721,15.2,10.5073025604818));
#234439=CARTESIAN_POINT('Ctrl Pts',(-3.63027637096861,15.2,10.5106127035106));
#234440=CARTESIAN_POINT('Ctrl Pts',(-3.63383381765147,15.2,10.514750382071));
#234441=CARTESIAN_POINT('Ctrl Pts',(-3.63741319397896,15.2,10.5188968543991));
#234442=CARTESIAN_POINT('Ctrl Pts',(-3.641014487244,15.2,10.5230518920384));
#234443=CARTESIAN_POINT('Ctrl Pts',(-3.6438955216205,15.2,10.5263759218782));
#234444=CARTESIAN_POINT('Ctrl Pts',(-3.64679058301087,15.2,10.529705434639));
#234445=CARTESIAN_POINT('Ctrl Pts',(-3.64969966804937,15.2,10.5330403152547));
#234446=CARTESIAN_POINT('Ctrl Pts',(-3.65406329620166,15.2,10.5380426368598));
#234447=CARTESIAN_POINT('Ctrl Pts',(-3.65845847497241,15.2,10.5430570368939));
#234448=CARTESIAN_POINT('Ctrl Pts',(-3.66288518818665,15.2,10.5480831307529));
#234449=CARTESIAN_POINT('Ctrl Pts',(-3.66509854459271,15.2,10.5505961774541));
#234450=CARTESIAN_POINT('Ctrl Pts',(-3.66731978342341,15.2,10.5531121483658));
#234451=CARTESIAN_POINT('Ctrl Pts',(-3.66954890330144,15.2,10.5556309949829));
#234452=CARTESIAN_POINT('Ctrl Pts',(-3.67177802317947,15.2,10.5581498416));
#234453=CARTESIAN_POINT('Ctrl Pts',(-3.67401502376491,15.2,10.5606715651084));
#234454=CARTESIAN_POINT('Ctrl Pts',(-3.676259902225,15.2,10.563196116725));
#234455=CARTESIAN_POINT('Ctrl Pts',(-3.6785047806851,15.2,10.5657206683416));
#234456=CARTESIAN_POINT('Ctrl Pts',(-3.6807575386199,15.2,10.5682480502498));
#234457=CARTESIAN_POINT('Ctrl Pts',(-3.68301817103705,15.2,10.5707782142409));
#234458=CARTESIAN_POINT('Ctrl Pts',(-3.6852788034542,15.2,10.573308378232));
#234459=CARTESIAN_POINT('Ctrl Pts',(-3.6875473112629,15.2,10.5758413236252));
#234460=CARTESIAN_POINT('Ctrl Pts',(-3.68982369179299,15.2,10.5783770052844));
#234461=CARTESIAN_POINT('Ctrl Pts',(-3.69210007232306,15.2,10.5809126869436));
#234462=CARTESIAN_POINT('Ctrl Pts',(-3.6943843261847,15.2,10.5834511038387));
#234463=CARTESIAN_POINT('Ctrl Pts',(-3.69667645001699,15.2,10.5859922099127));
#234464=CARTESIAN_POINT('Ctrl Pts',(-3.69896857426568,15.2,10.5885333164482));
#234465=CARTESIAN_POINT('Ctrl Pts',(-3.70126856794999,15.2,10.591077112568));
#234466=CARTESIAN_POINT('Ctrl Pts',(-3.70357642874479,15.2,10.5936235520634));
#234467=CARTESIAN_POINT('Ctrl Pts',(-3.70588428912032,15.2,10.5961699910962));
#234468=CARTESIAN_POINT('Ctrl Pts',(-3.70820001685382,15.2,10.598719073504));
#234469=CARTESIAN_POINT('Ctrl Pts',(-3.71052360777007,15.2,10.6012707530365));
#234470=CARTESIAN_POINT('Ctrl Pts',(-3.71284719868632,15.2,10.603822432569));
#234471=CARTESIAN_POINT('Ctrl Pts',(-3.71517865447647,15.2,10.6063767092336));
#234472=CARTESIAN_POINT('Ctrl Pts',(-3.71751797077713,15.2,10.608933537819));
#234473=CARTESIAN_POINT('Ctrl Pts',(-3.7214168314199,15.2,10.6131949189494));
#234474=CARTESIAN_POINT('Ctrl Pts',(-3.72533752619572,15.2,10.6174633896348));
#234475=CARTESIAN_POINT('Ctrl Pts',(-3.72928004272464,15.2,10.6217387382463));
#234476=CARTESIAN_POINT('Ctrl Pts',(-3.73164555255604,15.2,10.62430394732));
#234477=CARTESIAN_POINT('Ctrl Pts',(-3.73401891745318,15.2,10.6268716324934));
#234478=CARTESIAN_POINT('Ctrl Pts',(-3.73640013474166,15.2,10.6294417504833));
#234479=CARTESIAN_POINT('Ctrl Pts',(-3.73878135203014,15.2,10.6320118684733));
#234480=CARTESIAN_POINT('Ctrl Pts',(-3.74117042115997,15.2,10.6345844179131));
#234481=CARTESIAN_POINT('Ctrl Pts',(-3.74356733853053,15.2,10.637159354486));
#234482=CARTESIAN_POINT('Ctrl Pts',(-3.74596425590109,15.2,10.6397342910589));
#234483=CARTESIAN_POINT('Ctrl Pts',(-3.74836902235136,15.2,10.6423116147494));
#234484=CARTESIAN_POINT('Ctrl Pts',(-3.75078163379996,15.2,10.6448912809926));
#234485=CARTESIAN_POINT('Ctrl Pts',(-3.75319424524857,15.2,10.6474709472357));
#234486=CARTESIAN_POINT('Ctrl Pts',(-3.7556147010266,15.2,10.6500529563808));
#234487=CARTESIAN_POINT('Ctrl Pts',(-3.75804299922897,15.2,10.6526372644532));
#234488=CARTESIAN_POINT('Ctrl Pts',(-3.76128073045955,15.2,10.6560830088629));
#234489=CARTESIAN_POINT('Ctrl Pts',(-3.76453239976366,15.2,10.6595328396923));
#234490=CARTESIAN_POINT('Ctrl Pts',(-3.767798001775,15.2,10.6629866534916));
#234491=CARTESIAN_POINT('Ctrl Pts',(-3.77024720306104,15.2,10.6655770136059));
#234492=CARTESIAN_POINT('Ctrl Pts',(-3.7727042400717,15.2,10.668169614095));
#234493=CARTESIAN_POINT('Ctrl Pts',(-3.77516911077313,15.2,10.6707644111672));
#234494=CARTESIAN_POINT('Ctrl Pts',(-3.77845560534022,15.2,10.674224140911));
#234495=CARTESIAN_POINT('Ctrl Pts',(-3.78175602236732,15.2,10.6776877768637));
#234496=CARTESIAN_POINT('Ctrl Pts',(-3.78507035577107,15.2,10.6811552147751));
#234497=CARTESIAN_POINT('Ctrl Pts',(-3.7875561055981,15.2,10.6837557929725));
#234498=CARTESIAN_POINT('Ctrl Pts',(-3.7900496824651,15.2,10.6863585104018));
#234499=CARTESIAN_POINT('Ctrl Pts',(-3.79255108276061,15.2,10.6889633244857));
#234500=CARTESIAN_POINT('Ctrl Pts',(-3.79672008340459,15.2,10.6933046814498));
#234501=CARTESIAN_POINT('Ctrl Pts',(-3.80091081499673,15.2,10.6976518615066));
#234502=CARTESIAN_POINT('Ctrl Pts',(-3.80512325902562,15.2,10.7020046667847));
#234503=CARTESIAN_POINT('Ctrl Pts',(-3.80765072535113,15.2,10.7046163498566));
#234504=CARTESIAN_POINT('Ctrl Pts',(-3.81018600785905,15.2,10.7072300574283));
#234505=CARTESIAN_POINT('Ctrl Pts',(-3.81272910222501,15.2,10.7098457485));
#234506=CARTESIAN_POINT('Ctrl Pts',(-3.81527219659096,15.2,10.7124614395716));
#234507=CARTESIAN_POINT('Ctrl Pts',(-3.81782310329824,15.2,10.7150791136598));
#234508=CARTESIAN_POINT('Ctrl Pts',(-3.82038181720456,15.2,10.7176987287728));
#234509=CARTESIAN_POINT('Ctrl Pts',(-3.82294053111088,15.2,10.7203183438857));
#234510=CARTESIAN_POINT('Ctrl Pts',(-3.8255070539345,15.2,10.7229398988736));
#234511=CARTESIAN_POINT('Ctrl Pts',(-3.82808137901035,15.2,10.7255633536591));
#234512=CARTESIAN_POINT('Ctrl Pts',(-3.83065570408619,15.2,10.7281868084446));
#234513=CARTESIAN_POINT('Ctrl Pts',(-3.8332378332639,15.2,10.7308121627396));
#234514=CARTESIAN_POINT('Ctrl Pts',(-3.83582776062707,15.2,10.7334393729356));
#234515=CARTESIAN_POINT('Ctrl Pts',(-3.83841768846073,15.2,10.7360665836088));
#234516=CARTESIAN_POINT('Ctrl Pts',(-3.8410154146883,15.2,10.7386956518243));
#234517=CARTESIAN_POINT('Ctrl Pts',(-3.84362093502635,15.2,10.7413265355402));
#234518=CARTESIAN_POINT('Ctrl Pts',(-3.84622645489106,15.2,10.7439574187782));
#234519=CARTESIAN_POINT('Ctrl Pts',(-3.84883976986375,15.2,10.7465901191161));
#234520=CARTESIAN_POINT('Ctrl Pts',(-3.85146087376917,15.2,10.7492245942705));
#234521=CARTESIAN_POINT('Ctrl Pts',(-3.85408197767459,15.2,10.7518590694249));
#234522=CARTESIAN_POINT('Ctrl Pts',(-3.85671087233616,15.2,10.7544953204529));
#234523=CARTESIAN_POINT('Ctrl Pts',(-3.85934755071074,15.2,10.7571333045357));
#234524=CARTESIAN_POINT('Ctrl Pts',(-3.86286312171717,15.2,10.7606506164864));
#234525=CARTESIAN_POINT('Ctrl Pts',(-3.86639253259233,15.2,10.7641710075372));
#234526=CARTESIAN_POINT('Ctrl Pts',(-3.86993577091234,15.2,10.7676943824156));
#234527=CARTESIAN_POINT('Ctrl Pts',(-3.87259320025582,15.2,10.7703369141744));
#234528=CARTESIAN_POINT('Ctrl Pts',(-3.87525840799319,15.2,10.7729811257754));
#234529=CARTESIAN_POINT('Ctrl Pts',(-3.87793138975772,15.2,10.7756269785351));
#234530=CARTESIAN_POINT('Ctrl Pts',(-3.88060437103665,15.2,10.7782728308142));
#234531=CARTESIAN_POINT('Ctrl Pts',(-3.88328512609018,15.2,10.7809203265349));
#234532=CARTESIAN_POINT('Ctrl Pts',(-3.88597364982652,15.2,10.7835694230221));
#234533=CARTESIAN_POINT('Ctrl Pts',(-3.89045452288323,15.2,10.7879845839946));
#234534=CARTESIAN_POINT('Ctrl Pts',(-3.89495697459219,15.2,10.7924041830756));
#234535=CARTESIAN_POINT('Ctrl Pts',(-3.89948097954192,15.2,10.7968280097552));
#234536=CARTESIAN_POINT('Ctrl Pts',(-3.90219538241314,15.2,10.7994823056665));
#234537=CARTESIAN_POINT('Ctrl Pts',(-3.90491754275119,15.2,10.8021381233159));
#234538=CARTESIAN_POINT('Ctrl Pts',(-3.90764746004228,15.2,10.8047954455155));
#234539=CARTESIAN_POINT('Ctrl Pts',(-3.91037737733337,15.2,10.8074527677151));
#234540=CARTESIAN_POINT('Ctrl Pts',(-3.91311505247005,15.2,10.8101115985174));
#234541=CARTESIAN_POINT('Ctrl Pts',(-3.91586047900006,15.2,10.812771925));
#234542=CARTESIAN_POINT('Ctrl Pts',(-3.20199116200006,12.2,9.86852965799999));
#234543=CARTESIAN_POINT('Ctrl Pts',(-3.20268658144428,12.2,9.87017541023993));
#234544=CARTESIAN_POINT('Ctrl Pts',(-3.20340918557853,12.2,9.8718717538802));
#234545=CARTESIAN_POINT('Ctrl Pts',(-3.20415921061787,12.2,9.87361750383371));
#234546=CARTESIAN_POINT('Ctrl Pts',(-3.20491285265707,12.2,9.87537167267594));
#234547=CARTESIAN_POINT('Ctrl Pts',(-3.20569417615054,12.2,9.87717573954122));
#234548=CARTESIAN_POINT('Ctrl Pts',(-3.20650339032002,12.2,9.87902857865426));
#234549=CARTESIAN_POINT('Ctrl Pts',(-3.207312604416,12.2,9.880881417599));
#234550=CARTESIAN_POINT('Ctrl Pts',(-3.20814971002311,12.2,9.88278302787072));
#234551=CARTESIAN_POINT('Ctrl Pts',(-3.20901491174167,12.2,9.88473231696656));
#234552=CARTESIAN_POINT('Ctrl Pts',(-3.20988011346024,12.2,9.88668160606242));
#234553=CARTESIAN_POINT('Ctrl Pts',(-3.21077340886668,12.2,9.88867857418553));
#234554=CARTESIAN_POINT('Ctrl Pts',(-3.21169499187759,12.2,9.89072215729398));
#234555=CARTESIAN_POINT('Ctrl Pts',(-3.2126165749722,12.2,9.89276574058806));
#234556=CARTESIAN_POINT('Ctrl Pts',(-3.21356644777639,12.2,9.89485593812154));
#234557=CARTESIAN_POINT('Ctrl Pts',(-3.21454479458166,12.2,9.89699171649106));
#234558=CARTESIAN_POINT('Ctrl Pts',(-3.21552314129806,12.2,9.89912749466659));
#234559=CARTESIAN_POINT('Ctrl Pts',(-3.21652996004167,12.2,9.9013088547466));
#234560=CARTESIAN_POINT('Ctrl Pts',(-3.21756543175881,12.2,9.90353478725925));
#234561=CARTESIAN_POINT('Ctrl Pts',(-3.21860090347595,12.2,9.9057607197719));
#234562=CARTESIAN_POINT('Ctrl Pts',(-3.21966502620654,12.2,9.90803122612666));
#234563=CARTESIAN_POINT('Ctrl Pts',(-3.22075797091556,12.2,9.91034532737397));
#234564=CARTESIAN_POINT('Ctrl Pts',(-3.22185091572386,12.2,9.91265942883149));
#234565=CARTESIAN_POINT('Ctrl Pts',(-3.22297268097742,12.2,9.91501712290282));
#234566=CARTESIAN_POINT('Ctrl Pts',(-3.22412343087545,12.2,9.91741745478656));
#234567=CARTESIAN_POINT('Ctrl Pts',(-3.22527418066896,12.2,9.91981778645227));
#234568=CARTESIAN_POINT('Ctrl Pts',(-3.22645391675033,12.2,9.92226075792395));
#234569=CARTESIAN_POINT('Ctrl Pts',(-3.22766278962434,12.2,9.92474543566884));
#234570=CARTESIAN_POINT('Ctrl Pts',(-3.22887166249836,12.2,9.92723011341373));
#234571=CARTESIAN_POINT('Ctrl Pts',(-3.23010967588672,12.2,9.9297564981219));
#234572=CARTESIAN_POINT('Ctrl Pts',(-3.23137697842272,12.2,9.93232368186017));
#234573=CARTESIAN_POINT('Ctrl Pts',(-3.23264428095873,12.2,9.93489086559843));
#234574=CARTESIAN_POINT('Ctrl Pts',(-3.23394087148897,12.2,9.93749884804353));
#234575=CARTESIAN_POINT('Ctrl Pts',(-3.23526689310548,12.2,9.94014674294464));
#234576=CARTESIAN_POINT('Ctrl Pts',(-3.23659291484242,12.2,9.94279463808627));
#234577=CARTESIAN_POINT('Ctrl Pts',(-3.23794836809883,12.2,9.94548244670671));
#234578=CARTESIAN_POINT('Ctrl Pts',(-3.23933338784228,12.2,9.94820930194037));
#234579=CARTESIAN_POINT('Ctrl Pts',(-3.24071840745992,12.2,9.95093615692632));
#234580=CARTESIAN_POINT('Ctrl Pts',(-3.24213299364532,12.2,9.95370206081285));
#234581=CARTESIAN_POINT('Ctrl Pts',(-3.243577277266,12.2,9.95650616497363));
#234582=CARTESIAN_POINT('Ctrl Pts',(-3.24502156088669,12.2,9.9593102691344));
#234583=CARTESIAN_POINT('Ctrl Pts',(-3.24649554203443,12.2,9.96215257803488));
#234584=CARTESIAN_POINT('Ctrl Pts',(-3.2479993435611,12.2,9.96503226217771));
#234585=CARTESIAN_POINT('Ctrl Pts',(-3.24950314522436,12.2,9.96791194658211));
#234586=CARTESIAN_POINT('Ctrl Pts',(-3.25103676978215,12.2,9.97082900819847));
#234587=CARTESIAN_POINT('Ctrl Pts',(-3.25260033336868,12.2,9.97378263869438));
#234588=CARTESIAN_POINT('Ctrl Pts',(-3.25416389681318,12.2,9.97673626892201));
#234589=CARTESIAN_POINT('Ctrl Pts',(-3.25575739994263,12.2,9.97972647059485));
#234590=CARTESIAN_POINT('Ctrl Pts',(-3.25738095647427,12.2,9.98275245099855));
#234591=CARTESIAN_POINT('Ctrl Pts',(-3.2592751058595,12.2,9.98628276165277));
#234592=CARTESIAN_POINT('Ctrl Pts',(-3.26121016215456,12.2,9.98986177345009));
#234593=CARTESIAN_POINT('Ctrl Pts',(-3.26318629436744,12.2,9.99348826166115));
#234594=CARTESIAN_POINT('Ctrl Pts',(-3.26488012189057,12.2,9.99659667996642));
#234595=CARTESIAN_POINT('Ctrl Pts',(-3.26660412830504,12.2,9.99973998038289));
#234596=CARTESIAN_POINT('Ctrl Pts',(-3.26835841574921,12.2,10.0029174077818));
#234597=CARTESIAN_POINT('Ctrl Pts',(-3.27011270319338,12.2,10.0060948351807));
#234598=CARTESIAN_POINT('Ctrl Pts',(-3.27189727326186,12.2,10.0093063905831));
#234599=CARTESIAN_POINT('Ctrl Pts',(-3.27371221977718,12.2,10.0125513371296));
#234600=CARTESIAN_POINT('Ctrl Pts',(-3.27552716645736,12.2,10.0157962839708));
#234601=CARTESIAN_POINT('Ctrl Pts',(-3.27737249207549,12.2,10.0190746216309));
#234602=CARTESIAN_POINT('Ctrl Pts',(-3.27924828868987,12.2,10.022385629562));
#234603=CARTESIAN_POINT('Ctrl Pts',(-3.28112408513387,12.2,10.0256966371923));
#234604=CARTESIAN_POINT('Ctrl Pts',(-3.28303035277036,12.2,10.0290403113476));
#234605=CARTESIAN_POINT('Ctrl Pts',(-3.28496717903332,12.2,10.0324159479749));
#234606=CARTESIAN_POINT('Ctrl Pts',(-3.28690400529629,12.2,10.0357915846023));
#234607=CARTESIAN_POINT('Ctrl Pts',(-3.28887139188969,12.2,10.0391991836307));
#234608=CARTESIAN_POINT('Ctrl Pts',(-3.29086942033179,12.2,10.0426380494257));
#234609=CARTESIAN_POINT('Ctrl Pts',(-3.29253444409405,12.2,10.0455037710257));
#234610=CARTESIAN_POINT('Ctrl Pts',(-3.29422074766736,12.2,10.0483912065221));
#234611=CARTESIAN_POINT('Ctrl Pts',(-3.29592837718012,12.2,10.0512999622848));
#234612=CARTESIAN_POINT('Ctrl Pts',(-3.29763600669288,12.2,10.0542087180476));
#234613=CARTESIAN_POINT('Ctrl Pts',(-3.29936496202567,12.2,10.0571387952304));
#234614=CARTESIAN_POINT('Ctrl Pts',(-3.30111528813566,12.2,10.0600898027987));
#234615=CARTESIAN_POINT('Ctrl Pts',(-3.30286561424566,12.2,10.0630408103671));
#234616=CARTESIAN_POINT('Ctrl Pts',(-3.3046373103465,12.2,10.0660127511514));
#234617=CARTESIAN_POINT('Ctrl Pts',(-3.3064304189657,12.2,10.0690052419983));
#234618=CARTESIAN_POINT('Ctrl Pts',(-3.3082235275849,12.2,10.0719977328452));
#234619=CARTESIAN_POINT('Ctrl Pts',(-3.31003804933333,12.2,10.0750107746777));
#234620=CARTESIAN_POINT('Ctrl Pts',(-3.31187402225,12.2,10.0780439912749));
#234621=CARTESIAN_POINT('Ctrl Pts',(-3.31370999516666,12.2,10.0810772078722));
#234622=CARTESIAN_POINT('Ctrl Pts',(-3.31556742195911,12.2,10.0841305979709));
#234623=CARTESIAN_POINT('Ctrl Pts',(-3.31744634050936,12.2,10.0872037954849));
#234624=CARTESIAN_POINT('Ctrl Pts',(-3.31932525905961,12.2,10.0902769929989));
#234625=CARTESIAN_POINT('Ctrl Pts',(-3.32122566964693,12.2,10.0933699945971));
#234626=CARTESIAN_POINT('Ctrl Pts',(-3.32314760742583,12.2,10.0964824386953));
#234627=CARTESIAN_POINT('Ctrl Pts',(-3.32506954520472,12.2,10.0995948827935));
#234628=CARTESIAN_POINT('Ctrl Pts',(-3.3270130109442,12.2,10.1027267661829));
#234629=CARTESIAN_POINT('Ctrl Pts',(-3.32897804032031,12.2,10.1058777329895));
#234630=CARTESIAN_POINT('Ctrl Pts',(-3.33094306969641,12.2,10.109028699796));
#234631=CARTESIAN_POINT('Ctrl Pts',(-3.33292966250359,12.2,10.1121987499762));
#234632=CARTESIAN_POINT('Ctrl Pts',(-3.33493785121653,12.2,10.1153875286785));
#234633=CARTESIAN_POINT('Ctrl Pts',(-3.33694603992947,12.2,10.1185763073808));
#234634=CARTESIAN_POINT('Ctrl Pts',(-3.33897582562212,12.2,10.1217838150371));
#234635=CARTESIAN_POINT('Ctrl Pts',(-3.341027239235,12.2,10.1250097044136));
#234636=CARTESIAN_POINT('Ctrl Pts',(-3.34307865284788,12.2,10.12823559379));
#234637=CARTESIAN_POINT('Ctrl Pts',(-3.34515169463332,12.2,10.1314798639918));
#234638=CARTESIAN_POINT('Ctrl Pts',(-3.347246394774,12.2,10.13474217191));
#234639=CARTESIAN_POINT('Ctrl Pts',(-3.34934109468635,12.2,10.1380044794726));
#234640=CARTESIAN_POINT('Ctrl Pts',(-3.35145745234407,12.2,10.1412848267573));
#234641=CARTESIAN_POINT('Ctrl Pts',(-3.35359549717868,12.2,10.1445828725769));
#234642=CARTESIAN_POINT('Ctrl Pts',(-3.35573354224635,12.2,10.147880918756));
#234643=CARTESIAN_POINT('Ctrl Pts',(-3.35789327309978,12.2,10.1511966652487));
#234644=CARTESIAN_POINT('Ctrl Pts',(-3.36007471747301,12.2,10.154529778789));
#234645=CARTESIAN_POINT('Ctrl Pts',(-3.36225616184624,12.2,10.1578628923292));
#234646=CARTESIAN_POINT('Ctrl Pts',(-3.36445931938858,12.2,10.1612133721887));
#234647=CARTESIAN_POINT('Ctrl Pts',(-3.36668421619232,12.2,10.1645808900345));
#234648=CARTESIAN_POINT('Ctrl Pts',(-3.36890911299606,12.2,10.1679484078802));
#234649=CARTESIAN_POINT('Ctrl Pts',(-3.37115574774714,12.2,10.1713329633753));
#234650=CARTESIAN_POINT('Ctrl Pts',(-3.37342414626175,12.2,10.1747342338218));
#234651=CARTESIAN_POINT('Ctrl Pts',(-3.37569254477636,12.2,10.1781355042684));
#234652=CARTESIAN_POINT('Ctrl Pts',(-3.37798270410007,12.2,10.1815534888374));
#234653=CARTESIAN_POINT('Ctrl Pts',(-3.38029464930727,12.2,10.1849878675171));
#234654=CARTESIAN_POINT('Ctrl Pts',(-3.38260659451446,12.2,10.1884222461968));
#234655=CARTESIAN_POINT('Ctrl Pts',(-3.38494032557501,12.2,10.1918730190686));
#234656=CARTESIAN_POINT('Ctrl Pts',(-3.38729586154608,12.2,10.1953398710816));
#234657=CARTESIAN_POINT('Ctrl Pts',(-3.38918029042563,12.2,10.1981133528432));
#234658=CARTESIAN_POINT('Ctrl Pts',(-3.39107867605716,12.2,10.2008971257044));
#234659=CARTESIAN_POINT('Ctrl Pts',(-3.39299102653591,12.2,10.2036910291637));
#234660=CARTESIAN_POINT('Ctrl Pts',(-3.3949033767541,12.2,10.2064849322425));
#234661=CARTESIAN_POINT('Ctrl Pts',(-3.39682969380659,12.2,10.2092889669479));
#234662=CARTESIAN_POINT('Ctrl Pts',(-3.39876998509151,12.2,10.212102974995));
#234663=CARTESIAN_POINT('Ctrl Pts',(-3.4007102766408,12.2,10.2149169834255));
#234664=CARTESIAN_POINT('Ctrl Pts',(-3.40266454477786,12.2,10.2177409653266));
#234665=CARTESIAN_POINT('Ctrl Pts',(-3.40463279638604,12.2,10.2205747644817));
#234666=CARTESIAN_POINT('Ctrl Pts',(-3.40660104772605,12.2,10.2234085632507));
#234667=CARTESIAN_POINT('Ctrl Pts',(-3.40858328470009,12.2,10.2262521778303));
#234668=CARTESIAN_POINT('Ctrl Pts',(-3.41057951346875,12.2,10.2291054567943));
#234669=CARTESIAN_POINT('Ctrl Pts',(-3.41257574250939,12.2,10.2319587361471));
#234670=CARTESIAN_POINT('Ctrl Pts',(-3.41458596445438,12.2,10.2348216778638));
#234671=CARTESIAN_POINT('Ctrl Pts',(-3.41661018723228,12.2,10.2376941297432));
#234672=CARTESIAN_POINT('Ctrl Pts',(-3.41863440973437,12.2,10.2405665812312));
#234673=CARTESIAN_POINT('Ctrl Pts',(-3.42067263302535,12.2,10.243448542084));
#234674=CARTESIAN_POINT('Ctrl Pts',(-3.42272486435613,12.2,10.2463398615689));
#234675=CARTESIAN_POINT('Ctrl Pts',(-3.42477709596653,12.2,10.2492311814477));
#234676=CARTESIAN_POINT('Ctrl Pts',(-3.42684333537578,12.2,10.2521318602606));
#234677=CARTESIAN_POINT('Ctrl Pts',(-3.42892359077642,12.2,10.2550417470436));
#234678=CARTESIAN_POINT('Ctrl Pts',(-3.43100384589363,12.2,10.2579516334301));
#234679=CARTESIAN_POINT('Ctrl Pts',(-3.43309811610132,12.2,10.2608707296476));
#234680=CARTESIAN_POINT('Ctrl Pts',(-3.43520640737197,12.2,10.2637988857962));
#234681=CARTESIAN_POINT('Ctrl Pts',(-3.43731469892987,12.2,10.2667270423437));
#234682=CARTESIAN_POINT('Ctrl Pts',(-3.43943701277246,12.2,10.2696642592505));
#234683=CARTESIAN_POINT('Ctrl Pts',(-3.441573353,12.2,10.2726103893));
#234684=CARTESIAN_POINT('Ctrl Pts',(-3.44370969322754,12.2,10.2755565193494));
#234685=CARTESIAN_POINT('Ctrl Pts',(-3.44586006123727,12.2,10.2785115640471));
#234686=CARTESIAN_POINT('Ctrl Pts',(-3.44802446207889,12.2,10.2814753760429));
#234687=CARTESIAN_POINT('Ctrl Pts',(-3.45018886262561,12.2,10.2844391876348));
#234688=CARTESIAN_POINT('Ctrl Pts',(-3.45236729561783,12.2,10.2874117685059));
#234689=CARTESIAN_POINT('Ctrl Pts',(-3.45455976678185,12.2,10.2903929728313));
#234690=CARTESIAN_POINT('Ctrl Pts',(-3.45675223824459,12.2,10.2933741775628));
#234691=CARTESIAN_POINT('Ctrl Pts',(-3.45895874662397,12.2,10.2963640064009));
#234692=CARTESIAN_POINT('Ctrl Pts',(-3.46117929807973,12.2,10.2993623177318));
#234693=CARTESIAN_POINT('Ctrl Pts',(-3.46339984923295,12.2,10.3023606286542));
#234694=CARTESIAN_POINT('Ctrl Pts',(-3.4656344423705,12.2,10.3053674211172));
#234695=CARTESIAN_POINT('Ctrl Pts',(-3.46788308157464,12.2,10.3083825535369));
#234696=CARTESIAN_POINT('Ctrl Pts',(-3.47013172108516,12.2,10.3113976863673));
#234697=CARTESIAN_POINT('Ctrl Pts',(-3.47239440733028,12.2,10.3144211612114));
#234698=CARTESIAN_POINT('Ctrl Pts',(-3.47467114234711,12.2,10.3174528366399));
#234699=CARTESIAN_POINT('Ctrl Pts',(-3.47694787705374,12.2,10.3204845116554));
#234700=CARTESIAN_POINT('Ctrl Pts',(-3.47923866226773,12.2,10.3235243868145));
#234701=CARTESIAN_POINT('Ctrl Pts',(-3.48154350007838,12.2,10.3265723245092));
#234702=CARTESIAN_POINT('Ctrl Pts',(-3.48384833820305,12.2,10.3296202626192));
#234703=CARTESIAN_POINT('Ctrl Pts',(-3.48616722792945,12.2,10.3326762637497));
#234704=CARTESIAN_POINT('Ctrl Pts',(-3.48850017472419,12.2,10.3357401892505));
#234705=CARTESIAN_POINT('Ctrl Pts',(-3.49083312120106,12.2,10.3388041143339));
#234706=CARTESIAN_POINT('Ctrl Pts',(-3.49318012223099,12.2,10.3418759657323));
#234707=CARTESIAN_POINT('Ctrl Pts',(-3.49554118143247,12.2,10.3449556055781));
#234708=CARTESIAN_POINT('Ctrl Pts',(-3.49790224095564,12.2,10.3480352458436));
#234709=CARTESIAN_POINT('Ctrl Pts',(-3.500277358181,12.2,10.3511226757644));
#234710=CARTESIAN_POINT('Ctrl Pts',(-3.50266653497879,12.2,10.3542177605447));
#234711=CARTESIAN_POINT('Ctrl Pts',(-3.50505571145104,12.2,10.3573128449033));
#234712=CARTESIAN_POINT('Ctrl Pts',(-3.50745894693715,12.2,10.3604155837631));
#234713=CARTESIAN_POINT('Ctrl Pts',(-3.50987624340478,12.2,10.3635258435081));
#234714=CARTESIAN_POINT('Ctrl Pts',(-3.51229354020175,12.2,10.3666361036768));
#234715=CARTESIAN_POINT('Ctrl Pts',(-3.51472489772667,12.2,10.3697538860703));
#234716=CARTESIAN_POINT('Ctrl Pts',(-3.51717031726001,12.2,10.3728790569771));
#234717=CARTESIAN_POINT('Ctrl Pts',(-3.51961573646016,12.2,10.3760042274581));
#234718=CARTESIAN_POINT('Ctrl Pts',(-3.52207521794367,12.2,10.3791367884607));
#234719=CARTESIAN_POINT('Ctrl Pts',(-3.52454876162892,12.2,10.3822766062033));
#234720=CARTESIAN_POINT('Ctrl Pts',(-3.52702230565118,12.2,10.3854164243736));
#234721=CARTESIAN_POINT('Ctrl Pts',(-3.52950991046368,12.2,10.3885635023003));
#234722=CARTESIAN_POINT('Ctrl Pts',(-3.53201157926666,12.2,10.3917177072499));
#234723=CARTESIAN_POINT('Ctrl Pts',(-3.53451324806963,12.2,10.3948719121996));
#234724=CARTESIAN_POINT('Ctrl Pts',(-3.53702897848819,12.2,10.3980332456585));
#234725=CARTESIAN_POINT('Ctrl Pts',(-3.53955877190529,12.2,10.4012015797763));
#234726=CARTESIAN_POINT('Ctrl Pts',(-3.54208856497771,12.2,10.4043699134625));
#234727=CARTESIAN_POINT('Ctrl Pts',(-3.54463242003439,12.2,10.4075452463144));
#234728=CARTESIAN_POINT('Ctrl Pts',(-3.54719033649102,12.2,10.4107274519982));
#234729=CARTESIAN_POINT('Ctrl Pts',(-3.54974825329616,12.2,10.4139096581156));
#234730=CARTESIAN_POINT('Ctrl Pts',(-3.55232023240676,12.2,10.4170987356293));
#234731=CARTESIAN_POINT('Ctrl Pts',(-3.55490627140033,12.2,10.4202945599637));
#234732=CARTESIAN_POINT('Ctrl Pts',(-3.55749231004154,12.2,10.4234903838627));
#234733=CARTESIAN_POINT('Ctrl Pts',(-3.56009240990104,12.2,10.4266929540727));
#234734=CARTESIAN_POINT('Ctrl Pts',(-3.5627065683531,12.2,10.429902143921));
#234735=CARTESIAN_POINT('Ctrl Pts',(-3.56532072716133,12.2,10.4331113342066));
#234736=CARTESIAN_POINT('Ctrl Pts',(-3.56794894534067,12.2,10.4363271470235));
#234737=CARTESIAN_POINT('Ctrl Pts',(-3.5705912202078,12.2,10.4395494552551));
#234738=CARTESIAN_POINT('Ctrl Pts',(-3.57323349471492,12.2,10.4427717630476));
#234739=CARTESIAN_POINT('Ctrl Pts',(-3.57588982754871,12.2,10.4460005664673));
#234740=CARTESIAN_POINT('Ctrl Pts',(-3.57856021479592,12.2,10.4492357450305));
#234741=CARTESIAN_POINT('Ctrl Pts',(-3.58123060240697,12.2,10.4524709240346));
#234742=CARTESIAN_POINT('Ctrl Pts',(-3.58391504561995,12.2,10.4557124753742));
#234743=CARTESIAN_POINT('Ctrl Pts',(-3.58661354171241,12.2,10.4589602782739));
#234744=CARTESIAN_POINT('Ctrl Pts',(-3.58931203743721,12.2,10.462208080731));
#234745=CARTESIAN_POINT('Ctrl Pts',(-3.59202458546189,12.2,10.4654621349174));
#234746=CARTESIAN_POINT('Ctrl Pts',(-3.59475118323754,12.2,10.4687223199836));
#234747=CARTESIAN_POINT('Ctrl Pts',(-3.5974777813847,12.2,10.471982505494));
#234748=CARTESIAN_POINT('Ctrl Pts',(-3.60021842976976,12.2,10.4752488211395));
#234749=CARTESIAN_POINT('Ctrl Pts',(-3.60297312454354,12.2,10.4785211462772));
#234750=CARTESIAN_POINT('Ctrl Pts',(-3.60572781894201,12.2,10.481793470969));
#234751=CARTESIAN_POINT('Ctrl Pts',(-3.6084965606601,12.2,10.4850718073905));
#234752=CARTESIAN_POINT('Ctrl Pts',(-3.61127934448668,12.2,10.4883560339547));
#234753=CARTESIAN_POINT('Ctrl Pts',(-3.61406212869242,12.2,10.4916402609663));
#234754=CARTESIAN_POINT('Ctrl Pts',(-3.61685895664683,12.2,10.4949303804037));
#234755=CARTESIAN_POINT('Ctrl Pts',(-3.61966982279999,12.2,10.49822627325));
#234756=CARTESIAN_POINT('Ctrl Pts',(-3.62318340529995,12.2,10.5023461390832));
#234757=CARTESIAN_POINT('Ctrl Pts',(-3.62671892428574,12.2,10.5064750249501));
#234758=CARTESIAN_POINT('Ctrl Pts',(-3.63027637096861,12.2,10.5106127035106));
#234759=CARTESIAN_POINT('Ctrl Pts',(-3.63312232808224,12.2,10.5139228460883));
#234760=CARTESIAN_POINT('Ctrl Pts',(-3.63598232039704,12.2,10.5172386164151));
#234761=CARTESIAN_POINT('Ctrl Pts',(-3.63885634077177,12.2,10.5205598981986));
#234762=CARTESIAN_POINT('Ctrl Pts',(-3.64173036153809,12.2,10.5238811804346));
#234763=CARTESIAN_POINT('Ctrl Pts',(-3.64461841053906,12.2,10.5272079721989));
#234764=CARTESIAN_POINT('Ctrl Pts',(-3.647520483975,12.2,10.5305401629916));
#234765=CARTESIAN_POINT('Ctrl Pts',(-3.65042255741093,12.2,10.5338723537843));
#234766=CARTESIAN_POINT('Ctrl Pts',(-3.65333865578462,12.2,10.537209939386));
#234767=CARTESIAN_POINT('Ctrl Pts',(-3.65626877194575,12.2,10.5405528090132));
#234768=CARTESIAN_POINT('Ctrl Pts',(-3.65846635886699,12.2,10.5430599610058));
#234769=CARTESIAN_POINT('Ctrl Pts',(-3.66067183178057,12.2,10.5455700840516));
#234770=CARTESIAN_POINT('Ctrl Pts',(-3.66288518818664,12.2,10.5480831307529));
#234771=CARTESIAN_POINT('Ctrl Pts',(-3.66509854459271,12.2,10.5505961774541));
#234772=CARTESIAN_POINT('Ctrl Pts',(-3.66731978342341,12.2,10.5531121483658));
#234773=CARTESIAN_POINT('Ctrl Pts',(-3.66954890330144,12.2,10.5556309949829));
#234774=CARTESIAN_POINT('Ctrl Pts',(-3.67177802317947,12.2,10.5581498416));
#234775=CARTESIAN_POINT('Ctrl Pts',(-3.67401502376491,12.2,10.5606715651084));
#234776=CARTESIAN_POINT('Ctrl Pts',(-3.676259902225,12.2,10.563196116725));
#234777=CARTESIAN_POINT('Ctrl Pts',(-3.67850478068509,12.2,10.5657206683416));
#234778=CARTESIAN_POINT('Ctrl Pts',(-3.6807575386199,12.2,10.5682480502498));
#234779=CARTESIAN_POINT('Ctrl Pts',(-3.68301817103705,12.2,10.5707782142409));
#234780=CARTESIAN_POINT('Ctrl Pts',(-3.6852788034542,12.2,10.573308378232));
#234781=CARTESIAN_POINT('Ctrl Pts',(-3.6875473112629,12.2,10.5758413236252));
#234782=CARTESIAN_POINT('Ctrl Pts',(-3.68982369179298,12.2,10.5783770052844));
#234783=CARTESIAN_POINT('Ctrl Pts',(-3.69210007232306,12.2,10.5809126869436));
#234784=CARTESIAN_POINT('Ctrl Pts',(-3.6943843261847,12.2,10.5834511038387));
#234785=CARTESIAN_POINT('Ctrl Pts',(-3.69667645001699,12.2,10.5859922099127));
#234786=CARTESIAN_POINT('Ctrl Pts',(-3.69896857426568,12.2,10.5885333164482));
#234787=CARTESIAN_POINT('Ctrl Pts',(-3.70126856795,12.2,10.591077112568));
#234788=CARTESIAN_POINT('Ctrl Pts',(-3.70357642874479,12.2,10.5936235520634));
#234789=CARTESIAN_POINT('Ctrl Pts',(-3.70588428912032,12.2,10.5961699910962));
#234790=CARTESIAN_POINT('Ctrl Pts',(-3.70820001685383,12.2,10.598719073504));
#234791=CARTESIAN_POINT('Ctrl Pts',(-3.71052360777008,12.2,10.6012707530365));
#234792=CARTESIAN_POINT('Ctrl Pts',(-3.71284719868633,12.2,10.603822432569));
#234793=CARTESIAN_POINT('Ctrl Pts',(-3.71517865447647,12.2,10.6063767092336));
#234794=CARTESIAN_POINT('Ctrl Pts',(-3.71751797077713,12.2,10.608933537819));
#234795=CARTESIAN_POINT('Ctrl Pts',(-3.7198572870778,12.2,10.6114903664044));
#234796=CARTESIAN_POINT('Ctrl Pts',(-3.72220446275609,12.2,10.6140497471957));
#234797=CARTESIAN_POINT('Ctrl Pts',(-3.72455949751453,12.2,10.6166116347393));
#234798=CARTESIAN_POINT('Ctrl Pts',(-3.72691453227296,12.2,10.6191735222829));
#234799=CARTESIAN_POINT('Ctrl Pts',(-3.72927742419522,12.2,10.6217379156804));
#234800=CARTESIAN_POINT('Ctrl Pts',(-3.73164817052505,12.2,10.6243047707536));
#234801=CARTESIAN_POINT('Ctrl Pts',(-3.73401891685488,12.2,10.6268716258267));
#234802=CARTESIAN_POINT('Ctrl Pts',(-3.73639751738422,12.2,10.6294409428998));
#234803=CARTESIAN_POINT('Ctrl Pts',(-3.73878396875475,12.2,10.6320126769727));
#234804=CARTESIAN_POINT('Ctrl Pts',(-3.74117042055882,12.2,10.6345844115127));
#234805=CARTESIAN_POINT('Ctrl Pts',(-3.74356472289017,12.2,10.6371585625036));
#234806=CARTESIAN_POINT('Ctrl Pts',(-3.74596687274035,12.2,10.639735086045));
#234807=CARTESIAN_POINT('Ctrl Pts',(-3.74836902215414,12.2,10.6423116091184));
#234808=CARTESIAN_POINT('Ctrl Pts',(-3.75077902015069,12.2,10.644890504264));
#234809=CARTESIAN_POINT('Ctrl Pts',(-3.75319686072621,12.2,10.6474717275077));
#234810=CARTESIAN_POINT('Ctrl Pts',(-3.75561470130172,12.2,10.6500529507515));
#234811=CARTESIAN_POINT('Ctrl Pts',(-3.75804038713647,12.2,10.652636502409));
#234812=CARTESIAN_POINT('Ctrl Pts',(-3.76047391154872,12.2,10.6552223380235));
#234813=CARTESIAN_POINT('Ctrl Pts',(-3.76290743596097,12.2,10.6578081736381));
#234814=CARTESIAN_POINT('Ctrl Pts',(-3.76534880048897,12.2,10.6603962933774));
#234815=CARTESIAN_POINT('Ctrl Pts',(-3.767798001775,12.2,10.6629866534916));
#234816=CARTESIAN_POINT('Ctrl Pts',(-3.77024720306104,12.2,10.6655770136059));
#234817=CARTESIAN_POINT('Ctrl Pts',(-3.7727042400717,12.2,10.668169614095));
#234818=CARTESIAN_POINT('Ctrl Pts',(-3.77516911077313,12.2,10.6707644111672));
#234819=CARTESIAN_POINT('Ctrl Pts',(-3.77763398147455,12.2,10.6733592082394));
#234820=CARTESIAN_POINT('Ctrl Pts',(-3.78010668293379,12.2,10.6759562019948));
#234821=CARTESIAN_POINT('Ctrl Pts',(-3.78258721421758,12.2,10.6785553499834));
#234822=CARTESIAN_POINT('Ctrl Pts',(-3.78506774595201,12.2,10.6811544984441));
#234823=CARTESIAN_POINT('Ctrl Pts',(-3.787556105997,12.2,10.6837557992389));
#234824=CARTESIAN_POINT('Ctrl Pts',(-3.79005229077751,12.2,10.6863592113258));
#234825=CARTESIAN_POINT('Ctrl Pts',(-3.79254847510455,12.2,10.6889626229399));
#234826=CARTESIAN_POINT('Ctrl Pts',(-3.79505248375092,12.2,10.6915681452187));
#234827=CARTESIAN_POINT('Ctrl Pts',(-3.79756431320273,12.2,10.6941757354628));
#234828=CARTESIAN_POINT('Ctrl Pts',(-3.80007614265454,12.2,10.696783325707));
#234829=CARTESIAN_POINT('Ctrl Pts',(-3.80259579270012,12.2,10.6993929837127));
#234830=CARTESIAN_POINT('Ctrl Pts',(-3.80512325902562,12.2,10.7020046667847));
#234831=CARTESIAN_POINT('Ctrl Pts',(-3.80765072535113,12.2,10.7046163498566));
#234832=CARTESIAN_POINT('Ctrl Pts',(-3.81018600785905,12.2,10.7072300574283));
#234833=CARTESIAN_POINT('Ctrl Pts',(-3.81272910222501,12.2,10.7098457485));
#234834=CARTESIAN_POINT('Ctrl Pts',(-3.81527219659096,12.2,10.7124614395716));
#234835=CARTESIAN_POINT('Ctrl Pts',(-3.81782310329824,12.2,10.7150791136598));
#234836=CARTESIAN_POINT('Ctrl Pts',(-3.82038181720456,12.2,10.7176987287728));
#234837=CARTESIAN_POINT('Ctrl Pts',(-3.82294053111088,12.2,10.7203183438857));
#234838=CARTESIAN_POINT('Ctrl Pts',(-3.8255070539345,12.2,10.7229398988736));
#234839=CARTESIAN_POINT('Ctrl Pts',(-3.82808137901035,12.2,10.7255633536591));
#234840=CARTESIAN_POINT('Ctrl Pts',(-3.83065570408619,12.2,10.7281868084446));
#234841=CARTESIAN_POINT('Ctrl Pts',(-3.8332378332639,12.2,10.7308121627396));
#234842=CARTESIAN_POINT('Ctrl Pts',(-3.83582776062707,12.2,10.7334393729356));
#234843=CARTESIAN_POINT('Ctrl Pts',(-3.83841768846073,12.2,10.7360665836088));
#234844=CARTESIAN_POINT('Ctrl Pts',(-3.8410154146883,12.2,10.7386956518243));
#234845=CARTESIAN_POINT('Ctrl Pts',(-3.84362093502635,12.2,10.7413265355402));
#234846=CARTESIAN_POINT('Ctrl Pts',(-3.84622645489106,12.2,10.7439574187782));
#234847=CARTESIAN_POINT('Ctrl Pts',(-3.84883976986375,12.2,10.7465901191161));
#234848=CARTESIAN_POINT('Ctrl Pts',(-3.85146087376917,12.2,10.7492245942705));
#234849=CARTESIAN_POINT('Ctrl Pts',(-3.85408197767459,12.2,10.7518590694249));
#234850=CARTESIAN_POINT('Ctrl Pts',(-3.85671087233616,12.2,10.7544953204529));
#234851=CARTESIAN_POINT('Ctrl Pts',(-3.85934755071074,12.2,10.7571333045357));
#234852=CARTESIAN_POINT('Ctrl Pts',(-3.86286312171717,12.2,10.7606506164864));
#234853=CARTESIAN_POINT('Ctrl Pts',(-3.86639253259233,12.2,10.7641710075372));
#234854=CARTESIAN_POINT('Ctrl Pts',(-3.86993577091234,12.2,10.7676943824156));
#234855=CARTESIAN_POINT('Ctrl Pts',(-3.87259320025582,12.2,10.7703369141744));
#234856=CARTESIAN_POINT('Ctrl Pts',(-3.87525840799319,12.2,10.7729811257754));
#234857=CARTESIAN_POINT('Ctrl Pts',(-3.87793138975772,12.2,10.7756269785351));
#234858=CARTESIAN_POINT('Ctrl Pts',(-3.88060437103665,12.2,10.7782728308142));
#234859=CARTESIAN_POINT('Ctrl Pts',(-3.88328512609018,12.2,10.7809203265349));
#234860=CARTESIAN_POINT('Ctrl Pts',(-3.88597364982652,12.2,10.7835694230221));
#234861=CARTESIAN_POINT('Ctrl Pts',(-3.88955834797884,12.2,10.7871015515113));
#234862=CARTESIAN_POINT('Ctrl Pts',(-3.89315685641974,12.2,10.7906365222355));
#234863=CARTESIAN_POINT('Ctrl Pts',(-3.89676916219258,12.2,10.7941742225116));
#234864=CARTESIAN_POINT('Ctrl Pts',(-3.90038146845759,12.2,10.7977119232698));
#234865=CARTESIAN_POINT('Ctrl Pts',(-3.90400756999021,12.2,10.8012523489275));
#234866=CARTESIAN_POINT('Ctrl Pts',(-3.90764746004228,12.2,10.8047954455155));
#234867=CARTESIAN_POINT('Ctrl Pts',(-3.91037737733337,12.2,10.8074527677151));
#234868=CARTESIAN_POINT('Ctrl Pts',(-3.91311505247005,12.2,10.8101115985174));
#234869=CARTESIAN_POINT('Ctrl Pts',(-3.91586047900006,12.2,10.812771925));
#234870=CARTESIAN_POINT('Ctrl Pts',(-4.27433547000006,15.2,10.676144262));
#234871=CARTESIAN_POINT('Ctrl Pts',(-4.27433547000006,11.6,10.676144262));
#234872=CARTESIAN_POINT('Ctrl Pts',(-4.27439112800006,15.2,10.675381706));
#234873=CARTESIAN_POINT('Ctrl Pts',(-4.27439112800006,11.6,10.675381706));
#234874=CARTESIAN_POINT('Ctrl Pts',(-4.27450212700006,15.2,10.673857013));
#234875=CARTESIAN_POINT('Ctrl Pts',(-4.27450212700006,11.6,10.673857013));
#234876=CARTESIAN_POINT('Ctrl Pts',(-4.27466766800006,15.2,10.67157123));
#234877=CARTESIAN_POINT('Ctrl Pts',(-4.27466766800006,11.6,10.67157123));
#234878=CARTESIAN_POINT('Ctrl Pts',(-4.27488647400006,15.2,10.668526034));
#234879=CARTESIAN_POINT('Ctrl Pts',(-4.27488647400006,11.6,10.668526034));
#234880=CARTESIAN_POINT('Ctrl Pts',(-4.27515679000006,15.2,10.664723728));
#234881=CARTESIAN_POINT('Ctrl Pts',(-4.27515679000006,11.6,10.664723728));
#234882=CARTESIAN_POINT('Ctrl Pts',(-4.27542391400006,15.2,10.660925612));
#234883=CARTESIAN_POINT('Ctrl Pts',(-4.27542391400006,11.6,10.660925612));
#234884=CARTESIAN_POINT('Ctrl Pts',(-4.27568784900005,15.2,10.65713169));
#234885=CARTESIAN_POINT('Ctrl Pts',(-4.27568784900005,11.6,10.65713169));
#234886=CARTESIAN_POINT('Ctrl Pts',(-4.27594859700006,15.2,10.653341964));
#234887=CARTESIAN_POINT('Ctrl Pts',(-4.27594859700006,11.6,10.653341964));
#234888=CARTESIAN_POINT('Ctrl Pts',(-4.27620616000006,15.2,10.649556438));
#234889=CARTESIAN_POINT('Ctrl Pts',(-4.27620616000006,11.6,10.649556438));
#234890=CARTESIAN_POINT('Ctrl Pts',(-4.27646054400006,15.2,10.645775122));
#234891=CARTESIAN_POINT('Ctrl Pts',(-4.27646054400006,11.6,10.645775122));
#234892=CARTESIAN_POINT('Ctrl Pts',(-4.27671175300006,15.2,10.64199802));
#234893=CARTESIAN_POINT('Ctrl Pts',(-4.27671175300006,11.6,10.64199802));
#234894=CARTESIAN_POINT('Ctrl Pts',(-4.27695979400006,15.2,10.638225144));
#234895=CARTESIAN_POINT('Ctrl Pts',(-4.27695979400006,11.6,10.638225144));
#234896=CARTESIAN_POINT('Ctrl Pts',(-4.27720467300006,15.2,10.634456501));
#234897=CARTESIAN_POINT('Ctrl Pts',(-4.27720467300006,11.6,10.634456501));
#234898=CARTESIAN_POINT('Ctrl Pts',(-4.27744639700006,15.2,10.630692101));
#234899=CARTESIAN_POINT('Ctrl Pts',(-4.27744639700006,11.6,10.630692101));
#234900=CARTESIAN_POINT('Ctrl Pts',(-4.27768497200006,15.2,10.626931954));
#234901=CARTESIAN_POINT('Ctrl Pts',(-4.27768497200006,11.6,10.626931954));
#234902=CARTESIAN_POINT('Ctrl Pts',(-4.27792040200006,15.2,10.623176065));
#234903=CARTESIAN_POINT('Ctrl Pts',(-4.27792040200006,11.6,10.623176065));
#234904=CARTESIAN_POINT('Ctrl Pts',(-4.27815269400006,15.2,10.619424443));
#234905=CARTESIAN_POINT('Ctrl Pts',(-4.27815269400006,11.6,10.619424443));
#234906=CARTESIAN_POINT('Ctrl Pts',(-4.27838185100006,15.2,10.615677095));
#234907=CARTESIAN_POINT('Ctrl Pts',(-4.27838185100006,11.6,10.615677095));
#234908=CARTESIAN_POINT('Ctrl Pts',(-4.27860787900006,15.2,10.611934026));
#234909=CARTESIAN_POINT('Ctrl Pts',(-4.27860787900006,11.6,10.611934026));
#234910=CARTESIAN_POINT('Ctrl Pts',(-4.27883078100006,15.2,10.608195244));
#234911=CARTESIAN_POINT('Ctrl Pts',(-4.27883078100006,11.6,10.608195244));
#234912=CARTESIAN_POINT('Ctrl Pts',(-4.27905056400006,15.2,10.604460756));
#234913=CARTESIAN_POINT('Ctrl Pts',(-4.27905056400006,11.6,10.604460756));
#234914=CARTESIAN_POINT('Ctrl Pts',(-4.27926723000006,15.2,10.600730568));
#234915=CARTESIAN_POINT('Ctrl Pts',(-4.27926723000006,11.6,10.600730568));
#234916=CARTESIAN_POINT('Ctrl Pts',(-4.27948078700005,15.2,10.597004691));
#234917=CARTESIAN_POINT('Ctrl Pts',(-4.27948078700005,11.6,10.597004691));
#234918=CARTESIAN_POINT('Ctrl Pts',(-4.27969124100006,15.2,10.593283129));
#234919=CARTESIAN_POINT('Ctrl Pts',(-4.27969124100006,11.6,10.593283129));
#234920=CARTESIAN_POINT('Ctrl Pts',(-4.27989859400006,15.2,10.589565891));
#234921=CARTESIAN_POINT('Ctrl Pts',(-4.27989859400006,11.6,10.589565891));
#234922=CARTESIAN_POINT('Ctrl Pts',(-4.28010285400005,15.2,10.585852986));
#234923=CARTESIAN_POINT('Ctrl Pts',(-4.28010285400005,11.6,10.585852986));
#234924=CARTESIAN_POINT('Ctrl Pts',(-4.28030402700006,15.2,10.58214442));
#234925=CARTESIAN_POINT('Ctrl Pts',(-4.28030402700006,11.6,10.58214442));
#234926=CARTESIAN_POINT('Ctrl Pts',(-4.28050211700006,15.2,10.578440201));
#234927=CARTESIAN_POINT('Ctrl Pts',(-4.28050211700006,11.6,10.578440201));
#234928=CARTESIAN_POINT('Ctrl Pts',(-4.28069713000006,15.2,10.574740338));
#234929=CARTESIAN_POINT('Ctrl Pts',(-4.28069713000006,11.6,10.574740338));
#234930=CARTESIAN_POINT('Ctrl Pts',(-4.28088907200006,15.2,10.571044836));
#234931=CARTESIAN_POINT('Ctrl Pts',(-4.28088907200006,11.6,10.571044836));
#234932=CARTESIAN_POINT('Ctrl Pts',(-4.28107794500006,15.2,10.567353704));
#234933=CARTESIAN_POINT('Ctrl Pts',(-4.28107794500006,11.6,10.567353704));
#234934=CARTESIAN_POINT('Ctrl Pts',(-4.28126375700006,15.2,10.563666949));
#234935=CARTESIAN_POINT('Ctrl Pts',(-4.28126375700006,11.6,10.563666949));
#234936=CARTESIAN_POINT('Ctrl Pts',(-4.28144651400006,15.2,10.559984579));
#234937=CARTESIAN_POINT('Ctrl Pts',(-4.28144651400006,11.6,10.559984579));
#234938=CARTESIAN_POINT('Ctrl Pts',(-4.28162621900006,15.2,10.556306601));
#234939=CARTESIAN_POINT('Ctrl Pts',(-4.28162621900006,11.6,10.556306601));
#234940=CARTESIAN_POINT('Ctrl Pts',(-4.28180287800005,15.2,10.552633022));
#234941=CARTESIAN_POINT('Ctrl Pts',(-4.28180287800005,11.6,10.552633022));
#234942=CARTESIAN_POINT('Ctrl Pts',(-4.28197649800006,15.2,10.54896385));
#234943=CARTESIAN_POINT('Ctrl Pts',(-4.28197649800006,11.6,10.54896385));
#234944=CARTESIAN_POINT('Ctrl Pts',(-4.28214708400006,15.2,10.545299092));
#234945=CARTESIAN_POINT('Ctrl Pts',(-4.28214708400006,11.6,10.545299092));
#234946=CARTESIAN_POINT('Ctrl Pts',(-4.28231464000006,15.2,10.541638759));
#234947=CARTESIAN_POINT('Ctrl Pts',(-4.28231464000006,11.6,10.541638759));
#234948=CARTESIAN_POINT('Ctrl Pts',(-4.28247917400006,15.2,10.537982855));
#234949=CARTESIAN_POINT('Ctrl Pts',(-4.28247917400006,11.6,10.537982855));
#234950=CARTESIAN_POINT('Ctrl Pts',(-4.28264068800006,15.2,10.534331388));
#234951=CARTESIAN_POINT('Ctrl Pts',(-4.28264068800006,11.6,10.534331388));
#234952=CARTESIAN_POINT('Ctrl Pts',(-4.28279919100006,15.2,10.530684368));
#234953=CARTESIAN_POINT('Ctrl Pts',(-4.28279919100006,11.6,10.530684368));
#234954=CARTESIAN_POINT('Ctrl Pts',(-4.28295468700005,15.2,10.5270418));
#234955=CARTESIAN_POINT('Ctrl Pts',(-4.28295468700005,11.6,10.5270418));
#234956=CARTESIAN_POINT('Ctrl Pts',(-4.28310718100006,15.2,10.523403693));
#234957=CARTESIAN_POINT('Ctrl Pts',(-4.28310718100006,11.6,10.523403693));
#234958=CARTESIAN_POINT('Ctrl Pts',(-4.28325667900006,15.2,10.519770053));
#234959=CARTESIAN_POINT('Ctrl Pts',(-4.28325667900006,11.6,10.519770053));
#234960=CARTESIAN_POINT('Ctrl Pts',(-4.28340318700006,15.2,10.51614089));
#234961=CARTESIAN_POINT('Ctrl Pts',(-4.28340318700006,11.6,10.51614089));
#234962=CARTESIAN_POINT('Ctrl Pts',(-4.28354671000006,15.2,10.51251621));
#234963=CARTESIAN_POINT('Ctrl Pts',(-4.28354671000006,11.6,10.51251621));
#234964=CARTESIAN_POINT('Ctrl Pts',(-4.28368725400006,15.2,10.508896023));
#234965=CARTESIAN_POINT('Ctrl Pts',(-4.28368725400006,11.6,10.508896023));
#234966=CARTESIAN_POINT('Ctrl Pts',(-4.28382482400006,15.2,10.505280333));
#234967=CARTESIAN_POINT('Ctrl Pts',(-4.28382482400006,11.6,10.505280333));
#234968=CARTESIAN_POINT('Ctrl Pts',(-4.28395942700006,15.2,10.50166915));
#234969=CARTESIAN_POINT('Ctrl Pts',(-4.28395942700006,11.6,10.50166915));
#234970=CARTESIAN_POINT('Ctrl Pts',(-4.28409106600006,15.2,10.498062482));
#234971=CARTESIAN_POINT('Ctrl Pts',(-4.28409106600006,11.6,10.498062482));
#234972=CARTESIAN_POINT('Ctrl Pts',(-4.28421975000005,15.2,10.494460336));
#234973=CARTESIAN_POINT('Ctrl Pts',(-4.28421975000005,11.6,10.494460336));
#234974=CARTESIAN_POINT('Ctrl Pts',(-4.28434548300006,15.2,10.49086272));
#234975=CARTESIAN_POINT('Ctrl Pts',(-4.28434548300006,11.6,10.49086272));
#234976=CARTESIAN_POINT('Ctrl Pts',(-4.28446827000006,15.2,10.487269641));
#234977=CARTESIAN_POINT('Ctrl Pts',(-4.28446827000006,11.6,10.487269641));
#234978=CARTESIAN_POINT('Ctrl Pts',(-4.28458811800006,15.2,10.483681106));
#234979=CARTESIAN_POINT('Ctrl Pts',(-4.28458811800006,11.6,10.483681106));
#234980=CARTESIAN_POINT('Ctrl Pts',(-4.28470503200006,15.2,10.480097126));
#234981=CARTESIAN_POINT('Ctrl Pts',(-4.28470503200006,11.6,10.480097126));
#234982=CARTESIAN_POINT('Ctrl Pts',(-4.28481901900006,15.2,10.476517706));
#234983=CARTESIAN_POINT('Ctrl Pts',(-4.28481901900006,11.6,10.476517706));
#234984=CARTESIAN_POINT('Ctrl Pts',(-4.28493008300006,15.2,10.472942855));
#234985=CARTESIAN_POINT('Ctrl Pts',(-4.28493008300006,11.6,10.472942855));
#234986=CARTESIAN_POINT('Ctrl Pts',(-4.28503823100006,15.2,10.469372579));
#234987=CARTESIAN_POINT('Ctrl Pts',(-4.28503823100006,11.6,10.469372579));
#234988=CARTESIAN_POINT('Ctrl Pts',(-4.28514346700006,15.2,10.465806888));
#234989=CARTESIAN_POINT('Ctrl Pts',(-4.28514346700006,11.6,10.465806888));
#234990=CARTESIAN_POINT('Ctrl Pts',(-4.28524579900006,15.2,10.462245788));
#234991=CARTESIAN_POINT('Ctrl Pts',(-4.28524579900006,11.6,10.462245788));
#234992=CARTESIAN_POINT('Ctrl Pts',(-4.28534523200006,15.2,10.458689289));
#234993=CARTESIAN_POINT('Ctrl Pts',(-4.28534523200006,11.6,10.458689289));
#234994=CARTESIAN_POINT('Ctrl Pts',(-4.28544177100005,15.2,10.455137396));
#234995=CARTESIAN_POINT('Ctrl Pts',(-4.28544177100005,11.6,10.455137396));
#234996=CARTESIAN_POINT('Ctrl Pts',(-4.28553542400006,15.2,10.45159012));
#234997=CARTESIAN_POINT('Ctrl Pts',(-4.28553542400006,11.6,10.45159012));
#234998=CARTESIAN_POINT('Ctrl Pts',(-4.28562619500005,15.2,10.448047467));
#234999=CARTESIAN_POINT('Ctrl Pts',(-4.28562619500005,11.6,10.448047467));
#235000=CARTESIAN_POINT('Ctrl Pts',(-4.28571409100006,15.2,10.444509444));
#235001=CARTESIAN_POINT('Ctrl Pts',(-4.28571409100006,11.6,10.444509444));
#235002=CARTESIAN_POINT('Ctrl Pts',(-4.28579911600006,15.2,10.440976059));
#235003=CARTESIAN_POINT('Ctrl Pts',(-4.28579911600006,11.6,10.440976059));
#235004=CARTESIAN_POINT('Ctrl Pts',(-4.28588127900006,15.2,10.437447322));
#235005=CARTESIAN_POINT('Ctrl Pts',(-4.28588127900006,11.6,10.437447322));
#235006=CARTESIAN_POINT('Ctrl Pts',(-4.28596058300006,15.2,10.433923239));
#235007=CARTESIAN_POINT('Ctrl Pts',(-4.28596058300006,11.6,10.433923239));
#235008=CARTESIAN_POINT('Ctrl Pts',(-4.28603703500006,15.2,10.430403819));
#235009=CARTESIAN_POINT('Ctrl Pts',(-4.28603703500006,11.6,10.430403819));
#235010=CARTESIAN_POINT('Ctrl Pts',(-4.28611064200005,15.2,10.42688907));
#235011=CARTESIAN_POINT('Ctrl Pts',(-4.28611064200005,11.6,10.42688907));
#235012=CARTESIAN_POINT('Ctrl Pts',(-4.28618140900006,15.2,10.423378997));
#235013=CARTESIAN_POINT('Ctrl Pts',(-4.28618140900006,11.6,10.423378997));
#235014=CARTESIAN_POINT('Ctrl Pts',(-4.28624934300006,15.2,10.419873611));
#235015=CARTESIAN_POINT('Ctrl Pts',(-4.28624934300006,11.6,10.419873611));
#235016=CARTESIAN_POINT('Ctrl Pts',(-4.28631444800006,15.2,10.41637292));
#235017=CARTESIAN_POINT('Ctrl Pts',(-4.28631444800006,11.6,10.41637292));
#235018=CARTESIAN_POINT('Ctrl Pts',(-4.28637673200006,15.2,10.41287693));
#235019=CARTESIAN_POINT('Ctrl Pts',(-4.28637673200006,11.6,10.41287693));
#235020=CARTESIAN_POINT('Ctrl Pts',(-4.28643620100006,15.2,10.409385651));
#235021=CARTESIAN_POINT('Ctrl Pts',(-4.28643620100006,11.6,10.409385651));
#235022=CARTESIAN_POINT('Ctrl Pts',(-4.28649285900006,15.2,10.405899089));
#235023=CARTESIAN_POINT('Ctrl Pts',(-4.28649285900006,11.6,10.405899089));
#235024=CARTESIAN_POINT('Ctrl Pts',(-4.28654671400006,15.2,10.402417252));
#235025=CARTESIAN_POINT('Ctrl Pts',(-4.28654671400006,11.6,10.402417252));
#235026=CARTESIAN_POINT('Ctrl Pts',(-4.28659777200005,15.2,10.39894015));
#235027=CARTESIAN_POINT('Ctrl Pts',(-4.28659777200005,11.6,10.39894015));
#235028=CARTESIAN_POINT('Ctrl Pts',(-4.28664603900006,15.2,10.395467789));
#235029=CARTESIAN_POINT('Ctrl Pts',(-4.28664603900006,11.6,10.395467789));
#235030=CARTESIAN_POINT('Ctrl Pts',(-4.28669152200006,15.2,10.392000178));
#235031=CARTESIAN_POINT('Ctrl Pts',(-4.28669152200006,11.6,10.392000178));
#235032=CARTESIAN_POINT('Ctrl Pts',(-4.28673422400006,15.2,10.388537325));
#235033=CARTESIAN_POINT('Ctrl Pts',(-4.28673422400006,11.6,10.388537325));
#235034=CARTESIAN_POINT('Ctrl Pts',(-4.28677415500006,15.2,10.385079237));
#235035=CARTESIAN_POINT('Ctrl Pts',(-4.28677415500006,11.6,10.385079237));
#235036=CARTESIAN_POINT('Ctrl Pts',(-4.28681131900006,15.2,10.381625923));
#235037=CARTESIAN_POINT('Ctrl Pts',(-4.28681131900006,11.6,10.381625923));
#235038=CARTESIAN_POINT('Ctrl Pts',(-4.28684572400006,15.2,10.378177391));
#235039=CARTESIAN_POINT('Ctrl Pts',(-4.28684572400006,11.6,10.378177391));
#235040=CARTESIAN_POINT('Ctrl Pts',(-4.28687737400006,15.2,10.374733649));
#235041=CARTESIAN_POINT('Ctrl Pts',(-4.28687737400006,11.6,10.374733649));
#235042=CARTESIAN_POINT('Ctrl Pts',(-4.28690627700006,15.2,10.371294705));
#235043=CARTESIAN_POINT('Ctrl Pts',(-4.28690627700006,11.6,10.371294705));
#235044=CARTESIAN_POINT('Ctrl Pts',(-4.28693243800006,15.2,10.367860566));
#235045=CARTESIAN_POINT('Ctrl Pts',(-4.28693243800006,11.6,10.367860566));
#235046=CARTESIAN_POINT('Ctrl Pts',(-4.28695586400006,15.2,10.364431242));
#235047=CARTESIAN_POINT('Ctrl Pts',(-4.28695586400006,11.6,10.364431242));
#235048=CARTESIAN_POINT('Ctrl Pts',(-4.28697656200006,15.2,10.361006739));
#235049=CARTESIAN_POINT('Ctrl Pts',(-4.28697656200006,11.6,10.361006739));
#235050=CARTESIAN_POINT('Ctrl Pts',(-4.28699453700006,15.2,10.357587066));
#235051=CARTESIAN_POINT('Ctrl Pts',(-4.28699453700006,11.6,10.357587066));
#235052=CARTESIAN_POINT('Ctrl Pts',(-4.28700979600006,15.2,10.354172232));
#235053=CARTESIAN_POINT('Ctrl Pts',(-4.28700979600006,11.6,10.354172232));
#235054=CARTESIAN_POINT('Ctrl Pts',(-4.28702234600006,15.2,10.350762244));
#235055=CARTESIAN_POINT('Ctrl Pts',(-4.28702234600006,11.6,10.350762244));
#235056=CARTESIAN_POINT('Ctrl Pts',(-4.28703219200006,15.2,10.347357111));
#235057=CARTESIAN_POINT('Ctrl Pts',(-4.28703219200006,11.6,10.347357111));
#235058=CARTESIAN_POINT('Ctrl Pts',(-4.28703934200006,15.2,10.34395684));
#235059=CARTESIAN_POINT('Ctrl Pts',(-4.28703934200006,11.6,10.34395684));
#235060=CARTESIAN_POINT('Ctrl Pts',(-4.28704380100006,15.2,10.340561439));
#235061=CARTESIAN_POINT('Ctrl Pts',(-4.28704380100006,11.6,10.340561439));
#235062=CARTESIAN_POINT('Ctrl Pts',(-4.28704557600006,15.2,10.337170919));
#235063=CARTESIAN_POINT('Ctrl Pts',(-4.28704557600006,11.6,10.337170919));
#235064=CARTESIAN_POINT('Ctrl Pts',(-4.28704467500006,15.2,10.333785284));
#235065=CARTESIAN_POINT('Ctrl Pts',(-4.28704467500006,11.6,10.333785284));
#235066=CARTESIAN_POINT('Ctrl Pts',(-4.28704110100006,15.2,10.330404545));
#235067=CARTESIAN_POINT('Ctrl Pts',(-4.28704110100006,11.6,10.330404545));
#235068=CARTESIAN_POINT('Ctrl Pts',(-4.28703486500006,15.2,10.327028709));
#235069=CARTESIAN_POINT('Ctrl Pts',(-4.28703486500006,11.6,10.327028709));
#235070=CARTESIAN_POINT('Ctrl Pts',(-4.28702596900005,15.2,10.323657785));
#235071=CARTESIAN_POINT('Ctrl Pts',(-4.28702596900005,11.6,10.323657785));
#235072=CARTESIAN_POINT('Ctrl Pts',(-4.28701442200006,15.2,10.32029178));
#235073=CARTESIAN_POINT('Ctrl Pts',(-4.28701442200006,11.6,10.32029178));
#235074=CARTESIAN_POINT('Ctrl Pts',(-4.28700023100006,15.2,10.316930703));
#235075=CARTESIAN_POINT('Ctrl Pts',(-4.28700023100006,11.6,10.316930703));
#235076=CARTESIAN_POINT('Ctrl Pts',(-4.28698340200006,15.2,10.313574563));
#235077=CARTESIAN_POINT('Ctrl Pts',(-4.28698340200006,11.6,10.313574563));
#235078=CARTESIAN_POINT('Ctrl Pts',(-4.28696394100006,15.2,10.310223367));
#235079=CARTESIAN_POINT('Ctrl Pts',(-4.28696394100006,11.6,10.310223367));
#235080=CARTESIAN_POINT('Ctrl Pts',(-4.28694185400006,15.2,10.306877124));
#235081=CARTESIAN_POINT('Ctrl Pts',(-4.28694185400006,11.6,10.306877124));
#235082=CARTESIAN_POINT('Ctrl Pts',(-4.28691715100006,15.2,10.303535841));
#235083=CARTESIAN_POINT('Ctrl Pts',(-4.28691715100006,11.6,10.303535841));
#235084=CARTESIAN_POINT('Ctrl Pts',(-4.28688983500006,15.2,10.300199529));
#235085=CARTESIAN_POINT('Ctrl Pts',(-4.28688983500006,11.6,10.300199529));
#235086=CARTESIAN_POINT('Ctrl Pts',(-4.28685991400005,15.2,10.296868193));
#235087=CARTESIAN_POINT('Ctrl Pts',(-4.28685991400005,11.6,10.296868193));
#235088=CARTESIAN_POINT('Ctrl Pts',(-4.28682739500006,15.2,10.293541843));
#235089=CARTESIAN_POINT('Ctrl Pts',(-4.28682739500006,11.6,10.293541843));
#235090=CARTESIAN_POINT('Ctrl Pts',(-4.28679228500005,15.2,10.290220487));
#235091=CARTESIAN_POINT('Ctrl Pts',(-4.28679228500005,11.6,10.290220487));
#235092=CARTESIAN_POINT('Ctrl Pts',(-4.28675459000006,15.2,10.286904134));
#235093=CARTESIAN_POINT('Ctrl Pts',(-4.28675459000006,11.6,10.286904134));
#235094=CARTESIAN_POINT('Ctrl Pts',(-4.28671431600006,15.2,10.283592791));
#235095=CARTESIAN_POINT('Ctrl Pts',(-4.28671431600006,11.6,10.283592791));
#235096=CARTESIAN_POINT('Ctrl Pts',(-4.28667147200006,15.2,10.280286467));
#235097=CARTESIAN_POINT('Ctrl Pts',(-4.28667147200006,11.6,10.280286467));
#235098=CARTESIAN_POINT('Ctrl Pts',(-4.28662606400006,15.2,10.276985171));
#235099=CARTESIAN_POINT('Ctrl Pts',(-4.28662606400006,11.6,10.276985171));
#235100=CARTESIAN_POINT('Ctrl Pts',(-4.28657809700006,15.2,10.27368891));
#235101=CARTESIAN_POINT('Ctrl Pts',(-4.28657809700006,11.6,10.27368891));
#235102=CARTESIAN_POINT('Ctrl Pts',(-4.28652758000006,15.2,10.270397693));
#235103=CARTESIAN_POINT('Ctrl Pts',(-4.28652758000006,11.6,10.270397693));
#235104=CARTESIAN_POINT('Ctrl Pts',(-4.28647452000006,15.2,10.267111529));
#235105=CARTESIAN_POINT('Ctrl Pts',(-4.28647452000006,11.6,10.267111529));
#235106=CARTESIAN_POINT('Ctrl Pts',(-4.28641892300006,15.2,10.263830426));
#235107=CARTESIAN_POINT('Ctrl Pts',(-4.28641892300006,11.6,10.263830426));
#235108=CARTESIAN_POINT('Ctrl Pts',(-4.28636079500006,15.2,10.260554392));
#235109=CARTESIAN_POINT('Ctrl Pts',(-4.28636079500006,11.6,10.260554392));
#235110=CARTESIAN_POINT('Ctrl Pts',(-4.28630014400006,15.2,10.257283436));
#235111=CARTESIAN_POINT('Ctrl Pts',(-4.28630014400006,11.6,10.257283436));
#235112=CARTESIAN_POINT('Ctrl Pts',(-4.28623697700006,15.2,10.254017566));
#235113=CARTESIAN_POINT('Ctrl Pts',(-4.28623697700006,11.6,10.254017566));
#235114=CARTESIAN_POINT('Ctrl Pts',(-4.28617130100006,15.2,10.25075679));
#235115=CARTESIAN_POINT('Ctrl Pts',(-4.28617130100006,11.6,10.25075679));
#235116=CARTESIAN_POINT('Ctrl Pts',(-4.28610312300005,15.2,10.247501117));
#235117=CARTESIAN_POINT('Ctrl Pts',(-4.28610312300005,11.6,10.247501117));
#235118=CARTESIAN_POINT('Ctrl Pts',(-4.28603245100006,15.2,10.244250555));
#235119=CARTESIAN_POINT('Ctrl Pts',(-4.28603245100006,11.6,10.244250555));
#235120=CARTESIAN_POINT('Ctrl Pts',(-4.28595928900006,15.2,10.241005114));
#235121=CARTESIAN_POINT('Ctrl Pts',(-4.28595928900006,11.6,10.241005114));
#235122=CARTESIAN_POINT('Ctrl Pts',(-4.28588364700006,15.2,10.237764801));
#235123=CARTESIAN_POINT('Ctrl Pts',(-4.28588364700006,11.6,10.237764801));
#235124=CARTESIAN_POINT('Ctrl Pts',(-4.28580553100006,15.2,10.234529626));
#235125=CARTESIAN_POINT('Ctrl Pts',(-4.28580553100006,11.6,10.234529626));
#235126=CARTESIAN_POINT('Ctrl Pts',(-4.28572494800005,15.2,10.231299595));
#235127=CARTESIAN_POINT('Ctrl Pts',(-4.28572494800005,11.6,10.231299595));
#235128=CARTESIAN_POINT('Ctrl Pts',(-4.28564190400006,15.2,10.228074718));
#235129=CARTESIAN_POINT('Ctrl Pts',(-4.28564190400006,11.6,10.228074718));
#235130=CARTESIAN_POINT('Ctrl Pts',(-4.28555640900006,15.2,10.224855003));
#235131=CARTESIAN_POINT('Ctrl Pts',(-4.28555640900006,11.6,10.224855003));
#235132=CARTESIAN_POINT('Ctrl Pts',(-4.28546846800006,15.2,10.22164046));
#235133=CARTESIAN_POINT('Ctrl Pts',(-4.28546846800006,11.6,10.22164046));
#235134=CARTESIAN_POINT('Ctrl Pts',(-4.28537809000006,15.2,10.218431096));
#235135=CARTESIAN_POINT('Ctrl Pts',(-4.28537809000006,11.6,10.218431096));
#235136=CARTESIAN_POINT('Ctrl Pts',(-4.28528527900006,15.2,10.215226921));
#235137=CARTESIAN_POINT('Ctrl Pts',(-4.28528527900006,11.6,10.215226921));
#235138=CARTESIAN_POINT('Ctrl Pts',(-4.28519004500005,15.2,10.212027942));
#235139=CARTESIAN_POINT('Ctrl Pts',(-4.28519004500005,11.6,10.212027942));
#235140=CARTESIAN_POINT('Ctrl Pts',(-4.28509239400006,15.2,10.208834168));
#235141=CARTESIAN_POINT('Ctrl Pts',(-4.28509239400006,11.6,10.208834168));
#235142=CARTESIAN_POINT('Ctrl Pts',(-4.28499233400006,15.2,10.205645608));
#235143=CARTESIAN_POINT('Ctrl Pts',(-4.28499233400006,11.6,10.205645608));
#235144=CARTESIAN_POINT('Ctrl Pts',(-4.28488987300006,15.2,10.202462271));
#235145=CARTESIAN_POINT('Ctrl Pts',(-4.28488987300006,11.6,10.202462271));
#235146=CARTESIAN_POINT('Ctrl Pts',(-4.28478501700006,15.2,10.199284165));
#235147=CARTESIAN_POINT('Ctrl Pts',(-4.28478501700006,11.6,10.199284165));
#235148=CARTESIAN_POINT('Ctrl Pts',(-4.28467777300006,15.2,10.196111298));
#235149=CARTESIAN_POINT('Ctrl Pts',(-4.28467777300006,11.6,10.196111298));
#235150=CARTESIAN_POINT('Ctrl Pts',(-4.28456814900006,15.2,10.19294368));
#235151=CARTESIAN_POINT('Ctrl Pts',(-4.28456814900006,11.6,10.19294368));
#235152=CARTESIAN_POINT('Ctrl Pts',(-4.28445615200006,15.2,10.189781319));
#235153=CARTESIAN_POINT('Ctrl Pts',(-4.28445615200006,11.6,10.189781319));
#235154=CARTESIAN_POINT('Ctrl Pts',(-4.28434179100006,15.2,10.186624224));
#235155=CARTESIAN_POINT('Ctrl Pts',(-4.28434179100006,11.6,10.186624224));
#235156=CARTESIAN_POINT('Ctrl Pts',(-4.28422507200006,15.2,10.183472403));
#235157=CARTESIAN_POINT('Ctrl Pts',(-4.28422507200006,11.6,10.183472403));
#235158=CARTESIAN_POINT('Ctrl Pts',(-4.28410600200006,15.2,10.180325865));
#235159=CARTESIAN_POINT('Ctrl Pts',(-4.28410600200006,11.6,10.180325865));
#235160=CARTESIAN_POINT('Ctrl Pts',(-4.28398458900006,15.2,10.177184619));
#235161=CARTESIAN_POINT('Ctrl Pts',(-4.28398458900006,11.6,10.177184619));
#235162=CARTESIAN_POINT('Ctrl Pts',(-4.28386084200006,15.2,10.174048675));
#235163=CARTESIAN_POINT('Ctrl Pts',(-4.28386084200006,11.6,10.174048675));
#235164=CARTESIAN_POINT('Ctrl Pts',(-4.28373476600005,15.2,10.170918039));
#235165=CARTESIAN_POINT('Ctrl Pts',(-4.28373476600005,11.6,10.170918039));
#235166=CARTESIAN_POINT('Ctrl Pts',(-4.28360637100006,15.2,10.167792721));
#235167=CARTESIAN_POINT('Ctrl Pts',(-4.28360637100006,11.6,10.167792721));
#235168=CARTESIAN_POINT('Ctrl Pts',(-4.28347566200006,15.2,10.16467273));
#235169=CARTESIAN_POINT('Ctrl Pts',(-4.28347566200006,11.6,10.16467273));
#235170=CARTESIAN_POINT('Ctrl Pts',(-4.28334264800006,15.2,10.161558074));
#235171=CARTESIAN_POINT('Ctrl Pts',(-4.28334264800006,11.6,10.161558074));
#235172=CARTESIAN_POINT('Ctrl Pts',(-4.28320733700006,15.2,10.158448764));
#235173=CARTESIAN_POINT('Ctrl Pts',(-4.28320733700006,11.6,10.158448764));
#235174=CARTESIAN_POINT('Ctrl Pts',(-4.28306973600006,15.2,10.155344806));
#235175=CARTESIAN_POINT('Ctrl Pts',(-4.28306973600006,11.6,10.155344806));
#235176=CARTESIAN_POINT('Ctrl Pts',(-4.28292985300006,15.2,10.15224621));
#235177=CARTESIAN_POINT('Ctrl Pts',(-4.28292985300006,11.6,10.15224621));
#235178=CARTESIAN_POINT('Ctrl Pts',(-4.28278769500006,15.2,10.149152986));
#235179=CARTESIAN_POINT('Ctrl Pts',(-4.28278769500006,11.6,10.149152986));
#235180=CARTESIAN_POINT('Ctrl Pts',(-4.28264327100006,15.2,10.146065141));
#235181=CARTESIAN_POINT('Ctrl Pts',(-4.28264327100006,11.6,10.146065141));
#235182=CARTESIAN_POINT('Ctrl Pts',(-4.28249658600006,15.2,10.142982684));
#235183=CARTESIAN_POINT('Ctrl Pts',(-4.28249658600006,11.6,10.142982684));
#235184=CARTESIAN_POINT('Ctrl Pts',(-4.28234765100005,15.2,10.139905626));
#235185=CARTESIAN_POINT('Ctrl Pts',(-4.28234765100005,11.6,10.139905626));
#235186=CARTESIAN_POINT('Ctrl Pts',(-4.28219647300006,15.2,10.136833973));
#235187=CARTESIAN_POINT('Ctrl Pts',(-4.28219647300006,11.6,10.136833973));
#235188=CARTESIAN_POINT('Ctrl Pts',(-4.28204305800006,15.2,10.133767736));
#235189=CARTESIAN_POINT('Ctrl Pts',(-4.28204305800006,11.6,10.133767736));
#235190=CARTESIAN_POINT('Ctrl Pts',(-4.28188741600006,15.2,10.130706923));
#235191=CARTESIAN_POINT('Ctrl Pts',(-4.28188741600006,11.6,10.130706923));
#235192=CARTESIAN_POINT('Ctrl Pts',(-4.28172955300006,15.2,10.127651543));
#235193=CARTESIAN_POINT('Ctrl Pts',(-4.28172955300006,11.6,10.127651543));
#235194=CARTESIAN_POINT('Ctrl Pts',(-4.28156947900006,15.2,10.124601605));
#235195=CARTESIAN_POINT('Ctrl Pts',(-4.28156947900006,11.6,10.124601605));
#235196=CARTESIAN_POINT('Ctrl Pts',(-4.28140720000005,15.2,10.121557118));
#235197=CARTESIAN_POINT('Ctrl Pts',(-4.28140720000005,11.6,10.121557118));
#235198=CARTESIAN_POINT('Ctrl Pts',(-4.28124272500006,15.2,10.118518091));
#235199=CARTESIAN_POINT('Ctrl Pts',(-4.28124272500006,11.6,10.118518091));
#235200=CARTESIAN_POINT('Ctrl Pts',(-4.28107606100006,15.2,10.115484532));
#235201=CARTESIAN_POINT('Ctrl Pts',(-4.28107606100006,11.6,10.115484532));
#235202=CARTESIAN_POINT('Ctrl Pts',(-4.28090721700006,15.2,10.112456452));
#235203=CARTESIAN_POINT('Ctrl Pts',(-4.28090721700006,11.6,10.112456452));
#235204=CARTESIAN_POINT('Ctrl Pts',(-4.28073620000006,15.2,10.109433858));
#235205=CARTESIAN_POINT('Ctrl Pts',(-4.28073620000006,11.6,10.109433858));
#235206=CARTESIAN_POINT('Ctrl Pts',(-4.28056301900006,15.2,10.106416761));
#235207=CARTESIAN_POINT('Ctrl Pts',(-4.28056301900006,11.6,10.106416761));
#235208=CARTESIAN_POINT('Ctrl Pts',(-4.28038768100006,15.2,10.103405168));
#235209=CARTESIAN_POINT('Ctrl Pts',(-4.28038768100006,11.6,10.103405168));
#235210=CARTESIAN_POINT('Ctrl Pts',(-4.28021019500005,15.2,10.10039909));
#235211=CARTESIAN_POINT('Ctrl Pts',(-4.28021019500005,11.6,10.10039909));
#235212=CARTESIAN_POINT('Ctrl Pts',(-4.28003056900006,15.2,10.097398534));
#235213=CARTESIAN_POINT('Ctrl Pts',(-4.28003056900006,11.6,10.097398534));
#235214=CARTESIAN_POINT('Ctrl Pts',(-4.27984881000006,15.2,10.094403512));
#235215=CARTESIAN_POINT('Ctrl Pts',(-4.27984881000006,11.6,10.094403512));
#235216=CARTESIAN_POINT('Ctrl Pts',(-4.27966492800006,15.2,10.09141403));
#235217=CARTESIAN_POINT('Ctrl Pts',(-4.27966492800006,11.6,10.09141403));
#235218=CARTESIAN_POINT('Ctrl Pts',(-4.27947893000006,15.2,10.088430098));
#235219=CARTESIAN_POINT('Ctrl Pts',(-4.27947893000006,11.6,10.088430098));
#235220=CARTESIAN_POINT('Ctrl Pts',(-4.27929082400006,15.2,10.085451726));
#235221=CARTESIAN_POINT('Ctrl Pts',(-4.27929082400006,11.6,10.085451726));
#235222=CARTESIAN_POINT('Ctrl Pts',(-4.27910061900006,15.2,10.082478922));
#235223=CARTESIAN_POINT('Ctrl Pts',(-4.27910061900006,11.6,10.082478922));
#235224=CARTESIAN_POINT('Ctrl Pts',(-4.27890832200006,15.2,10.079511697));
#235225=CARTESIAN_POINT('Ctrl Pts',(-4.27890832200006,11.6,10.079511697));
#235226=CARTESIAN_POINT('Ctrl Pts',(-4.27871394300006,15.2,10.076550059));
#235227=CARTESIAN_POINT('Ctrl Pts',(-4.27871394300006,11.6,10.076550059));
#235228=CARTESIAN_POINT('Ctrl Pts',(-4.27851748900006,15.2,10.073594016));
#235229=CARTESIAN_POINT('Ctrl Pts',(-4.27851748900006,11.6,10.073594016));
#235230=CARTESIAN_POINT('Ctrl Pts',(-4.27831896900006,15.2,10.070643579));
#235231=CARTESIAN_POINT('Ctrl Pts',(-4.27831896900006,11.6,10.070643579));
#235232=CARTESIAN_POINT('Ctrl Pts',(-4.27811839100006,15.2,10.067698756));
#235233=CARTESIAN_POINT('Ctrl Pts',(-4.27811839100006,11.6,10.067698756));
#235234=CARTESIAN_POINT('Ctrl Pts',(-4.27791576400006,15.2,10.064759557));
#235235=CARTESIAN_POINT('Ctrl Pts',(-4.27791576400006,11.6,10.064759557));
#235236=CARTESIAN_POINT('Ctrl Pts',(-4.27771109500005,15.2,10.061825991));
#235237=CARTESIAN_POINT('Ctrl Pts',(-4.27771109500005,11.6,10.061825991));
#235238=CARTESIAN_POINT('Ctrl Pts',(-4.27750439400006,15.2,10.058898068));
#235239=CARTESIAN_POINT('Ctrl Pts',(-4.27750439400006,11.6,10.058898068));
#235240=CARTESIAN_POINT('Ctrl Pts',(-4.27729566900005,15.2,10.055975795));
#235241=CARTESIAN_POINT('Ctrl Pts',(-4.27729566900005,11.6,10.055975795));
#235242=CARTESIAN_POINT('Ctrl Pts',(-4.27708492800006,15.2,10.053059184));
#235243=CARTESIAN_POINT('Ctrl Pts',(-4.27708492800006,11.6,10.053059184));
#235244=CARTESIAN_POINT('Ctrl Pts',(-4.27687217900006,15.2,10.050148243));
#235245=CARTESIAN_POINT('Ctrl Pts',(-4.27687217900006,11.6,10.050148243));
#235246=CARTESIAN_POINT('Ctrl Pts',(-4.27665743200006,15.2,10.047242981));
#235247=CARTESIAN_POINT('Ctrl Pts',(-4.27665743200006,11.6,10.047242981));
#235248=CARTESIAN_POINT('Ctrl Pts',(-4.27644069500006,15.2,10.044343408));
#235249=CARTESIAN_POINT('Ctrl Pts',(-4.27644069500006,11.6,10.044343408));
#235250=CARTESIAN_POINT('Ctrl Pts',(-4.27622197600006,15.2,10.041449533));
#235251=CARTESIAN_POINT('Ctrl Pts',(-4.27622197600006,11.6,10.041449533));
#235252=CARTESIAN_POINT('Ctrl Pts',(-4.27600128400006,15.2,10.038561365));
#235253=CARTESIAN_POINT('Ctrl Pts',(-4.27600128400006,11.6,10.038561365));
#235254=CARTESIAN_POINT('Ctrl Pts',(-4.27577862800006,15.2,10.035678915));
#235255=CARTESIAN_POINT('Ctrl Pts',(-4.27577862800006,11.6,10.035678915));
#235256=CARTESIAN_POINT('Ctrl Pts',(-4.27555401700006,15.2,10.032802191));
#235257=CARTESIAN_POINT('Ctrl Pts',(-4.27555401700006,11.6,10.032802191));
#235258=CARTESIAN_POINT('Ctrl Pts',(-4.27532745900006,15.2,10.029931202));
#235259=CARTESIAN_POINT('Ctrl Pts',(-4.27532745900006,11.6,10.029931202));
#235260=CARTESIAN_POINT('Ctrl Pts',(-4.27509896100006,15.2,10.027065958));
#235261=CARTESIAN_POINT('Ctrl Pts',(-4.27509896100006,11.6,10.027065958));
#235262=CARTESIAN_POINT('Ctrl Pts',(-4.27486853600006,15.2,10.024206469));
#235263=CARTESIAN_POINT('Ctrl Pts',(-4.27486853600006,11.6,10.024206469));
#235264=CARTESIAN_POINT('Ctrl Pts',(-4.27463618900005,15.2,10.021352743));
#235265=CARTESIAN_POINT('Ctrl Pts',(-4.27463618900005,11.6,10.021352743));
#235266=CARTESIAN_POINT('Ctrl Pts',(-4.27440193100006,15.2,10.018504792));
#235267=CARTESIAN_POINT('Ctrl Pts',(-4.27440193100006,11.6,10.018504792));
#235268=CARTESIAN_POINT('Ctrl Pts',(-4.27416577000006,15.2,10.015662623));
#235269=CARTESIAN_POINT('Ctrl Pts',(-4.27416577000006,11.6,10.015662623));
#235270=CARTESIAN_POINT('Ctrl Pts',(-4.27392771400006,15.2,10.012826246));
#235271=CARTESIAN_POINT('Ctrl Pts',(-4.27392771400006,11.6,10.012826246));
#235272=CARTESIAN_POINT('Ctrl Pts',(-4.27368777400006,15.2,10.009995672));
#235273=CARTESIAN_POINT('Ctrl Pts',(-4.27368777400006,11.6,10.009995672));
#235274=CARTESIAN_POINT('Ctrl Pts',(-4.27344595700006,15.2,10.007170908));
#235275=CARTESIAN_POINT('Ctrl Pts',(-4.27344595700006,11.6,10.007170908));
#235276=CARTESIAN_POINT('Ctrl Pts',(-4.27320227300005,15.2,10.004351966));
#235277=CARTESIAN_POINT('Ctrl Pts',(-4.27320227300005,11.6,10.004351966));
#235278=CARTESIAN_POINT('Ctrl Pts',(-4.27295673100006,15.2,10.001538855));
#235279=CARTESIAN_POINT('Ctrl Pts',(-4.27295673100006,11.6,10.001538855));
#235280=CARTESIAN_POINT('Ctrl Pts',(-4.27270933900005,15.2,9.99873158399998));
#235281=CARTESIAN_POINT('Ctrl Pts',(-4.27270933900005,11.6,9.99873158399998));
#235282=CARTESIAN_POINT('Ctrl Pts',(-4.27246010700006,15.2,9.99593016199999));
#235283=CARTESIAN_POINT('Ctrl Pts',(-4.27246010700006,11.6,9.99593016199999));
#235284=CARTESIAN_POINT('Ctrl Pts',(-4.27220904400006,15.2,9.99313459999998));
#235285=CARTESIAN_POINT('Ctrl Pts',(-4.27220904400006,11.6,9.99313459999998));
#235286=CARTESIAN_POINT('Ctrl Pts',(-4.27195615900006,15.2,9.99034490599998));
#235287=CARTESIAN_POINT('Ctrl Pts',(-4.27195615900006,11.6,9.99034490599998));
#235288=CARTESIAN_POINT('Ctrl Pts',(-4.27170146000006,15.2,9.98756109299999));
#235289=CARTESIAN_POINT('Ctrl Pts',(-4.27170146000006,11.6,9.98756109299999));
#235290=CARTESIAN_POINT('Ctrl Pts',(-4.27144495900006,15.2,9.98478316599999));
#235291=CARTESIAN_POINT('Ctrl Pts',(-4.27144495900006,11.6,9.98478316599999));
#235292=CARTESIAN_POINT('Ctrl Pts',(-4.27118666200006,15.2,9.98201113799999));
#235293=CARTESIAN_POINT('Ctrl Pts',(-4.27118666200006,11.6,9.98201113799999));
#235294=CARTESIAN_POINT('Ctrl Pts',(-4.27092658000006,15.2,9.97924501799999));
#235295=CARTESIAN_POINT('Ctrl Pts',(-4.27092658000006,11.6,9.97924501799999));
#235296=CARTESIAN_POINT('Ctrl Pts',(-4.27066472200006,15.2,9.97648481499999));
#235297=CARTESIAN_POINT('Ctrl Pts',(-4.27066472200006,11.6,9.97648481499999));
#235298=CARTESIAN_POINT('Ctrl Pts',(-4.27040109700005,15.2,9.97373053899998));
#235299=CARTESIAN_POINT('Ctrl Pts',(-4.27040109700005,11.6,9.97373053899998));
#235300=CARTESIAN_POINT('Ctrl Pts',(-4.27013571500006,15.2,9.97098220099998));
#235301=CARTESIAN_POINT('Ctrl Pts',(-4.27013571500006,11.6,9.97098220099998));
#235302=CARTESIAN_POINT('Ctrl Pts',(-4.26986858400006,15.2,9.96823980899999));
#235303=CARTESIAN_POINT('Ctrl Pts',(-4.26986858400006,11.6,9.96823980899999));
#235304=CARTESIAN_POINT('Ctrl Pts',(-4.26959971500006,15.2,9.96550337299999));
#235305=CARTESIAN_POINT('Ctrl Pts',(-4.26959971500006,11.6,9.96550337299999));
#235306=CARTESIAN_POINT('Ctrl Pts',(-4.26932911600006,15.2,9.96277290399998));
#235307=CARTESIAN_POINT('Ctrl Pts',(-4.26932911600006,11.6,9.96277290399998));
#235308=CARTESIAN_POINT('Ctrl Pts',(-4.26905679700006,15.2,9.96004841099998));
#235309=CARTESIAN_POINT('Ctrl Pts',(-4.26905679700006,11.6,9.96004841099998));
#235310=CARTESIAN_POINT('Ctrl Pts',(-4.26878276800006,15.2,9.95732990399999));
#235311=CARTESIAN_POINT('Ctrl Pts',(-4.26878276800006,11.6,9.95732990399999));
#235312=CARTESIAN_POINT('Ctrl Pts',(-4.26850703700006,15.2,9.95461739299999));
#235313=CARTESIAN_POINT('Ctrl Pts',(-4.26850703700006,11.6,9.95461739299999));
#235314=CARTESIAN_POINT('Ctrl Pts',(-4.26822961600006,15.2,9.95191088699999));
#235315=CARTESIAN_POINT('Ctrl Pts',(-4.26822961600006,11.6,9.95191088699999));
#235316=CARTESIAN_POINT('Ctrl Pts',(-4.26795051200005,15.2,9.94921039699998));
#235317=CARTESIAN_POINT('Ctrl Pts',(-4.26795051200005,11.6,9.94921039699998));
#235318=CARTESIAN_POINT('Ctrl Pts',(-4.26766973600006,15.2,9.94651593299999));
#235319=CARTESIAN_POINT('Ctrl Pts',(-4.26766973600006,11.6,9.94651593299999));
#235320=CARTESIAN_POINT('Ctrl Pts',(-4.26738729700006,15.2,9.94382750399998));
#235321=CARTESIAN_POINT('Ctrl Pts',(-4.26738729700006,11.6,9.94382750399998));
#235322=CARTESIAN_POINT('Ctrl Pts',(-4.26710320500006,15.2,9.94114511999998));
#235323=CARTESIAN_POINT('Ctrl Pts',(-4.26710320500006,11.6,9.94114511999998));
#235324=CARTESIAN_POINT('Ctrl Pts',(-4.26681747000006,15.2,9.93846879199998));
#235325=CARTESIAN_POINT('Ctrl Pts',(-4.26681747000006,11.6,9.93846879199998));
#235326=CARTESIAN_POINT('Ctrl Pts',(-4.26653010100006,15.2,9.93579852999999));
#235327=CARTESIAN_POINT('Ctrl Pts',(-4.26653010100006,11.6,9.93579852999999));
#235328=CARTESIAN_POINT('Ctrl Pts',(-4.26624110800006,15.2,9.93313434199998));
#235329=CARTESIAN_POINT('Ctrl Pts',(-4.26624110800006,11.6,9.93313434199998));
#235330=CARTESIAN_POINT('Ctrl Pts',(-4.26595050100006,15.2,9.93047623999999));
#235331=CARTESIAN_POINT('Ctrl Pts',(-4.26595050100006,11.6,9.93047623999999));
#235332=CARTESIAN_POINT('Ctrl Pts',(-4.26565828900006,15.2,9.92782423299998));
#235333=CARTESIAN_POINT('Ctrl Pts',(-4.26565828900006,11.6,9.92782423299998));
#235334=CARTESIAN_POINT('Ctrl Pts',(-4.26536448300006,15.2,9.92517833199998));
#235335=CARTESIAN_POINT('Ctrl Pts',(-4.26536448300006,11.6,9.92517833199998));
#235336=CARTESIAN_POINT('Ctrl Pts',(-4.26506909200006,15.2,9.92253854599999));
#235337=CARTESIAN_POINT('Ctrl Pts',(-4.26506909200006,11.6,9.92253854599999));
#235338=CARTESIAN_POINT('Ctrl Pts',(-4.26477212700005,15.2,9.91990488699999));
#235339=CARTESIAN_POINT('Ctrl Pts',(-4.26477212700005,11.6,9.91990488699999));
#235340=CARTESIAN_POINT('Ctrl Pts',(-4.26447359700005,15.2,9.91727736199999));
#235341=CARTESIAN_POINT('Ctrl Pts',(-4.26447359700005,11.6,9.91727736199999));
#235342=CARTESIAN_POINT('Ctrl Pts',(-4.26417351300006,15.2,9.91465598399999));
#235343=CARTESIAN_POINT('Ctrl Pts',(-4.26417351300006,11.6,9.91465598399999));
#235344=CARTESIAN_POINT('Ctrl Pts',(-4.26387188300006,15.2,9.91204076199999));
#235345=CARTESIAN_POINT('Ctrl Pts',(-4.26387188300006,11.6,9.91204076199999));
#235346=CARTESIAN_POINT('Ctrl Pts',(-4.26356871900006,15.2,9.90943170599999));
#235347=CARTESIAN_POINT('Ctrl Pts',(-4.26356871900006,11.6,9.90943170599999));
#235348=CARTESIAN_POINT('Ctrl Pts',(-4.26326403000005,15.2,9.90682882699998));
#235349=CARTESIAN_POINT('Ctrl Pts',(-4.26326403000005,11.6,9.90682882699998));
#235350=CARTESIAN_POINT('Ctrl Pts',(-4.26295782600006,15.2,9.90423213399998));
#235351=CARTESIAN_POINT('Ctrl Pts',(-4.26295782600006,11.6,9.90423213399998));
#235352=CARTESIAN_POINT('Ctrl Pts',(-4.26265011800006,15.2,9.90164163799999));
#235353=CARTESIAN_POINT('Ctrl Pts',(-4.26265011800006,11.6,9.90164163799999));
#235354=CARTESIAN_POINT('Ctrl Pts',(-4.26234091700006,15.2,9.89905734999999));
#235355=CARTESIAN_POINT('Ctrl Pts',(-4.26234091700006,11.6,9.89905734999999));
#235356=CARTESIAN_POINT('Ctrl Pts',(-4.26203023000006,15.2,9.89647927799999));
#235357=CARTESIAN_POINT('Ctrl Pts',(-4.26203023000006,11.6,9.89647927799999));
#235358=CARTESIAN_POINT('Ctrl Pts',(-4.26171807100006,15.2,9.89390743499998));
#235359=CARTESIAN_POINT('Ctrl Pts',(-4.26171807100006,11.6,9.89390743499998));
#235360=CARTESIAN_POINT('Ctrl Pts',(-4.26140444800006,15.2,9.89134182899999));
#235361=CARTESIAN_POINT('Ctrl Pts',(-4.26140444800006,11.6,9.89134182899999));
#235362=CARTESIAN_POINT('Ctrl Pts',(-4.26108937200006,15.2,9.88878247099999));
#235363=CARTESIAN_POINT('Ctrl Pts',(-4.26108937200006,11.6,9.88878247099999));
#235364=CARTESIAN_POINT('Ctrl Pts',(-4.26077285200006,15.2,9.88622937299999));
#235365=CARTESIAN_POINT('Ctrl Pts',(-4.26077285200006,11.6,9.88622937299999));
#235366=CARTESIAN_POINT('Ctrl Pts',(-4.26045490200006,15.2,9.88368254399998));
#235367=CARTESIAN_POINT('Ctrl Pts',(-4.26045490200006,11.6,9.88368254399998));
#235368=CARTESIAN_POINT('Ctrl Pts',(-4.26013552800006,15.2,9.88114199399998));
#235369=CARTESIAN_POINT('Ctrl Pts',(-4.26013552800006,11.6,9.88114199399998));
#235370=CARTESIAN_POINT('Ctrl Pts',(-4.25981474300006,15.2,9.87860773299998));
#235371=CARTESIAN_POINT('Ctrl Pts',(-4.25981474300006,11.6,9.87860773299998));
#235372=CARTESIAN_POINT('Ctrl Pts',(-4.25949255700006,15.2,9.87607977399998));
#235373=CARTESIAN_POINT('Ctrl Pts',(-4.25949255700006,11.6,9.87607977399998));
#235374=CARTESIAN_POINT('Ctrl Pts',(-4.25916898100006,15.2,9.87355812399999));
#235375=CARTESIAN_POINT('Ctrl Pts',(-4.25916898100006,11.6,9.87355812399999));
#235376=CARTESIAN_POINT('Ctrl Pts',(-4.25884402500006,15.2,9.87104279699999));
#235377=CARTESIAN_POINT('Ctrl Pts',(-4.25884402500006,11.6,9.87104279699999));
#235378=CARTESIAN_POINT('Ctrl Pts',(-4.25851769900006,15.2,9.86853380099999));
#235379=CARTESIAN_POINT('Ctrl Pts',(-4.25851769900006,11.6,9.86853380099999));
#235380=CARTESIAN_POINT('Ctrl Pts',(-4.25819001500006,15.2,9.86603114699999));
#235381=CARTESIAN_POINT('Ctrl Pts',(-4.25819001500006,11.6,9.86603114699999));
#235382=CARTESIAN_POINT('Ctrl Pts',(-4.25786098300006,15.2,9.86353484599999));
#235383=CARTESIAN_POINT('Ctrl Pts',(-4.25786098300006,11.6,9.86353484599999));
#235384=CARTESIAN_POINT('Ctrl Pts',(-4.25753061300005,15.2,9.86104490899999));
#235385=CARTESIAN_POINT('Ctrl Pts',(-4.25753061300005,11.6,9.86104490899999));
#235386=CARTESIAN_POINT('Ctrl Pts',(-4.25719891700005,15.2,9.85856134499999));
#235387=CARTESIAN_POINT('Ctrl Pts',(-4.25719891700005,11.6,9.85856134499999));
#235388=CARTESIAN_POINT('Ctrl Pts',(-4.25686590500006,15.2,9.85608416599998));
#235389=CARTESIAN_POINT('Ctrl Pts',(-4.25686590500006,11.6,9.85608416599998));
#235390=CARTESIAN_POINT('Ctrl Pts',(-4.25653158900006,15.2,9.85361338199999));
#235391=CARTESIAN_POINT('Ctrl Pts',(-4.25653158900006,11.6,9.85361338199999));
#235392=CARTESIAN_POINT('Ctrl Pts',(-4.25619597800006,15.2,9.85114900499998));
#235393=CARTESIAN_POINT('Ctrl Pts',(-4.25619597800006,11.6,9.85114900499998));
#235394=CARTESIAN_POINT('Ctrl Pts',(-4.25585908500006,15.2,9.84869104299998));
#235395=CARTESIAN_POINT('Ctrl Pts',(-4.25585908500006,11.6,9.84869104299998));
#235396=CARTESIAN_POINT('Ctrl Pts',(-4.25552091900006,15.2,9.84623950899999));
#235397=CARTESIAN_POINT('Ctrl Pts',(-4.25552091900006,11.6,9.84623950899999));
#235398=CARTESIAN_POINT('Ctrl Pts',(-4.25518149200006,15.2,9.84379441199999));
#235399=CARTESIAN_POINT('Ctrl Pts',(-4.25518149200006,11.6,9.84379441199999));
#235400=CARTESIAN_POINT('Ctrl Pts',(-4.25484081400006,15.2,9.84135576499998));
#235401=CARTESIAN_POINT('Ctrl Pts',(-4.25484081400006,11.6,9.84135576499998));
#235402=CARTESIAN_POINT('Ctrl Pts',(-4.25449889700006,15.2,9.83892357599998));
#235403=CARTESIAN_POINT('Ctrl Pts',(-4.25449889700006,11.6,9.83892357599998));
#235404=CARTESIAN_POINT('Ctrl Pts',(-4.25415575200006,15.2,9.83649785799999));
#235405=CARTESIAN_POINT('Ctrl Pts',(-4.25415575200006,11.6,9.83649785799999));
#235406=CARTESIAN_POINT('Ctrl Pts',(-4.25381139100006,15.2,9.83407861999999));
#235407=CARTESIAN_POINT('Ctrl Pts',(-4.25381139100006,11.6,9.83407861999999));
#235408=CARTESIAN_POINT('Ctrl Pts',(-4.25346582400006,15.2,9.83166587499999));
#235409=CARTESIAN_POINT('Ctrl Pts',(-4.25346582400006,11.6,9.83166587499999));
#235410=CARTESIAN_POINT('Ctrl Pts',(-4.25311906200006,15.2,9.82925963199998));
#235411=CARTESIAN_POINT('Ctrl Pts',(-4.25311906200006,11.6,9.82925963199998));
#235412=CARTESIAN_POINT('Ctrl Pts',(-4.25277111700006,15.2,9.82685990299998));
#235413=CARTESIAN_POINT('Ctrl Pts',(-4.25277111700006,11.6,9.82685990299998));
#235414=CARTESIAN_POINT('Ctrl Pts',(-4.25242199900006,15.2,9.82446669799998));
#235415=CARTESIAN_POINT('Ctrl Pts',(-4.25242199900006,11.6,9.82446669799998));
#235416=CARTESIAN_POINT('Ctrl Pts',(-4.25207172200006,15.2,9.82208002899998));
#235417=CARTESIAN_POINT('Ctrl Pts',(-4.25207172200006,11.6,9.82208002899998));
#235418=CARTESIAN_POINT('Ctrl Pts',(-4.25172029400006,15.2,9.81969990599998));
#235419=CARTESIAN_POINT('Ctrl Pts',(-4.25172029400006,11.6,9.81969990599998));
#235420=CARTESIAN_POINT('Ctrl Pts',(-4.25136773000006,15.2,9.81732633999999));
#235421=CARTESIAN_POINT('Ctrl Pts',(-4.25136773000006,11.6,9.81732633999999));
#235422=CARTESIAN_POINT('Ctrl Pts',(-4.25101403800006,15.2,9.81495934199998));
#235423=CARTESIAN_POINT('Ctrl Pts',(-4.25101403800006,11.6,9.81495934199998));
#235424=CARTESIAN_POINT('Ctrl Pts',(-4.25065923100005,15.2,9.81259892299999));
#235425=CARTESIAN_POINT('Ctrl Pts',(-4.25065923100005,11.6,9.81259892299999));
#235426=CARTESIAN_POINT('Ctrl Pts',(-4.25030332100006,15.2,9.81024509399998));
#235427=CARTESIAN_POINT('Ctrl Pts',(-4.25030332100006,11.6,9.81024509399998));
#235428=CARTESIAN_POINT('Ctrl Pts',(-4.24994631900006,15.2,9.80789786699999));
#235429=CARTESIAN_POINT('Ctrl Pts',(-4.24994631900006,11.6,9.80789786699999));
#235430=CARTESIAN_POINT('Ctrl Pts',(-4.24958823700006,15.2,9.80555725299999));
#235431=CARTESIAN_POINT('Ctrl Pts',(-4.24958823700006,11.6,9.80555725299999));
#235432=CARTESIAN_POINT('Ctrl Pts',(-4.24922908600006,15.2,9.80322326199998));
#235433=CARTESIAN_POINT('Ctrl Pts',(-4.24922908600006,11.6,9.80322326199998));
#235434=CARTESIAN_POINT('Ctrl Pts',(-4.24886887800006,15.2,9.80089590599999));
#235435=CARTESIAN_POINT('Ctrl Pts',(-4.24886887800006,11.6,9.80089590599999));
#235436=CARTESIAN_POINT('Ctrl Pts',(-4.24850762500006,15.2,9.79857519499999));
#235437=CARTESIAN_POINT('Ctrl Pts',(-4.24850762500006,11.6,9.79857519499999));
#235438=CARTESIAN_POINT('Ctrl Pts',(-4.24814533900006,15.2,9.79626114099998));
#235439=CARTESIAN_POINT('Ctrl Pts',(-4.24814533900006,11.6,9.79626114099998));
#235440=CARTESIAN_POINT('Ctrl Pts',(-4.24778203100006,15.2,9.79395375599999));
#235441=CARTESIAN_POINT('Ctrl Pts',(-4.24778203100006,11.6,9.79395375599999));
#235442=CARTESIAN_POINT('Ctrl Pts',(-4.24741771300006,15.2,9.79165304999999));
#235443=CARTESIAN_POINT('Ctrl Pts',(-4.24741771300006,11.6,9.79165304999999));
#235444=CARTESIAN_POINT('Ctrl Pts',(-4.24705239800006,15.2,9.78935903399999));
#235445=CARTESIAN_POINT('Ctrl Pts',(-4.24705239800006,11.6,9.78935903399999));
#235446=CARTESIAN_POINT('Ctrl Pts',(-4.24668609600006,15.2,9.78707172099998));
#235447=CARTESIAN_POINT('Ctrl Pts',(-4.24668609600006,11.6,9.78707172099998));
#235448=CARTESIAN_POINT('Ctrl Pts',(-4.24631882000006,15.2,9.78479112099999));
#235449=CARTESIAN_POINT('Ctrl Pts',(-4.24631882000006,11.6,9.78479112099999));
#235450=CARTESIAN_POINT('Ctrl Pts',(-4.24595058300006,15.2,9.78251724599998));
#235451=CARTESIAN_POINT('Ctrl Pts',(-4.24595058300006,11.6,9.78251724599998));
#235452=CARTESIAN_POINT('Ctrl Pts',(-4.24558139600006,15.2,9.78025010599998));
#235453=CARTESIAN_POINT('Ctrl Pts',(-4.24558139600006,11.6,9.78025010599998));
#235454=CARTESIAN_POINT('Ctrl Pts',(-4.24521127100006,15.2,9.77798971399999));
#235455=CARTESIAN_POINT('Ctrl Pts',(-4.24521127100006,11.6,9.77798971399999));
#235456=CARTESIAN_POINT('Ctrl Pts',(-4.24484022100006,15.2,9.77573607999998));
#235457=CARTESIAN_POINT('Ctrl Pts',(-4.24484022100006,11.6,9.77573607999998));
#235458=CARTESIAN_POINT('Ctrl Pts',(-4.24446825700006,15.2,9.77348921599998));
#235459=CARTESIAN_POINT('Ctrl Pts',(-4.24446825700006,11.6,9.77348921599998));
#235460=CARTESIAN_POINT('Ctrl Pts',(-4.24409539300005,15.2,9.77124913399999));
#235461=CARTESIAN_POINT('Ctrl Pts',(-4.24409539300005,11.6,9.77124913399999));
#235462=CARTESIAN_POINT('Ctrl Pts',(-4.24372163900006,15.2,9.76901584499998));
#235463=CARTESIAN_POINT('Ctrl Pts',(-4.24372163900006,11.6,9.76901584499998));
#235464=CARTESIAN_POINT('Ctrl Pts',(-4.24334701000006,15.2,9.76678936199999));
#235465=CARTESIAN_POINT('Ctrl Pts',(-4.24334701000006,11.6,9.76678936199999));
#235466=CARTESIAN_POINT('Ctrl Pts',(-4.24297151500006,15.2,9.76456969299999));
#235467=CARTESIAN_POINT('Ctrl Pts',(-4.24297151500006,11.6,9.76456969299999));
#235468=CARTESIAN_POINT('Ctrl Pts',(-4.24259517000006,15.2,9.76235685299999));
#235469=CARTESIAN_POINT('Ctrl Pts',(-4.24259517000006,11.6,9.76235685299999));
#235470=CARTESIAN_POINT('Ctrl Pts',(-4.24221798600006,15.2,9.76015085199998));
#235471=CARTESIAN_POINT('Ctrl Pts',(-4.24221798600006,11.6,9.76015085199998));
#235472=CARTESIAN_POINT('Ctrl Pts',(-4.24183997500006,15.2,9.75795170199999));
#235473=CARTESIAN_POINT('Ctrl Pts',(-4.24183997500006,11.6,9.75795170199999));
#235474=CARTESIAN_POINT('Ctrl Pts',(-4.24146114900006,15.2,9.75575941499999));
#235475=CARTESIAN_POINT('Ctrl Pts',(-4.24146114900006,11.6,9.75575941499999));
#235476=CARTESIAN_POINT('Ctrl Pts',(-4.24108152400006,15.2,9.75357400099998));
#235477=CARTESIAN_POINT('Ctrl Pts',(-4.24108152400006,11.6,9.75357400099998));
#235478=CARTESIAN_POINT('Ctrl Pts',(-4.24070110900006,15.2,9.75139547399999));
#235479=CARTESIAN_POINT('Ctrl Pts',(-4.24070110900006,11.6,9.75139547399999));
#235480=CARTESIAN_POINT('Ctrl Pts',(-4.24031991700006,15.2,9.74922384499998));
#235481=CARTESIAN_POINT('Ctrl Pts',(-4.24031991700006,11.6,9.74922384499998));
#235482=CARTESIAN_POINT('Ctrl Pts',(-4.23993796200006,15.2,9.74705912499999));
#235483=CARTESIAN_POINT('Ctrl Pts',(-4.23993796200006,11.6,9.74705912499999));
#235484=CARTESIAN_POINT('Ctrl Pts',(-4.23955525800006,15.2,9.74490132499999));
#235485=CARTESIAN_POINT('Ctrl Pts',(-4.23955525800006,11.6,9.74490132499999));
#235486=CARTESIAN_POINT('Ctrl Pts',(-4.23917181600006,15.2,9.74275045999999));
#235487=CARTESIAN_POINT('Ctrl Pts',(-4.23917181600006,11.6,9.74275045999999));
#235488=CARTESIAN_POINT('Ctrl Pts',(-4.23878764900006,15.2,9.74060653899999));
#235489=CARTESIAN_POINT('Ctrl Pts',(-4.23878764900006,11.6,9.74060653899999));
#235490=CARTESIAN_POINT('Ctrl Pts',(-4.23840277000005,15.2,9.73846957399999));
#235491=CARTESIAN_POINT('Ctrl Pts',(-4.23840277000005,11.6,9.73846957399999));
#235492=CARTESIAN_POINT('Ctrl Pts',(-4.23801719200006,15.2,9.73633957899998));
#235493=CARTESIAN_POINT('Ctrl Pts',(-4.23801719200006,11.6,9.73633957899998));
#235494=CARTESIAN_POINT('Ctrl Pts',(-4.23763092900006,15.2,9.73421656399999));
#235495=CARTESIAN_POINT('Ctrl Pts',(-4.23763092900006,11.6,9.73421656399999));
#235496=CARTESIAN_POINT('Ctrl Pts',(-4.23724399200006,15.2,9.73210054199999));
#235497=CARTESIAN_POINT('Ctrl Pts',(-4.23724399200006,11.6,9.73210054199999));
#235498=CARTESIAN_POINT('Ctrl Pts',(-4.23685639800006,15.2,9.72999152399998));
#235499=CARTESIAN_POINT('Ctrl Pts',(-4.23685639800006,11.6,9.72999152399998));
#235500=CARTESIAN_POINT('Ctrl Pts',(-4.23646815600006,15.2,9.72788952199998));
#235501=CARTESIAN_POINT('Ctrl Pts',(-4.23646815600006,11.6,9.72788952199998));
#235502=CARTESIAN_POINT('Ctrl Pts',(-4.23607928100005,15.2,9.72579454999998));
#235503=CARTESIAN_POINT('Ctrl Pts',(-4.23607928100005,11.6,9.72579454999998));
#235504=CARTESIAN_POINT('Ctrl Pts',(-4.23568978700006,15.2,9.72370661699999));
#235505=CARTESIAN_POINT('Ctrl Pts',(-4.23568978700006,11.6,9.72370661699999));
#235506=CARTESIAN_POINT('Ctrl Pts',(-4.23529968600006,15.2,9.72162573799999));
#235507=CARTESIAN_POINT('Ctrl Pts',(-4.23529968600006,11.6,9.72162573799999));
#235508=CARTESIAN_POINT('Ctrl Pts',(-4.23490899300006,15.2,9.71955192299998));
#235509=CARTESIAN_POINT('Ctrl Pts',(-4.23490899300006,11.6,9.71955192299998));
#235510=CARTESIAN_POINT('Ctrl Pts',(-4.23451772000006,15.2,9.71748518599998));
#235511=CARTESIAN_POINT('Ctrl Pts',(-4.23451772000006,11.6,9.71748518599998));
#235512=CARTESIAN_POINT('Ctrl Pts',(-4.23412588100006,15.2,9.71542553699998));
#235513=CARTESIAN_POINT('Ctrl Pts',(-4.23412588100006,11.6,9.71542553699998));
#235514=CARTESIAN_POINT('Ctrl Pts',(-4.23373349000006,15.2,9.71337299099999));
#235515=CARTESIAN_POINT('Ctrl Pts',(-4.23373349000006,11.6,9.71337299099999));
#235516=CARTESIAN_POINT('Ctrl Pts',(-4.23334055900006,15.2,9.71132755799999));
#235517=CARTESIAN_POINT('Ctrl Pts',(-4.23334055900006,11.6,9.71132755799999));
#235518=CARTESIAN_POINT('Ctrl Pts',(-4.23294710300006,15.2,9.70928924999999));
#235519=CARTESIAN_POINT('Ctrl Pts',(-4.23294710300006,11.6,9.70928924999999));
#235520=CARTESIAN_POINT('Ctrl Pts',(-4.23255313500006,15.2,9.70725808199998));
#235521=CARTESIAN_POINT('Ctrl Pts',(-4.23255313500006,11.6,9.70725808199998));
#235522=CARTESIAN_POINT('Ctrl Pts',(-4.23215867100006,15.2,9.70523406399998));
#235523=CARTESIAN_POINT('Ctrl Pts',(-4.23215867100006,11.6,9.70523406399998));
#235524=CARTESIAN_POINT('Ctrl Pts',(-4.23176372200006,15.2,9.70321720899998));
#235525=CARTESIAN_POINT('Ctrl Pts',(-4.23176372200006,11.6,9.70321720899998));
#235526=CARTESIAN_POINT('Ctrl Pts',(-4.23136830300006,15.2,9.70120752899999));
#235527=CARTESIAN_POINT('Ctrl Pts',(-4.23136830300006,11.6,9.70120752899999));
#235528=CARTESIAN_POINT('Ctrl Pts',(-4.23097242800006,15.2,9.69920503799998));
#235529=CARTESIAN_POINT('Ctrl Pts',(-4.23097242800006,11.6,9.69920503799998));
#235530=CARTESIAN_POINT('Ctrl Pts',(-4.23057611000006,15.2,9.69720974699998));
#235531=CARTESIAN_POINT('Ctrl Pts',(-4.23057611000006,11.6,9.69720974699998));
#235532=CARTESIAN_POINT('Ctrl Pts',(-4.23017936500006,15.2,9.69522166899999));
#235533=CARTESIAN_POINT('Ctrl Pts',(-4.23017936500006,11.6,9.69522166899999));
#235534=CARTESIAN_POINT('Ctrl Pts',(-4.22978220600006,15.2,9.69324081599999));
#235535=CARTESIAN_POINT('Ctrl Pts',(-4.22978220600006,11.6,9.69324081599999));
#235536=CARTESIAN_POINT('Ctrl Pts',(-4.22938464600006,15.2,9.69126720099998));
#235537=CARTESIAN_POINT('Ctrl Pts',(-4.22938464600006,11.6,9.69126720099998));
#235538=CARTESIAN_POINT('Ctrl Pts',(-4.22898670100006,15.2,9.68930083699998));
#235539=CARTESIAN_POINT('Ctrl Pts',(-4.22898670100006,11.6,9.68930083699998));
#235540=CARTESIAN_POINT('Ctrl Pts',(-4.22858838400006,15.2,9.68734173599999));
#235541=CARTESIAN_POINT('Ctrl Pts',(-4.22858838400006,11.6,9.68734173599999));
#235542=CARTESIAN_POINT('Ctrl Pts',(-4.22818971000006,15.2,9.68538991099999));
#235543=CARTESIAN_POINT('Ctrl Pts',(-4.22818971000006,11.6,9.68538991099999));
#235544=CARTESIAN_POINT('Ctrl Pts',(-4.22779069300006,15.2,9.68344537499998));
#235545=CARTESIAN_POINT('Ctrl Pts',(-4.22779069300006,11.6,9.68344537499998));
#235546=CARTESIAN_POINT('Ctrl Pts',(-4.22739134800006,15.2,9.68150814099998));
#235547=CARTESIAN_POINT('Ctrl Pts',(-4.22739134800006,11.6,9.68150814099998));
#235548=CARTESIAN_POINT('Ctrl Pts',(-4.22699168900006,15.2,9.67957821999999));
#235549=CARTESIAN_POINT('Ctrl Pts',(-4.22699168900006,11.6,9.67957821999999));
#235550=CARTESIAN_POINT('Ctrl Pts',(-4.22659173000006,15.2,9.67765562699999));
#235551=CARTESIAN_POINT('Ctrl Pts',(-4.22659173000006,11.6,9.67765562699999));
#235552=CARTESIAN_POINT('Ctrl Pts',(-4.22619148700006,15.2,9.67574037199999));
#235553=CARTESIAN_POINT('Ctrl Pts',(-4.22619148700006,11.6,9.67574037199999));
#235554=CARTESIAN_POINT('Ctrl Pts',(-4.22579097300006,15.2,9.67383247099999));
#235555=CARTESIAN_POINT('Ctrl Pts',(-4.22579097300006,11.6,9.67383247099999));
#235556=CARTESIAN_POINT('Ctrl Pts',(-4.22539020400006,15.2,9.67193193599999));
#235557=CARTESIAN_POINT('Ctrl Pts',(-4.22539020400006,11.6,9.67193193599999));
#235558=CARTESIAN_POINT('Ctrl Pts',(-4.22498919400006,15.2,9.67003877999998));
#235559=CARTESIAN_POINT('Ctrl Pts',(-4.22498919400006,11.6,9.67003877999998));
#235560=CARTESIAN_POINT('Ctrl Pts',(-4.22458795900006,15.2,9.66815301399999));
#235561=CARTESIAN_POINT('Ctrl Pts',(-4.22458795900006,11.6,9.66815301399999));
#235562=CARTESIAN_POINT('Ctrl Pts',(-4.22418651100006,15.2,9.66627465399998));
#235563=CARTESIAN_POINT('Ctrl Pts',(-4.22418651100006,11.6,9.66627465399998));
#235564=CARTESIAN_POINT('Ctrl Pts',(-4.22378486900006,15.2,9.66440371099999));
#235565=CARTESIAN_POINT('Ctrl Pts',(-4.22378486900006,11.6,9.66440371099999));
#235566=CARTESIAN_POINT('Ctrl Pts',(-4.22338304400006,15.2,9.66254019799998));
#235567=CARTESIAN_POINT('Ctrl Pts',(-4.22338304400006,11.6,9.66254019799998));
#235568=CARTESIAN_POINT('Ctrl Pts',(-4.22298105500006,15.2,9.66068412999999));
#235569=CARTESIAN_POINT('Ctrl Pts',(-4.22298105500006,11.6,9.66068412999999));
#235570=CARTESIAN_POINT('Ctrl Pts',(-4.22257891300006,15.2,9.65883551899999));
#235571=CARTESIAN_POINT('Ctrl Pts',(-4.22257891300006,11.6,9.65883551899999));
#235572=CARTESIAN_POINT('Ctrl Pts',(-4.22217663700006,15.2,9.65699437699998));
#235573=CARTESIAN_POINT('Ctrl Pts',(-4.22217663700006,11.6,9.65699437699998));
#235574=CARTESIAN_POINT('Ctrl Pts',(-4.22177423900005,15.2,9.65516071999998));
#235575=CARTESIAN_POINT('Ctrl Pts',(-4.22177423900005,11.6,9.65516071999998));
#235576=CARTESIAN_POINT('Ctrl Pts',(-4.22137173800006,15.2,9.65333455899999));
#235577=CARTESIAN_POINT('Ctrl Pts',(-4.22137173800006,11.6,9.65333455899999));
#235578=CARTESIAN_POINT('Ctrl Pts',(-4.22096914500006,15.2,9.65151590699998));
#235579=CARTESIAN_POINT('Ctrl Pts',(-4.22096914500006,11.6,9.65151590699998));
#235580=CARTESIAN_POINT('Ctrl Pts',(-4.22056647800006,15.2,9.64970477999999));
#235581=CARTESIAN_POINT('Ctrl Pts',(-4.22056647800006,11.6,9.64970477999999));
#235582=CARTESIAN_POINT('Ctrl Pts',(-4.22016375200006,15.2,9.64790118999998));
#235583=CARTESIAN_POINT('Ctrl Pts',(-4.22016375200006,11.6,9.64790118999998));
#235584=CARTESIAN_POINT('Ctrl Pts',(-4.21976098500005,15.2,9.64610514899999));
#235585=CARTESIAN_POINT('Ctrl Pts',(-4.21976098500005,11.6,9.64610514899999));
#235586=CARTESIAN_POINT('Ctrl Pts',(-4.21935818800006,15.2,9.64431667199998));
#235587=CARTESIAN_POINT('Ctrl Pts',(-4.21935818800006,11.6,9.64431667199998));
#235588=CARTESIAN_POINT('Ctrl Pts',(-4.21895537900006,15.2,9.64253577199998));
#235589=CARTESIAN_POINT('Ctrl Pts',(-4.21895537900006,11.6,9.64253577199998));
#235590=CARTESIAN_POINT('Ctrl Pts',(-4.21855257300006,15.2,9.64076246299998));
#235591=CARTESIAN_POINT('Ctrl Pts',(-4.21855257300006,11.6,9.64076246299998));
#235592=CARTESIAN_POINT('Ctrl Pts',(-4.21814978800006,15.2,9.63899675899999));
#235593=CARTESIAN_POINT('Ctrl Pts',(-4.21814978800006,11.6,9.63899675899999));
#235594=CARTESIAN_POINT('Ctrl Pts',(-4.21774703800006,15.2,9.63723867199998));
#235595=CARTESIAN_POINT('Ctrl Pts',(-4.21774703800006,11.6,9.63723867199998));
#235596=CARTESIAN_POINT('Ctrl Pts',(-4.21734434000006,15.2,9.63548821799998));
#235597=CARTESIAN_POINT('Ctrl Pts',(-4.21734434000006,11.6,9.63548821799998));
#235598=CARTESIAN_POINT('Ctrl Pts',(-4.21694170800006,15.2,9.63374540799999));
#235599=CARTESIAN_POINT('Ctrl Pts',(-4.21694170800006,11.6,9.63374540799999));
#235600=CARTESIAN_POINT('Ctrl Pts',(-4.21653916000006,15.2,9.63201025699998));
#235601=CARTESIAN_POINT('Ctrl Pts',(-4.21653916000006,11.6,9.63201025699998));
#235602=CARTESIAN_POINT('Ctrl Pts',(-4.21613671100006,15.2,9.63028277899999));
#235603=CARTESIAN_POINT('Ctrl Pts',(-4.21613671100006,11.6,9.63028277899999));
#235604=CARTESIAN_POINT('Ctrl Pts',(-4.21573437800006,15.2,9.62856298799998));
#235605=CARTESIAN_POINT('Ctrl Pts',(-4.21573437800006,11.6,9.62856298799998));
#235606=CARTESIAN_POINT('Ctrl Pts',(-4.21533217800006,15.2,9.62685089699999));
#235607=CARTESIAN_POINT('Ctrl Pts',(-4.21533217800006,11.6,9.62685089699999));
#235608=CARTESIAN_POINT('Ctrl Pts',(-4.21493012500005,15.2,9.62514652099999));
#235609=CARTESIAN_POINT('Ctrl Pts',(-4.21493012500005,11.6,9.62514652099999));
#235610=CARTESIAN_POINT('Ctrl Pts',(-4.21452823700006,15.2,9.62344987199998));
#235611=CARTESIAN_POINT('Ctrl Pts',(-4.21452823700006,11.6,9.62344987199998));
#235612=CARTESIAN_POINT('Ctrl Pts',(-4.21412653100006,15.2,9.62176096799999));
#235613=CARTESIAN_POINT('Ctrl Pts',(-4.21412653100006,11.6,9.62176096799999));
#235614=CARTESIAN_POINT('Ctrl Pts',(-4.21372502200006,15.2,9.62007981799999));
#235615=CARTESIAN_POINT('Ctrl Pts',(-4.21372502200006,11.6,9.62007981799999));
#235616=CARTESIAN_POINT('Ctrl Pts',(-4.21332372900006,15.2,9.61840643899999));
#235617=CARTESIAN_POINT('Ctrl Pts',(-4.21332372900006,11.6,9.61840643899999));
#235618=CARTESIAN_POINT('Ctrl Pts',(-4.21292266500005,15.2,9.61674084599998));
#235619=CARTESIAN_POINT('Ctrl Pts',(-4.21292266500005,11.6,9.61674084599998));
#235620=CARTESIAN_POINT('Ctrl Pts',(-4.21252185100006,15.2,9.61508304999998));
#235621=CARTESIAN_POINT('Ctrl Pts',(-4.21252185100006,11.6,9.61508304999998));
#235622=CARTESIAN_POINT('Ctrl Pts',(-4.21212130000006,15.2,9.61343306699998));
#235623=CARTESIAN_POINT('Ctrl Pts',(-4.21212130000006,11.6,9.61343306699998));
#235624=CARTESIAN_POINT('Ctrl Pts',(-4.21172103100006,15.2,9.61179091199998));
#235625=CARTESIAN_POINT('Ctrl Pts',(-4.21172103100006,11.6,9.61179091199998));
#235626=CARTESIAN_POINT('Ctrl Pts',(-4.21132106100006,15.2,9.61015659799998));
#235627=CARTESIAN_POINT('Ctrl Pts',(-4.21132106100006,11.6,9.61015659799998));
#235628=CARTESIAN_POINT('Ctrl Pts',(-4.21092140700006,15.2,9.60853013999999));
#235629=CARTESIAN_POINT('Ctrl Pts',(-4.21092140700006,11.6,9.60853013999999));
#235630=CARTESIAN_POINT('Ctrl Pts',(-4.21052208400006,15.2,9.60691155199999));
#235631=CARTESIAN_POINT('Ctrl Pts',(-4.21052208400006,11.6,9.60691155199999));
#235632=CARTESIAN_POINT('Ctrl Pts',(-4.21012311300006,15.2,9.60530084899998));
#235633=CARTESIAN_POINT('Ctrl Pts',(-4.21012311300006,11.6,9.60530084899998));
#235634=CARTESIAN_POINT('Ctrl Pts',(-4.20972450800006,15.2,9.60369804499998));
#235635=CARTESIAN_POINT('Ctrl Pts',(-4.20972450800006,11.6,9.60369804499998));
#235636=CARTESIAN_POINT('Ctrl Pts',(-4.20932628800006,15.2,9.60210315399999));
#235637=CARTESIAN_POINT('Ctrl Pts',(-4.20932628800006,11.6,9.60210315399999));
#235638=CARTESIAN_POINT('Ctrl Pts',(-4.20892847000006,15.2,9.60051619099998));
#235639=CARTESIAN_POINT('Ctrl Pts',(-4.20892847000006,11.6,9.60051619099998));
#235640=CARTESIAN_POINT('Ctrl Pts',(-4.20853107200006,15.2,9.59893717199999));
#235641=CARTESIAN_POINT('Ctrl Pts',(-4.20853107200006,11.6,9.59893717199999));
#235642=CARTESIAN_POINT('Ctrl Pts',(-4.20813411000006,15.2,9.59736610999999));
#235643=CARTESIAN_POINT('Ctrl Pts',(-4.20813411000006,11.6,9.59736610999999));
#235644=CARTESIAN_POINT('Ctrl Pts',(-4.20773760400006,15.2,9.59580301999999));
#235645=CARTESIAN_POINT('Ctrl Pts',(-4.20773760400006,11.6,9.59580301999999));
#235646=CARTESIAN_POINT('Ctrl Pts',(-4.20734156900005,15.2,9.59424791599999));
#235647=CARTESIAN_POINT('Ctrl Pts',(-4.20734156900005,11.6,9.59424791599999));
#235648=CARTESIAN_POINT('Ctrl Pts',(-4.20694602600006,15.2,9.59270081399998));
#235649=CARTESIAN_POINT('Ctrl Pts',(-4.20694602600006,11.6,9.59270081399998));
#235650=CARTESIAN_POINT('Ctrl Pts',(-4.20655098900006,15.2,9.59116172999998));
#235651=CARTESIAN_POINT('Ctrl Pts',(-4.20655098900006,11.6,9.59116172999998));
#235652=CARTESIAN_POINT('Ctrl Pts',(-4.20615648000005,15.2,9.58963067599999));
#235653=CARTESIAN_POINT('Ctrl Pts',(-4.20615648000005,11.6,9.58963067599999));
#235654=CARTESIAN_POINT('Ctrl Pts',(-4.20576251400006,15.2,9.58810766899998));
#235655=CARTESIAN_POINT('Ctrl Pts',(-4.20576251400006,11.6,9.58810766899998));
#235656=CARTESIAN_POINT('Ctrl Pts',(-4.20536911100006,15.2,9.58659272299998));
#235657=CARTESIAN_POINT('Ctrl Pts',(-4.20536911100006,11.6,9.58659272299998));
#235658=CARTESIAN_POINT('Ctrl Pts',(-4.20497628800006,15.2,9.58508585299998));
#235659=CARTESIAN_POINT('Ctrl Pts',(-4.20497628800006,11.6,9.58508585299998));
#235660=CARTESIAN_POINT('Ctrl Pts',(-4.20458406400006,15.2,9.58358707499999));
#235661=CARTESIAN_POINT('Ctrl Pts',(-4.20458406400006,11.6,9.58358707499999));
#235662=CARTESIAN_POINT('Ctrl Pts',(-4.20419245700006,15.2,9.58209640399998));
#235663=CARTESIAN_POINT('Ctrl Pts',(-4.20419245700006,11.6,9.58209640399998));
#235664=CARTESIAN_POINT('Ctrl Pts',(-4.20380148500006,15.2,9.58061385399999));
#235665=CARTESIAN_POINT('Ctrl Pts',(-4.20380148500006,11.6,9.58061385399999));
#235666=CARTESIAN_POINT('Ctrl Pts',(-4.20341116800006,15.2,9.57913944099998));
#235667=CARTESIAN_POINT('Ctrl Pts',(-4.20341116800006,11.6,9.57913944099998));
#235668=CARTESIAN_POINT('Ctrl Pts',(-4.20302152300006,15.2,9.57767318099998));
#235669=CARTESIAN_POINT('Ctrl Pts',(-4.20302152300006,11.6,9.57767318099998));
#235670=CARTESIAN_POINT('Ctrl Pts',(-4.20263256900006,15.2,9.57621508899998));
#235671=CARTESIAN_POINT('Ctrl Pts',(-4.20263256900006,11.6,9.57621508899998));
#235672=CARTESIAN_POINT('Ctrl Pts',(-4.20224432600006,15.2,9.57476517899998));
#235673=CARTESIAN_POINT('Ctrl Pts',(-4.20224432600006,11.6,9.57476517899998));
#235674=CARTESIAN_POINT('Ctrl Pts',(-4.20185681200006,15.2,9.57332346799999));
#235675=CARTESIAN_POINT('Ctrl Pts',(-4.20185681200006,11.6,9.57332346799999));
#235676=CARTESIAN_POINT('Ctrl Pts',(-4.20147004500006,15.2,9.57188997099998));
#235677=CARTESIAN_POINT('Ctrl Pts',(-4.20147004500006,11.6,9.57188997099998));
#235678=CARTESIAN_POINT('Ctrl Pts',(-4.20108404600006,15.2,9.57046470299998));
#235679=CARTESIAN_POINT('Ctrl Pts',(-4.20108404600006,11.6,9.57046470299998));
#235680=CARTESIAN_POINT('Ctrl Pts',(-4.20069883300005,15.2,9.56904768099999));
#235681=CARTESIAN_POINT('Ctrl Pts',(-4.20069883300005,11.6,9.56904768099999));
#235682=CARTESIAN_POINT('Ctrl Pts',(-4.20031442400005,15.2,9.56763891999999));
#235683=CARTESIAN_POINT('Ctrl Pts',(-4.20031442400005,11.6,9.56763891999999));
#235684=CARTESIAN_POINT('Ctrl Pts',(-4.19993084100006,15.2,9.56623843399999));
#235685=CARTESIAN_POINT('Ctrl Pts',(-4.19993084100006,11.6,9.56623843399999));
#235686=CARTESIAN_POINT('Ctrl Pts',(-4.19954810100006,15.2,9.56484624099998));
#235687=CARTESIAN_POINT('Ctrl Pts',(-4.19954810100006,11.6,9.56484624099998));
#235688=CARTESIAN_POINT('Ctrl Pts',(-4.19916622500006,15.2,9.56346235699998));
#235689=CARTESIAN_POINT('Ctrl Pts',(-4.19916622500006,11.6,9.56346235699998));
#235690=CARTESIAN_POINT('Ctrl Pts',(-4.19878523200006,15.2,9.56208679599998));
#235691=CARTESIAN_POINT('Ctrl Pts',(-4.19878523200006,11.6,9.56208679599998));
#235692=CARTESIAN_POINT('Ctrl Pts',(-4.19840514200006,15.2,9.56071957599999));
#235693=CARTESIAN_POINT('Ctrl Pts',(-4.19840514200006,11.6,9.56071957599999));
#235694=CARTESIAN_POINT('Ctrl Pts',(-4.19802597400006,15.2,9.55936071099998));
#235695=CARTESIAN_POINT('Ctrl Pts',(-4.19802597400006,11.6,9.55936071099998));
#235696=CARTESIAN_POINT('Ctrl Pts',(-4.19764774800006,15.2,9.55801021899998));
#235697=CARTESIAN_POINT('Ctrl Pts',(-4.19764774800006,11.6,9.55801021899998));
#235698=CARTESIAN_POINT('Ctrl Pts',(-4.19727048400006,15.2,9.55666811399999));
#235699=CARTESIAN_POINT('Ctrl Pts',(-4.19727048400006,11.6,9.55666811399999));
#235700=CARTESIAN_POINT('Ctrl Pts',(-4.19689420300006,15.2,9.55533441399999));
#235701=CARTESIAN_POINT('Ctrl Pts',(-4.19689420300006,11.6,9.55533441399999));
#235702=CARTESIAN_POINT('Ctrl Pts',(-4.19651892300006,15.2,9.55400913399998));
#235703=CARTESIAN_POINT('Ctrl Pts',(-4.19651892300006,11.6,9.55400913399998));
#235704=CARTESIAN_POINT('Ctrl Pts',(-4.19614466600006,15.2,9.55269229099999));
#235705=CARTESIAN_POINT('Ctrl Pts',(-4.19614466600006,11.6,9.55269229099999));
#235706=CARTESIAN_POINT('Ctrl Pts',(-4.19577145300006,15.2,9.55138390099999));
#235707=CARTESIAN_POINT('Ctrl Pts',(-4.19577145300006,11.6,9.55138390099999));
#235708=CARTESIAN_POINT('Ctrl Pts',(-4.19539930100005,15.2,9.55008397999999));
#235709=CARTESIAN_POINT('Ctrl Pts',(-4.19539930100005,11.6,9.55008397999999));
#235710=CARTESIAN_POINT('Ctrl Pts',(-4.19502823500006,15.2,9.54879254499998));
#235711=CARTESIAN_POINT('Ctrl Pts',(-4.19502823500006,11.6,9.54879254499998));
#235712=CARTESIAN_POINT('Ctrl Pts',(-4.19465827200006,15.2,9.54750961399998));
#235713=CARTESIAN_POINT('Ctrl Pts',(-4.19465827200006,11.6,9.54750961399998));
#235714=CARTESIAN_POINT('Ctrl Pts',(-4.19428943400006,15.2,9.54623519999998));
#235715=CARTESIAN_POINT('Ctrl Pts',(-4.19428943400006,11.6,9.54623519999998));
#235716=CARTESIAN_POINT('Ctrl Pts',(-4.19392174100006,15.2,9.54496932299998));
#235717=CARTESIAN_POINT('Ctrl Pts',(-4.19392174100006,11.6,9.54496932299998));
#235718=CARTESIAN_POINT('Ctrl Pts',(-4.19355521500006,15.2,9.54371199799999));
#235719=CARTESIAN_POINT('Ctrl Pts',(-4.19355521500006,11.6,9.54371199799999));
#235720=CARTESIAN_POINT('Ctrl Pts',(-4.19318987800006,15.2,9.54246324299999));
#235721=CARTESIAN_POINT('Ctrl Pts',(-4.19318987800006,11.6,9.54246324299999));
#235722=CARTESIAN_POINT('Ctrl Pts',(-4.19282574800006,15.2,9.54122307299999));
#235723=CARTESIAN_POINT('Ctrl Pts',(-4.19282574800006,11.6,9.54122307299999));
#235724=CARTESIAN_POINT('Ctrl Pts',(-4.19246284900006,15.2,9.53999150599999));
#235725=CARTESIAN_POINT('Ctrl Pts',(-4.19246284900006,11.6,9.53999150599999));
#235726=CARTESIAN_POINT('Ctrl Pts',(-4.19210120000006,15.2,9.53876855899999));
#235727=CARTESIAN_POINT('Ctrl Pts',(-4.19210120000006,11.6,9.53876855899999));
#235728=CARTESIAN_POINT('Ctrl Pts',(-4.19174082500006,15.2,9.53755424899999));
#235729=CARTESIAN_POINT('Ctrl Pts',(-4.19174082500006,11.6,9.53755424899999));
#235730=CARTESIAN_POINT('Ctrl Pts',(-4.19138174300006,15.2,9.53634859299999));
#235731=CARTESIAN_POINT('Ctrl Pts',(-4.19138174300006,11.6,9.53634859299999));
#235732=CARTESIAN_POINT('Ctrl Pts',(-4.19102397700006,15.2,9.53515160799999));
#235733=CARTESIAN_POINT('Ctrl Pts',(-4.19102397700006,11.6,9.53515160799999));
#235734=CARTESIAN_POINT('Ctrl Pts',(-4.19066754800006,15.2,9.53396331099999));
#235735=CARTESIAN_POINT('Ctrl Pts',(-4.19066754800006,11.6,9.53396331099999));
#235736=CARTESIAN_POINT('Ctrl Pts',(-4.19031247800006,15.2,9.53278371999998));
#235737=CARTESIAN_POINT('Ctrl Pts',(-4.19031247800006,11.6,9.53278371999998));
#235738=CARTESIAN_POINT('Ctrl Pts',(-4.18995878900006,15.2,9.53161285199998));
#235739=CARTESIAN_POINT('Ctrl Pts',(-4.18995878900006,11.6,9.53161285199998));
#235740=CARTESIAN_POINT('Ctrl Pts',(-4.18960650400006,15.2,9.53045072299999));
#235741=CARTESIAN_POINT('Ctrl Pts',(-4.18960650400006,11.6,9.53045072299999));
#235742=CARTESIAN_POINT('Ctrl Pts',(-4.18925564400006,15.2,9.52929735399999));
#235743=CARTESIAN_POINT('Ctrl Pts',(-4.18925564400006,11.6,9.52929735399999));
#235744=CARTESIAN_POINT('Ctrl Pts',(-4.18890623100006,15.2,9.52815275899999));
#235745=CARTESIAN_POINT('Ctrl Pts',(-4.18890623100006,11.6,9.52815275899999));
#235746=CARTESIAN_POINT('Ctrl Pts',(-4.18855828800006,15.2,9.52701695699999));
#235747=CARTESIAN_POINT('Ctrl Pts',(-4.18855828800006,11.6,9.52701695699999));
#235748=CARTESIAN_POINT('Ctrl Pts',(-4.18821183700006,15.2,9.52588996599999));
#235749=CARTESIAN_POINT('Ctrl Pts',(-4.18821183700006,11.6,9.52588996599999));
#235750=CARTESIAN_POINT('Ctrl Pts',(-4.18786690100006,15.2,9.52477180399999));
#235751=CARTESIAN_POINT('Ctrl Pts',(-4.18786690100006,11.6,9.52477180399999));
#235752=CARTESIAN_POINT('Ctrl Pts',(-4.18752350300006,15.2,9.52366248799999));
#235753=CARTESIAN_POINT('Ctrl Pts',(-4.18752350300006,11.6,9.52366248799999));
#235754=CARTESIAN_POINT('Ctrl Pts',(-4.18718166500006,15.2,9.52256203599998));
#235755=CARTESIAN_POINT('Ctrl Pts',(-4.18718166500006,11.6,9.52256203599998));
#235756=CARTESIAN_POINT('Ctrl Pts',(-4.18684141000006,15.2,9.52147046599999));
#235757=CARTESIAN_POINT('Ctrl Pts',(-4.18684141000006,11.6,9.52147046599999));
#235758=CARTESIAN_POINT('Ctrl Pts',(-4.18650276200006,15.2,9.52038779699999));
#235759=CARTESIAN_POINT('Ctrl Pts',(-4.18650276200006,11.6,9.52038779699999));
#235760=CARTESIAN_POINT('Ctrl Pts',(-4.18616574200006,15.2,9.51931404499998));
#235761=CARTESIAN_POINT('Ctrl Pts',(-4.18616574200006,11.6,9.51931404499998));
#235762=CARTESIAN_POINT('Ctrl Pts',(-4.18583037600006,15.2,9.51824923099998));
#235763=CARTESIAN_POINT('Ctrl Pts',(-4.18583037600006,11.6,9.51824923099998));
#235764=CARTESIAN_POINT('Ctrl Pts',(-4.18549668600006,15.2,9.51719337099998));
#235765=CARTESIAN_POINT('Ctrl Pts',(-4.18549668600006,11.6,9.51719337099998));
#235766=CARTESIAN_POINT('Ctrl Pts',(-4.18516469500006,15.2,9.51614648399998));
#235767=CARTESIAN_POINT('Ctrl Pts',(-4.18516469500006,11.6,9.51614648399998));
#235768=CARTESIAN_POINT('Ctrl Pts',(-4.18483442700006,15.2,9.51510858999999));
#235769=CARTESIAN_POINT('Ctrl Pts',(-4.18483442700006,11.6,9.51510858999999));
#235770=CARTESIAN_POINT('Ctrl Pts',(-4.18450590700005,15.2,9.51407970499999));
#235771=CARTESIAN_POINT('Ctrl Pts',(-4.18450590700005,11.6,9.51407970499999));
#235772=CARTESIAN_POINT('Ctrl Pts',(-4.18417915700006,15.2,9.51305984799999));
#235773=CARTESIAN_POINT('Ctrl Pts',(-4.18417915700006,11.6,9.51305984799999));
#235774=CARTESIAN_POINT('Ctrl Pts',(-4.18385420200006,15.2,9.51204903999999));
#235775=CARTESIAN_POINT('Ctrl Pts',(-4.18385420200006,11.6,9.51204903999999));
#235776=CARTESIAN_POINT('Ctrl Pts',(-4.18353106500006,15.2,9.51104729699999));
#235777=CARTESIAN_POINT('Ctrl Pts',(-4.18353106500006,11.6,9.51104729699999));
#235778=CARTESIAN_POINT('Ctrl Pts',(-4.18320977200006,15.2,9.51005463899998));
#235779=CARTESIAN_POINT('Ctrl Pts',(-4.18320977200006,11.6,9.51005463899998));
#235780=CARTESIAN_POINT('Ctrl Pts',(-4.18289034700006,15.2,9.50907108499998));
#235781=CARTESIAN_POINT('Ctrl Pts',(-4.18289034700006,11.6,9.50907108499998));
#235782=CARTESIAN_POINT('Ctrl Pts',(-4.18257281300006,15.2,9.50809665399999));
#235783=CARTESIAN_POINT('Ctrl Pts',(-4.18257281300006,11.6,9.50809665399999));
#235784=CARTESIAN_POINT('Ctrl Pts',(-4.18225719600006,15.2,9.50713136399998));
#235785=CARTESIAN_POINT('Ctrl Pts',(-4.18225719600006,11.6,9.50713136399998));
#235786=CARTESIAN_POINT('Ctrl Pts',(-4.18194352100006,15.2,9.50617523599998));
#235787=CARTESIAN_POINT('Ctrl Pts',(-4.18194352100006,11.6,9.50617523599998));
#235788=CARTESIAN_POINT('Ctrl Pts',(-4.18163181000006,15.2,9.50522828699999));
#235789=CARTESIAN_POINT('Ctrl Pts',(-4.18163181000006,11.6,9.50522828699999));
#235790=CARTESIAN_POINT('Ctrl Pts',(-4.18132209200006,15.2,9.50429053799999));
#235791=CARTESIAN_POINT('Ctrl Pts',(-4.18132209200006,11.6,9.50429053799999));
#235792=CARTESIAN_POINT('Ctrl Pts',(-4.18101438900006,15.2,9.50336200799999));
#235793=CARTESIAN_POINT('Ctrl Pts',(-4.18101438900006,11.6,9.50336200799999));
#235794=CARTESIAN_POINT('Ctrl Pts',(-4.18070872900006,15.2,9.50244271599999));
#235795=CARTESIAN_POINT('Ctrl Pts',(-4.18070872900006,11.6,9.50244271599999));
#235796=CARTESIAN_POINT('Ctrl Pts',(-4.18040513600006,15.2,9.50153268199998));
#235797=CARTESIAN_POINT('Ctrl Pts',(-4.18040513600006,11.6,9.50153268199998));
#235798=CARTESIAN_POINT('Ctrl Pts',(-4.18010363500006,15.2,9.50063192499999));
#235799=CARTESIAN_POINT('Ctrl Pts',(-4.18010363500006,11.6,9.50063192499999));
#235800=CARTESIAN_POINT('Ctrl Pts',(-4.17980425200006,15.2,9.49974046699998));
#235801=CARTESIAN_POINT('Ctrl Pts',(-4.17980425200006,11.6,9.49974046699998));
#235802=CARTESIAN_POINT('Ctrl Pts',(-4.17950701400006,15.2,9.49885832499999));
#235803=CARTESIAN_POINT('Ctrl Pts',(-4.17950701400006,11.6,9.49885832499999));
#235804=CARTESIAN_POINT('Ctrl Pts',(-4.17921364400006,15.2,9.49799054599998));
#235805=CARTESIAN_POINT('Ctrl Pts',(-4.17921364400006,11.6,9.49799054599998));
#235806=CARTESIAN_POINT('Ctrl Pts',(-4.17898102000006,15.2,9.49730470699999));
#235807=CARTESIAN_POINT('Ctrl Pts',(-4.17898102000006,11.6,9.49730470699999));
#235808=CARTESIAN_POINT('Ctrl Pts',(-4.17880795500006,15.2,9.49679570899999));
#235809=CARTESIAN_POINT('Ctrl Pts',(-4.17880795500006,11.6,9.49679570899999));
#235810=CARTESIAN_POINT('Ctrl Pts',(-4.17869357200006,15.2,9.49645984699998));
#235811=CARTESIAN_POINT('Ctrl Pts',(-4.17869357200006,11.6,9.49645984699998));
#235812=CARTESIAN_POINT('Ctrl Pts',(-4.17863732200006,15.2,9.49629481199998));
#235813=CARTESIAN_POINT('Ctrl Pts',(-4.17863732200006,11.6,9.49629481199998));
#235814=CARTESIAN_POINT('',(-4.17863732200006,12.2,9.49629481099999));
#235815=CARTESIAN_POINT('',(-4.17863732200006,15.2,9.49629481099999));
#235816=CARTESIAN_POINT('',(-4.17863732200006,12.2,9.49629481099999));
#235817=CARTESIAN_POINT('Ctrl Pts',(-4.27433547000006,12.2,10.676144262));
#235818=CARTESIAN_POINT('Ctrl Pts',(-4.2747065234345,12.2,10.671060553948));
#235819=CARTESIAN_POINT('Ctrl Pts',(-4.2750690771701,12.2,10.6659880182638));
#235820=CARTESIAN_POINT('Ctrl Pts',(-4.27542311679964,12.2,10.6609266596558));
#235821=CARTESIAN_POINT('Ctrl Pts',(-4.27568864649767,12.2,10.6571306410445));
#235822=CARTESIAN_POINT('Ctrl Pts',(-4.2759493913633,12.2,10.6533409101855));
#235823=CARTESIAN_POINT('Ctrl Pts',(-4.2762053652829,12.2,10.649557489718));
#235824=CARTESIAN_POINT('Ctrl Pts',(-4.27646133920251,12.2,10.6457740692505));
#235825=CARTESIAN_POINT('Ctrl Pts',(-4.27671254300291,12.2,10.6419969605181));
#235826=CARTESIAN_POINT('Ctrl Pts',(-4.27695900353521,12.2,10.638226201864));
#235827=CARTESIAN_POINT('Ctrl Pts',(-4.27736977110396,12.2,10.6319416038789));
#235828=CARTESIAN_POINT('Ctrl Pts',(-4.2777673688425,12.2,10.6256746519071));
#235829=CARTESIAN_POINT('Ctrl Pts',(-4.27815191030016,12.2,10.6194255110747));
#235830=CARTESIAN_POINT('Ctrl Pts',(-4.27838263516637,12.2,10.6156760267115));
#235831=CARTESIAN_POINT('Ctrl Pts',(-4.27860865834068,12.2,10.6119329518277));
#235832=CARTESIAN_POINT('Ctrl Pts',(-4.27883000120862,12.2,10.6081963174882));
#235833=CARTESIAN_POINT('Ctrl Pts',(-4.27905134407656,12.2,10.6044596831487));
#235834=CARTESIAN_POINT('Ctrl Pts',(-4.27926800538995,12.2,10.600729488635));
#235835=CARTESIAN_POINT('Ctrl Pts',(-4.27948001121656,12.2,10.597005769795));
#235836=CARTESIAN_POINT('Ctrl Pts',(-4.27969201704318,12.2,10.593282050955));
#235837=CARTESIAN_POINT('Ctrl Pts',(-4.27989936530154,12.2,10.5895648059536));
#235838=CARTESIAN_POINT('Ctrl Pts',(-4.28010208221125,12.2,10.5858540711712));
#235839=CARTESIAN_POINT('Ctrl Pts',(-4.28030479912095,12.2,10.5821433363888));
#235840=CARTESIAN_POINT('Ctrl Pts',(-4.28050288434764,12.2,10.5784391108726));
#235841=CARTESIAN_POINT('Ctrl Pts',(-4.28069636217457,12.2,10.5747414290894));
#235842=CARTESIAN_POINT('Ctrl Pts',(-4.28088984003665,12.2,10.5710437466344));
#235843=CARTESIAN_POINT('Ctrl Pts',(-4.2810787083641,12.2,10.567352606848));
#235844=CARTESIAN_POINT('Ctrl Pts',(-4.28126299326526,12.2,10.5636680444384));
#235845=CARTESIAN_POINT('Ctrl Pts',(-4.281508706411,12.2,10.5587552956745));
#235846=CARTESIAN_POINT('Ctrl Pts',(-4.28174626834262,12.2,10.5538542388258));
#235847=CARTESIAN_POINT('Ctrl Pts',(-4.2819757394916,12.2,10.5489649535366));
#235848=CARTESIAN_POINT('Ctrl Pts',(-4.28214784286115,12.2,10.5452979894032));
#235849=CARTESIAN_POINT('Ctrl Pts',(-4.28231539458777,12.2,10.5416376492828));
#235850=CARTESIAN_POINT('Ctrl Pts',(-4.28247841904058,12.2,10.537983964665));
#235851=CARTESIAN_POINT('Ctrl Pts',(-4.28264144349338,12.2,10.5343302800471));
#235852=CARTESIAN_POINT('Ctrl Pts',(-4.28279994102149,12.2,10.5306832527622));
#235853=CARTESIAN_POINT('Ctrl Pts',(-4.28295393647485,12.2,10.5270429160185));
#235854=CARTESIAN_POINT('Ctrl Pts',(-4.28310793195617,12.2,10.5234025786136));
#235855=CARTESIAN_POINT('Ctrl Pts',(-4.28325742481123,12.2,10.5197689313521));
#235856=CARTESIAN_POINT('Ctrl Pts',(-4.28340244079003,12.2,10.5161420099926));
#235857=CARTESIAN_POINT('Ctrl Pts',(-4.28354745674248,12.2,10.512515089292));
#235858=CARTESIAN_POINT('Ctrl Pts',(-4.28368799532503,12.2,10.5088948948327));
#235859=CARTESIAN_POINT('Ctrl Pts',(-4.28382408224304,12.2,10.5052814590342));
#235860=CARTESIAN_POINT('Ctrl Pts',(-4.28396016916104,12.2,10.5016680232358));
#235861=CARTESIAN_POINT('Ctrl Pts',(-4.28409180340222,12.2,10.4980613483429));
#235862=CARTESIAN_POINT('Ctrl Pts',(-4.28421901227221,12.2,10.4944614680993));
#235863=CARTESIAN_POINT('Ctrl Pts',(-4.2843462211422,12.2,10.4908615878557));
#235864=CARTESIAN_POINT('Ctrl Pts',(-4.28446900302106,12.2,10.4872685014029));
#235865=CARTESIAN_POINT('Ctrl Pts',(-4.28458738451676,12.2,10.4836822446999));
#235866=CARTESIAN_POINT('Ctrl Pts',(-4.28470576601246,12.2,10.4800959879969));
#235867=CARTESIAN_POINT('Ctrl Pts',(-4.28481974750833,12.2,10.4765165618769));
#235868=CARTESIAN_POINT('Ctrl Pts',(-4.28492935396307,12.2,10.4729439991728));
#235869=CARTESIAN_POINT('Ctrl Pts',(-4.2850389604178,12.2,10.4693714364686));
#235870=CARTESIAN_POINT('Ctrl Pts',(-4.2851441913145,12.2,10.4658057377307));
#235871=CARTESIAN_POINT('Ctrl Pts',(-4.28524507422809,12.2,10.4622469389841));
#235872=CARTESIAN_POINT('Ctrl Pts',(-4.28534595716001,12.2,10.458688139591));
#235873=CARTESIAN_POINT('Ctrl Pts',(-4.28544249107404,12.2,10.4551362394581));
#235874=CARTESIAN_POINT('Ctrl Pts',(-4.28553470354518,12.2,10.4515912749855));
#235875=CARTESIAN_POINT('Ctrl Pts',(-4.28562691599958,12.2,10.4480463111568));
#235876=CARTESIAN_POINT('Ctrl Pts',(-4.28571480596557,12.2,10.4445082806642));
#235877=CARTESIAN_POINT('Ctrl Pts',(-4.28579840046622,12.2,10.4409772202835));
#235878=CARTESIAN_POINT('Ctrl Pts',(-4.28588199496686,12.2,10.4374461599028));
#235879=CARTESIAN_POINT('Ctrl Pts',(-4.28596129374462,12.2,10.4339220701717));
#235880=CARTESIAN_POINT('Ctrl Pts',(-4.28603632374153,12.2,10.4304049863417));
#235881=CARTESIAN_POINT('Ctrl Pts',(-4.28611135373843,12.2,10.4268879025117));
#235882=CARTESIAN_POINT('Ctrl Pts',(-4.28618211578584,12.2,10.4233778225227));
#235883=CARTESIAN_POINT('Ctrl Pts',(-4.28624863578342,12.2,10.4198747847333));
#235884=CARTESIAN_POINT('Ctrl Pts',(-4.28631515578101,12.2,10.4163717469438));
#235885=CARTESIAN_POINT('Ctrl Pts',(-4.28637743427876,12.2,10.4128757504375));
#235886=CARTESIAN_POINT('Ctrl Pts',(-4.28643549827702,12.2,10.409386830647));
#235887=CARTESIAN_POINT('Ctrl Pts',(-4.28649356227528,12.2,10.4058979108565));
#235888=CARTESIAN_POINT('Ctrl Pts',(-4.28654741120594,12.2,10.4024160668704));
#235889=CARTESIAN_POINT('Ctrl Pts',(-4.28659707424877,12.2,10.3989413359473));
#235890=CARTESIAN_POINT('Ctrl Pts',(-4.28664673729159,12.2,10.3954666050241));
#235891=CARTESIAN_POINT('Ctrl Pts',(-4.28669221410867,12.2,10.3919989867295));
#235892=CARTESIAN_POINT('Ctrl Pts',(-4.28673353119108,12.2,10.388538517021));
#235893=CARTESIAN_POINT('Ctrl Pts',(-4.28677484828098,12.2,10.3850780466838));
#235894=CARTESIAN_POINT('Ctrl Pts',(-4.28681200728638,12.2,10.3816247245819));
#235895=CARTESIAN_POINT('Ctrl Pts',(-4.28684503529062,12.2,10.3781785877487));
#235896=CARTESIAN_POINT('Ctrl Pts',(-4.2868890726196,12.2,10.3735837396812));
#235897=CARTESIAN_POINT('Ctrl Pts',(-4.2869257653162,12.2,10.3690016644425));
#235898=CARTESIAN_POINT('Ctrl Pts',(-4.28695518198094,12.2,10.3644324476486));
#235899=CARTESIAN_POINT('Ctrl Pts',(-4.2869772444805,12.2,10.3610055348975));
#235900=CARTESIAN_POINT('Ctrl Pts',(-4.28699521373003,12.2,10.3575858545576));
#235901=CARTESIAN_POINT('Ctrl Pts',(-4.28700911873069,12.2,10.3541734441769));
#235902=CARTESIAN_POINT('Ctrl Pts',(-4.28702302373135,12.2,10.3507610337962));
#235903=CARTESIAN_POINT('Ctrl Pts',(-4.28703286426514,12.2,10.3473558933516));
#235904=CARTESIAN_POINT('Ctrl Pts',(-4.28703866926548,12.2,10.3439580582657));
#235905=CARTESIAN_POINT('Ctrl Pts',(-4.28704447426688,12.2,10.3405602225625));
#235906=CARTESIAN_POINT('Ctrl Pts',(-4.2870462437338,12.2,10.3371696939698));
#235907=CARTESIAN_POINT('Ctrl Pts',(-4.28704400681626,12.2,10.3337865072291));
#235908=CARTESIAN_POINT('Ctrl Pts',(-4.28704176989913,12.2,10.330403321103));
#235909=CARTESIAN_POINT('Ctrl Pts',(-4.28703552706555,12.2,10.3270274781099));
#235910=CARTESIAN_POINT('Ctrl Pts',(-4.28702530623224,12.2,10.3236590143996));
#235911=CARTESIAN_POINT('Ctrl Pts',(-4.28701508539893,12.2,10.3202905506893));
#235912=CARTESIAN_POINT('Ctrl Pts',(-4.28700088849951,12.2,10.31692946624));
#235913=CARTESIAN_POINT('Ctrl Pts',(-4.28698274400007,12.2,10.3135757990134));
#235914=CARTESIAN_POINT('Ctrl Pts',(-4.28696459950062,12.2,10.3102221317867));
#235915=CARTESIAN_POINT('Ctrl Pts',(-4.28694250683259,12.2,10.3068758804302));
#235916=CARTESIAN_POINT('Ctrl Pts',(-4.28691649779177,12.2,10.303537083703));
#235917=CARTESIAN_POINT('Ctrl Pts',(-4.28688181906753,12.2,10.299085354329));
#235918=CARTESIAN_POINT('Ctrl Pts',(-4.28684017474549,12.2,10.294646875694));
#235919=CARTESIAN_POINT('Ctrl Pts',(-4.28679163874214,12.2,10.2902217370098));
#235920=CARTESIAN_POINT('Ctrl Pts',(-4.28674310274541,12.2,10.2857965989284));
#235921=CARTESIAN_POINT('Ctrl Pts',(-4.28668767350513,12.2,10.281384800212));
#235922=CARTESIAN_POINT('Ctrl Pts',(-4.28662542428844,12.2,10.2769864301263));
#235923=CARTESIAN_POINT('Ctrl Pts',(-4.28656317506327,12.2,10.2725880594413));
#235924=CARTESIAN_POINT('Ctrl Pts',(-4.28649410615311,12.2,10.2682031168017));
#235925=CARTESIAN_POINT('Ctrl Pts',(-4.28641829025571,12.2,10.263831692624));
#235926=CARTESIAN_POINT('Ctrl Pts',(-4.28634247436864,12.2,10.2594602690419));
#235927=CARTESIAN_POINT('Ctrl Pts',(-4.28625991067458,12.2,10.2551023641315));
#235928=CARTESIAN_POINT('Ctrl Pts',(-4.28617067551565,12.2,10.2507580660969));
#235929=CARTESIAN_POINT('Ctrl Pts',(-4.28608144034455,12.2,10.2464137674704));
#235930=CARTESIAN_POINT('Ctrl Pts',(-4.2859855331171,12.2,10.2420830764593));
#235931=CARTESIAN_POINT('Ctrl Pts',(-4.28588302849997,12.2,10.2377660851138));
#235932=CARTESIAN_POINT('Ctrl Pts',(-4.28578052389681,12.2,10.2334490943565));
#235933=CARTESIAN_POINT('Ctrl Pts',(-4.28567142076814,12.2,10.2291458008511));
#235934=CARTESIAN_POINT('Ctrl Pts',(-4.28555579755016,12.2,10.2248562965974));
#235935=CARTESIAN_POINT('Ctrl Pts',(-4.28544017431643,12.2,10.2205667917593));
#235936=CARTESIAN_POINT('Ctrl Pts',(-4.28531802998582,12.2,10.2162910774664));
#235937=CARTESIAN_POINT('Ctrl Pts',(-4.28518944075618,12.2,10.2120292429017));
#235938=CARTESIAN_POINT('Ctrl Pts',(-4.28502870422787,12.2,10.2067019499861));
#235939=CARTESIAN_POINT('Ctrl Pts',(-4.28485790027205,12.2,10.2013963461367));
#235940=CARTESIAN_POINT('Ctrl Pts',(-4.28467717797987,12.2,10.1961126098878));
#235941=CARTESIAN_POINT('Ctrl Pts',(-4.28453260015794,12.2,10.1918856212343));
#235942=CARTESIAN_POINT('Ctrl Pts',(-4.28438167610898,12.2,10.187672629227));
#235943=CARTESIAN_POINT('Ctrl Pts',(-4.28422448428119,12.2,10.1834737243593));
#235944=CARTESIAN_POINT('Ctrl Pts',(-4.28406729243199,12.2,10.1792748189195));
#235945=CARTESIAN_POINT('Ctrl Pts',(-4.28390383270413,12.2,10.1750900033216));
#235946=CARTESIAN_POINT('Ctrl Pts',(-4.28373418619449,12.2,10.1709193681508));
#235947=CARTESIAN_POINT('Ctrl Pts',(-4.28356453970795,12.2,10.1667487335482));
#235948=CARTESIAN_POINT('Ctrl Pts',(-4.28338870502266,12.2,10.1625922801512));
#235949=CARTESIAN_POINT('Ctrl Pts',(-4.28320676453816,12.2,10.1584501027105));
#235950=CARTESIAN_POINT('Ctrl Pts',(-4.28302482402886,12.2,10.1543079247055));
#235951=CARTESIAN_POINT('Ctrl Pts',(-4.2828367775892,12.2,10.1501800218122));
#235952=CARTESIAN_POINT('Ctrl Pts',(-4.28264270579995,12.2,10.1460664880138));
#235953=CARTESIAN_POINT('Ctrl Pts',(-4.2823515981425,12.2,10.1398961878767));
#235954=CARTESIAN_POINT('Ctrl Pts',(-4.28204693588855,12.2,10.1337582201124));
#235955=CARTESIAN_POINT('Ctrl Pts',(-4.28172900023402,12.2,10.1276529038328));
#235956=CARTESIAN_POINT('Ctrl Pts',(-4.28151704311174,12.2,10.12358269261));
#235957=CARTESIAN_POINT('Ctrl Pts',(-4.28129918708875,12.2,10.1195269932723));
#235958=CARTESIAN_POINT('Ctrl Pts',(-4.28107551596507,12.2,10.1154859013864));
#235959=CARTESIAN_POINT('Ctrl Pts',(-4.28085184487187,12.2,10.111444810051));
#235960=CARTESIAN_POINT('Ctrl Pts',(-4.28062235906594,12.2,10.1074183267127));
#235961=CARTESIAN_POINT('Ctrl Pts',(-4.2803871440302,12.2,10.1034065473725));
#235962=CARTESIAN_POINT('Ctrl Pts',(-4.28015192896241,12.2,10.0993947674857));
#235963=CARTESIAN_POINT('Ctrl Pts',(-4.27991098485616,12.2,10.0953976926212));
#235964=CARTESIAN_POINT('Ctrl Pts',(-4.27966439900824,12.2,10.0914154174972));
#235965=CARTESIAN_POINT('Ctrl Pts',(-4.27941781319392,12.2,10.0874331429158));
#235966=CARTESIAN_POINT('Ctrl Pts',(-4.27916558455114,12.2,10.083465668519));
#235967=CARTESIAN_POINT('Ctrl Pts',(-4.27890780151722,12.2,10.0795130943962));
#235968=CARTESIAN_POINT('Ctrl Pts',(-4.27865001844819,12.2,10.0755605197348));
#235969=CARTESIAN_POINT('Ctrl Pts',(-4.27838668119251,12.2,10.0716228424832));
#235970=CARTESIAN_POINT('Ctrl Pts',(-4.27811787873341,12.2,10.0677001619916));
#235971=CARTESIAN_POINT('Ctrl Pts',(-4.27784907627432,12.2,10.0637774815));
#235972=CARTESIAN_POINT('Ctrl Pts',(-4.27757480808126,12.2,10.059869798263));
#235973=CARTESIAN_POINT('Ctrl Pts',(-4.27729516495435,12.2,10.0559772098302));
#235974=CARTESIAN_POINT('Ctrl Pts',(-4.27701552186555,12.2,10.0520846219277));
#235975=CARTESIAN_POINT('Ctrl Pts',(-4.27673050254173,12.2,10.0482071298711));
#235976=CARTESIAN_POINT('Ctrl Pts',(-4.27644019950861,12.2,10.0443448325026));
#235977=CARTESIAN_POINT('Ctrl Pts',(-4.27614989643593,12.2,10.0404825346078));
#235978=CARTESIAN_POINT('Ctrl Pts',(-4.27585430870949,12.2,10.0366354319501));
#235979=CARTESIAN_POINT('Ctrl Pts',(-4.27555353019256,12.2,10.0328036241318));
#235980=CARTESIAN_POINT('Ctrl Pts',(-4.27525275171662,12.2,10.0289718168355));
#235981=CARTESIAN_POINT('Ctrl Pts',(-4.27494678016914,12.2,10.0251553036538));
#235982=CARTESIAN_POINT('Ctrl Pts',(-4.27463571125046,12.2,10.0213541870191));
#235983=CARTESIAN_POINT('Ctrl Pts',(-4.27432464228939,12.2,10.0175530698665));
#235984=CARTESIAN_POINT('Ctrl Pts',(-4.27400847515131,12.2,10.0137673486649));
#235985=CARTESIAN_POINT('Ctrl Pts',(-4.27368730472844,12.2,10.0099971239946));
#235986=CARTESIAN_POINT('Ctrl Pts',(-4.27336613434934,12.2,10.006226899838));
#235987=CARTESIAN_POINT('Ctrl Pts',(-4.27303996060248,12.2,10.0024721738233));
#235988=CARTESIAN_POINT('Ctrl Pts',(-4.27270887901876,12.2,9.99873304657241));
#235989=CARTESIAN_POINT('Ctrl Pts',(-4.27237779738992,12.2,9.99499391881202));
#235990=CARTESIAN_POINT('Ctrl Pts',(-4.27204180844105,12.2,9.99127039013132));
#235991=CARTESIAN_POINT('Ctrl Pts',(-4.27170100942217,12.2,9.98756256426363));
#235992=CARTESIAN_POINT('Ctrl Pts',(-4.27136021044972,12.2,9.98385473890112));
#235993=CARTESIAN_POINT('Ctrl Pts',(-4.27101460124211,12.2,9.98016261534298));
#235994=CARTESIAN_POINT('Ctrl Pts',(-4.27066428030921,12.2,9.97648629729179));
#235995=CARTESIAN_POINT('Ctrl Pts',(-4.27031395932858,12.2,9.9728099787397));
#235996=CARTESIAN_POINT('Ctrl Pts',(-4.26995892684053,12.2,9.96914946685526));
#235997=CARTESIAN_POINT('Ctrl Pts',(-4.2695992824873,12.2,9.96550486443546));
#235998=CARTESIAN_POINT('Ctrl Pts',(-4.26923963818306,12.2,9.96186026251223));
#235999=CARTESIAN_POINT('Ctrl Pts',(-4.26887538143253,12.2,9.95823157145245));
#236000=CARTESIAN_POINT('Ctrl Pts',(-4.2685066145187,12.2,9.95461889485727));
#236001=CARTESIAN_POINT('Ctrl Pts',(-4.26813784755462,12.2,9.95100621776984));
#236002=CARTESIAN_POINT('Ctrl Pts',(-4.26776456999435,12.2,9.94740955630047));
#236003=CARTESIAN_POINT('Ctrl Pts',(-4.26738688374982,12.2,9.94382901525582));
#236004=CARTESIAN_POINT('Ctrl Pts',(-4.26700919755674,12.2,9.94024847469902));
#236005=CARTESIAN_POINT('Ctrl Pts',(-4.26662710346733,12.2,9.93668405593333));
#236006=CARTESIAN_POINT('Ctrl Pts',(-4.26624070455491,12.2,9.93313586405506));
#236007=CARTESIAN_POINT('Ctrl Pts',(-4.26585430558985,12.2,9.92958767169334));
#236008=CARTESIAN_POINT('Ctrl Pts',(-4.26546360139382,12.2,9.92605570684429));
#236009=CARTESIAN_POINT('Ctrl Pts',(-4.26506869848341,12.2,9.92254007770825));
#236010=CARTESIAN_POINT('Ctrl Pts',(-4.26467379557299,12.2,9.91902444857221));
#236011=CARTESIAN_POINT('Ctrl Pts',(-4.26427469426488,12.2,9.91552515396028));
#236012=CARTESIAN_POINT('Ctrl Pts',(-4.26387149940915,12.2,9.91204230293883));
#236013=CARTESIAN_POINT('Ctrl Pts',(-4.26346830460836,12.2,9.9085594523919));
#236014=CARTESIAN_POINT('Ctrl Pts',(-4.26306101635192,12.2,9.90509304465542));
#236015=CARTESIAN_POINT('Ctrl Pts',(-4.26264974471702,12.2,9.90164318997728));
#236016=CARTESIAN_POINT('Ctrl Pts',(-4.26223847302608,12.2,9.8981933348291));
#236017=CARTESIAN_POINT('Ctrl Pts',(-4.26182321624367,12.2,9.89476003202304));
#236018=CARTESIAN_POINT('Ctrl Pts',(-4.26140408466487,12.2,9.89134339044965));
#236019=CARTESIAN_POINT('Ctrl Pts',(-4.26098495314319,12.2,9.88792674934179));
#236020=CARTESIAN_POINT('Ctrl Pts',(-4.26056194661368,12.2,9.88452677233173));
#236021=CARTESIAN_POINT('Ctrl Pts',(-4.26013517525992,12.2,9.88114356655165));
#236022=CARTESIAN_POINT('Ctrl Pts',(-4.25970840384802,12.2,9.87776036031061));
#236023=CARTESIAN_POINT('Ctrl Pts',(-4.25927786927716,12.2,9.87439392724852));
#236024=CARTESIAN_POINT('Ctrl Pts',(-4.25884368245371,12.2,9.87104437928898));
#236025=CARTESIAN_POINT('Ctrl Pts',(-4.25840949568942,12.2,9.86769483178581));
#236026=CARTESIAN_POINT('Ctrl Pts',(-4.25797165759425,12.2,9.86436216844285));
#236027=CARTESIAN_POINT('Ctrl Pts',(-4.25753028151945,12.2,9.86104650254614));
#236028=CARTESIAN_POINT('Ctrl Pts',(-4.25697856138085,12.2,9.85690191983642));
#236029=CARTESIAN_POINT('Ctrl Pts',(-4.25642131451988,12.2,9.85278389537457));
#236030=CARTESIAN_POINT('Ctrl Pts',(-4.25585876681183,12.2,9.84869265023431));
#236031=CARTESIAN_POINT('Ctrl Pts',(-4.25529621910378,12.2,9.84460140509407));
#236032=CARTESIAN_POINT('Ctrl Pts',(-4.2547283681252,12.2,9.84053693985943));
#236033=CARTESIAN_POINT('Ctrl Pts',(-4.25415544798371,12.2,9.83649947803545));
#236034=CARTESIAN_POINT('Ctrl Pts',(-4.25358252784223,12.2,9.83246201621147));
#236035=CARTESIAN_POINT('Ctrl Pts',(-4.25300453683896,12.2,9.8284515587888));
#236036=CARTESIAN_POINT('Ctrl Pts',(-4.25242170920007,12.2,9.82446833198325));
#236037=CARTESIAN_POINT('Ctrl Pts',(-4.25183888156118,12.2,9.8204851051777));
#236038=CARTESIAN_POINT('Ctrl Pts',(-4.25125121781118,12.2,9.81652910891104));
#236039=CARTESIAN_POINT('Ctrl Pts',(-4.25065895524174,12.2,9.81260057050826));
#236040=CARTESIAN_POINT('Ctrl Pts',(-4.2500666926723,12.2,9.80867203210549));
#236041=CARTESIAN_POINT('Ctrl Pts',(-4.24946983258581,12.2,9.80477095492088));
#236042=CARTESIAN_POINT('Ctrl Pts',(-4.24886861674974,12.2,9.80089756726447));
#236043=CARTESIAN_POINT('Ctrl Pts',(-4.24814715777266,12.2,9.79624950224567));
#236044=CARTESIAN_POINT('Ctrl Pts',(-4.24741942834645,12.2,9.79164131051814));
#236045=CARTESIAN_POINT('Ctrl Pts',(-4.24668585254002,12.2,9.78707339951571));
#236046=CARTESIAN_POINT('Ctrl Pts',(-4.2460745393458,12.2,9.78326680687536));
#236047=CARTESIAN_POINT('Ctrl Pts',(-4.24545916916256,12.2,9.77948818608018));
#236048=CARTESIAN_POINT('Ctrl Pts',(-4.24483999256554,12.2,9.77573777274536));
#236049=CARTESIAN_POINT('Ctrl Pts',(-4.24397314531621,12.2,9.77048719399486));
#236050=CARTESIAN_POINT('Ctrl Pts',(-4.24309883772286,12.2,9.76529190508791));
#236051=CARTESIAN_POINT('Ctrl Pts',(-4.24221777920889,12.2,9.76015256451001));
#236052=CARTESIAN_POINT('Ctrl Pts',(-4.24158845170871,12.2,9.75648160701153));
#236053=CARTESIAN_POINT('Ctrl Pts',(-4.24095568009751,12.2,9.75283919465116));
#236054=CARTESIAN_POINT('Ctrl Pts',(-4.24031972620845,12.2,9.74922557201375));
#236055=CARTESIAN_POINT('Ctrl Pts',(-4.2396837723194,12.2,9.74561194937635));
#236056=CARTESIAN_POINT('Ctrl Pts',(-4.23904464084114,12.2,9.74202711456287));
#236057=CARTESIAN_POINT('Ctrl Pts',(-4.23840259518385,12.2,9.7384713160539));
#236058=CARTESIAN_POINT('Ctrl Pts',(-4.23776054952657,12.2,9.73491551754493));
#236059=CARTESIAN_POINT('Ctrl Pts',(-4.23711559314335,12.2,9.73138875573448));
#236060=CARTESIAN_POINT('Ctrl Pts',(-4.23646799765702,12.2,9.72789127900078));
#236061=CARTESIAN_POINT('Ctrl Pts',(-4.2358204021707,12.2,9.72439380226707));
#236062=CARTESIAN_POINT('Ctrl Pts',(-4.23517016980378,12.2,9.72092561085328));
#236063=CARTESIAN_POINT('Ctrl Pts',(-4.2345175784147,12.2,9.71748695759181));
#236064=CARTESIAN_POINT('Ctrl Pts',(-4.23386498709676,12.2,9.71404830470516));
#236065=CARTESIAN_POINT('Ctrl Pts',(-4.23321003576421,12.2,9.71063918967047));
#236066=CARTESIAN_POINT('Ctrl Pts',(-4.23255301104433,12.2,9.70725986996694));
#236067=CARTESIAN_POINT('Ctrl Pts',(-4.23189598625284,12.2,9.70388054989506));
#236068=CARTESIAN_POINT('Ctrl Pts',(-4.2312368871308,12.2,9.70053102310878));
#236069=CARTESIAN_POINT('Ctrl Pts',(-4.2305760033115,12.2,9.69721155067576));
#236070=CARTESIAN_POINT('Ctrl Pts',(-4.2299151194922,12.2,9.69389207824274));
#236071=CARTESIAN_POINT('Ctrl Pts',(-4.22925245200468,12.2,9.69060265873773));
#236072=CARTESIAN_POINT('Ctrl Pts',(-4.22858829481882,12.2,9.68734355537835));
#236073=CARTESIAN_POINT('Ctrl Pts',(-4.22779130615235,12.2,9.68343263113394));
#236074=CARTESIAN_POINT('Ctrl Pts',(-4.22699217381486,12.2,9.6795653639219));
#236075=CARTESIAN_POINT('Ctrl Pts',(-4.22619141918777,12.2,9.67574221004985));
#236076=CARTESIAN_POINT('Ctrl Pts',(-4.22539066463342,12.2,9.67191905652509));
#236077=CARTESIAN_POINT('Ctrl Pts',(-4.22458828779082,12.2,9.66814002206272));
#236078=CARTESIAN_POINT('Ctrl Pts',(-4.22378482331636,12.2,9.66440556851488));
#236079=CARTESIAN_POINT('Ctrl Pts',(-4.2229813588419,12.2,9.66067111496704));
#236080=CARTESIAN_POINT('Ctrl Pts',(-4.22217680665631,12.2,9.65698124692656));
#236081=CARTESIAN_POINT('Ctrl Pts',(-4.22137171510227,12.2,9.65333643647374));
#236082=CARTESIAN_POINT('Ctrl Pts',(-4.22056662347509,12.2,9.64969162568985));
#236083=CARTESIAN_POINT('Ctrl Pts',(-4.21976099198116,12.2,9.64609187621979));
#236084=CARTESIAN_POINT('Ctrl Pts',(-4.21895537968725,12.2,9.64253766936251));
#236085=CARTESIAN_POINT('Ctrl Pts',(-4.21814976746651,12.2,9.63898346282806));
#236086=CARTESIAN_POINT('Ctrl Pts',(-4.21734417902692,12.2,9.63547480160025));
#236087=CARTESIAN_POINT('Ctrl Pts',(-4.21653918472285,12.2,9.6320121750614));
#236088=CARTESIAN_POINT('Ctrl Pts',(-4.21573419041879,12.2,9.62854954852252));
#236089=CARTESIAN_POINT('Ctrl Pts',(-4.2149297924647,12.2,9.62513295846334));
#236090=CARTESIAN_POINT('Ctrl Pts',(-4.21412658032717,12.2,9.62176290675044));
#236091=CARTESIAN_POINT('Ctrl Pts',(-4.21332336818964,12.2,9.61839285503754));
#236092=CARTESIAN_POINT('Ctrl Pts',(-4.21252134197498,12.2,9.61506933917448));
#236093=CARTESIAN_POINT('Ctrl Pts',(-4.21172110583728,12.2,9.61179287262372));
#236094=CARTESIAN_POINT('Ctrl Pts',(-4.21092086962689,12.2,9.60851640577534));
#236095=CARTESIAN_POINT('Ctrl Pts',(-4.21012242359162,12.2,9.60528698742304));
#236096=CARTESIAN_POINT('Ctrl Pts',(-4.20932638846501,12.2,9.60210513583504));
#236097=CARTESIAN_POINT('Ctrl Pts',(-4.20853035341071,12.2,9.59892328453606));
#236098=CARTESIAN_POINT('Ctrl Pts',(-4.20773672958122,12.2,9.59578900219158));
#236099=CARTESIAN_POINT('Ctrl Pts',(-4.20694615260982,12.2,9.59270281863497));
#236100=CARTESIAN_POINT('Ctrl Pts',(-4.20615557563842,12.2,9.58961663507837));
#236101=CARTESIAN_POINT('Ctrl Pts',(-4.20536804630726,12.2,9.58657854854546));
#236102=CARTESIAN_POINT('Ctrl Pts',(-4.20458421833549,12.2,9.58358910206744));
#236103=CARTESIAN_POINT('Ctrl Pts',(-4.20380039029253,12.2,9.58059965531788));
#236104=CARTESIAN_POINT('Ctrl Pts',(-4.20302026224988,12.2,9.57765884706463));
#236105=CARTESIAN_POINT('Ctrl Pts',(-4.20224450820779,12.2,9.57476722857584));
#236106=CARTESIAN_POINT('Ctrl Pts',(-4.20133946193105,12.2,9.57139367406625));
#236107=CARTESIAN_POINT('Ctrl Pts',(-4.20044036512269,12.2,9.56808707192141));
#236108=CARTESIAN_POINT('Ctrl Pts',(-4.19954831706672,12.2,9.56484831853584));
#236109=CARTESIAN_POINT('Ctrl Pts',(-4.19878370435803,12.2,9.56207224388113));
#236110=CARTESIAN_POINT('Ctrl Pts',(-4.1980242714748,12.2,9.55934601747287));
#236111=CARTESIAN_POINT('Ctrl Pts',(-4.197270729684,12.2,9.55667021507928));
#236112=CARTESIAN_POINT('Ctrl Pts',(-4.19651718796165,12.2,9.55399441292872));
#236113=CARTESIAN_POINT('Ctrl Pts',(-4.1957695365185,12.2,9.55136903429433));
#236114=CARTESIAN_POINT('Ctrl Pts',(-4.19502851079205,12.2,9.5487946709594));
#236115=CARTESIAN_POINT('Ctrl Pts',(-4.1942874850656,12.2,9.54622030762448));
#236116=CARTESIAN_POINT('Ctrl Pts',(-4.19355308117839,12.2,9.54369695800809));
#236117=CARTESIAN_POINT('Ctrl Pts',(-4.19282605578763,12.2,9.541225224011));
#236118=CARTESIAN_POINT('Ctrl Pts',(-4.19209903033082,12.2,9.5387534897894));
#236119=CARTESIAN_POINT('Ctrl Pts',(-4.19137938308842,12.2,9.53633337259027));
#236120=CARTESIAN_POINT('Ctrl Pts',(-4.19066788768123,12.2,9.53396548726263));
#236121=CARTESIAN_POINT('Ctrl Pts',(-4.18995639233869,12.2,9.53159760215006));
#236122=CARTESIAN_POINT('Ctrl Pts',(-4.18925305123314,12.2,9.52928194966766));
#236123=CARTESIAN_POINT('Ctrl Pts',(-4.18855866100837,12.2,9.52701915974989));
#236124=CARTESIAN_POINT('Ctrl Pts',(-4.18786427078361,12.2,9.52475636983213));
#236125=CARTESIAN_POINT('Ctrl Pts',(-4.18717883320019,12.2,9.5225464444494));
#236126=CARTESIAN_POINT('Ctrl Pts',(-4.18650316910709,12.2,9.5203900265003));
#236127=CARTESIAN_POINT('Ctrl Pts',(-4.18582750495263,12.2,9.51823360835532));
#236128=CARTESIAN_POINT('Ctrl Pts',(-4.18516161557193,12.2,9.51613070056786));
#236129=CARTESIAN_POINT('Ctrl Pts',(-4.18450634945362,12.2,9.51408196179326));
#236130=CARTESIAN_POINT('Ctrl Pts',(-4.18385108339483,12.2,9.51203322320476));
#236131=CARTESIAN_POINT('Ctrl Pts',(-4.18320643897126,12.2,9.51003865696222));
#236132=CARTESIAN_POINT('Ctrl Pts',(-4.18257329224142,12.2,9.50809893927401));
#236133=CARTESIAN_POINT('Ctrl Pts',(-4.18194014551157,12.2,9.50615922158582));
#236134=CARTESIAN_POINT('Ctrl Pts',(-4.1813184946867,12.2,9.50427435327746));
#236135=CARTESIAN_POINT('Ctrl Pts',(-4.18070924579163,12.2,9.50244503059149));
#236136=CARTESIAN_POINT('Ctrl Pts',(-4.18000137932716,12.2,9.50031960009414));
#236137=CARTESIAN_POINT('Ctrl Pts',(-4.17931024776035,12.2,9.49826914627287));
#236138=CARTESIAN_POINT('Ctrl Pts',(-4.17863732200006,12.2,9.49629481199998));
#236139=CARTESIAN_POINT('Ctrl Pts',(-4.17863732200006,15.2,9.49629481199998));
#236140=CARTESIAN_POINT('Ctrl Pts',(-4.17921371838994,15.2,9.49798593339028));
#236141=CARTESIAN_POINT('Ctrl Pts',(-4.17980347320432,15.2,9.49973290402222));
#236142=CARTESIAN_POINT('Ctrl Pts',(-4.18040565894242,15.2,9.50153500107752));
#236143=CARTESIAN_POINT('Ctrl Pts',(-4.18101074872453,15.2,9.50334578875573));
#236144=CARTESIAN_POINT('Ctrl Pts',(-4.1816283933862,15.2,9.50521223961533));
#236145=CARTESIAN_POINT('Ctrl Pts',(-4.18225768153594,15.2,9.50713365465256));
#236146=CARTESIAN_POINT('Ctrl Pts',(-4.18288696962852,15.2,9.50905506951527));
#236147=CARTESIAN_POINT('Ctrl Pts',(-4.18352790475704,15.2,9.5110314483653));
#236148=CARTESIAN_POINT('Ctrl Pts',(-4.18417960573337,15.2,9.51306211020822));
#236149=CARTESIAN_POINT('Ctrl Pts',(-4.1848313067097,15.2,9.51509277205115));
#236150=CARTESIAN_POINT('Ctrl Pts',(-4.18549377339311,15.2,9.51717771630879));
#236151=CARTESIAN_POINT('Ctrl Pts',(-4.18616615540168,15.2,9.51931627925147));
#236152=CARTESIAN_POINT('Ctrl Pts',(-4.18683853747134,15.2,9.5214548423884));
#236153=CARTESIAN_POINT('Ctrl Pts',(-4.18752083262044,15.2,9.52364702327699));
#236154=CARTESIAN_POINT('Ctrl Pts',(-4.1882122158254,15.2,9.52589217348629));
#236155=CARTESIAN_POINT('Ctrl Pts',(-4.18890359896757,15.2,9.52813732349166));
#236156=CARTESIAN_POINT('Ctrl Pts',(-4.18960406803121,15.2,9.53043544456723));
#236157=CARTESIAN_POINT('Ctrl Pts',(-4.1903128232587,15.2,9.53278590074263));
#236158=CARTESIAN_POINT('Ctrl Pts',(-4.19102157848618,15.2,9.53513635691803));
#236159=CARTESIAN_POINT('Ctrl Pts',(-4.19173861711225,15.2,9.53753914979113));
#236160=CARTESIAN_POINT('Ctrl Pts',(-4.19246316150225,15.2,9.53999366086634));
#236161=CARTESIAN_POINT('Ctrl Pts',(-4.19318770595807,15.2,9.54244817216449));
#236162=CARTESIAN_POINT('Ctrl Pts',(-4.19391975577318,15.2,9.54495440119413));
#236163=CARTESIAN_POINT('Ctrl Pts',(-4.19465855331391,15.2,9.54751174358699));
#236164=CARTESIAN_POINT('Ctrl Pts',(-4.19539735078753,15.2,9.55006908574756));
#236165=CARTESIAN_POINT('Ctrl Pts',(-4.19614289568474,15.2,9.55267754192277));
#236166=CARTESIAN_POINT('Ctrl Pts',(-4.19689445332436,15.2,9.55533651916169));
#236167=CARTESIAN_POINT('Ctrl Pts',(-4.1977712706161,15.2,9.55843865943478));
#236168=CARTESIAN_POINT('Ctrl Pts',(-4.1986562689413,15.2,9.56160956489805));
#236169=CARTESIAN_POINT('Ctrl Pts',(-4.19954831706672,15.2,9.56484831853583));
#236170=CARTESIAN_POINT('Ctrl Pts',(-4.2004403651227,15.2,9.56808707192145));
#236171=CARTESIAN_POINT('Ctrl Pts',(-4.20133946193105,15.2,9.57139367406625));
#236172=CARTESIAN_POINT('Ctrl Pts',(-4.20224450820779,15.2,9.57476722857585));
#236173=CARTESIAN_POINT('Ctrl Pts',(-4.20302026224988,15.2,9.57765884706465));
#236174=CARTESIAN_POINT('Ctrl Pts',(-4.20380039029253,15.2,9.58059965531788));
#236175=CARTESIAN_POINT('Ctrl Pts',(-4.20458421833549,15.2,9.58358910206742));
#236176=CARTESIAN_POINT('Ctrl Pts',(-4.20549868427881,15.2,9.58707678953456));
#236177=CARTESIAN_POINT('Ctrl Pts',(-4.20641818769237,15.2,9.59063067933664));
#236178=CARTESIAN_POINT('Ctrl Pts',(-4.20734169189859,15.2,9.59424991633104));
#236179=CARTESIAN_POINT('Ctrl Pts',(-4.2083971253285,15.2,9.59838618738307));
#236180=CARTESIAN_POINT('Ctrl Pts',(-4.20945778375829,15.2,9.60260780484146));
#236181=CARTESIAN_POINT('Ctrl Pts',(-4.21052217185471,15.2,9.60691352288959));
#236182=CARTESIAN_POINT('Ctrl Pts',(-4.2113204629814,15.2,9.61014281164567));
#236183=CARTESIAN_POINT('Ctrl Pts',(-4.21212085226043,15.2,9.61341940851326));
#236184=CARTESIAN_POINT('Ctrl Pts',(-4.21292272751096,15.2,9.61674279561319));
#236185=CARTESIAN_POINT('Ctrl Pts',(-4.21385824852733,15.2,9.62062008011029));
#236186=CARTESIAN_POINT('Ctrl Pts',(-4.21479579237643,15.2,9.62456105328443));
#236187=CARTESIAN_POINT('Ctrl Pts',(-4.21573441113736,15.2,9.62856491264251));
#236188=CARTESIAN_POINT('Ctrl Pts',(-4.21667302997136,15.2,9.63256877231232));
#236189=CARTESIAN_POINT('Ctrl Pts',(-4.2176127251419,15.2,9.63663551817651));
#236190=CARTESIAN_POINT('Ctrl Pts',(-4.21855257821636,15.2,9.64076436423164));
#236191=CARTESIAN_POINT('Ctrl Pts',(-4.21935816652408,15.2,9.64430337495235));
#236192=CARTESIAN_POINT('Ctrl Pts',(-4.22016386916651,15.2,9.64788801128926));
#236193=CARTESIAN_POINT('Ctrl Pts',(-4.22096912638729,15.2,9.65151778782094));
#236194=CARTESIAN_POINT('Ctrl Pts',(-4.2217743836812,15.2,9.65514756468235));
#236195=CARTESIAN_POINT('Ctrl Pts',(-4.22257919142725,15.2,9.65882248044371));
#236196=CARTESIAN_POINT('Ctrl Pts',(-4.22338300301115,15.2,9.66254205958484));
#236197=CARTESIAN_POINT('Ctrl Pts',(-4.22418681452204,15.2,9.6662616383881));
#236198=CARTESIAN_POINT('Ctrl Pts',(-4.2249896287625,15.2,9.67002587872989));
#236199=CARTESIAN_POINT('Ctrl Pts',(-4.22579090923339,15.2,9.67383431250824));
#236200=CARTESIAN_POINT('Ctrl Pts',(-4.22659218970429,15.2,9.67764274628658));
#236201=CARTESIAN_POINT('Ctrl Pts',(-4.2273919355869,15.2,9.68149537398921));
#236202=CARTESIAN_POINT('Ctrl Pts',(-4.22818962418122,15.2,9.6853917328731));
#236203=CARTESIAN_POINT('Ctrl Pts',(-4.22885436470064,15.2,9.68863869872765));
#236204=CARTESIAN_POINT('Ctrl Pts',(-4.22951767659558,15.2,9.69191603427981));
#236205=CARTESIAN_POINT('Ctrl Pts',(-4.23017926145678,15.2,9.69522347504213));
#236206=CARTESIAN_POINT('Ctrl Pts',(-4.23097316333349,15.2,9.69919240417321));
#236207=CARTESIAN_POINT('Ctrl Pts',(-4.23176458125156,15.2,9.70320468565965));
#236208=CARTESIAN_POINT('Ctrl Pts',(-4.23255301104433,15.2,9.70725986996693));
#236209=CARTESIAN_POINT('Ctrl Pts',(-4.23321003576421,15.2,9.71063918967048));
#236210=CARTESIAN_POINT('Ctrl Pts',(-4.23386498709675,15.2,9.71404830470513));
#236211=CARTESIAN_POINT('Ctrl Pts',(-4.2345175784147,15.2,9.71748695759181));
#236212=CARTESIAN_POINT('Ctrl Pts',(-4.23517016980379,15.2,9.72092561085331));
#236213=CARTESIAN_POINT('Ctrl Pts',(-4.23582040217069,15.2,9.72439380226706));
#236214=CARTESIAN_POINT('Ctrl Pts',(-4.23646799765702,15.2,9.72789127900078));
#236215=CARTESIAN_POINT('Ctrl Pts',(-4.23737463135201,15.2,9.73278774650424));
#236216=CARTESIAN_POINT('Ctrl Pts',(-4.23827609342614,15.2,9.73774161429728));
#236217=CARTESIAN_POINT('Ctrl Pts',(-4.23917163474972,15.2,9.74275219602297));
#236218=CARTESIAN_POINT('Ctrl Pts',(-4.23993924155866,15.2,9.74704698013636));
#236219=CARTESIAN_POINT('Ctrl Pts',(-4.24070250021962,15.2,9.75138343396793));
#236220=CARTESIAN_POINT('Ctrl Pts',(-4.24146094910906,15.2,9.75576113280609));
#236221=CARTESIAN_POINT('Ctrl Pts',(-4.24209298987322,15.2,9.75940921530378));
#236222=CARTESIAN_POINT('Ctrl Pts',(-4.24272169185712,15.2,9.76308593987567));
#236223=CARTESIAN_POINT('Ctrl Pts',(-4.24334679348582,15.2,9.76679106512824));
#236224=CARTESIAN_POINT('Ctrl Pts',(-4.24409691548114,15.2,9.77123721567362));
#236225=CARTESIAN_POINT('Ctrl Pts',(-4.2448418516324,15.2,9.77572426313554));
#236226=CARTESIAN_POINT('Ctrl Pts',(-4.24558116158898,15.2,9.78025179346843));
#236227=CARTESIAN_POINT('Ctrl Pts',(-4.24644368977094,15.2,9.78553391157326));
#236228=CARTESIAN_POINT('Ctrl Pts',(-4.247298559351,15.2,9.79087113116104));
#236229=CARTESIAN_POINT('Ctrl Pts',(-4.24814508343819,15.2,9.79626280778627));
#236230=CARTESIAN_POINT('Ctrl Pts',(-4.24874974353813,15.2,9.8001140056156));
#236231=CARTESIAN_POINT('Ctrl Pts',(-4.24935014721639,15.2,9.80399298727936));
#236232=CARTESIAN_POINT('Ctrl Pts',(-4.24994604895274,15.2,9.80789951998627));
#236233=CARTESIAN_POINT('Ctrl Pts',(-4.2508994917179,15.2,9.81414997223214));
#236234=CARTESIAN_POINT('Ctrl Pts',(-4.25184140905278,15.2,9.82047095736259));
#236235=CARTESIAN_POINT('Ctrl Pts',(-4.25277082370742,15.2,9.82686153349416));
#236236=CARTESIAN_POINT('Ctrl Pts',(-4.25346788474588,15.2,9.83165446591934));
#236237=CARTESIAN_POINT('Ctrl Pts',(-4.25415791115355,15.2,9.83648654525185));
#236238=CARTESIAN_POINT('Ctrl Pts',(-4.25484050430775,15.2,9.84135738001288));
#236239=CARTESIAN_POINT('Ctrl Pts',(-4.25563686289465,15.2,9.84704001990375));
#236240=CARTESIAN_POINT('Ctrl Pts',(-4.25642309746418,15.2,9.85277540969495));
#236241=CARTESIAN_POINT('Ctrl Pts',(-4.25719858794428,15.2,9.85856294069254));
#236242=CARTESIAN_POINT('Ctrl Pts',(-4.25764172541323,15.2,9.8618701016488));
#236243=CARTESIAN_POINT('Ctrl Pts',(-4.25808135401352,15.2,9.86519428752709));
#236244=CARTESIAN_POINT('Ctrl Pts',(-4.2585173594837,15.2,9.8685353865022));
#236245=CARTESIAN_POINT('Ctrl Pts',(-4.25895336489447,15.2,9.87187648502209));
#236246=CARTESIAN_POINT('Ctrl Pts',(-4.25938574655631,15.2,9.87523449595351));
#236247=CARTESIAN_POINT('Ctrl Pts',(-4.25981439268832,15.2,9.87860930789814));
#236248=CARTESIAN_POINT('Ctrl Pts',(-4.26035020039713,15.2,9.88282782317378));
#236249=CARTESIAN_POINT('Ctrl Pts',(-4.26088017021993,15.2,9.88707258871565));
#236250=CARTESIAN_POINT('Ctrl Pts',(-4.26140408466487,15.2,9.89134339044964));
#236251=CARTESIAN_POINT('Ctrl Pts',(-4.26182321624367,15.2,9.89476003202305));
#236252=CARTESIAN_POINT('Ctrl Pts',(-4.26223847302608,15.2,9.89819333482909));
#236253=CARTESIAN_POINT('Ctrl Pts',(-4.26264974471702,15.2,9.90164318997727));
#236254=CARTESIAN_POINT('Ctrl Pts',(-4.26306101635192,15.2,9.90509304465541));
#236255=CARTESIAN_POINT('Ctrl Pts',(-4.26346830460836,15.2,9.90855945239188));
#236256=CARTESIAN_POINT('Ctrl Pts',(-4.26387149940915,15.2,9.91204230293881));
#236257=CARTESIAN_POINT('Ctrl Pts',(-4.26427469426487,15.2,9.91552515396027));
#236258=CARTESIAN_POINT('Ctrl Pts',(-4.26467379557299,15.2,9.9190244485722));
#236259=CARTESIAN_POINT('Ctrl Pts',(-4.26506869848341,15.2,9.92254007770824));
#236260=CARTESIAN_POINT('Ctrl Pts',(-4.26556232709453,15.2,9.92693461388879));
#236261=CARTESIAN_POINT('Ctrl Pts',(-4.26604939472039,15.2,9.9313546749043));
#236262=CARTESIAN_POINT('Ctrl Pts',(-4.26652969500033,15.2,9.93580004853568));
#236263=CARTESIAN_POINT('Ctrl Pts',(-4.26691393519288,15.2,9.93935634715005));
#236264=CARTESIAN_POINT('Ctrl Pts',(-4.26729384461615,15.2,9.94292884718883));
#236265=CARTESIAN_POINT('Ctrl Pts',(-4.26766932019701,15.2,9.94651744117152));
#236266=CARTESIAN_POINT('Ctrl Pts',(-4.26804479582903,15.2,9.95010603564316));
#236267=CARTESIAN_POINT('Ctrl Pts',(-4.26841583695788,15.2,9.95371072518317));
#236268=CARTESIAN_POINT('Ctrl Pts',(-4.26878234253341,15.2,9.95733140299159));
#236269=CARTESIAN_POINT('Ctrl Pts',(-4.26914884810893,15.2,9.9609520808));
#236270=CARTESIAN_POINT('Ctrl Pts',(-4.26951081723672,15.2,9.96458874757144));
#236271=CARTESIAN_POINT('Ctrl Pts',(-4.2698681495335,15.2,9.96824129860545));
#236272=CARTESIAN_POINT('Ctrl Pts',(-4.27022548178158,15.2,9.9718938491418));
#236273=CARTESIAN_POINT('Ctrl Pts',(-4.27057817702668,15.2,9.97556228326248));
#236274=CARTESIAN_POINT('Ctrl Pts',(-4.27092613599984,15.2,9.97924649725576));
#236275=CARTESIAN_POINT('Ctrl Pts',(-4.2712740950204,15.2,9.98293071175102));
#236276=CARTESIAN_POINT('Ctrl Pts',(-4.27161731734856,15.2,9.98663070625335));
#236277=CARTESIAN_POINT('Ctrl Pts',(-4.27195570558873,15.2,9.99034637679078));
#236278=CARTESIAN_POINT('Ctrl Pts',(-4.27254788493986,15.2,9.9968487994719));
#236279=CARTESIAN_POINT('Ctrl Pts',(-4.27312525655407,15.2,10.0033992315922));
#236280=CARTESIAN_POINT('Ctrl Pts',(-4.27368730472844,15.2,10.0099971239946));
#236281=CARTESIAN_POINT('Ctrl Pts',(-4.27400847515131,15.2,10.0137673486648));
#236282=CARTESIAN_POINT('Ctrl Pts',(-4.2743246422894,15.2,10.0175530698666));
#236283=CARTESIAN_POINT('Ctrl Pts',(-4.27463571125046,15.2,10.0213541870191));
#236284=CARTESIAN_POINT('Ctrl Pts',(-4.27494678016913,15.2,10.0251553036538));
#236285=CARTESIAN_POINT('Ctrl Pts',(-4.27525275171662,15.2,10.0289718168355));
#236286=CARTESIAN_POINT('Ctrl Pts',(-4.27555353019256,15.2,10.0328036241318));
#236287=CARTESIAN_POINT('Ctrl Pts',(-4.27585430870949,15.2,10.0366354319501));
#236288=CARTESIAN_POINT('Ctrl Pts',(-4.27614989643593,15.2,10.0404825346078));
#236289=CARTESIAN_POINT('Ctrl Pts',(-4.27644019950861,15.2,10.0443448325026));
#236290=CARTESIAN_POINT('Ctrl Pts',(-4.27680307832968,15.2,10.0491727046079));
#236291=CARTESIAN_POINT('Ctrl Pts',(-4.27715770080089,15.2,10.0540243188455));
#236292=CARTESIAN_POINT('Ctrl Pts',(-4.27750388802267,15.2,10.0588994808606));
#236293=CARTESIAN_POINT('Ctrl Pts',(-4.27778083777745,15.2,10.0627996101538));
#236294=CARTESIAN_POINT('Ctrl Pts',(-4.27805239009721,15.2,10.0667148098635));
#236295=CARTESIAN_POINT('Ctrl Pts',(-4.27831845446491,15.2,10.070644981874));
#236296=CARTESIAN_POINT('Ctrl Pts',(-4.27865103495171,15.2,10.0755576972888));
#236297=CARTESIAN_POINT('Ctrl Pts',(-4.27897504112487,15.2,10.0804938051893));
#236298=CARTESIAN_POINT('Ctrl Pts',(-4.27929029919678,15.2,10.0854531174493));
#236299=CARTESIAN_POINT('Ctrl Pts',(-4.27954250566806,15.2,10.0894205674736));
#236300=CARTESIAN_POINT('Ctrl Pts',(-4.27978911339308,15.2,10.093402866558));
#236301=CARTESIAN_POINT('Ctrl Pts',(-4.28003003579472,15.2,10.0973999177768));
#236302=CARTESIAN_POINT('Ctrl Pts',(-4.28039141936436,15.2,10.1033954940604));
#236303=CARTESIAN_POINT('Ctrl Pts',(-4.28074000931003,15.2,10.109424264108));
#236304=CARTESIAN_POINT('Ctrl Pts',(-4.28107551596507,15.2,10.1154859013864));
#236305=CARTESIAN_POINT('Ctrl Pts',(-4.28129918708875,15.2,10.1195269932723));
#236306=CARTESIAN_POINT('Ctrl Pts',(-4.28151704311174,15.2,10.12358269261));
#236307=CARTESIAN_POINT('Ctrl Pts',(-4.28172900023402,15.2,10.1276529038328));
#236308=CARTESIAN_POINT('Ctrl Pts',(-4.28199394662242,15.2,10.132740667584));
#236309=CARTESIAN_POINT('Ctrl Pts',(-4.28224967473366,15.2,10.1378511060601));
#236310=CARTESIAN_POINT('Ctrl Pts',(-4.28249602349531,15.2,10.1429840343042));
#236311=CARTESIAN_POINT('Ctrl Pts',(-4.28274237225697,15.2,10.1481169625483));
#236312=CARTESIAN_POINT('Ctrl Pts',(-4.28297933891394,15.2,10.1532723804865));
#236313=CARTESIAN_POINT('Ctrl Pts',(-4.28320676453816,15.2,10.1584501027105));
#236314=CARTESIAN_POINT('Ctrl Pts',(-4.28338870502266,15.2,10.1625922801511));
#236315=CARTESIAN_POINT('Ctrl Pts',(-4.28356453970795,15.2,10.1667487335482));
#236316=CARTESIAN_POINT('Ctrl Pts',(-4.28373418619449,15.2,10.1709193681508));
#236317=CARTESIAN_POINT('Ctrl Pts',(-4.28390383270413,15.2,10.1750900033216));
#236318=CARTESIAN_POINT('Ctrl Pts',(-4.28406729243199,15.2,10.1792748189195));
#236319=CARTESIAN_POINT('Ctrl Pts',(-4.28422448428119,15.2,10.1834737243593));
#236320=CARTESIAN_POINT('Ctrl Pts',(-4.28438167610898,15.2,10.187672629227));
#236321=CARTESIAN_POINT('Ctrl Pts',(-4.28453260015794,15.2,10.1918856212343));
#236322=CARTESIAN_POINT('Ctrl Pts',(-4.28467717797987,15.2,10.1961126098878));
#236323=CARTESIAN_POINT('Ctrl Pts',(-4.2848217558215,15.2,10.2003395991173));
#236324=CARTESIAN_POINT('Ctrl Pts',(-4.28495998530959,15.2,10.2045805832818));
#236325=CARTESIAN_POINT('Ctrl Pts',(-4.2850917917608,15.2,10.2088354718479));
#236326=CARTESIAN_POINT('Ctrl Pts',(-4.28522359819404,15.2,10.2130903598343));
#236327=CARTESIAN_POINT('Ctrl Pts',(-4.28534898008323,15.2,10.2173591505687));
#236328=CARTESIAN_POINT('Ctrl Pts',(-4.28546785869113,15.2,10.2216417541536));
#236329=CARTESIAN_POINT('Ctrl Pts',(-4.28558673731522,15.2,10.2259243583219));
#236330=CARTESIAN_POINT('Ctrl Pts',(-4.28569911563389,15.2,10.2302207757055));
#236331=CARTESIAN_POINT('Ctrl Pts',(-4.28580491425033,15.2,10.2345309123858));
#236332=CARTESIAN_POINT('Ctrl Pts',(-4.28591071285237,15.2,10.2388410484787));
#236333=CARTESIAN_POINT('Ctrl Pts',(-4.2860099334585,15.2,10.2431649054134));
#236334=CARTESIAN_POINT('Ctrl Pts',(-4.28610249945161,15.2,10.2475023940574));
#236335=CARTESIAN_POINT('Ctrl Pts',(-4.28621820695246,15.2,10.2529242553057));
#236336=CARTESIAN_POINT('Ctrl Pts',(-4.28632352038913,15.2,10.2583674126997));
#236337=CARTESIAN_POINT('Ctrl Pts',(-4.28641829025571,15.2,10.263831692624));
#236338=CARTESIAN_POINT('Ctrl Pts',(-4.2865320141018,15.2,10.2703888288905));
#236339=CARTESIAN_POINT('Ctrl Pts',(-4.28663055673067,15.2,10.2769763806085));
#236340=CARTESIAN_POINT('Ctrl Pts',(-4.28671367348414,15.2,10.2835940464713));
#236341=CARTESIAN_POINT('Ctrl Pts',(-4.28676908464557,15.2,10.288005823112));
#236342=CARTESIAN_POINT('Ctrl Pts',(-4.28681763861068,15.2,10.2924309831509));
#236343=CARTESIAN_POINT('Ctrl Pts',(-4.28685926449661,15.2,10.2968694391205));
#236344=CARTESIAN_POINT('Ctrl Pts',(-4.28690089038822,15.2,10.3013078956949));
#236345=CARTESIAN_POINT('Ctrl Pts',(-4.28693558675733,15.2,10.3057596469692));
#236346=CARTESIAN_POINT('Ctrl Pts',(-4.2869632845374,15.2,10.3102246058812));
#236347=CARTESIAN_POINT('Ctrl Pts',(-4.28700483120372,15.2,10.3169220436409));
#236348=CARTESIAN_POINT('Ctrl Pts',(-4.28703062650878,15.2,10.3236491973451));
#236349=CARTESIAN_POINT('Ctrl Pts',(-4.28704043542509,15.2,10.3304057707665));
#236350=CARTESIAN_POINT('Ctrl Pts',(-4.28704533988324,15.2,10.3337840574773));
#236351=CARTESIAN_POINT('Ctrl Pts',(-4.28704624763323,15.2,10.3371696990708));
#236352=CARTESIAN_POINT('Ctrl Pts',(-4.28704313000869,15.2,10.3405626588219));
#236353=CARTESIAN_POINT('Ctrl Pts',(-4.28704001238415,15.2,10.343955618573));
#236354=CARTESIAN_POINT('Ctrl Pts',(-4.28703286856856,15.2,10.3473558971951));
#236355=CARTESIAN_POINT('Ctrl Pts',(-4.28702167002721,15.2,10.3507634570741));
#236356=CARTESIAN_POINT('Ctrl Pts',(-4.28700673863739,15.2,10.3553068706586));
#236357=CARTESIAN_POINT('Ctrl Pts',(-4.28698459864969,15.2,10.3598632302321));
#236358=CARTESIAN_POINT('Ctrl Pts',(-4.28695518198094,15.2,10.3644324476486));
#236359=CARTESIAN_POINT('Ctrl Pts',(-4.2869257653162,15.2,10.3690016644425));
#236360=CARTESIAN_POINT('Ctrl Pts',(-4.2868890726196,15.2,10.3735837396813));
#236361=CARTESIAN_POINT('Ctrl Pts',(-4.28684503529062,15.2,10.3781785877487));
#236362=CARTESIAN_POINT('Ctrl Pts',(-4.28681200728638,15.2,10.3816247245818));
#236363=CARTESIAN_POINT('Ctrl Pts',(-4.28677484828098,15.2,10.3850780466838));
#236364=CARTESIAN_POINT('Ctrl Pts',(-4.28673353119107,15.2,10.388538517021));
#236365=CARTESIAN_POINT('Ctrl Pts',(-4.28669221410867,15.2,10.3919989867296));
#236366=CARTESIAN_POINT('Ctrl Pts',(-4.28664673729159,15.2,10.3954666050241));
#236367=CARTESIAN_POINT('Ctrl Pts',(-4.28659707424877,15.2,10.3989413359473));
#236368=CARTESIAN_POINT('Ctrl Pts',(-4.28653085686134,15.2,10.4035743103011));
#236369=CARTESIAN_POINT('Ctrl Pts',(-4.28645719745508,15.2,10.4082199292731));
#236370=CARTESIAN_POINT('Ctrl Pts',(-4.28637602823998,15.2,10.4128781073359));
#236371=CARTESIAN_POINT('Ctrl Pts',(-4.2863151513259,15.2,10.4163717410417));
#236372=CARTESIAN_POINT('Ctrl Pts',(-4.28625005169543,15.2,10.4198724393804));
#236373=CARTESIAN_POINT('Ctrl Pts',(-4.2861807007402,15.2,10.4233801679603));
#236374=CARTESIAN_POINT('Ctrl Pts',(-4.28611134977236,15.2,10.4268878971774));
#236375=CARTESIAN_POINT('Ctrl Pts',(-4.28603774857834,15.2,10.4304026542049));
#236376=CARTESIAN_POINT('Ctrl Pts',(-4.2859598699831,15.2,10.4339244055093));
#236377=CARTESIAN_POINT('Ctrl Pts',(-4.28588199140202,15.2,10.437446156174));
#236378=CARTESIAN_POINT('Ctrl Pts',(-4.28579983431833,15.2,10.4409749009018));
#236379=CARTESIAN_POINT('Ctrl Pts',(-4.28571337327498,15.2,10.4445106042007));
#236380=CARTESIAN_POINT('Ctrl Pts',(-4.28562691223164,15.2,10.4480463074996));
#236381=CARTESIAN_POINT('Ctrl Pts',(-4.28553614595324,15.2,10.451588966932));
#236382=CARTESIAN_POINT('Ctrl Pts',(-4.28544104945631,15.2,10.4551385505953));
#236383=CARTESIAN_POINT('Ctrl Pts',(-4.28531425413284,15.2,10.4598713285981));
#236384=CARTESIAN_POINT('Ctrl Pts',(-4.28517975971091,15.2,10.4646164143845));
#236385=CARTESIAN_POINT('Ctrl Pts',(-4.28503750305668,15.2,10.4693737244388));
#236386=CARTESIAN_POINT('Ctrl Pts',(-4.28489524638305,15.2,10.4741310351412));
#236387=CARTESIAN_POINT('Ctrl Pts',(-4.28474522652536,15.2,10.4789005686615));
#236388=CARTESIAN_POINT('Ctrl Pts',(-4.28458738451676,15.2,10.4836822446999));
#236389=CARTESIAN_POINT('Ctrl Pts',(-4.28446900302105,15.2,10.487268501403));
#236390=CARTESIAN_POINT('Ctrl Pts',(-4.2843462211422,15.2,10.4908615878557));
#236391=CARTESIAN_POINT('Ctrl Pts',(-4.28421901227221,15.2,10.4944614680993));
#236392=CARTESIAN_POINT('Ctrl Pts',(-4.28404940043015,15.2,10.4992613088601));
#236393=CARTESIAN_POINT('Ctrl Pts',(-4.28387192050986,15.2,10.5040732302728));
#236394=CARTESIAN_POINT('Ctrl Pts',(-4.28368651048981,15.2,10.508897148));
#236395=CARTESIAN_POINT('Ctrl Pts',(-4.28354745298739,15.2,10.5125150859667));
#236396=CARTESIAN_POINT('Ctrl Pts',(-4.28340393492889,15.2,10.5161397719106));
#236397=CARTESIAN_POINT('Ctrl Pts',(-4.28325593147555,15.2,10.5197711726125));
#236398=CARTESIAN_POINT('Ctrl Pts',(-4.2831079280222,15.2,10.5234025733145));
#236399=CARTESIAN_POINT('Ctrl Pts',(-4.28295543912772,15.2,10.527040687749));
#236400=CARTESIAN_POINT('Ctrl Pts',(-4.28279843925842,15.2,10.5306854810333));
#236401=CARTESIAN_POINT('Ctrl Pts',(-4.28253677280009,15.2,10.5367601367277));
#236402=CARTESIAN_POINT('Ctrl Pts',(-4.28226257845127,15.2,10.5428533464254));
#236403=CARTESIAN_POINT('Ctrl Pts',(-4.2819757394916,15.2,10.5489649535366));
#236404=CARTESIAN_POINT('Ctrl Pts',(-4.28174626834262,15.2,10.5538542388258));
#236405=CARTESIAN_POINT('Ctrl Pts',(-4.281508706411,15.2,10.5587552956745));
#236406=CARTESIAN_POINT('Ctrl Pts',(-4.28126299326526,15.2,10.5636680444384));
#236407=CARTESIAN_POINT('Ctrl Pts',(-4.28095585180797,15.2,10.5698089808952));
#236408=CARTESIAN_POINT('Ctrl Pts',(-4.28063597617033,15.2,10.575968186299));
#236409=CARTESIAN_POINT('Ctrl Pts',(-4.28030325631027,15.2,10.5821455059503));
#236410=CARTESIAN_POINT('Ctrl Pts',(-4.27997053645021,15.2,10.5883228256015));
#236411=CARTESIAN_POINT('Ctrl Pts',(-4.27962497293089,15.2,10.5945182582029));
#236412=CARTESIAN_POINT('Ctrl Pts',(-4.279266452775,15.2,10.6007316449704));
#236413=CARTESIAN_POINT('Ctrl Pts',(-4.27905134068927,15.2,10.6044596768954));
#236414=CARTESIAN_POINT('Ctrl Pts',(-4.27883156299022,15.2,10.6081941721879));
#236415=CARTESIAN_POINT('Ctrl Pts',(-4.27860709758235,15.2,10.6119350969261));
#236416=CARTESIAN_POINT('Ctrl Pts',(-4.27823298855564,15.2,10.6181699717163));
#236417=CARTESIAN_POINT('Ctrl Pts',(-4.27784585964581,15.2,10.624422708598));
#236418=CARTESIAN_POINT('Ctrl Pts',(-4.27744560978577,15.2,10.6306931633881));
#236419=CARTESIAN_POINT('Ctrl Pts',(-4.27720545983485,15.2,10.634455436809));
#236420=CARTESIAN_POINT('Ctrl Pts',(-4.27696058651593,15.2,10.6382240885234));
#236421=CARTESIAN_POINT('Ctrl Pts',(-4.27671096093733,15.2,10.6419990772812));
#236422=CARTESIAN_POINT('Ctrl Pts',(-4.27646133540409,15.2,10.6457740653533));
#236423=CARTESIAN_POINT('Ctrl Pts',(-4.27620695657065,15.2,10.6495553893138));
#236424=CARTESIAN_POINT('Ctrl Pts',(-4.27594780073323,15.2,10.6533430147828));
#236425=CARTESIAN_POINT('Ctrl Pts',(-4.27568864489581,15.2,10.6571306402518));
#236426=CARTESIAN_POINT('Ctrl Pts',(-4.27542471209421,15.2,10.660924565292));
#236427=CARTESIAN_POINT('Ctrl Pts',(-4.27515599200001,15.2,10.6647247759375));
#236428=CARTESIAN_POINT('Ctrl Pts',(-4.27488727190581,15.2,10.668524986583));
#236429=CARTESIAN_POINT('Ctrl Pts',(-4.27461376005061,15.2,10.6723314813073));
#236430=CARTESIAN_POINT('Ctrl Pts',(-4.27433547000006,15.2,10.676144262));
#236431=CARTESIAN_POINT('Origin',(-5.66257110645729E-14,15.2,-1.77635683940025E-14));
#236432=CARTESIAN_POINT('',(-4.5738377119823,15.2,9.31239140029717));
#236433=CARTESIAN_POINT('',(-4.5738377119823,12.2,9.31239140029717));
#236434=CARTESIAN_POINT('',(-4.57383771200006,15.2,9.31239139999998));
#236435=CARTESIAN_POINT('Origin',(-5.66257110645729E-14,12.2,-1.77635683940025E-14));
#236436=CARTESIAN_POINT('Origin',(-5.66257110645729E-14,15.2,-1.77635683940025E-14));
#236437=CARTESIAN_POINT('Origin',(-5.66257110645729E-14,15.2,-1.77635683940025E-14));
#236438=CARTESIAN_POINT('',(-5.41482055400006,15.2,10.145428447));
#236439=CARTESIAN_POINT('',(-5.75020264100006,15.2,9.95917514599999));
#236440=CARTESIAN_POINT('Origin',(-5.66257110645729E-14,15.2,-1.77635683940025E-14));
#236441=CARTESIAN_POINT('',(-5.75020264100006,12.2,9.95917514599999));
#236442=CARTESIAN_POINT('',(-5.75020264100006,15.2,9.95917514599999));
#236443=CARTESIAN_POINT('',(-5.41482055400006,12.2,10.145428447));
#236444=CARTESIAN_POINT('Origin',(-5.66257110645729E-14,12.2,-1.77635683940025E-14));
#236445=CARTESIAN_POINT('',(-5.41482055400006,15.2,10.145428447));
#236446=CARTESIAN_POINT('Ctrl Pts',(-5.75020264100006,15.2,9.95917514599999));
#236447=CARTESIAN_POINT('Ctrl Pts',(-5.75020264100006,11.6,9.95917514599999));
#236448=CARTESIAN_POINT('Ctrl Pts',(-5.75014921100006,15.2,9.95841243099999));
#236449=CARTESIAN_POINT('Ctrl Pts',(-5.75014921100006,11.6,9.95841243099999));
#236450=CARTESIAN_POINT('Ctrl Pts',(-5.75004209300006,15.2,9.95688745999999));
#236451=CARTESIAN_POINT('Ctrl Pts',(-5.75004209300006,11.6,9.95688745999999));
#236452=CARTESIAN_POINT('Ctrl Pts',(-5.74988064800006,15.2,9.95460138499999));
#236453=CARTESIAN_POINT('Ctrl Pts',(-5.74988064800006,11.6,9.95460138499999));
#236454=CARTESIAN_POINT('Ctrl Pts',(-5.74966385000006,15.2,9.95155604499999));
#236455=CARTESIAN_POINT('Ctrl Pts',(-5.74966385000006,11.6,9.95155604499999));
#236456=CARTESIAN_POINT('Ctrl Pts',(-5.74939029000006,15.2,9.94775396999999));
#236457=CARTESIAN_POINT('Ctrl Pts',(-5.74939029000006,11.6,9.94775396999999));
#236458=CARTESIAN_POINT('Ctrl Pts',(-5.74911416700005,15.2,9.94395649799999));
#236459=CARTESIAN_POINT('Ctrl Pts',(-5.74911416700005,11.6,9.94395649799999));
#236460=CARTESIAN_POINT('Ctrl Pts',(-5.74883548500006,15.2,9.94016363199999));
#236461=CARTESIAN_POINT('Ctrl Pts',(-5.74883548500006,11.6,9.94016363199999));
#236462=CARTESIAN_POINT('Ctrl Pts',(-5.74855424400006,15.2,9.93637536999999));
#236463=CARTESIAN_POINT('Ctrl Pts',(-5.74855424400006,11.6,9.93637536999999));
#236464=CARTESIAN_POINT('Ctrl Pts',(-5.74827044900006,15.2,9.93259172099999));
#236465=CARTESIAN_POINT('Ctrl Pts',(-5.74827044900006,11.6,9.93259172099999));
#236466=CARTESIAN_POINT('Ctrl Pts',(-5.74798410500006,15.2,9.92881268999999));
#236467=CARTESIAN_POINT('Ctrl Pts',(-5.74798410500006,11.6,9.92881268999999));
#236468=CARTESIAN_POINT('Ctrl Pts',(-5.74769522100006,15.2,9.92503828399999));
#236469=CARTESIAN_POINT('Ctrl Pts',(-5.74769522100006,11.6,9.92503828399999));
#236470=CARTESIAN_POINT('Ctrl Pts',(-5.74740380000006,15.2,9.92126850899999));
#236471=CARTESIAN_POINT('Ctrl Pts',(-5.74740380000006,11.6,9.92126850899999));
#236472=CARTESIAN_POINT('Ctrl Pts',(-5.74710985300006,15.2,9.91750337599999));
#236473=CARTESIAN_POINT('Ctrl Pts',(-5.74710985300006,11.6,9.91750337599999));
#236474=CARTESIAN_POINT('Ctrl Pts',(-5.74681338800006,15.2,9.91374289199998));
#236475=CARTESIAN_POINT('Ctrl Pts',(-5.74681338800006,11.6,9.91374289199998));
#236476=CARTESIAN_POINT('Ctrl Pts',(-5.74651440900006,15.2,9.90998706399999));
#236477=CARTESIAN_POINT('Ctrl Pts',(-5.74651440900006,11.6,9.90998706399999));
#236478=CARTESIAN_POINT('Ctrl Pts',(-5.74621292500006,15.2,9.90623589899998));
#236479=CARTESIAN_POINT('Ctrl Pts',(-5.74621292500006,11.6,9.90623589899998));
#236480=CARTESIAN_POINT('Ctrl Pts',(-5.74590894000006,15.2,9.90248940599999));
#236481=CARTESIAN_POINT('Ctrl Pts',(-5.74590894000006,11.6,9.90248940599999));
#236482=CARTESIAN_POINT('Ctrl Pts',(-5.74560246200006,15.2,9.89874758699998));
#236483=CARTESIAN_POINT('Ctrl Pts',(-5.74560246200006,11.6,9.89874758699998));
#236484=CARTESIAN_POINT('Ctrl Pts',(-5.74529349500006,15.2,9.89501044999999));
#236485=CARTESIAN_POINT('Ctrl Pts',(-5.74529349500006,11.6,9.89501044999999));
#236486=CARTESIAN_POINT('Ctrl Pts',(-5.74498204400006,15.2,9.89127800199999));
#236487=CARTESIAN_POINT('Ctrl Pts',(-5.74498204400006,11.6,9.89127800199999));
#236488=CARTESIAN_POINT('Ctrl Pts',(-5.74466811600006,15.2,9.88755024699999));
#236489=CARTESIAN_POINT('Ctrl Pts',(-5.74466811600006,11.6,9.88755024699999));
#236490=CARTESIAN_POINT('Ctrl Pts',(-5.74435171600006,15.2,9.88382719299998));
#236491=CARTESIAN_POINT('Ctrl Pts',(-5.74435171600006,11.6,9.88382719299998));
#236492=CARTESIAN_POINT('Ctrl Pts',(-5.74403285200006,15.2,9.88010884599999));
#236493=CARTESIAN_POINT('Ctrl Pts',(-5.74403285200006,11.6,9.88010884599999));
#236494=CARTESIAN_POINT('Ctrl Pts',(-5.74371152900006,15.2,9.87639521399998));
#236495=CARTESIAN_POINT('Ctrl Pts',(-5.74371152900006,11.6,9.87639521399998));
#236496=CARTESIAN_POINT('Ctrl Pts',(-5.74338775500006,15.2,9.87268630299998));
#236497=CARTESIAN_POINT('Ctrl Pts',(-5.74338775500006,11.6,9.87268630299998));
#236498=CARTESIAN_POINT('Ctrl Pts',(-5.74306153500006,15.2,9.86898211999998));
#236499=CARTESIAN_POINT('Ctrl Pts',(-5.74306153500006,11.6,9.86898211999998));
#236500=CARTESIAN_POINT('Ctrl Pts',(-5.74273287600006,15.2,9.86528267199999));
#236501=CARTESIAN_POINT('Ctrl Pts',(-5.74273287600006,11.6,9.86528267199999));
#236502=CARTESIAN_POINT('Ctrl Pts',(-5.74240178500006,15.2,9.86158796599998));
#236503=CARTESIAN_POINT('Ctrl Pts',(-5.74240178500006,11.6,9.86158796599998));
#236504=CARTESIAN_POINT('Ctrl Pts',(-5.74206826800006,15.2,9.85789800899998));
#236505=CARTESIAN_POINT('Ctrl Pts',(-5.74206826800006,11.6,9.85789800899998));
#236506=CARTESIAN_POINT('Ctrl Pts',(-5.74173233000006,15.2,9.85421280699999));
#236507=CARTESIAN_POINT('Ctrl Pts',(-5.74173233000006,11.6,9.85421280699999));
#236508=CARTESIAN_POINT('Ctrl Pts',(-5.74139397800006,15.2,9.85053236499999));
#236509=CARTESIAN_POINT('Ctrl Pts',(-5.74139397800006,11.6,9.85053236499999));
#236510=CARTESIAN_POINT('Ctrl Pts',(-5.74105321900006,15.2,9.84685669199998));
#236511=CARTESIAN_POINT('Ctrl Pts',(-5.74105321900006,11.6,9.84685669199998));
#236512=CARTESIAN_POINT('Ctrl Pts',(-5.74071005800006,15.2,9.84318579399999));
#236513=CARTESIAN_POINT('Ctrl Pts',(-5.74071005800006,11.6,9.84318579399999));
#236514=CARTESIAN_POINT('Ctrl Pts',(-5.74036450400006,15.2,9.83951967699999));
#236515=CARTESIAN_POINT('Ctrl Pts',(-5.74036450400006,11.6,9.83951967699999));
#236516=CARTESIAN_POINT('Ctrl Pts',(-5.74001656100006,15.2,9.83585834899999));
#236517=CARTESIAN_POINT('Ctrl Pts',(-5.74001656100006,11.6,9.83585834899999));
#236518=CARTESIAN_POINT('Ctrl Pts',(-5.73966623600006,15.2,9.83220181499998));
#236519=CARTESIAN_POINT('Ctrl Pts',(-5.73966623600006,11.6,9.83220181499998));
#236520=CARTESIAN_POINT('Ctrl Pts',(-5.73931353600006,15.2,9.82855008299998));
#236521=CARTESIAN_POINT('Ctrl Pts',(-5.73931353600006,11.6,9.82855008299998));
#236522=CARTESIAN_POINT('Ctrl Pts',(-5.73895846700006,15.2,9.82490316099998));
#236523=CARTESIAN_POINT('Ctrl Pts',(-5.73895846700006,11.6,9.82490316099998));
#236524=CARTESIAN_POINT('Ctrl Pts',(-5.73860103600006,15.2,9.82126105199999));
#236525=CARTESIAN_POINT('Ctrl Pts',(-5.73860103600006,11.6,9.82126105199999));
#236526=CARTESIAN_POINT('Ctrl Pts',(-5.73824124900006,15.2,9.81762376799999));
#236527=CARTESIAN_POINT('Ctrl Pts',(-5.73824124900006,11.6,9.81762376799999));
#236528=CARTESIAN_POINT('Ctrl Pts',(-5.73787911300006,15.2,9.81399130999998));
#236529=CARTESIAN_POINT('Ctrl Pts',(-5.73787911300006,11.6,9.81399130999998));
#236530=CARTESIAN_POINT('Ctrl Pts',(-5.73751463500006,15.2,9.81036368899998));
#236531=CARTESIAN_POINT('Ctrl Pts',(-5.73751463500006,11.6,9.81036368899998));
#236532=CARTESIAN_POINT('Ctrl Pts',(-5.73714782000006,15.2,9.80674091099999));
#236533=CARTESIAN_POINT('Ctrl Pts',(-5.73714782000006,11.6,9.80674091099999));
#236534=CARTESIAN_POINT('Ctrl Pts',(-5.73677867600006,15.2,9.80312298099999));
#236535=CARTESIAN_POINT('Ctrl Pts',(-5.73677867600006,11.6,9.80312298099999));
#236536=CARTESIAN_POINT('Ctrl Pts',(-5.73640720900006,15.2,9.79950990699999));
#236537=CARTESIAN_POINT('Ctrl Pts',(-5.73640720900006,11.6,9.79950990699999));
#236538=CARTESIAN_POINT('Ctrl Pts',(-5.73603342500006,15.2,9.79590169699998));
#236539=CARTESIAN_POINT('Ctrl Pts',(-5.73603342500006,11.6,9.79590169699998));
#236540=CARTESIAN_POINT('Ctrl Pts',(-5.73565733200006,15.2,9.79229835499999));
#236541=CARTESIAN_POINT('Ctrl Pts',(-5.73565733200006,11.6,9.79229835499999));
#236542=CARTESIAN_POINT('Ctrl Pts',(-5.73527893600006,15.2,9.78869988999998));
#236543=CARTESIAN_POINT('Ctrl Pts',(-5.73527893600006,11.6,9.78869988999998));
#236544=CARTESIAN_POINT('Ctrl Pts',(-5.73489824300006,15.2,9.78510630799999));
#236545=CARTESIAN_POINT('Ctrl Pts',(-5.73489824300006,11.6,9.78510630799999));
#236546=CARTESIAN_POINT('Ctrl Pts',(-5.73451526200006,15.2,9.78151761599998));
#236547=CARTESIAN_POINT('Ctrl Pts',(-5.73451526200006,11.6,9.78151761599998));
#236548=CARTESIAN_POINT('Ctrl Pts',(-5.73412999600006,15.2,9.77793381999999));
#236549=CARTESIAN_POINT('Ctrl Pts',(-5.73412999600006,11.6,9.77793381999999));
#236550=CARTESIAN_POINT('Ctrl Pts',(-5.73374245400006,15.2,9.77435492899998));
#236551=CARTESIAN_POINT('Ctrl Pts',(-5.73374245400006,11.6,9.77435492899998));
#236552=CARTESIAN_POINT('Ctrl Pts',(-5.73335264400006,15.2,9.77078094799998));
#236553=CARTESIAN_POINT('Ctrl Pts',(-5.73335264400006,11.6,9.77078094799998));
#236554=CARTESIAN_POINT('Ctrl Pts',(-5.73296057100006,15.2,9.76721188399999));
#236555=CARTESIAN_POINT('Ctrl Pts',(-5.73296057100006,11.6,9.76721188399999));
#236556=CARTESIAN_POINT('Ctrl Pts',(-5.73256624100006,15.2,9.76364774399999));
#236557=CARTESIAN_POINT('Ctrl Pts',(-5.73256624100006,11.6,9.76364774399999));
#236558=CARTESIAN_POINT('Ctrl Pts',(-5.73216966200006,15.2,9.76008853499999));
#236559=CARTESIAN_POINT('Ctrl Pts',(-5.73216966200006,11.6,9.76008853499999));
#236560=CARTESIAN_POINT('Ctrl Pts',(-5.73177084200006,15.2,9.75653426499999));
#236561=CARTESIAN_POINT('Ctrl Pts',(-5.73177084200006,11.6,9.75653426499999));
#236562=CARTESIAN_POINT('Ctrl Pts',(-5.73136978500006,15.2,9.75298493899999));
#236563=CARTESIAN_POINT('Ctrl Pts',(-5.73136978500006,11.6,9.75298493899999));
#236564=CARTESIAN_POINT('Ctrl Pts',(-5.73096649900006,15.2,9.74944056499999));
#236565=CARTESIAN_POINT('Ctrl Pts',(-5.73096649900006,11.6,9.74944056499999));
#236566=CARTESIAN_POINT('Ctrl Pts',(-5.73056099300006,15.2,9.74590114899998));
#236567=CARTESIAN_POINT('Ctrl Pts',(-5.73056099300006,11.6,9.74590114899998));
#236568=CARTESIAN_POINT('Ctrl Pts',(-5.73015327100006,15.2,9.74236669799998));
#236569=CARTESIAN_POINT('Ctrl Pts',(-5.73015327100006,11.6,9.74236669799998));
#236570=CARTESIAN_POINT('Ctrl Pts',(-5.72974334100006,15.2,9.73883721999999));
#236571=CARTESIAN_POINT('Ctrl Pts',(-5.72974334100006,11.6,9.73883721999999));
#236572=CARTESIAN_POINT('Ctrl Pts',(-5.72933121000006,15.2,9.73531272199999));
#236573=CARTESIAN_POINT('Ctrl Pts',(-5.72933121000006,11.6,9.73531272199999));
#236574=CARTESIAN_POINT('Ctrl Pts',(-5.72891688500006,15.2,9.73179320899998));
#236575=CARTESIAN_POINT('Ctrl Pts',(-5.72891688500006,11.6,9.73179320899998));
#236576=CARTESIAN_POINT('Ctrl Pts',(-5.72850037300006,15.2,9.72827868899999));
#236577=CARTESIAN_POINT('Ctrl Pts',(-5.72850037300006,11.6,9.72827868899999));
#236578=CARTESIAN_POINT('Ctrl Pts',(-5.72808168000006,15.2,9.72476916899998));
#236579=CARTESIAN_POINT('Ctrl Pts',(-5.72808168000006,11.6,9.72476916899998));
#236580=CARTESIAN_POINT('Ctrl Pts',(-5.72766081400006,15.2,9.72126465699999));
#236581=CARTESIAN_POINT('Ctrl Pts',(-5.72766081400006,11.6,9.72126465699999));
#236582=CARTESIAN_POINT('Ctrl Pts',(-5.72723778200006,15.2,9.71776515799998));
#236583=CARTESIAN_POINT('Ctrl Pts',(-5.72723778200006,11.6,9.71776515799998));
#236584=CARTESIAN_POINT('Ctrl Pts',(-5.72681259100006,15.2,9.71427067999999));
#236585=CARTESIAN_POINT('Ctrl Pts',(-5.72681259100006,11.6,9.71427067999999));
#236586=CARTESIAN_POINT('Ctrl Pts',(-5.72638524800006,15.2,9.71078122899998));
#236587=CARTESIAN_POINT('Ctrl Pts',(-5.72638524800006,11.6,9.71078122899998));
#236588=CARTESIAN_POINT('Ctrl Pts',(-5.72595575900006,15.2,9.70729681399998));
#236589=CARTESIAN_POINT('Ctrl Pts',(-5.72595575900006,11.6,9.70729681399998));
#236590=CARTESIAN_POINT('Ctrl Pts',(-5.72552413200006,15.2,9.70381743999998));
#236591=CARTESIAN_POINT('Ctrl Pts',(-5.72552413200006,11.6,9.70381743999998));
#236592=CARTESIAN_POINT('Ctrl Pts',(-5.72509037500006,15.2,9.70034311599999));
#236593=CARTESIAN_POINT('Ctrl Pts',(-5.72509037500006,11.6,9.70034311599999));
#236594=CARTESIAN_POINT('Ctrl Pts',(-5.72465449300006,15.2,9.69687384599998));
#236595=CARTESIAN_POINT('Ctrl Pts',(-5.72465449300006,11.6,9.69687384599998));
#236596=CARTESIAN_POINT('Ctrl Pts',(-5.72421649500006,15.2,9.69340963899998));
#236597=CARTESIAN_POINT('Ctrl Pts',(-5.72421649500006,11.6,9.69340963899998));
#236598=CARTESIAN_POINT('Ctrl Pts',(-5.72377638800006,15.2,9.68995050099998));
#236599=CARTESIAN_POINT('Ctrl Pts',(-5.72377638800006,11.6,9.68995050099998));
#236600=CARTESIAN_POINT('Ctrl Pts',(-5.72333417800006,15.2,9.68649644199999));
#236601=CARTESIAN_POINT('Ctrl Pts',(-5.72333417800006,11.6,9.68649644199999));
#236602=CARTESIAN_POINT('Ctrl Pts',(-5.72288987300006,15.2,9.68304746399999));
#236603=CARTESIAN_POINT('Ctrl Pts',(-5.72288987300006,11.6,9.68304746399999));
#236604=CARTESIAN_POINT('Ctrl Pts',(-5.72244348000006,15.2,9.67960357899998));
#236605=CARTESIAN_POINT('Ctrl Pts',(-5.72244348000006,11.6,9.67960357899998));
#236606=CARTESIAN_POINT('Ctrl Pts',(-5.72199500700005,15.2,9.67616478899998));
#236607=CARTESIAN_POINT('Ctrl Pts',(-5.72199500700005,11.6,9.67616478899998));
#236608=CARTESIAN_POINT('Ctrl Pts',(-5.72154446100006,15.2,9.67273110599999));
#236609=CARTESIAN_POINT('Ctrl Pts',(-5.72154446100006,11.6,9.67273110599999));
#236610=CARTESIAN_POINT('Ctrl Pts',(-5.72109184700006,15.2,9.66930253499999));
#236611=CARTESIAN_POINT('Ctrl Pts',(-5.72109184700006,11.6,9.66930253499999));
#236612=CARTESIAN_POINT('Ctrl Pts',(-5.72063717600006,15.2,9.66587908099999));
#236613=CARTESIAN_POINT('Ctrl Pts',(-5.72063717600006,11.6,9.66587908099999));
#236614=CARTESIAN_POINT('Ctrl Pts',(-5.72018045300006,15.2,9.66246075399999));
#236615=CARTESIAN_POINT('Ctrl Pts',(-5.72018045300006,11.6,9.66246075399999));
#236616=CARTESIAN_POINT('Ctrl Pts',(-5.71972168400006,15.2,9.65904755899999));
#236617=CARTESIAN_POINT('Ctrl Pts',(-5.71972168400006,11.6,9.65904755899999));
#236618=CARTESIAN_POINT('Ctrl Pts',(-5.71926088000006,15.2,9.65563950599999));
#236619=CARTESIAN_POINT('Ctrl Pts',(-5.71926088000006,11.6,9.65563950599999));
#236620=CARTESIAN_POINT('Ctrl Pts',(-5.71879804600006,15.2,9.65223659799998));
#236621=CARTESIAN_POINT('Ctrl Pts',(-5.71879804600006,11.6,9.65223659799998));
#236622=CARTESIAN_POINT('Ctrl Pts',(-5.71833319100006,15.2,9.64883884499999));
#236623=CARTESIAN_POINT('Ctrl Pts',(-5.71833319100006,11.6,9.64883884499999));
#236624=CARTESIAN_POINT('Ctrl Pts',(-5.71786631900006,15.2,9.64544625299999));
#236625=CARTESIAN_POINT('Ctrl Pts',(-5.71786631900006,11.6,9.64544625299999));
#236626=CARTESIAN_POINT('Ctrl Pts',(-5.71739744200006,15.2,9.64205882999998));
#236627=CARTESIAN_POINT('Ctrl Pts',(-5.71739744200006,11.6,9.64205882999998));
#236628=CARTESIAN_POINT('Ctrl Pts',(-5.71692656400006,15.2,9.63867658199998));
#236629=CARTESIAN_POINT('Ctrl Pts',(-5.71692656400006,11.6,9.63867658199998));
#236630=CARTESIAN_POINT('Ctrl Pts',(-5.71645369500006,15.2,9.63529951699999));
#236631=CARTESIAN_POINT('Ctrl Pts',(-5.71645369500006,11.6,9.63529951699999));
#236632=CARTESIAN_POINT('Ctrl Pts',(-5.71597884000006,15.2,9.63192764199999));
#236633=CARTESIAN_POINT('Ctrl Pts',(-5.71597884000006,11.6,9.63192764199999));
#236634=CARTESIAN_POINT('Ctrl Pts',(-5.71550200800006,15.2,9.62856096299999));
#236635=CARTESIAN_POINT('Ctrl Pts',(-5.71550200800006,11.6,9.62856096299999));
#236636=CARTESIAN_POINT('Ctrl Pts',(-5.71502320600006,15.2,9.62519948899999));
#236637=CARTESIAN_POINT('Ctrl Pts',(-5.71502320600006,11.6,9.62519948899999));
#236638=CARTESIAN_POINT('Ctrl Pts',(-5.71454244100006,15.2,9.62184322599999));
#236639=CARTESIAN_POINT('Ctrl Pts',(-5.71454244100006,11.6,9.62184322599999));
#236640=CARTESIAN_POINT('Ctrl Pts',(-5.71405972300006,15.2,9.61849218099999));
#236641=CARTESIAN_POINT('Ctrl Pts',(-5.71405972300006,11.6,9.61849218099999));
#236642=CARTESIAN_POINT('Ctrl Pts',(-5.71357505700006,15.2,9.61514635999999));
#236643=CARTESIAN_POINT('Ctrl Pts',(-5.71357505700006,11.6,9.61514635999999));
#236644=CARTESIAN_POINT('Ctrl Pts',(-5.71308845100006,15.2,9.61180577299999));
#236645=CARTESIAN_POINT('Ctrl Pts',(-5.71308845100006,11.6,9.61180577299999));
#236646=CARTESIAN_POINT('Ctrl Pts',(-5.71259991400006,15.2,9.60847042699999));
#236647=CARTESIAN_POINT('Ctrl Pts',(-5.71259991400006,11.6,9.60847042699999));
#236648=CARTESIAN_POINT('Ctrl Pts',(-5.71210945300006,15.2,9.60514032599999));
#236649=CARTESIAN_POINT('Ctrl Pts',(-5.71210945300006,11.6,9.60514032599999));
#236650=CARTESIAN_POINT('Ctrl Pts',(-5.71161707500006,15.2,9.60181547999999));
#236651=CARTESIAN_POINT('Ctrl Pts',(-5.71161707500006,11.6,9.60181547999999));
#236652=CARTESIAN_POINT('Ctrl Pts',(-5.71112278800006,15.2,9.59849589599998));
#236653=CARTESIAN_POINT('Ctrl Pts',(-5.71112278800006,11.6,9.59849589599998));
#236654=CARTESIAN_POINT('Ctrl Pts',(-5.71062660000006,15.2,9.59518157899998));
#236655=CARTESIAN_POINT('Ctrl Pts',(-5.71062660000006,11.6,9.59518157899998));
#236656=CARTESIAN_POINT('Ctrl Pts',(-5.71012851900006,15.2,9.59187253999998));
#236657=CARTESIAN_POINT('Ctrl Pts',(-5.71012851900006,11.6,9.59187253999998));
#236658=CARTESIAN_POINT('Ctrl Pts',(-5.70962855200006,15.2,9.58856878299999));
#236659=CARTESIAN_POINT('Ctrl Pts',(-5.70962855200006,11.6,9.58856878299999));
#236660=CARTESIAN_POINT('Ctrl Pts',(-5.70912670800006,15.2,9.58527031499998));
#236661=CARTESIAN_POINT('Ctrl Pts',(-5.70912670800006,11.6,9.58527031499998));
#236662=CARTESIAN_POINT('Ctrl Pts',(-5.70862299300006,15.2,9.58197714699999));
#236663=CARTESIAN_POINT('Ctrl Pts',(-5.70862299300006,11.6,9.58197714699999));
#236664=CARTESIAN_POINT('Ctrl Pts',(-5.70811741600005,15.2,9.57868928199998));
#236665=CARTESIAN_POINT('Ctrl Pts',(-5.70811741600005,11.6,9.57868928199998));
#236666=CARTESIAN_POINT('Ctrl Pts',(-5.70760998500006,15.2,9.57540672899999));
#236667=CARTESIAN_POINT('Ctrl Pts',(-5.70760998500006,11.6,9.57540672899999));
#236668=CARTESIAN_POINT('Ctrl Pts',(-5.70710070700006,15.2,9.57212949599998));
#236669=CARTESIAN_POINT('Ctrl Pts',(-5.70710070700006,11.6,9.57212949599998));
#236670=CARTESIAN_POINT('Ctrl Pts',(-5.70658959100006,15.2,9.56885758899999));
#236671=CARTESIAN_POINT('Ctrl Pts',(-5.70658959100006,11.6,9.56885758899999));
#236672=CARTESIAN_POINT('Ctrl Pts',(-5.70607664400006,15.2,9.56559101699998));
#236673=CARTESIAN_POINT('Ctrl Pts',(-5.70607664400006,11.6,9.56559101699998));
#236674=CARTESIAN_POINT('Ctrl Pts',(-5.70556187300006,15.2,9.56232978499998));
#236675=CARTESIAN_POINT('Ctrl Pts',(-5.70556187300006,11.6,9.56232978499998));
#236676=CARTESIAN_POINT('Ctrl Pts',(-5.70504528900006,15.2,9.55907390199998));
#236677=CARTESIAN_POINT('Ctrl Pts',(-5.70504528900006,11.6,9.55907390199998));
#236678=CARTESIAN_POINT('Ctrl Pts',(-5.70452689700006,15.2,9.55582337399999));
#236679=CARTESIAN_POINT('Ctrl Pts',(-5.70452689700006,11.6,9.55582337399999));
#236680=CARTESIAN_POINT('Ctrl Pts',(-5.70400670700006,15.2,9.55257820999999));
#236681=CARTESIAN_POINT('Ctrl Pts',(-5.70400670700006,11.6,9.55257820999999));
#236682=CARTESIAN_POINT('Ctrl Pts',(-5.70348472500006,15.2,9.54933841599999));
#236683=CARTESIAN_POINT('Ctrl Pts',(-5.70348472500006,11.6,9.54933841599999));
#236684=CARTESIAN_POINT('Ctrl Pts',(-5.70296096200006,15.2,9.54610399999999));
#236685=CARTESIAN_POINT('Ctrl Pts',(-5.70296096200006,11.6,9.54610399999999));
#236686=CARTESIAN_POINT('Ctrl Pts',(-5.70243542200005,15.2,9.54287496899998));
#236687=CARTESIAN_POINT('Ctrl Pts',(-5.70243542200005,11.6,9.54287496899998));
#236688=CARTESIAN_POINT('Ctrl Pts',(-5.70190811700006,15.2,9.53965132899998));
#236689=CARTESIAN_POINT('Ctrl Pts',(-5.70190811700006,11.6,9.53965132899998));
#236690=CARTESIAN_POINT('Ctrl Pts',(-5.70137905300006,15.2,9.53643308999998));
#236691=CARTESIAN_POINT('Ctrl Pts',(-5.70137905300006,11.6,9.53643308999998));
#236692=CARTESIAN_POINT('Ctrl Pts',(-5.70084823800006,15.2,9.53322025799999));
#236693=CARTESIAN_POINT('Ctrl Pts',(-5.70084823800006,11.6,9.53322025799999));
#236694=CARTESIAN_POINT('Ctrl Pts',(-5.70031568100006,15.2,9.53001284099999));
#236695=CARTESIAN_POINT('Ctrl Pts',(-5.70031568100006,11.6,9.53001284099999));
#236696=CARTESIAN_POINT('Ctrl Pts',(-5.69978139000006,15.2,9.52681084599998));
#236697=CARTESIAN_POINT('Ctrl Pts',(-5.69978139000006,11.6,9.52681084599998));
#236698=CARTESIAN_POINT('Ctrl Pts',(-5.69924537300006,15.2,9.52361427899999));
#236699=CARTESIAN_POINT('Ctrl Pts',(-5.69924537300006,11.6,9.52361427899999));
#236700=CARTESIAN_POINT('Ctrl Pts',(-5.69870763900005,15.2,9.52042314999998));
#236701=CARTESIAN_POINT('Ctrl Pts',(-5.69870763900005,11.6,9.52042314999998));
#236702=CARTESIAN_POINT('Ctrl Pts',(-5.69816819400006,15.2,9.51723746499999));
#236703=CARTESIAN_POINT('Ctrl Pts',(-5.69816819400006,11.6,9.51723746499999));
#236704=CARTESIAN_POINT('Ctrl Pts',(-5.69762704900006,15.2,9.51405723099998));
#236705=CARTESIAN_POINT('Ctrl Pts',(-5.69762704900006,11.6,9.51405723099998));
#236706=CARTESIAN_POINT('Ctrl Pts',(-5.69708421000006,15.2,9.51088245499999));
#236707=CARTESIAN_POINT('Ctrl Pts',(-5.69708421000006,11.6,9.51088245499999));
#236708=CARTESIAN_POINT('Ctrl Pts',(-5.69653968800006,15.2,9.50771314699999));
#236709=CARTESIAN_POINT('Ctrl Pts',(-5.69653968800006,11.6,9.50771314699999));
#236710=CARTESIAN_POINT('Ctrl Pts',(-5.69599348800006,15.2,9.50454931199998));
#236711=CARTESIAN_POINT('Ctrl Pts',(-5.69599348800006,11.6,9.50454931199998));
#236712=CARTESIAN_POINT('Ctrl Pts',(-5.69544562100006,15.2,9.50139095799998));
#236713=CARTESIAN_POINT('Ctrl Pts',(-5.69544562100006,11.6,9.50139095799998));
#236714=CARTESIAN_POINT('Ctrl Pts',(-5.69489609500006,15.2,9.49823809399999));
#236715=CARTESIAN_POINT('Ctrl Pts',(-5.69489609500006,11.6,9.49823809399999));
#236716=CARTESIAN_POINT('Ctrl Pts',(-5.69434491600005,15.2,9.49509072499998));
#236717=CARTESIAN_POINT('Ctrl Pts',(-5.69434491600005,11.6,9.49509072499998));
#236718=CARTESIAN_POINT('Ctrl Pts',(-5.69379209600006,15.2,9.49194885999999));
#236719=CARTESIAN_POINT('Ctrl Pts',(-5.69379209600006,11.6,9.49194885999999));
#236720=CARTESIAN_POINT('Ctrl Pts',(-5.69323764100006,15.2,9.48881250699999));
#236721=CARTESIAN_POINT('Ctrl Pts',(-5.69323764100006,11.6,9.48881250699999));
#236722=CARTESIAN_POINT('Ctrl Pts',(-5.69268155900006,15.2,9.48568167099998));
#236723=CARTESIAN_POINT('Ctrl Pts',(-5.69268155900006,11.6,9.48568167099998));
#236724=CARTESIAN_POINT('Ctrl Pts',(-5.69212386100006,15.2,9.48255636199999));
#236725=CARTESIAN_POINT('Ctrl Pts',(-5.69212386100006,11.6,9.48255636199999));
#236726=CARTESIAN_POINT('Ctrl Pts',(-5.69156455400006,15.2,9.47943658699998));
#236727=CARTESIAN_POINT('Ctrl Pts',(-5.69156455400006,11.6,9.47943658699998));
#236728=CARTESIAN_POINT('Ctrl Pts',(-5.69100364700006,15.2,9.47632235299999));
#236729=CARTESIAN_POINT('Ctrl Pts',(-5.69100364700006,11.6,9.47632235299999));
#236730=CARTESIAN_POINT('Ctrl Pts',(-5.69044114800006,15.2,9.47321366899999));
#236731=CARTESIAN_POINT('Ctrl Pts',(-5.69044114800006,11.6,9.47321366899999));
#236732=CARTESIAN_POINT('Ctrl Pts',(-5.68987706600006,15.2,9.47011053899999));
#236733=CARTESIAN_POINT('Ctrl Pts',(-5.68987706600006,11.6,9.47011053899999));
#236734=CARTESIAN_POINT('Ctrl Pts',(-5.68931140900006,15.2,9.46701297399999));
#236735=CARTESIAN_POINT('Ctrl Pts',(-5.68931140900006,11.6,9.46701297399999));
#236736=CARTESIAN_POINT('Ctrl Pts',(-5.68874418700006,15.2,9.46392098099999));
#236737=CARTESIAN_POINT('Ctrl Pts',(-5.68874418700006,11.6,9.46392098099999));
#236738=CARTESIAN_POINT('Ctrl Pts',(-5.68817540700006,15.2,9.46083456599998));
#236739=CARTESIAN_POINT('Ctrl Pts',(-5.68817540700006,11.6,9.46083456599998));
#236740=CARTESIAN_POINT('Ctrl Pts',(-5.68760507800006,15.2,9.45775373799999));
#236741=CARTESIAN_POINT('Ctrl Pts',(-5.68760507800006,11.6,9.45775373799999));
#236742=CARTESIAN_POINT('Ctrl Pts',(-5.68703321000006,15.2,9.45467850399999));
#236743=CARTESIAN_POINT('Ctrl Pts',(-5.68703321000006,11.6,9.45467850399999));
#236744=CARTESIAN_POINT('Ctrl Pts',(-5.68645981100006,15.2,9.45160887199999));
#236745=CARTESIAN_POINT('Ctrl Pts',(-5.68645981100006,11.6,9.45160887199999));
#236746=CARTESIAN_POINT('Ctrl Pts',(-5.68588489000006,15.2,9.44854484899999));
#236747=CARTESIAN_POINT('Ctrl Pts',(-5.68588489000006,11.6,9.44854484899999));
#236748=CARTESIAN_POINT('Ctrl Pts',(-5.68530845500006,15.2,9.44548644399998));
#236749=CARTESIAN_POINT('Ctrl Pts',(-5.68530845500006,11.6,9.44548644399998));
#236750=CARTESIAN_POINT('Ctrl Pts',(-5.68473051600006,15.2,9.44243366199998));
#236751=CARTESIAN_POINT('Ctrl Pts',(-5.68473051600006,11.6,9.44243366199998));
#236752=CARTESIAN_POINT('Ctrl Pts',(-5.68415108000006,15.2,9.43938651299998));
#236753=CARTESIAN_POINT('Ctrl Pts',(-5.68415108000006,11.6,9.43938651299998));
#236754=CARTESIAN_POINT('Ctrl Pts',(-5.68357015700006,15.2,9.43634500399998));
#236755=CARTESIAN_POINT('Ctrl Pts',(-5.68357015700006,11.6,9.43634500399998));
#236756=CARTESIAN_POINT('Ctrl Pts',(-5.68298775600006,15.2,9.43330914299998));
#236757=CARTESIAN_POINT('Ctrl Pts',(-5.68298775600006,11.6,9.43330914299998));
#236758=CARTESIAN_POINT('Ctrl Pts',(-5.68240388700006,15.2,9.43027893699998));
#236759=CARTESIAN_POINT('Ctrl Pts',(-5.68240388700006,11.6,9.43027893699998));
#236760=CARTESIAN_POINT('Ctrl Pts',(-5.68181855600006,15.2,9.42725439299998));
#236761=CARTESIAN_POINT('Ctrl Pts',(-5.68181855600006,11.6,9.42725439299998));
#236762=CARTESIAN_POINT('Ctrl Pts',(-5.68123177500006,15.2,9.42423552099999));
#236763=CARTESIAN_POINT('Ctrl Pts',(-5.68123177500006,11.6,9.42423552099999));
#236764=CARTESIAN_POINT('Ctrl Pts',(-5.68064355000006,15.2,9.42122232699998));
#236765=CARTESIAN_POINT('Ctrl Pts',(-5.68064355000006,11.6,9.42122232699998));
#236766=CARTESIAN_POINT('Ctrl Pts',(-5.68005389300006,15.2,9.41821481799998));
#236767=CARTESIAN_POINT('Ctrl Pts',(-5.68005389300006,11.6,9.41821481799998));
#236768=CARTESIAN_POINT('Ctrl Pts',(-5.67946281200006,15.2,9.41521300399998));
#236769=CARTESIAN_POINT('Ctrl Pts',(-5.67946281200006,11.6,9.41521300399998));
#236770=CARTESIAN_POINT('Ctrl Pts',(-5.67887031500006,15.2,9.41221689099999));
#236771=CARTESIAN_POINT('Ctrl Pts',(-5.67887031500006,11.6,9.41221689099999));
#236772=CARTESIAN_POINT('Ctrl Pts',(-5.67827641300005,15.2,9.40922648699999));
#236773=CARTESIAN_POINT('Ctrl Pts',(-5.67827641300005,11.6,9.40922648699999));
#236774=CARTESIAN_POINT('Ctrl Pts',(-5.67768111200006,15.2,9.40624179999999));
#236775=CARTESIAN_POINT('Ctrl Pts',(-5.67768111200006,11.6,9.40624179999999));
#236776=CARTESIAN_POINT('Ctrl Pts',(-5.67708442500006,15.2,9.40326283799998));
#236777=CARTESIAN_POINT('Ctrl Pts',(-5.67708442500006,11.6,9.40326283799998));
#236778=CARTESIAN_POINT('Ctrl Pts',(-5.67648635800006,15.2,9.40028960799999));
#236779=CARTESIAN_POINT('Ctrl Pts',(-5.67648635800006,11.6,9.40028960799999));
#236780=CARTESIAN_POINT('Ctrl Pts',(-5.67588692200006,15.2,9.39732211899998));
#236781=CARTESIAN_POINT('Ctrl Pts',(-5.67588692200006,11.6,9.39732211899998));
#236782=CARTESIAN_POINT('Ctrl Pts',(-5.67528612600006,15.2,9.39436037699998));
#236783=CARTESIAN_POINT('Ctrl Pts',(-5.67528612600006,11.6,9.39436037699998));
#236784=CARTESIAN_POINT('Ctrl Pts',(-5.67468397900006,15.2,9.39140439199999));
#236785=CARTESIAN_POINT('Ctrl Pts',(-5.67468397900006,11.6,9.39140439199999));
#236786=CARTESIAN_POINT('Ctrl Pts',(-5.67408048900006,15.2,9.38845416899999));
#236787=CARTESIAN_POINT('Ctrl Pts',(-5.67408048900006,11.6,9.38845416899999));
#236788=CARTESIAN_POINT('Ctrl Pts',(-5.67347566800006,15.2,9.38550971899998));
#236789=CARTESIAN_POINT('Ctrl Pts',(-5.67347566800006,11.6,9.38550971899998));
#236790=CARTESIAN_POINT('Ctrl Pts',(-5.67286952300006,15.2,9.38257104699998));
#236791=CARTESIAN_POINT('Ctrl Pts',(-5.67286952300006,11.6,9.38257104699998));
#236792=CARTESIAN_POINT('Ctrl Pts',(-5.67226206500006,15.2,9.37963816299998));
#236793=CARTESIAN_POINT('Ctrl Pts',(-5.67226206500006,11.6,9.37963816299998));
#236794=CARTESIAN_POINT('Ctrl Pts',(-5.67165330200006,15.2,9.37671107499998));
#236795=CARTESIAN_POINT('Ctrl Pts',(-5.67165330200006,11.6,9.37671107499998));
#236796=CARTESIAN_POINT('Ctrl Pts',(-5.67104324500006,15.2,9.37378978899999));
#236797=CARTESIAN_POINT('Ctrl Pts',(-5.67104324500006,11.6,9.37378978899999));
#236798=CARTESIAN_POINT('Ctrl Pts',(-5.67043190200006,15.2,9.37087431299998));
#236799=CARTESIAN_POINT('Ctrl Pts',(-5.67043190200006,11.6,9.37087431299998));
#236800=CARTESIAN_POINT('Ctrl Pts',(-5.66981928200006,15.2,9.36796465599999));
#236801=CARTESIAN_POINT('Ctrl Pts',(-5.66981928200006,11.6,9.36796465599999));
#236802=CARTESIAN_POINT('Ctrl Pts',(-5.66920539700006,15.2,9.36506082599998));
#236803=CARTESIAN_POINT('Ctrl Pts',(-5.66920539700006,11.6,9.36506082599998));
#236804=CARTESIAN_POINT('Ctrl Pts',(-5.66859025400006,15.2,9.36216282899998));
#236805=CARTESIAN_POINT('Ctrl Pts',(-5.66859025400006,11.6,9.36216282899998));
#236806=CARTESIAN_POINT('Ctrl Pts',(-5.66797386300006,15.2,9.35927067599999));
#236807=CARTESIAN_POINT('Ctrl Pts',(-5.66797386300006,11.6,9.35927067599999));
#236808=CARTESIAN_POINT('Ctrl Pts',(-5.66735623500006,15.2,9.35638437199999));
#236809=CARTESIAN_POINT('Ctrl Pts',(-5.66735623500006,11.6,9.35638437199999));
#236810=CARTESIAN_POINT('Ctrl Pts',(-5.66673737800006,15.2,9.35350392799998));
#236811=CARTESIAN_POINT('Ctrl Pts',(-5.66673737800006,11.6,9.35350392799998));
#236812=CARTESIAN_POINT('Ctrl Pts',(-5.66611730300006,15.2,9.35062934799999));
#236813=CARTESIAN_POINT('Ctrl Pts',(-5.66611730300006,11.6,9.35062934799999));
#236814=CARTESIAN_POINT('Ctrl Pts',(-5.66549601900006,15.2,9.34776064299999));
#236815=CARTESIAN_POINT('Ctrl Pts',(-5.66549601900006,11.6,9.34776064299999));
#236816=CARTESIAN_POINT('Ctrl Pts',(-5.66487353500006,15.2,9.34489782099998));
#236817=CARTESIAN_POINT('Ctrl Pts',(-5.66487353500006,11.6,9.34489782099998));
#236818=CARTESIAN_POINT('Ctrl Pts',(-5.66424986200006,15.2,9.34204088699998));
#236819=CARTESIAN_POINT('Ctrl Pts',(-5.66424986200006,11.6,9.34204088699998));
#236820=CARTESIAN_POINT('Ctrl Pts',(-5.66362500900006,15.2,9.33918985199998));
#236821=CARTESIAN_POINT('Ctrl Pts',(-5.66362500900006,11.6,9.33918985199998));
#236822=CARTESIAN_POINT('Ctrl Pts',(-5.66299898600006,15.2,9.33634472299998));
#236823=CARTESIAN_POINT('Ctrl Pts',(-5.66299898600006,11.6,9.33634472299998));
#236824=CARTESIAN_POINT('Ctrl Pts',(-5.66237180200006,15.2,9.33350550899998));
#236825=CARTESIAN_POINT('Ctrl Pts',(-5.66237180200006,11.6,9.33350550899998));
#236826=CARTESIAN_POINT('Ctrl Pts',(-5.66174346800006,15.2,9.33067221699999));
#236827=CARTESIAN_POINT('Ctrl Pts',(-5.66174346800006,11.6,9.33067221699999));
#236828=CARTESIAN_POINT('Ctrl Pts',(-5.66111399400006,15.2,9.32784485499998));
#236829=CARTESIAN_POINT('Ctrl Pts',(-5.66111399400006,11.6,9.32784485499998));
#236830=CARTESIAN_POINT('Ctrl Pts',(-5.66048338800006,15.2,9.32502342999998));
#236831=CARTESIAN_POINT('Ctrl Pts',(-5.66048338800006,11.6,9.32502342999998));
#236832=CARTESIAN_POINT('Ctrl Pts',(-5.65985166300006,15.2,9.32220795299998));
#236833=CARTESIAN_POINT('Ctrl Pts',(-5.65985166300006,11.6,9.32220795299998));
#236834=CARTESIAN_POINT('Ctrl Pts',(-5.65921882600006,15.2,9.31939842899999));
#236835=CARTESIAN_POINT('Ctrl Pts',(-5.65921882600006,11.6,9.31939842899999));
#236836=CARTESIAN_POINT('Ctrl Pts',(-5.65858488900005,15.2,9.31659486699999));
#236837=CARTESIAN_POINT('Ctrl Pts',(-5.65858488900005,11.6,9.31659486699999));
#236838=CARTESIAN_POINT('Ctrl Pts',(-5.65794986000006,15.2,9.31379727699999));
#236839=CARTESIAN_POINT('Ctrl Pts',(-5.65794986000006,11.6,9.31379727699999));
#236840=CARTESIAN_POINT('Ctrl Pts',(-5.65731375200006,15.2,9.31100566499998));
#236841=CARTESIAN_POINT('Ctrl Pts',(-5.65731375200006,11.6,9.31100566499998));
#236842=CARTESIAN_POINT('Ctrl Pts',(-5.65667657200006,15.2,9.30822003899999));
#236843=CARTESIAN_POINT('Ctrl Pts',(-5.65667657200006,11.6,9.30822003899999));
#236844=CARTESIAN_POINT('Ctrl Pts',(-5.65603833200006,15.2,9.30544040799998));
#236845=CARTESIAN_POINT('Ctrl Pts',(-5.65603833200006,11.6,9.30544040799998));
#236846=CARTESIAN_POINT('Ctrl Pts',(-5.65539904000006,15.2,9.30266678099999));
#236847=CARTESIAN_POINT('Ctrl Pts',(-5.65539904000006,11.6,9.30266678099999));
#236848=CARTESIAN_POINT('Ctrl Pts',(-5.65475870900006,15.2,9.29989916499999));
#236849=CARTESIAN_POINT('Ctrl Pts',(-5.65475870900006,11.6,9.29989916499999));
#236850=CARTESIAN_POINT('Ctrl Pts',(-5.65411734800006,15.2,9.29713756699999));
#236851=CARTESIAN_POINT('Ctrl Pts',(-5.65411734800006,11.6,9.29713756699999));
#236852=CARTESIAN_POINT('Ctrl Pts',(-5.65347496700006,15.2,9.29438199899998));
#236853=CARTESIAN_POINT('Ctrl Pts',(-5.65347496700006,11.6,9.29438199899998));
#236854=CARTESIAN_POINT('Ctrl Pts',(-5.65283157700006,15.2,9.29163246499999));
#236855=CARTESIAN_POINT('Ctrl Pts',(-5.65283157700006,11.6,9.29163246499999));
#236856=CARTESIAN_POINT('Ctrl Pts',(-5.65218718700006,15.2,9.28888897499998));
#236857=CARTESIAN_POINT('Ctrl Pts',(-5.65218718700006,11.6,9.28888897499998));
#236858=CARTESIAN_POINT('Ctrl Pts',(-5.65154180700006,15.2,9.28615153699998));
#236859=CARTESIAN_POINT('Ctrl Pts',(-5.65154180700006,11.6,9.28615153699998));
#236860=CARTESIAN_POINT('Ctrl Pts',(-5.65089545000006,15.2,9.28342015999998));
#236861=CARTESIAN_POINT('Ctrl Pts',(-5.65089545000006,11.6,9.28342015999998));
#236862=CARTESIAN_POINT('Ctrl Pts',(-5.65024812400006,15.2,9.28069485099999));
#236863=CARTESIAN_POINT('Ctrl Pts',(-5.65024812400006,11.6,9.28069485099999));
#236864=CARTESIAN_POINT('Ctrl Pts',(-5.64959984100006,15.2,9.27797561899999));
#236865=CARTESIAN_POINT('Ctrl Pts',(-5.64959984100006,11.6,9.27797561899999));
#236866=CARTESIAN_POINT('Ctrl Pts',(-5.64895061000006,15.2,9.27526247199999));
#236867=CARTESIAN_POINT('Ctrl Pts',(-5.64895061000006,11.6,9.27526247199999));
#236868=CARTESIAN_POINT('Ctrl Pts',(-5.64830044100006,15.2,9.27255541899999));
#236869=CARTESIAN_POINT('Ctrl Pts',(-5.64830044100006,11.6,9.27255541899999));
#236870=CARTESIAN_POINT('Ctrl Pts',(-5.64764934600006,15.2,9.26985446699998));
#236871=CARTESIAN_POINT('Ctrl Pts',(-5.64764934600006,11.6,9.26985446699998));
#236872=CARTESIAN_POINT('Ctrl Pts',(-5.64699733600006,15.2,9.26715962499999));
#236873=CARTESIAN_POINT('Ctrl Pts',(-5.64699733600006,11.6,9.26715962499999));
#236874=CARTESIAN_POINT('Ctrl Pts',(-5.64634442000005,15.2,9.26447090199999));
#236875=CARTESIAN_POINT('Ctrl Pts',(-5.64634442000005,11.6,9.26447090199999));
#236876=CARTESIAN_POINT('Ctrl Pts',(-5.64569060900006,15.2,9.26178830599999));
#236877=CARTESIAN_POINT('Ctrl Pts',(-5.64569060900006,11.6,9.26178830599999));
#236878=CARTESIAN_POINT('Ctrl Pts',(-5.64503591600006,15.2,9.25911184399999));
#236879=CARTESIAN_POINT('Ctrl Pts',(-5.64503591600006,11.6,9.25911184399999));
#236880=CARTESIAN_POINT('Ctrl Pts',(-5.64438034700006,15.2,9.25644152499999));
#236881=CARTESIAN_POINT('Ctrl Pts',(-5.64438034700006,11.6,9.25644152499999));
#236882=CARTESIAN_POINT('Ctrl Pts',(-5.64372391600005,15.2,9.25377735799999));
#236883=CARTESIAN_POINT('Ctrl Pts',(-5.64372391600005,11.6,9.25377735799999));
#236884=CARTESIAN_POINT('Ctrl Pts',(-5.64306663300005,15.2,9.25111935199999));
#236885=CARTESIAN_POINT('Ctrl Pts',(-5.64306663300005,11.6,9.25111935199999));
#236886=CARTESIAN_POINT('Ctrl Pts',(-5.64240850900006,15.2,9.24846751399999));
#236887=CARTESIAN_POINT('Ctrl Pts',(-5.64240850900006,11.6,9.24846751399999));
#236888=CARTESIAN_POINT('Ctrl Pts',(-5.64174955500006,15.2,9.24582185199998));
#236889=CARTESIAN_POINT('Ctrl Pts',(-5.64174955500006,11.6,9.24582185199998));
#236890=CARTESIAN_POINT('Ctrl Pts',(-5.64108978100006,15.2,9.24318237599999));
#236891=CARTESIAN_POINT('Ctrl Pts',(-5.64108978100006,11.6,9.24318237599999));
#236892=CARTESIAN_POINT('Ctrl Pts',(-5.64042919800006,15.2,9.24054909399998));
#236893=CARTESIAN_POINT('Ctrl Pts',(-5.64042919800006,11.6,9.24054909399998));
#236894=CARTESIAN_POINT('Ctrl Pts',(-5.63976781800006,15.2,9.23792201399999));
#236895=CARTESIAN_POINT('Ctrl Pts',(-5.63976781800006,11.6,9.23792201399999));
#236896=CARTESIAN_POINT('Ctrl Pts',(-5.63910565000006,15.2,9.23530114499999));
#236897=CARTESIAN_POINT('Ctrl Pts',(-5.63910565000006,11.6,9.23530114499999));
#236898=CARTESIAN_POINT('Ctrl Pts',(-5.63844270700006,15.2,9.23268649399999));
#236899=CARTESIAN_POINT('Ctrl Pts',(-5.63844270700006,11.6,9.23268649399999));
#236900=CARTESIAN_POINT('Ctrl Pts',(-5.63777899900006,15.2,9.23007807199999));
#236901=CARTESIAN_POINT('Ctrl Pts',(-5.63777899900006,11.6,9.23007807199999));
#236902=CARTESIAN_POINT('Ctrl Pts',(-5.63711453700006,15.2,9.22747588499998));
#236903=CARTESIAN_POINT('Ctrl Pts',(-5.63711453700006,11.6,9.22747588499998));
#236904=CARTESIAN_POINT('Ctrl Pts',(-5.63644933200006,15.2,9.22487994299999));
#236905=CARTESIAN_POINT('Ctrl Pts',(-5.63644933200006,11.6,9.22487994299999));
#236906=CARTESIAN_POINT('Ctrl Pts',(-5.63578339500006,15.2,9.22229025499998));
#236907=CARTESIAN_POINT('Ctrl Pts',(-5.63578339500006,11.6,9.22229025499998));
#236908=CARTESIAN_POINT('Ctrl Pts',(-5.63511673800006,15.2,9.21970682799999));
#236909=CARTESIAN_POINT('Ctrl Pts',(-5.63511673800006,11.6,9.21970682799999));
#236910=CARTESIAN_POINT('Ctrl Pts',(-5.63444937200006,15.2,9.21712967099998));
#236911=CARTESIAN_POINT('Ctrl Pts',(-5.63444937200006,11.6,9.21712967099998));
#236912=CARTESIAN_POINT('Ctrl Pts',(-5.63378130700006,15.2,9.21455879299998));
#236913=CARTESIAN_POINT('Ctrl Pts',(-5.63378130700006,11.6,9.21455879299998));
#236914=CARTESIAN_POINT('Ctrl Pts',(-5.63311255600006,15.2,9.21199420299999));
#236915=CARTESIAN_POINT('Ctrl Pts',(-5.63311255600006,11.6,9.21199420299999));
#236916=CARTESIAN_POINT('Ctrl Pts',(-5.63244312900006,15.2,9.20943590799999));
#236917=CARTESIAN_POINT('Ctrl Pts',(-5.63244312900006,11.6,9.20943590799999));
#236918=CARTESIAN_POINT('Ctrl Pts',(-5.63177303700006,15.2,9.20688391799998));
#236919=CARTESIAN_POINT('Ctrl Pts',(-5.63177303700006,11.6,9.20688391799998));
#236920=CARTESIAN_POINT('Ctrl Pts',(-5.63110229300006,15.2,9.20433824199998));
#236921=CARTESIAN_POINT('Ctrl Pts',(-5.63110229300006,11.6,9.20433824199998));
#236922=CARTESIAN_POINT('Ctrl Pts',(-5.63043090700006,15.2,9.20179888799998));
#236923=CARTESIAN_POINT('Ctrl Pts',(-5.63043090700006,11.6,9.20179888799998));
#236924=CARTESIAN_POINT('Ctrl Pts',(-5.62975889100006,15.2,9.19926586199999));
#236925=CARTESIAN_POINT('Ctrl Pts',(-5.62975889100006,11.6,9.19926586199999));
#236926=CARTESIAN_POINT('Ctrl Pts',(-5.62908625600006,15.2,9.19673917799999));
#236927=CARTESIAN_POINT('Ctrl Pts',(-5.62908625600006,11.6,9.19673917799999));
#236928=CARTESIAN_POINT('Ctrl Pts',(-5.62841301500006,15.2,9.19421884099999));
#236929=CARTESIAN_POINT('Ctrl Pts',(-5.62841301500006,11.6,9.19421884099999));
#236930=CARTESIAN_POINT('Ctrl Pts',(-5.62773917800006,15.2,9.19170486099999));
#236931=CARTESIAN_POINT('Ctrl Pts',(-5.62773917800006,11.6,9.19170486099999));
#236932=CARTESIAN_POINT('Ctrl Pts',(-5.62706475600006,15.2,9.18919724599998));
#236933=CARTESIAN_POINT('Ctrl Pts',(-5.62706475600006,11.6,9.18919724599998));
#236934=CARTESIAN_POINT('Ctrl Pts',(-5.62638976200006,15.2,9.18669600399999));
#236935=CARTESIAN_POINT('Ctrl Pts',(-5.62638976200006,11.6,9.18669600399999));
#236936=CARTESIAN_POINT('Ctrl Pts',(-5.62571420700006,15.2,9.18420114599999));
#236937=CARTESIAN_POINT('Ctrl Pts',(-5.62571420700006,11.6,9.18420114599999));
#236938=CARTESIAN_POINT('Ctrl Pts',(-5.62503810400006,15.2,9.18171267899999));
#236939=CARTESIAN_POINT('Ctrl Pts',(-5.62503810400006,11.6,9.18171267899999));
#236940=CARTESIAN_POINT('Ctrl Pts',(-5.62436146300006,15.2,9.17923061299999));
#236941=CARTESIAN_POINT('Ctrl Pts',(-5.62436146300006,11.6,9.17923061299999));
#236942=CARTESIAN_POINT('Ctrl Pts',(-5.62368429600006,15.2,9.17675495599998));
#236943=CARTESIAN_POINT('Ctrl Pts',(-5.62368429600006,11.6,9.17675495599998));
#236944=CARTESIAN_POINT('Ctrl Pts',(-5.62300661500006,15.2,9.17428571699999));
#236945=CARTESIAN_POINT('Ctrl Pts',(-5.62300661500006,11.6,9.17428571699999));
#236946=CARTESIAN_POINT('Ctrl Pts',(-5.62232843300006,15.2,9.17182290399998));
#236947=CARTESIAN_POINT('Ctrl Pts',(-5.62232843300006,11.6,9.17182290399998));
#236948=CARTESIAN_POINT('Ctrl Pts',(-5.62164976000005,15.2,9.16936652699999));
#236949=CARTESIAN_POINT('Ctrl Pts',(-5.62164976000005,11.6,9.16936652699999));
#236950=CARTESIAN_POINT('Ctrl Pts',(-5.62097061000006,15.2,9.16691659399999));
#236951=CARTESIAN_POINT('Ctrl Pts',(-5.62097061000006,11.6,9.16691659399999));
#236952=CARTESIAN_POINT('Ctrl Pts',(-5.62029099200006,15.2,9.16447311499999));
#236953=CARTESIAN_POINT('Ctrl Pts',(-5.62029099200006,11.6,9.16447311499999));
#236954=CARTESIAN_POINT('Ctrl Pts',(-5.61961092000006,15.2,9.16203609799998));
#236955=CARTESIAN_POINT('Ctrl Pts',(-5.61961092000006,11.6,9.16203609799998));
#236956=CARTESIAN_POINT('Ctrl Pts',(-5.61893040700006,15.2,9.15960555299998));
#236957=CARTESIAN_POINT('Ctrl Pts',(-5.61893040700006,11.6,9.15960555299998));
#236958=CARTESIAN_POINT('Ctrl Pts',(-5.61824946300006,15.2,9.15718148599998));
#236959=CARTESIAN_POINT('Ctrl Pts',(-5.61824946300006,11.6,9.15718148599998));
#236960=CARTESIAN_POINT('Ctrl Pts',(-5.61756810100006,15.2,9.15476390999999));
#236961=CARTESIAN_POINT('Ctrl Pts',(-5.61756810100006,11.6,9.15476390999999));
#236962=CARTESIAN_POINT('Ctrl Pts',(-5.61688633400006,15.2,9.15235282999999));
#236963=CARTESIAN_POINT('Ctrl Pts',(-5.61688633400006,11.6,9.15235282999999));
#236964=CARTESIAN_POINT('Ctrl Pts',(-5.61620417200006,15.2,9.14994825799998));
#236965=CARTESIAN_POINT('Ctrl Pts',(-5.61620417200006,11.6,9.14994825799998));
#236966=CARTESIAN_POINT('Ctrl Pts',(-5.61552163000006,15.2,9.14755020199999));
#236967=CARTESIAN_POINT('Ctrl Pts',(-5.61552163000006,11.6,9.14755020199999));
#236968=CARTESIAN_POINT('Ctrl Pts',(-5.61483871800006,15.2,9.14515866899999));
#236969=CARTESIAN_POINT('Ctrl Pts',(-5.61483871800006,11.6,9.14515866899999));
#236970=CARTESIAN_POINT('Ctrl Pts',(-5.61415544800006,15.2,9.14277367099999));
#236971=CARTESIAN_POINT('Ctrl Pts',(-5.61415544800006,11.6,9.14277367099999));
#236972=CARTESIAN_POINT('Ctrl Pts',(-5.61347183500006,15.2,9.14039521599998));
#236973=CARTESIAN_POINT('Ctrl Pts',(-5.61347183500006,11.6,9.14039521599998));
#236974=CARTESIAN_POINT('Ctrl Pts',(-5.61278788900006,15.2,9.13802331199999));
#236975=CARTESIAN_POINT('Ctrl Pts',(-5.61278788900006,11.6,9.13802331199999));
#236976=CARTESIAN_POINT('Ctrl Pts',(-5.61210362400006,15.2,9.13565796999999));
#236977=CARTESIAN_POINT('Ctrl Pts',(-5.61210362400006,11.6,9.13565796999999));
#236978=CARTESIAN_POINT('Ctrl Pts',(-5.61141905000006,15.2,9.13329919799999));
#236979=CARTESIAN_POINT('Ctrl Pts',(-5.61141905000006,11.6,9.13329919799999));
#236980=CARTESIAN_POINT('Ctrl Pts',(-5.61073418300006,15.2,9.13094700499999));
#236981=CARTESIAN_POINT('Ctrl Pts',(-5.61073418300006,11.6,9.13094700499999));
#236982=CARTESIAN_POINT('Ctrl Pts',(-5.61004903300006,15.2,9.12860139899998));
#236983=CARTESIAN_POINT('Ctrl Pts',(-5.61004903300006,11.6,9.12860139899998));
#236984=CARTESIAN_POINT('Ctrl Pts',(-5.60936361400006,15.2,9.12626239199999));
#236985=CARTESIAN_POINT('Ctrl Pts',(-5.60936361400006,11.6,9.12626239199999));
#236986=CARTESIAN_POINT('Ctrl Pts',(-5.60867793700006,15.2,9.12392998999999));
#236987=CARTESIAN_POINT('Ctrl Pts',(-5.60867793700006,11.6,9.12392998999999));
#236988=CARTESIAN_POINT('Ctrl Pts',(-5.60799201700006,15.2,9.12160420499998));
#236989=CARTESIAN_POINT('Ctrl Pts',(-5.60799201700006,11.6,9.12160420499998));
#236990=CARTESIAN_POINT('Ctrl Pts',(-5.60730586500005,15.2,9.11928504299999));
#236991=CARTESIAN_POINT('Ctrl Pts',(-5.60730586500005,11.6,9.11928504299999));
#236992=CARTESIAN_POINT('Ctrl Pts',(-5.60661949400005,15.2,9.11697251599998));
#236993=CARTESIAN_POINT('Ctrl Pts',(-5.60661949400005,11.6,9.11697251599998));
#236994=CARTESIAN_POINT('Ctrl Pts',(-5.60593291600005,15.2,9.11466663299999));
#236995=CARTESIAN_POINT('Ctrl Pts',(-5.60593291600005,11.6,9.11466663299999));
#236996=CARTESIAN_POINT('Ctrl Pts',(-5.60524614600006,15.2,9.11236740199998));
#236997=CARTESIAN_POINT('Ctrl Pts',(-5.60524614600006,11.6,9.11236740199998));
#236998=CARTESIAN_POINT('Ctrl Pts',(-5.60455919600006,15.2,9.11007483299999));
#236999=CARTESIAN_POINT('Ctrl Pts',(-5.60455919600006,11.6,9.11007483299999));
#237000=CARTESIAN_POINT('Ctrl Pts',(-5.60387207800006,15.2,9.10778893299998));
#237001=CARTESIAN_POINT('Ctrl Pts',(-5.60387207800006,11.6,9.10778893299998));
#237002=CARTESIAN_POINT('Ctrl Pts',(-5.60318480600006,15.2,9.10550971499998));
#237003=CARTESIAN_POINT('Ctrl Pts',(-5.60318480600006,11.6,9.10550971499998));
#237004=CARTESIAN_POINT('Ctrl Pts',(-5.60249739200006,15.2,9.10323718699999));
#237005=CARTESIAN_POINT('Ctrl Pts',(-5.60249739200006,11.6,9.10323718699999));
#237006=CARTESIAN_POINT('Ctrl Pts',(-5.60180985100006,15.2,9.10097135599998));
#237007=CARTESIAN_POINT('Ctrl Pts',(-5.60180985100006,11.6,9.10097135599998));
#237008=CARTESIAN_POINT('Ctrl Pts',(-5.60112219400006,15.2,9.09871223399998));
#237009=CARTESIAN_POINT('Ctrl Pts',(-5.60112219400006,11.6,9.09871223399998));
#237010=CARTESIAN_POINT('Ctrl Pts',(-5.60043443500006,15.2,9.09645982999999));
#237011=CARTESIAN_POINT('Ctrl Pts',(-5.60043443500006,11.6,9.09645982999999));
#237012=CARTESIAN_POINT('Ctrl Pts',(-5.59974658800006,15.2,9.09421415199999));
#237013=CARTESIAN_POINT('Ctrl Pts',(-5.59974658800006,11.6,9.09421415199999));
#237014=CARTESIAN_POINT('Ctrl Pts',(-5.59905866400006,15.2,9.09197521199999));
#237015=CARTESIAN_POINT('Ctrl Pts',(-5.59905866400006,11.6,9.09197521199999));
#237016=CARTESIAN_POINT('Ctrl Pts',(-5.59837067900006,15.2,9.08974301499999));
#237017=CARTESIAN_POINT('Ctrl Pts',(-5.59837067900006,11.6,9.08974301499999));
#237018=CARTESIAN_POINT('Ctrl Pts',(-5.59768264500006,15.2,9.08751757599998));
#237019=CARTESIAN_POINT('Ctrl Pts',(-5.59768264500006,11.6,9.08751757599998));
#237020=CARTESIAN_POINT('Ctrl Pts',(-5.59699457500006,15.2,9.08529889999999));
#237021=CARTESIAN_POINT('Ctrl Pts',(-5.59699457500006,11.6,9.08529889999999));
#237022=CARTESIAN_POINT('Ctrl Pts',(-5.59630648300006,15.2,9.08308699799999));
#237023=CARTESIAN_POINT('Ctrl Pts',(-5.59630648300006,11.6,9.08308699799999));
#237024=CARTESIAN_POINT('Ctrl Pts',(-5.59561838300006,15.2,9.08088187899999));
#237025=CARTESIAN_POINT('Ctrl Pts',(-5.59561838300006,11.6,9.08088187899999));
#237026=CARTESIAN_POINT('Ctrl Pts',(-5.59493028800006,15.2,9.07868355399999));
#237027=CARTESIAN_POINT('Ctrl Pts',(-5.59493028800006,11.6,9.07868355399999));
#237028=CARTESIAN_POINT('Ctrl Pts',(-5.59424221100006,15.2,9.07649203199998));
#237029=CARTESIAN_POINT('Ctrl Pts',(-5.59424221100006,11.6,9.07649203199998));
#237030=CARTESIAN_POINT('Ctrl Pts',(-5.59355416600006,15.2,9.07430732199998));
#237031=CARTESIAN_POINT('Ctrl Pts',(-5.59355416600006,11.6,9.07430732199998));
#237032=CARTESIAN_POINT('Ctrl Pts',(-5.59286616700006,15.2,9.07212943299999));
#237033=CARTESIAN_POINT('Ctrl Pts',(-5.59286616700006,11.6,9.07212943299999));
#237034=CARTESIAN_POINT('Ctrl Pts',(-5.59217822700006,15.2,9.06995837499998));
#237035=CARTESIAN_POINT('Ctrl Pts',(-5.59217822700006,11.6,9.06995837499998));
#237036=CARTESIAN_POINT('Ctrl Pts',(-5.59149036100006,15.2,9.06779415799999));
#237037=CARTESIAN_POINT('Ctrl Pts',(-5.59149036100006,11.6,9.06779415799999));
#237038=CARTESIAN_POINT('Ctrl Pts',(-5.59080258200006,15.2,9.06563679099998));
#237039=CARTESIAN_POINT('Ctrl Pts',(-5.59080258200006,11.6,9.06563679099998));
#237040=CARTESIAN_POINT('Ctrl Pts',(-5.59011490400006,15.2,9.06348628499998));
#237041=CARTESIAN_POINT('Ctrl Pts',(-5.59011490400006,11.6,9.06348628499998));
#237042=CARTESIAN_POINT('Ctrl Pts',(-5.58942734000006,15.2,9.06134264799999));
#237043=CARTESIAN_POINT('Ctrl Pts',(-5.58942734000006,11.6,9.06134264799999));
#237044=CARTESIAN_POINT('Ctrl Pts',(-5.58873990500006,15.2,9.05920589099999));
#237045=CARTESIAN_POINT('Ctrl Pts',(-5.58873990500006,11.6,9.05920589099999));
#237046=CARTESIAN_POINT('Ctrl Pts',(-5.58805261400006,15.2,9.05707602299999));
#237047=CARTESIAN_POINT('Ctrl Pts',(-5.58805261400006,11.6,9.05707602299999));
#237048=CARTESIAN_POINT('Ctrl Pts',(-5.58736547800006,15.2,9.05495305299999));
#237049=CARTESIAN_POINT('Ctrl Pts',(-5.58736547800006,11.6,9.05495305299999));
#237050=CARTESIAN_POINT('Ctrl Pts',(-5.58667851500006,15.2,9.05283699299999));
#237051=CARTESIAN_POINT('Ctrl Pts',(-5.58667851500006,11.6,9.05283699299999));
#237052=CARTESIAN_POINT('Ctrl Pts',(-5.58599173500006,15.2,9.05072784999999));
#237053=CARTESIAN_POINT('Ctrl Pts',(-5.58599173500006,11.6,9.05072784999999));
#237054=CARTESIAN_POINT('Ctrl Pts',(-5.58530515500006,15.2,9.04862563599998));
#237055=CARTESIAN_POINT('Ctrl Pts',(-5.58530515500006,11.6,9.04862563599998));
#237056=CARTESIAN_POINT('Ctrl Pts',(-5.58461878900006,15.2,9.04653035999999));
#237057=CARTESIAN_POINT('Ctrl Pts',(-5.58461878900006,11.6,9.04653035999999));
#237058=CARTESIAN_POINT('Ctrl Pts',(-5.58393265100006,15.2,9.04444203099998));
#237059=CARTESIAN_POINT('Ctrl Pts',(-5.58393265100006,11.6,9.04444203099998));
#237060=CARTESIAN_POINT('Ctrl Pts',(-5.58324675400006,15.2,9.04236066099998));
#237061=CARTESIAN_POINT('Ctrl Pts',(-5.58324675400006,11.6,9.04236066099998));
#237062=CARTESIAN_POINT('Ctrl Pts',(-5.58256111400006,15.2,9.04028625599998));
#237063=CARTESIAN_POINT('Ctrl Pts',(-5.58256111400006,11.6,9.04028625599998));
#237064=CARTESIAN_POINT('Ctrl Pts',(-5.58187574600006,15.2,9.03821882999999));
#237065=CARTESIAN_POINT('Ctrl Pts',(-5.58187574600006,11.6,9.03821882999999));
#237066=CARTESIAN_POINT('Ctrl Pts',(-5.58119066300006,15.2,9.03615839199999));
#237067=CARTESIAN_POINT('Ctrl Pts',(-5.58119066300006,11.6,9.03615839199999));
#237068=CARTESIAN_POINT('Ctrl Pts',(-5.58050588000006,15.2,9.03410494999999));
#237069=CARTESIAN_POINT('Ctrl Pts',(-5.58050588000006,11.6,9.03410494999999));
#237070=CARTESIAN_POINT('Ctrl Pts',(-5.57982141200006,15.2,9.03205851399999));
#237071=CARTESIAN_POINT('Ctrl Pts',(-5.57982141200006,11.6,9.03205851399999));
#237072=CARTESIAN_POINT('Ctrl Pts',(-5.57913727300006,15.2,9.03001909699999));
#237073=CARTESIAN_POINT('Ctrl Pts',(-5.57913727300006,11.6,9.03001909699999));
#237074=CARTESIAN_POINT('Ctrl Pts',(-5.57845347900006,15.2,9.02798670599999));
#237075=CARTESIAN_POINT('Ctrl Pts',(-5.57845347900006,11.6,9.02798670599999));
#237076=CARTESIAN_POINT('Ctrl Pts',(-5.57777004300006,15.2,9.02596135299999));
#237077=CARTESIAN_POINT('Ctrl Pts',(-5.57777004300006,11.6,9.02596135299999));
#237078=CARTESIAN_POINT('Ctrl Pts',(-5.57708698100006,15.2,9.02394304599999));
#237079=CARTESIAN_POINT('Ctrl Pts',(-5.57708698100006,11.6,9.02394304599999));
#237080=CARTESIAN_POINT('Ctrl Pts',(-5.57640430800006,15.2,9.02193179699999));
#237081=CARTESIAN_POINT('Ctrl Pts',(-5.57640430800006,11.6,9.02193179699999));
#237082=CARTESIAN_POINT('Ctrl Pts',(-5.57572203700006,15.2,9.01992761499999));
#237083=CARTESIAN_POINT('Ctrl Pts',(-5.57572203700006,11.6,9.01992761499999));
#237084=CARTESIAN_POINT('Ctrl Pts',(-5.57504018500006,15.2,9.01793050999999));
#237085=CARTESIAN_POINT('Ctrl Pts',(-5.57504018500006,11.6,9.01793050999999));
#237086=CARTESIAN_POINT('Ctrl Pts',(-5.57435876800006,15.2,9.01594049299998));
#237087=CARTESIAN_POINT('Ctrl Pts',(-5.57435876800006,11.6,9.01594049299998));
#237088=CARTESIAN_POINT('Ctrl Pts',(-5.57367779900006,15.2,9.01395757299999));
#237089=CARTESIAN_POINT('Ctrl Pts',(-5.57367779900006,11.6,9.01395757299999));
#237090=CARTESIAN_POINT('Ctrl Pts',(-5.57299729300006,15.2,9.01198176199999));
#237091=CARTESIAN_POINT('Ctrl Pts',(-5.57299729300006,11.6,9.01198176199999));
#237092=CARTESIAN_POINT('Ctrl Pts',(-5.57231726600006,15.2,9.01001306799999));
#237093=CARTESIAN_POINT('Ctrl Pts',(-5.57231726600006,11.6,9.01001306799999));
#237094=CARTESIAN_POINT('Ctrl Pts',(-5.57163773400006,15.2,9.00805150299998));
#237095=CARTESIAN_POINT('Ctrl Pts',(-5.57163773400006,11.6,9.00805150299998));
#237096=CARTESIAN_POINT('Ctrl Pts',(-5.57095871100006,15.2,9.00609707599998));
#237097=CARTESIAN_POINT('Ctrl Pts',(-5.57095871100006,11.6,9.00609707599998));
#237098=CARTESIAN_POINT('Ctrl Pts',(-5.57028021400006,15.2,9.00414979799999));
#237099=CARTESIAN_POINT('Ctrl Pts',(-5.57028021400006,11.6,9.00414979799999));
#237100=CARTESIAN_POINT('Ctrl Pts',(-5.56960225700006,15.2,9.00220967899998));
#237101=CARTESIAN_POINT('Ctrl Pts',(-5.56960225700006,11.6,9.00220967899998));
#237102=CARTESIAN_POINT('Ctrl Pts',(-5.56892485500006,15.2,9.00027672899999));
#237103=CARTESIAN_POINT('Ctrl Pts',(-5.56892485500006,11.6,9.00027672899999));
#237104=CARTESIAN_POINT('Ctrl Pts',(-5.56824802500006,15.2,8.99835095899999));
#237105=CARTESIAN_POINT('Ctrl Pts',(-5.56824802500006,11.6,8.99835095899999));
#237106=CARTESIAN_POINT('Ctrl Pts',(-5.56757178200006,15.2,8.99643237899999));
#237107=CARTESIAN_POINT('Ctrl Pts',(-5.56757178200006,11.6,8.99643237899999));
#237108=CARTESIAN_POINT('Ctrl Pts',(-5.56689614200006,15.2,8.99452099999999));
#237109=CARTESIAN_POINT('Ctrl Pts',(-5.56689614200006,11.6,8.99452099999999));
#237110=CARTESIAN_POINT('Ctrl Pts',(-5.56622112000006,15.2,8.99261682999999));
#237111=CARTESIAN_POINT('Ctrl Pts',(-5.56622112000006,11.6,8.99261682999999));
#237112=CARTESIAN_POINT('Ctrl Pts',(-5.56554673300006,15.2,8.99071988199999));
#237113=CARTESIAN_POINT('Ctrl Pts',(-5.56554673300006,11.6,8.99071988199999));
#237114=CARTESIAN_POINT('Ctrl Pts',(-5.56487299500006,15.2,8.98883016799999));
#237115=CARTESIAN_POINT('Ctrl Pts',(-5.56487299500006,11.6,8.98883016799999));
#237116=CARTESIAN_POINT('Ctrl Pts',(-5.56419992400006,15.2,8.98694769299999));
#237117=CARTESIAN_POINT('Ctrl Pts',(-5.56419992400006,11.6,8.98694769299999));
#237118=CARTESIAN_POINT('Ctrl Pts',(-5.56352753400006,15.2,8.98507247299998));
#237119=CARTESIAN_POINT('Ctrl Pts',(-5.56352753400006,11.6,8.98507247299998));
#237120=CARTESIAN_POINT('Ctrl Pts',(-5.56285584300006,15.2,8.98320451499998));
#237121=CARTESIAN_POINT('Ctrl Pts',(-5.56285584300006,11.6,8.98320451499998));
#237122=CARTESIAN_POINT('Ctrl Pts',(-5.56218486400006,15.2,8.98134383099999));
#237123=CARTESIAN_POINT('Ctrl Pts',(-5.56218486400006,11.6,8.98134383099999));
#237124=CARTESIAN_POINT('Ctrl Pts',(-5.56151461700006,15.2,8.97949043099998));
#237125=CARTESIAN_POINT('Ctrl Pts',(-5.56151461700006,11.6,8.97949043099998));
#237126=CARTESIAN_POINT('Ctrl Pts',(-5.56084511600006,15.2,8.97764432799999));
#237127=CARTESIAN_POINT('Ctrl Pts',(-5.56084511600006,11.6,8.97764432799999));
#237128=CARTESIAN_POINT('Ctrl Pts',(-5.56017637800006,15.2,8.97580552899999));
#237129=CARTESIAN_POINT('Ctrl Pts',(-5.56017637800006,11.6,8.97580552899999));
#237130=CARTESIAN_POINT('Ctrl Pts',(-5.55950841800006,15.2,8.97397404599998));
#237131=CARTESIAN_POINT('Ctrl Pts',(-5.55950841800006,11.6,8.97397404599998));
#237132=CARTESIAN_POINT('Ctrl Pts',(-5.55884125300006,15.2,8.97214989099999));
#237133=CARTESIAN_POINT('Ctrl Pts',(-5.55884125300006,11.6,8.97214989099999));
#237134=CARTESIAN_POINT('Ctrl Pts',(-5.55817490100006,15.2,8.97033307399998));
#237135=CARTESIAN_POINT('Ctrl Pts',(-5.55817490100006,11.6,8.97033307399998));
#237136=CARTESIAN_POINT('Ctrl Pts',(-5.55750937700005,15.2,8.96852360499999));
#237137=CARTESIAN_POINT('Ctrl Pts',(-5.55750937700005,11.6,8.96852360499999));
#237138=CARTESIAN_POINT('Ctrl Pts',(-5.55684469700005,15.2,8.96672149499998));
#237139=CARTESIAN_POINT('Ctrl Pts',(-5.55684469700005,11.6,8.96672149499998));
#237140=CARTESIAN_POINT('Ctrl Pts',(-5.55618088000006,15.2,8.96492675499999));
#237141=CARTESIAN_POINT('Ctrl Pts',(-5.55618088000006,11.6,8.96492675499999));
#237142=CARTESIAN_POINT('Ctrl Pts',(-5.55551794000006,15.2,8.96313939699999));
#237143=CARTESIAN_POINT('Ctrl Pts',(-5.55551794000006,11.6,8.96313939699999));
#237144=CARTESIAN_POINT('Ctrl Pts',(-5.55485589600006,15.2,8.96135942899999));
#237145=CARTESIAN_POINT('Ctrl Pts',(-5.55485589600006,11.6,8.96135942899999));
#237146=CARTESIAN_POINT('Ctrl Pts',(-5.55419476400006,15.2,8.95958686499998));
#237147=CARTESIAN_POINT('Ctrl Pts',(-5.55419476400006,11.6,8.95958686499998));
#237148=CARTESIAN_POINT('Ctrl Pts',(-5.55353456000006,15.2,8.95782171299999));
#237149=CARTESIAN_POINT('Ctrl Pts',(-5.55353456000006,11.6,8.95782171299999));
#237150=CARTESIAN_POINT('Ctrl Pts',(-5.55287530200006,15.2,8.95606398699999));
#237151=CARTESIAN_POINT('Ctrl Pts',(-5.55287530200006,11.6,8.95606398699999));
#237152=CARTESIAN_POINT('Ctrl Pts',(-5.55221700600006,15.2,8.95431369599999));
#237153=CARTESIAN_POINT('Ctrl Pts',(-5.55221700600006,11.6,8.95431369599999));
#237154=CARTESIAN_POINT('Ctrl Pts',(-5.55155969100006,15.2,8.95257084999999));
#237155=CARTESIAN_POINT('Ctrl Pts',(-5.55155969100006,11.6,8.95257084999999));
#237156=CARTESIAN_POINT('Ctrl Pts',(-5.55090337300006,15.2,8.95083546399999));
#237157=CARTESIAN_POINT('Ctrl Pts',(-5.55090337300006,11.6,8.95083546399999));
#237158=CARTESIAN_POINT('Ctrl Pts',(-5.55024806800006,15.2,8.94910754499998));
#237159=CARTESIAN_POINT('Ctrl Pts',(-5.55024806800006,11.6,8.94910754499998));
#237160=CARTESIAN_POINT('Ctrl Pts',(-5.54959379600006,15.2,8.94738710499999));
#237161=CARTESIAN_POINT('Ctrl Pts',(-5.54959379600006,11.6,8.94738710499999));
#237162=CARTESIAN_POINT('Ctrl Pts',(-5.54894057200006,15.2,8.94567415599998));
#237163=CARTESIAN_POINT('Ctrl Pts',(-5.54894057200006,11.6,8.94567415599998));
#237164=CARTESIAN_POINT('Ctrl Pts',(-5.54828841500006,15.2,8.94396870899998));
#237165=CARTESIAN_POINT('Ctrl Pts',(-5.54828841500006,11.6,8.94396870899998));
#237166=CARTESIAN_POINT('Ctrl Pts',(-5.54763734200006,15.2,8.94227077499998));
#237167=CARTESIAN_POINT('Ctrl Pts',(-5.54763734200006,11.6,8.94227077499998));
#237168=CARTESIAN_POINT('Ctrl Pts',(-5.54698737000006,15.2,8.94058036599999));
#237169=CARTESIAN_POINT('Ctrl Pts',(-5.54698737000006,11.6,8.94058036599999));
#237170=CARTESIAN_POINT('Ctrl Pts',(-5.54633851800006,15.2,8.93889749199998));
#237171=CARTESIAN_POINT('Ctrl Pts',(-5.54633851800006,11.6,8.93889749199998));
#237172=CARTESIAN_POINT('Ctrl Pts',(-5.54569080200006,15.2,8.93722216299999));
#237173=CARTESIAN_POINT('Ctrl Pts',(-5.54569080200006,11.6,8.93722216299999));
#237174=CARTESIAN_POINT('Ctrl Pts',(-5.54504424100006,15.2,8.93555439299998));
#237175=CARTESIAN_POINT('Ctrl Pts',(-5.54504424100006,11.6,8.93555439299998));
#237176=CARTESIAN_POINT('Ctrl Pts',(-5.54439885200006,15.2,8.93389419199998));
#237177=CARTESIAN_POINT('Ctrl Pts',(-5.54439885200006,11.6,8.93389419199998));
#237178=CARTESIAN_POINT('Ctrl Pts',(-5.54375465500006,15.2,8.93224157199998));
#237179=CARTESIAN_POINT('Ctrl Pts',(-5.54375465500006,11.6,8.93224157199998));
#237180=CARTESIAN_POINT('Ctrl Pts',(-5.54311166500006,15.2,8.93059654399998));
#237181=CARTESIAN_POINT('Ctrl Pts',(-5.54311166500006,11.6,8.93059654399998));
#237182=CARTESIAN_POINT('Ctrl Pts',(-5.54246990300006,15.2,8.92895911799998));
#237183=CARTESIAN_POINT('Ctrl Pts',(-5.54246990300006,11.6,8.92895911799998));
#237184=CARTESIAN_POINT('Ctrl Pts',(-5.54182938400006,15.2,8.92732930799998));
#237185=CARTESIAN_POINT('Ctrl Pts',(-5.54182938400006,11.6,8.92732930799998));
#237186=CARTESIAN_POINT('Ctrl Pts',(-5.54119012900006,15.2,8.92570712399999));
#237187=CARTESIAN_POINT('Ctrl Pts',(-5.54119012900006,11.6,8.92570712399999));
#237188=CARTESIAN_POINT('Ctrl Pts',(-5.54055215600005,15.2,8.92409257799999));
#237189=CARTESIAN_POINT('Ctrl Pts',(-5.54055215600005,11.6,8.92409257799999));
#237190=CARTESIAN_POINT('Ctrl Pts',(-5.53991548100006,15.2,8.92248568099999));
#237191=CARTESIAN_POINT('Ctrl Pts',(-5.53991548100006,11.6,8.92248568099999));
#237192=CARTESIAN_POINT('Ctrl Pts',(-5.53928012500006,15.2,8.92088644499999));
#237193=CARTESIAN_POINT('Ctrl Pts',(-5.53928012500006,11.6,8.92088644499999));
#237194=CARTESIAN_POINT('Ctrl Pts',(-5.53864610500006,15.2,8.91929488199998));
#237195=CARTESIAN_POINT('Ctrl Pts',(-5.53864610500006,11.6,8.91929488199998));
#237196=CARTESIAN_POINT('Ctrl Pts',(-5.53801344100005,15.2,8.91771100199998));
#237197=CARTESIAN_POINT('Ctrl Pts',(-5.53801344100005,11.6,8.91771100199998));
#237198=CARTESIAN_POINT('Ctrl Pts',(-5.53738215100006,15.2,8.91613481799999));
#237199=CARTESIAN_POINT('Ctrl Pts',(-5.53738215100006,11.6,8.91613481799999));
#237200=CARTESIAN_POINT('Ctrl Pts',(-5.53675225300006,15.2,8.91456634199999));
#237201=CARTESIAN_POINT('Ctrl Pts',(-5.53675225300006,11.6,8.91456634199999));
#237202=CARTESIAN_POINT('Ctrl Pts',(-5.53612376700006,15.2,8.91300558499999));
#237203=CARTESIAN_POINT('Ctrl Pts',(-5.53612376700006,11.6,8.91300558499999));
#237204=CARTESIAN_POINT('Ctrl Pts',(-5.53549671100006,15.2,8.91145255899998));
#237205=CARTESIAN_POINT('Ctrl Pts',(-5.53549671100006,11.6,8.91145255899998));
#237206=CARTESIAN_POINT('Ctrl Pts',(-5.53487110500006,15.2,8.90990727499998));
#237207=CARTESIAN_POINT('Ctrl Pts',(-5.53487110500006,11.6,8.90990727499998));
#237208=CARTESIAN_POINT('Ctrl Pts',(-5.53424696700006,15.2,8.90836974599999));
#237209=CARTESIAN_POINT('Ctrl Pts',(-5.53424696700006,11.6,8.90836974599999));
#237210=CARTESIAN_POINT('Ctrl Pts',(-5.53362431700006,15.2,8.90683998299998));
#237211=CARTESIAN_POINT('Ctrl Pts',(-5.53362431700006,11.6,8.90683998299998));
#237212=CARTESIAN_POINT('Ctrl Pts',(-5.53300317300006,15.2,8.90531799899998));
#237213=CARTESIAN_POINT('Ctrl Pts',(-5.53300317300006,11.6,8.90531799899998));
#237214=CARTESIAN_POINT('Ctrl Pts',(-5.53238355700006,15.2,8.90380380499998));
#237215=CARTESIAN_POINT('Ctrl Pts',(-5.53238355700006,11.6,8.90380380499998));
#237216=CARTESIAN_POINT('Ctrl Pts',(-5.53176548500006,15.2,8.90229741299999));
#237217=CARTESIAN_POINT('Ctrl Pts',(-5.53176548500006,11.6,8.90229741299999));
#237218=CARTESIAN_POINT('Ctrl Pts',(-5.53114897900006,15.2,8.90079883599999));
#237219=CARTESIAN_POINT('Ctrl Pts',(-5.53114897900006,11.6,8.90079883599999));
#237220=CARTESIAN_POINT('Ctrl Pts',(-5.53053405700005,15.2,8.89930808399999));
#237221=CARTESIAN_POINT('Ctrl Pts',(-5.53053405700005,11.6,8.89930808399999));
#237222=CARTESIAN_POINT('Ctrl Pts',(-5.52992074000006,15.2,8.89782517099999));
#237223=CARTESIAN_POINT('Ctrl Pts',(-5.52992074000006,11.6,8.89782517099999));
#237224=CARTESIAN_POINT('Ctrl Pts',(-5.52930904600006,15.2,8.89635010899998));
#237225=CARTESIAN_POINT('Ctrl Pts',(-5.52930904600006,11.6,8.89635010899998));
#237226=CARTESIAN_POINT('Ctrl Pts',(-5.52869899600006,15.2,8.89488290899998));
#237227=CARTESIAN_POINT('Ctrl Pts',(-5.52869899600006,11.6,8.89488290899998));
#237228=CARTESIAN_POINT('Ctrl Pts',(-5.52809061100006,15.2,8.89342358399999));
#237229=CARTESIAN_POINT('Ctrl Pts',(-5.52809061100006,11.6,8.89342358399999));
#237230=CARTESIAN_POINT('Ctrl Pts',(-5.52748390800006,15.2,8.89197214599999));
#237231=CARTESIAN_POINT('Ctrl Pts',(-5.52748390800006,11.6,8.89197214599999));
#237232=CARTESIAN_POINT('Ctrl Pts',(-5.52687891000006,15.2,8.89052860699999));
#237233=CARTESIAN_POINT('Ctrl Pts',(-5.52687891000006,11.6,8.89052860699999));
#237234=CARTESIAN_POINT('Ctrl Pts',(-5.52627563500006,15.2,8.88909297999999));
#237235=CARTESIAN_POINT('Ctrl Pts',(-5.52627563500006,11.6,8.88909297999999));
#237236=CARTESIAN_POINT('Ctrl Pts',(-5.52567410500005,15.2,8.88766527599999));
#237237=CARTESIAN_POINT('Ctrl Pts',(-5.52567410500005,11.6,8.88766527599999));
#237238=CARTESIAN_POINT('Ctrl Pts',(-5.52507433900006,15.2,8.88624550999998));
#237239=CARTESIAN_POINT('Ctrl Pts',(-5.52507433900006,11.6,8.88624550999998));
#237240=CARTESIAN_POINT('Ctrl Pts',(-5.52447635900006,15.2,8.88483369099998));
#237241=CARTESIAN_POINT('Ctrl Pts',(-5.52447635900006,11.6,8.88483369099998));
#237242=CARTESIAN_POINT('Ctrl Pts',(-5.52388018300006,15.2,8.88342983299999));
#237243=CARTESIAN_POINT('Ctrl Pts',(-5.52388018300006,11.6,8.88342983299999));
#237244=CARTESIAN_POINT('Ctrl Pts',(-5.52328583400006,15.2,8.88203394999999));
#237245=CARTESIAN_POINT('Ctrl Pts',(-5.52328583400006,11.6,8.88203394999999));
#237246=CARTESIAN_POINT('Ctrl Pts',(-5.52269333100006,15.2,8.88064605199999));
#237247=CARTESIAN_POINT('Ctrl Pts',(-5.52269333100006,11.6,8.88064605199999));
#237248=CARTESIAN_POINT('Ctrl Pts',(-5.52210269600006,15.2,8.87926615299998));
#237249=CARTESIAN_POINT('Ctrl Pts',(-5.52210269600006,11.6,8.87926615299998));
#237250=CARTESIAN_POINT('Ctrl Pts',(-5.52151394900006,15.2,8.87789426599999));
#237251=CARTESIAN_POINT('Ctrl Pts',(-5.52151394900006,11.6,8.87789426599999));
#237252=CARTESIAN_POINT('Ctrl Pts',(-5.52092711200006,15.2,8.87653040299998));
#237253=CARTESIAN_POINT('Ctrl Pts',(-5.52092711200006,11.6,8.87653040299998));
#237254=CARTESIAN_POINT('Ctrl Pts',(-5.52034220400006,15.2,8.87517457499998));
#237255=CARTESIAN_POINT('Ctrl Pts',(-5.52034220400006,11.6,8.87517457499998));
#237256=CARTESIAN_POINT('Ctrl Pts',(-5.51975924900006,15.2,8.87382679799998));
#237257=CARTESIAN_POINT('Ctrl Pts',(-5.51975924900006,11.6,8.87382679799998));
#237258=CARTESIAN_POINT('Ctrl Pts',(-5.51917826500006,15.2,8.87248708199999));
#237259=CARTESIAN_POINT('Ctrl Pts',(-5.51917826500006,11.6,8.87248708199999));
#237260=CARTESIAN_POINT('Ctrl Pts',(-5.51859927600006,15.2,8.87115544199998));
#237261=CARTESIAN_POINT('Ctrl Pts',(-5.51859927600006,11.6,8.87115544199998));
#237262=CARTESIAN_POINT('Ctrl Pts',(-5.51802230300006,15.2,8.86983188899999));
#237263=CARTESIAN_POINT('Ctrl Pts',(-5.51802230300006,11.6,8.86983188899999));
#237264=CARTESIAN_POINT('Ctrl Pts',(-5.51744736700006,15.2,8.86851643699998));
#237265=CARTESIAN_POINT('Ctrl Pts',(-5.51744736700006,11.6,8.86851643699998));
#237266=CARTESIAN_POINT('Ctrl Pts',(-5.51687448900006,15.2,8.86720909899999));
#237267=CARTESIAN_POINT('Ctrl Pts',(-5.51687448900006,11.6,8.86720909899999));
#237268=CARTESIAN_POINT('Ctrl Pts',(-5.51630369100006,15.2,8.86590988699999));
#237269=CARTESIAN_POINT('Ctrl Pts',(-5.51630369100006,11.6,8.86590988699999));
#237270=CARTESIAN_POINT('Ctrl Pts',(-5.51573499600006,15.2,8.86461881499999));
#237271=CARTESIAN_POINT('Ctrl Pts',(-5.51573499600006,11.6,8.86461881499999));
#237272=CARTESIAN_POINT('Ctrl Pts',(-5.51516842500006,15.2,8.86333589499999));
#237273=CARTESIAN_POINT('Ctrl Pts',(-5.51516842500006,11.6,8.86333589499999));
#237274=CARTESIAN_POINT('Ctrl Pts',(-5.51460400000006,15.2,8.86206114199998));
#237275=CARTESIAN_POINT('Ctrl Pts',(-5.51460400000006,11.6,8.86206114199998));
#237276=CARTESIAN_POINT('Ctrl Pts',(-5.51404174200006,15.2,8.86079456799998));
#237277=CARTESIAN_POINT('Ctrl Pts',(-5.51404174200006,11.6,8.86079456799998));
#237278=CARTESIAN_POINT('Ctrl Pts',(-5.51348167600006,15.2,8.85953618499999));
#237279=CARTESIAN_POINT('Ctrl Pts',(-5.51348167600006,11.6,8.85953618499999));
#237280=CARTESIAN_POINT('Ctrl Pts',(-5.51292382200006,15.2,8.85828600699998));
#237281=CARTESIAN_POINT('Ctrl Pts',(-5.51292382200006,11.6,8.85828600699998));
#237282=CARTESIAN_POINT('Ctrl Pts',(-5.51236820400006,15.2,8.85704404899998));
#237283=CARTESIAN_POINT('Ctrl Pts',(-5.51236820400006,11.6,8.85704404899998));
#237284=CARTESIAN_POINT('Ctrl Pts',(-5.51181484300006,15.2,8.85581032199998));
#237285=CARTESIAN_POINT('Ctrl Pts',(-5.51181484300006,11.6,8.85581032199998));
#237286=CARTESIAN_POINT('Ctrl Pts',(-5.51126376200005,15.2,8.85458484099999));
#237287=CARTESIAN_POINT('Ctrl Pts',(-5.51126376200005,11.6,8.85458484099999));
#237288=CARTESIAN_POINT('Ctrl Pts',(-5.51071498500006,15.2,8.85336761899998));
#237289=CARTESIAN_POINT('Ctrl Pts',(-5.51071498500006,11.6,8.85336761899998));
#237290=CARTESIAN_POINT('Ctrl Pts',(-5.51016853400006,15.2,8.85215866799999));
#237291=CARTESIAN_POINT('Ctrl Pts',(-5.51016853400006,11.6,8.85215866799999));
#237292=CARTESIAN_POINT('Ctrl Pts',(-5.50962443100006,15.2,8.85095800399998));
#237293=CARTESIAN_POINT('Ctrl Pts',(-5.50962443100006,11.6,8.85095800399998));
#237294=CARTESIAN_POINT('Ctrl Pts',(-5.50908270000006,15.2,8.84976563899999));
#237295=CARTESIAN_POINT('Ctrl Pts',(-5.50908270000006,11.6,8.84976563899999));
#237296=CARTESIAN_POINT('Ctrl Pts',(-5.50854336400006,15.2,8.84858158699998));
#237297=CARTESIAN_POINT('Ctrl Pts',(-5.50854336400006,11.6,8.84858158699998));
#237298=CARTESIAN_POINT('Ctrl Pts',(-5.50800644600006,15.2,8.84740586199998));
#237299=CARTESIAN_POINT('Ctrl Pts',(-5.50800644600006,11.6,8.84740586199998));
#237300=CARTESIAN_POINT('Ctrl Pts',(-5.50747197000006,15.2,8.84623847599999));
#237301=CARTESIAN_POINT('Ctrl Pts',(-5.50747197000006,11.6,8.84623847599999));
#237302=CARTESIAN_POINT('Ctrl Pts',(-5.50693996000006,15.2,8.84507944399999));
#237303=CARTESIAN_POINT('Ctrl Pts',(-5.50693996000006,11.6,8.84507944399999));
#237304=CARTESIAN_POINT('Ctrl Pts',(-5.50641043800006,15.2,8.84392878099998));
#237305=CARTESIAN_POINT('Ctrl Pts',(-5.50641043800006,11.6,8.84392878099998));
#237306=CARTESIAN_POINT('Ctrl Pts',(-5.50588342800006,15.2,8.84278649899999));
#237307=CARTESIAN_POINT('Ctrl Pts',(-5.50588342800006,11.6,8.84278649899999));
#237308=CARTESIAN_POINT('Ctrl Pts',(-5.50535895400006,15.2,8.84165261399998));
#237309=CARTESIAN_POINT('Ctrl Pts',(-5.50535895400006,11.6,8.84165261399998));
#237310=CARTESIAN_POINT('Ctrl Pts',(-5.50483704200006,15.2,8.84052713699998));
#237311=CARTESIAN_POINT('Ctrl Pts',(-5.50483704200006,11.6,8.84052713699998));
#237312=CARTESIAN_POINT('Ctrl Pts',(-5.50431771200006,15.2,8.83941008399999));
#237313=CARTESIAN_POINT('Ctrl Pts',(-5.50431771200006,11.6,8.83941008399999));
#237314=CARTESIAN_POINT('Ctrl Pts',(-5.50380099200006,15.2,8.83830146899999));
#237315=CARTESIAN_POINT('Ctrl Pts',(-5.50380099200006,11.6,8.83830146899999));
#237316=CARTESIAN_POINT('Ctrl Pts',(-5.50328690400006,15.2,8.83720130499999));
#237317=CARTESIAN_POINT('Ctrl Pts',(-5.50328690400006,11.6,8.83720130499999));
#237318=CARTESIAN_POINT('Ctrl Pts',(-5.50277547400006,15.2,8.83610960699999));
#237319=CARTESIAN_POINT('Ctrl Pts',(-5.50277547400006,11.6,8.83610960699999));
#237320=CARTESIAN_POINT('Ctrl Pts',(-5.50226672400006,15.2,8.83502638999998));
#237321=CARTESIAN_POINT('Ctrl Pts',(-5.50226672400006,11.6,8.83502638999998));
#237322=CARTESIAN_POINT('Ctrl Pts',(-5.50176068200006,15.2,8.83395166599998));
#237323=CARTESIAN_POINT('Ctrl Pts',(-5.50176068200006,11.6,8.83395166599998));
#237324=CARTESIAN_POINT('Ctrl Pts',(-5.50125736900006,15.2,8.83288545099998));
#237325=CARTESIAN_POINT('Ctrl Pts',(-5.50125736900006,11.6,8.83288545099998));
#237326=CARTESIAN_POINT('Ctrl Pts',(-5.50075681300005,15.2,8.83182775999998));
#237327=CARTESIAN_POINT('Ctrl Pts',(-5.50075681300005,11.6,8.83182775999998));
#237328=CARTESIAN_POINT('Ctrl Pts',(-5.50025903800006,15.2,8.83077860499998));
#237329=CARTESIAN_POINT('Ctrl Pts',(-5.50025903800006,11.6,8.83077860499998));
#237330=CARTESIAN_POINT('Ctrl Pts',(-5.49976406900006,15.2,8.82973800399999));
#237331=CARTESIAN_POINT('Ctrl Pts',(-5.49976406900006,11.6,8.82973800399999));
#237332=CARTESIAN_POINT('Ctrl Pts',(-5.49927193100006,15.2,8.82870596699998));
#237333=CARTESIAN_POINT('Ctrl Pts',(-5.49927193100006,11.6,8.82870596699998));
#237334=CARTESIAN_POINT('Ctrl Pts',(-5.49878265000006,15.2,8.82768251199998));
#237335=CARTESIAN_POINT('Ctrl Pts',(-5.49878265000006,11.6,8.82768251199998));
#237336=CARTESIAN_POINT('Ctrl Pts',(-5.49829625000006,15.2,8.82666765299999));
#237337=CARTESIAN_POINT('Ctrl Pts',(-5.49829625000006,11.6,8.82666765299999));
#237338=CARTESIAN_POINT('Ctrl Pts',(-5.49781275900005,15.2,8.82566140499998));
#237339=CARTESIAN_POINT('Ctrl Pts',(-5.49781275900005,11.6,8.82566140499998));
#237340=CARTESIAN_POINT('Ctrl Pts',(-5.49733220000006,15.2,8.82466378199998));
#237341=CARTESIAN_POINT('Ctrl Pts',(-5.49733220000006,11.6,8.82466378199998));
#237342=CARTESIAN_POINT('Ctrl Pts',(-5.49685460100005,15.2,8.82367479799999));
#237343=CARTESIAN_POINT('Ctrl Pts',(-5.49685460100005,11.6,8.82367479799999));
#237344=CARTESIAN_POINT('Ctrl Pts',(-5.49637998700006,15.2,8.82269446999998));
#237345=CARTESIAN_POINT('Ctrl Pts',(-5.49637998700006,11.6,8.82269446999998));
#237346=CARTESIAN_POINT('Ctrl Pts',(-5.49590838400006,15.2,8.82172280999999));
#237347=CARTESIAN_POINT('Ctrl Pts',(-5.49590838400006,11.6,8.82172280999999));
#237348=CARTESIAN_POINT('Ctrl Pts',(-5.49543982000006,15.2,8.82075983599999));
#237349=CARTESIAN_POINT('Ctrl Pts',(-5.49543982000006,11.6,8.82075983599999));
#237350=CARTESIAN_POINT('Ctrl Pts',(-5.49497431900006,15.2,8.81980556199998));
#237351=CARTESIAN_POINT('Ctrl Pts',(-5.49497431900006,11.6,8.81980556199998));
#237352=CARTESIAN_POINT('Ctrl Pts',(-5.49451190900006,15.2,8.81886000199999));
#237353=CARTESIAN_POINT('Ctrl Pts',(-5.49451190900006,11.6,8.81886000199999));
#237354=CARTESIAN_POINT('Ctrl Pts',(-5.49405261600006,15.2,8.81792317399999));
#237355=CARTESIAN_POINT('Ctrl Pts',(-5.49405261600006,11.6,8.81792317399999));
#237356=CARTESIAN_POINT('Ctrl Pts',(-5.49359646800006,15.2,8.81699508999999));
#237357=CARTESIAN_POINT('Ctrl Pts',(-5.49359646800006,11.6,8.81699508999999));
#237358=CARTESIAN_POINT('Ctrl Pts',(-5.49314349000006,15.2,8.81607576599999));
#237359=CARTESIAN_POINT('Ctrl Pts',(-5.49314349000006,11.6,8.81607576599999));
#237360=CARTESIAN_POINT('Ctrl Pts',(-5.49269371000006,15.2,8.81516521899999));
#237361=CARTESIAN_POINT('Ctrl Pts',(-5.49269371000006,11.6,8.81516521899999));
#237362=CARTESIAN_POINT('Ctrl Pts',(-5.49224715600006,15.2,8.81426346299998));
#237363=CARTESIAN_POINT('Ctrl Pts',(-5.49224715600006,11.6,8.81426346299998));
#237364=CARTESIAN_POINT('Ctrl Pts',(-5.49180385400006,15.2,8.81337051399999));
#237365=CARTESIAN_POINT('Ctrl Pts',(-5.49180385400006,11.6,8.81337051399999));
#237366=CARTESIAN_POINT('Ctrl Pts',(-5.49136383300006,15.2,8.81248638799999));
#237367=CARTESIAN_POINT('Ctrl Pts',(-5.49136383300006,11.6,8.81248638799999));
#237368=CARTESIAN_POINT('Ctrl Pts',(-5.49092711900006,15.2,8.81161109899999));
#237369=CARTESIAN_POINT('Ctrl Pts',(-5.49092711900006,11.6,8.81161109899999));
#237370=CARTESIAN_POINT('Ctrl Pts',(-5.49049374100006,15.2,8.81074466399999));
#237371=CARTESIAN_POINT('Ctrl Pts',(-5.49049374100006,11.6,8.81074466399999));
#237372=CARTESIAN_POINT('Ctrl Pts',(-5.49006372600005,15.2,8.80988709899999));
#237373=CARTESIAN_POINT('Ctrl Pts',(-5.49006372600005,11.6,8.80988709899999));
#237374=CARTESIAN_POINT('Ctrl Pts',(-5.48963710300006,15.2,8.80903841899999));
#237375=CARTESIAN_POINT('Ctrl Pts',(-5.48963710300006,11.6,8.80903841899999));
#237376=CARTESIAN_POINT('Ctrl Pts',(-5.48921390000006,15.2,8.80819863999999));
#237377=CARTESIAN_POINT('Ctrl Pts',(-5.48921390000006,11.6,8.80819863999999));
#237378=CARTESIAN_POINT('Ctrl Pts',(-5.48879414500006,15.2,8.80736777799999));
#237379=CARTESIAN_POINT('Ctrl Pts',(-5.48879414500006,11.6,8.80736777799999));
#237380=CARTESIAN_POINT('Ctrl Pts',(-5.48838026300006,15.2,8.80655058299999));
#237381=CARTESIAN_POINT('Ctrl Pts',(-5.48838026300006,11.6,8.80655058299999));
#237382=CARTESIAN_POINT('Ctrl Pts',(-5.48805240300006,15.2,8.80590482999999));
#237383=CARTESIAN_POINT('Ctrl Pts',(-5.48805240300006,11.6,8.80590482999999));
#237384=CARTESIAN_POINT('Ctrl Pts',(-5.48780866100006,15.2,8.80542564399999));
#237385=CARTESIAN_POINT('Ctrl Pts',(-5.48780866100006,11.6,8.80542564399999));
#237386=CARTESIAN_POINT('Ctrl Pts',(-5.48764764400006,15.2,8.80510947799999));
#237387=CARTESIAN_POINT('Ctrl Pts',(-5.48764764400006,11.6,8.80510947799999));
#237388=CARTESIAN_POINT('Ctrl Pts',(-5.48756848000005,15.2,8.80495412799998));
#237389=CARTESIAN_POINT('Ctrl Pts',(-5.48756848000005,11.6,8.80495412799998));
#237390=CARTESIAN_POINT('',(-5.48756847926628,12.2,8.8049541278923));
#237391=CARTESIAN_POINT('',(-5.48756847926628,15.2,8.8049541278923));
#237392=CARTESIAN_POINT('',(-5.48756847900005,12.2,8.80495412799998));
#237393=CARTESIAN_POINT('Ctrl Pts',(-5.75020264100006,12.2,9.95917514599999));
#237394=CARTESIAN_POINT('Ctrl Pts',(-5.74993549095152,12.2,9.9553615703072));
#237395=CARTESIAN_POINT('Ctrl Pts',(-5.74966449066059,12.2,9.9515548942664));
#237396=CARTESIAN_POINT('Ctrl Pts',(-5.74938964931735,12.2,9.9477551211625));
#237397=CARTESIAN_POINT('Ctrl Pts',(-5.74911480797412,12.2,9.9439553480586));
#237398=CARTESIAN_POINT('Ctrl Pts',(-5.74883612314145,12.2,9.94016247891821));
#237399=CARTESIAN_POINT('Ctrl Pts',(-5.74855360555471,12.2,9.93637652394917));
#237400=CARTESIAN_POINT('Ctrl Pts',(-5.74827108796797,12.2,9.93259056898012));
#237401=CARTESIAN_POINT('Ctrl Pts',(-5.7479847387856,12.2,9.9288115322695));
#237402=CARTESIAN_POINT('Ctrl Pts',(-5.74769458688,12.2,9.92503944261393));
#237403=CARTESIAN_POINT('Ctrl Pts',(-5.74740443492168,12.2,9.92126735227309));
#237404=CARTESIAN_POINT('Ctrl Pts',(-5.74711048097896,12.2,9.91750221114257));
#237405=CARTESIAN_POINT('Ctrl Pts',(-5.74681275947684,12.2,9.91374405518067));
#237406=CARTESIAN_POINT('Ctrl Pts',(-5.74641579756416,12.2,9.9087331817027));
#237407=CARTESIAN_POINT('Ctrl Pts',(-5.74601213592458,12.2,9.90373472732586));
#237408=CARTESIAN_POINT('Ctrl Pts',(-5.74560183979189,12.2,9.89874875789932));
#237409=CARTESIAN_POINT('Ctrl Pts',(-5.7452941176784,12.2,9.89500928065957));
#237410=CARTESIAN_POINT('Ctrl Pts',(-5.74498266154822,12.2,9.89127682692236));
#237411=CARTESIAN_POINT('Ctrl Pts',(-5.74466749808602,12.2,9.88755142295411));
#237412=CARTESIAN_POINT('Ctrl Pts',(-5.74435233462383,12.2,9.88382601898586));
#237413=CARTESIAN_POINT('Ctrl Pts',(-5.7440334642415,12.2,9.88010766589182));
#237414=CARTESIAN_POINT('Ctrl Pts',(-5.7437109162954,12.2,9.87639639506733));
#237415=CARTESIAN_POINT('Ctrl Pts',(-5.74338836829068,12.2,9.87268512356862));
#237416=CARTESIAN_POINT('Ctrl Pts',(-5.74306214242661,12.2,9.86898093364698));
#237417=CARTESIAN_POINT('Ctrl Pts',(-5.74273226791983,12.2,9.86528385669397));
#237418=CARTESIAN_POINT('Ctrl Pts',(-5.74240239347298,12.2,9.8615867804126));
#237419=CARTESIAN_POINT('Ctrl Pts',(-5.74206887086801,12.2,9.85789681791419));
#237420=CARTESIAN_POINT('Ctrl Pts',(-5.74173172646327,12.2,9.85421399663196));
#237421=CARTESIAN_POINT('Ctrl Pts',(-5.74139458205854,12.2,9.85053117534973));
#237422=CARTESIAN_POINT('Ctrl Pts',(-5.7410538166555,12.2,9.84685549606329));
#237423=CARTESIAN_POINT('Ctrl Pts',(-5.7407094597081,12.2,9.84318698926327));
#237424=CARTESIAN_POINT('Ctrl Pts',(-5.74025031713242,12.2,9.8382956470854));
#237425=CARTESIAN_POINT('Ctrl Pts',(-5.73978478907412,12.2,9.83341705457963));
#237426=CARTESIAN_POINT('Ctrl Pts',(-5.73931294383556,12.2,9.82855128625382));
#237427=CARTESIAN_POINT('Ctrl Pts',(-5.7388410985327,12.2,9.82368551726505));
#237428=CARTESIAN_POINT('Ctrl Pts',(-5.73836293617649,12.2,9.81883257119429));
#237429=CARTESIAN_POINT('Ctrl Pts',(-5.73787852748342,12.2,9.81399251920826));
#237430=CARTESIAN_POINT('Ctrl Pts',(-5.73751522099661,12.2,9.81036248054847));
#237431=CARTESIAN_POINT('Ctrl Pts',(-5.73714840027663,12.2,9.80673969659675));
#237432=CARTESIAN_POINT('Ctrl Pts',(-5.73677809529038,12.2,9.80312419539415));
#237433=CARTESIAN_POINT('Ctrl Pts',(-5.73640779030415,12.2,9.79950869419157));
#237434=CARTESIAN_POINT('Ctrl Pts',(-5.73603400032777,12.2,9.79590047784658));
#237435=CARTESIAN_POINT('Ctrl Pts',(-5.73565675632303,12.2,9.79229957492169));
#237436=CARTESIAN_POINT('Ctrl Pts',(-5.73527951231829,12.2,9.7886986719968));
#237437=CARTESIAN_POINT('Ctrl Pts',(-5.73489881386939,12.2,9.78510508405244));
#237438=CARTESIAN_POINT('Ctrl Pts',(-5.73451469088382,12.2,9.78151884080674));
#237439=CARTESIAN_POINT('Ctrl Pts',(-5.73413056782845,12.2,9.77793259690953));
#237440=CARTESIAN_POINT('Ctrl Pts',(-5.73374301927213,12.2,9.77435369890607));
#237441=CARTESIAN_POINT('Ctrl Pts',(-5.73335207817319,12.2,9.77078217647135));
#237442=CARTESIAN_POINT('Ctrl Pts',(-5.73296113714526,12.2,9.76721065468546));
#237443=CARTESIAN_POINT('Ctrl Pts',(-5.73256680065918,12.2,9.76364650816581));
#237444=CARTESIAN_POINT('Ctrl Pts',(-5.73216910167334,12.2,9.76008976933738));
#237445=CARTESIAN_POINT('Ctrl Pts',(-5.73177140268751,12.2,9.75653303050894));
#237446=CARTESIAN_POINT('Ctrl Pts',(-5.73137033940206,12.2,9.75298369883793));
#237447=CARTESIAN_POINT('Ctrl Pts',(-5.73096594395841,12.2,9.74944180450826));
#237448=CARTESIAN_POINT('Ctrl Pts',(-5.73056154851477,12.2,9.7458999101786));
#237449=CARTESIAN_POINT('Ctrl Pts',(-5.73015382069627,12.2,9.74236545274034));
#237450=CARTESIAN_POINT('Ctrl Pts',(-5.72974279079483,12.2,9.73883846536783));
#237451=CARTESIAN_POINT('Ctrl Pts',(-5.72933176089338,12.2,9.73531147799533));
#237452=CARTESIAN_POINT('Ctrl Pts',(-5.72891742976949,12.2,9.73179195911153));
#237453=CARTESIAN_POINT('Ctrl Pts',(-5.72849982784751,12.2,9.72827993968783));
#237454=CARTESIAN_POINT('Ctrl Pts',(-5.72808222592554,12.2,9.72476792026413));
#237455=CARTESIAN_POINT('Ctrl Pts',(-5.72766135324335,12.2,9.72126340178625));
#237456=CARTESIAN_POINT('Ctrl Pts',(-5.72723724234253,12.2,9.71776641399561));
#237457=CARTESIAN_POINT('Ctrl Pts',(-5.72681313136466,12.2,9.71426942556968));
#237458=CARTESIAN_POINT('Ctrl Pts',(-5.72638578180256,12.2,9.7107799679459));
#237459=CARTESIAN_POINT('Ctrl Pts',(-5.72595522440622,12.2,9.70729807352422));
#237460=CARTESIAN_POINT('Ctrl Pts',(-5.72552466708808,12.2,9.70381617973508));
#237461=CARTESIAN_POINT('Ctrl Pts',(-5.72509090325346,12.2,9.70034184909557));
#237462=CARTESIAN_POINT('Ctrl Pts',(-5.72465396393573,12.2,9.69687511134718));
#237463=CARTESIAN_POINT('Ctrl Pts',(-5.72407137820521,12.2,9.69225279455926));
#237464=CARTESIAN_POINT('Ctrl Pts',(-5.72348314890852,12.2,9.6876439789108));
#237465=CARTESIAN_POINT('Ctrl Pts',(-5.72288935109454,12.2,9.68304873783347));
#237466=CARTESIAN_POINT('Ctrl Pts',(-5.72244400271384,12.2,9.67960230686893));
#237467=CARTESIAN_POINT('Ctrl Pts',(-5.72199552346502,12.2,9.67616351120767));
#237468=CARTESIAN_POINT('Ctrl Pts',(-5.72154394414852,12.2,9.67273238474793));
#237469=CARTESIAN_POINT('Ctrl Pts',(-5.72109236474997,12.2,9.66930125766486));
#237470=CARTESIAN_POINT('Ctrl Pts',(-5.72063768680056,12.2,9.66587779716734));
#237471=CARTESIAN_POINT('Ctrl Pts',(-5.72017994144195,12.2,9.66246203629698));
#237472=CARTESIAN_POINT('Ctrl Pts',(-5.71972219616651,12.2,9.65904627604715));
#237473=CARTESIAN_POINT('Ctrl Pts',(-5.71926138459955,12.2,9.65563821605519));
#237474=CARTESIAN_POINT('Ctrl Pts',(-5.7187975406578,12.2,9.65223788634609));
#237475=CARTESIAN_POINT('Ctrl Pts',(-5.71833369671606,12.2,9.64883755663699));
#237476=CARTESIAN_POINT('Ctrl Pts',(-5.71786681870139,12.2,9.64544495857255));
#237477=CARTESIAN_POINT('Ctrl Pts',(-5.71739694179965,12.2,9.64206012376353));
#237478=CARTESIAN_POINT('Ctrl Pts',(-5.71692706489791,12.2,9.63867528895451));
#237479=CARTESIAN_POINT('Ctrl Pts',(-5.71645418855203,12.2,9.6352982172959));
#237480=CARTESIAN_POINT('Ctrl Pts',(-5.71597834573384,12.2,9.63192894102801));
#237481=CARTESIAN_POINT('Ctrl Pts',(-5.71550250291565,12.2,9.62855966476013));
#237482=CARTESIAN_POINT('Ctrl Pts',(-5.71502369361811,12.2,9.62519818419446));
#237483=CARTESIAN_POINT('Ctrl Pts',(-5.71454195276087,12.2,9.62184453085728));
#237484=CARTESIAN_POINT('Ctrl Pts',(-5.71406021190362,12.2,9.6184908775201));
#237485=CARTESIAN_POINT('Ctrl Pts',(-5.71357553915492,12.2,9.61514504987407));
#237486=CARTESIAN_POINT('Ctrl Pts',(-5.7130879683397,12.2,9.61180708395261));
#237487=CARTESIAN_POINT('Ctrl Pts',(-5.71243787386034,12.2,9.60735646231972));
#237488=CARTESIAN_POINT('Ctrl Pts',(-5.71178262856641,12.2,9.60291981283576));
#237489=CARTESIAN_POINT('Ctrl Pts',(-5.71112231274963,12.2,9.59849721279693));
#237490=CARTESIAN_POINT('Ctrl Pts',(-5.71046199702282,12.2,9.59407461336068));
#237491=CARTESIAN_POINT('Ctrl Pts',(-5.70979661216269,12.2,9.58966606351618));
#237492=CARTESIAN_POINT('Ctrl Pts',(-5.70912624038468,12.2,9.58527164065176));
#237493=CARTESIAN_POINT('Ctrl Pts',(-5.70845586851532,12.2,9.58087721718861));
#237494=CARTESIAN_POINT('Ctrl Pts',(-5.70778050929827,12.2,9.57649692026289));
#237495=CARTESIAN_POINT('Ctrl Pts',(-5.70710024748341,12.2,9.57213082752493));
#237496=CARTESIAN_POINT('Ctrl Pts',(-5.70641998566856,12.2,9.56776473478699));
#237497=CARTESIAN_POINT('Ctrl Pts',(-5.70573482013369,12.2,9.56341284680068));
#237498=CARTESIAN_POINT('Ctrl Pts',(-5.70504483692893,12.2,9.55907524006574));
#237499=CARTESIAN_POINT('Ctrl Pts',(-5.70418235806398,12.2,9.55365323253354));
#237500=CARTESIAN_POINT('Ctrl Pts',(-5.70331235030193,12.2,9.54825354162456));
#237501=CARTESIAN_POINT('Ctrl Pts',(-5.70243498081483,12.2,9.54287631748661));
#237502=CARTESIAN_POINT('Ctrl Pts',(-5.70173308511039,12.2,9.5385745374729));
#237503=CARTESIAN_POINT('Ctrl Pts',(-5.70102647864994,12.2,9.53428713733559));
#237504=CARTESIAN_POINT('Ctrl Pts',(-5.70031524750008,12.2,9.53001419649159));
#237505=CARTESIAN_POINT('Ctrl Pts',(-5.6996040163502,12.2,9.52574125564758));
#237506=CARTESIAN_POINT('Ctrl Pts',(-5.69888816126923,12.2,9.52148277250805));
#237507=CARTESIAN_POINT('Ctrl Pts',(-5.69816776884062,12.2,9.51723882705606));
#237508=CARTESIAN_POINT('Ctrl Pts',(-5.69744737651016,12.2,9.5129948821823));
#237509=CARTESIAN_POINT('Ctrl Pts',(-5.69672244811368,12.2,9.50876547365796));
#237510=CARTESIAN_POINT('Ctrl Pts',(-5.69599307122557,12.2,9.50455068226114));
#237511=CARTESIAN_POINT('Ctrl Pts',(-5.69526369423808,12.2,9.50033589029005));
#237512=CARTESIAN_POINT('Ctrl Pts',(-5.69452986974228,12.2,9.49613571546167));
#237513=CARTESIAN_POINT('Ctrl Pts',(-5.69379168714604,12.2,9.49195023729062));
#237514=CARTESIAN_POINT('Ctrl Pts',(-5.69305350465039,12.2,9.48776475968983));
#237515=CARTESIAN_POINT('Ctrl Pts',(-5.6923109623803,12.2,9.48359397737877));
#237516=CARTESIAN_POINT('Ctrl Pts',(-5.69156415405275,12.2,9.47943797260649));
#237517=CARTESIAN_POINT('Ctrl Pts',(-5.69081734562345,12.2,9.47528196726795));
#237518=CARTESIAN_POINT('Ctrl Pts',(-5.69006626941694,12.2,9.47114073810043));
#237519=CARTESIAN_POINT('Ctrl Pts',(-5.68931101761546,12.2,9.46701436639292));
#237520=CARTESIAN_POINT('Ctrl Pts',(-5.68855576591689,12.2,9.46288799524762));
#237521=CARTESIAN_POINT('Ctrl Pts',(-5.68779633764698,12.2,9.45877648099271));
#237522=CARTESIAN_POINT('Ctrl Pts',(-5.68703282732078,12.2,9.45467990482663));
#237523=CARTESIAN_POINT('Ctrl Pts',(-5.68626931689054,12.2,9.45058332810239));
#237524=CARTESIAN_POINT('Ctrl Pts',(-5.68550172414315,12.2,9.44650168983546));
#237525=CARTESIAN_POINT('Ctrl Pts',(-5.68473014171196,12.2,9.44243506989263));
#237526=CARTESIAN_POINT('Ctrl Pts',(-5.68395855938589,12.2,9.43836845050387));
#237527=CARTESIAN_POINT('Ctrl Pts',(-5.68318298730471,12.2,9.43431685203927));
#237528=CARTESIAN_POINT('Ctrl Pts',(-5.68240352166316,12.2,9.43028035311073));
#237529=CARTESIAN_POINT('Ctrl Pts',(-5.68142918953157,12.2,9.42523472903758));
#237530=CARTESIAN_POINT('Ctrl Pts',(-5.68044877176978,12.2,9.4202127011226));
#237531=CARTESIAN_POINT('Ctrl Pts',(-5.67946245808954,12.2,9.41521442959361));
#237532=CARTESIAN_POINT('Ctrl Pts',(-5.67867340710234,12.2,9.4112158121525));
#237533=CARTESIAN_POINT('Ctrl Pts',(-5.67788058174245,12.2,9.40723239801872));
#237534=CARTESIAN_POINT('Ctrl Pts',(-5.67708407997659,12.2,9.40326427069235));
#237535=CARTESIAN_POINT('Ctrl Pts',(-5.67628757831925,12.2,9.39929614390663));
#237536=CARTESIAN_POINT('Ctrl Pts',(-5.67548740023762,12.2,9.39534330398449));
#237537=CARTESIAN_POINT('Ctrl Pts',(-5.67468364341482,12.2,9.39140583319371));
#237538=CARTESIAN_POINT('Ctrl Pts',(-5.67387988648249,12.2,9.38746836186645));
#237539=CARTESIAN_POINT('Ctrl Pts',(-5.67307255176684,12.2,9.3835462594334));
#237540=CARTESIAN_POINT('Ctrl Pts',(-5.67226173877452,12.2,9.3796396119806));
#237541=CARTESIAN_POINT('Ctrl Pts',(-5.67145092589267,12.2,9.37573296506008));
#237542=CARTESIAN_POINT('Ctrl Pts',(-5.67063663471935,12.2,9.37184177027394));
#237543=CARTESIAN_POINT('Ctrl Pts',(-5.66981896584209,12.2,9.36796611336693));
#237544=CARTESIAN_POINT('Ctrl Pts',(-5.66900129685342,12.2,9.36409045593187));
#237545=CARTESIAN_POINT('Ctrl Pts',(-5.66818025009777,12.2,9.36023033498444));
#237546=CARTESIAN_POINT('Ctrl Pts',(-5.66735592777507,12.2,9.35638583694158));
#237547=CARTESIAN_POINT('Ctrl Pts',(-5.66653160545237,12.2,9.35254133889872));
#237548=CARTESIAN_POINT('Ctrl Pts',(-5.6657040078654,12.2,9.34871246241046));
#237549=CARTESIAN_POINT('Ctrl Pts',(-5.66487323759757,12.2,9.34489929242648));
#237550=CARTESIAN_POINT('Ctrl Pts',(-5.66404246744294,12.2,9.34108612296205));
#237551=CARTESIAN_POINT('Ctrl Pts',(-5.66320852526101,12.2,9.33728865905224));
#237552=CARTESIAN_POINT('Ctrl Pts',(-5.66237151449231,12.2,9.33350698951084));
#237553=CARTESIAN_POINT('Ctrl Pts',(-5.66153450360957,12.2,9.32972531945419));
#237554=CARTESIAN_POINT('Ctrl Pts',(-5.66069442522793,12.2,9.3259594407618));
#237555=CARTESIAN_POINT('Ctrl Pts',(-5.6598513849039,12.2,9.32220944067015));
#237556=CARTESIAN_POINT('Ctrl Pts',(-5.65900834469473,12.2,9.31845944108943));
#237557=CARTESIAN_POINT('Ctrl Pts',(-5.65816234165263,12.2,9.3147253192317));
#237558=CARTESIAN_POINT('Ctrl Pts',(-5.6573134841111,12.2,9.31100716181236));
#237559=CARTESIAN_POINT('Ctrl Pts',(-5.6564646264539,12.2,9.30728900388642));
#237560=CARTESIAN_POINT('Ctrl Pts',(-5.65561291175167,12.2,9.30358681100157));
#237561=CARTESIAN_POINT('Ctrl Pts',(-5.6547584513844,12.2,9.29990066900679));
#237562=CARTESIAN_POINT('Ctrl Pts',(-5.65390399113354,12.2,9.29621452751426));
#237563=CARTESIAN_POINT('Ctrl Pts',(-5.65304678491376,12.2,9.29254443906502));
#237564=CARTESIAN_POINT('Ctrl Pts',(-5.65218693959533,12.2,9.28889048830712));
#237565=CARTESIAN_POINT('Ctrl Pts',(-5.65132709415975,12.2,9.28523653705136));
#237566=CARTESIAN_POINT('Ctrl Pts',(-5.65046461226275,12.2,9.28159872521422));
#237567=CARTESIAN_POINT('Ctrl Pts',(-5.64959960393766,12.2,9.27797713996233));
#237568=CARTESIAN_POINT('Ctrl Pts',(-5.64873459573042,12.2,9.27435555520388));
#237569=CARTESIAN_POINT('Ctrl Pts',(-5.64786705917064,12.2,9.27075019753865));
#237570=CARTESIAN_POINT('Ctrl Pts',(-5.64699710964295,12.2,9.26716115526246));
#237571=CARTESIAN_POINT('Ctrl Pts',(-5.64612715999673,12.2,9.26357211249726));
#237572=CARTESIAN_POINT('Ctrl Pts',(-5.64525479677636,12.2,9.2599993859021));
#237573=CARTESIAN_POINT('Ctrl Pts',(-5.64438013139521,12.2,9.25644306270936));
#237574=CARTESIAN_POINT('Ctrl Pts',(-5.64350546613323,12.2,9.25288674000116));
#237575=CARTESIAN_POINT('Ctrl Pts',(-5.64262850091339,12.2,9.24934682310634));
#237576=CARTESIAN_POINT('Ctrl Pts',(-5.64174935015214,12.2,9.24582339905934));
#237577=CARTESIAN_POINT('Ctrl Pts',(-5.64087019927111,12.2,9.24229997453227));
#237578=CARTESIAN_POINT('Ctrl Pts',(-5.63998886233218,12.2,9.23879304540355));
#237579=CARTESIAN_POINT('Ctrl Pts',(-5.63910545622447,12.2,9.23530269953089));
#237580=CARTESIAN_POINT('Ctrl Pts',(-5.63822205023712,12.2,9.23181235413379));
#237581=CARTESIAN_POINT('Ctrl Pts',(-5.63733657580295,12.2,9.22833859254533));
#237582=CARTESIAN_POINT('Ctrl Pts',(-5.63644914915349,12.2,9.22488150704849));
#237583=CARTESIAN_POINT('Ctrl Pts',(-5.6355617223831,12.2,9.22142442108061));
#237584=CARTESIAN_POINT('Ctrl Pts',(-5.63467234491252,12.2,9.21798400961427));
#237585=CARTESIAN_POINT('Ctrl Pts',(-5.63378113547506,12.2,9.21456036498324));
#237586=CARTESIAN_POINT('Ctrl Pts',(-5.63288992603761,12.2,9.21113672035222));
#237587=CARTESIAN_POINT('Ctrl Pts',(-5.63199688453049,12.2,9.20772984133425));
#237588=CARTESIAN_POINT('Ctrl Pts',(-5.63110213237044,12.2,9.204339821929));
#237589=CARTESIAN_POINT('Ctrl Pts',(-5.62998369235324,12.2,9.20010229836526));
#237590=CARTESIAN_POINT('Ctrl Pts',(-5.62886257929101,12.2,9.19589111373222));
#237591=CARTESIAN_POINT('Ctrl Pts',(-5.62773903191369,12.2,9.19170645279728));
#237592=CARTESIAN_POINT('Ctrl Pts',(-5.62684019386486,12.2,9.18835872350197));
#237593=CARTESIAN_POINT('Ctrl Pts',(-5.625939797677,12.2,9.18502796708053));
#237594=CARTESIAN_POINT('Ctrl Pts',(-5.62503796951673,12.2,9.18171427923325));
#237595=CARTESIAN_POINT('Ctrl Pts',(-5.62391068437783,12.2,9.17757216964991));
#237596=CARTESIAN_POINT('Ctrl Pts',(-5.62278115828237,12.2,9.17345672844954));
#237597=CARTESIAN_POINT('Ctrl Pts',(-5.62164964070778,12.2,9.16936813801436));
#237598=CARTESIAN_POINT('Ctrl Pts',(-5.6207444267221,12.2,9.16609726593362));
#237599=CARTESIAN_POINT('Ctrl Pts',(-5.61983793607136,12.2,9.16284357976905));
#237600=CARTESIAN_POINT('Ctrl Pts',(-5.61893029942346,12.2,9.15960717308741));
#237601=CARTESIAN_POINT('Ctrl Pts',(-5.61802266265188,12.2,9.15637076596481));
#237602=CARTESIAN_POINT('Ctrl Pts',(-5.61711387828576,12.2,9.15315163833275));
#237603=CARTESIAN_POINT('Ctrl Pts',(-5.61620407695839,12.2,9.14994988699158));
#237604=CARTESIAN_POINT('Ctrl Pts',(-5.61506682536117,12.2,9.14594769803325));
#237605=CARTESIAN_POINT('Ctrl Pts',(-5.61392798338796,12.2,9.14197265617118));
#237606=CARTESIAN_POINT('Ctrl Pts',(-5.6127878092161,12.2,9.13802495247277));
#237607=CARTESIAN_POINT('Ctrl Pts',(-5.61141960025961,12.2,9.1332877082068));
#237608=CARTESIAN_POINT('Ctrl Pts',(-5.61004947107491,12.2,9.12858982978641));
#237609=CARTESIAN_POINT('Ctrl Pts',(-5.60867787629147,12.2,9.12393164445396));
#237610=CARTESIAN_POINT('Ctrl Pts',(-5.60753488059709,12.2,9.12004982320255));
#237611=CARTESIAN_POINT('Ctrl Pts',(-5.60639086607488,12.2,9.11619556654622));
#237612=CARTESIAN_POINT('Ctrl Pts',(-5.60524610107492,12.2,9.11236906772532));
#237613=CARTESIAN_POINT('Ctrl Pts',(-5.60410133607495,12.2,9.10854256890443));
#237614=CARTESIAN_POINT('Ctrl Pts',(-5.60295581869722,12.2,9.10474382618153));
#237615=CARTESIAN_POINT('Ctrl Pts',(-5.6018098221,12.2,9.10097303347169));
#237616=CARTESIAN_POINT('Ctrl Pts',(-5.60066382550279,12.2,9.09720224076185));
#237617=CARTESIAN_POINT('Ctrl Pts',(-5.59951734752811,12.2,9.09345939971335));
#237618=CARTESIAN_POINT('Ctrl Pts',(-5.59837066675902,12.2,9.08974470441861));
#237619=CARTESIAN_POINT('Ctrl Pts',(-5.59722398598992,12.2,9.08603000912386));
#237620=CARTESIAN_POINT('Ctrl Pts',(-5.59607710063339,12.2,9.08234345933323));
#237621=CARTESIAN_POINT('Ctrl Pts',(-5.59493029250839,12.2,9.07868525474991));
#237622=CARTESIAN_POINT('Ctrl Pts',(-5.59378348438339,12.2,9.07502705016658));
#237623=CARTESIAN_POINT('Ctrl Pts',(-5.5926367517213,12.2,9.07139718914201));
#237624=CARTESIAN_POINT('Ctrl Pts',(-5.59149038275776,12.2,9.06779587051462));
#237625=CARTESIAN_POINT('Ctrl Pts',(-5.59034401379422,12.2,9.06419455188722));
#237626=CARTESIAN_POINT('Ctrl Pts',(-5.58919800655289,12.2,9.06062177750013));
#237627=CARTESIAN_POINT('Ctrl Pts',(-5.58805265273349,12.2,9.05707774729331));
#237628=CARTESIAN_POINT('Ctrl Pts',(-5.58667822820014,12.2,9.05282491119965));
#237629=CARTESIAN_POINT('Ctrl Pts',(-5.58530474388339,12.2,9.04861346827768));
#237630=CARTESIAN_POINT('Ctrl Pts',(-5.58393271134984,12.2,9.04444377092733));
#237631=CARTESIAN_POINT('Ctrl Pts',(-5.58278935086367,12.2,9.04096902300913));
#237632=CARTESIAN_POINT('Ctrl Pts',(-5.58164699923366,12.2,9.03752326494521));
#237633=CARTESIAN_POINT('Ctrl Pts',(-5.58050595874235,12.2,9.0341067015268));
#237634=CARTESIAN_POINT('Ctrl Pts',(-5.57936491825104,12.2,9.03069013810839));
#237635=CARTESIAN_POINT('Ctrl Pts',(-5.57822518878895,12.2,9.02730277234991));
#237636=CARTESIAN_POINT('Ctrl Pts',(-5.57708707823338,12.2,9.02394481047491));
#237637=CARTESIAN_POINT('Ctrl Pts',(-5.57594896767782,12.2,9.0205868485999));
#237638=CARTESIAN_POINT('Ctrl Pts',(-5.57481247511014,12.2,9.01725829134079));
#237639=CARTESIAN_POINT('Ctrl Pts',(-5.57367791475777,12.2,9.01395935021478));
#237640=CARTESIAN_POINT('Ctrl Pts',(-5.57254335440539,12.2,9.01066040908877));
#237641=CARTESIAN_POINT('Ctrl Pts',(-5.5714107252538,12.2,9.00739108364779));
#237642=CARTESIAN_POINT('Ctrl Pts',(-5.57028034893447,12.2,9.00415158753824));
#237643=CARTESIAN_POINT('Ctrl Pts',(-5.56892389740056,12.2,9.000264192348));
#237644=CARTESIAN_POINT('Ctrl Pts',(-5.56757068516641,12.2,8.99641975147935));
#237645=CARTESIAN_POINT('Ctrl Pts',(-5.56622127879861,12.2,8.99261863569892));
#237646=CARTESIAN_POINT('Ctrl Pts',(-5.56464697128781,12.2,8.98818400039156));
#237647=CARTESIAN_POINT('Ctrl Pts',(-5.56307783979562,12.2,8.98380833995238));
#237648=CARTESIAN_POINT('Ctrl Pts',(-5.56151480345205,12.2,8.97949225499847));
#237649=CARTESIAN_POINT('Ctrl Pts',(-5.56017505808426,12.2,8.97579275380143));
#237650=CARTESIAN_POINT('Ctrl Pts',(-5.55883978913277,12.2,8.97213702198428));
#237651=CARTESIAN_POINT('Ctrl Pts',(-5.55750958809756,12.2,8.96852544494693));
#237652=CARTESIAN_POINT('Ctrl Pts',(-5.55617938706234,12.2,8.96491386790956));
#237653=CARTESIAN_POINT('Ctrl Pts',(-5.55485425574631,12.2,8.9613464458006));
#237654=CARTESIAN_POINT('Ctrl Pts',(-5.5535347966272,12.2,8.95782356984224));
#237655=CARTESIAN_POINT('Ctrl Pts',(-5.55221533738825,12.2,8.9543006935639));
#237656=CARTESIAN_POINT('Ctrl Pts',(-5.5509015511998,12.2,8.95082236482315));
#237657=CARTESIAN_POINT('Ctrl Pts',(-5.54959405796215,12.2,8.94738897755463));
#237658=CARTESIAN_POINT('Ctrl Pts',(-5.54828656484325,12.2,8.94395559059797));
#237659=CARTESIAN_POINT('Ctrl Pts',(-5.54698536469283,12.2,8.94056714961191));
#237660=CARTESIAN_POINT('Ctrl Pts',(-5.54569109073397,12.2,8.9372240527181));
#237661=CARTESIAN_POINT('Ctrl Pts',(-5.54418110437024,12.2,8.93332377280619));
#237662=CARTESIAN_POINT('Ctrl Pts',(-5.5426805454644,12.2,8.92948521613576));
#237663=CARTESIAN_POINT('Ctrl Pts',(-5.5411904494138,12.2,8.92570903331536));
#237664=CARTESIAN_POINT('Ctrl Pts',(-5.53970035347921,12.2,8.92193285078899));
#237665=CARTESIAN_POINT('Ctrl Pts',(-5.538220717002,12.2,8.91821904147287));
#237666=CARTESIAN_POINT('Ctrl Pts',(-5.53675260612054,12.2,8.91456827209934));
#237667=CARTESIAN_POINT('Ctrl Pts',(-5.53549422521805,12.2,8.91143904084229));
#237668=CARTESIAN_POINT('Ctrl Pts',(-5.53424431178302,12.2,8.90835612258975));
#237669=CARTESIAN_POINT('Ctrl Pts',(-5.53300355488246,12.2,8.90531994634296));
#237670=CARTESIAN_POINT('Ctrl Pts',(-5.5317627980946,12.2,8.90228377037196));
#237671=CARTESIAN_POINT('Ctrl Pts',(-5.5305311975227,12.2,8.89929433457227));
#237672=CARTESIAN_POINT('Ctrl Pts',(-5.52930945706666,12.2,8.89635207467712));
#237673=CARTESIAN_POINT('Ctrl Pts',(-5.52808771661062,12.2,8.89340981478197));
#237674=CARTESIAN_POINT('Ctrl Pts',(-5.52687583869639,12.2,8.8905147286601));
#237675=CARTESIAN_POINT('Ctrl Pts',(-5.52567454615598,12.2,8.88766726076028));
#237676=CARTESIAN_POINT('Ctrl Pts',(-5.52447325350644,12.2,8.88481979260182));
#237677=CARTESIAN_POINT('Ctrl Pts',(-5.52328254651625,12.2,8.88201993990632));
#237678=CARTESIAN_POINT('Ctrl Pts',(-5.52210316795247,12.2,8.87926815584179));
#237679=CARTESIAN_POINT('Ctrl Pts',(-5.52072722645542,12.2,8.87605774147475));
#237680=CARTESIAN_POINT('Ctrl Pts',(-5.51936670204286,12.2,8.872912750883));
#237681=CARTESIAN_POINT('Ctrl Pts',(-5.51802281237559,12.2,8.86983391452923));
#237682=CARTESIAN_POINT('Ctrl Pts',(-5.51687090681198,12.2,8.86719491163209));
#237683=CARTESIAN_POINT('Ctrl Pts',(-5.51573122094952,12.2,8.86460451174798));
#237684=CARTESIAN_POINT('Ctrl Pts',(-5.51460454172202,12.2,8.8620631866116));
#237685=CARTESIAN_POINT('Ctrl Pts',(-5.51347786259685,12.2,8.85952186170608));
#237686=CARTESIAN_POINT('Ctrl Pts',(-5.5123641921156,12.2,8.85702960658179));
#237687=CARTESIAN_POINT('Ctrl Pts',(-5.51126433798386,12.2,8.85458690574268));
#237688=CARTESIAN_POINT('Ctrl Pts',(-5.51016448385213,12.2,8.85214420490356));
#237689=CARTESIAN_POINT('Ctrl Pts',(-5.50907844657921,12.2,8.84975105569927));
#237690=CARTESIAN_POINT('Ctrl Pts',(-5.50800705661713,12.2,8.84740794703099));
#237691=CARTESIAN_POINT('Ctrl Pts',(-5.50693566655775,12.2,8.84506483814988));
#237692=CARTESIAN_POINT('Ctrl Pts',(-5.50587892557387,12.2,8.84277177049773));
#237693=CARTESIAN_POINT('Ctrl Pts',(-5.50483768746601,12.2,8.84052924276642));
#237694=CARTESIAN_POINT('Ctrl Pts',(-5.50379644945272,12.2,8.83828671523881));
#237695=CARTESIAN_POINT('Ctrl Pts',(-5.50277071518834,12.2,8.83609472958039));
#237696=CARTESIAN_POINT('Ctrl Pts',(-5.50176136430836,12.2,8.83395379324156));
#237697=CARTESIAN_POINT('Ctrl Pts',(-5.50075201342838,12.2,8.83181285690271));
#237698=CARTESIAN_POINT('Ctrl Pts',(-5.49975904705876,12.2,8.82972297281965));
#237699=CARTESIAN_POINT('Ctrl Pts',(-5.49878337037779,12.2,8.82768466120553));
#237700=CARTESIAN_POINT('Ctrl Pts',(-5.49780769360818,12.2,8.82564634940626));
#237701=CARTESIAN_POINT('Ctrl Pts',(-5.49684930633088,12.2,8.82365961269094));
#237702=CARTESIAN_POINT('Ctrl Pts',(-5.49590914361422,12.2,8.82172498125569));
#237703=CARTESIAN_POINT('Ctrl Pts',(-5.49481228723953,12.2,8.81946791151152));
#237704=CARTESIAN_POINT('Ctrl Pts',(-5.49374023430851,12.2,8.81728176750281));
#237705=CARTESIAN_POINT('Ctrl Pts',(-5.49269451657012,12.2,8.81516741694201));
#237706=CARTESIAN_POINT('Ctrl Pts',(-5.49179818697538,12.2,8.81335511624967));
#237707=CARTESIAN_POINT('Ctrl Pts',(-5.49092120719362,12.2,8.81159556257829));
#237708=CARTESIAN_POINT('Ctrl Pts',(-5.49006457389832,12.2,8.80988932007226));
#237709=CARTESIAN_POINT('Ctrl Pts',(-5.48921205189506,12.2,8.80819126643918));
#237710=CARTESIAN_POINT('Ctrl Pts',(-5.48837968070687,12.2,8.80654601357679));
#237711=CARTESIAN_POINT('Ctrl Pts',(-5.48756848000005,12.2,8.80495412799998));
#237712=CARTESIAN_POINT('Ctrl Pts',(-5.48756848000005,15.2,8.80495412799998));
#237713=CARTESIAN_POINT('Ctrl Pts',(-5.48837968070687,15.2,8.80654601357679));
#237714=CARTESIAN_POINT('Ctrl Pts',(-5.48921205189504,15.2,8.80819126643915));
#237715=CARTESIAN_POINT('Ctrl Pts',(-5.49006457389831,15.2,8.80988932007225));
#237716=CARTESIAN_POINT('Ctrl Pts',(-5.49092120719362,15.2,8.8115955625783));
#237717=CARTESIAN_POINT('Ctrl Pts',(-5.49179818697536,15.2,8.81335511624963));
#237718=CARTESIAN_POINT('Ctrl Pts',(-5.49269451657011,15.2,8.81516741694201));
#237719=CARTESIAN_POINT('Ctrl Pts',(-5.49359084608345,15.2,8.81697971746977));
#237720=CARTESIAN_POINT('Ctrl Pts',(-5.49450652515063,15.2,8.81884476540288));
#237721=CARTESIAN_POINT('Ctrl Pts',(-5.49544058578336,15.2,8.82076201099989));
#237722=CARTESIAN_POINT('Ctrl Pts',(-5.49637464641609,15.2,8.82267925659689));
#237723=CARTESIAN_POINT('Ctrl Pts',(-5.49732709035238,15.2,8.82464870093832));
#237724=CARTESIAN_POINT('Ctrl Pts',(-5.49829697711458,15.2,8.82666980554617));
#237725=CARTESIAN_POINT('Ctrl Pts',(-5.49926686396487,15.2,8.82869091033763));
#237726=CARTESIAN_POINT('Ctrl Pts',(-5.50025419360363,15.2,8.83076367833718));
#237727=CARTESIAN_POINT('Ctrl Pts',(-5.50125805832612,15.2,8.83288758220641));
#237728=CARTESIAN_POINT('Ctrl Pts',(-5.50226192295742,15.2,8.8350114858827));
#237729=CARTESIAN_POINT('Ctrl Pts',(-5.50328231865006,15.2,8.83718652781323));
#237730=CARTESIAN_POINT('Ctrl Pts',(-5.5043183644505,15.2,8.83941219349258));
#237731=CARTESIAN_POINT('Ctrl Pts',(-5.50535441025094,15.2,8.84163785917193));
#237732=CARTESIAN_POINT('Ctrl Pts',(-5.50640610429802,15.2,8.84391414896002));
#237733=CARTESIAN_POINT('Ctrl Pts',(-5.5074725864253,15.2,8.84624056437332));
#237734=CARTESIAN_POINT('Ctrl Pts',(-5.50853906864946,15.2,8.84856697999794));
#237735=CARTESIAN_POINT('Ctrl Pts',(-5.50962034222604,15.2,8.85094351624675));
#237736=CARTESIAN_POINT('Ctrl Pts',(-5.51071556661954,15.2,8.85336968704797));
#237737=CARTESIAN_POINT('Ctrl Pts',(-5.51181079091355,15.2,8.85579585762881));
#237738=CARTESIAN_POINT('Ctrl Pts',(-5.51291996980978,15.2,8.85827166116062));
#237739=CARTESIAN_POINT('Ctrl Pts',(-5.51404229001959,15.2,8.86079661590439));
#237740=CARTESIAN_POINT('Ctrl Pts',(-5.51516461022939,15.2,8.86332157064815));
#237741=CARTESIAN_POINT('Ctrl Pts',(-5.51630007107144,15.2,8.86589567752959));
#237742=CARTESIAN_POINT('Ctrl Pts',(-5.51744788144586,15.2,8.86851846534883));
#237743=CARTESIAN_POINT('Ctrl Pts',(-5.51859569182028,15.2,8.87114125316808));
#237744=CARTESIAN_POINT('Ctrl Pts',(-5.5197558527907,15.2,8.87381272284725));
#237745=CARTESIAN_POINT('Ctrl Pts',(-5.52092759416398,15.2,8.87653241149513));
#237746=CARTESIAN_POINT('Ctrl Pts',(-5.52209933564371,15.2,8.87925210039004));
#237747=CARTESIAN_POINT('Ctrl Pts',(-5.52328265745795,15.2,8.88202000658138));
#237748=CARTESIAN_POINT('Ctrl Pts',(-5.52447681010683,15.2,8.88483568140355));
#237749=CARTESIAN_POINT('Ctrl Pts',(-5.52567096264723,15.2,8.88765135596996));
#237750=CARTESIAN_POINT('Ctrl Pts',(-5.52687594692147,15.2,8.89051479484123));
#237751=CARTESIAN_POINT('Ctrl Pts',(-5.52809103154949,15.2,8.89342555574859));
#237752=CARTESIAN_POINT('Ctrl Pts',(-5.52930611617751,15.2,8.89633631665595));
#237753=CARTESIAN_POINT('Ctrl Pts',(-5.53053130171095,15.2,8.89929439942638));
#237754=CARTESIAN_POINT('Ctrl Pts',(-5.53176587633214,15.2,8.90229936639737));
#237755=CARTESIAN_POINT('Ctrl Pts',(-5.53300045106547,15.2,8.90530433364132));
#237756=CARTESIAN_POINT('Ctrl Pts',(-5.53424441464971,15.2,8.90835618651478));
#237757=CARTESIAN_POINT('Ctrl Pts',(-5.53549707355168,15.2,8.91145449468562));
#237758=CARTESIAN_POINT('Ctrl Pts',(-5.53716728530718,15.2,8.91558557196529));
#237759=CARTESIAN_POINT('Ctrl Pts',(-5.53885295407835,15.2,8.91979923571209));
#237760=CARTESIAN_POINT('Ctrl Pts',(-5.54055248061121,15.2,8.92409449043401));
#237761=CARTESIAN_POINT('Ctrl Pts',(-5.5418271254819,15.2,8.9273159314023));
#237762=CARTESIAN_POINT('Ctrl Pts',(-5.54310956685195,15.2,8.93058326810023));
#237763=CARTESIAN_POINT('Ctrl Pts',(-5.54439914988813,15.2,8.93389608706122));
#237764=CARTESIAN_POINT('Ctrl Pts',(-5.54568873292429,15.2,8.9372089060222));
#237765=CARTESIAN_POINT('Ctrl Pts',(-5.54698545873912,15.2,8.94056720793066));
#237766=CARTESIAN_POINT('Ctrl Pts',(-5.548288685858,15.2,8.94397058688728));
#237767=CARTESIAN_POINT('Ctrl Pts',(-5.54959191309526,15.2,8.94737396615303));
#237768=CARTESIAN_POINT('Ctrl Pts',(-5.55090164314147,15.2,8.95082242237315));
#237769=CARTESIAN_POINT('Ctrl Pts',(-5.55221725129677,15.2,8.95431555748214));
#237770=CARTESIAN_POINT('Ctrl Pts',(-5.5537521272987,15.2,8.95839088130004));
#237771=CARTESIAN_POINT('Ctrl Pts',(-5.5552950027022,15.2,8.96252701461721));
#237772=CARTESIAN_POINT('Ctrl Pts',(-5.55684491256358,15.2,8.9667233371162));
#237773=CARTESIAN_POINT('Ctrl Pts',(-5.55817340688563,15.2,8.97032018539255));
#237774=CARTESIAN_POINT('Ctrl Pts',(-5.55950707039987,15.2,8.97396125362317));
#237775=CARTESIAN_POINT('Ctrl Pts',(-5.56084530680633,15.2,8.97764615424259));
#237776=CARTESIAN_POINT('Ctrl Pts',(-5.56218354309126,15.2,8.98133105452729));
#237777=CARTESIAN_POINT('Ctrl Pts',(-5.56352635542562,15.2,8.98505979070993));
#237778=CARTESIAN_POINT('Ctrl Pts',(-5.5648731617161,15.2,8.98883197783986));
#237779=CARTESIAN_POINT('Ctrl Pts',(-5.56599550033229,15.2,8.99197546722902));
#237780=CARTESIAN_POINT('Ctrl Pts',(-5.56712061307784,15.2,8.9951491329666));
#237781=CARTESIAN_POINT('Ctrl Pts',(-5.56824817175838,15.2,8.99835275650824));
#237782=CARTESIAN_POINT('Ctrl Pts',(-5.56937573043893,15.2,9.00155638004988));
#237783=CARTESIAN_POINT('Ctrl Pts',(-5.57050573425664,15.2,9.0047899622257));
#237784=CARTESIAN_POINT('Ctrl Pts',(-5.57163786127567,15.2,9.00805328751836));
#237785=CARTESIAN_POINT('Ctrl Pts',(-5.57276998829469,15.2,9.01131661281102));
#237786=CARTESIAN_POINT('Ctrl Pts',(-5.57390423831316,15.2,9.01460968192142));
#237787=CARTESIAN_POINT('Ctrl Pts',(-5.57504029379936,15.2,9.01793228220072));
#237788=CARTESIAN_POINT('Ctrl Pts',(-5.57617634928556,15.2,9.02125488248005));
#237789=CARTESIAN_POINT('Ctrl Pts',(-5.57731421228004,15.2,9.02460701374191));
#237790=CARTESIAN_POINT('Ctrl Pts',(-5.57845356859958,15.2,9.0279884656879));
#237791=CARTESIAN_POINT('Ctrl Pts',(-5.5795929249191,15.2,9.03136991763389));
#237792=CARTESIAN_POINT('Ctrl Pts',(-5.5807337767866,15.2,9.03478069173103));
#237793=CARTESIAN_POINT('Ctrl Pts',(-5.5818758173993,15.2,9.038220577391));
#237794=CARTESIAN_POINT('Ctrl Pts',(-5.58301785801198,15.2,9.04166046305097));
#237795=CARTESIAN_POINT('Ctrl Pts',(-5.58416108892741,15.2,9.04512946387174));
#237796=CARTESIAN_POINT('Ctrl Pts',(-5.58530520864971,15.2,9.04862737095745));
#237797=CARTESIAN_POINT('Ctrl Pts',(-5.586449328372,15.2,9.05212527804315));
#237798=CARTESIAN_POINT('Ctrl Pts',(-5.58759433792207,15.2,9.05565209412931));
#237799=CARTESIAN_POINT('Ctrl Pts',(-5.58873994111656,15.2,9.05920761371498));
#237800=CARTESIAN_POINT('Ctrl Pts',(-5.58988554418619,15.2,9.06276313291309));
#237801=CARTESIAN_POINT('Ctrl Pts',(-5.59103174240287,15.2,9.06634735731795));
#237802=CARTESIAN_POINT('Ctrl Pts',(-5.59217824533343,15.2,9.06996008476906));
#237803=CARTESIAN_POINT('Ctrl Pts',(-5.59332474838896,15.2,9.07357281261395));
#237804=CARTESIAN_POINT('Ctrl Pts',(-5.59447155673893,15.2,9.0772140417278));
#237805=CARTESIAN_POINT('Ctrl Pts',(-5.59561838410005,15.2,9.08088357700327));
#237806=CARTESIAN_POINT('Ctrl Pts',(-5.59699457700837,15.2,9.0852870195738));
#237807=CARTESIAN_POINT('Ctrl Pts',(-5.59837080003111,15.2,9.08973121982136));
#237808=CARTESIAN_POINT('Ctrl Pts',(-5.59974656892481,15.2,9.09421583687551));
#237809=CARTESIAN_POINT('Ctrl Pts',(-5.60112233769354,15.2,9.09870045352233));
#237810=CARTESIAN_POINT('Ctrl Pts',(-5.60249765169999,15.2,9.10322548737409));
#237811=CARTESIAN_POINT('Ctrl Pts',(-5.60387203948339,15.2,9.10779060345824));
#237812=CARTESIAN_POINT('Ctrl Pts',(-5.60501736267784,15.2,9.11159486699994));
#237813=CARTESIAN_POINT('Ctrl Pts',(-5.60616204281116,15.2,9.1154269623499));
#237814=CARTESIAN_POINT('Ctrl Pts',(-5.60730581024172,15.2,9.11928670172491));
#237815=CARTESIAN_POINT('Ctrl Pts',(-5.60844957767228,15.2,9.12314644109992));
#237816=CARTESIAN_POINT('Ctrl Pts',(-5.60959243311217,15.2,9.12703382065645));
#237817=CARTESIAN_POINT('Ctrl Pts',(-5.61073411228401,15.2,9.13094865178538));
#237818=CARTESIAN_POINT('Ctrl Pts',(-5.61187579145585,15.2,9.13486348291431));
#237819=CARTESIAN_POINT('Ctrl Pts',(-5.61301629485239,15.2,9.1388057639527));
#237820=CARTESIAN_POINT('Ctrl Pts',(-5.61415536228288,15.2,9.14277530700969));
#237821=CARTESIAN_POINT('Ctrl Pts',(-5.61529442971336,15.2,9.14674485006667));
#237822=CARTESIAN_POINT('Ctrl Pts',(-5.61643206056331,15.2,9.15074165550071));
#237823=CARTESIAN_POINT('Ctrl Pts',(-5.61756799979934,15.2,9.15476553432159));
#237824=CARTESIAN_POINT('Ctrl Pts',(-5.61847675111387,15.2,9.15798463711512));
#237825=CARTESIAN_POINT('Ctrl Pts',(-5.61938441988889,15.2,9.16122106714949));
#237826=CARTESIAN_POINT('Ctrl Pts',(-5.62029087836019,15.2,9.16447473004455));
#237827=CARTESIAN_POINT('Ctrl Pts',(-5.62165056625239,15.2,9.16935522505212));
#237828=CARTESIAN_POINT('Ctrl Pts',(-5.62300752557406,15.2,9.17427449394248));
#237829=CARTESIAN_POINT('Ctrl Pts',(-5.62436133164763,15.2,9.17923221579866));
#237830=CARTESIAN_POINT('Ctrl Pts',(-5.62548950331412,15.2,9.18336365045365));
#237831=CARTESIAN_POINT('Ctrl Pts',(-5.62661548441389,15.2,9.1875217914062));
#237832=CARTESIAN_POINT('Ctrl Pts',(-5.62773903191369,15.2,9.19170645279729));
#237833=CARTESIAN_POINT('Ctrl Pts',(-5.62863786984005,15.2,9.19505418163649));
#237834=CARTESIAN_POINT('Ctrl Pts',(-5.6295351495047,15.2,9.19841888476983));
#237835=CARTESIAN_POINT('Ctrl Pts',(-5.63043074949112,15.2,9.20180047006429));
#237836=CARTESIAN_POINT('Ctrl Pts',(-5.63132634959957,15.2,9.20518205581948));
#237837=CARTESIAN_POINT('Ctrl Pts',(-5.63222026960582,15.2,9.20858052142326));
#237838=CARTESIAN_POINT('Ctrl Pts',(-5.63311238715426,15.2,9.21199577733332));
#237839=CARTESIAN_POINT('Ctrl Pts',(-5.63400450458114,15.2,9.21541103277805));
#237840=CARTESIAN_POINT('Ctrl Pts',(-5.63489482026935,15.2,9.21884307782336));
#237841=CARTESIAN_POINT('Ctrl Pts',(-5.63578321491908,15.2,9.22229181998481));
#237842=CARTESIAN_POINT('Ctrl Pts',(-5.63667160968986,15.2,9.22574056261614));
#237843=CARTESIAN_POINT('Ctrl Pts',(-5.63755808296118,15.2,9.22920600362623));
#237844=CARTESIAN_POINT('Ctrl Pts',(-5.63844251588672,15.2,9.23268805171361));
#237845=CARTESIAN_POINT('Ctrl Pts',(-5.63932694869176,15.2,9.23617009932656));
#237846=CARTESIAN_POINT('Ctrl Pts',(-5.64020934203601,15.2,9.23966875339003));
#237847=CARTESIAN_POINT('Ctrl Pts',(-5.64108957868642,15.2,9.24318392421271));
#237848=CARTESIAN_POINT('Ctrl Pts',(-5.64196981545676,15.2,9.24669909551434));
#237849=CARTESIAN_POINT('Ctrl Pts',(-5.64284789486573,15.2,9.25023078388459));
#237850=CARTESIAN_POINT('Ctrl Pts',(-5.64372370307997,15.2,9.25377889852347));
#237851=CARTESIAN_POINT('Ctrl Pts',(-5.64459951117489,15.2,9.25732701267892));
#237852=CARTESIAN_POINT('Ctrl Pts',(-5.6454730461678,15.2,9.26089155483734));
#237853=CARTESIAN_POINT('Ctrl Pts',(-5.64634419614031,15.2,9.26447243322206));
#237854=CARTESIAN_POINT('Ctrl Pts',(-5.6472153462315,15.2,9.26805331209466));
#237855=CARTESIAN_POINT('Ctrl Pts',(-5.64808411009603,15.2,9.27165052980303));
#237856=CARTESIAN_POINT('Ctrl Pts',(-5.64895037558753,15.2,9.27526399577882));
#237857=CARTESIAN_POINT('Ctrl Pts',(-5.64981664096099,15.2,9.27887746126226));
#237858=CARTESIAN_POINT('Ctrl Pts',(-5.6506804058044,15.2,9.2825071761591));
#237859=CARTESIAN_POINT('Ctrl Pts',(-5.6515415625676,15.2,9.28615305163715));
#237860=CARTESIAN_POINT('Ctrl Pts',(-5.65240271944813,15.2,9.28979892761194));
#237861=CARTESIAN_POINT('Ctrl Pts',(-5.65326126612513,15.2,9.29346096444077));
#237862=CARTESIAN_POINT('Ctrl Pts',(-5.65411709300898,15.2,9.29713907443577));
#237863=CARTESIAN_POINT('Ctrl Pts',(-5.65497291977623,15.2,9.30081718392962));
#237864=CARTESIAN_POINT('Ctrl Pts',(-5.65582602800805,15.2,9.30451136711493));
#237865=CARTESIAN_POINT('Ctrl Pts',(-5.65667630682771,15.2,9.30822153714331));
#237866=CARTESIAN_POINT('Ctrl Pts',(-5.65752658576323,15.2,9.3119317076772));
#237867=CARTESIAN_POINT('Ctrl Pts',(-5.65837403603183,15.2,9.31565786302655));
#237868=CARTESIAN_POINT('Ctrl Pts',(-5.65921855096674,15.2,9.31939991950826));
#237869=CARTESIAN_POINT('Ctrl Pts',(-5.66027419457785,15.2,9.32407748985547));
#237870=CARTESIAN_POINT('Ctrl Pts',(-5.66132525094591,15.2,9.32877990219764));
#237871=CARTESIAN_POINT('Ctrl Pts',(-5.6623715144923,15.2,9.33350698951083));
#237872=CARTESIAN_POINT('Ctrl Pts',(-5.663208525261,15.2,9.33728865905223));
#237873=CARTESIAN_POINT('Ctrl Pts',(-5.66404246744295,15.2,9.34108612296205));
#237874=CARTESIAN_POINT('Ctrl Pts',(-5.66487323759757,15.2,9.34489929242647));
#237875=CARTESIAN_POINT('Ctrl Pts',(-5.66591170037575,15.2,9.34966575464665));
#237876=CARTESIAN_POINT('Ctrl Pts',(-5.66694520574292,15.2,9.35445675794985));
#237877=CARTESIAN_POINT('Ctrl Pts',(-5.66797355359056,15.2,9.35927213767007));
#237878=CARTESIAN_POINT('Ctrl Pts',(-5.66900190143821,15.2,9.36408751739028));
#237879=CARTESIAN_POINT('Ctrl Pts',(-5.67002509118624,15.2,9.36892727354967));
#237880=CARTESIAN_POINT('Ctrl Pts',(-5.67104292339023,15.2,9.37379124094371));
#237881=CARTESIAN_POINT('Ctrl Pts',(-5.6718571891978,15.2,9.37768241507101));
#237882=CARTESIAN_POINT('Ctrl Pts',(-5.67266802738892,15.2,9.38158908314757));
#237883=CARTESIAN_POINT('Ctrl Pts',(-5.67347533709937,15.2,9.38551116386238));
#237884=CARTESIAN_POINT('Ctrl Pts',(-5.67428264669981,15.2,9.3894332440428));
#237885=CARTESIAN_POINT('Ctrl Pts',(-5.67508642826762,15.2,9.39337073568389));
#237886=CARTESIAN_POINT('Ctrl Pts',(-5.67588658186924,15.2,9.39732355513697));
#237887=CARTESIAN_POINT('Ctrl Pts',(-5.67688677395304,15.2,9.40226457985725));
#237888=CARTESIAN_POINT('Ctrl Pts',(-5.67788129892583,15.2,9.40722955454376));
#237889=CARTESIAN_POINT('Ctrl Pts',(-5.67886996357909,15.2,9.41221831759741));
#237890=CARTESIAN_POINT('Ctrl Pts',(-5.67985862823235,15.2,9.41720708065103));
#237891=CARTESIAN_POINT('Ctrl Pts',(-5.68084143453745,15.2,9.42221963124322));
#237892=CARTESIAN_POINT('Ctrl Pts',(-5.68181819333666,15.2,9.42725581038204));
#237893=CARTESIAN_POINT('Ctrl Pts',(-5.68259960041862,15.2,9.43128475391268));
#237894=CARTESIAN_POINT('Ctrl Pts',(-5.68337713665193,15.2,9.43532881861802));
#237895=CARTESIAN_POINT('Ctrl Pts',(-5.68415070830494,15.2,9.43938792334023));
#237896=CARTESIAN_POINT('Ctrl Pts',(-5.68492427985255,15.2,9.44344702750939));
#237897=CARTESIAN_POINT('Ctrl Pts',(-5.68569388470651,15.2,9.44752117148939));
#237898=CARTESIAN_POINT('Ctrl Pts',(-5.68645943036657,15.2,9.45161027359803));
#237899=CARTESIAN_POINT('Ctrl Pts',(-5.68722497613093,15.2,9.45569937626379));
#237900=CARTESIAN_POINT('Ctrl Pts',(-5.68798646369477,15.2,9.45980343745117));
#237901=CARTESIAN_POINT('Ctrl Pts',(-5.68874379751725,15.2,9.46392237552773));
#237902=CARTESIAN_POINT('Ctrl Pts',(-5.68950113123655,15.2,9.46804131304309));
#237903=CARTESIAN_POINT('Ctrl Pts',(-5.69025431255785,15.2,9.47217512884282));
#237904=CARTESIAN_POINT('Ctrl Pts',(-5.69100324888595,15.2,9.47632373977996));
#237905=CARTESIAN_POINT('Ctrl Pts',(-5.69193941937261,15.2,9.48150950387533));
#237906=CARTESIAN_POINT('Ctrl Pts',(-5.69286895895104,15.2,9.4867183898619));
#237907=CARTESIAN_POINT('Ctrl Pts',(-5.69379168714604,15.2,9.49195023729061));
#237908=CARTESIAN_POINT('Ctrl Pts',(-5.69452986974229,15.2,9.49613571546169));
#237909=CARTESIAN_POINT('Ctrl Pts',(-5.69526369423808,15.2,9.50033589029004));
#237910=CARTESIAN_POINT('Ctrl Pts',(-5.69599307122557,15.2,9.50455068226113));
#237911=CARTESIAN_POINT('Ctrl Pts',(-5.69672244811368,15.2,9.50876547365795));
#237912=CARTESIAN_POINT('Ctrl Pts',(-5.69744737651016,15.2,9.51299488218227));
#237913=CARTESIAN_POINT('Ctrl Pts',(-5.69816776884062,15.2,9.51723882705605));
#237914=CARTESIAN_POINT('Ctrl Pts',(-5.69888816126923,15.2,9.52148277250805));
#237915=CARTESIAN_POINT('Ctrl Pts',(-5.6996040163502,15.2,9.52574125564758));
#237916=CARTESIAN_POINT('Ctrl Pts',(-5.70031524750007,15.2,9.53001419649159));
#237917=CARTESIAN_POINT('Ctrl Pts',(-5.70102647864994,15.2,9.53428713733559));
#237918=CARTESIAN_POINT('Ctrl Pts',(-5.70173308511039,15.2,9.53857453747291));
#237919=CARTESIAN_POINT('Ctrl Pts',(-5.70243498081483,15.2,9.54287631748663));
#237920=CARTESIAN_POINT('Ctrl Pts',(-5.70331235030193,15.2,9.54825354162458));
#237921=CARTESIAN_POINT('Ctrl Pts',(-5.70418235806398,15.2,9.55365323253357));
#237922=CARTESIAN_POINT('Ctrl Pts',(-5.70504483692893,15.2,9.55907524006574));
#237923=CARTESIAN_POINT('Ctrl Pts',(-5.70573482013369,15.2,9.56341284680066));
#237924=CARTESIAN_POINT('Ctrl Pts',(-5.70641998566856,15.2,9.56776473478698));
#237925=CARTESIAN_POINT('Ctrl Pts',(-5.70710024748341,15.2,9.57213082752493));
#237926=CARTESIAN_POINT('Ctrl Pts',(-5.70778050929827,15.2,9.57649692026288));
#237927=CARTESIAN_POINT('Ctrl Pts',(-5.70845586851532,15.2,9.58087721718862));
#237928=CARTESIAN_POINT('Ctrl Pts',(-5.70912624038468,15.2,9.58527164065176));
#237929=CARTESIAN_POINT('Ctrl Pts',(-5.70962901924102,15.2,9.58856745794975));
#237930=CARTESIAN_POINT('Ctrl Pts',(-5.71012899295645,15.2,9.59187122166135));
#237931=CARTESIAN_POINT('Ctrl Pts',(-5.7106261268379,15.2,9.5951828990824));
#237932=CARTESIAN_POINT('Ctrl Pts',(-5.71112326071935,15.2,9.59849457650346));
#237933=CARTESIAN_POINT('Ctrl Pts',(-5.71161755495503,15.2,9.60181416741631));
#237934=CARTESIAN_POINT('Ctrl Pts',(-5.71210897381193,15.2,9.60514164008776));
#237935=CARTESIAN_POINT('Ctrl Pts',(-5.71260039266882,15.2,9.60846911275921));
#237936=CARTESIAN_POINT('Ctrl Pts',(-5.71308893673439,15.2,9.61180446530472));
#237937=CARTESIAN_POINT('Ctrl Pts',(-5.71357457200841,15.2,9.61514766847493));
#237938=CARTESIAN_POINT('Ctrl Pts',(-5.71406020728244,15.2,9.61849087164514));
#237939=CARTESIAN_POINT('Ctrl Pts',(-5.71454293244824,15.2,9.62184192355668));
#237940=CARTESIAN_POINT('Ctrl Pts',(-5.71502271522273,15.2,9.62520079139228));
#237941=CARTESIAN_POINT('Ctrl Pts',(-5.71566242564682,15.2,9.62967928224652));
#237942=CARTESIAN_POINT('Ctrl Pts',(-5.71629690240109,15.2,9.63417167009037));
#237943=CARTESIAN_POINT('Ctrl Pts',(-5.71692606629968,15.2,9.63867787839555));
#237944=CARTESIAN_POINT('Ctrl Pts',(-5.71771252113005,15.2,9.64431063847005));
#237945=CARTESIAN_POINT('Ctrl Pts',(-5.71849067527367,15.2,9.64996499311837));
#237946=CARTESIAN_POINT('Ctrl Pts',(-5.71926037263409,15.2,9.65564079305067));
#237947=CARTESIAN_POINT('Ctrl Pts',(-5.71972219103355,15.2,9.65904627288631));
#237948=CARTESIAN_POINT('Ctrl Pts',(-5.72018096653319,15.2,9.66245947332991));
#237949=CARTESIAN_POINT('Ctrl Pts',(-5.72063666305803,15.2,9.66588036308127));
#237950=CARTESIAN_POINT('Ctrl Pts',(-5.72109235958287,15.2,9.66930125283264));
#237951=CARTESIAN_POINT('Ctrl Pts',(-5.72154497974812,15.2,9.67272983001225));
#237952=CARTESIAN_POINT('Ctrl Pts',(-5.72199448873382,15.2,9.67616606569472));
#237953=CARTESIAN_POINT('Ctrl Pts',(-5.72259383402086,15.2,9.68074771306325));
#237954=CARTESIAN_POINT('Ctrl Pts',(-5.72318765166253,15.2,9.68534297297453));
#237955=CARTESIAN_POINT('Ctrl Pts',(-5.72377586217057,15.2,9.68995176992973));
#237956=CARTESIAN_POINT('Ctrl Pts',(-5.72436407275876,15.2,9.69456056751288));
#237957=CARTESIAN_POINT('Ctrl Pts',(-5.72494667749919,15.2,9.69918290426117));
#237958=CARTESIAN_POINT('Ctrl Pts',(-5.72552359947508,15.2,9.70381870245827));
#237959=CARTESIAN_POINT('Ctrl Pts',(-5.7259562909177,15.2,9.70729555079027));
#237960=CARTESIAN_POINT('Ctrl Pts',(-5.7263857865021,15.2,9.71077997264693));
#237961=CARTESIAN_POINT('Ctrl Pts',(-5.72681205294523,15.2,9.71427193639443));
#237962=CARTESIAN_POINT('Ctrl Pts',(-5.72723831938836,15.2,9.71776390014192));
#237963=CARTESIAN_POINT('Ctrl Pts',(-5.7276613577794,15.2,9.72126340479125));
#237964=CARTESIAN_POINT('Ctrl Pts',(-5.7280811366605,15.2,9.72477042029647));
#237965=CARTESIAN_POINT('Ctrl Pts',(-5.72850091554159,15.2,9.7282774358017));
#237966=CARTESIAN_POINT('Ctrl Pts',(-5.72891743400788,15.2,9.73179196267777));
#237967=CARTESIAN_POINT('Ctrl Pts',(-5.72933066140999,15.2,9.73531396750714));
#237968=CARTESIAN_POINT('Ctrl Pts',(-5.72974388888716,15.2,9.73883597297633));
#237969=CARTESIAN_POINT('Ctrl Pts',(-5.73015382556341,15.2,9.74236545763926));
#237970=CARTESIAN_POINT('Ctrl Pts',(-5.73056043912205,15.2,9.74590239102933));
#237971=CARTESIAN_POINT('Ctrl Pts',(-5.73110259041047,15.2,9.75061830114518));
#237972=CARTESIAN_POINT('Ctrl Pts',(-5.73163883638298,15.2,9.75534745111485));
#237973=CARTESIAN_POINT('Ctrl Pts',(-5.73216910167334,15.2,9.76008976933737));
#237974=CARTESIAN_POINT('Ctrl Pts',(-5.73256680065918,15.2,9.76364650816578));
#237975=CARTESIAN_POINT('Ctrl Pts',(-5.73296113714526,15.2,9.76721065468546));
#237976=CARTESIAN_POINT('Ctrl Pts',(-5.73335207817319,15.2,9.77078217647135));
#237977=CARTESIAN_POINT('Ctrl Pts',(-5.73387333292443,15.2,9.77554420595173));
#237978=CARTESIAN_POINT('Ctrl Pts',(-5.73438855558706,15.2,9.78031934826769));
#237979=CARTESIAN_POINT('Ctrl Pts',(-5.73489767095043,15.2,9.78510753049486));
#237980=CARTESIAN_POINT('Ctrl Pts',(-5.73527950743827,15.2,9.78869866683903));
#237981=CARTESIAN_POINT('Ctrl Pts',(-5.73565790982831,15.2,9.79229713869466));
#237982=CARTESIAN_POINT('Ctrl Pts',(-5.73603284773307,15.2,9.79590291403834));
#237983=CARTESIAN_POINT('Ctrl Pts',(-5.73640778563784,15.2,9.79950868938202));
#237984=CARTESIAN_POINT('Ctrl Pts',(-5.73677925878964,15.2,9.80312176930429));
#237985=CARTESIAN_POINT('Ctrl Pts',(-5.73714723769324,15.2,9.80674212263043));
#237986=CARTESIAN_POINT('Ctrl Pts',(-5.73751521659685,15.2,9.81036247595658));
#237987=CARTESIAN_POINT('Ctrl Pts',(-5.73787970076735,15.2,9.8139901034239));
#237988=CARTESIAN_POINT('Ctrl Pts',(-5.73824066167139,15.2,9.81762497379087));
#237989=CARTESIAN_POINT('Ctrl Pts',(-5.738601622641,15.2,9.82125984481817));
#237990=CARTESIAN_POINT('Ctrl Pts',(-5.73895905982627,15.2,9.82490195918079));
#237991=CARTESIAN_POINT('Ctrl Pts',(-5.73931294383556,15.2,9.82855128625383));
#237992=CARTESIAN_POINT('Ctrl Pts',(-5.73966682778055,15.2,9.83220061266392));
#237993=CARTESIAN_POINT('Ctrl Pts',(-5.74001715879615,15.2,9.83585715292475));
#237994=CARTESIAN_POINT('Ctrl Pts',(-5.74036390684213,15.2,9.83952087493385));
#237995=CARTESIAN_POINT('Ctrl Pts',(-5.74094182027308,15.2,9.84562707850421));
#237996=CARTESIAN_POINT('Ctrl Pts',(-5.7415097845072,15.2,9.8517532334744));
#237997=CARTESIAN_POINT('Ctrl Pts',(-5.74206766283972,15.2,9.85789919854551));
#237998=CARTESIAN_POINT('Ctrl Pts',(-5.74240238982707,15.2,9.86158677745418));
#237999=CARTESIAN_POINT('Ctrl Pts',(-5.74273348638127,15.2,9.86528148937079));
#238000=CARTESIAN_POINT('Ctrl Pts',(-5.74306092528571,15.2,9.86898330415355));
#238001=CARTESIAN_POINT('Ctrl Pts',(-5.74338836419016,15.2,9.8726851189363));
#238002=CARTESIAN_POINT('Ctrl Pts',(-5.74371214432723,15.2,9.8763940359381));
#238003=CARTESIAN_POINT('Ctrl Pts',(-5.74403223727537,15.2,9.88011002473664));
#238004=CARTESIAN_POINT('Ctrl Pts',(-5.7444590278535,15.2,9.88506467624303));
#238005=CARTESIAN_POINT('Ctrl Pts',(-5.74487926264892,15.2,9.89003189909693));
#238006=CARTESIAN_POINT('Ctrl Pts',(-5.74529287394912,15.2,9.89501162141076));
#238007=CARTESIAN_POINT('Ctrl Pts',(-5.74560308249471,15.2,9.89874641399425));
#238008=CARTESIAN_POINT('Ctrl Pts',(-5.74590956580592,15.2,9.90248823867143));
#238009=CARTESIAN_POINT('Ctrl Pts',(-5.74621229984941,15.2,9.90623706775886));
#238010=CARTESIAN_POINT('Ctrl Pts',(-5.74651503383789,15.2,9.90998589616525));
#238011=CARTESIAN_POINT('Ctrl Pts',(-5.74681401800992,15.2,9.91374173087964));
#238012=CARTESIAN_POINT('Ctrl Pts',(-5.74710922349887,15.2,9.91750453866021));
#238013=CARTESIAN_POINT('Ctrl Pts',(-5.74740442898781,15.2,9.92126734644077));
#238014=CARTESIAN_POINT('Ctrl Pts',(-5.7476958564595,15.2,9.92503712840675));
#238015=CARTESIAN_POINT('Ctrl Pts',(-5.74798346995034,15.2,9.92881384624504));
#238016=CARTESIAN_POINT('Ctrl Pts',(-5.74836695458738,15.2,9.93384946980072));
#238017=CARTESIAN_POINT('Ctrl Pts',(-5.74874365740803,15.2,9.93889742376812));
#238018=CARTESIAN_POINT('Ctrl Pts',(-5.74911352715627,15.2,9.94395764863093));
#238019=CARTESIAN_POINT('Ctrl Pts',(-5.7494833969549,15.2,9.94901787418319));
#238020=CARTESIAN_POINT('Ctrl Pts',(-5.74984644090299,15.2,9.95409037794774));
#238021=CARTESIAN_POINT('Ctrl Pts',(-5.75020264100006,15.2,9.95917514599999));
#238022=CARTESIAN_POINT('Ctrl Pts',(-4.57383771200006,15.2,9.31239140099999));
#238023=CARTESIAN_POINT('Ctrl Pts',(-4.57383771200006,11.6,9.31239140099999));
#238024=CARTESIAN_POINT('Ctrl Pts',(-4.57392774300006,15.2,9.31254071599999));
#238025=CARTESIAN_POINT('Ctrl Pts',(-4.57392774300006,11.6,9.31254071599999));
#238026=CARTESIAN_POINT('Ctrl Pts',(-4.57411102300005,15.2,9.31284451799998));
#238027=CARTESIAN_POINT('Ctrl Pts',(-4.57411102300005,11.6,9.31284451799998));
#238028=CARTESIAN_POINT('Ctrl Pts',(-4.57438896300006,15.2,9.31330471299999));
#238029=CARTESIAN_POINT('Ctrl Pts',(-4.57438896300006,11.6,9.31330471299999));
#238030=CARTESIAN_POINT('Ctrl Pts',(-4.57476383600006,15.2,9.31392435799999));
#238031=CARTESIAN_POINT('Ctrl Pts',(-4.57476383600006,11.6,9.31392435799999));
#238032=CARTESIAN_POINT('Ctrl Pts',(-4.57523877600006,15.2,9.31470764399998));
#238033=CARTESIAN_POINT('Ctrl Pts',(-4.57523877600006,11.6,9.31470764399998));
#238034=CARTESIAN_POINT('Ctrl Pts',(-4.57572221400006,15.2,9.31550313999999));
#238035=CARTESIAN_POINT('Ctrl Pts',(-4.57572221400006,11.6,9.31550313999999));
#238036=CARTESIAN_POINT('Ctrl Pts',(-4.57621139800006,15.2,9.31630627599999));
#238037=CARTESIAN_POINT('Ctrl Pts',(-4.57621139800006,11.6,9.31630627599999));
#238038=CARTESIAN_POINT('Ctrl Pts',(-4.57670633000006,15.2,9.31711702099999));
#238039=CARTESIAN_POINT('Ctrl Pts',(-4.57670633000006,11.6,9.31711702099999));
#238040=CARTESIAN_POINT('Ctrl Pts',(-4.57720701300006,15.2,9.31793534099998));
#238041=CARTESIAN_POINT('Ctrl Pts',(-4.57720701300006,11.6,9.31793534099998));
#238042=CARTESIAN_POINT('Ctrl Pts',(-4.57771344700006,15.2,9.31876120399998));
#238043=CARTESIAN_POINT('Ctrl Pts',(-4.57771344700006,11.6,9.31876120399998));
#238044=CARTESIAN_POINT('Ctrl Pts',(-4.57822563400006,15.2,9.31959457899998));
#238045=CARTESIAN_POINT('Ctrl Pts',(-4.57822563400006,11.6,9.31959457899998));
#238046=CARTESIAN_POINT('Ctrl Pts',(-4.57874357500006,15.2,9.32043543399999));
#238047=CARTESIAN_POINT('Ctrl Pts',(-4.57874357500006,11.6,9.32043543399999));
#238048=CARTESIAN_POINT('Ctrl Pts',(-4.57926727100006,15.2,9.32128373599999));
#238049=CARTESIAN_POINT('Ctrl Pts',(-4.57926727100006,11.6,9.32128373599999));
#238050=CARTESIAN_POINT('Ctrl Pts',(-4.57979672400006,15.2,9.32213945399998));
#238051=CARTESIAN_POINT('Ctrl Pts',(-4.57979672400006,11.6,9.32213945399998));
#238052=CARTESIAN_POINT('Ctrl Pts',(-4.58033193500006,15.2,9.32300255699998));
#238053=CARTESIAN_POINT('Ctrl Pts',(-4.58033193500006,11.6,9.32300255699998));
#238054=CARTESIAN_POINT('Ctrl Pts',(-4.58087290500006,15.2,9.32387301399999));
#238055=CARTESIAN_POINT('Ctrl Pts',(-4.58087290500006,11.6,9.32387301399999));
#238056=CARTESIAN_POINT('Ctrl Pts',(-4.58141963700006,15.2,9.32475079299999));
#238057=CARTESIAN_POINT('Ctrl Pts',(-4.58141963700006,11.6,9.32475079299999));
#238058=CARTESIAN_POINT('Ctrl Pts',(-4.58197213000005,15.2,9.32563586399999));
#238059=CARTESIAN_POINT('Ctrl Pts',(-4.58197213000005,11.6,9.32563586399999));
#238060=CARTESIAN_POINT('Ctrl Pts',(-4.58253038600006,15.2,9.32652819599999));
#238061=CARTESIAN_POINT('Ctrl Pts',(-4.58253038600006,11.6,9.32652819599999));
#238062=CARTESIAN_POINT('Ctrl Pts',(-4.58309440700006,15.2,9.32742775599999));
#238063=CARTESIAN_POINT('Ctrl Pts',(-4.58309440700006,11.6,9.32742775599999));
#238064=CARTESIAN_POINT('Ctrl Pts',(-4.58366419400006,15.2,9.32833451799999));
#238065=CARTESIAN_POINT('Ctrl Pts',(-4.58366419400006,11.6,9.32833451799999));
#238066=CARTESIAN_POINT('Ctrl Pts',(-4.58423974600006,15.2,9.32924844799999));
#238067=CARTESIAN_POINT('Ctrl Pts',(-4.58423974600006,11.6,9.32924844799999));
#238068=CARTESIAN_POINT('Ctrl Pts',(-4.58482106700006,15.2,9.33016951699998));
#238069=CARTESIAN_POINT('Ctrl Pts',(-4.58482106700006,11.6,9.33016951699998));
#238070=CARTESIAN_POINT('Ctrl Pts',(-4.58540815800006,15.2,9.33109769499998));
#238071=CARTESIAN_POINT('Ctrl Pts',(-4.58540815800006,11.6,9.33109769499998));
#238072=CARTESIAN_POINT('Ctrl Pts',(-4.58600101700006,15.2,9.33203295199998));
#238073=CARTESIAN_POINT('Ctrl Pts',(-4.58600101700006,11.6,9.33203295199998));
#238074=CARTESIAN_POINT('Ctrl Pts',(-4.58659964900006,15.2,9.33297525799999));
#238075=CARTESIAN_POINT('Ctrl Pts',(-4.58659964900006,11.6,9.33297525799999));
#238076=CARTESIAN_POINT('Ctrl Pts',(-4.58720405300006,15.2,9.33392458399998));
#238077=CARTESIAN_POINT('Ctrl Pts',(-4.58720405300006,11.6,9.33392458399998));
#238078=CARTESIAN_POINT('Ctrl Pts',(-4.58781423100006,15.2,9.33488089999998));
#238079=CARTESIAN_POINT('Ctrl Pts',(-4.58781423100006,11.6,9.33488089999998));
#238080=CARTESIAN_POINT('Ctrl Pts',(-4.58843018200006,15.2,9.33584417599998));
#238081=CARTESIAN_POINT('Ctrl Pts',(-4.58843018200006,11.6,9.33584417599998));
#238082=CARTESIAN_POINT('Ctrl Pts',(-4.58905191000006,15.2,9.33681438399999));
#238083=CARTESIAN_POINT('Ctrl Pts',(-4.58905191000006,11.6,9.33681438399999));
#238084=CARTESIAN_POINT('Ctrl Pts',(-4.58967941300005,15.2,9.33779149299999));
#238085=CARTESIAN_POINT('Ctrl Pts',(-4.58967941300005,11.6,9.33779149299999));
#238086=CARTESIAN_POINT('Ctrl Pts',(-4.59031269500006,15.2,9.33877547699998));
#238087=CARTESIAN_POINT('Ctrl Pts',(-4.59031269500006,11.6,9.33877547699998));
#238088=CARTESIAN_POINT('Ctrl Pts',(-4.59095175400006,15.2,9.33976630499998));
#238089=CARTESIAN_POINT('Ctrl Pts',(-4.59095175400006,11.6,9.33976630499998));
#238090=CARTESIAN_POINT('Ctrl Pts',(-4.59159659200005,15.2,9.34076394799998));
#238091=CARTESIAN_POINT('Ctrl Pts',(-4.59159659200005,11.6,9.34076394799998));
#238092=CARTESIAN_POINT('Ctrl Pts',(-4.59224721200005,15.2,9.34176837899999));
#238093=CARTESIAN_POINT('Ctrl Pts',(-4.59224721200005,11.6,9.34176837899999));
#238094=CARTESIAN_POINT('Ctrl Pts',(-4.59290361300006,15.2,9.34277956799999));
#238095=CARTESIAN_POINT('Ctrl Pts',(-4.59290361300006,11.6,9.34277956799999));
#238096=CARTESIAN_POINT('Ctrl Pts',(-4.59356579600006,15.2,9.34379748799999));
#238097=CARTESIAN_POINT('Ctrl Pts',(-4.59356579600006,11.6,9.34379748799999));
#238098=CARTESIAN_POINT('Ctrl Pts',(-4.59423376100006,15.2,9.34482210999998));
#238099=CARTESIAN_POINT('Ctrl Pts',(-4.59423376100006,11.6,9.34482210999998));
#238100=CARTESIAN_POINT('Ctrl Pts',(-4.59490751000006,15.2,9.34585340599998));
#238101=CARTESIAN_POINT('Ctrl Pts',(-4.59490751000006,11.6,9.34585340599998));
#238102=CARTESIAN_POINT('Ctrl Pts',(-4.59558704400005,15.2,9.34689134799999));
#238103=CARTESIAN_POINT('Ctrl Pts',(-4.59558704400005,11.6,9.34689134799999));
#238104=CARTESIAN_POINT('Ctrl Pts',(-4.59627236400006,15.2,9.34793590899999));
#238105=CARTESIAN_POINT('Ctrl Pts',(-4.59627236400006,11.6,9.34793590899999));
#238106=CARTESIAN_POINT('Ctrl Pts',(-4.59696347000006,15.2,9.34898706099998));
#238107=CARTESIAN_POINT('Ctrl Pts',(-4.59696347000006,11.6,9.34898706099998));
#238108=CARTESIAN_POINT('Ctrl Pts',(-4.59766036300006,15.2,9.35004477499999));
#238109=CARTESIAN_POINT('Ctrl Pts',(-4.59766036300006,11.6,9.35004477499999));
#238110=CARTESIAN_POINT('Ctrl Pts',(-4.59836304400006,15.2,9.35110902499999));
#238111=CARTESIAN_POINT('Ctrl Pts',(-4.59836304400006,11.6,9.35110902499999));
#238112=CARTESIAN_POINT('Ctrl Pts',(-4.59907151400006,15.2,9.35217978299999));
#238113=CARTESIAN_POINT('Ctrl Pts',(-4.59907151400006,11.6,9.35217978299999));
#238114=CARTESIAN_POINT('Ctrl Pts',(-4.59978577200006,15.2,9.35325702199999));
#238115=CARTESIAN_POINT('Ctrl Pts',(-4.59978577200006,11.6,9.35325702199999));
#238116=CARTESIAN_POINT('Ctrl Pts',(-4.60050582200005,15.2,9.35434071699999));
#238117=CARTESIAN_POINT('Ctrl Pts',(-4.60050582200005,11.6,9.35434071699999));
#238118=CARTESIAN_POINT('Ctrl Pts',(-4.60123166200006,15.2,9.35543083699999));
#238119=CARTESIAN_POINT('Ctrl Pts',(-4.60123166200006,11.6,9.35543083699999));
#238120=CARTESIAN_POINT('Ctrl Pts',(-4.60196329300006,15.2,9.35652735799999));
#238121=CARTESIAN_POINT('Ctrl Pts',(-4.60196329300006,11.6,9.35652735799999));
#238122=CARTESIAN_POINT('Ctrl Pts',(-4.60270071600006,15.2,9.35763025299998));
#238123=CARTESIAN_POINT('Ctrl Pts',(-4.60270071600006,11.6,9.35763025299998));
#238124=CARTESIAN_POINT('Ctrl Pts',(-4.60344393200006,15.2,9.35873949499998));
#238125=CARTESIAN_POINT('Ctrl Pts',(-4.60344393200006,11.6,9.35873949499998));
#238126=CARTESIAN_POINT('Ctrl Pts',(-4.60419294300006,15.2,9.35985505699998));
#238127=CARTESIAN_POINT('Ctrl Pts',(-4.60419294300006,11.6,9.35985505699998));
#238128=CARTESIAN_POINT('Ctrl Pts',(-4.60494774600006,15.2,9.36097691299998));
#238129=CARTESIAN_POINT('Ctrl Pts',(-4.60494774600006,11.6,9.36097691299998));
#238130=CARTESIAN_POINT('Ctrl Pts',(-4.60570834500006,15.2,9.36210503599998));
#238131=CARTESIAN_POINT('Ctrl Pts',(-4.60570834500006,11.6,9.36210503599998));
#238132=CARTESIAN_POINT('Ctrl Pts',(-4.60647473900006,15.2,9.36323940099999));
#238133=CARTESIAN_POINT('Ctrl Pts',(-4.60647473900006,11.6,9.36323940099999));
#238134=CARTESIAN_POINT('Ctrl Pts',(-4.60724692800006,15.2,9.36437998099999));
#238135=CARTESIAN_POINT('Ctrl Pts',(-4.60724692800006,11.6,9.36437998099999));
#238136=CARTESIAN_POINT('Ctrl Pts',(-4.60802491400006,15.2,9.36552675199999));
#238137=CARTESIAN_POINT('Ctrl Pts',(-4.60802491400006,11.6,9.36552675199999));
#238138=CARTESIAN_POINT('Ctrl Pts',(-4.60880869800006,15.2,9.36667968599998));
#238139=CARTESIAN_POINT('Ctrl Pts',(-4.60880869800006,11.6,9.36667968599998));
#238140=CARTESIAN_POINT('Ctrl Pts',(-4.60959827800006,15.2,9.36783875799998));
#238141=CARTESIAN_POINT('Ctrl Pts',(-4.60959827800006,11.6,9.36783875799998));
#238142=CARTESIAN_POINT('Ctrl Pts',(-4.61039365600006,15.2,9.36900394299998));
#238143=CARTESIAN_POINT('Ctrl Pts',(-4.61039365600006,11.6,9.36900394299998));
#238144=CARTESIAN_POINT('Ctrl Pts',(-4.61119483300005,15.2,9.37017521399999));
#238145=CARTESIAN_POINT('Ctrl Pts',(-4.61119483300005,11.6,9.37017521399999));
#238146=CARTESIAN_POINT('Ctrl Pts',(-4.61200180900006,15.2,9.37135254599998));
#238147=CARTESIAN_POINT('Ctrl Pts',(-4.61200180900006,11.6,9.37135254599998));
#238148=CARTESIAN_POINT('Ctrl Pts',(-4.61281458500006,15.2,9.37253591599998));
#238149=CARTESIAN_POINT('Ctrl Pts',(-4.61281458500006,11.6,9.37253591599998));
#238150=CARTESIAN_POINT('Ctrl Pts',(-4.61363316000006,15.2,9.37372529599998));
#238151=CARTESIAN_POINT('Ctrl Pts',(-4.61363316000006,11.6,9.37372529599998));
#238152=CARTESIAN_POINT('Ctrl Pts',(-4.61445753500006,15.2,9.37492066099999));
#238153=CARTESIAN_POINT('Ctrl Pts',(-4.61445753500006,11.6,9.37492066099999));
#238154=CARTESIAN_POINT('Ctrl Pts',(-4.61528771100006,15.2,9.37612198899998));
#238155=CARTESIAN_POINT('Ctrl Pts',(-4.61528771100006,11.6,9.37612198899998));
#238156=CARTESIAN_POINT('Ctrl Pts',(-4.61612368800006,15.2,9.37732925099999));
#238157=CARTESIAN_POINT('Ctrl Pts',(-4.61612368800006,11.6,9.37732925099999));
#238158=CARTESIAN_POINT('Ctrl Pts',(-4.61696546700006,15.2,9.37854242499998));
#238159=CARTESIAN_POINT('Ctrl Pts',(-4.61696546700006,11.6,9.37854242499998));
#238160=CARTESIAN_POINT('Ctrl Pts',(-4.61781304700006,15.2,9.37976148599999));
#238161=CARTESIAN_POINT('Ctrl Pts',(-4.61781304700006,11.6,9.37976148599999));
#238162=CARTESIAN_POINT('Ctrl Pts',(-4.61866643000006,15.2,9.38098640999998));
#238163=CARTESIAN_POINT('Ctrl Pts',(-4.61866643000006,11.6,9.38098640999998));
#238164=CARTESIAN_POINT('Ctrl Pts',(-4.61952561600006,15.2,9.38221716999998));
#238165=CARTESIAN_POINT('Ctrl Pts',(-4.61952561600006,11.6,9.38221716999998));
#238166=CARTESIAN_POINT('Ctrl Pts',(-4.62039060400006,15.2,9.38345374299999));
#238167=CARTESIAN_POINT('Ctrl Pts',(-4.62039060400006,11.6,9.38345374299999));
#238168=CARTESIAN_POINT('Ctrl Pts',(-4.62126139600006,15.2,9.38469610499999));
#238169=CARTESIAN_POINT('Ctrl Pts',(-4.62126139600006,11.6,9.38469610499999));
#238170=CARTESIAN_POINT('Ctrl Pts',(-4.62213799200006,15.2,9.38594423299998));
#238171=CARTESIAN_POINT('Ctrl Pts',(-4.62213799200006,11.6,9.38594423299998));
#238172=CARTESIAN_POINT('Ctrl Pts',(-4.62302039000006,15.2,9.38719810099998));
#238173=CARTESIAN_POINT('Ctrl Pts',(-4.62302039000006,11.6,9.38719810099998));
#238174=CARTESIAN_POINT('Ctrl Pts',(-4.62390859300006,15.2,9.38845768599998));
#238175=CARTESIAN_POINT('Ctrl Pts',(-4.62390859300006,11.6,9.38845768599998));
#238176=CARTESIAN_POINT('Ctrl Pts',(-4.62480260100006,15.2,9.38972296299998));
#238177=CARTESIAN_POINT('Ctrl Pts',(-4.62480260100006,11.6,9.38972296299998));
#238178=CARTESIAN_POINT('Ctrl Pts',(-4.62570241200006,15.2,9.39099390799999));
#238179=CARTESIAN_POINT('Ctrl Pts',(-4.62570241200006,11.6,9.39099390799999));
#238180=CARTESIAN_POINT('Ctrl Pts',(-4.62660802900006,15.2,9.39227049999998));
#238181=CARTESIAN_POINT('Ctrl Pts',(-4.62660802900006,11.6,9.39227049999998));
#238182=CARTESIAN_POINT('Ctrl Pts',(-4.62751945100006,15.2,9.39355271299998));
#238183=CARTESIAN_POINT('Ctrl Pts',(-4.62751945100006,11.6,9.39355271299998));
#238184=CARTESIAN_POINT('Ctrl Pts',(-4.62843667800006,15.2,9.39484052499999));
#238185=CARTESIAN_POINT('Ctrl Pts',(-4.62843667800006,11.6,9.39484052499999));
#238186=CARTESIAN_POINT('Ctrl Pts',(-4.62935971000006,15.2,9.39613391099999));
#238187=CARTESIAN_POINT('Ctrl Pts',(-4.62935971000006,11.6,9.39613391099999));
#238188=CARTESIAN_POINT('Ctrl Pts',(-4.63028854800006,15.2,9.39743284799999));
#238189=CARTESIAN_POINT('Ctrl Pts',(-4.63028854800006,11.6,9.39743284799999));
#238190=CARTESIAN_POINT('Ctrl Pts',(-4.63122319200005,15.2,9.39873731299999));
#238191=CARTESIAN_POINT('Ctrl Pts',(-4.63122319200005,11.6,9.39873731299999));
#238192=CARTESIAN_POINT('Ctrl Pts',(-4.63216364200006,15.2,9.40004728399998));
#238193=CARTESIAN_POINT('Ctrl Pts',(-4.63216364200006,11.6,9.40004728399998));
#238194=CARTESIAN_POINT('Ctrl Pts',(-4.63310989700005,15.2,9.40136273599999));
#238195=CARTESIAN_POINT('Ctrl Pts',(-4.63310989700005,11.6,9.40136273599999));
#238196=CARTESIAN_POINT('Ctrl Pts',(-4.63406195900006,15.2,9.40268364799999));
#238197=CARTESIAN_POINT('Ctrl Pts',(-4.63406195900006,11.6,9.40268364799999));
#238198=CARTESIAN_POINT('Ctrl Pts',(-4.63501982700006,15.2,9.40400999499998));
#238199=CARTESIAN_POINT('Ctrl Pts',(-4.63501982700006,11.6,9.40400999499998));
#238200=CARTESIAN_POINT('Ctrl Pts',(-4.63598350100006,15.2,9.40534175599998));
#238201=CARTESIAN_POINT('Ctrl Pts',(-4.63598350100006,11.6,9.40534175599998));
#238202=CARTESIAN_POINT('Ctrl Pts',(-4.63695298200006,15.2,9.40667890699999));
#238203=CARTESIAN_POINT('Ctrl Pts',(-4.63695298200006,11.6,9.40667890699999));
#238204=CARTESIAN_POINT('Ctrl Pts',(-4.63792827000006,15.2,9.40802142699999));
#238205=CARTESIAN_POINT('Ctrl Pts',(-4.63792827000006,11.6,9.40802142699999));
#238206=CARTESIAN_POINT('Ctrl Pts',(-4.63890936300006,15.2,9.40936929099998));
#238207=CARTESIAN_POINT('Ctrl Pts',(-4.63890936300006,11.6,9.40936929099998));
#238208=CARTESIAN_POINT('Ctrl Pts',(-4.63989626400005,15.2,9.41072247999998));
#238209=CARTESIAN_POINT('Ctrl Pts',(-4.63989626400005,11.6,9.41072247999998));
#238210=CARTESIAN_POINT('Ctrl Pts',(-4.64088897100006,15.2,9.41208096799999));
#238211=CARTESIAN_POINT('Ctrl Pts',(-4.64088897100006,11.6,9.41208096799999));
#238212=CARTESIAN_POINT('Ctrl Pts',(-4.64188748400006,15.2,9.41344473399998));
#238213=CARTESIAN_POINT('Ctrl Pts',(-4.64188748400006,11.6,9.41344473399998));
#238214=CARTESIAN_POINT('Ctrl Pts',(-4.64289180500006,15.2,9.41481375799999));
#238215=CARTESIAN_POINT('Ctrl Pts',(-4.64289180500006,11.6,9.41481375799999));
#238216=CARTESIAN_POINT('Ctrl Pts',(-4.64390193100006,15.2,9.41618801499999));
#238217=CARTESIAN_POINT('Ctrl Pts',(-4.64390193100006,11.6,9.41618801499999));
#238218=CARTESIAN_POINT('Ctrl Pts',(-4.64491786500006,15.2,9.41756748299999));
#238219=CARTESIAN_POINT('Ctrl Pts',(-4.64491786500006,11.6,9.41756748299999));
#238220=CARTESIAN_POINT('Ctrl Pts',(-4.64593960400006,15.2,9.41895214299999));
#238221=CARTESIAN_POINT('Ctrl Pts',(-4.64593960400006,11.6,9.41895214299999));
#238222=CARTESIAN_POINT('Ctrl Pts',(-4.64696715100006,15.2,9.42034196999998));
#238223=CARTESIAN_POINT('Ctrl Pts',(-4.64696715100006,11.6,9.42034196999998));
#238224=CARTESIAN_POINT('Ctrl Pts',(-4.64800050300005,15.2,9.42173694399998));
#238225=CARTESIAN_POINT('Ctrl Pts',(-4.64800050300005,11.6,9.42173694399998));
#238226=CARTESIAN_POINT('Ctrl Pts',(-4.64903966300006,15.2,9.42313704299998));
#238227=CARTESIAN_POINT('Ctrl Pts',(-4.64903966300006,11.6,9.42313704299998));
#238228=CARTESIAN_POINT('Ctrl Pts',(-4.65008462800006,15.2,9.42454224399999));
#238229=CARTESIAN_POINT('Ctrl Pts',(-4.65008462800006,11.6,9.42454224399999));
#238230=CARTESIAN_POINT('Ctrl Pts',(-4.65113540000006,15.2,9.42595252799999));
#238231=CARTESIAN_POINT('Ctrl Pts',(-4.65113540000006,11.6,9.42595252799999));
#238232=CARTESIAN_POINT('Ctrl Pts',(-4.65219197700006,15.2,9.42736787099999));
#238233=CARTESIAN_POINT('Ctrl Pts',(-4.65219197700006,11.6,9.42736787099999));
#238234=CARTESIAN_POINT('Ctrl Pts',(-4.65325436000006,15.2,9.42878825399998));
#238235=CARTESIAN_POINT('Ctrl Pts',(-4.65325436000006,11.6,9.42878825399998));
#238236=CARTESIAN_POINT('Ctrl Pts',(-4.65432255000006,15.2,9.43021365399999));
#238237=CARTESIAN_POINT('Ctrl Pts',(-4.65432255000006,11.6,9.43021365399999));
#238238=CARTESIAN_POINT('Ctrl Pts',(-4.65539654500006,15.2,9.43164404899999));
#238239=CARTESIAN_POINT('Ctrl Pts',(-4.65539654500006,11.6,9.43164404899999));
#238240=CARTESIAN_POINT('Ctrl Pts',(-4.65647634500006,15.2,9.43307941999999));
#238241=CARTESIAN_POINT('Ctrl Pts',(-4.65647634500006,11.6,9.43307941999999));
#238242=CARTESIAN_POINT('Ctrl Pts',(-4.65756195100006,15.2,9.43451974499999));
#238243=CARTESIAN_POINT('Ctrl Pts',(-4.65756195100006,11.6,9.43451974499999));
#238244=CARTESIAN_POINT('Ctrl Pts',(-4.65865336200006,15.2,9.43596500399998));
#238245=CARTESIAN_POINT('Ctrl Pts',(-4.65865336200006,11.6,9.43596500399998));
#238246=CARTESIAN_POINT('Ctrl Pts',(-4.65975057800006,15.2,9.43741517399998));
#238247=CARTESIAN_POINT('Ctrl Pts',(-4.65975057800006,11.6,9.43741517399998));
#238248=CARTESIAN_POINT('Ctrl Pts',(-4.66085359800006,15.2,9.43887023499999));
#238249=CARTESIAN_POINT('Ctrl Pts',(-4.66085359800006,11.6,9.43887023499999));
#238250=CARTESIAN_POINT('Ctrl Pts',(-4.66196242400006,15.2,9.44033016699999));
#238251=CARTESIAN_POINT('Ctrl Pts',(-4.66196242400006,11.6,9.44033016699999));
#238252=CARTESIAN_POINT('Ctrl Pts',(-4.66307705300006,15.2,9.44179494899998));
#238253=CARTESIAN_POINT('Ctrl Pts',(-4.66307705300006,11.6,9.44179494899998));
#238254=CARTESIAN_POINT('Ctrl Pts',(-4.66419748600006,15.2,9.44326456099999));
#238255=CARTESIAN_POINT('Ctrl Pts',(-4.66419748600006,11.6,9.44326456099999));
#238256=CARTESIAN_POINT('Ctrl Pts',(-4.66532372300006,15.2,9.44473897999998));
#238257=CARTESIAN_POINT('Ctrl Pts',(-4.66532372300006,11.6,9.44473897999998));
#238258=CARTESIAN_POINT('Ctrl Pts',(-4.66645576400006,15.2,9.44621818799998));
#238259=CARTESIAN_POINT('Ctrl Pts',(-4.66645576400006,11.6,9.44621818799998));
#238260=CARTESIAN_POINT('Ctrl Pts',(-4.66759360800006,15.2,9.44770216299998));
#238261=CARTESIAN_POINT('Ctrl Pts',(-4.66759360800006,11.6,9.44770216299998));
#238262=CARTESIAN_POINT('Ctrl Pts',(-4.66873725400006,15.2,9.44919088699999));
#238263=CARTESIAN_POINT('Ctrl Pts',(-4.66873725400006,11.6,9.44919088699999));
#238264=CARTESIAN_POINT('Ctrl Pts',(-4.66988670400006,15.2,9.45068433699999));
#238265=CARTESIAN_POINT('Ctrl Pts',(-4.66988670400006,11.6,9.45068433699999));
#238266=CARTESIAN_POINT('Ctrl Pts',(-4.67104195500006,15.2,9.45218249399998));
#238267=CARTESIAN_POINT('Ctrl Pts',(-4.67104195500006,11.6,9.45218249399998));
#238268=CARTESIAN_POINT('Ctrl Pts',(-4.67220300900006,15.2,9.45368533799999));
#238269=CARTESIAN_POINT('Ctrl Pts',(-4.67220300900006,11.6,9.45368533799999));
#238270=CARTESIAN_POINT('Ctrl Pts',(-4.67336986400006,15.2,9.45519284899999));
#238271=CARTESIAN_POINT('Ctrl Pts',(-4.67336986400006,11.6,9.45519284899999));
#238272=CARTESIAN_POINT('Ctrl Pts',(-4.67454252000006,15.2,9.45670500699999));
#238273=CARTESIAN_POINT('Ctrl Pts',(-4.67454252000006,11.6,9.45670500699999));
#238274=CARTESIAN_POINT('Ctrl Pts',(-4.67572097800006,15.2,9.45822179199999));
#238275=CARTESIAN_POINT('Ctrl Pts',(-4.67572097800006,11.6,9.45822179199999));
#238276=CARTESIAN_POINT('Ctrl Pts',(-4.67690523600006,15.2,9.45974318399998));
#238277=CARTESIAN_POINT('Ctrl Pts',(-4.67690523600006,11.6,9.45974318399998));
#238278=CARTESIAN_POINT('Ctrl Pts',(-4.67809529500006,15.2,9.46126916199999));
#238279=CARTESIAN_POINT('Ctrl Pts',(-4.67809529500006,11.6,9.46126916199999));
#238280=CARTESIAN_POINT('Ctrl Pts',(-4.67929115300006,15.2,9.46279970999999));
#238281=CARTESIAN_POINT('Ctrl Pts',(-4.67929115300006,11.6,9.46279970999999));
#238282=CARTESIAN_POINT('Ctrl Pts',(-4.68049281000006,15.2,9.46433480499999));
#238283=CARTESIAN_POINT('Ctrl Pts',(-4.68049281000006,11.6,9.46433480499999));
#238284=CARTESIAN_POINT('Ctrl Pts',(-4.68170026700006,15.2,9.46587442799999));
#238285=CARTESIAN_POINT('Ctrl Pts',(-4.68170026700006,11.6,9.46587442799999));
#238286=CARTESIAN_POINT('Ctrl Pts',(-4.68291352300006,15.2,9.46741856099998));
#238287=CARTESIAN_POINT('Ctrl Pts',(-4.68291352300006,11.6,9.46741856099998));
#238288=CARTESIAN_POINT('Ctrl Pts',(-4.68413257500006,15.2,9.46896718199999));
#238289=CARTESIAN_POINT('Ctrl Pts',(-4.68413257500006,11.6,9.46896718199999));
#238290=CARTESIAN_POINT('Ctrl Pts',(-4.68535742700006,15.2,9.47052027399998));
#238291=CARTESIAN_POINT('Ctrl Pts',(-4.68535742700006,11.6,9.47052027399998));
#238292=CARTESIAN_POINT('Ctrl Pts',(-4.68658807500006,15.2,9.47207781699999));
#238293=CARTESIAN_POINT('Ctrl Pts',(-4.68658807500006,11.6,9.47207781699999));
#238294=CARTESIAN_POINT('Ctrl Pts',(-4.68782452000006,15.2,9.47363979199999));
#238295=CARTESIAN_POINT('Ctrl Pts',(-4.68782452000006,11.6,9.47363979199999));
#238296=CARTESIAN_POINT('Ctrl Pts',(-4.68906676200006,15.2,9.47520617899999));
#238297=CARTESIAN_POINT('Ctrl Pts',(-4.68906676200006,11.6,9.47520617899999));
#238298=CARTESIAN_POINT('Ctrl Pts',(-4.69031479900006,15.2,9.47677695899999));
#238299=CARTESIAN_POINT('Ctrl Pts',(-4.69031479900006,11.6,9.47677695899999));
#238300=CARTESIAN_POINT('Ctrl Pts',(-4.69156863100006,15.2,9.47835211399998));
#238301=CARTESIAN_POINT('Ctrl Pts',(-4.69156863100006,11.6,9.47835211399998));
#238302=CARTESIAN_POINT('Ctrl Pts',(-4.69282825900006,15.2,9.47993162399998));
#238303=CARTESIAN_POINT('Ctrl Pts',(-4.69282825900006,11.6,9.47993162399998));
#238304=CARTESIAN_POINT('Ctrl Pts',(-4.69409368100006,15.2,9.48151547099998));
#238305=CARTESIAN_POINT('Ctrl Pts',(-4.69409368100006,11.6,9.48151547099998));
#238306=CARTESIAN_POINT('Ctrl Pts',(-4.69536489600006,15.2,9.48310363499999));
#238307=CARTESIAN_POINT('Ctrl Pts',(-4.69536489600006,11.6,9.48310363499999));
#238308=CARTESIAN_POINT('Ctrl Pts',(-4.69664190500006,15.2,9.48469609699998));
#238309=CARTESIAN_POINT('Ctrl Pts',(-4.69664190500006,11.6,9.48469609699998));
#238310=CARTESIAN_POINT('Ctrl Pts',(-4.69792470700006,15.2,9.48629284099999));
#238311=CARTESIAN_POINT('Ctrl Pts',(-4.69792470700006,11.6,9.48629284099999));
#238312=CARTESIAN_POINT('Ctrl Pts',(-4.69921330000005,15.2,9.48789384499998));
#238313=CARTESIAN_POINT('Ctrl Pts',(-4.69921330000005,11.6,9.48789384499998));
#238314=CARTESIAN_POINT('Ctrl Pts',(-4.70050768500006,15.2,9.48949909199998));
#238315=CARTESIAN_POINT('Ctrl Pts',(-4.70050768500006,11.6,9.48949909199998));
#238316=CARTESIAN_POINT('Ctrl Pts',(-4.70180786100006,15.2,9.49110856299999));
#238317=CARTESIAN_POINT('Ctrl Pts',(-4.70180786100006,11.6,9.49110856299999));
#238318=CARTESIAN_POINT('Ctrl Pts',(-4.70311382900006,15.2,9.49272224099998));
#238319=CARTESIAN_POINT('Ctrl Pts',(-4.70311382900006,11.6,9.49272224099998));
#238320=CARTESIAN_POINT('Ctrl Pts',(-4.70442558400006,15.2,9.49434010499999));
#238321=CARTESIAN_POINT('Ctrl Pts',(-4.70442558400006,11.6,9.49434010499999));
#238322=CARTESIAN_POINT('Ctrl Pts',(-4.70574313000006,15.2,9.49596213799998));
#238323=CARTESIAN_POINT('Ctrl Pts',(-4.70574313000006,11.6,9.49596213799998));
#238324=CARTESIAN_POINT('Ctrl Pts',(-4.70706646400005,15.2,9.49758832299998));
#238325=CARTESIAN_POINT('Ctrl Pts',(-4.70706646400005,11.6,9.49758832299998));
#238326=CARTESIAN_POINT('Ctrl Pts',(-4.70839558700006,15.2,9.49921863999998));
#238327=CARTESIAN_POINT('Ctrl Pts',(-4.70839558700006,11.6,9.49921863999998));
#238328=CARTESIAN_POINT('Ctrl Pts',(-4.70973049600006,15.2,9.50085307099998));
#238329=CARTESIAN_POINT('Ctrl Pts',(-4.70973049600006,11.6,9.50085307099998));
#238330=CARTESIAN_POINT('Ctrl Pts',(-4.71107119200005,15.2,9.50249159799998));
#238331=CARTESIAN_POINT('Ctrl Pts',(-4.71107119200005,11.6,9.50249159799998));
#238332=CARTESIAN_POINT('Ctrl Pts',(-4.71241767400006,15.2,9.50413420399999));
#238333=CARTESIAN_POINT('Ctrl Pts',(-4.71241767400006,11.6,9.50413420399999));
#238334=CARTESIAN_POINT('Ctrl Pts',(-4.71376994200006,15.2,9.50578086899998));
#238335=CARTESIAN_POINT('Ctrl Pts',(-4.71376994200006,11.6,9.50578086899998));
#238336=CARTESIAN_POINT('Ctrl Pts',(-4.71512799400006,15.2,9.50743157599998));
#238337=CARTESIAN_POINT('Ctrl Pts',(-4.71512799400006,11.6,9.50743157599998));
#238338=CARTESIAN_POINT('Ctrl Pts',(-4.71649183100006,15.2,9.50908630899999));
#238339=CARTESIAN_POINT('Ctrl Pts',(-4.71649183100006,11.6,9.50908630899999));
#238340=CARTESIAN_POINT('Ctrl Pts',(-4.71786144900006,15.2,9.51074504599998));
#238341=CARTESIAN_POINT('Ctrl Pts',(-4.71786144900006,11.6,9.51074504599998));
#238342=CARTESIAN_POINT('Ctrl Pts',(-4.71923685300006,15.2,9.51240777399999));
#238343=CARTESIAN_POINT('Ctrl Pts',(-4.71923685300006,11.6,9.51240777399999));
#238344=CARTESIAN_POINT('Ctrl Pts',(-4.72061803600006,15.2,9.51407447099999));
#238345=CARTESIAN_POINT('Ctrl Pts',(-4.72061803600006,11.6,9.51407447099999));
#238346=CARTESIAN_POINT('Ctrl Pts',(-4.72200500100006,15.2,9.51574512299998));
#238347=CARTESIAN_POINT('Ctrl Pts',(-4.72200500100006,11.6,9.51574512299998));
#238348=CARTESIAN_POINT('Ctrl Pts',(-4.72339774700006,15.2,9.51741970899998));
#238349=CARTESIAN_POINT('Ctrl Pts',(-4.72339774700006,11.6,9.51741970899998));
#238350=CARTESIAN_POINT('Ctrl Pts',(-4.72479627200006,15.2,9.51909821399998));
#238351=CARTESIAN_POINT('Ctrl Pts',(-4.72479627200006,11.6,9.51909821399998));
#238352=CARTESIAN_POINT('Ctrl Pts',(-4.72620057700006,15.2,9.52078061999998));
#238353=CARTESIAN_POINT('Ctrl Pts',(-4.72620057700006,11.6,9.52078061999998));
#238354=CARTESIAN_POINT('Ctrl Pts',(-4.72761065900006,15.2,9.52246690899998));
#238355=CARTESIAN_POINT('Ctrl Pts',(-4.72761065900006,11.6,9.52246690899998));
#238356=CARTESIAN_POINT('Ctrl Pts',(-4.72902651900006,15.2,9.52415706299998));
#238357=CARTESIAN_POINT('Ctrl Pts',(-4.72902651900006,11.6,9.52415706299998));
#238358=CARTESIAN_POINT('Ctrl Pts',(-4.73044815600006,15.2,9.52585106599999));
#238359=CARTESIAN_POINT('Ctrl Pts',(-4.73044815600006,11.6,9.52585106599999));
#238360=CARTESIAN_POINT('Ctrl Pts',(-4.73187556800006,15.2,9.52754889999999));
#238361=CARTESIAN_POINT('Ctrl Pts',(-4.73187556800006,11.6,9.52754889999999));
#238362=CARTESIAN_POINT('Ctrl Pts',(-4.73330875600006,15.2,9.52925054899998));
#238363=CARTESIAN_POINT('Ctrl Pts',(-4.73330875600006,11.6,9.52925054899998));
#238364=CARTESIAN_POINT('Ctrl Pts',(-4.73474771700006,15.2,9.53095599399998));
#238365=CARTESIAN_POINT('Ctrl Pts',(-4.73474771700006,11.6,9.53095599399998));
#238366=CARTESIAN_POINT('Ctrl Pts',(-4.73619245300006,15.2,9.53266521799998));
#238367=CARTESIAN_POINT('Ctrl Pts',(-4.73619245300006,11.6,9.53266521799998));
#238368=CARTESIAN_POINT('Ctrl Pts',(-4.73764296000006,15.2,9.53437820499998));
#238369=CARTESIAN_POINT('Ctrl Pts',(-4.73764296000006,11.6,9.53437820499998));
#238370=CARTESIAN_POINT('Ctrl Pts',(-4.73909923900006,15.2,9.53609493799998));
#238371=CARTESIAN_POINT('Ctrl Pts',(-4.73909923900006,11.6,9.53609493799998));
#238372=CARTESIAN_POINT('Ctrl Pts',(-4.74056129000005,15.2,9.53781539999999));
#238373=CARTESIAN_POINT('Ctrl Pts',(-4.74056129000005,11.6,9.53781539999999));
#238374=CARTESIAN_POINT('Ctrl Pts',(-4.74202911100006,15.2,9.53953957299999));
#238375=CARTESIAN_POINT('Ctrl Pts',(-4.74202911100006,11.6,9.53953957299999));
#238376=CARTESIAN_POINT('Ctrl Pts',(-4.74350270100006,15.2,9.54126744099998));
#238377=CARTESIAN_POINT('Ctrl Pts',(-4.74350270100006,11.6,9.54126744099998));
#238378=CARTESIAN_POINT('Ctrl Pts',(-4.74498205900006,15.2,9.54299898599999));
#238379=CARTESIAN_POINT('Ctrl Pts',(-4.74498205900006,11.6,9.54299898599999));
#238380=CARTESIAN_POINT('Ctrl Pts',(-4.74646718500006,15.2,9.54473419399999));
#238381=CARTESIAN_POINT('Ctrl Pts',(-4.74646718500006,11.6,9.54473419399999));
#238382=CARTESIAN_POINT('Ctrl Pts',(-4.74795807700006,15.2,9.54647304599998));
#238383=CARTESIAN_POINT('Ctrl Pts',(-4.74795807700006,11.6,9.54647304599998));
#238384=CARTESIAN_POINT('Ctrl Pts',(-4.74945473400005,15.2,9.54821552599999));
#238385=CARTESIAN_POINT('Ctrl Pts',(-4.74945473400005,11.6,9.54821552599999));
#238386=CARTESIAN_POINT('Ctrl Pts',(-4.75095715700006,15.2,9.54996161699999));
#238387=CARTESIAN_POINT('Ctrl Pts',(-4.75095715700006,11.6,9.54996161699999));
#238388=CARTESIAN_POINT('Ctrl Pts',(-4.75246534500006,15.2,9.55171130299998));
#238389=CARTESIAN_POINT('Ctrl Pts',(-4.75246534500006,11.6,9.55171130299998));
#238390=CARTESIAN_POINT('Ctrl Pts',(-4.75397929400006,15.2,9.55346456799998));
#238391=CARTESIAN_POINT('Ctrl Pts',(-4.75397929400006,11.6,9.55346456799998));
#238392=CARTESIAN_POINT('Ctrl Pts',(-4.75549900600006,15.2,9.55522139399999));
#238393=CARTESIAN_POINT('Ctrl Pts',(-4.75549900600006,11.6,9.55522139399999));
#238394=CARTESIAN_POINT('Ctrl Pts',(-4.75702447800006,15.2,9.55698176499999));
#238395=CARTESIAN_POINT('Ctrl Pts',(-4.75702447800006,11.6,9.55698176499999));
#238396=CARTESIAN_POINT('Ctrl Pts',(-4.75855571100006,15.2,9.55874566599999));
#238397=CARTESIAN_POINT('Ctrl Pts',(-4.75855571100006,11.6,9.55874566599999));
#238398=CARTESIAN_POINT('Ctrl Pts',(-4.76009270400006,15.2,9.56051307899998));
#238399=CARTESIAN_POINT('Ctrl Pts',(-4.76009270400006,11.6,9.56051307899998));
#238400=CARTESIAN_POINT('Ctrl Pts',(-4.76163545500006,15.2,9.56228398899999));
#238401=CARTESIAN_POINT('Ctrl Pts',(-4.76163545500006,11.6,9.56228398899999));
#238402=CARTESIAN_POINT('Ctrl Pts',(-4.76318396200006,15.2,9.56405837999998));
#238403=CARTESIAN_POINT('Ctrl Pts',(-4.76318396200006,11.6,9.56405837999998));
#238404=CARTESIAN_POINT('Ctrl Pts',(-4.76473822700005,15.2,9.56583623399998));
#238405=CARTESIAN_POINT('Ctrl Pts',(-4.76473822700005,11.6,9.56583623399998));
#238406=CARTESIAN_POINT('Ctrl Pts',(-4.76629824600006,15.2,9.56761753699999));
#238407=CARTESIAN_POINT('Ctrl Pts',(-4.76629824600006,11.6,9.56761753699999));
#238408=CARTESIAN_POINT('Ctrl Pts',(-4.76786402100006,15.2,9.56940227099999));
#238409=CARTESIAN_POINT('Ctrl Pts',(-4.76786402100006,11.6,9.56940227099999));
#238410=CARTESIAN_POINT('Ctrl Pts',(-4.76943554800005,15.2,9.57119042099999));
#238411=CARTESIAN_POINT('Ctrl Pts',(-4.76943554800005,11.6,9.57119042099999));
#238412=CARTESIAN_POINT('Ctrl Pts',(-4.77101282700006,15.2,9.57298197199999));
#238413=CARTESIAN_POINT('Ctrl Pts',(-4.77101282700006,11.6,9.57298197199999));
#238414=CARTESIAN_POINT('Ctrl Pts',(-4.77259585800006,15.2,9.57477690599998));
#238415=CARTESIAN_POINT('Ctrl Pts',(-4.77259585800006,11.6,9.57477690599998));
#238416=CARTESIAN_POINT('Ctrl Pts',(-4.77418464000006,15.2,9.57657520799999));
#238417=CARTESIAN_POINT('Ctrl Pts',(-4.77418464000006,11.6,9.57657520799999));
#238418=CARTESIAN_POINT('Ctrl Pts',(-4.77577917000006,15.2,9.57837686299998));
#238419=CARTESIAN_POINT('Ctrl Pts',(-4.77577917000006,11.6,9.57837686299998));
#238420=CARTESIAN_POINT('Ctrl Pts',(-4.77737944900006,15.2,9.58018185499999));
#238421=CARTESIAN_POINT('Ctrl Pts',(-4.77737944900006,11.6,9.58018185499999));
#238422=CARTESIAN_POINT('Ctrl Pts',(-4.77898547500006,15.2,9.58199016699999));
#238423=CARTESIAN_POINT('Ctrl Pts',(-4.77898547500006,11.6,9.58199016699999));
#238424=CARTESIAN_POINT('Ctrl Pts',(-4.78059724700006,15.2,9.58380178399998));
#238425=CARTESIAN_POINT('Ctrl Pts',(-4.78059724700006,11.6,9.58380178399998));
#238426=CARTESIAN_POINT('Ctrl Pts',(-4.78221476400006,15.2,9.58561669099998));
#238427=CARTESIAN_POINT('Ctrl Pts',(-4.78221476400006,11.6,9.58561669099998));
#238428=CARTESIAN_POINT('Ctrl Pts',(-4.78383802500006,15.2,9.58743487199998));
#238429=CARTESIAN_POINT('Ctrl Pts',(-4.78383802500006,11.6,9.58743487199998));
#238430=CARTESIAN_POINT('Ctrl Pts',(-4.78546702900006,15.2,9.58925631099999));
#238431=CARTESIAN_POINT('Ctrl Pts',(-4.78546702900006,11.6,9.58925631099999));
#238432=CARTESIAN_POINT('Ctrl Pts',(-4.78710177500006,15.2,9.59108099199998));
#238433=CARTESIAN_POINT('Ctrl Pts',(-4.78710177500006,11.6,9.59108099199998));
#238434=CARTESIAN_POINT('Ctrl Pts',(-4.78874226100006,15.2,9.59290890199998));
#238435=CARTESIAN_POINT('Ctrl Pts',(-4.78874226100006,11.6,9.59290890199998));
#238436=CARTESIAN_POINT('Ctrl Pts',(-4.79038848700006,15.2,9.59474002299999));
#238437=CARTESIAN_POINT('Ctrl Pts',(-4.79038848700006,11.6,9.59474002299999));
#238438=CARTESIAN_POINT('Ctrl Pts',(-4.79204045200006,15.2,9.59657433899999));
#238439=CARTESIAN_POINT('Ctrl Pts',(-4.79204045200006,11.6,9.59657433899999));
#238440=CARTESIAN_POINT('Ctrl Pts',(-4.79369815400006,15.2,9.59841183799998));
#238441=CARTESIAN_POINT('Ctrl Pts',(-4.79369815400006,11.6,9.59841183799998));
#238442=CARTESIAN_POINT('Ctrl Pts',(-4.79536159200006,15.2,9.60025250299999));
#238443=CARTESIAN_POINT('Ctrl Pts',(-4.79536159200006,11.6,9.60025250299999));
#238444=CARTESIAN_POINT('Ctrl Pts',(-4.79703076500006,15.2,9.60209631699998));
#238445=CARTESIAN_POINT('Ctrl Pts',(-4.79703076500006,11.6,9.60209631699998));
#238446=CARTESIAN_POINT('Ctrl Pts',(-4.79870567300006,15.2,9.60394326799998));
#238447=CARTESIAN_POINT('Ctrl Pts',(-4.79870567300006,11.6,9.60394326799998));
#238448=CARTESIAN_POINT('Ctrl Pts',(-4.80038631200006,15.2,9.60579333799998));
#238449=CARTESIAN_POINT('Ctrl Pts',(-4.80038631200006,11.6,9.60579333799998));
#238450=CARTESIAN_POINT('Ctrl Pts',(-4.80207268400005,15.2,9.60764651399998));
#238451=CARTESIAN_POINT('Ctrl Pts',(-4.80207268400005,11.6,9.60764651399998));
#238452=CARTESIAN_POINT('Ctrl Pts',(-4.80376478700006,15.2,9.60950277999999));
#238453=CARTESIAN_POINT('Ctrl Pts',(-4.80376478700006,11.6,9.60950277999999));
#238454=CARTESIAN_POINT('Ctrl Pts',(-4.80546261900006,15.2,9.61136212099999));
#238455=CARTESIAN_POINT('Ctrl Pts',(-4.80546261900006,11.6,9.61136212099999));
#238456=CARTESIAN_POINT('Ctrl Pts',(-4.80716617900006,15.2,9.61322452199998));
#238457=CARTESIAN_POINT('Ctrl Pts',(-4.80716617900006,11.6,9.61322452199998));
#238458=CARTESIAN_POINT('Ctrl Pts',(-4.80887546500006,15.2,9.61508996699998));
#238459=CARTESIAN_POINT('Ctrl Pts',(-4.80887546500006,11.6,9.61508996699998));
#238460=CARTESIAN_POINT('Ctrl Pts',(-4.81059047700006,15.2,9.61695844399999));
#238461=CARTESIAN_POINT('Ctrl Pts',(-4.81059047700006,11.6,9.61695844399999));
#238462=CARTESIAN_POINT('Ctrl Pts',(-4.81231121400006,15.2,9.61882993499999));
#238463=CARTESIAN_POINT('Ctrl Pts',(-4.81231121400006,11.6,9.61882993499999));
#238464=CARTESIAN_POINT('Ctrl Pts',(-4.81403767400006,15.2,9.62070442599998));
#238465=CARTESIAN_POINT('Ctrl Pts',(-4.81403767400006,11.6,9.62070442599998));
#238466=CARTESIAN_POINT('Ctrl Pts',(-4.81576985700006,15.2,9.62258190399999));
#238467=CARTESIAN_POINT('Ctrl Pts',(-4.81576985700006,11.6,9.62258190399999));
#238468=CARTESIAN_POINT('Ctrl Pts',(-4.81750776000006,15.2,9.62446235199998));
#238469=CARTESIAN_POINT('Ctrl Pts',(-4.81750776000006,11.6,9.62446235199998));
#238470=CARTESIAN_POINT('Ctrl Pts',(-4.81925138400006,15.2,9.62634575599999));
#238471=CARTESIAN_POINT('Ctrl Pts',(-4.81925138400006,11.6,9.62634575599999));
#238472=CARTESIAN_POINT('Ctrl Pts',(-4.82100072500006,15.2,9.62823210199998));
#238473=CARTESIAN_POINT('Ctrl Pts',(-4.82100072500006,11.6,9.62823210199998));
#238474=CARTESIAN_POINT('Ctrl Pts',(-4.82275578500006,15.2,9.63012137399998));
#238475=CARTESIAN_POINT('Ctrl Pts',(-4.82275578500006,11.6,9.63012137399998));
#238476=CARTESIAN_POINT('Ctrl Pts',(-4.82451656000006,15.2,9.63201355899999));
#238477=CARTESIAN_POINT('Ctrl Pts',(-4.82451656000006,11.6,9.63201355899999));
#238478=CARTESIAN_POINT('Ctrl Pts',(-4.82628304900006,15.2,9.63390864199998));
#238479=CARTESIAN_POINT('Ctrl Pts',(-4.82628304900006,11.6,9.63390864199998));
#238480=CARTESIAN_POINT('Ctrl Pts',(-4.82805525200006,15.2,9.63580660699999));
#238481=CARTESIAN_POINT('Ctrl Pts',(-4.82805525200006,11.6,9.63580660699999));
#238482=CARTESIAN_POINT('Ctrl Pts',(-4.82983316700006,15.2,9.63770744199999));
#238483=CARTESIAN_POINT('Ctrl Pts',(-4.82983316700006,11.6,9.63770744199999));
#238484=CARTESIAN_POINT('Ctrl Pts',(-4.83161679300006,15.2,9.63961113099998));
#238485=CARTESIAN_POINT('Ctrl Pts',(-4.83161679300006,11.6,9.63961113099998));
#238486=CARTESIAN_POINT('Ctrl Pts',(-4.83340612800006,15.2,9.64151765999999));
#238487=CARTESIAN_POINT('Ctrl Pts',(-4.83340612800006,11.6,9.64151765999999));
#238488=CARTESIAN_POINT('Ctrl Pts',(-4.83520117200006,15.2,9.64342701399998));
#238489=CARTESIAN_POINT('Ctrl Pts',(-4.83520117200006,11.6,9.64342701399998));
#238490=CARTESIAN_POINT('Ctrl Pts',(-4.83700192300006,15.2,9.64533917999999));
#238491=CARTESIAN_POINT('Ctrl Pts',(-4.83700192300006,11.6,9.64533917999999));
#238492=CARTESIAN_POINT('Ctrl Pts',(-4.83880838000006,15.2,9.64725414299998));
#238493=CARTESIAN_POINT('Ctrl Pts',(-4.83880838000006,11.6,9.64725414299998));
#238494=CARTESIAN_POINT('Ctrl Pts',(-4.84062054100006,15.2,9.64917188799999));
#238495=CARTESIAN_POINT('Ctrl Pts',(-4.84062054100006,11.6,9.64917188799999));
#238496=CARTESIAN_POINT('Ctrl Pts',(-4.84243840500006,15.2,9.65109240199999));
#238497=CARTESIAN_POINT('Ctrl Pts',(-4.84243840500006,11.6,9.65109240199999));
#238498=CARTESIAN_POINT('Ctrl Pts',(-4.84426197000006,15.2,9.65301567099999));
#238499=CARTESIAN_POINT('Ctrl Pts',(-4.84426197000006,11.6,9.65301567099999));
#238500=CARTESIAN_POINT('Ctrl Pts',(-4.84609123600006,15.2,9.65494167999999));
#238501=CARTESIAN_POINT('Ctrl Pts',(-4.84609123600006,11.6,9.65494167999999));
#238502=CARTESIAN_POINT('Ctrl Pts',(-4.84792620100006,15.2,9.65687041299999));
#238503=CARTESIAN_POINT('Ctrl Pts',(-4.84792620100006,11.6,9.65687041299999));
#238504=CARTESIAN_POINT('Ctrl Pts',(-4.84976686400006,15.2,9.65880186099999));
#238505=CARTESIAN_POINT('Ctrl Pts',(-4.84976686400006,11.6,9.65880186099999));
#238506=CARTESIAN_POINT('Ctrl Pts',(-4.85161322400006,15.2,9.66073600499998));
#238507=CARTESIAN_POINT('Ctrl Pts',(-4.85161322400006,11.6,9.66073600499998));
#238508=CARTESIAN_POINT('Ctrl Pts',(-4.85346527800006,15.2,9.66267283399999));
#238509=CARTESIAN_POINT('Ctrl Pts',(-4.85346527800006,11.6,9.66267283399999));
#238510=CARTESIAN_POINT('Ctrl Pts',(-4.85532302500006,15.2,9.66461233499999));
#238511=CARTESIAN_POINT('Ctrl Pts',(-4.85532302500006,11.6,9.66461233499999));
#238512=CARTESIAN_POINT('Ctrl Pts',(-4.85718646500006,15.2,9.66655448999998));
#238513=CARTESIAN_POINT('Ctrl Pts',(-4.85718646500006,11.6,9.66655448999998));
#238514=CARTESIAN_POINT('Ctrl Pts',(-4.85905559600006,15.2,9.66849928799999));
#238515=CARTESIAN_POINT('Ctrl Pts',(-4.85905559600006,11.6,9.66849928799999));
#238516=CARTESIAN_POINT('Ctrl Pts',(-4.86093041600006,15.2,9.67044671499998));
#238517=CARTESIAN_POINT('Ctrl Pts',(-4.86093041600006,11.6,9.67044671499998));
#238518=CARTESIAN_POINT('Ctrl Pts',(-4.86281092400006,15.2,9.67239675599998));
#238519=CARTESIAN_POINT('Ctrl Pts',(-4.86281092400006,11.6,9.67239675599998));
#238520=CARTESIAN_POINT('Ctrl Pts',(-4.86469712000006,15.2,9.67434939899999));
#238521=CARTESIAN_POINT('Ctrl Pts',(-4.86469712000006,11.6,9.67434939899999));
#238522=CARTESIAN_POINT('Ctrl Pts',(-4.86658900000006,15.2,9.67630462899999));
#238523=CARTESIAN_POINT('Ctrl Pts',(-4.86658900000006,11.6,9.67630462899999));
#238524=CARTESIAN_POINT('Ctrl Pts',(-4.86848656400006,15.2,9.67826243299999));
#238525=CARTESIAN_POINT('Ctrl Pts',(-4.86848656400006,11.6,9.67826243299999));
#238526=CARTESIAN_POINT('Ctrl Pts',(-4.87038981000006,15.2,9.68022279599998));
#238527=CARTESIAN_POINT('Ctrl Pts',(-4.87038981000006,11.6,9.68022279599998));
#238528=CARTESIAN_POINT('Ctrl Pts',(-4.87229873800006,15.2,9.68218570599999));
#238529=CARTESIAN_POINT('Ctrl Pts',(-4.87229873800006,11.6,9.68218570599999));
#238530=CARTESIAN_POINT('Ctrl Pts',(-4.87421334500006,15.2,9.68415114799999));
#238531=CARTESIAN_POINT('Ctrl Pts',(-4.87421334500006,11.6,9.68415114799999));
#238532=CARTESIAN_POINT('Ctrl Pts',(-4.87613363000006,15.2,9.68611911099998));
#238533=CARTESIAN_POINT('Ctrl Pts',(-4.87613363000006,11.6,9.68611911099998));
#238534=CARTESIAN_POINT('Ctrl Pts',(-4.87805959200006,15.2,9.68808957899999));
#238535=CARTESIAN_POINT('Ctrl Pts',(-4.87805959200006,11.6,9.68808957899999));
#238536=CARTESIAN_POINT('Ctrl Pts',(-4.87999122900006,15.2,9.69006253899998));
#238537=CARTESIAN_POINT('Ctrl Pts',(-4.87999122900006,11.6,9.69006253899998));
#238538=CARTESIAN_POINT('Ctrl Pts',(-4.88192854000006,15.2,9.69203797799998));
#238539=CARTESIAN_POINT('Ctrl Pts',(-4.88192854000006,11.6,9.69203797799998));
#238540=CARTESIAN_POINT('Ctrl Pts',(-4.88387152300006,15.2,9.69401588199998));
#238541=CARTESIAN_POINT('Ctrl Pts',(-4.88387152300006,11.6,9.69401588199998));
#238542=CARTESIAN_POINT('Ctrl Pts',(-4.88582017800006,15.2,9.69599623899999));
#238543=CARTESIAN_POINT('Ctrl Pts',(-4.88582017800006,11.6,9.69599623899999));
#238544=CARTESIAN_POINT('Ctrl Pts',(-4.88777450100006,15.2,9.69797903399999));
#238545=CARTESIAN_POINT('Ctrl Pts',(-4.88777450100006,11.6,9.69797903399999));
#238546=CARTESIAN_POINT('Ctrl Pts',(-4.88973449200006,15.2,9.69996425399999));
#238547=CARTESIAN_POINT('Ctrl Pts',(-4.88973449200006,11.6,9.69996425399999));
#238548=CARTESIAN_POINT('Ctrl Pts',(-4.89170014900006,15.2,9.70195188799998));
#238549=CARTESIAN_POINT('Ctrl Pts',(-4.89170014900006,11.6,9.70195188799998));
#238550=CARTESIAN_POINT('Ctrl Pts',(-4.89367147200006,15.2,9.70394191899998));
#238551=CARTESIAN_POINT('Ctrl Pts',(-4.89367147200006,11.6,9.70394191899998));
#238552=CARTESIAN_POINT('Ctrl Pts',(-4.89564845800006,15.2,9.70593433699998));
#238553=CARTESIAN_POINT('Ctrl Pts',(-4.89564845800006,11.6,9.70593433699998));
#238554=CARTESIAN_POINT('Ctrl Pts',(-4.89763110500006,15.2,9.70792912699999));
#238555=CARTESIAN_POINT('Ctrl Pts',(-4.89763110500006,11.6,9.70792912699999));
#238556=CARTESIAN_POINT('Ctrl Pts',(-4.89961941300006,15.2,9.70992627699999));
#238557=CARTESIAN_POINT('Ctrl Pts',(-4.89961941300006,11.6,9.70992627699999));
#238558=CARTESIAN_POINT('Ctrl Pts',(-4.90161338000005,15.2,9.71192577199999));
#238559=CARTESIAN_POINT('Ctrl Pts',(-4.90161338000005,11.6,9.71192577199999));
#238560=CARTESIAN_POINT('Ctrl Pts',(-4.90361300500005,15.2,9.71392760099998));
#238561=CARTESIAN_POINT('Ctrl Pts',(-4.90361300500005,11.6,9.71392760099998));
#238562=CARTESIAN_POINT('Ctrl Pts',(-4.90561828400006,15.2,9.71593175099999));
#238563=CARTESIAN_POINT('Ctrl Pts',(-4.90561828400006,11.6,9.71593175099999));
#238564=CARTESIAN_POINT('Ctrl Pts',(-4.90762921800005,15.2,9.71793820799999));
#238565=CARTESIAN_POINT('Ctrl Pts',(-4.90762921800005,11.6,9.71793820799999));
#238566=CARTESIAN_POINT('Ctrl Pts',(-4.90964580500005,15.2,9.71994695899999));
#238567=CARTESIAN_POINT('Ctrl Pts',(-4.90964580500005,11.6,9.71994695899999));
#238568=CARTESIAN_POINT('Ctrl Pts',(-4.91166804300006,15.2,9.72195799099998));
#238569=CARTESIAN_POINT('Ctrl Pts',(-4.91166804300006,11.6,9.72195799099998));
#238570=CARTESIAN_POINT('Ctrl Pts',(-4.91369593100006,15.2,9.72397129099999));
#238571=CARTESIAN_POINT('Ctrl Pts',(-4.91369593100006,11.6,9.72397129099999));
#238572=CARTESIAN_POINT('Ctrl Pts',(-4.91572946500006,15.2,9.72598684699998));
#238573=CARTESIAN_POINT('Ctrl Pts',(-4.91572946500006,11.6,9.72598684699998));
#238574=CARTESIAN_POINT('Ctrl Pts',(-4.91776864800006,15.2,9.72800464599998));
#238575=CARTESIAN_POINT('Ctrl Pts',(-4.91776864800006,11.6,9.72800464599998));
#238576=CARTESIAN_POINT('Ctrl Pts',(-4.91981347500006,15.2,9.73002467499999));
#238577=CARTESIAN_POINT('Ctrl Pts',(-4.91981347500006,11.6,9.73002467499999));
#238578=CARTESIAN_POINT('Ctrl Pts',(-4.92186394500005,15.2,9.73204692099999));
#238579=CARTESIAN_POINT('Ctrl Pts',(-4.92186394500005,11.6,9.73204692099999));
#238580=CARTESIAN_POINT('Ctrl Pts',(-4.92392005600006,15.2,9.73407136999998));
#238581=CARTESIAN_POINT('Ctrl Pts',(-4.92392005600006,11.6,9.73407136999998));
#238582=CARTESIAN_POINT('Ctrl Pts',(-4.92598180900006,15.2,9.73609801199999));
#238583=CARTESIAN_POINT('Ctrl Pts',(-4.92598180900006,11.6,9.73609801199999));
#238584=CARTESIAN_POINT('Ctrl Pts',(-4.92804919800006,15.2,9.73812683299998));
#238585=CARTESIAN_POINT('Ctrl Pts',(-4.92804919800006,11.6,9.73812683299998));
#238586=CARTESIAN_POINT('Ctrl Pts',(-4.93012222500006,15.2,9.74015781999999));
#238587=CARTESIAN_POINT('Ctrl Pts',(-4.93012222500006,11.6,9.74015781999999));
#238588=CARTESIAN_POINT('Ctrl Pts',(-4.93220088800006,15.2,9.74219095999998));
#238589=CARTESIAN_POINT('Ctrl Pts',(-4.93220088800006,11.6,9.74219095999998));
#238590=CARTESIAN_POINT('Ctrl Pts',(-4.93428518500005,15.2,9.74422624199999));
#238591=CARTESIAN_POINT('Ctrl Pts',(-4.93428518500005,11.6,9.74422624199999));
#238592=CARTESIAN_POINT('Ctrl Pts',(-4.93637511200006,15.2,9.74626365299999));
#238593=CARTESIAN_POINT('Ctrl Pts',(-4.93637511200006,11.6,9.74626365299999));
#238594=CARTESIAN_POINT('Ctrl Pts',(-4.93847067100006,15.2,9.74830317899999));
#238595=CARTESIAN_POINT('Ctrl Pts',(-4.93847067100006,11.6,9.74830317899999));
#238596=CARTESIAN_POINT('Ctrl Pts',(-4.94057185900005,15.2,9.75034480899998));
#238597=CARTESIAN_POINT('Ctrl Pts',(-4.94057185900005,11.6,9.75034480899998));
#238598=CARTESIAN_POINT('Ctrl Pts',(-4.94267867400006,15.2,9.75238852899999));
#238599=CARTESIAN_POINT('Ctrl Pts',(-4.94267867400006,11.6,9.75238852899999));
#238600=CARTESIAN_POINT('Ctrl Pts',(-4.94479111300006,15.2,9.75443432799998));
#238601=CARTESIAN_POINT('Ctrl Pts',(-4.94479111300006,11.6,9.75443432799998));
#238602=CARTESIAN_POINT('Ctrl Pts',(-4.94690917700006,15.2,9.75648219399999));
#238603=CARTESIAN_POINT('Ctrl Pts',(-4.94690917700006,11.6,9.75648219399999));
#238604=CARTESIAN_POINT('Ctrl Pts',(-4.94903286400006,15.2,9.75853211399999));
#238605=CARTESIAN_POINT('Ctrl Pts',(-4.94903286400006,11.6,9.75853211399999));
#238606=CARTESIAN_POINT('Ctrl Pts',(-4.95116217100006,15.2,9.76058407399999));
#238607=CARTESIAN_POINT('Ctrl Pts',(-4.95116217100006,11.6,9.76058407399999));
#238608=CARTESIAN_POINT('Ctrl Pts',(-4.95329709600006,15.2,9.76263806399999));
#238609=CARTESIAN_POINT('Ctrl Pts',(-4.95329709600006,11.6,9.76263806399999));
#238610=CARTESIAN_POINT('Ctrl Pts',(-4.95543763800006,15.2,9.76469406999998));
#238611=CARTESIAN_POINT('Ctrl Pts',(-4.95543763800006,11.6,9.76469406999998));
#238612=CARTESIAN_POINT('Ctrl Pts',(-4.95758379700006,15.2,9.76675208199998));
#238613=CARTESIAN_POINT('Ctrl Pts',(-4.95758379700006,11.6,9.76675208199998));
#238614=CARTESIAN_POINT('Ctrl Pts',(-4.95973556900006,15.2,9.76881208499999));
#238615=CARTESIAN_POINT('Ctrl Pts',(-4.95973556900006,11.6,9.76881208499999));
#238616=CARTESIAN_POINT('Ctrl Pts',(-4.96189295400006,15.2,9.77087406899999));
#238617=CARTESIAN_POINT('Ctrl Pts',(-4.96189295400006,11.6,9.77087406899999));
#238618=CARTESIAN_POINT('Ctrl Pts',(-4.96405594800006,15.2,9.77293802099998));
#238619=CARTESIAN_POINT('Ctrl Pts',(-4.96405594800006,11.6,9.77293802099998));
#238620=CARTESIAN_POINT('Ctrl Pts',(-4.96622455200006,15.2,9.77500392799998));
#238621=CARTESIAN_POINT('Ctrl Pts',(-4.96622455200006,11.6,9.77500392799998));
#238622=CARTESIAN_POINT('Ctrl Pts',(-4.96839876200006,15.2,9.77707177899998));
#238623=CARTESIAN_POINT('Ctrl Pts',(-4.96839876200006,11.6,9.77707177899998));
#238624=CARTESIAN_POINT('Ctrl Pts',(-4.97057857800006,15.2,9.77914156199999));
#238625=CARTESIAN_POINT('Ctrl Pts',(-4.97057857800006,11.6,9.77914156199999));
#238626=CARTESIAN_POINT('Ctrl Pts',(-4.97276399800006,15.2,9.78121326499998));
#238627=CARTESIAN_POINT('Ctrl Pts',(-4.97276399800006,11.6,9.78121326499998));
#238628=CARTESIAN_POINT('Ctrl Pts',(-4.97495501900006,15.2,9.78328687399999));
#238629=CARTESIAN_POINT('Ctrl Pts',(-4.97495501900006,11.6,9.78328687399999));
#238630=CARTESIAN_POINT('Ctrl Pts',(-4.97715164100006,15.2,9.78536237999998));
#238631=CARTESIAN_POINT('Ctrl Pts',(-4.97715164100006,11.6,9.78536237999998));
#238632=CARTESIAN_POINT('Ctrl Pts',(-4.97935386100006,15.2,9.78743976799999));
#238633=CARTESIAN_POINT('Ctrl Pts',(-4.97935386100006,11.6,9.78743976799999));
#238634=CARTESIAN_POINT('Ctrl Pts',(-4.98156167800006,15.2,9.78951902899999));
#238635=CARTESIAN_POINT('Ctrl Pts',(-4.98156167800006,11.6,9.78951902899999));
#238636=CARTESIAN_POINT('Ctrl Pts',(-4.98377508900006,15.2,9.79160014799999));
#238637=CARTESIAN_POINT('Ctrl Pts',(-4.98377508900006,11.6,9.79160014799999));
#238638=CARTESIAN_POINT('Ctrl Pts',(-4.98599409400006,15.2,9.79368311599998));
#238639=CARTESIAN_POINT('Ctrl Pts',(-4.98599409400006,11.6,9.79368311599998));
#238640=CARTESIAN_POINT('Ctrl Pts',(-4.98821869000006,15.2,9.79576792099999));
#238641=CARTESIAN_POINT('Ctrl Pts',(-4.98821869000006,11.6,9.79576792099999));
#238642=CARTESIAN_POINT('Ctrl Pts',(-4.99044887700006,15.2,9.79785454799998));
#238643=CARTESIAN_POINT('Ctrl Pts',(-4.99044887700006,11.6,9.79785454799998));
#238644=CARTESIAN_POINT('Ctrl Pts',(-4.99268465100006,15.2,9.79994298899998));
#238645=CARTESIAN_POINT('Ctrl Pts',(-4.99268465100006,11.6,9.79994298899998));
#238646=CARTESIAN_POINT('Ctrl Pts',(-4.99492601100005,15.2,9.80203322899998));
#238647=CARTESIAN_POINT('Ctrl Pts',(-4.99492601100005,11.6,9.80203322899998));
#238648=CARTESIAN_POINT('Ctrl Pts',(-4.99717295600006,15.2,9.80412525899998));
#238649=CARTESIAN_POINT('Ctrl Pts',(-4.99717295600006,11.6,9.80412525899998));
#238650=CARTESIAN_POINT('Ctrl Pts',(-4.99942548400006,15.2,9.80621906499999));
#238651=CARTESIAN_POINT('Ctrl Pts',(-4.99942548400006,11.6,9.80621906499999));
#238652=CARTESIAN_POINT('Ctrl Pts',(-5.00168359100006,15.2,9.80831463699998));
#238653=CARTESIAN_POINT('Ctrl Pts',(-5.00168359100006,11.6,9.80831463699998));
#238654=CARTESIAN_POINT('Ctrl Pts',(-5.00394727800006,15.2,9.81041196199998));
#238655=CARTESIAN_POINT('Ctrl Pts',(-5.00394727800006,11.6,9.81041196199998));
#238656=CARTESIAN_POINT('Ctrl Pts',(-5.00621654300006,15.2,9.81251102999998));
#238657=CARTESIAN_POINT('Ctrl Pts',(-5.00621654300006,11.6,9.81251102999998));
#238658=CARTESIAN_POINT('Ctrl Pts',(-5.00849138300006,15.2,9.81461182699999));
#238659=CARTESIAN_POINT('Ctrl Pts',(-5.00849138300006,11.6,9.81461182699999));
#238660=CARTESIAN_POINT('Ctrl Pts',(-5.01077179700006,15.2,9.81671434299999));
#238661=CARTESIAN_POINT('Ctrl Pts',(-5.01077179700006,11.6,9.81671434299999));
#238662=CARTESIAN_POINT('Ctrl Pts',(-5.01305778100006,15.2,9.81881856699999));
#238663=CARTESIAN_POINT('Ctrl Pts',(-5.01305778100006,11.6,9.81881856699999));
#238664=CARTESIAN_POINT('Ctrl Pts',(-5.01534933700006,15.2,9.82092448699999));
#238665=CARTESIAN_POINT('Ctrl Pts',(-5.01534933700006,11.6,9.82092448699999));
#238666=CARTESIAN_POINT('Ctrl Pts',(-5.01764646100006,15.2,9.82303208999999));
#238667=CARTESIAN_POINT('Ctrl Pts',(-5.01764646100006,11.6,9.82303208999999));
#238668=CARTESIAN_POINT('Ctrl Pts',(-5.01994915100005,15.2,9.82514136699999));
#238669=CARTESIAN_POINT('Ctrl Pts',(-5.01994915100005,11.6,9.82514136699999));
#238670=CARTESIAN_POINT('Ctrl Pts',(-5.02225740500006,15.2,9.82725230399998));
#238671=CARTESIAN_POINT('Ctrl Pts',(-5.02225740500006,11.6,9.82725230399998));
#238672=CARTESIAN_POINT('Ctrl Pts',(-5.02457122300005,15.2,9.82936489099998));
#238673=CARTESIAN_POINT('Ctrl Pts',(-5.02457122300005,11.6,9.82936489099998));
#238674=CARTESIAN_POINT('Ctrl Pts',(-5.02689060100006,15.2,9.83147911699999));
#238675=CARTESIAN_POINT('Ctrl Pts',(-5.02689060100006,11.6,9.83147911699999));
#238676=CARTESIAN_POINT('Ctrl Pts',(-5.02921553800006,15.2,9.83359496999999));
#238677=CARTESIAN_POINT('Ctrl Pts',(-5.02921553800006,11.6,9.83359496999999));
#238678=CARTESIAN_POINT('Ctrl Pts',(-5.03154603200006,15.2,9.83571243799998));
#238679=CARTESIAN_POINT('Ctrl Pts',(-5.03154603200006,11.6,9.83571243799998));
#238680=CARTESIAN_POINT('Ctrl Pts',(-5.03388208200006,15.2,9.83783151099999));
#238681=CARTESIAN_POINT('Ctrl Pts',(-5.03388208200006,11.6,9.83783151099999));
#238682=CARTESIAN_POINT('Ctrl Pts',(-5.03622368600006,15.2,9.83995217699999));
#238683=CARTESIAN_POINT('Ctrl Pts',(-5.03622368600006,11.6,9.83995217699999));
#238684=CARTESIAN_POINT('Ctrl Pts',(-5.03857084100006,15.2,9.84207442399999));
#238685=CARTESIAN_POINT('Ctrl Pts',(-5.03857084100006,11.6,9.84207442399999));
#238686=CARTESIAN_POINT('Ctrl Pts',(-5.04092354500006,15.2,9.84419824299999));
#238687=CARTESIAN_POINT('Ctrl Pts',(-5.04092354500006,11.6,9.84419824299999));
#238688=CARTESIAN_POINT('Ctrl Pts',(-5.04328179800006,15.2,9.84632361999999));
#238689=CARTESIAN_POINT('Ctrl Pts',(-5.04328179800006,11.6,9.84632361999999));
#238690=CARTESIAN_POINT('Ctrl Pts',(-5.04564559600006,15.2,9.84845054499999));
#238691=CARTESIAN_POINT('Ctrl Pts',(-5.04564559600006,11.6,9.84845054499999));
#238692=CARTESIAN_POINT('Ctrl Pts',(-5.04801493800006,15.2,9.85057900699999));
#238693=CARTESIAN_POINT('Ctrl Pts',(-5.04801493800006,11.6,9.85057900699999));
#238694=CARTESIAN_POINT('Ctrl Pts',(-5.05038982300006,15.2,9.85270899499999));
#238695=CARTESIAN_POINT('Ctrl Pts',(-5.05038982300006,11.6,9.85270899499999));
#238696=CARTESIAN_POINT('Ctrl Pts',(-5.05277024800006,15.2,9.85484049699998));
#238697=CARTESIAN_POINT('Ctrl Pts',(-5.05277024800006,11.6,9.85484049699998));
#238698=CARTESIAN_POINT('Ctrl Pts',(-5.05515621200006,15.2,9.85697350299999));
#238699=CARTESIAN_POINT('Ctrl Pts',(-5.05515621200006,11.6,9.85697350299999));
#238700=CARTESIAN_POINT('Ctrl Pts',(-5.05754771100006,15.2,9.85910800099998));
#238701=CARTESIAN_POINT('Ctrl Pts',(-5.05754771100006,11.6,9.85910800099998));
#238702=CARTESIAN_POINT('Ctrl Pts',(-5.05994474700006,15.2,9.86124398099999));
#238703=CARTESIAN_POINT('Ctrl Pts',(-5.05994474700006,11.6,9.86124398099999));
#238704=CARTESIAN_POINT('Ctrl Pts',(-5.06234731400006,15.2,9.86338143099999));
#238705=CARTESIAN_POINT('Ctrl Pts',(-5.06234731400006,11.6,9.86338143099999));
#238706=CARTESIAN_POINT('Ctrl Pts',(-5.06475541200006,15.2,9.86552034099999));
#238707=CARTESIAN_POINT('Ctrl Pts',(-5.06475541200006,11.6,9.86552034099999));
#238708=CARTESIAN_POINT('Ctrl Pts',(-5.06716903900006,15.2,9.86766069799998));
#238709=CARTESIAN_POINT('Ctrl Pts',(-5.06716903900006,11.6,9.86766069799998));
#238710=CARTESIAN_POINT('Ctrl Pts',(-5.06958819300006,15.2,9.86980249299998));
#238711=CARTESIAN_POINT('Ctrl Pts',(-5.06958819300006,11.6,9.86980249299998));
#238712=CARTESIAN_POINT('Ctrl Pts',(-5.07201287200005,15.2,9.87194571499998));
#238713=CARTESIAN_POINT('Ctrl Pts',(-5.07201287200005,11.6,9.87194571499998));
#238714=CARTESIAN_POINT('Ctrl Pts',(-5.07444307400006,15.2,9.87409035099999));
#238715=CARTESIAN_POINT('Ctrl Pts',(-5.07444307400006,11.6,9.87409035099999));
#238716=CARTESIAN_POINT('Ctrl Pts',(-5.07687879800006,15.2,9.87623639299999));
#238717=CARTESIAN_POINT('Ctrl Pts',(-5.07687879800006,11.6,9.87623639299999));
#238718=CARTESIAN_POINT('Ctrl Pts',(-5.07932004000006,15.2,9.87838382899999));
#238719=CARTESIAN_POINT('Ctrl Pts',(-5.07932004000006,11.6,9.87838382899999));
#238720=CARTESIAN_POINT('Ctrl Pts',(-5.08176679900005,15.2,9.88053264699998));
#238721=CARTESIAN_POINT('Ctrl Pts',(-5.08176679900005,11.6,9.88053264699998));
#238722=CARTESIAN_POINT('Ctrl Pts',(-5.08421907400006,15.2,9.88268283699998));
#238723=CARTESIAN_POINT('Ctrl Pts',(-5.08421907400006,11.6,9.88268283699998));
#238724=CARTESIAN_POINT('Ctrl Pts',(-5.08667686200006,15.2,9.88483438899999));
#238725=CARTESIAN_POINT('Ctrl Pts',(-5.08667686200006,11.6,9.88483438899999));
#238726=CARTESIAN_POINT('Ctrl Pts',(-5.08914016200006,15.2,9.88698729199999));
#238727=CARTESIAN_POINT('Ctrl Pts',(-5.08914016200006,11.6,9.88698729199999));
#238728=CARTESIAN_POINT('Ctrl Pts',(-5.09160897100006,15.2,9.88914153399998));
#238729=CARTESIAN_POINT('Ctrl Pts',(-5.09160897100006,11.6,9.88914153399998));
#238730=CARTESIAN_POINT('Ctrl Pts',(-5.09408328700006,15.2,9.89129710499999));
#238731=CARTESIAN_POINT('Ctrl Pts',(-5.09408328700006,11.6,9.89129710499999));
#238732=CARTESIAN_POINT('Ctrl Pts',(-5.09656311000006,15.2,9.89345399499998));
#238733=CARTESIAN_POINT('Ctrl Pts',(-5.09656311000006,11.6,9.89345399499998));
#238734=CARTESIAN_POINT('Ctrl Pts',(-5.09904843500006,15.2,9.89561219199998));
#238735=CARTESIAN_POINT('Ctrl Pts',(-5.09904843500006,11.6,9.89561219199998));
#238736=CARTESIAN_POINT('Ctrl Pts',(-5.10153926200006,15.2,9.89777168599998));
#238737=CARTESIAN_POINT('Ctrl Pts',(-5.10153926200006,11.6,9.89777168599998));
#238738=CARTESIAN_POINT('Ctrl Pts',(-5.10403558800006,15.2,9.89993246799998));
#238739=CARTESIAN_POINT('Ctrl Pts',(-5.10403558800006,11.6,9.89993246799998));
#238740=CARTESIAN_POINT('Ctrl Pts',(-5.10653741200006,15.2,9.90209452499998));
#238741=CARTESIAN_POINT('Ctrl Pts',(-5.10653741200006,11.6,9.90209452499998));
#238742=CARTESIAN_POINT('Ctrl Pts',(-5.10904473100006,15.2,9.90425784699998));
#238743=CARTESIAN_POINT('Ctrl Pts',(-5.10904473100006,11.6,9.90425784699998));
#238744=CARTESIAN_POINT('Ctrl Pts',(-5.11155754400006,15.2,9.90642242299998));
#238745=CARTESIAN_POINT('Ctrl Pts',(-5.11155754400006,11.6,9.90642242299998));
#238746=CARTESIAN_POINT('Ctrl Pts',(-5.11407584900006,15.2,9.90858824399999));
#238747=CARTESIAN_POINT('Ctrl Pts',(-5.11407584900006,11.6,9.90858824399999));
#238748=CARTESIAN_POINT('Ctrl Pts',(-5.11659964300006,15.2,9.91075529899998));
#238749=CARTESIAN_POINT('Ctrl Pts',(-5.11659964300006,11.6,9.91075529899998));
#238750=CARTESIAN_POINT('Ctrl Pts',(-5.11912892400006,15.2,9.91292357699999));
#238751=CARTESIAN_POINT('Ctrl Pts',(-5.11912892400006,11.6,9.91292357699999));
#238752=CARTESIAN_POINT('Ctrl Pts',(-5.12166369100005,15.2,9.91509306699999));
#238753=CARTESIAN_POINT('Ctrl Pts',(-5.12166369100005,11.6,9.91509306699999));
#238754=CARTESIAN_POINT('Ctrl Pts',(-5.12420394100006,15.2,9.91726375999999));
#238755=CARTESIAN_POINT('Ctrl Pts',(-5.12420394100006,11.6,9.91726375999999));
#238756=CARTESIAN_POINT('Ctrl Pts',(-5.12674967300006,15.2,9.91943564499999));
#238757=CARTESIAN_POINT('Ctrl Pts',(-5.12674967300006,11.6,9.91943564499999));
#238758=CARTESIAN_POINT('Ctrl Pts',(-5.12930088400006,15.2,9.92160870999999));
#238759=CARTESIAN_POINT('Ctrl Pts',(-5.12930088400006,11.6,9.92160870999999));
#238760=CARTESIAN_POINT('Ctrl Pts',(-5.13185757200006,15.2,9.92378294799998));
#238761=CARTESIAN_POINT('Ctrl Pts',(-5.13185757200006,11.6,9.92378294799998));
#238762=CARTESIAN_POINT('Ctrl Pts',(-5.13441973600006,15.2,9.92595834399999));
#238763=CARTESIAN_POINT('Ctrl Pts',(-5.13441973600006,11.6,9.92595834399999));
#238764=CARTESIAN_POINT('Ctrl Pts',(-5.13698737300006,15.2,9.92813489299999));
#238765=CARTESIAN_POINT('Ctrl Pts',(-5.13698737300006,11.6,9.92813489299999));
#238766=CARTESIAN_POINT('Ctrl Pts',(-5.13956048100006,15.2,9.93031258099998));
#238767=CARTESIAN_POINT('Ctrl Pts',(-5.13956048100006,11.6,9.93031258099998));
#238768=CARTESIAN_POINT('Ctrl Pts',(-5.14213905800006,15.2,9.93249139799998));
#238769=CARTESIAN_POINT('Ctrl Pts',(-5.14213905800006,11.6,9.93249139799998));
#238770=CARTESIAN_POINT('Ctrl Pts',(-5.14472310200006,15.2,9.93467133499998));
#238771=CARTESIAN_POINT('Ctrl Pts',(-5.14472310200006,11.6,9.93467133499998));
#238772=CARTESIAN_POINT('Ctrl Pts',(-5.14731261100006,15.2,9.93685238099999));
#238773=CARTESIAN_POINT('Ctrl Pts',(-5.14731261100006,11.6,9.93685238099999));
#238774=CARTESIAN_POINT('Ctrl Pts',(-5.14990758400006,15.2,9.93903452699998));
#238775=CARTESIAN_POINT('Ctrl Pts',(-5.14990758400006,11.6,9.93903452699998));
#238776=CARTESIAN_POINT('Ctrl Pts',(-5.15250801600006,15.2,9.94121776099998));
#238777=CARTESIAN_POINT('Ctrl Pts',(-5.15250801600006,11.6,9.94121776099998));
#238778=CARTESIAN_POINT('Ctrl Pts',(-5.15511390900006,15.2,9.94340207299999));
#238779=CARTESIAN_POINT('Ctrl Pts',(-5.15511390900006,11.6,9.94340207299999));
#238780=CARTESIAN_POINT('Ctrl Pts',(-5.15772525600006,15.2,9.94558745399999));
#238781=CARTESIAN_POINT('Ctrl Pts',(-5.15772525600006,11.6,9.94558745399999));
#238782=CARTESIAN_POINT('Ctrl Pts',(-5.16034206000006,15.2,9.94777389299998));
#238783=CARTESIAN_POINT('Ctrl Pts',(-5.16034206000006,11.6,9.94777389299998));
#238784=CARTESIAN_POINT('Ctrl Pts',(-5.16296431600006,15.2,9.94996137999999));
#238785=CARTESIAN_POINT('Ctrl Pts',(-5.16296431600006,11.6,9.94996137999999));
#238786=CARTESIAN_POINT('Ctrl Pts',(-5.16559202200006,15.2,9.95214990599998));
#238787=CARTESIAN_POINT('Ctrl Pts',(-5.16559202200006,11.6,9.95214990599998));
#238788=CARTESIAN_POINT('Ctrl Pts',(-5.16822517700006,15.2,9.95433945799999));
#238789=CARTESIAN_POINT('Ctrl Pts',(-5.16822517700006,11.6,9.95433945799999));
#238790=CARTESIAN_POINT('Ctrl Pts',(-5.17086377800006,15.2,9.95653002999998));
#238791=CARTESIAN_POINT('Ctrl Pts',(-5.17086377800006,11.6,9.95653002999998));
#238792=CARTESIAN_POINT('Ctrl Pts',(-5.17350782200006,15.2,9.95872160899999));
#238793=CARTESIAN_POINT('Ctrl Pts',(-5.17350782200006,11.6,9.95872160899999));
#238794=CARTESIAN_POINT('Ctrl Pts',(-5.17615730900006,15.2,9.96091418599999));
#238795=CARTESIAN_POINT('Ctrl Pts',(-5.17615730900006,11.6,9.96091418599999));
#238796=CARTESIAN_POINT('Ctrl Pts',(-5.17881223600006,15.2,9.96310774999999));
#238797=CARTESIAN_POINT('Ctrl Pts',(-5.17881223600006,11.6,9.96310774999999));
#238798=CARTESIAN_POINT('Ctrl Pts',(-5.18147260100006,15.2,9.96530229299999));
#238799=CARTESIAN_POINT('Ctrl Pts',(-5.18147260100006,11.6,9.96530229299999));
#238800=CARTESIAN_POINT('Ctrl Pts',(-5.18413840200005,15.2,9.96749780299999));
#238801=CARTESIAN_POINT('Ctrl Pts',(-5.18413840200005,11.6,9.96749780299999));
#238802=CARTESIAN_POINT('Ctrl Pts',(-5.18680963500006,15.2,9.96969427199998));
#238803=CARTESIAN_POINT('Ctrl Pts',(-5.18680963500006,11.6,9.96969427199998));
#238804=CARTESIAN_POINT('Ctrl Pts',(-5.18948630100006,15.2,9.97189168799999));
#238805=CARTESIAN_POINT('Ctrl Pts',(-5.18948630100006,11.6,9.97189168799999));
#238806=CARTESIAN_POINT('Ctrl Pts',(-5.19216839500006,15.2,9.97409004199999));
#238807=CARTESIAN_POINT('Ctrl Pts',(-5.19216839500006,11.6,9.97409004199999));
#238808=CARTESIAN_POINT('Ctrl Pts',(-5.19485591800006,15.2,9.97628932499998));
#238809=CARTESIAN_POINT('Ctrl Pts',(-5.19485591800006,11.6,9.97628932499998));
#238810=CARTESIAN_POINT('Ctrl Pts',(-5.19754886400006,15.2,9.97848952599998));
#238811=CARTESIAN_POINT('Ctrl Pts',(-5.19754886400006,11.6,9.97848952599998));
#238812=CARTESIAN_POINT('Ctrl Pts',(-5.20024723500006,15.2,9.98069063599999));
#238813=CARTESIAN_POINT('Ctrl Pts',(-5.20024723500006,11.6,9.98069063599999));
#238814=CARTESIAN_POINT('Ctrl Pts',(-5.20295102500006,15.2,9.98289264499999));
#238815=CARTESIAN_POINT('Ctrl Pts',(-5.20295102500006,11.6,9.98289264499999));
#238816=CARTESIAN_POINT('Ctrl Pts',(-5.20566023400006,15.2,9.98509554099999));
#238817=CARTESIAN_POINT('Ctrl Pts',(-5.20566023400006,11.6,9.98509554099999));
#238818=CARTESIAN_POINT('Ctrl Pts',(-5.20837486000006,15.2,9.98729931899998));
#238819=CARTESIAN_POINT('Ctrl Pts',(-5.20837486000006,11.6,9.98729931899998));
#238820=CARTESIAN_POINT('Ctrl Pts',(-5.21109490000006,15.2,9.98950396499998));
#238821=CARTESIAN_POINT('Ctrl Pts',(-5.21109490000006,11.6,9.98950396499998));
#238822=CARTESIAN_POINT('Ctrl Pts',(-5.21382035100006,15.2,9.99170947099999));
#238823=CARTESIAN_POINT('Ctrl Pts',(-5.21382035100006,11.6,9.99170947099999));
#238824=CARTESIAN_POINT('Ctrl Pts',(-5.21655121300006,15.2,9.99391582499998));
#238825=CARTESIAN_POINT('Ctrl Pts',(-5.21655121300006,11.6,9.99391582499998));
#238826=CARTESIAN_POINT('Ctrl Pts',(-5.21928748300006,15.2,9.99612302199999));
#238827=CARTESIAN_POINT('Ctrl Pts',(-5.21928748300006,11.6,9.99612302199999));
#238828=CARTESIAN_POINT('Ctrl Pts',(-5.22202915800006,15.2,9.99833104799999));
#238829=CARTESIAN_POINT('Ctrl Pts',(-5.22202915800006,11.6,9.99833104799999));
#238830=CARTESIAN_POINT('Ctrl Pts',(-5.22477623600006,15.2,10.000539896));
#238831=CARTESIAN_POINT('Ctrl Pts',(-5.22477623600006,11.6,10.000539896));
#238832=CARTESIAN_POINT('Ctrl Pts',(-5.22752871700006,15.2,10.002749555));
#238833=CARTESIAN_POINT('Ctrl Pts',(-5.22752871700006,11.6,10.002749555));
#238834=CARTESIAN_POINT('Ctrl Pts',(-5.23028659500006,15.2,10.004960015));
#238835=CARTESIAN_POINT('Ctrl Pts',(-5.23028659500006,11.6,10.004960015));
#238836=CARTESIAN_POINT('Ctrl Pts',(-5.23304987100006,15.2,10.007171268));
#238837=CARTESIAN_POINT('Ctrl Pts',(-5.23304987100006,11.6,10.007171268));
#238838=CARTESIAN_POINT('Ctrl Pts',(-5.23581854200006,15.2,10.009383303));
#238839=CARTESIAN_POINT('Ctrl Pts',(-5.23581854200006,11.6,10.009383303));
#238840=CARTESIAN_POINT('Ctrl Pts',(-5.23859260500006,15.2,10.011596111));
#238841=CARTESIAN_POINT('Ctrl Pts',(-5.23859260500006,11.6,10.011596111));
#238842=CARTESIAN_POINT('Ctrl Pts',(-5.24137205800006,15.2,10.013809682));
#238843=CARTESIAN_POINT('Ctrl Pts',(-5.24137205800006,11.6,10.013809682));
#238844=CARTESIAN_POINT('Ctrl Pts',(-5.24415689800006,15.2,10.016024007));
#238845=CARTESIAN_POINT('Ctrl Pts',(-5.24415689800006,11.6,10.016024007));
#238846=CARTESIAN_POINT('Ctrl Pts',(-5.24694712600006,15.2,10.018239077));
#238847=CARTESIAN_POINT('Ctrl Pts',(-5.24694712600006,11.6,10.018239077));
#238848=CARTESIAN_POINT('Ctrl Pts',(-5.24974273600006,15.2,10.020454882));
#238849=CARTESIAN_POINT('Ctrl Pts',(-5.24974273600006,11.6,10.020454882));
#238850=CARTESIAN_POINT('Ctrl Pts',(-5.25254372800006,15.2,10.022671411));
#238851=CARTESIAN_POINT('Ctrl Pts',(-5.25254372800006,11.6,10.022671411));
#238852=CARTESIAN_POINT('Ctrl Pts',(-5.25535010000006,15.2,10.024888657));
#238853=CARTESIAN_POINT('Ctrl Pts',(-5.25535010000006,11.6,10.024888657));
#238854=CARTESIAN_POINT('Ctrl Pts',(-5.25816184700005,15.2,10.02710661));
#238855=CARTESIAN_POINT('Ctrl Pts',(-5.25816184700005,11.6,10.02710661));
#238856=CARTESIAN_POINT('Ctrl Pts',(-5.26097897100006,15.2,10.02932526));
#238857=CARTESIAN_POINT('Ctrl Pts',(-5.26097897100006,11.6,10.02932526));
#238858=CARTESIAN_POINT('Ctrl Pts',(-5.26380146600006,15.2,10.031544597));
#238859=CARTESIAN_POINT('Ctrl Pts',(-5.26380146600006,11.6,10.031544597));
#238860=CARTESIAN_POINT('Ctrl Pts',(-5.26662933100006,15.2,10.033764612));
#238861=CARTESIAN_POINT('Ctrl Pts',(-5.26662933100006,11.6,10.033764612));
#238862=CARTESIAN_POINT('Ctrl Pts',(-5.26946256500006,15.2,10.035985297));
#238863=CARTESIAN_POINT('Ctrl Pts',(-5.26946256500006,11.6,10.035985297));
#238864=CARTESIAN_POINT('Ctrl Pts',(-5.27230116500006,15.2,10.038206641));
#238865=CARTESIAN_POINT('Ctrl Pts',(-5.27230116500006,11.6,10.038206641));
#238866=CARTESIAN_POINT('Ctrl Pts',(-5.27514512800006,15.2,10.040428636));
#238867=CARTESIAN_POINT('Ctrl Pts',(-5.27514512800006,11.6,10.040428636));
#238868=CARTESIAN_POINT('Ctrl Pts',(-5.27799445100006,15.2,10.042651272));
#238869=CARTESIAN_POINT('Ctrl Pts',(-5.27799445100006,11.6,10.042651272));
#238870=CARTESIAN_POINT('Ctrl Pts',(-5.28084913500006,15.2,10.044874539));
#238871=CARTESIAN_POINT('Ctrl Pts',(-5.28084913500006,11.6,10.044874539));
#238872=CARTESIAN_POINT('Ctrl Pts',(-5.28370917500006,15.2,10.047098429));
#238873=CARTESIAN_POINT('Ctrl Pts',(-5.28370917500006,11.6,10.047098429));
#238874=CARTESIAN_POINT('Ctrl Pts',(-5.28657456900006,15.2,10.049322933));
#238875=CARTESIAN_POINT('Ctrl Pts',(-5.28657456900006,11.6,10.049322933));
#238876=CARTESIAN_POINT('Ctrl Pts',(-5.28944531600006,15.2,10.05154804));
#238877=CARTESIAN_POINT('Ctrl Pts',(-5.28944531600006,11.6,10.05154804));
#238878=CARTESIAN_POINT('Ctrl Pts',(-5.29232141300006,15.2,10.053773742));
#238879=CARTESIAN_POINT('Ctrl Pts',(-5.29232141300006,11.6,10.053773742));
#238880=CARTESIAN_POINT('Ctrl Pts',(-5.29520285700006,15.2,10.056000029));
#238881=CARTESIAN_POINT('Ctrl Pts',(-5.29520285700006,11.6,10.056000029));
#238882=CARTESIAN_POINT('Ctrl Pts',(-5.29808964700006,15.2,10.058226893));
#238883=CARTESIAN_POINT('Ctrl Pts',(-5.29808964700006,11.6,10.058226893));
#238884=CARTESIAN_POINT('Ctrl Pts',(-5.30098178000006,15.2,10.060454325));
#238885=CARTESIAN_POINT('Ctrl Pts',(-5.30098178000006,11.6,10.060454325));
#238886=CARTESIAN_POINT('Ctrl Pts',(-5.30387925400006,15.2,10.062682315));
#238887=CARTESIAN_POINT('Ctrl Pts',(-5.30387925400006,11.6,10.062682315));
#238888=CARTESIAN_POINT('Ctrl Pts',(-5.30678206600006,15.2,10.064910854));
#238889=CARTESIAN_POINT('Ctrl Pts',(-5.30678206600006,11.6,10.064910854));
#238890=CARTESIAN_POINT('Ctrl Pts',(-5.30969021500006,15.2,10.067139933));
#238891=CARTESIAN_POINT('Ctrl Pts',(-5.30969021500006,11.6,10.067139933));
#238892=CARTESIAN_POINT('Ctrl Pts',(-5.31260369800005,15.2,10.069369543));
#238893=CARTESIAN_POINT('Ctrl Pts',(-5.31260369800005,11.6,10.069369543));
#238894=CARTESIAN_POINT('Ctrl Pts',(-5.31552251300006,15.2,10.071599674));
#238895=CARTESIAN_POINT('Ctrl Pts',(-5.31552251300006,11.6,10.071599674));
#238896=CARTESIAN_POINT('Ctrl Pts',(-5.31844665700006,15.2,10.073830318));
#238897=CARTESIAN_POINT('Ctrl Pts',(-5.31844665700006,11.6,10.073830318));
#238898=CARTESIAN_POINT('Ctrl Pts',(-5.32137612800006,15.2,10.076061465));
#238899=CARTESIAN_POINT('Ctrl Pts',(-5.32137612800006,11.6,10.076061465));
#238900=CARTESIAN_POINT('Ctrl Pts',(-5.32431092300006,15.2,10.078293108));
#238901=CARTESIAN_POINT('Ctrl Pts',(-5.32431092300006,11.6,10.078293108));
#238902=CARTESIAN_POINT('Ctrl Pts',(-5.32725104100006,15.2,10.080525236));
#238903=CARTESIAN_POINT('Ctrl Pts',(-5.32725104100006,11.6,10.080525236));
#238904=CARTESIAN_POINT('Ctrl Pts',(-5.33019647900006,15.2,10.08275784));
#238905=CARTESIAN_POINT('Ctrl Pts',(-5.33019647900006,11.6,10.08275784));
#238906=CARTESIAN_POINT('Ctrl Pts',(-5.33314723600006,15.2,10.084990912));
#238907=CARTESIAN_POINT('Ctrl Pts',(-5.33314723600006,11.6,10.084990912));
#238908=CARTESIAN_POINT('Ctrl Pts',(-5.33610330800006,15.2,10.087224443));
#238909=CARTESIAN_POINT('Ctrl Pts',(-5.33610330800006,11.6,10.087224443));
#238910=CARTESIAN_POINT('Ctrl Pts',(-5.33906469200006,15.2,10.089458424));
#238911=CARTESIAN_POINT('Ctrl Pts',(-5.33906469200006,11.6,10.089458424));
#238912=CARTESIAN_POINT('Ctrl Pts',(-5.34203138800006,15.2,10.091692848));
#238913=CARTESIAN_POINT('Ctrl Pts',(-5.34203138800006,11.6,10.091692848));
#238914=CARTESIAN_POINT('Ctrl Pts',(-5.34500339300005,15.2,10.093927703));
#238915=CARTESIAN_POINT('Ctrl Pts',(-5.34500339300005,11.6,10.093927703));
#238916=CARTESIAN_POINT('Ctrl Pts',(-5.34798070300006,15.2,10.096162981));
#238917=CARTESIAN_POINT('Ctrl Pts',(-5.34798070300006,11.6,10.096162981));
#238918=CARTESIAN_POINT('Ctrl Pts',(-5.35096331800006,15.2,10.098398674));
#238919=CARTESIAN_POINT('Ctrl Pts',(-5.35096331800006,11.6,10.098398674));
#238920=CARTESIAN_POINT('Ctrl Pts',(-5.35395123500006,15.2,10.100634772));
#238921=CARTESIAN_POINT('Ctrl Pts',(-5.35395123500006,11.6,10.100634772));
#238922=CARTESIAN_POINT('Ctrl Pts',(-5.35694445000006,15.2,10.102871266));
#238923=CARTESIAN_POINT('Ctrl Pts',(-5.35694445000006,11.6,10.102871266));
#238924=CARTESIAN_POINT('Ctrl Pts',(-5.35994296100006,15.2,10.105108146));
#238925=CARTESIAN_POINT('Ctrl Pts',(-5.35994296100006,11.6,10.105108146));
#238926=CARTESIAN_POINT('Ctrl Pts',(-5.36294676700006,15.2,10.107345405));
#238927=CARTESIAN_POINT('Ctrl Pts',(-5.36294676700006,11.6,10.107345405));
#238928=CARTESIAN_POINT('Ctrl Pts',(-5.36595586500006,15.2,10.109583033));
#238929=CARTESIAN_POINT('Ctrl Pts',(-5.36595586500006,11.6,10.109583033));
#238930=CARTESIAN_POINT('Ctrl Pts',(-5.36897025300005,15.2,10.111821023));
#238931=CARTESIAN_POINT('Ctrl Pts',(-5.36897025300005,11.6,10.111821023));
#238932=CARTESIAN_POINT('Ctrl Pts',(-5.37198992800006,15.2,10.114059368));
#238933=CARTESIAN_POINT('Ctrl Pts',(-5.37198992800006,11.6,10.114059368));
#238934=CARTESIAN_POINT('Ctrl Pts',(-5.37501489000006,15.2,10.116298058));
#238935=CARTESIAN_POINT('Ctrl Pts',(-5.37501489000006,11.6,10.116298058));
#238936=CARTESIAN_POINT('Ctrl Pts',(-5.37804513400006,15.2,10.118537086));
#238937=CARTESIAN_POINT('Ctrl Pts',(-5.37804513400006,11.6,10.118537086));
#238938=CARTESIAN_POINT('Ctrl Pts',(-5.38108066000006,15.2,10.120776443));
#238939=CARTESIAN_POINT('Ctrl Pts',(-5.38108066000006,11.6,10.120776443));
#238940=CARTESIAN_POINT('Ctrl Pts',(-5.38412146300006,15.2,10.123016119));
#238941=CARTESIAN_POINT('Ctrl Pts',(-5.38412146300006,11.6,10.123016119));
#238942=CARTESIAN_POINT('Ctrl Pts',(-5.38716754200006,15.2,10.125256103));
#238943=CARTESIAN_POINT('Ctrl Pts',(-5.38716754200006,11.6,10.125256103));
#238944=CARTESIAN_POINT('Ctrl Pts',(-5.39021889300006,15.2,10.127496384));
#238945=CARTESIAN_POINT('Ctrl Pts',(-5.39021889300006,11.6,10.127496384));
#238946=CARTESIAN_POINT('Ctrl Pts',(-5.39327551300006,15.2,10.129736951));
#238947=CARTESIAN_POINT('Ctrl Pts',(-5.39327551300006,11.6,10.129736951));
#238948=CARTESIAN_POINT('Ctrl Pts',(-5.39633740000006,15.2,10.131977797));
#238949=CARTESIAN_POINT('Ctrl Pts',(-5.39633740000006,11.6,10.131977797));
#238950=CARTESIAN_POINT('Ctrl Pts',(-5.39940455200006,15.2,10.134218911));
#238951=CARTESIAN_POINT('Ctrl Pts',(-5.39940455200006,11.6,10.134218911));
#238952=CARTESIAN_POINT('Ctrl Pts',(-5.40247696800006,15.2,10.136460288));
#238953=CARTESIAN_POINT('Ctrl Pts',(-5.40247696800006,11.6,10.136460288));
#238954=CARTESIAN_POINT('Ctrl Pts',(-5.40555464400006,15.2,10.138701926));
#238955=CARTESIAN_POINT('Ctrl Pts',(-5.40555464400006,11.6,10.138701926));
#238956=CARTESIAN_POINT('Ctrl Pts',(-5.40863758200006,15.2,10.140943822));
#238957=CARTESIAN_POINT('Ctrl Pts',(-5.40863758200006,11.6,10.140943822));
#238958=CARTESIAN_POINT('Ctrl Pts',(-5.41110814000006,15.2,10.142737544));
#238959=CARTESIAN_POINT('Ctrl Pts',(-5.41110814000006,11.6,10.142737544));
#238960=CARTESIAN_POINT('Ctrl Pts',(-5.41296342700006,15.2,10.144082951));
#238961=CARTESIAN_POINT('Ctrl Pts',(-5.41296342700006,11.6,10.144082951));
#238962=CARTESIAN_POINT('Ctrl Pts',(-5.41420133600006,15.2,10.14497994));
#238963=CARTESIAN_POINT('Ctrl Pts',(-5.41420133600006,11.6,10.14497994));
#238964=CARTESIAN_POINT('Ctrl Pts',(-5.41482055400006,15.2,10.145428447));
#238965=CARTESIAN_POINT('Ctrl Pts',(-5.41482055400006,11.6,10.145428447));
#238966=CARTESIAN_POINT('Ctrl Pts',(-4.57383771200006,15.2,9.31239140099999));
#238967=CARTESIAN_POINT('Ctrl Pts',(-4.57476026596749,15.2,9.31392144227075));
#238968=CARTESIAN_POINT('Ctrl Pts',(-4.57571693063136,15.2,9.31549767344762));
#238969=CARTESIAN_POINT('Ctrl Pts',(-4.57670776761648,15.2,9.31711891458901));
#238970=CARTESIAN_POINT('Ctrl Pts',(-4.57770338291839,15.2,9.3187479741747));
#238971=CARTESIAN_POINT('Ctrl Pts',(-4.57873349932321,15.2,9.32042248440087));
#238972=CARTESIAN_POINT('Ctrl Pts',(-4.57979816360307,15.2,9.32214130041629));
#238973=CARTESIAN_POINT('Ctrl Pts',(-4.58086282778624,15.2,9.32386011627559));
#238974=CARTESIAN_POINT('Ctrl Pts',(-4.58196204052454,15.2,9.3256232394989));
#238975=CARTESIAN_POINT('Ctrl Pts',(-4.58309584848333,15.2,9.32742955643324));
#238976=CARTESIAN_POINT('Ctrl Pts',(-4.58422965644212,15.2,9.32923587336759));
#238977=CARTESIAN_POINT('Ctrl Pts',(-4.58539805581099,15.2,9.33108538570202));
#238978=CARTESIAN_POINT('Ctrl Pts',(-4.5866010919087,15.2,9.33297701280869));
#238979=CARTESIAN_POINT('Ctrl Pts',(-4.58780412811569,15.2,9.33486864008717));
#238980=CARTESIAN_POINT('Ctrl Pts',(-4.58904179835032,15.2,9.3368023811214));
#238981=CARTESIAN_POINT('Ctrl Pts',(-4.59031413942202,15.2,9.33877718823185));
#238982=CARTESIAN_POINT('Ctrl Pts',(-4.59158648037816,15.2,9.3407519951629));
#238983=CARTESIAN_POINT('Ctrl Pts',(-4.59289349278484,15.2,9.34276786523277));
#238984=CARTESIAN_POINT('Ctrl Pts',(-4.59423520699227,15.2,9.34482377850085));
#238985=CARTESIAN_POINT('Ctrl Pts',(-4.59557692119971,15.2,9.34687969176892));
#238986=CARTESIAN_POINT('Ctrl Pts',(-4.59695334020937,15.2,9.34897564855469));
#238987=CARTESIAN_POINT('Ctrl Pts',(-4.59836449115657,15.2,9.35111065189206));
#238988=CARTESIAN_POINT('Ctrl Pts',(-4.59977564223195,15.2,9.35324565542336));
#238989=CARTESIAN_POINT('Ctrl Pts',(-4.60122152508665,15.2,9.35541970736789));
#238990=CARTESIAN_POINT('Ctrl Pts',(-4.60270216441973,15.2,9.35763183999105));
#238991=CARTESIAN_POINT('Ctrl Pts',(-4.60418280361831,15.2,9.35984397241328));
#238992=CARTESIAN_POINT('Ctrl Pts',(-4.6056982021311,15.2,9.36209418225622));
#238993=CARTESIAN_POINT('Ctrl Pts',(-4.60724837732629,15.2,9.3643815288414));
#238994=CARTESIAN_POINT('Ctrl Pts',(-4.60879855252149,15.2,9.3666688754266));
#238995=CARTESIAN_POINT('Ctrl Pts',(-4.61038350695556,15.2,9.3689933576671));
#238996=CARTESIAN_POINT('Ctrl Pts',(-4.6120032588952,15.2,9.37135405532975));
#238997=CARTESIAN_POINT('Ctrl Pts',(-4.61362301083484,15.2,9.3737147529924));
#238998=CARTESIAN_POINT('Ctrl Pts',(-4.61527755807128,15.2,9.37611166566726));
#238999=CARTESIAN_POINT('Ctrl Pts',(-4.61696691709086,15.2,9.37854389649315));
#239000=CARTESIAN_POINT('Ctrl Pts',(-4.6186562762639,15.2,9.38097612753998));
#239001=CARTESIAN_POINT('Ctrl Pts',(-4.62038044845697,15.2,9.38344367610693));
#239002=CARTESIAN_POINT('Ctrl Pts',(-4.62213944263767,15.2,9.38594566816143));
#239003=CARTESIAN_POINT('Ctrl Pts',(-4.6238984366586,15.2,9.38844765998867));
#239004=CARTESIAN_POINT('Ctrl Pts',(-4.62569225330738,15.2,9.3909840917222));
#239005=CARTESIAN_POINT('Ctrl Pts',(-4.62752090224917,15.2,9.39355411272376));
#239006=CARTESIAN_POINT('Ctrl Pts',(-4.62934955119095,15.2,9.39612413372532));
#239007=CARTESIAN_POINT('Ctrl Pts',(-4.63121303150607,15.2,9.39872774061056));
#239008=CARTESIAN_POINT('Ctrl Pts',(-4.63311134851809,15.2,9.40136410067924));
#239009=CARTESIAN_POINT('Ctrl Pts',(-4.63500966570253,15.2,9.4040004609874));
#239010=CARTESIAN_POINT('Ctrl Pts',(-4.63694282087363,15.2,9.40666957294035));
#239011=CARTESIAN_POINT('Ctrl Pts',(-4.63891081506573,15.2,9.40937062233894));
#239012=CARTESIAN_POINT('Ctrl Pts',(-4.64087880907908,15.2,9.41207167149219));
#239013=CARTESIAN_POINT('Ctrl Pts',(-4.64288164336394,15.2,9.4148046567033));
#239014=CARTESIAN_POINT('Ctrl Pts',(-4.64491931629907,15.2,9.41756878094868));
#239015=CARTESIAN_POINT('Ctrl Pts',(-4.64695698923421,15.2,9.42033290519406));
#239016=CARTESIAN_POINT('Ctrl Pts',(-4.64902950220755,15.2,9.42312816917165));
#239017=CARTESIAN_POINT('Ctrl Pts',(-4.6511368510453,15.2,9.42595379248362));
#239018=CARTESIAN_POINT('Ctrl Pts',(-4.65359542481695,15.2,9.42925035318534));
#239019=CARTESIAN_POINT('Ctrl Pts',(-4.65610141511994,15.2,9.43258823538629));
#239020=CARTESIAN_POINT('Ctrl Pts',(-4.65865481324068,15.2,9.43596623177363));
#239021=CARTESIAN_POINT('Ctrl Pts',(-4.66084344008771,15.2,9.4388616570982));
#239022=CARTESIAN_POINT('Ctrl Pts',(-4.66306689591328,15.2,9.44178655333729));
#239023=CARTESIAN_POINT('Ctrl Pts',(-4.66532517374552,15.2,9.44474017689466));
#239024=CARTESIAN_POINT('Ctrl Pts',(-4.66758345178288,15.2,9.44769380072034));
#239025=CARTESIAN_POINT('Ctrl Pts',(-4.66987655041343,15.2,9.45067615305848));
#239026=CARTESIAN_POINT('Ctrl Pts',(-4.67220445949194,15.2,9.45368650504122));
#239027=CARTESIAN_POINT('Ctrl Pts',(-4.67453236835901,15.2,9.45669685675053));
#239028=CARTESIAN_POINT('Ctrl Pts',(-4.67689508776213,15.2,9.45973520739468));
#239029=CARTESIAN_POINT('Ctrl Pts',(-4.67929260275832,15.2,9.46280084678327));
#239030=CARTESIAN_POINT('Ctrl Pts',(-4.68169011775453,15.2,9.46586648617186));
#239031=CARTESIAN_POINT('Ctrl Pts',(-4.68412243088815,15.2,9.46895940989894));
#239032=CARTESIAN_POINT('Ctrl Pts',(-4.68658952400309,15.2,9.4720789246899));
#239033=CARTESIAN_POINT('Ctrl Pts',(-4.68864543500689,15.2,9.47467852044349));
#239034=CARTESIAN_POINT('Ctrl Pts',(-4.69072549924712,15.2,9.47729657986748));
#239035=CARTESIAN_POINT('Ctrl Pts',(-4.69282970737086,15.2,9.47993270806098));
#239036=CARTESIAN_POINT('Ctrl Pts',(-4.6949339154946,15.2,9.48256883625449));
#239037=CARTESIAN_POINT('Ctrl Pts',(-4.6970622661773,15.2,9.48522303222623));
#239038=CARTESIAN_POINT('Ctrl Pts',(-4.6992147478427,15.2,9.48789490555864));
#239039=CARTESIAN_POINT('Ctrl Pts',(-4.70136722950811,15.2,9.49056677889104));
#239040=CARTESIAN_POINT('Ctrl Pts',(-4.70354384382776,15.2,9.49325633019734));
#239041=CARTESIAN_POINT('Ctrl Pts',(-4.70574457703213,15.2,9.49596317597347));
#239042=CARTESIAN_POINT('Ctrl Pts',(-4.70882560356623,15.2,9.49975276011908));
#239043=CARTESIAN_POINT('Ctrl Pts',(-4.71195390343062,15.2,9.50357623959669));
#239044=CARTESIAN_POINT('Ctrl Pts',(-4.71512944035681,15.2,9.50743258263018));
#239045=CARTESIAN_POINT('Ctrl Pts',(-4.71739768098306,15.2,9.51018711332549));
#239046=CARTESIAN_POINT('Ctrl Pts',(-4.71969002076825,15.2,9.51295841089987));
#239047=CARTESIAN_POINT('Ctrl Pts',(-4.72200644651065,15.2,9.51574610687361));
#239048=CARTESIAN_POINT('Ctrl Pts',(-4.72432287225306,15.2,9.51853380284735));
#239049=CARTESIAN_POINT('Ctrl Pts',(-4.72666338292401,15.2,9.52133789712864));
#239050=CARTESIAN_POINT('Ctrl Pts',(-4.72902796355096,15.2,9.52415802560216));
#239051=CARTESIAN_POINT('Ctrl Pts',(-4.73186546020021,15.2,9.52754217964744));
#239052=CARTESIAN_POINT('Ctrl Pts',(-4.73473761700197,15.2,9.53094942444381));
#239053=CARTESIAN_POINT('Ctrl Pts',(-4.73764440299298,15.2,9.5343791415015));
#239054=CARTESIAN_POINT('Ctrl Pts',(-4.74006672474018,15.2,9.53723723915343));
#239055=CARTESIAN_POINT('Ctrl Pts',(-4.74251309794936,15.2,9.54011094335487));
#239056=CARTESIAN_POINT('Ctrl Pts',(-4.74498350114504,15.2,9.54299990189731));
#239057=CARTESIAN_POINT('Ctrl Pts',(-4.74794798487213,15.2,9.54646665202229));
#239058=CARTESIAN_POINT('Ctrl Pts',(-4.75094707373819,15.2,9.54995537003719));
#239059=CARTESIAN_POINT('Ctrl Pts',(-4.75398073454314,15.2,9.5534654580754));
#239060=CARTESIAN_POINT('Ctrl Pts',(-4.75650878530578,15.2,9.55639053154686));
#239061=CARTESIAN_POINT('Ctrl Pts',(-4.75906084568695,15.2,9.5593304440794));
#239062=CARTESIAN_POINT('Ctrl Pts',(-4.76163689403192,15.2,9.56228485923167));
#239063=CARTESIAN_POINT('Ctrl Pts',(-4.76421294237689,15.2,9.56523927438394));
#239064=CARTESIAN_POINT('Ctrl Pts',(-4.76681298099999,15.2,9.56820818934995));
#239065=CARTESIAN_POINT('Ctrl Pts',(-4.76943698599999,15.2,9.57119127122495));
#239066=CARTESIAN_POINT('Ctrl Pts',(-4.77206099099999,15.2,9.57417435309995));
#239067=CARTESIAN_POINT('Ctrl Pts',(-4.77470896513332,15.2,9.57717160057217));
#239068=CARTESIAN_POINT('Ctrl Pts',(-4.77738088575833,15.2,9.58018268501661));
#239069=CARTESIAN_POINT('Ctrl Pts',(-4.78005280638332,15.2,9.58319376946106));
#239070=CARTESIAN_POINT('Ctrl Pts',(-4.78274867302241,15.2,9.58621869019334));
#239071=CARTESIAN_POINT('Ctrl Pts',(-4.78546846449315,15.2,9.58925712152662));
#239072=CARTESIAN_POINT('Ctrl Pts',(-4.7881882559639,15.2,9.5922955528599));
#239073=CARTESIAN_POINT('Ctrl Pts',(-4.79093197165212,15.2,9.59534749539425));
#239074=CARTESIAN_POINT('Ctrl Pts',(-4.79369958818114,15.2,9.59841262970049));
#239075=CARTESIAN_POINT('Ctrl Pts',(-4.79646720471015,15.2,9.60147776400672));
#239076=CARTESIAN_POINT('Ctrl Pts',(-4.79925872137746,15.2,9.60455608719596));
#239077=CARTESIAN_POINT('Ctrl Pts',(-4.80207411693426,15.2,9.60764728671052));
#239078=CARTESIAN_POINT('Ctrl Pts',(-4.80432643319557,15.2,9.61012024612001));
#239079=CARTESIAN_POINT('Ctrl Pts',(-4.80659403095663,15.2,9.61260144500197));
#239080=CARTESIAN_POINT('Ctrl Pts',(-4.80887689616048,15.2,9.61509072458878));
#239081=CARTESIAN_POINT('Ctrl Pts',(-4.81115976167537,15.2,9.61758000451475));
#239082=CARTESIAN_POINT('Ctrl Pts',(-4.81345789653998,15.2,9.62007736431501));
#239083=CARTESIAN_POINT('Ctrl Pts',(-4.8157712872226,15.2,9.62258264672984));
#239084=CARTESIAN_POINT('Ctrl Pts',(-4.81808467759003,15.2,9.62508792880332));
#239085=CARTESIAN_POINT('Ctrl Pts',(-4.82041332386271,15.2,9.6276011322502));
#239086=CARTESIAN_POINT('Ctrl Pts',(-4.82275721339178,15.2,9.63012210182111));
#239087=CARTESIAN_POINT('Ctrl Pts',(-4.8251011032402,15.2,9.63264307173551));
#239088=CARTESIAN_POINT('Ctrl Pts',(-4.82746023410303,15.2,9.63517180770189));
#239089=CARTESIAN_POINT('Ctrl Pts',(-4.82983459474329,15.2,9.63770815551836));
#239090=CARTESIAN_POINT('Ctrl Pts',(-4.83280254538185,15.2,9.64087859011614));
#239091=CARTESIAN_POINT('Ctrl Pts',(-4.83579429141281,15.2,9.64406091733611));
#239092=CARTESIAN_POINT('Ctrl Pts',(-4.83880980620569,15.2,9.64725483872557));
#239093=CARTESIAN_POINT('Ctrl Pts',(-4.84122221784278,15.2,9.64980997562827));
#239094=CARTESIAN_POINT('Ctrl Pts',(-4.84364984006019,15.2,9.65237253423784));
#239095=CARTESIAN_POINT('Ctrl Pts',(-4.84609266035894,15.2,9.65494236063813));
#239096=CARTESIAN_POINT('Ctrl Pts',(-4.84853548099051,15.2,9.65751218738855));
#239097=CARTESIAN_POINT('Ctrl Pts',(-4.85099350050283,15.2,9.66008928352968));
#239098=CARTESIAN_POINT('Ctrl Pts',(-4.85346670126002,15.2,9.66267350196005));
#239099=CARTESIAN_POINT('Ctrl Pts',(-4.85593990168022,15.2,9.66525772003833));
#239100=CARTESIAN_POINT('Ctrl Pts',(-4.85842828586079,15.2,9.66784905781328));
#239101=CARTESIAN_POINT('Ctrl Pts',(-4.86093183759901,15.2,9.67044736810013));
#239102=CARTESIAN_POINT('Ctrl Pts',(-4.86343538967833,15.2,9.67304567874101));
#239103=CARTESIAN_POINT('Ctrl Pts',(-4.86595411115633,15.2,9.67565096279927));
#239104=CARTESIAN_POINT('Ctrl Pts',(-4.86848798451667,15.2,9.67826307277497));
#239105=CARTESIAN_POINT('Ctrl Pts',(-4.871021857877,15.2,9.68087518275067));
#239106=CARTESIAN_POINT('Ctrl Pts',(-4.87357088501963,15.2,9.68349411850492));
#239107=CARTESIAN_POINT('Ctrl Pts',(-4.87613504966092,15.2,9.68611973770425));
#239108=CARTESIAN_POINT('Ctrl Pts',(-4.87934025493847,15.2,9.6894017611668));
#239109=CARTESIAN_POINT('Ctrl Pts',(-4.88256911357549,15.2,9.69269422372325));
#239110=CARTESIAN_POINT('Ctrl Pts',(-4.88582159460791,15.2,9.69599684808464));
#239111=CARTESIAN_POINT('Ctrl Pts',(-4.88907407599485,15.2,9.69929947280602));
#239112=CARTESIAN_POINT('Ctrl Pts',(-4.89235017880925,15.2,9.70261225813285));
#239113=CARTESIAN_POINT('Ctrl Pts',(-4.89564987283507,15.2,9.70593492959035));
#239114=CARTESIAN_POINT('Ctrl Pts',(-4.89828962819959,15.2,9.70859306690122));
#239115=CARTESIAN_POINT('Ctrl Pts',(-4.90094448255246,15.2,9.71125752991908));
#239116=CARTESIAN_POINT('Ctrl Pts',(-4.90361441854349,15.2,9.71392818124345));
#239117=CARTESIAN_POINT('Ctrl Pts',(-4.90628435417074,15.2,9.71659883220395));
#239118=CARTESIAN_POINT('Ctrl Pts',(-4.90896937153359,15.2,9.71927567117847));
#239119=CARTESIAN_POINT('Ctrl Pts',(-4.91166945503354,15.2,9.72195855756964));
#239120=CARTESIAN_POINT('Ctrl Pts',(-4.91436953890137,15.2,9.72464144432635));
#239121=CARTESIAN_POINT('Ctrl Pts',(-4.91708468775954,15.2,9.72733038059476));
#239122=CARTESIAN_POINT('Ctrl Pts',(-4.91981488574166,15.2,9.73002522924162));
#239123=CARTESIAN_POINT('Ctrl Pts',(-4.92254508372378,15.2,9.73272007788849));
#239124=CARTESIAN_POINT('Ctrl Pts',(-4.92529033043266,15.2,9.73542083757215));
#239125=CARTESIAN_POINT('Ctrl Pts',(-4.92805060791798,15.2,9.73812737494249));
#239126=CARTESIAN_POINT('Ctrl Pts',(-4.93150095421049,15.2,9.74151054610225));
#239127=CARTESIAN_POINT('Ctrl Pts',(-4.9349747893646,15.2,9.74490274330435));
#239128=CARTESIAN_POINT('Ctrl Pts',(-4.93847207780089,15.2,9.74830370453012));
#239129=CARTESIAN_POINT('Ctrl Pts',(-4.94126990900737,15.2,9.75102447395558));
#239130=CARTESIAN_POINT('Ctrl Pts',(-4.9440827488653,15.2,9.75375085150939));
#239131=CARTESIAN_POINT('Ctrl Pts',(-4.94691058274166,15.2,9.75648270749163));
#239132=CARTESIAN_POINT('Ctrl Pts',(-4.95044537489446,15.2,9.75989752728333));
#239133=CARTESIAN_POINT('Ctrl Pts',(-4.95400359138006,15.2,9.76332090234733));
#239134=CARTESIAN_POINT('Ctrl Pts',(-4.95758520028529,15.2,9.7667525797935));
#239135=CARTESIAN_POINT('Ctrl Pts',(-4.96045048717524,15.2,9.76949792152602));
#239136=CARTESIAN_POINT('Ctrl Pts',(-4.96333074418707,15.2,9.77224857637798));
#239137=CARTESIAN_POINT('Ctrl Pts',(-4.96622595305998,15.2,9.77500441354105));
#239138=CARTESIAN_POINT('Ctrl Pts',(-4.96912116232735,15.2,9.77776025107961));
#239139=CARTESIAN_POINT('Ctrl Pts',(-4.97203132389892,15.2,9.78052127271589));
#239140=CARTESIAN_POINT('Ctrl Pts',(-4.97495641922499,15.2,9.78328734819996));
#239141=CARTESIAN_POINT('Ctrl Pts',(-4.97788151455105,15.2,9.78605342368403));
#239142=CARTESIAN_POINT('Ctrl Pts',(-4.98082154396223,15.2,9.78882455369373));
#239143=CARTESIAN_POINT('Ctrl Pts',(-4.98377648795814,15.2,9.79160061067886));
#239144=CARTESIAN_POINT('Ctrl Pts',(-4.98673143155143,15.2,9.79437666728574));
#239145=CARTESIAN_POINT('Ctrl Pts',(-4.98970129161222,15.2,9.79715765280033));
#239146=CARTESIAN_POINT('Ctrl Pts',(-4.99268604725613,15.2,9.79994343857227));
#239147=CARTESIAN_POINT('Ctrl Pts',(-4.99567080330671,15.2,9.80272922472378));
#239148=CARTESIAN_POINT('Ctrl Pts',(-4.99867045681854,15.2,9.80551981199932));
#239149=CARTESIAN_POINT('Ctrl Pts',(-5.00168498641251,15.2,9.80831507568061));
#239150=CARTESIAN_POINT('Ctrl Pts',(-5.00469951559576,15.2,9.81111033898105));
#239151=CARTESIAN_POINT('Ctrl Pts',(-5.0077289243289,15.2,9.81391027793642));
#239152=CARTESIAN_POINT('Ctrl Pts',(-5.01077318930126,15.2,9.81671476976241));
#239153=CARTESIAN_POINT('Ctrl Pts',(-5.01457852082781,15.2,9.82022038483147));
#239154=CARTESIAN_POINT('Ctrl Pts',(-5.01840706932721,15.2,9.82373311438685));
#239155=CARTESIAN_POINT('Ctrl Pts',(-5.0222587957149,15.2,9.8272527162615));
#239156=CARTESIAN_POINT('Ctrl Pts',(-5.025340176993,15.2,9.83006839791467));
#239157=CARTESIAN_POINT('Ctrl Pts',(-5.02843639195027,15.2,9.83288847990333));
#239158=CARTESIAN_POINT('Ctrl Pts',(-5.03154742144318,15.2,9.83571283964316));
#239159=CARTESIAN_POINT('Ctrl Pts',(-5.03465845051223,15.2,9.83853719899818));
#239160=CARTESIAN_POINT('Ctrl Pts',(-5.03778429444,15.2,9.84136583653362));
#239161=CARTESIAN_POINT('Ctrl Pts',(-5.04092493196006,15.2,9.84419863230176));
#239162=CARTESIAN_POINT('Ctrl Pts',(-5.04406556990802,15.2,9.84703142845587));
#239163=CARTESIAN_POINT('Ctrl Pts',(-5.04722100165779,15.2,9.84986838148272));
#239164=CARTESIAN_POINT('Ctrl Pts',(-5.05039120827597,15.2,9.85270937374893));
#239165=CARTESIAN_POINT('Ctrl Pts',(-5.05356141446222,15.2,9.85555036562805));
#239166=CARTESIAN_POINT('Ctrl Pts',(-5.0567463944388,15.2,9.85839539608307));
#239167=CARTESIAN_POINT('Ctrl Pts',(-5.05994612933577,15.2,9.86124434810325));
#239168=CARTESIAN_POINT('Ctrl Pts',(-5.06314586466869,15.2,9.86409330051159));
#239169=CARTESIAN_POINT('Ctrl Pts',(-5.0663603525594,15.2,9.86694617314427));
#239170=CARTESIAN_POINT('Ctrl Pts',(-5.06958957451412,15.2,9.86980284996687));
#239171=CARTESIAN_POINT('Ctrl Pts',(-5.07281879602887,15.2,9.87265952640025));
#239172=CARTESIAN_POINT('Ctrl Pts',(-5.07606275176289,15.2,9.87552000617176));
#239173=CARTESIAN_POINT('Ctrl Pts',(-5.07932141871721,15.2,9.87838417404834));
#239174=CARTESIAN_POINT('Ctrl Pts',(-5.08258008611553,15.2,9.88124834231517));
#239175=CARTESIAN_POINT('Ctrl Pts',(-5.08585346667749,15.2,9.88411619782126));
#239176=CARTESIAN_POINT('Ctrl Pts',(-5.08914153926058,15.2,9.8869876267686));
#239177=CARTESIAN_POINT('Ctrl Pts',(-5.09325162976544,15.2,9.89057691275715));
#239178=CARTESIAN_POINT('Ctrl Pts',(-5.09738467648186,15.2,9.89417177972964));
#239179=CARTESIAN_POINT('Ctrl Pts',(-5.1015406370386,15.2,9.89777200820212));
#239180=CARTESIAN_POINT('Ctrl Pts',(-5.1048654052122,15.2,9.90065219074466));
#239181=CARTESIAN_POINT('Ctrl Pts',(-5.10820483833011,15.2,9.90353580377543));
#239182=CARTESIAN_POINT('Ctrl Pts',(-5.11155891644328,15.2,9.90642273376129));
#239183=CARTESIAN_POINT('Ctrl Pts',(-5.11575151442747,15.2,9.91003139653861));
#239184=CARTESIAN_POINT('Ctrl Pts',(-5.1199669927257,15.2,9.91364524398836));
#239185=CARTESIAN_POINT('Ctrl Pts',(-5.12420531099141,15.2,9.91726405757157));
#239186=CARTESIAN_POINT('Ctrl Pts',(-5.12844362925711,15.2,9.92088287115478));
#239187=CARTESIAN_POINT('Ctrl Pts',(-5.13270478658228,15.2,9.92450664837962));
#239188=CARTESIAN_POINT('Ctrl Pts',(-5.13698874046996,15.2,9.92813517754603));
#239189=CARTESIAN_POINT('Ctrl Pts',(-5.1404159037669,15.2,9.93103800103736));
#239190=CARTESIAN_POINT('Ctrl Pts',(-5.1438576560605,15.2,9.93394386255447));
#239191=CARTESIAN_POINT('Ctrl Pts',(-5.14731397724949,15.2,9.93685265621291));
#239192=CARTESIAN_POINT('Ctrl Pts',(-5.14990621790577,15.2,9.93903425125858));
#239193=CARTESIAN_POINT('Ctrl Pts',(-5.15250665283528,15.2,9.94121749463809));
#239194=CARTESIAN_POINT('Ctrl Pts',(-5.1551152725857,15.2,9.94340234023529));
#239195=CARTESIAN_POINT('Ctrl Pts',(-5.15859343209497,15.2,9.94631546756593));
#239196=CARTESIAN_POINT('Ctrl Pts',(-5.16208614350369,15.2,9.94923144470889));
#239197=CARTESIAN_POINT('Ctrl Pts',(-5.1655933836599,15.2,9.95215016208109));
#239198=CARTESIAN_POINT('Ctrl Pts',(-5.16822381437438,15.2,9.95433920060733));
#239199=CARTESIAN_POINT('Ctrl Pts',(-5.17086241754123,15.2,9.95652978147573));
#239200=CARTESIAN_POINT('Ctrl Pts',(-5.17350918330201,15.2,9.95872185896119));
#239201=CARTESIAN_POINT('Ctrl Pts',(-5.17615594858197,15.2,9.96091393604842));
#239202=CARTESIAN_POINT('Ctrl Pts',(-5.17881087761979,15.2,9.96310750943556));
#239203=CARTESIAN_POINT('Ctrl Pts',(-5.18147396027375,15.2,9.9653025350226));
#239204=CARTESIAN_POINT('Ctrl Pts',(-5.18413704292771,15.2,9.96749756060964));
#239205=CARTESIAN_POINT('Ctrl Pts',(-5.18680827830424,15.2,9.96969403832184));
#239206=CARTESIAN_POINT('Ctrl Pts',(-5.18948765805245,15.2,9.97189192250198));
#239207=CARTESIAN_POINT('Ctrl Pts',(-5.19216703780065,15.2,9.97408980668212));
#239208=CARTESIAN_POINT('Ctrl Pts',(-5.1948545619333,15.2,9.97628909860128));
#239209=CARTESIAN_POINT('Ctrl Pts',(-5.19755022018089,15.2,9.97848975323964));
#239210=CARTESIAN_POINT('Ctrl Pts',(-5.20204298409011,15.2,9.98215751110351));
#239211=CARTESIAN_POINT('Ctrl Pts',(-5.20655834381664,15.2,9.98582905468885));
#239212=CARTESIAN_POINT('Ctrl Pts',(-5.211096252775,15.2,9.98950417996664));
#239213=CARTESIAN_POINT('Ctrl Pts',(-5.21381899805108,15.2,9.99170925505321));
#239214=CARTESIAN_POINT('Ctrl Pts',(-5.21654986176848,15.2,9.99391561852303));
#239215=CARTESIAN_POINT('Ctrl Pts',(-5.21928883395992,15.2,9.9961232290677));
#239216=CARTESIAN_POINT('Ctrl Pts',(-5.22385378777816,15.2,9.99980258010917));
#239217=CARTESIAN_POINT('Ctrl Pts',(-5.22844126430996,15.2,10.0034853915535));
#239218=CARTESIAN_POINT('Ctrl Pts',(-5.23305121974749,15.2,10.0071714635146));
#239219=CARTESIAN_POINT('Ctrl Pts',(-5.23581719290951,15.2,10.009383106611));
#239220=CARTESIAN_POINT('Ctrl Pts',(-5.23859125816533,15.2,10.0115959230892));
#239221=CARTESIAN_POINT('Ctrl Pts',(-5.24137340448022,15.2,10.0138098702587));
#239222=CARTESIAN_POINT('Ctrl Pts',(-5.24415555079511,15.2,10.0160238174281));
#239223=CARTESIAN_POINT('Ctrl Pts',(-5.24694578005942,15.2,10.0182388963809));
#239224=CARTESIAN_POINT('Ctrl Pts',(-5.24974408087331,15.2,10.0204550625502));
#239225=CARTESIAN_POINT('Ctrl Pts',(-5.25254238219556,15.2,10.0226712291221));
#239226=CARTESIAN_POINT('Ctrl Pts',(-5.25534875605342,15.2,10.0248884837444));
#239227=CARTESIAN_POINT('Ctrl Pts',(-5.25816319179689,15.2,10.0271067847336));
#239228=CARTESIAN_POINT('Ctrl Pts',(-5.26285391735428,15.2,10.0308039525116));
#239229=CARTESIAN_POINT('Ctrl Pts',(-5.26756703761759,15.2,10.0345040229674));
#239230=CARTESIAN_POINT('Ctrl Pts',(-5.27230250636941,15.2,10.0382068042176));
#239231=CARTESIAN_POINT('Ctrl Pts',(-5.27514378751726,15.2,10.040428472887));
#239232=CARTESIAN_POINT('Ctrl Pts',(-5.27799311282972,15.2,10.0426511173498));
#239233=CARTESIAN_POINT('Ctrl Pts',(-5.28085047457791,15.2,10.0448746951719));
#239234=CARTESIAN_POINT('Ctrl Pts',(-5.2837078363261,15.2,10.0470982729939));
#239235=CARTESIAN_POINT('Ctrl Pts',(-5.28657323216704,15.2,10.0493227853067));
#239236=CARTESIAN_POINT('Ctrl Pts',(-5.28944665381334,15.2,10.0515481889759));
#239237=CARTESIAN_POINT('Ctrl Pts',(-5.29232007545964,15.2,10.0537735926451));
#239238=CARTESIAN_POINT('Ctrl Pts',(-5.29520152157165,15.2,10.0559998878642));
#239239=CARTESIAN_POINT('Ctrl Pts',(-5.29809098275833,15.2,10.0582270349916));
#239240=CARTESIAN_POINT('Ctrl Pts',(-5.30098044394502,15.2,10.0604541821191));
#239241=CARTESIAN_POINT('Ctrl Pts',(-5.30387791968971,15.2,10.0626821805881));
#239242=CARTESIAN_POINT('Ctrl Pts',(-5.30678339991677,15.2,10.0649109887571));
#239243=CARTESIAN_POINT('Ctrl Pts',(-5.30968888014384,15.2,10.067139796926));
#239244=CARTESIAN_POINT('Ctrl Pts',(-5.31260236536263,15.2,10.0693694150215));
#239245=CARTESIAN_POINT('Ctrl Pts',(-5.31552384469318,15.2,10.0715998018018));
#239246=CARTESIAN_POINT('Ctrl Pts',(-5.31844532402372,15.2,10.0738301885821));
#239247=CARTESIAN_POINT('Ctrl Pts',(-5.32137479686746,15.2,10.0760613441946));
#239248=CARTESIAN_POINT('Ctrl Pts',(-5.32431225309297,15.2,10.0782932287801));
#239249=CARTESIAN_POINT('Ctrl Pts',(-5.32724970985212,15.2,10.080525113771));
#239250=CARTESIAN_POINT('Ctrl Pts',(-5.33019515076354,15.2,10.0827577261622));
#239251=CARTESIAN_POINT('Ctrl Pts',(-5.33314856540219,15.2,10.0849910272368));
#239252=CARTESIAN_POINT('Ctrl Pts',(-5.33610197950431,15.2,10.0872243279058));
#239253=CARTESIAN_POINT('Ctrl Pts',(-5.33906336546433,15.2,10.0894583174414));
#239254=CARTESIAN_POINT('Ctrl Pts',(-5.34203271556546,15.2,10.0916929560269));
#239255=CARTESIAN_POINT('Ctrl Pts',(-5.34500206566659,15.2,10.0939275946124));
#239256=CARTESIAN_POINT('Ctrl Pts',(-5.34797937788091,15.2,10.0961628806231));
#239257=CARTESIAN_POINT('Ctrl Pts',(-5.35096464349439,15.2,10.0983987752604));
#239258=CARTESIAN_POINT('Ctrl Pts',(-5.35394990910786,15.2,10.1006346698976));
#239259=CARTESIAN_POINT('Ctrl Pts',(-5.35694312649271,15.2,10.1028711720024));
#239260=CARTESIAN_POINT('Ctrl Pts',(-5.35994428473061,15.2,10.1051082407229));
#239261=CARTESIAN_POINT('Ctrl Pts',(-5.36294544296851,15.2,10.1073453094435));
#239262=CARTESIAN_POINT('Ctrl Pts',(-5.36595454318158,15.2,10.1095829447707));
#239263=CARTESIAN_POINT('Ctrl Pts',(-5.36897157444628,15.2,10.111821111481));
#239264=CARTESIAN_POINT('Ctrl Pts',(-5.37198860571097,15.2,10.1140592781913));
#239265=CARTESIAN_POINT('Ctrl Pts',(-5.37501356911677,15.2,10.1162979761266));
#239266=CARTESIAN_POINT('Ctrl Pts',(-5.37804645379717,15.2,10.1185371677535));
#239267=CARTESIAN_POINT('Ctrl Pts',(-5.38107933902854,15.2,10.1207763597872));
#239268=CARTESIAN_POINT('Ctrl Pts',(-5.38412014552048,15.2,10.1230160458294));
#239269=CARTESIAN_POINT('Ctrl Pts',(-5.38716886067296,15.2,10.1252561777383));
#239270=CARTESIAN_POINT('Ctrl Pts',(-5.39123381328652,15.2,10.1282430196053));
#239271=CARTESIAN_POINT('Ctrl Pts',(-5.39531282323273,15.2,10.1312306500592));
#239272=CARTESIAN_POINT('Ctrl Pts',(-5.39940586797222,15.2,10.1342189767729));
#239273=CARTESIAN_POINT('Ctrl Pts',(-5.40452217431482,15.2,10.1379543854705));
#239274=CARTESIAN_POINT('Ctrl Pts',(-5.40966040287515,15.2,10.1416908878519));
#239275=CARTESIAN_POINT('Ctrl Pts',(-5.41482055400006,15.2,10.145428447));
#239276=CARTESIAN_POINT('Ctrl Pts',(-4.57383771200006,12.2,9.31239140099999));
#239277=CARTESIAN_POINT('Ctrl Pts',(-4.57476026596749,12.2,9.31392144227075));
#239278=CARTESIAN_POINT('Ctrl Pts',(-4.57571693063136,12.2,9.31549767344762));
#239279=CARTESIAN_POINT('Ctrl Pts',(-4.57670776761648,12.2,9.31711891458901));
#239280=CARTESIAN_POINT('Ctrl Pts',(-4.57770338291839,12.2,9.3187479741747));
#239281=CARTESIAN_POINT('Ctrl Pts',(-4.57873349932321,12.2,9.32042248440087));
#239282=CARTESIAN_POINT('Ctrl Pts',(-4.57979816360307,12.2,9.32214130041629));
#239283=CARTESIAN_POINT('Ctrl Pts',(-4.58086282778624,12.2,9.32386011627559));
#239284=CARTESIAN_POINT('Ctrl Pts',(-4.58196204052454,12.2,9.3256232394989));
#239285=CARTESIAN_POINT('Ctrl Pts',(-4.58309584848333,12.2,9.32742955643324));
#239286=CARTESIAN_POINT('Ctrl Pts',(-4.58422965644212,12.2,9.32923587336759));
#239287=CARTESIAN_POINT('Ctrl Pts',(-4.58539805581098,12.2,9.33108538570202));
#239288=CARTESIAN_POINT('Ctrl Pts',(-4.5866010919087,12.2,9.33297701280868));
#239289=CARTESIAN_POINT('Ctrl Pts',(-4.58780412811569,12.2,9.33486864008716));
#239290=CARTESIAN_POINT('Ctrl Pts',(-4.58904179835032,12.2,9.3368023811214));
#239291=CARTESIAN_POINT('Ctrl Pts',(-4.59031413942202,12.2,9.33877718823185));
#239292=CARTESIAN_POINT('Ctrl Pts',(-4.59158648037816,12.2,9.3407519951629));
#239293=CARTESIAN_POINT('Ctrl Pts',(-4.59289349278484,12.2,9.34276786523277));
#239294=CARTESIAN_POINT('Ctrl Pts',(-4.59423520699227,12.2,9.34482377850085));
#239295=CARTESIAN_POINT('Ctrl Pts',(-4.59557692119971,12.2,9.34687969176892));
#239296=CARTESIAN_POINT('Ctrl Pts',(-4.59695334020937,12.2,9.34897564855469));
#239297=CARTESIAN_POINT('Ctrl Pts',(-4.59836449115657,12.2,9.35111065189206));
#239298=CARTESIAN_POINT('Ctrl Pts',(-4.59977564223195,12.2,9.35324565542336));
#239299=CARTESIAN_POINT('Ctrl Pts',(-4.60122152508665,12.2,9.35541970736789));
#239300=CARTESIAN_POINT('Ctrl Pts',(-4.60270216441973,12.2,9.35763183999105));
#239301=CARTESIAN_POINT('Ctrl Pts',(-4.60442957677324,12.2,9.36021266108334));
#239302=CARTESIAN_POINT('Ctrl Pts',(-4.60620429860251,12.2,9.36284530880486));
#239303=CARTESIAN_POINT('Ctrl Pts',(-4.60802636339002,12.2,9.36552829264974));
#239304=CARTESIAN_POINT('Ctrl Pts',(-4.60958813339028,12.2,9.36782799335679));
#239305=CARTESIAN_POINT('Ctrl Pts',(-4.61118468385317,12.2,9.3701646730684));
#239306=CARTESIAN_POINT('Ctrl Pts',(-4.61281603494449,12.2,9.37253741878356));
#239307=CARTESIAN_POINT('Ctrl Pts',(-4.61444738588763,12.2,9.37491016428319));
#239308=CARTESIAN_POINT('Ctrl Pts',(-4.61611353471978,12.2,9.37731897119552));
#239309=CARTESIAN_POINT('Ctrl Pts',(-4.61781449782618,12.2,9.37976295185827));
#239310=CARTESIAN_POINT('Ctrl Pts',(-4.61951546093257,12.2,9.38220693252101));
#239311=CARTESIAN_POINT('Ctrl Pts',(-4.62125123994448,12.2,9.38468608118922));
#239312=CARTESIAN_POINT('Ctrl Pts',(-4.62302184112864,12.2,9.38719953009641));
#239313=CARTESIAN_POINT('Ctrl Pts',(-4.6247924423128,12.2,9.38971297900361));
#239314=CARTESIAN_POINT('Ctrl Pts',(-4.62659787004367,12.2,9.39226072433133));
#239315=CARTESIAN_POINT('Ctrl Pts',(-4.62843812905775,12.2,9.39484191823525));
#239316=CARTESIAN_POINT('Ctrl Pts',(-4.63027838823899,12.2,9.39742311237363));
#239317=CARTESIAN_POINT('Ctrl Pts',(-4.63215348059029,12.2,9.40003775161533));
#239318=CARTESIAN_POINT('Ctrl Pts',(-4.63406341061257,12.2,9.40268500692767));
#239319=CARTESIAN_POINT('Ctrl Pts',(-4.63597334046135,12.2,9.40533226199957));
#239320=CARTESIAN_POINT('Ctrl Pts',(-4.63791810764904,12.2,9.40801213166054));
#239321=CARTESIAN_POINT('Ctrl Pts',(-4.63989771540892,12.2,9.41072380464395));
#239322=CARTESIAN_POINT('Ctrl Pts',(-4.6418773231688,12.2,9.41343547762736));
#239323=CARTESIAN_POINT('Ctrl Pts',(-4.64389176980347,12.2,9.41617895134211));
#239324=CARTESIAN_POINT('Ctrl Pts',(-4.64594105572663,12.2,9.41895343448918));
#239325=CARTESIAN_POINT('Ctrl Pts',(-4.64799034183593,12.2,9.42172791788825));
#239326=CARTESIAN_POINT('Ctrl Pts',(-4.65007446833195,12.2,9.4245334084654));
#239327=CARTESIAN_POINT('Ctrl Pts',(-4.65219342861563,12.2,9.42736913112128));
#239328=CARTESIAN_POINT('Ctrl Pts',(-4.65431238870683,12.2,9.43020485351956));
#239329=CARTESIAN_POINT('Ctrl Pts',(-4.65646618639365,12.2,9.43307080644905));
#239330=CARTESIAN_POINT('Ctrl Pts',(-4.65865481324067,12.2,9.43596623177362));
#239331=CARTESIAN_POINT('Ctrl Pts',(-4.6608434400877,12.2,9.4388616570982));
#239332=CARTESIAN_POINT('Ctrl Pts',(-4.66306689591328,12.2,9.44178655333729));
#239333=CARTESIAN_POINT('Ctrl Pts',(-4.66532517374552,12.2,9.44474017689466));
#239334=CARTESIAN_POINT('Ctrl Pts',(-4.66758345178288,12.2,9.44769380072034));
#239335=CARTESIAN_POINT('Ctrl Pts',(-4.66987655041343,12.2,9.45067615305848));
#239336=CARTESIAN_POINT('Ctrl Pts',(-4.67220445949194,12.2,9.45368650504122));
#239337=CARTESIAN_POINT('Ctrl Pts',(-4.67453236835901,12.2,9.45669685675053));
#239338=CARTESIAN_POINT('Ctrl Pts',(-4.67689508776212,12.2,9.45973520739468));
#239339=CARTESIAN_POINT('Ctrl Pts',(-4.67929260275832,12.2,9.46280084678327));
#239340=CARTESIAN_POINT('Ctrl Pts',(-4.68169011775452,12.2,9.46586648617185));
#239341=CARTESIAN_POINT('Ctrl Pts',(-4.68412243088815,12.2,9.46895940989894));
#239342=CARTESIAN_POINT('Ctrl Pts',(-4.68658952400309,12.2,9.4720789246899));
#239343=CARTESIAN_POINT('Ctrl Pts',(-4.68864543500689,12.2,9.47467852044349));
#239344=CARTESIAN_POINT('Ctrl Pts',(-4.69072549924711,12.2,9.47729657986747));
#239345=CARTESIAN_POINT('Ctrl Pts',(-4.69282970737085,12.2,9.47993270806097));
#239346=CARTESIAN_POINT('Ctrl Pts',(-4.6949339154946,12.2,9.48256883625448));
#239347=CARTESIAN_POINT('Ctrl Pts',(-4.6970622661773,12.2,9.48522303222622));
#239348=CARTESIAN_POINT('Ctrl Pts',(-4.6992147478427,12.2,9.48789490555864));
#239349=CARTESIAN_POINT('Ctrl Pts',(-4.70136722950811,12.2,9.49056677889104));
#239350=CARTESIAN_POINT('Ctrl Pts',(-4.70354384382777,12.2,9.49325633019736));
#239351=CARTESIAN_POINT('Ctrl Pts',(-4.70574457703214,12.2,9.49596317597348));
#239352=CARTESIAN_POINT('Ctrl Pts',(-4.70794531023652,12.2,9.49867002174962));
#239353=CARTESIAN_POINT('Ctrl Pts',(-4.71017016228889,12.2,9.50139416217774));
#239354=CARTESIAN_POINT('Ctrl Pts',(-4.71241912048333,12.2,9.50413521877494));
#239355=CARTESIAN_POINT('Ctrl Pts',(-4.71466807867776,12.2,9.50687627537216));
#239356=CARTESIAN_POINT('Ctrl Pts',(-4.71694114226853,12.2,9.50963424797214));
#239357=CARTESIAN_POINT('Ctrl Pts',(-4.71923829783458,12.2,9.51240876631813));
#239358=CARTESIAN_POINT('Ctrl Pts',(-4.7219948844137,12.2,9.51573818821234));
#239359=CARTESIAN_POINT('Ctrl Pts',(-4.72478616143365,12.2,9.51909143503971));
#239360=CARTESIAN_POINT('Ctrl Pts',(-4.72761210332947,12.2,9.5224678750827));
#239361=CARTESIAN_POINT('Ctrl Pts',(-4.72996705499488,12.2,9.52528157522075));
#239362=CARTESIAN_POINT('Ctrl Pts',(-4.7323460798498,12.2,9.52811138336476));
#239363=CARTESIAN_POINT('Ctrl Pts',(-4.73474916054298,12.2,9.53095693857228));
#239364=CARTESIAN_POINT('Ctrl Pts',(-4.73715224123617,12.2,9.53380249377979));
#239365=CARTESIAN_POINT('Ctrl Pts',(-4.73957937754315,12.2,9.53666379824648));
#239366=CARTESIAN_POINT('Ctrl Pts',(-4.74203055324866,12.2,9.53954049673171));
#239367=CARTESIAN_POINT('Ctrl Pts',(-4.7454621992898,12.2,9.54356787467374));
#239368=CARTESIAN_POINT('Ctrl Pts',(-4.74894095910263,12.2,9.54762542499845));
#239369=CARTESIAN_POINT('Ctrl Pts',(-4.75246678546484,12.2,9.55171219792427));
#239370=CARTESIAN_POINT('Ctrl Pts',(-4.7549852328272,12.2,9.55463132139726));
#239371=CARTESIAN_POINT('Ctrl Pts',(-4.75752769061257,12.2,9.55756535308842));
#239372=CARTESIAN_POINT('Ctrl Pts',(-4.76009414379801,12.2,9.56051395358395));
#239373=CARTESIAN_POINT('Ctrl Pts',(-4.76266059698344,12.2,9.56346255407949));
#239374=CARTESIAN_POINT('Ctrl Pts',(-4.7652510413178,12.2,9.56642572413825));
#239375=CARTESIAN_POINT('Ctrl Pts',(-4.7678654593753,12.2,9.5694031253894));
#239376=CARTESIAN_POINT('Ctrl Pts',(-4.77047987743282,12.2,9.57238052664055));
#239377=CARTESIAN_POINT('Ctrl Pts',(-4.7731182668074,12.2,9.57537216075861));
#239378=CARTESIAN_POINT('Ctrl Pts',(-4.77578060757324,12.2,9.57837769763475));
#239379=CARTESIAN_POINT('Ctrl Pts',(-4.77844294833908,12.2,9.58138323451087));
#239380=CARTESIAN_POINT('Ctrl Pts',(-4.7811292404081,12.2,9.58440267245112));
#239381=CARTESIAN_POINT('Ctrl Pts',(-4.7838394611045,12.2,9.58743568689668));
#239382=CARTESIAN_POINT('Ctrl Pts',(-4.78654968150549,12.2,9.59046870101163));
#239383=CARTESIAN_POINT('Ctrl Pts',(-4.78928383057515,12.2,9.59351529082321));
#239384=CARTESIAN_POINT('Ctrl Pts',(-4.79204188589758,12.2,9.59657513430806));
#239385=CARTESIAN_POINT('Ctrl Pts',(-4.79479994152064,12.2,9.59963497812644));
#239386=CARTESIAN_POINT('Ctrl Pts',(-4.79758190235162,12.2,9.60270807775291));
#239387=CARTESIAN_POINT('Ctrl Pts',(-4.80038774484966,12.2,9.6057941140713));
#239388=CARTESIAN_POINT('Ctrl Pts',(-4.80263241897043,12.2,9.60826294326056));
#239389=CARTESIAN_POINT('Ctrl Pts',(-4.80489237982827,12.2,9.6107400537771));
#239390=CARTESIAN_POINT('Ctrl Pts',(-4.80716761051822,12.2,9.61322528303498));
#239391=CARTESIAN_POINT('Ctrl Pts',(-4.80944284089817,12.2,9.61571051195425));
#239392=CARTESIAN_POINT('Ctrl Pts',(-4.81173334270475,12.2,9.61820386151296));
#239393=CARTESIAN_POINT('Ctrl Pts',(-4.81403910434802,12.2,9.62070517230767));
#239394=CARTESIAN_POINT('Ctrl Pts',(-4.81634486630545,12.2,9.62320648344316));
#239395=CARTESIAN_POINT('Ctrl Pts',(-4.81866588735043,12.2,9.6257157563322));
#239396=CARTESIAN_POINT('Ctrl Pts',(-4.82100215469999,12.2,9.62823283352495));
#239397=CARTESIAN_POINT('Ctrl Pts',(-4.82333842204956,12.2,9.63074991071771));
#239398=CARTESIAN_POINT('Ctrl Pts',(-4.82568993509809,12.2,9.63327479296411));
#239399=CARTESIAN_POINT('Ctrl Pts',(-4.8280566803953,12.2,9.6358073248807));
#239400=CARTESIAN_POINT('Ctrl Pts',(-4.83042342537005,12.2,9.63833985645222));
#239401=CARTESIAN_POINT('Ctrl Pts',(-4.83280540244183,12.2,9.64088003873382));
#239402=CARTESIAN_POINT('Ctrl Pts',(-4.8352025987567,12.2,9.64342771698156));
#239403=CARTESIAN_POINT('Ctrl Pts',(-4.8375997953982,12.2,9.64597539557641));
#239404=CARTESIAN_POINT('Ctrl Pts',(-4.84001221130751,12.2,9.64853057063131));
#239405=CARTESIAN_POINT('Ctrl Pts',(-4.84243983066359,12.2,9.6510930911606));
#239406=CARTESIAN_POINT('Ctrl Pts',(-4.84486744968889,12.2,9.65365561134075));
#239407=CARTESIAN_POINT('Ctrl Pts',(-4.84731027312334,12.2,9.65622547540048));
#239408=CARTESIAN_POINT('Ctrl Pts',(-4.84976828803252,12.2,9.65880253485601));
#239409=CARTESIAN_POINT('Ctrl Pts',(-4.85222630327661,12.2,9.66137959466266));
#239410=CARTESIAN_POINT('Ctrl Pts',(-4.85469950740546,12.2,9.66396385021861));
#239411=CARTESIAN_POINT('Ctrl Pts',(-4.85718788811116,12.2,9.66655515110101));
#239412=CARTESIAN_POINT('Ctrl Pts',(-4.85967626847782,12.2,9.66914645163035));
#239413=CARTESIAN_POINT('Ctrl Pts',(-4.86217982392334,12.2,9.67174479865601));
#239414=CARTESIAN_POINT('Ctrl Pts',(-4.86469854082757,12.2,9.67435004555372));
#239415=CARTESIAN_POINT('Ctrl Pts',(-4.86721725807497,12.2,9.67695529280638));
#239416=CARTESIAN_POINT('Ctrl Pts',(-4.86975113472418,12.2,9.67956743921541));
#239417=CARTESIAN_POINT('Ctrl Pts',(-4.87230015797519,12.2,9.68218633924745));
#239418=CARTESIAN_POINT('Ctrl Pts',(-4.87484918087891,12.2,9.68480523892268));
#239419=CARTESIAN_POINT('Ctrl Pts',(-4.87741334870079,12.2,9.68743089394396));
#239420=CARTESIAN_POINT('Ctrl Pts',(-4.87999264711747,12.2,9.6900631583597));
#239421=CARTESIAN_POINT('Ctrl Pts',(-4.88257194588559,12.2,9.69269542313408));
#239422=CARTESIAN_POINT('Ctrl Pts',(-4.88516637549803,12.2,9.69533429833834));
#239423=CARTESIAN_POINT('Ctrl Pts',(-4.8877759181968,12.2,9.69797964048295));
#239424=CARTESIAN_POINT('Ctrl Pts',(-4.89038546054003,12.2,9.70062498226713));
#239425=CARTESIAN_POINT('Ctrl Pts',(-4.89301011783022,12.2,9.70327679264166));
#239426=CARTESIAN_POINT('Ctrl Pts',(-4.89564987283507,12.2,9.70593492959036));
#239427=CARTESIAN_POINT('Ctrl Pts',(-4.8982896281996,12.2,9.70859306690123));
#239428=CARTESIAN_POINT('Ctrl Pts',(-4.90094448255246,12.2,9.71125752991908));
#239429=CARTESIAN_POINT('Ctrl Pts',(-4.90361441854349,12.2,9.71392818124345));
#239430=CARTESIAN_POINT('Ctrl Pts',(-4.90628435417074,12.2,9.71659883220395));
#239431=CARTESIAN_POINT('Ctrl Pts',(-4.90896937153359,12.2,9.71927567117847));
#239432=CARTESIAN_POINT('Ctrl Pts',(-4.91166945503354,12.2,9.72195855756964));
#239433=CARTESIAN_POINT('Ctrl Pts',(-4.91436953890137,12.2,9.72464144432635));
#239434=CARTESIAN_POINT('Ctrl Pts',(-4.91708468775954,12.2,9.72733038059476));
#239435=CARTESIAN_POINT('Ctrl Pts',(-4.91981488574166,12.2,9.73002522924162));
#239436=CARTESIAN_POINT('Ctrl Pts',(-4.92254508372378,12.2,9.73272007788849));
#239437=CARTESIAN_POINT('Ctrl Pts',(-4.92529033043266,12.2,9.73542083757215));
#239438=CARTESIAN_POINT('Ctrl Pts',(-4.92805060791798,12.2,9.73812737494249));
#239439=CARTESIAN_POINT('Ctrl Pts',(-4.93150095421049,12.2,9.74151054610225));
#239440=CARTESIAN_POINT('Ctrl Pts',(-4.9349747893646,12.2,9.74490274330435));
#239441=CARTESIAN_POINT('Ctrl Pts',(-4.93847207780089,12.2,9.74830370453012));
#239442=CARTESIAN_POINT('Ctrl Pts',(-4.94126990900737,12.2,9.75102447395558));
#239443=CARTESIAN_POINT('Ctrl Pts',(-4.9440827488653,12.2,9.75375085150939));
#239444=CARTESIAN_POINT('Ctrl Pts',(-4.94691058274166,12.2,9.75648270749163));
#239445=CARTESIAN_POINT('Ctrl Pts',(-4.94973841661802,12.2,9.75921456347388));
#239446=CARTESIAN_POINT('Ctrl Pts',(-4.9525812420822,12.2,9.76195189447893));
#239447=CARTESIAN_POINT('Ctrl Pts',(-4.95543904268393,12.2,9.76469457190673));
#239448=CARTESIAN_POINT('Ctrl Pts',(-4.95829684289628,12.2,9.76743724896085));
#239449=CARTESIAN_POINT('Ctrl Pts',(-4.96116961884604,12.2,9.77018527197734));
#239450=CARTESIAN_POINT('Ctrl Pts',(-4.96405735045637,12.2,9.77293850976476));
#239451=CARTESIAN_POINT('Ctrl Pts',(-4.96694508246016,12.2,9.7756917479273));
#239452=CARTESIAN_POINT('Ctrl Pts',(-4.96984777142485,12.2,9.77845020178681));
#239453=CARTESIAN_POINT('Ctrl Pts',(-4.97276539875204,12.2,9.78121374199347));
#239454=CARTESIAN_POINT('Ctrl Pts',(-4.97568302568169,12.2,9.78397728182361));
#239455=CARTESIAN_POINT('Ctrl Pts',(-4.97861559135946,12.2,9.78674590821701));
#239456=CARTESIAN_POINT('Ctrl Pts',(-4.98156307628418,12.2,9.78951949332327));
#239457=CARTESIAN_POINT('Ctrl Pts',(-4.98451056161049,12.2,9.79229307880742));
#239458=CARTESIAN_POINT('Ctrl Pts',(-4.98747296679975,12.2,9.79507162412833));
#239459=CARTESIAN_POINT('Ctrl Pts',(-4.99045027401854,12.2,9.79785500166922));
#239460=CARTESIAN_POINT('Ctrl Pts',(-4.99342758083166,12.2,9.80063837883087));
#239461=CARTESIAN_POINT('Ctrl Pts',(-4.99641978861896,12.2,9.80342658877003));
#239462=CARTESIAN_POINT('Ctrl Pts',(-4.9994268783554,12.2,9.80621950606972));
#239463=CARTESIAN_POINT('Ctrl Pts',(-5.00243396850156,12.2,9.80901242374994));
#239464=CARTESIAN_POINT('Ctrl Pts',(-5.00545594083468,12.2,9.81181004931772));
#239465=CARTESIAN_POINT('Ctrl Pts',(-5.0084927767234,12.2,9.81461225697076));
#239466=CARTESIAN_POINT('Ctrl Pts',(-5.01152961219835,12.2,9.817414464242));
#239467=CARTESIAN_POINT('Ctrl Pts',(-5.01458130980638,12.2,9.82022125617337));
#239468=CARTESIAN_POINT('Ctrl Pts',(-5.01764785199863,12.2,9.82303250799866));
#239469=CARTESIAN_POINT('Ctrl Pts',(-5.0214810300523,12.2,9.82654657306755));
#239470=CARTESIAN_POINT('Ctrl Pts',(-5.02533740099083,12.2,9.83006760720912));
#239471=CARTESIAN_POINT('Ctrl Pts',(-5.02921692680806,12.2,9.83359537335714));
#239472=CARTESIAN_POINT('Ctrl Pts',(-5.03232054763099,12.2,9.83641758642936));
#239473=CARTESIAN_POINT('Ctrl Pts',(-5.03543898912901,12.2,9.83924410764632));
#239474=CARTESIAN_POINT('Ctrl Pts',(-5.03857222852295,12.2,9.84207481718975));
#239475=CARTESIAN_POINT('Ctrl Pts',(-5.04170546748999,12.2,9.8449055263475));
#239476=CARTESIAN_POINT('Ctrl Pts',(-5.04485350569852,12.2,9.84774042287108));
#239477=CARTESIAN_POINT('Ctrl Pts',(-5.04801632321622,12.2,9.85057938802747));
#239478=CARTESIAN_POINT('Ctrl Pts',(-5.05117914116484,12.2,9.85341835357065));
#239479=CARTESIAN_POINT('Ctrl Pts',(-5.05435673855256,12.2,9.85626138720605));
#239480=CARTESIAN_POINT('Ctrl Pts',(-5.05754909518551,12.2,9.85910837148525));
#239481=CARTESIAN_POINT('Ctrl Pts',(-5.0607414513835,12.2,9.86195535537653));
#239482=CARTESIAN_POINT('Ctrl Pts',(-5.06394856671036,12.2,9.86480629036144));
#239483=CARTESIAN_POINT('Ctrl Pts',(-5.06717042022323,12.2,9.86766105701654));
#239484=CARTESIAN_POINT('Ctrl Pts',(-5.07039227417506,12.2,9.8705158240606));
#239485=CARTESIAN_POINT('Ctrl Pts',(-5.07362886695891,12.2,9.87337442401065));
#239486=CARTESIAN_POINT('Ctrl Pts',(-5.07688017752499,12.2,9.87623674149997));
#239487=CARTESIAN_POINT('Ctrl Pts',(-5.08013148809106,12.2,9.87909905898929));
#239488=CARTESIAN_POINT('Ctrl Pts',(-5.08339751522832,12.2,9.88196509166517));
#239489=CARTESIAN_POINT('Ctrl Pts',(-5.08667824051974,12.2,9.88483472721083));
#239490=CARTESIAN_POINT('Ctrl Pts',(-5.08995896536416,12.2,9.8877043623655));
#239491=CARTESIAN_POINT('Ctrl Pts',(-5.09325438740614,12.2,9.89057759854236));
#239492=CARTESIAN_POINT('Ctrl Pts',(-5.09656448553942,12.2,9.89345432176468));
#239493=CARTESIAN_POINT('Ctrl Pts',(-5.09987458412369,12.2,9.89633104537896));
#239494=CARTESIAN_POINT('Ctrl Pts',(-5.10319935768475,12.2,9.89921125672229));
#239495=CARTESIAN_POINT('Ctrl Pts',(-5.10653878631267,12.2,9.90209484171311));
#239496=CARTESIAN_POINT('Ctrl Pts',(-5.1098782144856,12.2,9.90497842631103));
#239497=CARTESIAN_POINT('Ctrl Pts',(-5.11323229825945,12.2,9.90786538397246));
#239498=CARTESIAN_POINT('Ctrl Pts',(-5.11660101448308,12.2,9.91075560451373));
#239499=CARTESIAN_POINT('Ctrl Pts',(-5.11912755176556,12.2,9.91292327001814));
#239500=CARTESIAN_POINT('Ctrl Pts',(-5.12166232012438,12.2,9.91509276950053));
#239501=CARTESIAN_POINT('Ctrl Pts',(-5.12420531099141,12.2,9.91726405757157));
#239502=CARTESIAN_POINT('Ctrl Pts',(-5.12674830185844,12.2,9.91943534564261));
#239503=CARTESIAN_POINT('Ctrl Pts',(-5.12929951468617,12.2,9.92160842102179));
#239504=CARTESIAN_POINT('Ctrl Pts',(-5.13185894042538,12.2,9.9237832371092));
#239505=CARTESIAN_POINT('Ctrl Pts',(-5.13527150838763,12.2,9.92668299215579));
#239506=CARTESIAN_POINT('Ctrl Pts',(-5.13869867745111,12.2,9.92958584293589));
#239507=CARTESIAN_POINT('Ctrl Pts',(-5.14214042475012,12.2,9.93249167798341));
#239508=CARTESIAN_POINT('Ctrl Pts',(-5.14472173498992,12.2,9.9346710540711));
#239509=CARTESIAN_POINT('Ctrl Pts',(-5.14731124624545,12.2,9.93685210977489));
#239510=CARTESIAN_POINT('Ctrl Pts',(-5.14990894852532,12.2,9.93903479877876));
#239511=CARTESIAN_POINT('Ctrl Pts',(-5.1525066508052,12.2,9.94121748778262));
#239512=CARTESIAN_POINT('Ctrl Pts',(-5.15511254422633,12.2,9.94340180893082));
#239513=CARTESIAN_POINT('Ctrl Pts',(-5.15772661967765,12.2,9.9455877180854));
#239514=CARTESIAN_POINT('Ctrl Pts',(-5.16034069512897,12.2,9.94777362723999));
#239515=CARTESIAN_POINT('Ctrl Pts',(-5.16296295342327,12.2,9.94996112395252));
#239516=CARTESIAN_POINT('Ctrl Pts',(-5.1655933836599,12.2,9.95215016208109));
#239517=CARTESIAN_POINT('Ctrl Pts',(-5.16822381437438,12.2,9.95433920060733));
#239518=CARTESIAN_POINT('Ctrl Pts',(-5.17086241754122,12.2,9.95652978147573));
#239519=CARTESIAN_POINT('Ctrl Pts',(-5.17350918330201,12.2,9.95872185896119));
#239520=CARTESIAN_POINT('Ctrl Pts',(-5.17615594858197,12.2,9.96091393604842));
#239521=CARTESIAN_POINT('Ctrl Pts',(-5.17881087761979,12.2,9.96310750943556));
#239522=CARTESIAN_POINT('Ctrl Pts',(-5.18147396027375,12.2,9.9653025350226));
#239523=CARTESIAN_POINT('Ctrl Pts',(-5.18413704292771,12.2,9.96749756060964));
#239524=CARTESIAN_POINT('Ctrl Pts',(-5.18680827830424,12.2,9.96969403832184));
#239525=CARTESIAN_POINT('Ctrl Pts',(-5.18948765805245,12.2,9.97189192250198));
#239526=CARTESIAN_POINT('Ctrl Pts',(-5.19216703780065,12.2,9.97408980668212));
#239527=CARTESIAN_POINT('Ctrl Pts',(-5.19485456193329,12.2,9.97628909860128));
#239528=CARTESIAN_POINT('Ctrl Pts',(-5.19755022018089,12.2,9.97848975323964));
#239529=CARTESIAN_POINT('Ctrl Pts',(-5.20024587842848,12.2,9.98069040787801));
#239530=CARTESIAN_POINT('Ctrl Pts',(-5.20294967075378,12.2,9.98289242505667));
#239531=CARTESIAN_POINT('Ctrl Pts',(-5.20566158794621,12.2,9.98509576118484));
#239532=CARTESIAN_POINT('Ctrl Pts',(-5.20837350513864,12.2,9.987299097313));
#239533=CARTESIAN_POINT('Ctrl Pts',(-5.21109354685551,12.2,9.98950375336609));
#239534=CARTESIAN_POINT('Ctrl Pts',(-5.21382170313026,12.2,9.99170968257742));
#239535=CARTESIAN_POINT('Ctrl Pts',(-5.21654985990064,12.2,9.99391561218949));
#239536=CARTESIAN_POINT('Ctrl Pts',(-5.21928613254833,12.2,9.99612281737696));
#239537=CARTESIAN_POINT('Ctrl Pts',(-5.22203050936495,12.2,9.99833125394809));
#239538=CARTESIAN_POINT('Ctrl Pts',(-5.22568967762284,12.2,10.0012758353743));
#239539=CARTESIAN_POINT('Ctrl Pts',(-5.22936325569896,12.2,10.0042226061868));
#239540=CARTESIAN_POINT('Ctrl Pts',(-5.23305121974749,12.2,10.0071714635146));
#239541=CARTESIAN_POINT('Ctrl Pts',(-5.23581719290951,12.2,10.009383106611));
#239542=CARTESIAN_POINT('Ctrl Pts',(-5.23859125816533,12.2,10.0115959230892));
#239543=CARTESIAN_POINT('Ctrl Pts',(-5.24137340448021,12.2,10.0138098702587));
#239544=CARTESIAN_POINT('Ctrl Pts',(-5.24415555079511,12.2,10.0160238174281));
#239545=CARTESIAN_POINT('Ctrl Pts',(-5.24694578005942,12.2,10.0182388963809));
#239546=CARTESIAN_POINT('Ctrl Pts',(-5.24974408087331,12.2,10.0204550625502));
#239547=CARTESIAN_POINT('Ctrl Pts',(-5.25254238219556,12.2,10.0226712291221));
#239548=CARTESIAN_POINT('Ctrl Pts',(-5.25534875605342,12.2,10.0248884837444));
#239549=CARTESIAN_POINT('Ctrl Pts',(-5.25816319179689,12.2,10.0271067847336));
#239550=CARTESIAN_POINT('Ctrl Pts',(-5.26097762702906,12.2,10.0293250853198));
#239551=CARTESIAN_POINT('Ctrl Pts',(-5.26380012431079,12.2,10.0315444305893));
#239552=CARTESIAN_POINT('Ctrl Pts',(-5.266630673542,12.2,10.033764779717));
#239553=CARTESIAN_POINT('Ctrl Pts',(-5.26946122277321,12.2,10.0359851288448));
#239554=CARTESIAN_POINT('Ctrl Pts',(-5.27229982520972,12.2,10.038206481656));
#239555=CARTESIAN_POINT('Ctrl Pts',(-5.27514646803592,12.2,10.040428796252));
#239556=CARTESIAN_POINT('Ctrl Pts',(-5.27894199163181,12.2,10.0433918822454));
#239557=CARTESIAN_POINT('Ctrl Pts',(-5.28275181314442,12.2,10.0463566772549));
#239558=CARTESIAN_POINT('Ctrl Pts',(-5.28657590660809,12.2,10.04932308329));
#239559=CARTESIAN_POINT('Ctrl Pts',(-5.28944397735713,12.2,10.0515478883215));
#239560=CARTESIAN_POINT('Ctrl Pts',(-5.29232007685848,12.2,10.0537735986116));
#239561=CARTESIAN_POINT('Ctrl Pts',(-5.29520419411207,12.2,10.056000173727));
#239562=CARTESIAN_POINT('Ctrl Pts',(-5.29808831084171,12.2,10.0582267484379));
#239563=CARTESIAN_POINT('Ctrl Pts',(-5.30098044610427,12.2,10.0604541888238));
#239564=CARTESIAN_POINT('Ctrl Pts',(-5.30388058883292,12.2,10.0626824524929));
#239565=CARTESIAN_POINT('Ctrl Pts',(-5.30678073156158,12.2,10.064910716162));
#239566=CARTESIAN_POINT('Ctrl Pts',(-5.30968888229533,12.2,10.0671398035896));
#239567=CARTESIAN_POINT('Ctrl Pts',(-5.31260503099433,12.2,10.0693696732687));
#239568=CARTESIAN_POINT('Ctrl Pts',(-5.31552117969334,12.2,10.0715995429478));
#239569=CARTESIAN_POINT('Ctrl Pts',(-5.31844532627391,12.2,10.0738301947855));
#239570=CARTESIAN_POINT('Ctrl Pts',(-5.32137745901401,12.2,10.0760615889646));
#239571=CARTESIAN_POINT('Ctrl Pts',(-5.32430959175411,12.2,10.0782929831437));
#239572=CARTESIAN_POINT('Ctrl Pts',(-5.32724971121994,12.2,10.0805251195378));
#239573=CARTESIAN_POINT('Ctrl Pts',(-5.33019780840379,12.2,10.0827579567483));
#239574=CARTESIAN_POINT('Ctrl Pts',(-5.33314590558764,12.2,10.0849907939588));
#239575=CARTESIAN_POINT('Ctrl Pts',(-5.33610197956263,12.2,10.0872243325942));
#239576=CARTESIAN_POINT('Ctrl Pts',(-5.33906601932884,12.2,10.0894585342213));
#239577=CARTESIAN_POINT('Ctrl Pts',(-5.34203005963352,12.2,10.0916927362542));
#239578=CARTESIAN_POINT('Ctrl Pts',(-5.34500206706547,12.2,10.0939276001457));
#239579=CARTESIAN_POINT('Ctrl Pts',(-5.34798202987464,12.2,10.0961630852207));
#239580=CARTESIAN_POINT('Ctrl Pts',(-5.35096199214246,12.2,10.0983985698895));
#239581=CARTESIAN_POINT('Ctrl Pts',(-5.35394991167131,12.2,10.1006346766355));
#239582=CARTESIAN_POINT('Ctrl Pts',(-5.35694577458804,12.2,10.1028713629577));
#239583=CARTESIAN_POINT('Ctrl Pts',(-5.35994163750477,12.2,10.1051080492799));
#239584=CARTESIAN_POINT('Ctrl Pts',(-5.36294544513714,12.2,10.1073453154085));
#239585=CARTESIAN_POINT('Ctrl Pts',(-5.36595718782008,12.2,10.1095831237439));
#239586=CARTESIAN_POINT('Ctrl Pts',(-5.36896893050303,12.2,10.1118209320793));
#239587=CARTESIAN_POINT('Ctrl Pts',(-5.37198860785999,12.2,10.1140592842313));
#239588=CARTESIAN_POINT('Ctrl Pts',(-5.37501621054167,12.2,10.1162981424833));
#239589=CARTESIAN_POINT('Ctrl Pts',(-5.37804381322335,12.2,10.1185370007353));
#239590=CARTESIAN_POINT('Ctrl Pts',(-5.38107934096302,12.2,10.1207763667539));
#239591=CARTESIAN_POINT('Ctrl Pts',(-5.3841227816434,12.2,10.1230161957558));
#239592=CARTESIAN_POINT('Ctrl Pts',(-5.38716622232378,12.2,10.1252560247578));
#239593=CARTESIAN_POINT('Ctrl Pts',(-5.39021757578411,12.2,10.1274963145027));
#239594=CARTESIAN_POINT('Ctrl Pts',(-5.39327682915818,12.2,10.1297370202831));
#239595=CARTESIAN_POINT('Ctrl Pts',(-5.39735583402745,12.2,10.1327246282618));
#239596=CARTESIAN_POINT('Ctrl Pts',(-5.40144888360935,12.2,10.135712968183));
#239597=CARTESIAN_POINT('Ctrl Pts',(-5.40555595979698,12.2,10.1387019907558));
#239598=CARTESIAN_POINT('Ctrl Pts',(-5.40863626665791,12.2,10.1409437574818));
#239599=CARTESIAN_POINT('Ctrl Pts',(-5.4117244634376,12.2,10.1431859115926));
#239600=CARTESIAN_POINT('Ctrl Pts',(-5.41482055400006,12.2,10.145428447));
#239601=CARTESIAN_POINT('Origin',(-5.66257110645729E-14,15.2,-1.77635683940025E-14));
#239602=CARTESIAN_POINT('',(-5.85257411492611,15.2,8.56667970922507));
#239603=CARTESIAN_POINT('',(-5.85257411492611,12.2,8.56667970922507));
#239604=CARTESIAN_POINT('',(-5.85257411500006,15.2,8.56667970899998));
#239605=CARTESIAN_POINT('Origin',(-5.66257110645729E-14,12.2,-1.77635683940025E-14));
#239606=CARTESIAN_POINT('Origin',(-5.66257110645729E-14,15.2,-1.77635683940025E-14));
#239607=CARTESIAN_POINT('Origin',(-5.66257110645729E-14,15.2,-1.77635683940025E-14));
#239608=CARTESIAN_POINT('',(-6.80355049700006,15.2,9.27155330199999));
#239609=CARTESIAN_POINT('',(-7.10901226959732,15.2,9.03946594391174));
#239610=CARTESIAN_POINT('Origin',(-5.66257110645729E-14,15.2,-1.77635683940025E-14));
#239611=CARTESIAN_POINT('',(-7.10901226959732,12.2,9.03946594391174));
#239612=CARTESIAN_POINT('',(-7.10901227000006,15.2,9.03946594399999));
#239613=CARTESIAN_POINT('',(-6.80355049700006,12.2,9.27155330199999));
#239614=CARTESIAN_POINT('Origin',(-5.66257110645729E-14,12.2,-1.77635683940025E-14));
#239615=CARTESIAN_POINT('',(-6.80355049700006,15.2,9.27155330199999));
#239616=CARTESIAN_POINT('Ctrl Pts',(-5.85257411500006,15.2,8.56667970999998));
#239617=CARTESIAN_POINT('Ctrl Pts',(-5.85257411500006,11.6,8.56667970999998));
#239618=CARTESIAN_POINT('Ctrl Pts',(-5.85268447900006,15.2,8.56681469199999));
#239619=CARTESIAN_POINT('Ctrl Pts',(-5.85268447900006,11.6,8.56681469199999));
#239620=CARTESIAN_POINT('Ctrl Pts',(-5.85290912900006,15.2,8.56708931899998));
#239621=CARTESIAN_POINT('Ctrl Pts',(-5.85290912900006,11.6,8.56708931899998));
#239622=CARTESIAN_POINT('Ctrl Pts',(-5.85324973300006,15.2,8.56750527399999));
#239623=CARTESIAN_POINT('Ctrl Pts',(-5.85324973300006,11.6,8.56750527399999));
#239624=CARTESIAN_POINT('Ctrl Pts',(-5.85370897500006,15.2,8.56806526199998));
#239625=CARTESIAN_POINT('Ctrl Pts',(-5.85370897500006,11.6,8.56806526199998));
#239626=CARTESIAN_POINT('Ctrl Pts',(-5.85429055500006,15.2,8.56877298399999));
#239627=CARTESIAN_POINT('Ctrl Pts',(-5.85429055500006,11.6,8.56877298399999));
#239628=CARTESIAN_POINT('Ctrl Pts',(-5.85488228100006,15.2,8.56949158299999));
#239629=CARTESIAN_POINT('Ctrl Pts',(-5.85488228100006,11.6,8.56949158299999));
#239630=CARTESIAN_POINT('Ctrl Pts',(-5.85548078500006,15.2,8.57021692599999));
#239631=CARTESIAN_POINT('Ctrl Pts',(-5.85548078500006,11.6,8.57021692599999));
#239632=CARTESIAN_POINT('Ctrl Pts',(-5.85608606100006,15.2,8.57094898199998));
#239633=CARTESIAN_POINT('Ctrl Pts',(-5.85608606100006,11.6,8.57094898199998));
#239634=CARTESIAN_POINT('Ctrl Pts',(-5.85669810700006,15.2,8.57168771799999));
#239635=CARTESIAN_POINT('Ctrl Pts',(-5.85669810700006,11.6,8.57168771799999));
#239636=CARTESIAN_POINT('Ctrl Pts',(-5.85731691800006,15.2,8.57243310399999));
#239637=CARTESIAN_POINT('Ctrl Pts',(-5.85731691800006,11.6,8.57243310399999));
#239638=CARTESIAN_POINT('Ctrl Pts',(-5.85794249300006,15.2,8.57318510299999));
#239639=CARTESIAN_POINT('Ctrl Pts',(-5.85794249300006,11.6,8.57318510299999));
#239640=CARTESIAN_POINT('Ctrl Pts',(-5.85857482800006,15.2,8.57394368799999));
#239641=CARTESIAN_POINT('Ctrl Pts',(-5.85857482800006,11.6,8.57394368799999));
#239642=CARTESIAN_POINT('Ctrl Pts',(-5.85921392000006,15.2,8.57470882699998));
#239643=CARTESIAN_POINT('Ctrl Pts',(-5.85921392000006,11.6,8.57470882699998));
#239644=CARTESIAN_POINT('Ctrl Pts',(-5.85985976600006,15.2,8.57548048599998));
#239645=CARTESIAN_POINT('Ctrl Pts',(-5.85985976600006,11.6,8.57548048599998));
#239646=CARTESIAN_POINT('Ctrl Pts',(-5.86051236100006,15.2,8.57625863599999));
#239647=CARTESIAN_POINT('Ctrl Pts',(-5.86051236100006,11.6,8.57625863599999));
#239648=CARTESIAN_POINT('Ctrl Pts',(-5.86117170400006,15.2,8.57704324399998));
#239649=CARTESIAN_POINT('Ctrl Pts',(-5.86117170400006,11.6,8.57704324399998));
#239650=CARTESIAN_POINT('Ctrl Pts',(-5.86183779200006,15.2,8.57783428099999));
#239651=CARTESIAN_POINT('Ctrl Pts',(-5.86183779200006,11.6,8.57783428099999));
#239652=CARTESIAN_POINT('Ctrl Pts',(-5.86251062000006,15.2,8.57863171499999));
#239653=CARTESIAN_POINT('Ctrl Pts',(-5.86251062000006,11.6,8.57863171499999));
#239654=CARTESIAN_POINT('Ctrl Pts',(-5.86319018700006,15.2,8.57943551599998));
#239655=CARTESIAN_POINT('Ctrl Pts',(-5.86319018700006,11.6,8.57943551599998));
#239656=CARTESIAN_POINT('Ctrl Pts',(-5.86387648700006,15.2,8.58024565199998));
#239657=CARTESIAN_POINT('Ctrl Pts',(-5.86387648700006,11.6,8.58024565199998));
#239658=CARTESIAN_POINT('Ctrl Pts',(-5.86456952000006,15.2,8.58106209499999));
#239659=CARTESIAN_POINT('Ctrl Pts',(-5.86456952000006,11.6,8.58106209499999));
#239660=CARTESIAN_POINT('Ctrl Pts',(-5.86526928000006,15.2,8.58188481199999));
#239661=CARTESIAN_POINT('Ctrl Pts',(-5.86526928000006,11.6,8.58188481199999));
#239662=CARTESIAN_POINT('Ctrl Pts',(-5.86597576600006,15.2,8.58271377599999));
#239663=CARTESIAN_POINT('Ctrl Pts',(-5.86597576600006,11.6,8.58271377599999));
#239664=CARTESIAN_POINT('Ctrl Pts',(-5.86668897300005,15.2,8.58354895499998));
#239665=CARTESIAN_POINT('Ctrl Pts',(-5.86668897300005,11.6,8.58354895499998));
#239666=CARTESIAN_POINT('Ctrl Pts',(-5.86740890000006,15.2,8.58439031999998));
#239667=CARTESIAN_POINT('Ctrl Pts',(-5.86740890000006,11.6,8.58439031999998));
#239668=CARTESIAN_POINT('Ctrl Pts',(-5.86813554300006,15.2,8.58523783999999));
#239669=CARTESIAN_POINT('Ctrl Pts',(-5.86813554300006,11.6,8.58523783999999));
#239670=CARTESIAN_POINT('Ctrl Pts',(-5.86886889700006,15.2,8.58609148699998));
#239671=CARTESIAN_POINT('Ctrl Pts',(-5.86886889700006,11.6,8.58609148699998));
#239672=CARTESIAN_POINT('Ctrl Pts',(-5.86960896300006,15.2,8.58695123199999));
#239673=CARTESIAN_POINT('Ctrl Pts',(-5.86960896300006,11.6,8.58695123199999));
#239674=CARTESIAN_POINT('Ctrl Pts',(-5.87035573300006,15.2,8.58781704399998));
#239675=CARTESIAN_POINT('Ctrl Pts',(-5.87035573300006,11.6,8.58781704399998));
#239676=CARTESIAN_POINT('Ctrl Pts',(-5.87110920700006,15.2,8.58868889599999));
#239677=CARTESIAN_POINT('Ctrl Pts',(-5.87110920700006,11.6,8.58868889599999));
#239678=CARTESIAN_POINT('Ctrl Pts',(-5.87186938100006,15.2,8.58956675699999));
#239679=CARTESIAN_POINT('Ctrl Pts',(-5.87186938100006,11.6,8.58956675699999));
#239680=CARTESIAN_POINT('Ctrl Pts',(-5.87263625200006,15.2,8.59045059899999));
#239681=CARTESIAN_POINT('Ctrl Pts',(-5.87263625200006,11.6,8.59045059899999));
#239682=CARTESIAN_POINT('Ctrl Pts',(-5.87340981600006,15.2,8.59134039399999));
#239683=CARTESIAN_POINT('Ctrl Pts',(-5.87340981600006,11.6,8.59134039399999));
#239684=CARTESIAN_POINT('Ctrl Pts',(-5.87419007000006,15.2,8.59223611299999));
#239685=CARTESIAN_POINT('Ctrl Pts',(-5.87419007000006,11.6,8.59223611299999));
#239686=CARTESIAN_POINT('Ctrl Pts',(-5.87497701300006,15.2,8.59313772699998));
#239687=CARTESIAN_POINT('Ctrl Pts',(-5.87497701300006,11.6,8.59313772699998));
#239688=CARTESIAN_POINT('Ctrl Pts',(-5.87577063900006,15.2,8.59404520899999));
#239689=CARTESIAN_POINT('Ctrl Pts',(-5.87577063900006,11.6,8.59404520899999));
#239690=CARTESIAN_POINT('Ctrl Pts',(-5.87657094700006,15.2,8.59495852899999));
#239691=CARTESIAN_POINT('Ctrl Pts',(-5.87657094700006,11.6,8.59495852899999));
#239692=CARTESIAN_POINT('Ctrl Pts',(-5.87737793200006,15.2,8.59587765999999));
#239693=CARTESIAN_POINT('Ctrl Pts',(-5.87737793200006,11.6,8.59587765999999));
#239694=CARTESIAN_POINT('Ctrl Pts',(-5.87819159300006,15.2,8.59680257399998));
#239695=CARTESIAN_POINT('Ctrl Pts',(-5.87819159300006,11.6,8.59680257399998));
#239696=CARTESIAN_POINT('Ctrl Pts',(-5.87901192500006,15.2,8.59773324399999));
#239697=CARTESIAN_POINT('Ctrl Pts',(-5.87901192500006,11.6,8.59773324399999));
#239698=CARTESIAN_POINT('Ctrl Pts',(-5.87983892500006,15.2,8.59866964099999));
#239699=CARTESIAN_POINT('Ctrl Pts',(-5.87983892500006,11.6,8.59866964099999));
#239700=CARTESIAN_POINT('Ctrl Pts',(-5.88067259200006,15.2,8.59961173899999));
#239701=CARTESIAN_POINT('Ctrl Pts',(-5.88067259200006,11.6,8.59961173899999));
#239702=CARTESIAN_POINT('Ctrl Pts',(-5.88151291900005,15.2,8.60055950999998));
#239703=CARTESIAN_POINT('Ctrl Pts',(-5.88151291900005,11.6,8.60055950999998));
#239704=CARTESIAN_POINT('Ctrl Pts',(-5.88235990700006,15.2,8.60151292499998));
#239705=CARTESIAN_POINT('Ctrl Pts',(-5.88235990700006,11.6,8.60151292499998));
#239706=CARTESIAN_POINT('Ctrl Pts',(-5.88321355000006,15.2,8.60247195899999));
#239707=CARTESIAN_POINT('Ctrl Pts',(-5.88321355000006,11.6,8.60247195899999));
#239708=CARTESIAN_POINT('Ctrl Pts',(-5.88407384700006,15.2,8.60343658499998));
#239709=CARTESIAN_POINT('Ctrl Pts',(-5.88407384700006,11.6,8.60343658499998));
#239710=CARTESIAN_POINT('Ctrl Pts',(-5.88494079200006,15.2,8.60440677399998));
#239711=CARTESIAN_POINT('Ctrl Pts',(-5.88494079200006,11.6,8.60440677399998));
#239712=CARTESIAN_POINT('Ctrl Pts',(-5.88581438400006,15.2,8.60538250099999));
#239713=CARTESIAN_POINT('Ctrl Pts',(-5.88581438400006,11.6,8.60538250099999));
#239714=CARTESIAN_POINT('Ctrl Pts',(-5.88669462000006,15.2,8.60636373999998));
#239715=CARTESIAN_POINT('Ctrl Pts',(-5.88669462000006,11.6,8.60636373999998));
#239716=CARTESIAN_POINT('Ctrl Pts',(-5.88758149600006,15.2,8.60735046199999));
#239717=CARTESIAN_POINT('Ctrl Pts',(-5.88758149600006,11.6,8.60735046199999));
#239718=CARTESIAN_POINT('Ctrl Pts',(-5.88847500900005,15.2,8.60834264199998));
#239719=CARTESIAN_POINT('Ctrl Pts',(-5.88847500900005,11.6,8.60834264199998));
#239720=CARTESIAN_POINT('Ctrl Pts',(-5.88937515600006,15.2,8.60934025399999));
#239721=CARTESIAN_POINT('Ctrl Pts',(-5.88937515600006,11.6,8.60934025399999));
#239722=CARTESIAN_POINT('Ctrl Pts',(-5.89028193300006,15.2,8.61034327099999));
#239723=CARTESIAN_POINT('Ctrl Pts',(-5.89028193300006,11.6,8.61034327099999));
#239724=CARTESIAN_POINT('Ctrl Pts',(-5.89119533900006,15.2,8.61135166799999));
#239725=CARTESIAN_POINT('Ctrl Pts',(-5.89119533900006,11.6,8.61135166799999));
#239726=CARTESIAN_POINT('Ctrl Pts',(-5.89211536900006,15.2,8.61236541799999));
#239727=CARTESIAN_POINT('Ctrl Pts',(-5.89211536900006,11.6,8.61236541799999));
#239728=CARTESIAN_POINT('Ctrl Pts',(-5.89304202000006,15.2,8.61338449399998));
#239729=CARTESIAN_POINT('Ctrl Pts',(-5.89304202000006,11.6,8.61338449399998));
#239730=CARTESIAN_POINT('Ctrl Pts',(-5.89397529000006,15.2,8.61440887399999));
#239731=CARTESIAN_POINT('Ctrl Pts',(-5.89397529000006,11.6,8.61440887399999));
#239732=CARTESIAN_POINT('Ctrl Pts',(-5.89491517500006,15.2,8.61543852799999));
#239733=CARTESIAN_POINT('Ctrl Pts',(-5.89491517500006,11.6,8.61543852799999));
#239734=CARTESIAN_POINT('Ctrl Pts',(-5.89586167100006,15.2,8.61647343299998));
#239735=CARTESIAN_POINT('Ctrl Pts',(-5.89586167100006,11.6,8.61647343299998));
#239736=CARTESIAN_POINT('Ctrl Pts',(-5.89681477700006,15.2,8.61751356399999));
#239737=CARTESIAN_POINT('Ctrl Pts',(-5.89681477700006,11.6,8.61751356399999));
#239738=CARTESIAN_POINT('Ctrl Pts',(-5.89777448900006,15.2,8.61855889399998));
#239739=CARTESIAN_POINT('Ctrl Pts',(-5.89777448900006,11.6,8.61855889399998));
#239740=CARTESIAN_POINT('Ctrl Pts',(-5.89874080200006,15.2,8.61960939799998));
#239741=CARTESIAN_POINT('Ctrl Pts',(-5.89874080200006,11.6,8.61960939799998));
#239742=CARTESIAN_POINT('Ctrl Pts',(-5.89971371600006,15.2,8.62066505199999));
#239743=CARTESIAN_POINT('Ctrl Pts',(-5.89971371600006,11.6,8.62066505199999));
#239744=CARTESIAN_POINT('Ctrl Pts',(-5.90069322500006,15.2,8.62172583099999));
#239745=CARTESIAN_POINT('Ctrl Pts',(-5.90069322500006,11.6,8.62172583099999));
#239746=CARTESIAN_POINT('Ctrl Pts',(-5.90167932900005,15.2,8.62279170899999));
#239747=CARTESIAN_POINT('Ctrl Pts',(-5.90167932900005,11.6,8.62279170899999));
#239748=CARTESIAN_POINT('Ctrl Pts',(-5.90267202200006,15.2,8.62386266099998));
#239749=CARTESIAN_POINT('Ctrl Pts',(-5.90267202200006,11.6,8.62386266099998));
#239750=CARTESIAN_POINT('Ctrl Pts',(-5.90367130100006,15.2,8.62493866499998));
#239751=CARTESIAN_POINT('Ctrl Pts',(-5.90367130100006,11.6,8.62493866499998));
#239752=CARTESIAN_POINT('Ctrl Pts',(-5.90467716500005,15.2,8.62601969299998));
#239753=CARTESIAN_POINT('Ctrl Pts',(-5.90467716500005,11.6,8.62601969299998));
#239754=CARTESIAN_POINT('Ctrl Pts',(-5.90568960800006,15.2,8.62710572199998));
#239755=CARTESIAN_POINT('Ctrl Pts',(-5.90568960800006,11.6,8.62710572199998));
#239756=CARTESIAN_POINT('Ctrl Pts',(-5.90670863000006,15.2,8.62819672699998));
#239757=CARTESIAN_POINT('Ctrl Pts',(-5.90670863000006,11.6,8.62819672699998));
#239758=CARTESIAN_POINT('Ctrl Pts',(-5.90773422600006,15.2,8.62929268599999));
#239759=CARTESIAN_POINT('Ctrl Pts',(-5.90773422600006,11.6,8.62929268599999));
#239760=CARTESIAN_POINT('Ctrl Pts',(-5.90876639200006,15.2,8.63039357199998));
#239761=CARTESIAN_POINT('Ctrl Pts',(-5.90876639200006,11.6,8.63039357199998));
#239762=CARTESIAN_POINT('Ctrl Pts',(-5.90980512700006,15.2,8.63149936299998));
#239763=CARTESIAN_POINT('Ctrl Pts',(-5.90980512700006,11.6,8.63149936299998));
#239764=CARTESIAN_POINT('Ctrl Pts',(-5.91085042600006,15.2,8.63261003299998));
#239765=CARTESIAN_POINT('Ctrl Pts',(-5.91085042600006,11.6,8.63261003299998));
#239766=CARTESIAN_POINT('Ctrl Pts',(-5.91190228800006,15.2,8.63372555999998));
#239767=CARTESIAN_POINT('Ctrl Pts',(-5.91190228800006,11.6,8.63372555999998));
#239768=CARTESIAN_POINT('Ctrl Pts',(-5.91296070800006,15.2,8.63484591899999));
#239769=CARTESIAN_POINT('Ctrl Pts',(-5.91296070800006,11.6,8.63484591899999));
#239770=CARTESIAN_POINT('Ctrl Pts',(-5.91402568300006,15.2,8.63597108799999));
#239771=CARTESIAN_POINT('Ctrl Pts',(-5.91402568300006,11.6,8.63597108799999));
#239772=CARTESIAN_POINT('Ctrl Pts',(-5.91509721000006,15.2,8.63710104099999));
#239773=CARTESIAN_POINT('Ctrl Pts',(-5.91509721000006,11.6,8.63710104099999));
#239774=CARTESIAN_POINT('Ctrl Pts',(-5.91617528800006,15.2,8.63823575499998));
#239775=CARTESIAN_POINT('Ctrl Pts',(-5.91617528800006,11.6,8.63823575499998));
#239776=CARTESIAN_POINT('Ctrl Pts',(-5.91725991000006,15.2,8.63937520899999));
#239777=CARTESIAN_POINT('Ctrl Pts',(-5.91725991000006,11.6,8.63937520899999));
#239778=CARTESIAN_POINT('Ctrl Pts',(-5.91835107500006,15.2,8.64051937699998));
#239779=CARTESIAN_POINT('Ctrl Pts',(-5.91835107500006,11.6,8.64051937699998));
#239780=CARTESIAN_POINT('Ctrl Pts',(-5.91944878200006,15.2,8.64166823699998));
#239781=CARTESIAN_POINT('Ctrl Pts',(-5.91944878200006,11.6,8.64166823699998));
#239782=CARTESIAN_POINT('Ctrl Pts',(-5.92055302300006,15.2,8.64282176599998));
#239783=CARTESIAN_POINT('Ctrl Pts',(-5.92055302300006,11.6,8.64282176599998));
#239784=CARTESIAN_POINT('Ctrl Pts',(-5.92166379800006,15.2,8.64397993999999));
#239785=CARTESIAN_POINT('Ctrl Pts',(-5.92166379800006,11.6,8.64397993999999));
#239786=CARTESIAN_POINT('Ctrl Pts',(-5.92278110400006,15.2,8.64514273699999));
#239787=CARTESIAN_POINT('Ctrl Pts',(-5.92278110400006,11.6,8.64514273699999));
#239788=CARTESIAN_POINT('Ctrl Pts',(-5.92390493600006,15.2,8.64631013299999));
#239789=CARTESIAN_POINT('Ctrl Pts',(-5.92390493600006,11.6,8.64631013299999));
#239790=CARTESIAN_POINT('Ctrl Pts',(-5.92503529200005,15.2,8.64748210699998));
#239791=CARTESIAN_POINT('Ctrl Pts',(-5.92503529200005,11.6,8.64748210699998));
#239792=CARTESIAN_POINT('Ctrl Pts',(-5.92617217000006,15.2,8.64865863599999));
#239793=CARTESIAN_POINT('Ctrl Pts',(-5.92617217000006,11.6,8.64865863599999));
#239794=CARTESIAN_POINT('Ctrl Pts',(-5.92731556500006,15.2,8.64983969599999));
#239795=CARTESIAN_POINT('Ctrl Pts',(-5.92731556500006,11.6,8.64983969599999));
#239796=CARTESIAN_POINT('Ctrl Pts',(-5.92846547400006,15.2,8.65102526599999));
#239797=CARTESIAN_POINT('Ctrl Pts',(-5.92846547400006,11.6,8.65102526599999));
#239798=CARTESIAN_POINT('Ctrl Pts',(-5.92962189500006,15.2,8.65221532199998));
#239799=CARTESIAN_POINT('Ctrl Pts',(-5.92962189500006,11.6,8.65221532199998));
#239800=CARTESIAN_POINT('Ctrl Pts',(-5.93078482300006,15.2,8.65340984299999));
#239801=CARTESIAN_POINT('Ctrl Pts',(-5.93078482300006,11.6,8.65340984299999));
#239802=CARTESIAN_POINT('Ctrl Pts',(-5.93195425800006,15.2,8.65460880699998));
#239803=CARTESIAN_POINT('Ctrl Pts',(-5.93195425800006,11.6,8.65460880699998));
#239804=CARTESIAN_POINT('Ctrl Pts',(-5.93313019300005,15.2,8.65581219199999));
#239805=CARTESIAN_POINT('Ctrl Pts',(-5.93313019300005,11.6,8.65581219199999));
#239806=CARTESIAN_POINT('Ctrl Pts',(-5.93431262700006,15.2,8.65701997399999));
#239807=CARTESIAN_POINT('Ctrl Pts',(-5.93431262700006,11.6,8.65701997399999));
#239808=CARTESIAN_POINT('Ctrl Pts',(-5.93550155700005,15.2,8.65823213299999));
#239809=CARTESIAN_POINT('Ctrl Pts',(-5.93550155700005,11.6,8.65823213299999));
#239810=CARTESIAN_POINT('Ctrl Pts',(-5.93669698000006,15.2,8.65944864499999));
#239811=CARTESIAN_POINT('Ctrl Pts',(-5.93669698000006,11.6,8.65944864499999));
#239812=CARTESIAN_POINT('Ctrl Pts',(-5.93789889100006,15.2,8.66066949099999));
#239813=CARTESIAN_POINT('Ctrl Pts',(-5.93789889100006,11.6,8.66066949099999));
#239814=CARTESIAN_POINT('Ctrl Pts',(-5.93910728800005,15.2,8.66189464799999));
#239815=CARTESIAN_POINT('Ctrl Pts',(-5.93910728800005,11.6,8.66189464799999));
#239816=CARTESIAN_POINT('Ctrl Pts',(-5.94032216900006,15.2,8.66312409399999));
#239817=CARTESIAN_POINT('Ctrl Pts',(-5.94032216900006,11.6,8.66312409399999));
#239818=CARTESIAN_POINT('Ctrl Pts',(-5.94154353000006,15.2,8.66435780699998));
#239819=CARTESIAN_POINT('Ctrl Pts',(-5.94154353000006,11.6,8.66435780699998));
#239820=CARTESIAN_POINT('Ctrl Pts',(-5.94277136700006,15.2,8.66559576699999));
#239821=CARTESIAN_POINT('Ctrl Pts',(-5.94277136700006,11.6,8.66559576699999));
#239822=CARTESIAN_POINT('Ctrl Pts',(-5.94400567700006,15.2,8.66683795199998));
#239823=CARTESIAN_POINT('Ctrl Pts',(-5.94400567700006,11.6,8.66683795199998));
#239824=CARTESIAN_POINT('Ctrl Pts',(-5.94524645700006,15.2,8.66808433999999));
#239825=CARTESIAN_POINT('Ctrl Pts',(-5.94524645700006,11.6,8.66808433999999));
#239826=CARTESIAN_POINT('Ctrl Pts',(-5.94649370400006,15.2,8.66933490999998));
#239827=CARTESIAN_POINT('Ctrl Pts',(-5.94649370400006,11.6,8.66933490999998));
#239828=CARTESIAN_POINT('Ctrl Pts',(-5.94774741600006,15.2,8.67058964199998));
#239829=CARTESIAN_POINT('Ctrl Pts',(-5.94774741600006,11.6,8.67058964199998));
#239830=CARTESIAN_POINT('Ctrl Pts',(-5.94900758800006,15.2,8.67184851399998));
#239831=CARTESIAN_POINT('Ctrl Pts',(-5.94900758800006,11.6,8.67184851399998));
#239832=CARTESIAN_POINT('Ctrl Pts',(-5.95027421800006,15.2,8.67311150599999));
#239833=CARTESIAN_POINT('Ctrl Pts',(-5.95027421800006,11.6,8.67311150599999));
#239834=CARTESIAN_POINT('Ctrl Pts',(-5.95154730300006,15.2,8.67437859499999));
#239835=CARTESIAN_POINT('Ctrl Pts',(-5.95154730300006,11.6,8.67437859499999));
#239836=CARTESIAN_POINT('Ctrl Pts',(-5.95282683800006,15.2,8.67564976199999));
#239837=CARTESIAN_POINT('Ctrl Pts',(-5.95282683800006,11.6,8.67564976199999));
#239838=CARTESIAN_POINT('Ctrl Pts',(-5.95411282100006,15.2,8.67692498599999));
#239839=CARTESIAN_POINT('Ctrl Pts',(-5.95411282100006,11.6,8.67692498599999));
#239840=CARTESIAN_POINT('Ctrl Pts',(-5.95540525000006,15.2,8.67820424599999));
#239841=CARTESIAN_POINT('Ctrl Pts',(-5.95540525000006,11.6,8.67820424599999));
#239842=CARTESIAN_POINT('Ctrl Pts',(-5.95670412000006,15.2,8.67948751999998));
#239843=CARTESIAN_POINT('Ctrl Pts',(-5.95670412000006,11.6,8.67948751999998));
#239844=CARTESIAN_POINT('Ctrl Pts',(-5.95800942900006,15.2,8.68077478999999));
#239845=CARTESIAN_POINT('Ctrl Pts',(-5.95800942900006,11.6,8.68077478999999));
#239846=CARTESIAN_POINT('Ctrl Pts',(-5.95932117300006,15.2,8.68206603399998));
#239847=CARTESIAN_POINT('Ctrl Pts',(-5.95932117300006,11.6,8.68206603399998));
#239848=CARTESIAN_POINT('Ctrl Pts',(-5.96063935000006,15.2,8.68336123199999));
#239849=CARTESIAN_POINT('Ctrl Pts',(-5.96063935000006,11.6,8.68336123199999));
#239850=CARTESIAN_POINT('Ctrl Pts',(-5.96196395500006,15.2,8.68466036399998));
#239851=CARTESIAN_POINT('Ctrl Pts',(-5.96196395500006,11.6,8.68466036399998));
#239852=CARTESIAN_POINT('Ctrl Pts',(-5.96329498600006,15.2,8.68596340999999));
#239853=CARTESIAN_POINT('Ctrl Pts',(-5.96329498600006,11.6,8.68596340999999));
#239854=CARTESIAN_POINT('Ctrl Pts',(-5.96463244000006,15.2,8.68727034899998));
#239855=CARTESIAN_POINT('Ctrl Pts',(-5.96463244000006,11.6,8.68727034899998));
#239856=CARTESIAN_POINT('Ctrl Pts',(-5.96597631400006,15.2,8.68858115999998));
#239857=CARTESIAN_POINT('Ctrl Pts',(-5.96597631400006,11.6,8.68858115999998));
#239858=CARTESIAN_POINT('Ctrl Pts',(-5.96732660300006,15.2,8.68989582599998));
#239859=CARTESIAN_POINT('Ctrl Pts',(-5.96732660300006,11.6,8.68989582599998));
#239860=CARTESIAN_POINT('Ctrl Pts',(-5.96868330600006,15.2,8.69121432499998));
#239861=CARTESIAN_POINT('Ctrl Pts',(-5.96868330600006,11.6,8.69121432499998));
#239862=CARTESIAN_POINT('Ctrl Pts',(-5.97004641900006,15.2,8.69253663699999));
#239863=CARTESIAN_POINT('Ctrl Pts',(-5.97004641900006,11.6,8.69253663699999));
#239864=CARTESIAN_POINT('Ctrl Pts',(-5.97141593900006,15.2,8.69386274199999));
#239865=CARTESIAN_POINT('Ctrl Pts',(-5.97141593900006,11.6,8.69386274199999));
#239866=CARTESIAN_POINT('Ctrl Pts',(-5.97279186200006,15.2,8.69519262299999));
#239867=CARTESIAN_POINT('Ctrl Pts',(-5.97279186200006,11.6,8.69519262299999));
#239868=CARTESIAN_POINT('Ctrl Pts',(-5.97417418500005,15.2,8.69652625599999));
#239869=CARTESIAN_POINT('Ctrl Pts',(-5.97417418500005,11.6,8.69652625599999));
#239870=CARTESIAN_POINT('Ctrl Pts',(-5.97556290600005,15.2,8.69786362499998));
#239871=CARTESIAN_POINT('Ctrl Pts',(-5.97556290600005,11.6,8.69786362499998));
#239872=CARTESIAN_POINT('Ctrl Pts',(-5.97695802100006,15.2,8.69920470999999));
#239873=CARTESIAN_POINT('Ctrl Pts',(-5.97695802100006,11.6,8.69920470999999));
#239874=CARTESIAN_POINT('Ctrl Pts',(-5.97835952600006,15.2,8.70054948899998));
#239875=CARTESIAN_POINT('Ctrl Pts',(-5.97835952600006,11.6,8.70054948899998));
#239876=CARTESIAN_POINT('Ctrl Pts',(-5.97976742000006,15.2,8.70189794599998));
#239877=CARTESIAN_POINT('Ctrl Pts',(-5.97976742000006,11.6,8.70189794599998));
#239878=CARTESIAN_POINT('Ctrl Pts',(-5.98118169700006,15.2,8.70325005899998));
#239879=CARTESIAN_POINT('Ctrl Pts',(-5.98118169700006,11.6,8.70325005899998));
#239880=CARTESIAN_POINT('Ctrl Pts',(-5.98260235600006,15.2,8.70460580999998));
#239881=CARTESIAN_POINT('Ctrl Pts',(-5.98260235600006,11.6,8.70460580999998));
#239882=CARTESIAN_POINT('Ctrl Pts',(-5.98402939300006,15.2,8.70596517899998));
#239883=CARTESIAN_POINT('Ctrl Pts',(-5.98402939300006,11.6,8.70596517899998));
#239884=CARTESIAN_POINT('Ctrl Pts',(-5.98546280500006,15.2,8.70732814899998));
#239885=CARTESIAN_POINT('Ctrl Pts',(-5.98546280500006,11.6,8.70732814899998));
#239886=CARTESIAN_POINT('Ctrl Pts',(-5.98690258900006,15.2,8.70869469899999));
#239887=CARTESIAN_POINT('Ctrl Pts',(-5.98690258900006,11.6,8.70869469899999));
#239888=CARTESIAN_POINT('Ctrl Pts',(-5.98834874000006,15.2,8.71006481099998));
#239889=CARTESIAN_POINT('Ctrl Pts',(-5.98834874000006,11.6,8.71006481099998));
#239890=CARTESIAN_POINT('Ctrl Pts',(-5.98980125800006,15.2,8.71143846499999));
#239891=CARTESIAN_POINT('Ctrl Pts',(-5.98980125800006,11.6,8.71143846499999));
#239892=CARTESIAN_POINT('Ctrl Pts',(-5.99126013800006,15.2,8.71281564199998));
#239893=CARTESIAN_POINT('Ctrl Pts',(-5.99126013800006,11.6,8.71281564199998));
#239894=CARTESIAN_POINT('Ctrl Pts',(-5.99272537600006,15.2,8.71419632499999));
#239895=CARTESIAN_POINT('Ctrl Pts',(-5.99272537600006,11.6,8.71419632499999));
#239896=CARTESIAN_POINT('Ctrl Pts',(-5.99419697000006,15.2,8.71558049499999));
#239897=CARTESIAN_POINT('Ctrl Pts',(-5.99419697000006,11.6,8.71558049499999));
#239898=CARTESIAN_POINT('Ctrl Pts',(-5.99567491600006,15.2,8.71696813099998));
#239899=CARTESIAN_POINT('Ctrl Pts',(-5.99567491600006,11.6,8.71696813099998));
#239900=CARTESIAN_POINT('Ctrl Pts',(-5.99715921200006,15.2,8.71835921799999));
#239901=CARTESIAN_POINT('Ctrl Pts',(-5.99715921200006,11.6,8.71835921799999));
#239902=CARTESIAN_POINT('Ctrl Pts',(-5.99864985300006,15.2,8.71975373399999));
#239903=CARTESIAN_POINT('Ctrl Pts',(-5.99864985300006,11.6,8.71975373399999));
#239904=CARTESIAN_POINT('Ctrl Pts',(-6.00014683800006,15.2,8.72115166199999));
#239905=CARTESIAN_POINT('Ctrl Pts',(-6.00014683800006,11.6,8.72115166199999));
#239906=CARTESIAN_POINT('Ctrl Pts',(-6.00165016300005,15.2,8.72255298499999));
#239907=CARTESIAN_POINT('Ctrl Pts',(-6.00165016300005,11.6,8.72255298499999));
#239908=CARTESIAN_POINT('Ctrl Pts',(-6.00315982300006,15.2,8.72395768299998));
#239909=CARTESIAN_POINT('Ctrl Pts',(-6.00315982300006,11.6,8.72395768299998));
#239910=CARTESIAN_POINT('Ctrl Pts',(-6.00467581700006,15.2,8.72536573799999));
#239911=CARTESIAN_POINT('Ctrl Pts',(-6.00467581700006,11.6,8.72536573799999));
#239912=CARTESIAN_POINT('Ctrl Pts',(-6.00619814200006,15.2,8.72677713199998));
#239913=CARTESIAN_POINT('Ctrl Pts',(-6.00619814200006,11.6,8.72677713199998));
#239914=CARTESIAN_POINT('Ctrl Pts',(-6.00772679200006,15.2,8.72819184599999));
#239915=CARTESIAN_POINT('Ctrl Pts',(-6.00772679200006,11.6,8.72819184599999));
#239916=CARTESIAN_POINT('Ctrl Pts',(-6.00926176600006,15.2,8.72960986299999));
#239917=CARTESIAN_POINT('Ctrl Pts',(-6.00926176600006,11.6,8.72960986299999));
#239918=CARTESIAN_POINT('Ctrl Pts',(-6.01080306100005,15.2,8.73103116499998));
#239919=CARTESIAN_POINT('Ctrl Pts',(-6.01080306100005,11.6,8.73103116499998));
#239920=CARTESIAN_POINT('Ctrl Pts',(-6.01235067300006,15.2,8.73245573399998));
#239921=CARTESIAN_POINT('Ctrl Pts',(-6.01235067300006,11.6,8.73245573399998));
#239922=CARTESIAN_POINT('Ctrl Pts',(-6.01390459900006,15.2,8.73388355199998));
#239923=CARTESIAN_POINT('Ctrl Pts',(-6.01390459900006,11.6,8.73388355199998));
#239924=CARTESIAN_POINT('Ctrl Pts',(-6.01546483600006,15.2,8.73531459999998));
#239925=CARTESIAN_POINT('Ctrl Pts',(-6.01546483600006,11.6,8.73531459999998));
#239926=CARTESIAN_POINT('Ctrl Pts',(-6.01703137900006,15.2,8.73674886199998));
#239927=CARTESIAN_POINT('Ctrl Pts',(-6.01703137900006,11.6,8.73674886199998));
#239928=CARTESIAN_POINT('Ctrl Pts',(-6.01860422800006,15.2,8.73818631899999));
#239929=CARTESIAN_POINT('Ctrl Pts',(-6.01860422800006,11.6,8.73818631899999));
#239930=CARTESIAN_POINT('Ctrl Pts',(-6.02018337700006,15.2,8.73962695399998));
#239931=CARTESIAN_POINT('Ctrl Pts',(-6.02018337700006,11.6,8.73962695399998));
#239932=CARTESIAN_POINT('Ctrl Pts',(-6.02176882400006,15.2,8.74107074799999));
#239933=CARTESIAN_POINT('Ctrl Pts',(-6.02176882400006,11.6,8.74107074799999));
#239934=CARTESIAN_POINT('Ctrl Pts',(-6.02336056600006,15.2,8.74251768599999));
#239935=CARTESIAN_POINT('Ctrl Pts',(-6.02336056600006,11.6,8.74251768599999));
#239936=CARTESIAN_POINT('Ctrl Pts',(-6.02495860000006,15.2,8.74396774899999));
#239937=CARTESIAN_POINT('Ctrl Pts',(-6.02495860000006,11.6,8.74396774899999));
#239938=CARTESIAN_POINT('Ctrl Pts',(-6.02656292100006,15.2,8.74542091899999));
#239939=CARTESIAN_POINT('Ctrl Pts',(-6.02656292100006,11.6,8.74542091899999));
#239940=CARTESIAN_POINT('Ctrl Pts',(-6.02817352800006,15.2,8.74687717999999));
#239941=CARTESIAN_POINT('Ctrl Pts',(-6.02817352800006,11.6,8.74687717999999));
#239942=CARTESIAN_POINT('Ctrl Pts',(-6.02979041500006,15.2,8.74833651299999));
#239943=CARTESIAN_POINT('Ctrl Pts',(-6.02979041500006,11.6,8.74833651299999));
#239944=CARTESIAN_POINT('Ctrl Pts',(-6.03141358200006,15.2,8.74979890199998));
#239945=CARTESIAN_POINT('Ctrl Pts',(-6.03141358200006,11.6,8.74979890199998));
#239946=CARTESIAN_POINT('Ctrl Pts',(-6.03304302400006,15.2,8.75126432999998));
#239947=CARTESIAN_POINT('Ctrl Pts',(-6.03304302400006,11.6,8.75126432999998));
#239948=CARTESIAN_POINT('Ctrl Pts',(-6.03467873800006,15.2,8.75273277899998));
#239949=CARTESIAN_POINT('Ctrl Pts',(-6.03467873800006,11.6,8.75273277899998));
#239950=CARTESIAN_POINT('Ctrl Pts',(-6.03632072000006,15.2,8.75420423299998));
#239951=CARTESIAN_POINT('Ctrl Pts',(-6.03632072000006,11.6,8.75420423299998));
#239952=CARTESIAN_POINT('Ctrl Pts',(-6.03796896800006,15.2,8.75567867399998));
#239953=CARTESIAN_POINT('Ctrl Pts',(-6.03796896800006,11.6,8.75567867399998));
#239954=CARTESIAN_POINT('Ctrl Pts',(-6.03962347900006,15.2,8.75715608399998));
#239955=CARTESIAN_POINT('Ctrl Pts',(-6.03962347900006,11.6,8.75715608399998));
#239956=CARTESIAN_POINT('Ctrl Pts',(-6.04128424700006,15.2,8.75863644799999));
#239957=CARTESIAN_POINT('Ctrl Pts',(-6.04128424700006,11.6,8.75863644799999));
#239958=CARTESIAN_POINT('Ctrl Pts',(-6.04295127300006,15.2,8.76011974899999));
#239959=CARTESIAN_POINT('Ctrl Pts',(-6.04295127300006,11.6,8.76011974899999));
#239960=CARTESIAN_POINT('Ctrl Pts',(-6.04462455100006,15.2,8.76160596799998));
#239961=CARTESIAN_POINT('Ctrl Pts',(-6.04462455100006,11.6,8.76160596799998));
#239962=CARTESIAN_POINT('Ctrl Pts',(-6.04630407800006,15.2,8.76309509099999));
#239963=CARTESIAN_POINT('Ctrl Pts',(-6.04630407800006,11.6,8.76309509099999));
#239964=CARTESIAN_POINT('Ctrl Pts',(-6.04798985100006,15.2,8.76458709899998));
#239965=CARTESIAN_POINT('Ctrl Pts',(-6.04798985100006,11.6,8.76458709899998));
#239966=CARTESIAN_POINT('Ctrl Pts',(-6.04968186800006,15.2,8.76608197799998));
#239967=CARTESIAN_POINT('Ctrl Pts',(-6.04968186800006,11.6,8.76608197799998));
#239968=CARTESIAN_POINT('Ctrl Pts',(-6.05138012300006,15.2,8.76757970899998));
#239969=CARTESIAN_POINT('Ctrl Pts',(-6.05138012300006,11.6,8.76757970899998));
#239970=CARTESIAN_POINT('Ctrl Pts',(-6.05308461500006,15.2,8.76908027599999));
#239971=CARTESIAN_POINT('Ctrl Pts',(-6.05308461500006,11.6,8.76908027599999));
#239972=CARTESIAN_POINT('Ctrl Pts',(-6.05479534000006,15.2,8.77058366199999));
#239973=CARTESIAN_POINT('Ctrl Pts',(-6.05479534000006,11.6,8.77058366199999));
#239974=CARTESIAN_POINT('Ctrl Pts',(-6.05651229500006,15.2,8.77208985199999));
#239975=CARTESIAN_POINT('Ctrl Pts',(-6.05651229500006,11.6,8.77208985199999));
#239976=CARTESIAN_POINT('Ctrl Pts',(-6.05823547800005,15.2,8.77359882999999));
#239977=CARTESIAN_POINT('Ctrl Pts',(-6.05823547800005,11.6,8.77359882999999));
#239978=CARTESIAN_POINT('Ctrl Pts',(-6.05996488300006,15.2,8.77511057699999));
#239979=CARTESIAN_POINT('Ctrl Pts',(-6.05996488300006,11.6,8.77511057699999));
#239980=CARTESIAN_POINT('Ctrl Pts',(-6.06170050700006,15.2,8.77662507799998));
#239981=CARTESIAN_POINT('Ctrl Pts',(-6.06170050700006,11.6,8.77662507799998));
#239982=CARTESIAN_POINT('Ctrl Pts',(-6.06344234900006,15.2,8.77814231799999));
#239983=CARTESIAN_POINT('Ctrl Pts',(-6.06344234900006,11.6,8.77814231799999));
#239984=CARTESIAN_POINT('Ctrl Pts',(-6.06519040500006,15.2,8.77966227799998));
#239985=CARTESIAN_POINT('Ctrl Pts',(-6.06519040500006,11.6,8.77966227799998));
#239986=CARTESIAN_POINT('Ctrl Pts',(-6.06694467000006,15.2,8.78118494499999));
#239987=CARTESIAN_POINT('Ctrl Pts',(-6.06694467000006,11.6,8.78118494499999));
#239988=CARTESIAN_POINT('Ctrl Pts',(-6.06870514300006,15.2,8.78271030099998));
#239989=CARTESIAN_POINT('Ctrl Pts',(-6.06870514300006,11.6,8.78271030099998));
#239990=CARTESIAN_POINT('Ctrl Pts',(-6.07047181900006,15.2,8.78423833099998));
#239991=CARTESIAN_POINT('Ctrl Pts',(-6.07047181900006,11.6,8.78423833099998));
#239992=CARTESIAN_POINT('Ctrl Pts',(-6.07224469600006,15.2,8.78576901799999));
#239993=CARTESIAN_POINT('Ctrl Pts',(-6.07224469600006,11.6,8.78576901799999));
#239994=CARTESIAN_POINT('Ctrl Pts',(-6.07402377100006,15.2,8.78730234699999));
#239995=CARTESIAN_POINT('Ctrl Pts',(-6.07402377100006,11.6,8.78730234699999));
#239996=CARTESIAN_POINT('Ctrl Pts',(-6.07580903900006,15.2,8.78883829999998));
#239997=CARTESIAN_POINT('Ctrl Pts',(-6.07580903900006,11.6,8.78883829999998));
#239998=CARTESIAN_POINT('Ctrl Pts',(-6.07760049900006,15.2,8.79037686399998));
#239999=CARTESIAN_POINT('Ctrl Pts',(-6.07760049900006,11.6,8.79037686399998));
#240000=CARTESIAN_POINT('Ctrl Pts',(-6.07939814500006,15.2,8.79191802199998));
#240001=CARTESIAN_POINT('Ctrl Pts',(-6.07939814500006,11.6,8.79191802199998));
#240002=CARTESIAN_POINT('Ctrl Pts',(-6.08120197600006,15.2,8.79346175699999));
#240003=CARTESIAN_POINT('Ctrl Pts',(-6.08120197600006,11.6,8.79346175699999));
#240004=CARTESIAN_POINT('Ctrl Pts',(-6.08301198700006,15.2,8.79500805499998));
#240005=CARTESIAN_POINT('Ctrl Pts',(-6.08301198700006,11.6,8.79500805499998));
#240006=CARTESIAN_POINT('Ctrl Pts',(-6.08482817700006,15.2,8.79655689899998));
#240007=CARTESIAN_POINT('Ctrl Pts',(-6.08482817700006,11.6,8.79655689899998));
#240008=CARTESIAN_POINT('Ctrl Pts',(-6.08665054100006,15.2,8.79810827499998));
#240009=CARTESIAN_POINT('Ctrl Pts',(-6.08665054100006,11.6,8.79810827499998));
#240010=CARTESIAN_POINT('Ctrl Pts',(-6.08847907600006,15.2,8.79966216699999));
#240011=CARTESIAN_POINT('Ctrl Pts',(-6.08847907600006,11.6,8.79966216699999));
#240012=CARTESIAN_POINT('Ctrl Pts',(-6.09031377800005,15.2,8.80121855699999));
#240013=CARTESIAN_POINT('Ctrl Pts',(-6.09031377800005,11.6,8.80121855699999));
#240014=CARTESIAN_POINT('Ctrl Pts',(-6.09215464600006,15.2,8.80277743299999));
#240015=CARTESIAN_POINT('Ctrl Pts',(-6.09215464600006,11.6,8.80277743299999));
#240016=CARTESIAN_POINT('Ctrl Pts',(-6.09400167400006,15.2,8.80433877799998));
#240017=CARTESIAN_POINT('Ctrl Pts',(-6.09400167400006,11.6,8.80433877799998));
#240018=CARTESIAN_POINT('Ctrl Pts',(-6.09585486000006,15.2,8.80590257699998));
#240019=CARTESIAN_POINT('Ctrl Pts',(-6.09585486000006,11.6,8.80590257699998));
#240020=CARTESIAN_POINT('Ctrl Pts',(-6.09771420200006,15.2,8.80746881399999));
#240021=CARTESIAN_POINT('Ctrl Pts',(-6.09771420200006,11.6,8.80746881399999));
#240022=CARTESIAN_POINT('Ctrl Pts',(-6.09957969400006,15.2,8.80903747399999));
#240023=CARTESIAN_POINT('Ctrl Pts',(-6.09957969400006,11.6,8.80903747399999));
#240024=CARTESIAN_POINT('Ctrl Pts',(-6.10145133600006,15.2,8.81060854199998));
#240025=CARTESIAN_POINT('Ctrl Pts',(-6.10145133600006,11.6,8.81060854199998));
#240026=CARTESIAN_POINT('Ctrl Pts',(-6.10332912100006,15.2,8.81218200199999));
#240027=CARTESIAN_POINT('Ctrl Pts',(-6.10332912100006,11.6,8.81218200199999));
#240028=CARTESIAN_POINT('Ctrl Pts',(-6.10521304800006,15.2,8.81375783999999));
#240029=CARTESIAN_POINT('Ctrl Pts',(-6.10521304800006,11.6,8.81375783999999));
#240030=CARTESIAN_POINT('Ctrl Pts',(-6.10710311400006,15.2,8.81533604099998));
#240031=CARTESIAN_POINT('Ctrl Pts',(-6.10710311400006,11.6,8.81533604099998));
#240032=CARTESIAN_POINT('Ctrl Pts',(-6.10899931500006,15.2,8.81691658799999));
#240033=CARTESIAN_POINT('Ctrl Pts',(-6.10899931500006,11.6,8.81691658799999));
#240034=CARTESIAN_POINT('Ctrl Pts',(-6.11090164700006,15.2,8.81849946799999));
#240035=CARTESIAN_POINT('Ctrl Pts',(-6.11090164700006,11.6,8.81849946799999));
#240036=CARTESIAN_POINT('Ctrl Pts',(-6.11281010800006,15.2,8.82008466499999));
#240037=CARTESIAN_POINT('Ctrl Pts',(-6.11281010800006,11.6,8.82008466499999));
#240038=CARTESIAN_POINT('Ctrl Pts',(-6.11472469300006,15.2,8.82167216499998));
#240039=CARTESIAN_POINT('Ctrl Pts',(-6.11472469300006,11.6,8.82167216499998));
#240040=CARTESIAN_POINT('Ctrl Pts',(-6.11664540100006,15.2,8.82326195199998));
#240041=CARTESIAN_POINT('Ctrl Pts',(-6.11664540100006,11.6,8.82326195199998));
#240042=CARTESIAN_POINT('Ctrl Pts',(-6.11857222800006,15.2,8.82485401199999));
#240043=CARTESIAN_POINT('Ctrl Pts',(-6.11857222800006,11.6,8.82485401199999));
#240044=CARTESIAN_POINT('Ctrl Pts',(-6.12050516900006,15.2,8.82644832899998));
#240045=CARTESIAN_POINT('Ctrl Pts',(-6.12050516900006,11.6,8.82644832899998));
#240046=CARTESIAN_POINT('Ctrl Pts',(-6.12244422200006,15.2,8.82804488899998));
#240047=CARTESIAN_POINT('Ctrl Pts',(-6.12244422200006,11.6,8.82804488899998));
#240048=CARTESIAN_POINT('Ctrl Pts',(-6.12438938300006,15.2,8.82964367799998));
#240049=CARTESIAN_POINT('Ctrl Pts',(-6.12438938300006,11.6,8.82964367799998));
#240050=CARTESIAN_POINT('Ctrl Pts',(-6.12634065100006,15.2,8.83124467999998));
#240051=CARTESIAN_POINT('Ctrl Pts',(-6.12634065100006,11.6,8.83124467999998));
#240052=CARTESIAN_POINT('Ctrl Pts',(-6.12829802000006,15.2,8.83284788199998));
#240053=CARTESIAN_POINT('Ctrl Pts',(-6.12829802000006,11.6,8.83284788199998));
#240054=CARTESIAN_POINT('Ctrl Pts',(-6.13026148800006,15.2,8.83445326699999));
#240055=CARTESIAN_POINT('Ctrl Pts',(-6.13026148800006,11.6,8.83445326699999));
#240056=CARTESIAN_POINT('Ctrl Pts',(-6.13223105200006,15.2,8.83606082299998));
#240057=CARTESIAN_POINT('Ctrl Pts',(-6.13223105200006,11.6,8.83606082299998));
#240058=CARTESIAN_POINT('Ctrl Pts',(-6.13420670700005,15.2,8.83767053499999));
#240059=CARTESIAN_POINT('Ctrl Pts',(-6.13420670700005,11.6,8.83767053499999));
#240060=CARTESIAN_POINT('Ctrl Pts',(-6.13618845100006,15.2,8.83928238599999));
#240061=CARTESIAN_POINT('Ctrl Pts',(-6.13618845100006,11.6,8.83928238599999));
#240062=CARTESIAN_POINT('Ctrl Pts',(-6.13817628100006,15.2,8.84089636499999));
#240063=CARTESIAN_POINT('Ctrl Pts',(-6.13817628100006,11.6,8.84089636499999));
#240064=CARTESIAN_POINT('Ctrl Pts',(-6.14017019300006,15.2,8.84251245499998));
#240065=CARTESIAN_POINT('Ctrl Pts',(-6.14017019300006,11.6,8.84251245499998));
#240066=CARTESIAN_POINT('Ctrl Pts',(-6.14217018400006,15.2,8.84413064299999));
#240067=CARTESIAN_POINT('Ctrl Pts',(-6.14217018400006,11.6,8.84413064299999));
#240068=CARTESIAN_POINT('Ctrl Pts',(-6.14417625100006,15.2,8.84575091399999));
#240069=CARTESIAN_POINT('Ctrl Pts',(-6.14417625100006,11.6,8.84575091399999));
#240070=CARTESIAN_POINT('Ctrl Pts',(-6.14618838900006,15.2,8.84737325599998));
#240071=CARTESIAN_POINT('Ctrl Pts',(-6.14618838900006,11.6,8.84737325599998));
#240072=CARTESIAN_POINT('Ctrl Pts',(-6.14820659700006,15.2,8.84899765099998));
#240073=CARTESIAN_POINT('Ctrl Pts',(-6.14820659700006,11.6,8.84899765099998));
#240074=CARTESIAN_POINT('Ctrl Pts',(-6.15023087000006,15.2,8.85062408799998));
#240075=CARTESIAN_POINT('Ctrl Pts',(-6.15023087000006,11.6,8.85062408799998));
#240076=CARTESIAN_POINT('Ctrl Pts',(-6.15226120500005,15.2,8.85225255099999));
#240077=CARTESIAN_POINT('Ctrl Pts',(-6.15226120500005,11.6,8.85225255099999));
#240078=CARTESIAN_POINT('Ctrl Pts',(-6.15429760000006,15.2,8.85388302599999));
#240079=CARTESIAN_POINT('Ctrl Pts',(-6.15429760000006,11.6,8.85388302599999));
#240080=CARTESIAN_POINT('Ctrl Pts',(-6.15634005000006,15.2,8.85551550099999));
#240081=CARTESIAN_POINT('Ctrl Pts',(-6.15634005000006,11.6,8.85551550099999));
#240082=CARTESIAN_POINT('Ctrl Pts',(-6.15838855200006,15.2,8.85714995899999));
#240083=CARTESIAN_POINT('Ctrl Pts',(-6.15838855200006,11.6,8.85714995899999));
#240084=CARTESIAN_POINT('Ctrl Pts',(-6.16044310400006,15.2,8.85878638799999));
#240085=CARTESIAN_POINT('Ctrl Pts',(-6.16044310400006,11.6,8.85878638799999));
#240086=CARTESIAN_POINT('Ctrl Pts',(-6.16250370100006,15.2,8.86042477299998));
#240087=CARTESIAN_POINT('Ctrl Pts',(-6.16250370100006,11.6,8.86042477299998));
#240088=CARTESIAN_POINT('Ctrl Pts',(-6.16457034000006,15.2,8.86206510199998));
#240089=CARTESIAN_POINT('Ctrl Pts',(-6.16457034000006,11.6,8.86206510199998));
#240090=CARTESIAN_POINT('Ctrl Pts',(-6.16664301800006,15.2,8.86370735799998));
#240091=CARTESIAN_POINT('Ctrl Pts',(-6.16664301800006,11.6,8.86370735799998));
#240092=CARTESIAN_POINT('Ctrl Pts',(-6.16872173200006,15.2,8.86535152999999));
#240093=CARTESIAN_POINT('Ctrl Pts',(-6.16872173200006,11.6,8.86535152999999));
#240094=CARTESIAN_POINT('Ctrl Pts',(-6.17080647900006,15.2,8.86699760299998));
#240095=CARTESIAN_POINT('Ctrl Pts',(-6.17080647900006,11.6,8.86699760299998));
#240096=CARTESIAN_POINT('Ctrl Pts',(-6.17289725400005,15.2,8.86864556399999));
#240097=CARTESIAN_POINT('Ctrl Pts',(-6.17289725400005,11.6,8.86864556399999));
#240098=CARTESIAN_POINT('Ctrl Pts',(-6.17499405600006,15.2,8.87029539799999));
#240099=CARTESIAN_POINT('Ctrl Pts',(-6.17499405600006,11.6,8.87029539799999));
#240100=CARTESIAN_POINT('Ctrl Pts',(-6.17709687900006,15.2,8.87194709099998));
#240101=CARTESIAN_POINT('Ctrl Pts',(-6.17709687900006,11.6,8.87194709099998));
#240102=CARTESIAN_POINT('Ctrl Pts',(-6.17920572100005,15.2,8.87360063199999));
#240103=CARTESIAN_POINT('Ctrl Pts',(-6.17920572100005,11.6,8.87360063199999));
#240104=CARTESIAN_POINT('Ctrl Pts',(-6.18132057900006,15.2,8.87525600499998));
#240105=CARTESIAN_POINT('Ctrl Pts',(-6.18132057900006,11.6,8.87525600499998));
#240106=CARTESIAN_POINT('Ctrl Pts',(-6.18344144900006,15.2,8.87691319699999));
#240107=CARTESIAN_POINT('Ctrl Pts',(-6.18344144900006,11.6,8.87691319699999));
#240108=CARTESIAN_POINT('Ctrl Pts',(-6.18556832800006,15.2,8.87857219399999));
#240109=CARTESIAN_POINT('Ctrl Pts',(-6.18556832800006,11.6,8.87857219399999));
#240110=CARTESIAN_POINT('Ctrl Pts',(-6.18770121400006,15.2,8.88023298499999));
#240111=CARTESIAN_POINT('Ctrl Pts',(-6.18770121400006,11.6,8.88023298499999));
#240112=CARTESIAN_POINT('Ctrl Pts',(-6.18984010100006,15.2,8.88189555299999));
#240113=CARTESIAN_POINT('Ctrl Pts',(-6.18984010100006,11.6,8.88189555299999));
#240114=CARTESIAN_POINT('Ctrl Pts',(-6.19198498800006,15.2,8.88355988699999));
#240115=CARTESIAN_POINT('Ctrl Pts',(-6.19198498800006,11.6,8.88355988699999));
#240116=CARTESIAN_POINT('Ctrl Pts',(-6.19413587000006,15.2,8.88522597299998));
#240117=CARTESIAN_POINT('Ctrl Pts',(-6.19413587000006,11.6,8.88522597299998));
#240118=CARTESIAN_POINT('Ctrl Pts',(-6.19629274400006,15.2,8.88689379699999));
#240119=CARTESIAN_POINT('Ctrl Pts',(-6.19629274400006,11.6,8.88689379699999));
#240120=CARTESIAN_POINT('Ctrl Pts',(-6.19845560700006,15.2,8.88856334699998));
#240121=CARTESIAN_POINT('Ctrl Pts',(-6.19845560700006,11.6,8.88856334699998));
#240122=CARTESIAN_POINT('Ctrl Pts',(-6.20062445500006,15.2,8.89023460999999));
#240123=CARTESIAN_POINT('Ctrl Pts',(-6.20062445500006,11.6,8.89023460999999));
#240124=CARTESIAN_POINT('Ctrl Pts',(-6.20279928600006,15.2,8.89190756899998));
#240125=CARTESIAN_POINT('Ctrl Pts',(-6.20279928600006,11.6,8.89190756899998));
#240126=CARTESIAN_POINT('Ctrl Pts',(-6.20498009600006,15.2,8.89358221499998));
#240127=CARTESIAN_POINT('Ctrl Pts',(-6.20498009600006,11.6,8.89358221499998));
#240128=CARTESIAN_POINT('Ctrl Pts',(-6.20716688100006,15.2,8.89525853399999));
#240129=CARTESIAN_POINT('Ctrl Pts',(-6.20716688100006,11.6,8.89525853399999));
#240130=CARTESIAN_POINT('Ctrl Pts',(-6.20935963800005,15.2,8.89693651099999));
#240131=CARTESIAN_POINT('Ctrl Pts',(-6.20935963800005,11.6,8.89693651099999));
#240132=CARTESIAN_POINT('Ctrl Pts',(-6.21155836400006,15.2,8.89861613499999));
#240133=CARTESIAN_POINT('Ctrl Pts',(-6.21155836400006,11.6,8.89861613499999));
#240134=CARTESIAN_POINT('Ctrl Pts',(-6.21376305600006,15.2,8.90029739199999));
#240135=CARTESIAN_POINT('Ctrl Pts',(-6.21376305600006,11.6,8.90029739199999));
#240136=CARTESIAN_POINT('Ctrl Pts',(-6.21597370900006,15.2,8.90198026899998));
#240137=CARTESIAN_POINT('Ctrl Pts',(-6.21597370900006,11.6,8.90198026899998));
#240138=CARTESIAN_POINT('Ctrl Pts',(-6.21819032200006,15.2,8.90366475299999));
#240139=CARTESIAN_POINT('Ctrl Pts',(-6.21819032200006,11.6,8.90366475299999));
#240140=CARTESIAN_POINT('Ctrl Pts',(-6.22041289000006,15.2,8.90535083099999));
#240141=CARTESIAN_POINT('Ctrl Pts',(-6.22041289000006,11.6,8.90535083099999));
#240142=CARTESIAN_POINT('Ctrl Pts',(-6.22264140900006,15.2,8.90703849099998));
#240143=CARTESIAN_POINT('Ctrl Pts',(-6.22264140900006,11.6,8.90703849099998));
#240144=CARTESIAN_POINT('Ctrl Pts',(-6.22487587700006,15.2,8.90872771899998));
#240145=CARTESIAN_POINT('Ctrl Pts',(-6.22487587700006,11.6,8.90872771899998));
#240146=CARTESIAN_POINT('Ctrl Pts',(-6.22711629100006,15.2,8.91041850199999));
#240147=CARTESIAN_POINT('Ctrl Pts',(-6.22711629100006,11.6,8.91041850199999));
#240148=CARTESIAN_POINT('Ctrl Pts',(-6.22936264600006,15.2,8.91211082799998));
#240149=CARTESIAN_POINT('Ctrl Pts',(-6.22936264600006,11.6,8.91211082799998));
#240150=CARTESIAN_POINT('Ctrl Pts',(-6.23161494000006,15.2,8.91380468399999));
#240151=CARTESIAN_POINT('Ctrl Pts',(-6.23161494000006,11.6,8.91380468399999));
#240152=CARTESIAN_POINT('Ctrl Pts',(-6.23387316900006,15.2,8.91550005599999));
#240153=CARTESIAN_POINT('Ctrl Pts',(-6.23387316900006,11.6,8.91550005599999));
#240154=CARTESIAN_POINT('Ctrl Pts',(-6.23613733000006,15.2,8.91719693299999));
#240155=CARTESIAN_POINT('Ctrl Pts',(-6.23613733000006,11.6,8.91719693299999));
#240156=CARTESIAN_POINT('Ctrl Pts',(-6.23840741900006,15.2,8.91889530199999));
#240157=CARTESIAN_POINT('Ctrl Pts',(-6.23840741900006,11.6,8.91889530199999));
#240158=CARTESIAN_POINT('Ctrl Pts',(-6.24068343300006,15.2,8.92059515099999));
#240159=CARTESIAN_POINT('Ctrl Pts',(-6.24068343300006,11.6,8.92059515099999));
#240160=CARTESIAN_POINT('Ctrl Pts',(-6.24296537000006,15.2,8.92229646399999));
#240161=CARTESIAN_POINT('Ctrl Pts',(-6.24296537000006,11.6,8.92229646399999));
#240162=CARTESIAN_POINT('Ctrl Pts',(-6.24525322300006,15.2,8.92399923299998));
#240163=CARTESIAN_POINT('Ctrl Pts',(-6.24525322300006,11.6,8.92399923299998));
#240164=CARTESIAN_POINT('Ctrl Pts',(-6.24754699300006,15.2,8.92570344299998));
#240165=CARTESIAN_POINT('Ctrl Pts',(-6.24754699300006,11.6,8.92570344299998));
#240166=CARTESIAN_POINT('Ctrl Pts',(-6.24984667300006,15.2,8.92740908099999));
#240167=CARTESIAN_POINT('Ctrl Pts',(-6.24984667300006,11.6,8.92740908099999));
#240168=CARTESIAN_POINT('Ctrl Pts',(-6.25215226200006,15.2,8.92911613599999));
#240169=CARTESIAN_POINT('Ctrl Pts',(-6.25215226200006,11.6,8.92911613599999));
#240170=CARTESIAN_POINT('Ctrl Pts',(-6.25446375500006,15.2,8.93082459399999));
#240171=CARTESIAN_POINT('Ctrl Pts',(-6.25446375500006,11.6,8.93082459399999));
#240172=CARTESIAN_POINT('Ctrl Pts',(-6.25678115000006,15.2,8.93253444399999));
#240173=CARTESIAN_POINT('Ctrl Pts',(-6.25678115000006,11.6,8.93253444399999));
#240174=CARTESIAN_POINT('Ctrl Pts',(-6.25910444300006,15.2,8.93424567299999));
#240175=CARTESIAN_POINT('Ctrl Pts',(-6.25910444300006,11.6,8.93424567299999));
#240176=CARTESIAN_POINT('Ctrl Pts',(-6.26143363000006,15.2,8.93595826899999));
#240177=CARTESIAN_POINT('Ctrl Pts',(-6.26143363000006,11.6,8.93595826899999));
#240178=CARTESIAN_POINT('Ctrl Pts',(-6.26376870900006,15.2,8.93767221899999));
#240179=CARTESIAN_POINT('Ctrl Pts',(-6.26376870900006,11.6,8.93767221899999));
#240180=CARTESIAN_POINT('Ctrl Pts',(-6.26610967500006,15.2,8.93938750999999));
#240181=CARTESIAN_POINT('Ctrl Pts',(-6.26610967500006,11.6,8.93938750999999));
#240182=CARTESIAN_POINT('Ctrl Pts',(-6.26845652500006,15.2,8.94110413199999));
#240183=CARTESIAN_POINT('Ctrl Pts',(-6.26845652500006,11.6,8.94110413199999));
#240184=CARTESIAN_POINT('Ctrl Pts',(-6.27080925800006,15.2,8.94282207099998));
#240185=CARTESIAN_POINT('Ctrl Pts',(-6.27080925800006,11.6,8.94282207099998));
#240186=CARTESIAN_POINT('Ctrl Pts',(-6.27316786700006,15.2,8.94454131499998));
#240187=CARTESIAN_POINT('Ctrl Pts',(-6.27316786700006,11.6,8.94454131499998));
#240188=CARTESIAN_POINT('Ctrl Pts',(-6.27553235100006,15.2,8.94626185399999));
#240189=CARTESIAN_POINT('Ctrl Pts',(-6.27553235100006,11.6,8.94626185399999));
#240190=CARTESIAN_POINT('Ctrl Pts',(-6.27790270500006,15.2,8.94798367199999));
#240191=CARTESIAN_POINT('Ctrl Pts',(-6.27790270500006,11.6,8.94798367199999));
#240192=CARTESIAN_POINT('Ctrl Pts',(-6.28027892800006,15.2,8.94970675999998));
#240193=CARTESIAN_POINT('Ctrl Pts',(-6.28027892800006,11.6,8.94970675999998));
#240194=CARTESIAN_POINT('Ctrl Pts',(-6.28266101400006,15.2,8.95143110399999));
#240195=CARTESIAN_POINT('Ctrl Pts',(-6.28266101400006,11.6,8.95143110399999));
#240196=CARTESIAN_POINT('Ctrl Pts',(-6.28504896100006,15.2,8.95315669399999));
#240197=CARTESIAN_POINT('Ctrl Pts',(-6.28504896100006,11.6,8.95315669399999));
#240198=CARTESIAN_POINT('Ctrl Pts',(-6.28744276500006,15.2,8.95488351599998));
#240199=CARTESIAN_POINT('Ctrl Pts',(-6.28744276500006,11.6,8.95488351599998));
#240200=CARTESIAN_POINT('Ctrl Pts',(-6.28984242200006,15.2,8.95661155799999));
#240201=CARTESIAN_POINT('Ctrl Pts',(-6.28984242200006,11.6,8.95661155799999));
#240202=CARTESIAN_POINT('Ctrl Pts',(-6.29224793100006,15.2,8.95834080999999));
#240203=CARTESIAN_POINT('Ctrl Pts',(-6.29224793100006,11.6,8.95834080999999));
#240204=CARTESIAN_POINT('Ctrl Pts',(-6.29465928600006,15.2,8.96007125899999));
#240205=CARTESIAN_POINT('Ctrl Pts',(-6.29465928600006,11.6,8.96007125899999));
#240206=CARTESIAN_POINT('Ctrl Pts',(-6.29707648500006,15.2,8.96180289199999));
#240207=CARTESIAN_POINT('Ctrl Pts',(-6.29707648500006,11.6,8.96180289199999));
#240208=CARTESIAN_POINT('Ctrl Pts',(-6.29949952400006,15.2,8.96353569899999));
#240209=CARTESIAN_POINT('Ctrl Pts',(-6.29949952400006,11.6,8.96353569899999));
#240210=CARTESIAN_POINT('Ctrl Pts',(-6.30192840000006,15.2,8.96526966599998));
#240211=CARTESIAN_POINT('Ctrl Pts',(-6.30192840000006,11.6,8.96526966599998));
#240212=CARTESIAN_POINT('Ctrl Pts',(-6.30436311000006,15.2,8.96700478399998));
#240213=CARTESIAN_POINT('Ctrl Pts',(-6.30436311000006,11.6,8.96700478399998));
#240214=CARTESIAN_POINT('Ctrl Pts',(-6.30680365000006,15.2,8.96874103899999));
#240215=CARTESIAN_POINT('Ctrl Pts',(-6.30680365000006,11.6,8.96874103899999));
#240216=CARTESIAN_POINT('Ctrl Pts',(-6.30925001600006,15.2,8.97047841899998));
#240217=CARTESIAN_POINT('Ctrl Pts',(-6.30925001600006,11.6,8.97047841899998));
#240218=CARTESIAN_POINT('Ctrl Pts',(-6.31170220500006,15.2,8.97221691499999));
#240219=CARTESIAN_POINT('Ctrl Pts',(-6.31170220500006,11.6,8.97221691499999));
#240220=CARTESIAN_POINT('Ctrl Pts',(-6.31416021400006,15.2,8.97395651199999));
#240221=CARTESIAN_POINT('Ctrl Pts',(-6.31416021400006,11.6,8.97395651199999));
#240222=CARTESIAN_POINT('Ctrl Pts',(-6.31662403900005,15.2,8.97569720099998));
#240223=CARTESIAN_POINT('Ctrl Pts',(-6.31662403900005,11.6,8.97569720099998));
#240224=CARTESIAN_POINT('Ctrl Pts',(-6.31909367800006,15.2,8.97743896899998));
#240225=CARTESIAN_POINT('Ctrl Pts',(-6.31909367800006,11.6,8.97743896899998));
#240226=CARTESIAN_POINT('Ctrl Pts',(-6.32156912600006,15.2,8.97918180399999));
#240227=CARTESIAN_POINT('Ctrl Pts',(-6.32156912600006,11.6,8.97918180399999));
#240228=CARTESIAN_POINT('Ctrl Pts',(-6.32405038000006,15.2,8.98092569599999));
#240229=CARTESIAN_POINT('Ctrl Pts',(-6.32405038000006,11.6,8.98092569599999));
#240230=CARTESIAN_POINT('Ctrl Pts',(-6.32653743600006,15.2,8.98267063199999));
#240231=CARTESIAN_POINT('Ctrl Pts',(-6.32653743600006,11.6,8.98267063199999));
#240232=CARTESIAN_POINT('Ctrl Pts',(-6.32903029200006,15.2,8.98441660099999));
#240233=CARTESIAN_POINT('Ctrl Pts',(-6.32903029200006,11.6,8.98441660099999));
#240234=CARTESIAN_POINT('Ctrl Pts',(-6.33152894400006,15.2,8.98616359099999));
#240235=CARTESIAN_POINT('Ctrl Pts',(-6.33152894400006,11.6,8.98616359099999));
#240236=CARTESIAN_POINT('Ctrl Pts',(-6.33403338800006,15.2,8.98791159199998));
#240237=CARTESIAN_POINT('Ctrl Pts',(-6.33403338800006,11.6,8.98791159199998));
#240238=CARTESIAN_POINT('Ctrl Pts',(-6.33654362200006,15.2,8.98966058999999));
#240239=CARTESIAN_POINT('Ctrl Pts',(-6.33654362200006,11.6,8.98966058999999));
#240240=CARTESIAN_POINT('Ctrl Pts',(-6.33905964000006,15.2,8.99141057699998));
#240241=CARTESIAN_POINT('Ctrl Pts',(-6.33905964000006,11.6,8.99141057699998));
#240242=CARTESIAN_POINT('Ctrl Pts',(-6.34158144100006,15.2,8.99316153799998));
#240243=CARTESIAN_POINT('Ctrl Pts',(-6.34158144100006,11.6,8.99316153799998));
#240244=CARTESIAN_POINT('Ctrl Pts',(-6.34410902100006,15.2,8.99491346499998));
#240245=CARTESIAN_POINT('Ctrl Pts',(-6.34410902100006,11.6,8.99491346499998));
#240246=CARTESIAN_POINT('Ctrl Pts',(-6.34664237500006,15.2,8.99666634499999));
#240247=CARTESIAN_POINT('Ctrl Pts',(-6.34664237500006,11.6,8.99666634499999));
#240248=CARTESIAN_POINT('Ctrl Pts',(-6.34918150200006,15.2,8.99842016499999));
#240249=CARTESIAN_POINT('Ctrl Pts',(-6.34918150200006,11.6,8.99842016499999));
#240250=CARTESIAN_POINT('Ctrl Pts',(-6.35172639700006,15.2,9.00017491799998));
#240251=CARTESIAN_POINT('Ctrl Pts',(-6.35172639700006,11.6,9.00017491799998));
#240252=CARTESIAN_POINT('Ctrl Pts',(-6.35427705800006,15.2,9.00193058899998));
#240253=CARTESIAN_POINT('Ctrl Pts',(-6.35427705800006,11.6,9.00193058899998));
#240254=CARTESIAN_POINT('Ctrl Pts',(-6.35683347900006,15.2,9.00368716799999));
#240255=CARTESIAN_POINT('Ctrl Pts',(-6.35683347900006,11.6,9.00368716799999));
#240256=CARTESIAN_POINT('Ctrl Pts',(-6.35939565800006,15.2,9.00544464399999));
#240257=CARTESIAN_POINT('Ctrl Pts',(-6.35939565800006,11.6,9.00544464399999));
#240258=CARTESIAN_POINT('Ctrl Pts',(-6.36196359200006,15.2,9.00720300599998));
#240259=CARTESIAN_POINT('Ctrl Pts',(-6.36196359200006,11.6,9.00720300599998));
#240260=CARTESIAN_POINT('Ctrl Pts',(-6.36453727800006,15.2,9.00896224299998));
#240261=CARTESIAN_POINT('Ctrl Pts',(-6.36453727800006,11.6,9.00896224299998));
#240262=CARTESIAN_POINT('Ctrl Pts',(-6.36711671100006,15.2,9.01072234299999));
#240263=CARTESIAN_POINT('Ctrl Pts',(-6.36711671100006,11.6,9.01072234299999));
#240264=CARTESIAN_POINT('Ctrl Pts',(-6.36970188900006,15.2,9.01248329499998));
#240265=CARTESIAN_POINT('Ctrl Pts',(-6.36970188900006,11.6,9.01248329499998));
#240266=CARTESIAN_POINT('Ctrl Pts',(-6.37229280700006,15.2,9.01424508899999));
#240267=CARTESIAN_POINT('Ctrl Pts',(-6.37229280700006,11.6,9.01424508899999));
#240268=CARTESIAN_POINT('Ctrl Pts',(-6.37488946300006,15.2,9.01600771299999));
#240269=CARTESIAN_POINT('Ctrl Pts',(-6.37488946300006,11.6,9.01600771299999));
#240270=CARTESIAN_POINT('Ctrl Pts',(-6.37749185300006,15.2,9.01777115699998));
#240271=CARTESIAN_POINT('Ctrl Pts',(-6.37749185300006,11.6,9.01777115699998));
#240272=CARTESIAN_POINT('Ctrl Pts',(-6.38009997400006,15.2,9.01953540799998));
#240273=CARTESIAN_POINT('Ctrl Pts',(-6.38009997400006,11.6,9.01953540799998));
#240274=CARTESIAN_POINT('Ctrl Pts',(-6.38271382100006,15.2,9.02130045699998));
#240275=CARTESIAN_POINT('Ctrl Pts',(-6.38271382100006,11.6,9.02130045699998));
#240276=CARTESIAN_POINT('Ctrl Pts',(-6.38533339300006,15.2,9.02306629299999));
#240277=CARTESIAN_POINT('Ctrl Pts',(-6.38533339300006,11.6,9.02306629299999));
#240278=CARTESIAN_POINT('Ctrl Pts',(-6.38795868400006,15.2,9.02483290399999));
#240279=CARTESIAN_POINT('Ctrl Pts',(-6.38795868400006,11.6,9.02483290399999));
#240280=CARTESIAN_POINT('Ctrl Pts',(-6.39058969200006,15.2,9.02660027899999));
#240281=CARTESIAN_POINT('Ctrl Pts',(-6.39058969200006,11.6,9.02660027899999));
#240282=CARTESIAN_POINT('Ctrl Pts',(-6.39322641400006,15.2,9.02836840899998));
#240283=CARTESIAN_POINT('Ctrl Pts',(-6.39322641400006,11.6,9.02836840899998));
#240284=CARTESIAN_POINT('Ctrl Pts',(-6.39586884500006,15.2,9.03013728199999));
#240285=CARTESIAN_POINT('Ctrl Pts',(-6.39586884500006,11.6,9.03013728199999));
#240286=CARTESIAN_POINT('Ctrl Pts',(-6.39851698300006,15.2,9.03190688599998));
#240287=CARTESIAN_POINT('Ctrl Pts',(-6.39851698300006,11.6,9.03190688599998));
#240288=CARTESIAN_POINT('Ctrl Pts',(-6.40117082500006,15.2,9.03367721299999));
#240289=CARTESIAN_POINT('Ctrl Pts',(-6.40117082500006,11.6,9.03367721299999));
#240290=CARTESIAN_POINT('Ctrl Pts',(-6.40383036500006,15.2,9.03544824899999));
#240291=CARTESIAN_POINT('Ctrl Pts',(-6.40383036500006,11.6,9.03544824899999));
#240292=CARTESIAN_POINT('Ctrl Pts',(-6.40649560100006,15.2,9.03721998699999));
#240293=CARTESIAN_POINT('Ctrl Pts',(-6.40649560100006,11.6,9.03721998699999));
#240294=CARTESIAN_POINT('Ctrl Pts',(-6.40916652900006,15.2,9.03899241299998));
#240295=CARTESIAN_POINT('Ctrl Pts',(-6.40916652900006,11.6,9.03899241299998));
#240296=CARTESIAN_POINT('Ctrl Pts',(-6.41184314700006,15.2,9.04076551799999));
#240297=CARTESIAN_POINT('Ctrl Pts',(-6.41184314700006,11.6,9.04076551799999));
#240298=CARTESIAN_POINT('Ctrl Pts',(-6.41452545100006,15.2,9.04253928999999));
#240299=CARTESIAN_POINT('Ctrl Pts',(-6.41452545100006,11.6,9.04253928999999));
#240300=CARTESIAN_POINT('Ctrl Pts',(-6.41721343700006,15.2,9.04431372099998));
#240301=CARTESIAN_POINT('Ctrl Pts',(-6.41721343700006,11.6,9.04431372099998));
#240302=CARTESIAN_POINT('Ctrl Pts',(-6.41990710100006,15.2,9.04608879799999));
#240303=CARTESIAN_POINT('Ctrl Pts',(-6.41990710100006,11.6,9.04608879799999));
#240304=CARTESIAN_POINT('Ctrl Pts',(-6.42260644100006,15.2,9.04786451099999));
#240305=CARTESIAN_POINT('Ctrl Pts',(-6.42260644100006,11.6,9.04786451099999));
#240306=CARTESIAN_POINT('Ctrl Pts',(-6.42531145200006,15.2,9.04964084999998));
#240307=CARTESIAN_POINT('Ctrl Pts',(-6.42531145200006,11.6,9.04964084999998));
#240308=CARTESIAN_POINT('Ctrl Pts',(-6.42802213200006,15.2,9.05141780399998));
#240309=CARTESIAN_POINT('Ctrl Pts',(-6.42802213200006,11.6,9.05141780399998));
#240310=CARTESIAN_POINT('Ctrl Pts',(-6.43073847600006,15.2,9.05319536199999));
#240311=CARTESIAN_POINT('Ctrl Pts',(-6.43073847600006,11.6,9.05319536199999));
#240312=CARTESIAN_POINT('Ctrl Pts',(-6.43346048200006,15.2,9.05497351499999));
#240313=CARTESIAN_POINT('Ctrl Pts',(-6.43346048200006,11.6,9.05497351499999));
#240314=CARTESIAN_POINT('Ctrl Pts',(-6.43618814600006,15.2,9.05675225099999));
#240315=CARTESIAN_POINT('Ctrl Pts',(-6.43618814600006,11.6,9.05675225099999));
#240316=CARTESIAN_POINT('Ctrl Pts',(-6.43892146400006,15.2,9.05853155999999));
#240317=CARTESIAN_POINT('Ctrl Pts',(-6.43892146400006,11.6,9.05853155999999));
#240318=CARTESIAN_POINT('Ctrl Pts',(-6.44166043400006,15.2,9.06031143299998));
#240319=CARTESIAN_POINT('Ctrl Pts',(-6.44166043400006,11.6,9.06031143299998));
#240320=CARTESIAN_POINT('Ctrl Pts',(-6.44440505000006,15.2,9.06209185799998));
#240321=CARTESIAN_POINT('Ctrl Pts',(-6.44440505000006,11.6,9.06209185799998));
#240322=CARTESIAN_POINT('Ctrl Pts',(-6.44715531200006,15.2,9.06387282399999));
#240323=CARTESIAN_POINT('Ctrl Pts',(-6.44715531200006,11.6,9.06387282399999));
#240324=CARTESIAN_POINT('Ctrl Pts',(-6.44991121200006,15.2,9.06565432299999));
#240325=CARTESIAN_POINT('Ctrl Pts',(-6.44991121200006,11.6,9.06565432299999));
#240326=CARTESIAN_POINT('Ctrl Pts',(-6.45267275100006,15.2,9.06743634299998));
#240327=CARTESIAN_POINT('Ctrl Pts',(-6.45267275100006,11.6,9.06743634299998));
#240328=CARTESIAN_POINT('Ctrl Pts',(-6.45543992300006,15.2,9.06921887599999));
#240329=CARTESIAN_POINT('Ctrl Pts',(-6.45543992300006,11.6,9.06921887599999));
#240330=CARTESIAN_POINT('Ctrl Pts',(-6.45821272400006,15.2,9.07100190799999));
#240331=CARTESIAN_POINT('Ctrl Pts',(-6.45821272400006,11.6,9.07100190799999));
#240332=CARTESIAN_POINT('Ctrl Pts',(-6.46099115300006,15.2,9.07278543099999));
#240333=CARTESIAN_POINT('Ctrl Pts',(-6.46099115300006,11.6,9.07278543099999));
#240334=CARTESIAN_POINT('Ctrl Pts',(-6.46377520500006,15.2,9.07456943399998));
#240335=CARTESIAN_POINT('Ctrl Pts',(-6.46377520500006,11.6,9.07456943399998));
#240336=CARTESIAN_POINT('Ctrl Pts',(-6.46656487700006,15.2,9.07635390799998));
#240337=CARTESIAN_POINT('Ctrl Pts',(-6.46656487700006,11.6,9.07635390799998));
#240338=CARTESIAN_POINT('Ctrl Pts',(-6.46936016400006,15.2,9.07813884199999));
#240339=CARTESIAN_POINT('Ctrl Pts',(-6.46936016400006,11.6,9.07813884199999));
#240340=CARTESIAN_POINT('Ctrl Pts',(-6.47216106400006,15.2,9.07992422599998));
#240341=CARTESIAN_POINT('Ctrl Pts',(-6.47216106400006,11.6,9.07992422599998));
#240342=CARTESIAN_POINT('Ctrl Pts',(-6.47496757400006,15.2,9.08171004999998));
#240343=CARTESIAN_POINT('Ctrl Pts',(-6.47496757400006,11.6,9.08171004999998));
#240344=CARTESIAN_POINT('Ctrl Pts',(-6.47777968900006,15.2,9.08349630299998));
#240345=CARTESIAN_POINT('Ctrl Pts',(-6.47777968900006,11.6,9.08349630299998));
#240346=CARTESIAN_POINT('Ctrl Pts',(-6.48059740600006,15.2,9.08528297699998));
#240347=CARTESIAN_POINT('Ctrl Pts',(-6.48059740600006,11.6,9.08528297699998));
#240348=CARTESIAN_POINT('Ctrl Pts',(-6.48342072100006,15.2,9.08707005899998));
#240349=CARTESIAN_POINT('Ctrl Pts',(-6.48342072100006,11.6,9.08707005899998));
#240350=CARTESIAN_POINT('Ctrl Pts',(-6.48624963200006,15.2,9.08885754199999));
#240351=CARTESIAN_POINT('Ctrl Pts',(-6.48624963200006,11.6,9.08885754199999));
#240352=CARTESIAN_POINT('Ctrl Pts',(-6.48908413600005,15.2,9.09064541299998));
#240353=CARTESIAN_POINT('Ctrl Pts',(-6.48908413600005,11.6,9.09064541299998));
#240354=CARTESIAN_POINT('Ctrl Pts',(-6.49192422700006,15.2,9.09243366499998));
#240355=CARTESIAN_POINT('Ctrl Pts',(-6.49192422700006,11.6,9.09243366499998));
#240356=CARTESIAN_POINT('Ctrl Pts',(-6.49476990200006,15.2,9.09422228699999));
#240357=CARTESIAN_POINT('Ctrl Pts',(-6.49476990200006,11.6,9.09422228699999));
#240358=CARTESIAN_POINT('Ctrl Pts',(-6.49762116000006,15.2,9.09601126699998));
#240359=CARTESIAN_POINT('Ctrl Pts',(-6.49762116000006,11.6,9.09601126699998));
#240360=CARTESIAN_POINT('Ctrl Pts',(-6.50047799400006,15.2,9.09780059799999));
#240361=CARTESIAN_POINT('Ctrl Pts',(-6.50047799400006,11.6,9.09780059799999));
#240362=CARTESIAN_POINT('Ctrl Pts',(-6.50334040400006,15.2,9.09959026799999));
#240363=CARTESIAN_POINT('Ctrl Pts',(-6.50334040400006,11.6,9.09959026799999));
#240364=CARTESIAN_POINT('Ctrl Pts',(-6.50620838300005,15.2,9.10138026899999));
#240365=CARTESIAN_POINT('Ctrl Pts',(-6.50620838300005,11.6,9.10138026899999));
#240366=CARTESIAN_POINT('Ctrl Pts',(-6.50908193000006,15.2,9.10317059099999));
#240367=CARTESIAN_POINT('Ctrl Pts',(-6.50908193000006,11.6,9.10317059099999));
#240368=CARTESIAN_POINT('Ctrl Pts',(-6.51196104100006,15.2,9.10496122099998));
#240369=CARTESIAN_POINT('Ctrl Pts',(-6.51196104100006,11.6,9.10496122099998));
#240370=CARTESIAN_POINT('Ctrl Pts',(-6.51484571200006,15.2,9.10675215299998));
#240371=CARTESIAN_POINT('Ctrl Pts',(-6.51484571200006,11.6,9.10675215299998));
#240372=CARTESIAN_POINT('Ctrl Pts',(-6.51773593900006,15.2,9.10854337499998));
#240373=CARTESIAN_POINT('Ctrl Pts',(-6.51773593900006,11.6,9.10854337499998));
#240374=CARTESIAN_POINT('Ctrl Pts',(-6.52063172100006,15.2,9.11033487799998));
#240375=CARTESIAN_POINT('Ctrl Pts',(-6.52063172100006,11.6,9.11033487799998));
#240376=CARTESIAN_POINT('Ctrl Pts',(-6.52353305100006,15.2,9.11212665299999));
#240377=CARTESIAN_POINT('Ctrl Pts',(-6.52353305100006,11.6,9.11212665299999));
#240378=CARTESIAN_POINT('Ctrl Pts',(-6.52643992800006,15.2,9.11391868799999));
#240379=CARTESIAN_POINT('Ctrl Pts',(-6.52643992800006,11.6,9.11391868799999));
#240380=CARTESIAN_POINT('Ctrl Pts',(-6.52935234800006,15.2,9.11571097599998));
#240381=CARTESIAN_POINT('Ctrl Pts',(-6.52935234800006,11.6,9.11571097599998));
#240382=CARTESIAN_POINT('Ctrl Pts',(-6.53227030700006,15.2,9.11750350599998));
#240383=CARTESIAN_POINT('Ctrl Pts',(-6.53227030700006,11.6,9.11750350599998));
#240384=CARTESIAN_POINT('Ctrl Pts',(-6.53519380100006,15.2,9.11929626799999));
#240385=CARTESIAN_POINT('Ctrl Pts',(-6.53519380100006,11.6,9.11929626799999));
#240386=CARTESIAN_POINT('Ctrl Pts',(-6.53812282700006,15.2,9.12108925299999));
#240387=CARTESIAN_POINT('Ctrl Pts',(-6.53812282700006,11.6,9.12108925299999));
#240388=CARTESIAN_POINT('Ctrl Pts',(-6.54105738300006,15.2,9.12288245099998));
#240389=CARTESIAN_POINT('Ctrl Pts',(-6.54105738300006,11.6,9.12288245099998));
#240390=CARTESIAN_POINT('Ctrl Pts',(-6.54399746300006,15.2,9.12467585299999));
#240391=CARTESIAN_POINT('Ctrl Pts',(-6.54399746300006,11.6,9.12467585299999));
#240392=CARTESIAN_POINT('Ctrl Pts',(-6.54694306500006,15.2,9.12646944899999));
#240393=CARTESIAN_POINT('Ctrl Pts',(-6.54694306500006,11.6,9.12646944899999));
#240394=CARTESIAN_POINT('Ctrl Pts',(-6.54989418600006,15.2,9.12826322899999));
#240395=CARTESIAN_POINT('Ctrl Pts',(-6.54989418600006,11.6,9.12826322899999));
#240396=CARTESIAN_POINT('Ctrl Pts',(-6.55285082000006,15.2,9.13005718499999));
#240397=CARTESIAN_POINT('Ctrl Pts',(-6.55285082000006,11.6,9.13005718499999));
#240398=CARTESIAN_POINT('Ctrl Pts',(-6.55581296600006,15.2,9.13185130499999));
#240399=CARTESIAN_POINT('Ctrl Pts',(-6.55581296600006,11.6,9.13185130499999));
#240400=CARTESIAN_POINT('Ctrl Pts',(-6.55878061900006,15.2,9.13364558199999));
#240401=CARTESIAN_POINT('Ctrl Pts',(-6.55878061900006,11.6,9.13364558199999));
#240402=CARTESIAN_POINT('Ctrl Pts',(-6.56175377600006,15.2,9.13544000499999));
#240403=CARTESIAN_POINT('Ctrl Pts',(-6.56175377600006,11.6,9.13544000499999));
#240404=CARTESIAN_POINT('Ctrl Pts',(-6.56473243500006,15.2,9.13723456399998));
#240405=CARTESIAN_POINT('Ctrl Pts',(-6.56473243500006,11.6,9.13723456399998));
#240406=CARTESIAN_POINT('Ctrl Pts',(-6.56771659000006,15.2,9.13902925199999));
#240407=CARTESIAN_POINT('Ctrl Pts',(-6.56771659000006,11.6,9.13902925199999));
#240408=CARTESIAN_POINT('Ctrl Pts',(-6.57070623700006,15.2,9.14082405799999));
#240409=CARTESIAN_POINT('Ctrl Pts',(-6.57070623700006,11.6,9.14082405799999));
#240410=CARTESIAN_POINT('Ctrl Pts',(-6.57370137600005,15.2,9.14261897199999));
#240411=CARTESIAN_POINT('Ctrl Pts',(-6.57370137600005,11.6,9.14261897199999));
#240412=CARTESIAN_POINT('Ctrl Pts',(-6.57670200100006,15.2,9.14441398599998));
#240413=CARTESIAN_POINT('Ctrl Pts',(-6.57670200100006,11.6,9.14441398599998));
#240414=CARTESIAN_POINT('Ctrl Pts',(-6.57970810800006,15.2,9.14620908999999));
#240415=CARTESIAN_POINT('Ctrl Pts',(-6.57970810800006,11.6,9.14620908999999));
#240416=CARTESIAN_POINT('Ctrl Pts',(-6.58271969500006,15.2,9.14800427499999));
#240417=CARTESIAN_POINT('Ctrl Pts',(-6.58271969500006,11.6,9.14800427499999));
#240418=CARTESIAN_POINT('Ctrl Pts',(-6.58573675800006,15.2,9.14979953099999));
#240419=CARTESIAN_POINT('Ctrl Pts',(-6.58573675800006,11.6,9.14979953099999));
#240420=CARTESIAN_POINT('Ctrl Pts',(-6.58875929300006,15.2,9.15159484899998));
#240421=CARTESIAN_POINT('Ctrl Pts',(-6.58875929300006,11.6,9.15159484899998));
#240422=CARTESIAN_POINT('Ctrl Pts',(-6.59178729700006,15.2,9.15339021899998));
#240423=CARTESIAN_POINT('Ctrl Pts',(-6.59178729700006,11.6,9.15339021899998));
#240424=CARTESIAN_POINT('Ctrl Pts',(-6.59482076700006,15.2,9.15518563399999));
#240425=CARTESIAN_POINT('Ctrl Pts',(-6.59482076700006,11.6,9.15518563399999));
#240426=CARTESIAN_POINT('Ctrl Pts',(-6.59785969700006,15.2,9.15698108299999));
#240427=CARTESIAN_POINT('Ctrl Pts',(-6.59785969700006,11.6,9.15698108299999));
#240428=CARTESIAN_POINT('Ctrl Pts',(-6.60090408600006,15.2,9.15877655699998));
#240429=CARTESIAN_POINT('Ctrl Pts',(-6.60090408600006,11.6,9.15877655699998));
#240430=CARTESIAN_POINT('Ctrl Pts',(-6.60395393000006,15.2,9.16057204699998));
#240431=CARTESIAN_POINT('Ctrl Pts',(-6.60395393000006,11.6,9.16057204699998));
#240432=CARTESIAN_POINT('Ctrl Pts',(-6.60700922500006,15.2,9.16236754499998));
#240433=CARTESIAN_POINT('Ctrl Pts',(-6.60700922500006,11.6,9.16236754499998));
#240434=CARTESIAN_POINT('Ctrl Pts',(-6.61006996700006,15.2,9.16416303799998));
#240435=CARTESIAN_POINT('Ctrl Pts',(-6.61006996700006,11.6,9.16416303799998));
#240436=CARTESIAN_POINT('Ctrl Pts',(-6.61313615300006,15.2,9.16595852199999));
#240437=CARTESIAN_POINT('Ctrl Pts',(-6.61313615300006,11.6,9.16595852199999));
#240438=CARTESIAN_POINT('Ctrl Pts',(-6.61620778000006,15.2,9.16775398399999));
#240439=CARTESIAN_POINT('Ctrl Pts',(-6.61620778000006,11.6,9.16775398399999));
#240440=CARTESIAN_POINT('Ctrl Pts',(-6.61928484300006,15.2,9.16954941699998));
#240441=CARTESIAN_POINT('Ctrl Pts',(-6.61928484300006,11.6,9.16954941699998));
#240442=CARTESIAN_POINT('Ctrl Pts',(-6.62236734000006,15.2,9.17134481099998));
#240443=CARTESIAN_POINT('Ctrl Pts',(-6.62236734000006,11.6,9.17134481099998));
#240444=CARTESIAN_POINT('Ctrl Pts',(-6.62545526800006,15.2,9.17314015699999));
#240445=CARTESIAN_POINT('Ctrl Pts',(-6.62545526800006,11.6,9.17314015699999));
#240446=CARTESIAN_POINT('Ctrl Pts',(-6.62854862100006,15.2,9.17493544599999));
#240447=CARTESIAN_POINT('Ctrl Pts',(-6.62854862100006,11.6,9.17493544599999));
#240448=CARTESIAN_POINT('Ctrl Pts',(-6.63164739700006,15.2,9.17673066999999));
#240449=CARTESIAN_POINT('Ctrl Pts',(-6.63164739700006,11.6,9.17673066999999));
#240450=CARTESIAN_POINT('Ctrl Pts',(-6.63475159200006,15.2,9.17852581799998));
#240451=CARTESIAN_POINT('Ctrl Pts',(-6.63475159200006,11.6,9.17852581799998));
#240452=CARTESIAN_POINT('Ctrl Pts',(-6.63786120400006,15.2,9.18032088299999));
#240453=CARTESIAN_POINT('Ctrl Pts',(-6.63786120400006,11.6,9.18032088299999));
#240454=CARTESIAN_POINT('Ctrl Pts',(-6.64097622600006,15.2,9.18211585499999));
#240455=CARTESIAN_POINT('Ctrl Pts',(-6.64097622600006,11.6,9.18211585499999));
#240456=CARTESIAN_POINT('Ctrl Pts',(-6.64409665800005,15.2,9.18391072499999));
#240457=CARTESIAN_POINT('Ctrl Pts',(-6.64409665800005,11.6,9.18391072499999));
#240458=CARTESIAN_POINT('Ctrl Pts',(-6.64722249500006,15.2,9.18570548399998));
#240459=CARTESIAN_POINT('Ctrl Pts',(-6.64722249500006,11.6,9.18570548399998));
#240460=CARTESIAN_POINT('Ctrl Pts',(-6.65035373400006,15.2,9.18750012399999));
#240461=CARTESIAN_POINT('Ctrl Pts',(-6.65035373400006,11.6,9.18750012399999));
#240462=CARTESIAN_POINT('Ctrl Pts',(-6.65349037000006,15.2,9.18929463599999));
#240463=CARTESIAN_POINT('Ctrl Pts',(-6.65349037000006,11.6,9.18929463599999));
#240464=CARTESIAN_POINT('Ctrl Pts',(-6.65663240100006,15.2,9.19108900999999));
#240465=CARTESIAN_POINT('Ctrl Pts',(-6.65663240100006,11.6,9.19108900999999));
#240466=CARTESIAN_POINT('Ctrl Pts',(-6.65977982200006,15.2,9.19288323799999));
#240467=CARTESIAN_POINT('Ctrl Pts',(-6.65977982200006,11.6,9.19288323799999));
#240468=CARTESIAN_POINT('Ctrl Pts',(-6.66293263000005,15.2,9.19467731099999));
#240469=CARTESIAN_POINT('Ctrl Pts',(-6.66293263000005,11.6,9.19467731099999));
#240470=CARTESIAN_POINT('Ctrl Pts',(-6.66609082400006,15.2,9.19647121999999));
#240471=CARTESIAN_POINT('Ctrl Pts',(-6.66609082400006,11.6,9.19647121999999));
#240472=CARTESIAN_POINT('Ctrl Pts',(-6.66925439600006,15.2,9.19826495599998));
#240473=CARTESIAN_POINT('Ctrl Pts',(-6.66925439600006,11.6,9.19826495599998));
#240474=CARTESIAN_POINT('Ctrl Pts',(-6.67242334600005,15.2,9.20005851099998));
#240475=CARTESIAN_POINT('Ctrl Pts',(-6.67242334600005,11.6,9.20005851099998));
#240476=CARTESIAN_POINT('Ctrl Pts',(-6.67559766800006,15.2,9.20185187599999));
#240477=CARTESIAN_POINT('Ctrl Pts',(-6.67559766800006,11.6,9.20185187599999));
#240478=CARTESIAN_POINT('Ctrl Pts',(-6.67877735900006,15.2,9.20364504199998));
#240479=CARTESIAN_POINT('Ctrl Pts',(-6.67877735900006,11.6,9.20364504199998));
#240480=CARTESIAN_POINT('Ctrl Pts',(-6.68196241700006,15.2,9.20543799999999));
#240481=CARTESIAN_POINT('Ctrl Pts',(-6.68196241700006,11.6,9.20543799999999));
#240482=CARTESIAN_POINT('Ctrl Pts',(-6.68515283700006,15.2,9.20723074199999));
#240483=CARTESIAN_POINT('Ctrl Pts',(-6.68515283700006,11.6,9.20723074199999));
#240484=CARTESIAN_POINT('Ctrl Pts',(-6.68834861700006,15.2,9.20902325999998));
#240485=CARTESIAN_POINT('Ctrl Pts',(-6.68834861700006,11.6,9.20902325999998));
#240486=CARTESIAN_POINT('Ctrl Pts',(-6.69154975100006,15.2,9.21081554299998));
#240487=CARTESIAN_POINT('Ctrl Pts',(-6.69154975100006,11.6,9.21081554299998));
#240488=CARTESIAN_POINT('Ctrl Pts',(-6.69475623700006,15.2,9.21260758499999));
#240489=CARTESIAN_POINT('Ctrl Pts',(-6.69475623700006,11.6,9.21260758499999));
#240490=CARTESIAN_POINT('Ctrl Pts',(-6.69796807000006,15.2,9.21439937499999));
#240491=CARTESIAN_POINT('Ctrl Pts',(-6.69796807000006,11.6,9.21439937499999));
#240492=CARTESIAN_POINT('Ctrl Pts',(-6.70118525000006,15.2,9.21619090599999));
#240493=CARTESIAN_POINT('Ctrl Pts',(-6.70118525000006,11.6,9.21619090599999));
#240494=CARTESIAN_POINT('Ctrl Pts',(-6.70440776900006,15.2,9.21798216799999));
#240495=CARTESIAN_POINT('Ctrl Pts',(-6.70440776900006,11.6,9.21798216799999));
#240496=CARTESIAN_POINT('Ctrl Pts',(-6.70763562600006,15.2,9.21977315299999));
#240497=CARTESIAN_POINT('Ctrl Pts',(-6.70763562600006,11.6,9.21977315299999));
#240498=CARTESIAN_POINT('Ctrl Pts',(-6.71086881600006,15.2,9.22156385299999));
#240499=CARTESIAN_POINT('Ctrl Pts',(-6.71086881600006,11.6,9.22156385299999));
#240500=CARTESIAN_POINT('Ctrl Pts',(-6.71410733700006,15.2,9.22335425999999));
#240501=CARTESIAN_POINT('Ctrl Pts',(-6.71410733700006,11.6,9.22335425999999));
#240502=CARTESIAN_POINT('Ctrl Pts',(-6.71735118500006,15.2,9.22514436399998));
#240503=CARTESIAN_POINT('Ctrl Pts',(-6.71735118500006,11.6,9.22514436399998));
#240504=CARTESIAN_POINT('Ctrl Pts',(-6.72060035600006,15.2,9.22693415799999));
#240505=CARTESIAN_POINT('Ctrl Pts',(-6.72060035600006,11.6,9.22693415799999));
#240506=CARTESIAN_POINT('Ctrl Pts',(-6.72385484600006,15.2,9.22872363199998));
#240507=CARTESIAN_POINT('Ctrl Pts',(-6.72385484600006,11.6,9.22872363199998));
#240508=CARTESIAN_POINT('Ctrl Pts',(-6.72711465300006,15.2,9.23051277999999));
#240509=CARTESIAN_POINT('Ctrl Pts',(-6.72711465300006,11.6,9.23051277999999));
#240510=CARTESIAN_POINT('Ctrl Pts',(-6.73037977400006,15.2,9.23230159099998));
#240511=CARTESIAN_POINT('Ctrl Pts',(-6.73037977400006,11.6,9.23230159099998));
#240512=CARTESIAN_POINT('Ctrl Pts',(-6.73365020100006,15.2,9.23409005699998));
#240513=CARTESIAN_POINT('Ctrl Pts',(-6.73365020100006,11.6,9.23409005699998));
#240514=CARTESIAN_POINT('Ctrl Pts',(-6.73692593500006,15.2,9.23587816999999));
#240515=CARTESIAN_POINT('Ctrl Pts',(-6.73692593500006,11.6,9.23587816999999));
#240516=CARTESIAN_POINT('Ctrl Pts',(-6.74020697000006,15.2,9.23766591999998));
#240517=CARTESIAN_POINT('Ctrl Pts',(-6.74020697000006,11.6,9.23766591999998));
#240518=CARTESIAN_POINT('Ctrl Pts',(-6.74349330200006,15.2,9.23945329999999));
#240519=CARTESIAN_POINT('Ctrl Pts',(-6.74349330200006,11.6,9.23945329999999));
#240520=CARTESIAN_POINT('Ctrl Pts',(-6.74678492800005,15.2,9.24124030099998));
#240521=CARTESIAN_POINT('Ctrl Pts',(-6.74678492800005,11.6,9.24124030099998));
#240522=CARTESIAN_POINT('Ctrl Pts',(-6.75008184500006,15.2,9.24302691299999));
#240523=CARTESIAN_POINT('Ctrl Pts',(-6.75008184500006,11.6,9.24302691299999));
#240524=CARTESIAN_POINT('Ctrl Pts',(-6.75338405000006,15.2,9.24481313199998));
#240525=CARTESIAN_POINT('Ctrl Pts',(-6.75338405000006,11.6,9.24481313199998));
#240526=CARTESIAN_POINT('Ctrl Pts',(-6.75669154000006,15.2,9.24659894899998));
#240527=CARTESIAN_POINT('Ctrl Pts',(-6.75669154000006,11.6,9.24659894899998));
#240528=CARTESIAN_POINT('Ctrl Pts',(-6.76000431000006,15.2,9.24838435599998));
#240529=CARTESIAN_POINT('Ctrl Pts',(-6.76000431000006,11.6,9.24838435599998));
#240530=CARTESIAN_POINT('Ctrl Pts',(-6.76332235800006,15.2,9.25016934499999));
#240531=CARTESIAN_POINT('Ctrl Pts',(-6.76332235800006,11.6,9.25016934499999));
#240532=CARTESIAN_POINT('Ctrl Pts',(-6.76664568000006,15.2,9.25195390799999));
#240533=CARTESIAN_POINT('Ctrl Pts',(-6.76664568000006,11.6,9.25195390799999));
#240534=CARTESIAN_POINT('Ctrl Pts',(-6.76997427200006,15.2,9.25373803599999));
#240535=CARTESIAN_POINT('Ctrl Pts',(-6.76997427200006,11.6,9.25373803599999));
#240536=CARTESIAN_POINT('Ctrl Pts',(-6.77330812800006,15.2,9.25552171799998));
#240537=CARTESIAN_POINT('Ctrl Pts',(-6.77330812800006,11.6,9.25552171799998));
#240538=CARTESIAN_POINT('Ctrl Pts',(-6.77664724700006,15.2,9.25730494399998));
#240539=CARTESIAN_POINT('Ctrl Pts',(-6.77664724700006,11.6,9.25730494399998));
#240540=CARTESIAN_POINT('Ctrl Pts',(-6.77999162100006,15.2,9.25908770299999));
#240541=CARTESIAN_POINT('Ctrl Pts',(-6.77999162100006,11.6,9.25908770299999));
#240542=CARTESIAN_POINT('Ctrl Pts',(-6.78334124800006,15.2,9.26086998699999));
#240543=CARTESIAN_POINT('Ctrl Pts',(-6.78334124800006,11.6,9.26086998699999));
#240544=CARTESIAN_POINT('Ctrl Pts',(-6.78669612400006,15.2,9.26265178799999));
#240545=CARTESIAN_POINT('Ctrl Pts',(-6.78669612400006,11.6,9.26265178799999));
#240546=CARTESIAN_POINT('Ctrl Pts',(-6.79005624900006,15.2,9.26443310199998));
#240547=CARTESIAN_POINT('Ctrl Pts',(-6.79005624900006,11.6,9.26443310199998));
#240548=CARTESIAN_POINT('Ctrl Pts',(-6.79342161700006,15.2,9.26621392399999));
#240549=CARTESIAN_POINT('Ctrl Pts',(-6.79342161700006,11.6,9.26621392399999));
#240550=CARTESIAN_POINT('Ctrl Pts',(-6.79679223000006,15.2,9.26799425399999));
#240551=CARTESIAN_POINT('Ctrl Pts',(-6.79679223000006,11.6,9.26799425399999));
#240552=CARTESIAN_POINT('Ctrl Pts',(-6.79949291500006,15.2,9.26941812099999));
#240553=CARTESIAN_POINT('Ctrl Pts',(-6.79949291500006,11.6,9.26941812099999));
#240554=CARTESIAN_POINT('Ctrl Pts',(-6.80152078900006,15.2,9.27048579799998));
#240555=CARTESIAN_POINT('Ctrl Pts',(-6.80152078900006,11.6,9.27048579799998));
#240556=CARTESIAN_POINT('Ctrl Pts',(-6.80287375200006,15.2,9.27119748399999));
#240557=CARTESIAN_POINT('Ctrl Pts',(-6.80287375200006,11.6,9.27119748399999));
#240558=CARTESIAN_POINT('Ctrl Pts',(-6.80355049700006,15.2,9.27155330199999));
#240559=CARTESIAN_POINT('Ctrl Pts',(-6.80355049700006,11.6,9.27155330199999));
#240560=CARTESIAN_POINT('Ctrl Pts',(-5.85257411500006,15.2,8.56667970999998));
#240561=CARTESIAN_POINT('Ctrl Pts',(-5.8537050266944,15.2,8.56806288496946));
#240562=CARTESIAN_POINT('Ctrl Pts',(-5.8548762742267,15.2,8.5694869238734));
#240563=CARTESIAN_POINT('Ctrl Pts',(-5.85608775334231,15.2,8.57095065186461));
#240564=CARTESIAN_POINT('Ctrl Pts',(-5.85730507482257,15.2,8.57242143869206));
#240565=CARTESIAN_POINT('Ctrl Pts',(-5.85856301277102,15.2,8.57393230486909));
#240566=CARTESIAN_POINT('Ctrl Pts',(-5.85986145340903,15.2,8.5754821088666));
#240567=CARTESIAN_POINT('Ctrl Pts',(-5.86115989392909,15.2,8.57703191272334));
#240568=CARTESIAN_POINT('Ctrl Pts',(-5.86249883775011,15.2,8.5786206548507));
#240569=CARTESIAN_POINT('Ctrl Pts',(-5.86387817019999,15.2,8.58024722870826));
#240570=CARTESIAN_POINT('Ctrl Pts',(-5.86525750264987,15.2,8.58187380256584));
#240571=CARTESIAN_POINT('Ctrl Pts',(-5.86667722397461,15.2,8.58353820930605));
#240572=CARTESIAN_POINT('Ctrl Pts',(-5.86813722065885,15.2,8.58523937157711));
#240573=CARTESIAN_POINT('Ctrl Pts',(-5.86959721747571,15.2,8.58694053400272));
#240574=CARTESIAN_POINT('Ctrl Pts',(-5.87109749092289,15.2,8.58867845508586));
#240575=CARTESIAN_POINT('Ctrl Pts',(-5.87263792542624,15.2,8.59045208743492));
#240576=CARTESIAN_POINT('Ctrl Pts',(-5.87417835978964,15.2,8.5922257196229));
#240577=CARTESIAN_POINT('Ctrl Pts',(-5.87575895551881,15.2,8.59403506540096));
#240578=CARTESIAN_POINT('Ctrl Pts',(-5.87737960096739,15.2,8.5958791057591));
#240579=CARTESIAN_POINT('Ctrl Pts',(-5.87927035408887,15.2,8.59803048628858));
#240580=CARTESIAN_POINT('Ctrl Pts',(-5.88121561762475,15.2,8.6002290925998));
#240581=CARTESIAN_POINT('Ctrl Pts',(-5.88321521364515,15.2,8.60247335719295));
#240582=CARTESIAN_POINT('Ctrl Pts',(-5.88492915300225,15.2,8.60439701245866));
#240583=CARTESIAN_POINT('Ctrl Pts',(-5.88668300813275,15.2,8.60635421247237));
#240584=CARTESIAN_POINT('Ctrl Pts',(-5.88847666749247,15.2,8.6083439999925));
#240585=CARTESIAN_POINT('Ctrl Pts',(-5.8902703268522,15.2,8.61033378751263));
#240586=CARTESIAN_POINT('Ctrl Pts',(-5.89210378938454,15.2,8.61235616293915));
#240587=CARTESIAN_POINT('Ctrl Pts',(-5.89397694364806,15.2,8.61441019244645));
#240588=CARTESIAN_POINT('Ctrl Pts',(-5.89585009808173,15.2,8.61646422214033));
#240589=CARTESIAN_POINT('Ctrl Pts',(-5.89776294240371,15.2,8.61854990460485));
#240590=CARTESIAN_POINT('Ctrl Pts',(-5.89971536501281,15.2,8.6206663334723));
#240591=CARTESIAN_POINT('Ctrl Pts',(-5.90166778744456,15.2,8.6227827621475));
#240592=CARTESIAN_POINT('Ctrl Pts',(-5.90365978830796,15.2,8.62492993613816));
#240593=CARTESIAN_POINT('Ctrl Pts',(-5.9056912528192,15.2,8.6271069661437));
#240594=CARTESIAN_POINT('Ctrl Pts',(-5.90772271733044,15.2,8.62928399614923));
#240595=CARTESIAN_POINT('Ctrl Pts',(-5.90979364614689,15.2,8.63149088590239));
#240596=CARTESIAN_POINT('Ctrl Pts',(-5.91190392740181,15.2,8.6337267679032));
#240597=CARTESIAN_POINT('Ctrl Pts',(-5.91401420865675,15.2,8.63596264990402));
#240598=CARTESIAN_POINT('Ctrl Pts',(-5.91616383903528,15.2,8.63822752557691));
#240599=CARTESIAN_POINT('Ctrl Pts',(-5.91835271020307,15.2,8.64052054974167));
#240600=CARTESIAN_POINT('Ctrl Pts',(-5.92054158156969,15.2,8.64281357411472));
#240601=CARTESIAN_POINT('Ctrl Pts',(-5.92276968905676,15.2,8.64513474665718));
#240602=CARTESIAN_POINT('Ctrl Pts',(-5.92503692259871,15.2,8.64748324586971));
#240603=CARTESIAN_POINT('Ctrl Pts',(-5.92730415593471,15.2,8.64983174486891));
#240604=CARTESIAN_POINT('Ctrl Pts',(-5.92961051367591,15.2,8.65220756702423));
#240605=CARTESIAN_POINT('Ctrl Pts',(-5.93195588292233,15.2,8.65460991210245));
#240606=CARTESIAN_POINT('Ctrl Pts',(-5.93430125216874,15.2,8.65701225718068));
#240607=CARTESIAN_POINT('Ctrl Pts',(-5.93668563130987,15.2,8.65944112073997));
#240608=CARTESIAN_POINT('Ctrl Pts',(-5.93910890871919,15.2,8.6618957199824));
#240609=CARTESIAN_POINT('Ctrl Pts',(-5.94153218634864,15.2,8.66435031944778));
#240610=CARTESIAN_POINT('Ctrl Pts',(-5.94399436180682,15.2,8.66683065198232));
#240611=CARTESIAN_POINT('Ctrl Pts',(-5.94649532036145,15.2,8.66933595061991));
#240612=CARTESIAN_POINT('Ctrl Pts',(-5.94899627868892,15.2,8.67184124902994));
#240613=CARTESIAN_POINT('Ctrl Pts',(-5.9515360211392,15.2,8.67437151465504));
#240614=CARTESIAN_POINT('Ctrl Pts',(-5.95411443247382,15.2,8.67692599499046));
#240615=CARTESIAN_POINT('Ctrl Pts',(-5.95669284380845,15.2,8.67948047532588));
#240616=CARTESIAN_POINT('Ctrl Pts',(-5.95930992571798,15.2,8.68205916772079));
#240617=CARTESIAN_POINT('Ctrl Pts',(-5.9619655612022,15.2,8.68466134220798));
#240618=CARTESIAN_POINT('Ctrl Pts',(-5.96462119692765,15.2,8.68726351693154));
#240619=CARTESIAN_POINT('Ctrl Pts',(-5.96731538830176,15.2,8.68988917133658));
#240620=CARTESIAN_POINT('Ctrl Pts',(-5.9700480210061,15.2,8.6925375855312));
#240621=CARTESIAN_POINT('Ctrl Pts',(-5.97323609212215,15.2,8.69562740173075));
#240622=CARTESIAN_POINT('Ctrl Pts',(-5.97647648353938,15.2,8.69874819882578));
#240623=CARTESIAN_POINT('Ctrl Pts',(-5.97976901548404,15.2,8.70189885973892));
#240624=CARTESIAN_POINT('Ctrl Pts',(-5.98259118605191,15.2,8.70459942655127));
#240625=CARTESIAN_POINT('Ctrl Pts',(-5.98545166310051,15.2,8.70732193373593));
#240626=CARTESIAN_POINT('Ctrl Pts',(-5.98835033198882,15.2,8.71006569677376));
#240627=CARTESIAN_POINT('Ctrl Pts',(-5.99076588926411,15.2,8.71235216584733));
#240628=CARTESIAN_POINT('Ctrl Pts',(-5.99320796928185,15.2,8.71465339406278));
#240629=CARTESIAN_POINT('Ctrl Pts',(-5.99567650379788,15.2,8.7169689939945));
#240630=CARTESIAN_POINT('Ctrl Pts',(-5.99863874510948,15.2,8.71974771381159));
#240631=CARTESIAN_POINT('Ctrl Pts',(-6.00163908157287,15.2,8.72254712691582));
#240632=CARTESIAN_POINT('Ctrl Pts',(-6.00467739972638,15.2,8.7253665727429));
#240633=CARTESIAN_POINT('Ctrl Pts',(-6.00720933161296,15.2,8.72771611101751));
#240634=CARTESIAN_POINT('Ctrl Pts',(-6.00976763708449,15.2,8.73007955979923));
#240635=CARTESIAN_POINT('Ctrl Pts',(-6.01235225166918,15.2,8.73245654639715));
#240636=CARTESIAN_POINT('Ctrl Pts',(-6.01493686625387,15.2,8.73483353299506));
#240637=CARTESIAN_POINT('Ctrl Pts',(-6.0175477886768,15.2,8.73722405546766));
#240638=CARTESIAN_POINT('Ctrl Pts',(-6.02018495166428,15.2,8.73962774394056));
#240639=CARTESIAN_POINT('Ctrl Pts',(-6.02282211465175,15.2,8.74203143241346));
#240640=CARTESIAN_POINT('Ctrl Pts',(-6.02548552030945,15.2,8.74444828894865));
#240641=CARTESIAN_POINT('Ctrl Pts',(-6.02817509836231,15.2,8.74687794830705));
#240642=CARTESIAN_POINT('Ctrl Pts',(-6.03086467641516,15.2,8.74930760766543));
#240643=CARTESIAN_POINT('Ctrl Pts',(-6.03358042886206,15.2,8.75175007007004));
#240644=CARTESIAN_POINT('Ctrl Pts',(-6.03632228685029,15.2,8.75420498007106));
#240645=CARTESIAN_POINT('Ctrl Pts',(-6.03906414483854,15.2,8.75665989007207));
#240646=CARTESIAN_POINT('Ctrl Pts',(-6.04183210986332,15.2,8.7591272449066));
#240647=CARTESIAN_POINT('Ctrl Pts',(-6.04462611361546,15.2,8.76160669428261));
#240648=CARTESIAN_POINT('Ctrl Pts',(-6.04742011706305,15.2,8.76408614338834));
#240649=CARTESIAN_POINT('Ctrl Pts',(-6.05024015951785,15.2,8.76657768876854));
#240650=CARTESIAN_POINT('Ctrl Pts',(-6.05308617288608,15.2,8.7690809804392));
#240651=CARTESIAN_POINT('Ctrl Pts',(-6.05593218656454,15.2,8.77158427238271));
#240652=CARTESIAN_POINT('Ctrl Pts',(-6.05880417311198,15.2,8.7740993139149));
#240653=CARTESIAN_POINT('Ctrl Pts',(-6.06170206109596,15.2,8.77662576238617));
#240654=CARTESIAN_POINT('Ctrl Pts',(-6.06459994907992,15.2,8.77915221085743));
#240655=CARTESIAN_POINT('Ctrl Pts',(-6.067523741601,15.2,8.78169006623308));
#240656=CARTESIAN_POINT('Ctrl Pts',(-6.07047336889934,15.2,8.78423899497077));
#240657=CARTESIAN_POINT('Ctrl Pts',(-6.07342299619768,15.2,8.78678792370845));
#240658=CARTESIAN_POINT('Ctrl Pts',(-6.07639846060521,15.2,8.78934792409357));
#240659=CARTESIAN_POINT('Ctrl Pts',(-6.07939969102053,15.2,8.7919186661069));
#240660=CARTESIAN_POINT('Ctrl Pts',(-6.08240092143587,15.2,8.79448940812023));
#240661=CARTESIAN_POINT('Ctrl Pts',(-6.08542792042408,15.2,8.79707089179773));
#240662=CARTESIAN_POINT('Ctrl Pts',(-6.0884806175755,15.2,8.79966279138051));
#240663=CARTESIAN_POINT('Ctrl Pts',(-6.09153331472692,15.2,8.80225469096329));
#240664=CARTESIAN_POINT('Ctrl Pts',(-6.09461171143183,15.2,8.80485700749638));
#240665=CARTESIAN_POINT('Ctrl Pts',(-6.09771573934714,15.2,8.80746941957917));
#240666=CARTESIAN_POINT('Ctrl Pts',(-6.10081976726246,15.2,8.81008183166197));
#240667=CARTESIAN_POINT('Ctrl Pts',(-6.10394942578958,15.2,8.81270433960326));
#240668=CARTESIAN_POINT('Ctrl Pts',(-6.10710464774828,15.2,8.81533662753186));
#240669=CARTESIAN_POINT('Ctrl Pts',(-6.11025986970697,15.2,8.81796891546045));
#240670=CARTESIAN_POINT('Ctrl Pts',(-6.11344065219998,15.2,8.82061098314996));
#240671=CARTESIAN_POINT('Ctrl Pts',(-6.11664693074166,15.2,8.8232625202333));
#240672=CARTESIAN_POINT('Ctrl Pts',(-6.11921195371481,15.2,8.82538375001559));
#240673=CARTESIAN_POINT('Ctrl Pts',(-6.12179329104539,15.2,8.82751103911801));
#240674=CARTESIAN_POINT('Ctrl Pts',(-6.12439091013305,15.2,8.82964423162374));
#240675=CARTESIAN_POINT('Ctrl Pts',(-6.1282873384106,15.2,8.83284402009169));
#240676=CARTESIAN_POINT('Ctrl Pts',(-6.13222039943412,15.2,8.83605709057581));
#240677=CARTESIAN_POINT('Ctrl Pts',(-6.13618997270815,15.2,8.83928291812583));
#240678=CARTESIAN_POINT('Ctrl Pts',(-6.13883635477065,15.2,8.84143346972817));
#240679=CARTESIAN_POINT('Ctrl Pts',(-6.14149896556602,15.2,8.84358969119049));
#240680=CARTESIAN_POINT('Ctrl Pts',(-6.14417776834535,15.2,8.84575143134652));
#240681=CARTESIAN_POINT('Ctrl Pts',(-6.14685657148967,15.2,8.84791317179709));
#240682=CARTESIAN_POINT('Ctrl Pts',(-6.14955156687227,15.2,8.85008043000093));
#240683=CARTESIAN_POINT('Ctrl Pts',(-6.15226271997685,15.2,8.85225305401811));
#240684=CARTESIAN_POINT('Ctrl Pts',(-6.15497387271203,15.2,8.85442567773928));
#240685=CARTESIAN_POINT('Ctrl Pts',(-6.15770118282183,15.2,8.8566036690137));
#240686=CARTESIAN_POINT('Ctrl Pts',(-6.16044461481811,15.2,8.85878687666801));
#240687=CARTESIAN_POINT('Ctrl Pts',(-6.16318804718819,15.2,8.86097008461978));
#240688=CARTESIAN_POINT('Ctrl Pts',(-6.16594759985984,15.2,8.86315851003598));
#240689=CARTESIAN_POINT('Ctrl Pts',(-6.16872324023332,15.2,8.86535200526663));
#240690=CARTESIAN_POINT('Ctrl Pts',(-6.1714988806068,15.2,8.86754550049727));
#240691=CARTESIAN_POINT('Ctrl Pts',(-6.17429060765719,15.2,8.86974406536465));
#240692=CARTESIAN_POINT('Ctrl Pts',(-6.17709838420074,15.2,8.87194755331857));
#240693=CARTESIAN_POINT('Ctrl Pts',(-6.17990616036172,15.2,8.87415104097227));
#240694=CARTESIAN_POINT('Ctrl Pts',(-6.18272998704516,15.2,8.87635945217491));
#240695=CARTESIAN_POINT('Ctrl Pts',(-6.18556982971473,15.2,8.87857264244846));
#240696=CARTESIAN_POINT('Ctrl Pts',(-6.18840967277123,15.2,8.88078583302355));
#240697=CARTESIAN_POINT('Ctrl Pts',(-6.19126553131142,15.2,8.88300380253621));
#240698=CARTESIAN_POINT('Ctrl Pts',(-6.19413736846955,15.2,8.88522640788004));
#240699=CARTESIAN_POINT('Ctrl Pts',(-6.1970092052364,15.2,8.88744901292103));
#240700=CARTESIAN_POINT('Ctrl Pts',(-6.19989702052897,15.2,8.88967625531975));
#240701=CARTESIAN_POINT('Ctrl Pts',(-6.20280078051276,15.2,8.8919079905259));
#240702=CARTESIAN_POINT('Ctrl Pts',(-6.20570454089219,15.2,8.89413972603612));
#240703=CARTESIAN_POINT('Ctrl Pts',(-6.2086242440458,15.2,8.89637595751569));
#240704=CARTESIAN_POINT('Ctrl Pts',(-6.21155985590939,15.2,8.89861654358345));
#240705=CARTESIAN_POINT('Ctrl Pts',(-6.21449546737302,15.2,8.90085712934594));
#240706=CARTESIAN_POINT('Ctrl Pts',(-6.21744698676785,15.2,8.90310206926141));
#240707=CARTESIAN_POINT('Ctrl Pts',(-6.22041437752423,15.2,8.90535122629947));
#240708=CARTESIAN_POINT('Ctrl Pts',(-6.2233817686849,15.2,8.90760038364398));
#240709=CARTESIAN_POINT('Ctrl Pts',(-6.22636503181418,15.2,8.90985375738626));
#240710=CARTESIAN_POINT('Ctrl Pts',(-6.22936413097865,15.2,8.91211121067622));
#240711=CARTESIAN_POINT('Ctrl Pts',(-6.23236322973449,15.2,8.9143686636586));
#240712=CARTESIAN_POINT('Ctrl Pts',(-6.23537816486081,15.2,8.91663019459918));
#240713=CARTESIAN_POINT('Ctrl Pts',(-6.23840889981864,15.2,8.91889567163792));
#240714=CARTESIAN_POINT('Ctrl Pts',(-6.2414396351894,15.2,8.92116114898534));
#240715=CARTESIAN_POINT('Ctrl Pts',(-6.24448617107701,15.2,8.92343056941171));
#240716=CARTESIAN_POINT('Ctrl Pts',(-6.24754847080049,15.2,8.92570380020251));
#240717=CARTESIAN_POINT('Ctrl Pts',(-6.25061077010671,15.2,8.92797703068358));
#240718=CARTESIAN_POINT('Ctrl Pts',(-6.25368883269314,15.2,8.93025407062779));
#240719=CARTESIAN_POINT('Ctrl Pts',(-6.25678262399416,15.2,8.93253478838541));
#240720=CARTESIAN_POINT('Ctrl Pts',(-6.25987641571672,15.2,8.93481550645377));
#240721=CARTESIAN_POINT('Ctrl Pts',(-6.26298593538979,15.2,8.93709990191645));
#240722=CARTESIAN_POINT('Ctrl Pts',(-6.2661111460188,15.2,8.9393878427182));
#240723=CARTESIAN_POINT('Ctrl Pts',(-6.26923635622199,15.2,8.94167578320821));
#240724=CARTESIAN_POINT('Ctrl Pts',(-6.27237725994355,15.2,8.94396727034327));
#240725=CARTESIAN_POINT('Ctrl Pts',(-6.27553381801724,15.2,8.94626217343309));
#240726=CARTESIAN_POINT('Ctrl Pts',(-6.278690376521,15.2,8.94855707683559));
#240727=CARTESIAN_POINT('Ctrl Pts',(-6.28186259152071,15.2,8.95085539533565));
#240728=CARTESIAN_POINT('Ctrl Pts',(-6.28505042524999,15.2,8.95315700201664));
#240729=CARTESIAN_POINT('Ctrl Pts',(-6.28903521719443,15.2,8.95603401021108));
#240730=CARTESIAN_POINT('Ctrl Pts',(-6.29304441381157,15.2,8.9589161537884));
#240731=CARTESIAN_POINT('Ctrl Pts',(-6.29707794501053,15.2,8.96180318546822));
#240732=CARTESIAN_POINT('Ctrl Pts',(-6.30030476970591,15.2,8.96411281062326));
#240733=CARTESIAN_POINT('Ctrl Pts',(-6.30354716929914,15.2,8.96642556458597));
#240734=CARTESIAN_POINT('Ctrl Pts',(-6.30680510597566,15.2,8.96874131989635));
#240735=CARTESIAN_POINT('Ctrl Pts',(-6.31169201165627,15.2,8.9722149533352));
#240736=CARTESIAN_POINT('Ctrl Pts',(-6.31661387607365,15.2,8.97569534314141));
#240737=CARTESIAN_POINT('Ctrl Pts',(-6.32157057776195,15.2,8.97918206841503));
#240738=CARTESIAN_POINT('Ctrl Pts',(-6.32652727900002,15.2,8.98266879337194));
#240739=CARTESIAN_POINT('Ctrl Pts',(-6.33151881653533,15.2,8.98616185404502));
#240740=CARTESIAN_POINT('Ctrl Pts',(-6.33654506776788,15.2,8.98966083700097));
#240741=CARTESIAN_POINT('Ctrl Pts',(-6.33989590222727,15.2,8.99199349251682));
#240742=CARTESIAN_POINT('Ctrl Pts',(-6.34326216468622,15.2,8.99432878125592));
#240743=CARTESIAN_POINT('Ctrl Pts',(-6.34664381870745,15.2,8.99666658038923));
#240744=CARTESIAN_POINT('Ctrl Pts',(-6.35002547226794,15.2,8.999004379204));
#240745=CARTESIAN_POINT('Ctrl Pts',(-6.35342251877061,15.2,9.00134469013906));
#240746=CARTESIAN_POINT('Ctrl Pts',(-6.35683491821284,15.2,9.00368739205848));
#240747=CARTESIAN_POINT('Ctrl Pts',(-6.36024731812,15.2,9.00603009429709));
#240748=CARTESIAN_POINT('Ctrl Pts',(-6.36367507370687,15.2,9.00837518923883));
#240749=CARTESIAN_POINT('Ctrl Pts',(-6.36711814750661,15.2,9.01072255620023));
#240750=CARTESIAN_POINT('Ctrl Pts',(-6.37056122083724,15.2,9.0130699228418));
#240751=CARTESIAN_POINT('Ctrl Pts',(-6.37401961178556,15.2,9.01541956307257));
#240752=CARTESIAN_POINT('Ctrl Pts',(-6.37749328522935,15.2,9.01777135844206));
#240753=CARTESIAN_POINT('Ctrl Pts',(-6.38183537738905,15.2,9.02071110289423));
#240754=CARTESIAN_POINT('Ctrl Pts',(-6.38620134575318,15.2,9.02365421482414));
#240755=CARTESIAN_POINT('Ctrl Pts',(-6.39059112019638,15.2,9.02660046753231));
#240756=CARTESIAN_POINT('Ctrl Pts',(-6.39410293994233,15.2,9.0289574698273));
#240757=CARTESIAN_POINT('Ctrl Pts',(-6.3976299954068,15.2,9.03131648287255));
#240758=CARTESIAN_POINT('Ctrl Pts',(-6.40117224982306,15.2,9.03367739050134));
#240759=CARTESIAN_POINT('Ctrl Pts',(-6.40471450375669,15.2,9.03603829780846));
#240760=CARTESIAN_POINT('Ctrl Pts',(-6.40827195387437,15.2,9.03840110095998));
#240761=CARTESIAN_POINT('Ctrl Pts',(-6.41184456798166,15.2,9.0407656844402));
#240762=CARTESIAN_POINT('Ctrl Pts',(-6.41720348987277,15.2,9.04431256014379));
#240763=CARTESIAN_POINT('Ctrl Pts',(-6.42259652490179,15.2,9.04786344487677));
#240764=CARTESIAN_POINT('Ctrl Pts',(-6.42802354861655,15.2,9.05141795540409));
#240765=CARTESIAN_POINT('Ctrl Pts',(-6.43164156393345,15.2,9.05378762876609));
#240766=CARTESIAN_POINT('Ctrl Pts',(-6.43527468541221,15.2,9.05615891414175));
#240767=CARTESIAN_POINT('Ctrl Pts',(-6.43892287666857,15.2,9.05853170078102));
#240768=CARTESIAN_POINT('Ctrl Pts',(-6.44439516380163,15.2,9.06209088090158));
#240769=CARTESIAN_POINT('Ctrl Pts',(-6.44990135729141,15.2,9.06565343737441));
#240770=CARTESIAN_POINT('Ctrl Pts',(-6.45544132967115,15.2,9.06921900041134));
#240771=CARTESIAN_POINT('Ctrl Pts',(-6.45913464492645,15.2,9.07159604265187));
#240772=CARTESIAN_POINT('Ctrl Pts',(-6.46284297496098,15.2,9.07397441871196));
#240773=CARTESIAN_POINT('Ctrl Pts',(-6.46656628077499,15.2,9.07635402300831));
#240774=CARTESIAN_POINT('Ctrl Pts',(-6.470289586589,15.2,9.07873362730465));
#240775=CARTESIAN_POINT('Ctrl Pts',(-6.47402786895481,15.2,9.08111445830117));
#240776=CARTESIAN_POINT('Ctrl Pts',(-6.47778109010532,15.2,9.08349640859776));
#240777=CARTESIAN_POINT('Ctrl Pts',(-6.48059600571252,15.2,9.08528287115794));
#240778=CARTESIAN_POINT('Ctrl Pts',(-6.48341932360841,15.2,9.08706996320477));
#240779=CARTESIAN_POINT('Ctrl Pts',(-6.48625103077295,15.2,9.08885763939586));
#240780=CARTESIAN_POINT('Ctrl Pts',(-6.48908273793749,15.2,9.09064531558694));
#240781=CARTESIAN_POINT('Ctrl Pts',(-6.49192283194672,15.2,9.09243357659325));
#240782=CARTESIAN_POINT('Ctrl Pts',(-6.49477129801062,15.2,9.09422237673664));
#240783=CARTESIAN_POINT('Ctrl Pts',(-6.49856925259,15.2,9.09660744348617));
#240784=CARTESIAN_POINT('Ctrl Pts',(-6.50238209094139,15.2,9.09899346830772));
#240785=CARTESIAN_POINT('Ctrl Pts',(-6.50620977434918,15.2,9.10138034883473));
#240786=CARTESIAN_POINT('Ctrl Pts',(-6.50908053755692,15.2,9.10317050963649));
#240787=CARTESIAN_POINT('Ctrl Pts',(-6.51195965244203,15.2,9.10496114953008));
#240788=CARTESIAN_POINT('Ctrl Pts',(-6.51484710165447,15.2,9.10675222591544));
#240789=CARTESIAN_POINT('Ctrl Pts',(-6.51773455034236,15.2,9.10854330197542));
#240790=CARTESIAN_POINT('Ctrl Pts',(-6.52063033495474,15.2,9.11033481415555));
#240791=CARTESIAN_POINT('Ctrl Pts',(-6.52353443828695,15.2,9.11212671838834));
#240792=CARTESIAN_POINT('Ctrl Pts',(-6.52740657588737,15.2,9.11451592392356));
#240793=CARTESIAN_POINT('Ctrl Pts',(-6.53129350428723,15.2,9.11690582679726));
#240794=CARTESIAN_POINT('Ctrl Pts',(-6.53519518368951,15.2,9.11929632354624));
#240795=CARTESIAN_POINT('Ctrl Pts',(-6.53812144337411,15.2,9.12108919618939));
#240796=CARTESIAN_POINT('Ctrl Pts',(-6.54105600216652,15.2,9.12288240300753));
#240797=CARTESIAN_POINT('Ctrl Pts',(-6.54399884285013,15.2,9.124675901109));
#240798=CARTESIAN_POINT('Ctrl Pts',(-6.5479226307847,15.2,9.12706723212817));
#240799=CARTESIAN_POINT('Ctrl Pts',(-6.55186114364701,15.2,9.12945908041037));
#240800=CARTESIAN_POINT('Ctrl Pts',(-6.55581434276936,15.2,9.13185134421828));
#240801=CARTESIAN_POINT('Ctrl Pts',(-6.55877924184182,15.2,9.13364554191125));
#240802=CARTESIAN_POINT('Ctrl Pts',(-6.56175240252545,15.2,9.13543997352207));
#240803=CARTESIAN_POINT('Ctrl Pts',(-6.56473380901396,15.2,9.13723459621502));
#240804=CARTESIAN_POINT('Ctrl Pts',(-6.56870901802639,15.2,9.13962742668962));
#240805=CARTESIAN_POINT('Ctrl Pts',(-6.572698884285,15.2,9.14202059782473));
#240806=CARTESIAN_POINT('Ctrl Pts',(-6.57670337217141,15.2,9.14441400889964));
#240807=CARTESIAN_POINT('Ctrl Pts',(-6.5807078595122,15.2,9.14680741964844));
#240808=CARTESIAN_POINT('Ctrl Pts',(-6.58472696791777,15.2,9.14920107096946));
#240809=CARTESIAN_POINT('Ctrl Pts',(-6.58876065992038,15.2,9.15159486182929));
#240810=CARTESIAN_POINT('Ctrl Pts',(-6.59279435247256,15.2,9.15398865301527));
#240811=CARTESIAN_POINT('Ctrl Pts',(-6.59684262835839,15.2,9.15638258605007));
#240812=CARTESIAN_POINT('Ctrl Pts',(-6.60090545033962,15.2,9.1587765613557));
#240813=CARTESIAN_POINT('Ctrl Pts',(-6.60395256654876,15.2,9.16057204267184));
#240814=CARTESIAN_POINT('Ctrl Pts',(-6.60700786469465,15.2,9.16236754814425));
#240815=CARTESIAN_POINT('Ctrl Pts',(-6.61007132833406,15.2,9.16416303587069));
#240816=CARTESIAN_POINT('Ctrl Pts',(-6.61313479197347,15.2,9.16595852359713));
#240817=CARTESIAN_POINT('Ctrl Pts',(-6.61620642181189,15.2,9.16775399461522));
#240818=CARTESIAN_POINT('Ctrl Pts',(-6.61928620149166,15.2,9.16954940725832));
#240819=CARTESIAN_POINT('Ctrl Pts',(-6.62236598117144,15.2,9.17134481990143));
#240820=CARTESIAN_POINT('Ctrl Pts',(-6.62545391225922,15.2,9.17314017388621));
#240821=CARTESIAN_POINT('Ctrl Pts',(-6.62854997639599,15.2,9.1749354295293));
#240822=CARTESIAN_POINT('Ctrl Pts',(-6.6337100834781,15.2,9.17792752237651));
#240823=CARTESIAN_POINT('Ctrl Pts',(-6.63889278531647,15.2,9.18091934074323));
#240824=CARTESIAN_POINT('Ctrl Pts',(-6.64409800892637,15.2,9.18391069706268));
#240825=CARTESIAN_POINT('Ctrl Pts',(-6.64722114297884,15.2,9.18570551078914));
#240826=CARTESIAN_POINT('Ctrl Pts',(-6.65035238486754,15.2,9.187500158895));
#240827=CARTESIAN_POINT('Ctrl Pts',(-6.65349171811769,15.2,9.18929460116947));
#240828=CARTESIAN_POINT('Ctrl Pts',(-6.65663105136784,15.2,9.19108904344394));
#240829=CARTESIAN_POINT('Ctrl Pts',(-6.65977847524454,15.2,9.19288327942405));
#240830=CARTESIAN_POINT('Ctrl Pts',(-6.66293397575377,15.2,9.1946772696089));
#240831=CARTESIAN_POINT('Ctrl Pts',(-6.66608947683624,15.2,9.19647126011965));
#240832=CARTESIAN_POINT('Ctrl Pts',(-6.66925305362938,15.2,9.19826500438034));
#240833=CARTESIAN_POINT('Ctrl Pts',(-6.67242468971643,15.2,9.20005846389096));
#240834=CARTESIAN_POINT('Ctrl Pts',(-6.6755963252273,15.2,9.20185192307577));
#240835=CARTESIAN_POINT('Ctrl Pts',(-6.67877601927939,15.2,9.20364509692724));
#240836=CARTESIAN_POINT('Ctrl Pts',(-6.6819637578726,15.2,9.20543794619541));
#240837=CARTESIAN_POINT('Ctrl Pts',(-6.68515149646582,15.2,9.20723079546358));
#240838=CARTESIAN_POINT('Ctrl Pts',(-6.6883472793714,15.2,9.20902332097525));
#240839=CARTESIAN_POINT('Ctrl Pts',(-6.69155108897791,15.2,9.21081548270995));
#240840=CARTESIAN_POINT('Ctrl Pts',(-6.69582283492591,15.2,9.21320503158101));
#240841=CARTESIAN_POINT('Ctrl Pts',(-6.70010885278324,15.2,9.21559393477689));
#240842=CARTESIAN_POINT('Ctrl Pts',(-6.70440910276358,15.2,9.21798209835952));
#240843=CARTESIAN_POINT('Ctrl Pts',(-6.70763429098122,15.2,9.21977322145323));
#240844=CARTESIAN_POINT('Ctrl Pts',(-6.71086748481779,15.2,9.22156392961348));
#240845=CARTESIAN_POINT('Ctrl Pts',(-6.71410866945659,15.2,9.22335418466526));
#240846=CARTESIAN_POINT('Ctrl Pts',(-6.71843024799363,15.2,9.22574119085892));
#240847=CARTESIAN_POINT('Ctrl Pts',(-6.72276603007051,15.2,9.22812739083048));
#240848=CARTESIAN_POINT('Ctrl Pts',(-6.72711598110286,15.2,9.23051269557998));
#240849=CARTESIAN_POINT('Ctrl Pts',(-6.7303784445253,15.2,9.23230167422336));
#240850=CARTESIAN_POINT('Ctrl Pts',(-6.73364887550538,15.2,9.23409014811298));
#240851=CARTESIAN_POINT('Ctrl Pts',(-6.73692725963246,15.2,9.23587807892906));
#240852=CARTESIAN_POINT('Ctrl Pts',(-6.74020564375954,15.2,9.23766600974515));
#240853=CARTESIAN_POINT('Ctrl Pts',(-6.74349197890263,15.2,9.23945339755863));
#240854=CARTESIAN_POINT('Ctrl Pts',(-6.74678625003185,15.2,9.24124020341047));
#240855=CARTESIAN_POINT('Ctrl Pts',(-6.75008052175955,15.2,9.2430270095869));
#240856=CARTESIAN_POINT('Ctrl Pts',(-6.75338273055612,15.2,9.24481323529649));
#240857=CARTESIAN_POINT('Ctrl Pts',(-6.75669286074662,15.2,9.24659884688925));
#240858=CARTESIAN_POINT('Ctrl Pts',(-6.76000299033577,15.2,9.24838445815763));
#240859=CARTESIAN_POINT('Ctrl Pts',(-6.76332104138283,15.2,9.25016945482603));
#240860=CARTESIAN_POINT('Ctrl Pts',(-6.766646997846,15.2,9.25195379942781));
#240861=CARTESIAN_POINT('Ctrl Pts',(-6.76997295430917,15.2,9.25373814402958));
#240862=CARTESIAN_POINT('Ctrl Pts',(-6.77330681482592,15.2,9.25552183562497));
#240863=CARTESIAN_POINT('Ctrl Pts',(-6.77664856080304,15.2,9.25730482727661));
#240864=CARTESIAN_POINT('Ctrl Pts',(-6.77999030678015,15.2,9.25908781892825));
#240865=CARTESIAN_POINT('Ctrl Pts',(-6.78333993605374,15.2,9.26087010917168));
#240866=CARTESIAN_POINT('Ctrl Pts',(-6.78669743619696,15.2,9.26265166624004));
#240867=CARTESIAN_POINT('Ctrl Pts',(-6.79229326997229,15.2,9.26562092812853));
#240868=CARTESIAN_POINT('Ctrl Pts',(-6.79791095410398,15.2,9.26858815135357));
#240869=CARTESIAN_POINT('Ctrl Pts',(-6.80355049700006,15.2,9.27155330199999));
#240870=CARTESIAN_POINT('Ctrl Pts',(-5.85257411500006,12.2,8.56667970999998));
#240871=CARTESIAN_POINT('Ctrl Pts',(-5.8537050266944,12.2,8.56806288496946));
#240872=CARTESIAN_POINT('Ctrl Pts',(-5.8548762742267,12.2,8.5694869238734));
#240873=CARTESIAN_POINT('Ctrl Pts',(-5.85608775334231,12.2,8.57095065186461));
#240874=CARTESIAN_POINT('Ctrl Pts',(-5.85730507482257,12.2,8.57242143869206));
#240875=CARTESIAN_POINT('Ctrl Pts',(-5.85856301277102,12.2,8.57393230486909));
#240876=CARTESIAN_POINT('Ctrl Pts',(-5.85986145340903,12.2,8.5754821088666));
#240877=CARTESIAN_POINT('Ctrl Pts',(-5.86115989392909,12.2,8.57703191272334));
#240878=CARTESIAN_POINT('Ctrl Pts',(-5.86249883775011,12.2,8.5786206548507));
#240879=CARTESIAN_POINT('Ctrl Pts',(-5.86387817019999,12.2,8.58024722870826));
#240880=CARTESIAN_POINT('Ctrl Pts',(-5.86525750264987,12.2,8.58187380256584));
#240881=CARTESIAN_POINT('Ctrl Pts',(-5.86667722397461,12.2,8.58353820930606));
#240882=CARTESIAN_POINT('Ctrl Pts',(-5.86813722065885,12.2,8.58523937157712));
#240883=CARTESIAN_POINT('Ctrl Pts',(-5.86959721747571,12.2,8.58694053400272));
#240884=CARTESIAN_POINT('Ctrl Pts',(-5.87109749092289,12.2,8.58867845508586));
#240885=CARTESIAN_POINT('Ctrl Pts',(-5.87263792542624,12.2,8.59045208743492));
#240886=CARTESIAN_POINT('Ctrl Pts',(-5.87417835978964,12.2,8.5922257196229));
#240887=CARTESIAN_POINT('Ctrl Pts',(-5.87575895551881,12.2,8.59403506540096));
#240888=CARTESIAN_POINT('Ctrl Pts',(-5.87737960096739,12.2,8.5958791057591));
#240889=CARTESIAN_POINT('Ctrl Pts',(-5.87900024641597,12.2,8.59772314611723));
#240890=CARTESIAN_POINT('Ctrl Pts',(-5.88066094034601,12.2,8.59960188503347));
#240891=CARTESIAN_POINT('Ctrl Pts',(-5.88236157069914,12.2,8.60151432962917));
#240892=CARTESIAN_POINT('Ctrl Pts',(-5.88406220120674,12.2,8.60342677439859));
#240893=CARTESIAN_POINT('Ctrl Pts',(-5.88580276684432,12.2,8.60537292884722));
#240894=CARTESIAN_POINT('Ctrl Pts',(-5.88758315544406,12.2,8.6073518267073));
#240895=CARTESIAN_POINT('Ctrl Pts',(-5.88936354388209,12.2,8.60933072438763));
#240896=CARTESIAN_POINT('Ctrl Pts',(-5.8911837544007,12.2,8.61134236845095));
#240897=CARTESIAN_POINT('Ctrl Pts',(-5.89304367483485,12.2,8.61338582004476));
#240898=CARTESIAN_POINT('Ctrl Pts',(-5.89490359526901,12.2,8.61542927163859));
#240899=CARTESIAN_POINT('Ctrl Pts',(-5.89680322566664,12.2,8.61750453153813));
#240900=CARTESIAN_POINT('Ctrl Pts',(-5.89874245209447,12.2,8.61961068537694));
#240901=CARTESIAN_POINT('Ctrl Pts',(-5.90068167852228,12.2,8.62171683921574));
#240902=CARTESIAN_POINT('Ctrl Pts',(-5.90266050315601,12.2,8.62385389007783));
#240903=CARTESIAN_POINT('Ctrl Pts',(-5.90467880958,12.2,8.62602094299706));
#240904=CARTESIAN_POINT('Ctrl Pts',(-5.90669711618733,12.2,8.62818799611313));
#240905=CARTESIAN_POINT('Ctrl Pts',(-5.90875490621511,12.2,8.63038505414048));
#240906=CARTESIAN_POINT('Ctrl Pts',(-5.91085206683112,12.2,8.63261124734639));
#240907=CARTESIAN_POINT('Ctrl Pts',(-5.91294922725662,12.2,8.63483744035008));
#240908=CARTESIAN_POINT('Ctrl Pts',(-5.91508575898494,12.2,8.6370927696049));
#240909=CARTESIAN_POINT('Ctrl Pts',(-5.917261545749,12.2,8.63937638753223));
#240910=CARTESIAN_POINT('Ctrl Pts',(-5.91943733251307,12.2,8.64166000545956));
#240911=CARTESIAN_POINT('Ctrl Pts',(-5.92165237917221,12.2,8.64397191098185));
#240912=CARTESIAN_POINT('Ctrl Pts',(-5.92390656675429,12.2,8.64631127722828));
#240913=CARTESIAN_POINT('Ctrl Pts',(-5.92616075454112,12.2,8.64865064368723));
#240914=CARTESIAN_POINT('Ctrl Pts',(-5.92845408727345,12.2,8.65101747241555));
#240915=CARTESIAN_POINT('Ctrl Pts',(-5.93078644981893,12.2,8.6534109538805));
#240916=CARTESIAN_POINT('Ctrl Pts',(-5.93311881215258,12.2,8.65580443512804));
#240917=CARTESIAN_POINT('Ctrl Pts',(-5.93549020490895,12.2,8.65822456958498));
#240918=CARTESIAN_POINT('Ctrl Pts',(-5.93790051249891,12.2,8.66067056875718));
#240919=CARTESIAN_POINT('Ctrl Pts',(-5.94031082008886,12.2,8.66311656792936));
#240920=CARTESIAN_POINT('Ctrl Pts',(-5.94276004699681,12.2,8.66558843074518));
#240921=CARTESIAN_POINT('Ctrl Pts',(-5.94524807348713,12.2,8.66808538523611));
#240922=CARTESIAN_POINT('Ctrl Pts',(-5.94773610020346,12.2,8.67058233995385));
#240923=CARTESIAN_POINT('Ctrl Pts',(-5.95026293231135,12.2,8.67310438872892));
#240924=CARTESIAN_POINT('Ctrl Pts',(-5.95282845024826,12.2,8.67565077649633));
#240925=CARTESIAN_POINT('Ctrl Pts',(-5.95539396795212,12.2,8.67819716403244));
#240926=CARTESIAN_POINT('Ctrl Pts',(-5.95799817570432,12.2,8.68076788892752));
#240927=CARTESIAN_POINT('Ctrl Pts',(-5.96064095702498,12.2,8.68336221549994));
#240928=CARTESIAN_POINT('Ctrl Pts',(-5.96328373834564,12.2,8.68595654207235));
#240929=CARTESIAN_POINT('Ctrl Pts',(-5.96596509279383,12.2,8.68857447029322));
#240930=CARTESIAN_POINT('Ctrl Pts',(-5.96868490824531,12.2,8.69121527799453));
#240931=CARTESIAN_POINT('Ctrl Pts',(-5.97140472394383,12.2,8.69385608593571));
#240932=CARTESIAN_POINT('Ctrl Pts',(-5.97416299909145,12.2,8.69651977286147));
#240933=CARTESIAN_POINT('Ctrl Pts',(-5.97695961882982,12.2,8.69920563384271));
#240934=CARTESIAN_POINT('Ctrl Pts',(-5.97975623831417,12.2,8.70189149457996));
#240935=CARTESIAN_POINT('Ctrl Pts',(-5.98259120274255,12.2,8.70459952736291));
#240936=CARTESIAN_POINT('Ctrl Pts',(-5.98546439798464,12.2,8.7073290440262));
#240937=CARTESIAN_POINT('Ctrl Pts',(-5.98833759322673,12.2,8.71005856068949));
#240938=CARTESIAN_POINT('Ctrl Pts',(-5.9912490184649,12.2,8.7128095585006));
#240939=CARTESIAN_POINT('Ctrl Pts',(-5.99419855785607,12.2,8.71558136139897));
#240940=CARTESIAN_POINT('Ctrl Pts',(-5.99665650743803,12.2,8.71789119723154));
#240941=CARTESIAN_POINT('Ctrl Pts',(-5.999140926204,12.2,8.72021548042008));
#240942=CARTESIAN_POINT('Ctrl Pts',(-6.00165174661927,12.2,8.72255382861377));
#240943=CARTESIAN_POINT('Ctrl Pts',(-6.00416256703455,12.2,8.72489217680747));
#240944=CARTESIAN_POINT('Ctrl Pts',(-6.00669978921481,12.2,8.7272445875713));
#240945=CARTESIAN_POINT('Ctrl Pts',(-6.00926334624026,12.2,8.72961068424866));
#240946=CARTESIAN_POINT('Ctrl Pts',(-6.0118269032657,12.2,8.73197678092602));
#240947=CARTESIAN_POINT('Ctrl Pts',(-6.01441679586664,12.2,8.73435656409993));
#240948=CARTESIAN_POINT('Ctrl Pts',(-6.01703295544998,12.2,8.73674966076662));
#240949=CARTESIAN_POINT('Ctrl Pts',(-6.01964911503334,12.2,8.7391427574333));
#240950=CARTESIAN_POINT('Ctrl Pts',(-6.02229154302258,12.2,8.74154916728469));
#240951=CARTESIAN_POINT('Ctrl Pts',(-6.02496017178478,12.2,8.74396852576794));
#240952=CARTESIAN_POINT('Ctrl Pts',(-6.02762880054697,12.2,8.74638788425118));
#240953=CARTESIAN_POINT('Ctrl Pts',(-6.03032362932119,12.2,8.74882019028705));
#240954=CARTESIAN_POINT('Ctrl Pts',(-6.03304459216976,12.2,8.75126508542659));
#240955=CARTESIAN_POINT('Ctrl Pts',(-6.03576555501833,12.2,8.75370998056613));
#240956=CARTESIAN_POINT('Ctrl Pts',(-6.03851265030239,12.2,8.75616746406093));
#240957=CARTESIAN_POINT('Ctrl Pts',(-6.04128581162318,12.2,8.75863718239488));
#240958=CARTESIAN_POINT('Ctrl Pts',(-6.04405897294397,12.2,8.76110690072884));
#240959=CARTESIAN_POINT('Ctrl Pts',(-6.04685820154622,12.2,8.76358885195297));
#240960=CARTESIAN_POINT('Ctrl Pts',(-6.04968342786972,12.2,8.76608269131449));
#240961=CARTESIAN_POINT('Ctrl Pts',(-6.05250865419322,12.2,8.768576530676));
#240962=CARTESIAN_POINT('Ctrl Pts',(-6.05535987785754,12.2,8.77108225413939));
#240963=CARTESIAN_POINT('Ctrl Pts',(-6.05823703390132,12.2,8.77359952261255));
#240964=CARTESIAN_POINT('Ctrl Pts',(-6.06111418994511,12.2,8.77611679108571));
#240965=CARTESIAN_POINT('Ctrl Pts',(-6.06401727443098,12.2,8.77864560073128));
#240966=CARTESIAN_POINT('Ctrl Pts',(-6.06694622234977,12.2,8.78118561760719));
#240967=CARTESIAN_POINT('Ctrl Pts',(-6.06987516994929,12.2,8.78372563420625));
#240968=CARTESIAN_POINT('Ctrl Pts',(-6.07282998071492,12.2,8.786276857245));
#240969=CARTESIAN_POINT('Ctrl Pts',(-6.07581058656847,12.2,8.7888389523815));
#240970=CARTESIAN_POINT('Ctrl Pts',(-6.07879119274691,12.2,8.79140104779728));
#240971=CARTESIAN_POINT('Ctrl Pts',(-6.08179759234439,12.2,8.7939740170629));
#240972=CARTESIAN_POINT('Ctrl Pts',(-6.08482972012007,12.2,8.79655753164537));
#240973=CARTESIAN_POINT('Ctrl Pts',(-6.08786184789574,12.2,8.79914104622784));
#240974=CARTESIAN_POINT('Ctrl Pts',(-6.0909197017099,12.2,8.80173510663794));
#240975=CARTESIAN_POINT('Ctrl Pts',(-6.09400321309667,12.2,8.80433939115098));
#240976=CARTESIAN_POINT('Ctrl Pts',(-6.09708672448344,12.2,8.80694367566402));
#240977=CARTESIAN_POINT('Ctrl Pts',(-6.10019589624247,12.2,8.80955818307048));
#240978=CARTESIAN_POINT('Ctrl Pts',(-6.10333065611952,12.2,8.81218259618701));
#240979=CARTESIAN_POINT('Ctrl Pts',(-6.10646541599657,12.2,8.81480700930354));
#240980=CARTESIAN_POINT('Ctrl Pts',(-6.10962576757645,12.2,8.8174413284776));
#240981=CARTESIAN_POINT('Ctrl Pts',(-6.11281163882513,12.2,8.82008524056044));
#240982=CARTESIAN_POINT('Ctrl Pts',(-6.11599751007381,12.2,8.82272915264328));
#240983=CARTESIAN_POINT('Ctrl Pts',(-6.11920890416203,12.2,8.82538265730971));
#240984=CARTESIAN_POINT('Ctrl Pts',(-6.12244574881345,12.2,8.8280454460592));
#240985=CARTESIAN_POINT('Ctrl Pts',(-6.12503522467571,12.2,8.8301756771749));
#240986=CARTESIAN_POINT('Ctrl Pts',(-6.1276409911997,12.2,8.8323118506449));
#240987=CARTESIAN_POINT('Ctrl Pts',(-6.13026301236389,12.2,8.83445381003581));
#240988=CARTESIAN_POINT('Ctrl Pts',(-6.13288503317083,12.2,8.83659576913488));
#240989=CARTESIAN_POINT('Ctrl Pts',(-6.13552330723175,12.2,8.83874351511705));
#240990=CARTESIAN_POINT('Ctrl Pts',(-6.13817780129148,12.2,8.84089689260732));
#240991=CARTESIAN_POINT('Ctrl Pts',(-6.14149591913739,12.2,8.84358861469019));
#240992=CARTESIAN_POINT('Ctrl Pts',(-6.14483937943672,12.2,8.84628913648997));
#240993=CARTESIAN_POINT('Ctrl Pts',(-6.1482081130465,12.2,8.84899816128117));
#240994=CARTESIAN_POINT('Ctrl Pts',(-6.15090310008119,12.2,8.85116538123226));
#240995=CARTESIAN_POINT('Ctrl Pts',(-6.15361426206229,12.2,8.85333804315749));
#240996=CARTESIAN_POINT('Ctrl Pts',(-6.15634156340415,12.2,8.85551599710769));
#240997=CARTESIAN_POINT('Ctrl Pts',(-6.15906886437442,12.2,8.85769395076114));
#240998=CARTESIAN_POINT('Ctrl Pts',(-6.16181230541788,12.2,8.85987719535591));
#240999=CARTESIAN_POINT('Ctrl Pts',(-6.16457184952455,12.2,8.86206558362111));
#241000=CARTESIAN_POINT('Ctrl Pts',(-6.16733139400721,12.2,8.86425397218447));
#241001=CARTESIAN_POINT('Ctrl Pts',(-6.17010704317239,12.2,8.86644750392904));
#241002=CARTESIAN_POINT('Ctrl Pts',(-6.1728987609367,12.2,8.86864603243807));
#241003=CARTESIAN_POINT('Ctrl Pts',(-6.17569047832064,12.2,8.87084456064756));
#241004=CARTESIAN_POINT('Ctrl Pts',(-6.17849826341207,12.2,8.87304808432517));
#241005=CARTESIAN_POINT('Ctrl Pts',(-6.18132208159866,12.2,8.87525645942121));
#241006=CARTESIAN_POINT('Ctrl Pts',(-6.18485185462046,12.2,8.87801692851691));
#241007=CARTESIAN_POINT('Ctrl Pts',(-6.18840667958956,12.2,8.88078497676334));
#241008=CARTESIAN_POINT('Ctrl Pts',(-6.19198648653269,12.2,8.8835603248185));
#241009=CARTESIAN_POINT('Ctrl Pts',(-6.19485033224328,12.2,8.88578060338364));
#241010=CARTESIAN_POINT('Ctrl Pts',(-6.19773016514467,12.2,8.88800555423823));
#241011=CARTESIAN_POINT('Ctrl Pts',(-6.20062595097021,12.2,8.89023503424894));
#241012=CARTESIAN_POINT('Ctrl Pts',(-6.20352173640121,12.2,8.89246451395588));
#241013=CARTESIAN_POINT('Ctrl Pts',(-6.20643347491972,12.2,8.89469852319395));
#241014=CARTESIAN_POINT('Ctrl Pts',(-6.20936112982526,12.2,8.89693692240018));
#241015=CARTESIAN_POINT('Ctrl Pts',(-6.21228878512968,12.2,8.8991753219114));
#241016=CARTESIAN_POINT('Ctrl Pts',(-6.21523235733809,12.2,8.90141811162485));
#241017=CARTESIAN_POINT('Ctrl Pts',(-6.21819181100042,12.2,8.90366515169204));
#241018=CARTESIAN_POINT('Ctrl Pts',(-6.22115126425952,12.2,8.90591219145307));
#241019=CARTESIAN_POINT('Ctrl Pts',(-6.22412659708769,12.2,8.90816348294659));
#241020=CARTESIAN_POINT('Ctrl Pts',(-6.22711777578594,12.2,8.91041888737288));
#241021=CARTESIAN_POINT('Ctrl Pts',(-6.23010895489176,12.2,8.91267429210646));
#241022=CARTESIAN_POINT('Ctrl Pts',(-6.23311597888741,12.2,8.91493380993174));
#241023=CARTESIAN_POINT('Ctrl Pts',(-6.23613881201039,12.2,8.91719730600985));
#241024=CARTESIAN_POINT('Ctrl Pts',(-6.23916164472152,12.2,8.91946080177955));
#241025=CARTESIAN_POINT('Ctrl Pts',(-6.24220028693525,12.2,8.92172827530357));
#241026=CARTESIAN_POINT('Ctrl Pts',(-6.24525470168394,12.2,8.92399959289528));
#241027=CARTESIAN_POINT('Ctrl Pts',(-6.24830911684879,12.2,8.92627091079644));
#241028=CARTESIAN_POINT('Ctrl Pts',(-6.25137930531514,12.2,8.92854607119243));
#241029=CARTESIAN_POINT('Ctrl Pts',(-6.25446523048333,12.2,8.93082494198331));
#241030=CARTESIAN_POINT('Ctrl Pts',(-6.25755115565152,12.2,8.93310381277419));
#241031=CARTESIAN_POINT('Ctrl Pts',(-6.26065281821597,12.2,8.93538639513491));
#241032=CARTESIAN_POINT('Ctrl Pts',(-6.26377018127636,12.2,8.93767255464877));
#241033=CARTESIAN_POINT('Ctrl Pts',(-6.26688754391201,12.2,8.93995871385113));
#241034=CARTESIAN_POINT('Ctrl Pts',(-6.27002060762435,12.2,8.94224845165325));
#241035=CARTESIAN_POINT('Ctrl Pts',(-6.27316933571452,12.2,8.9445416386984));
#241036=CARTESIAN_POINT('Ctrl Pts',(-6.27710524614898,12.2,8.94740812273918));
#241037=CARTESIAN_POINT('Ctrl Pts',(-6.28106563330555,12.2,8.9502799938222));
#241038=CARTESIAN_POINT('Ctrl Pts',(-6.28505042524998,12.2,8.95315700201663));
#241039=CARTESIAN_POINT('Ctrl Pts',(-6.28823825897927,12.2,8.95545860869762));
#241040=CARTESIAN_POINT('Ctrl Pts',(-6.29144171166596,12.2,8.95776350188735));
#241041=CARTESIAN_POINT('Ctrl Pts',(-6.29466074750965,12.2,8.96007155540234));
#241042=CARTESIAN_POINT('Ctrl Pts',(-6.29787978291474,12.2,8.96237960860286));
#241043=CARTESIAN_POINT('Ctrl Pts',(-6.30111440152655,12.2,8.96469082122153));
#241044=CARTESIAN_POINT('Ctrl Pts',(-6.30436456749779,12.2,8.96700506826507));
#241045=CARTESIAN_POINT('Ctrl Pts',(-6.30761473391185,12.2,8.96931931562392));
#241046=CARTESIAN_POINT('Ctrl Pts',(-6.3108804460394,12.2,8.97163659577479));
#241047=CARTESIAN_POINT('Ctrl Pts',(-6.31416166855315,12.2,8.973956785346));
#241048=CARTESIAN_POINT('Ctrl Pts',(-6.31744289061984,12.2,8.97627697460106));
#241049=CARTESIAN_POINT('Ctrl Pts',(-6.32073962418448,12.2,8.97860007301685));
#241050=CARTESIAN_POINT('Ctrl Pts',(-6.32405183024604,12.2,8.98092595682653));
#241051=CARTESIAN_POINT('Ctrl Pts',(-6.32819208816146,12.2,8.98383331182631));
#241052=CARTESIAN_POINT('Ctrl Pts',(-6.33235652492191,12.2,8.98674501776507));
#241053=CARTESIAN_POINT('Ctrl Pts',(-6.33654506776788,12.2,8.98966083700097));
#241054=CARTESIAN_POINT('Ctrl Pts',(-6.33989590222727,12.2,8.99199349251682));
#241055=CARTESIAN_POINT('Ctrl Pts',(-6.34326216468622,12.2,8.99432878125592));
#241056=CARTESIAN_POINT('Ctrl Pts',(-6.34664381870745,12.2,8.99666658038923));
#241057=CARTESIAN_POINT('Ctrl Pts',(-6.35002547226794,12.2,8.999004379204));
#241058=CARTESIAN_POINT('Ctrl Pts',(-6.35342251877061,12.2,9.00134469013906));
#241059=CARTESIAN_POINT('Ctrl Pts',(-6.35683491821284,12.2,9.00368739205848));
#241060=CARTESIAN_POINT('Ctrl Pts',(-6.36024731812,12.2,9.00603009429709));
#241061=CARTESIAN_POINT('Ctrl Pts',(-6.36367507370687,12.2,9.00837518923882));
#241062=CARTESIAN_POINT('Ctrl Pts',(-6.36711814750661,12.2,9.01072255620022));
#241063=CARTESIAN_POINT('Ctrl Pts',(-6.37056122083724,12.2,9.0130699228418));
#241064=CARTESIAN_POINT('Ctrl Pts',(-6.37401961178556,12.2,9.01541956307257));
#241065=CARTESIAN_POINT('Ctrl Pts',(-6.37749328522935,12.2,9.01777135844206));
#241066=CARTESIAN_POINT('Ctrl Pts',(-6.38183537738905,12.2,9.02071110289423));
#241067=CARTESIAN_POINT('Ctrl Pts',(-6.38620134575318,12.2,9.02365421482414));
#241068=CARTESIAN_POINT('Ctrl Pts',(-6.39059112019638,12.2,9.02660046753231));
#241069=CARTESIAN_POINT('Ctrl Pts',(-6.39410293994233,12.2,9.0289574698273));
#241070=CARTESIAN_POINT('Ctrl Pts',(-6.3976299954068,12.2,9.03131648287255));
#241071=CARTESIAN_POINT('Ctrl Pts',(-6.40117224982306,12.2,9.03367739050134));
#241072=CARTESIAN_POINT('Ctrl Pts',(-6.40471450375669,12.2,9.03603829780846));
#241073=CARTESIAN_POINT('Ctrl Pts',(-6.40827195387436,12.2,9.03840110095998));
#241074=CARTESIAN_POINT('Ctrl Pts',(-6.41184456798166,12.2,9.0407656844402));
#241075=CARTESIAN_POINT('Ctrl Pts',(-6.41631033598086,12.2,9.0437214140321));
#241076=CARTESIAN_POINT('Ctrl Pts',(-6.42079979358398,12.2,9.04667992758424));
#241077=CARTESIAN_POINT('Ctrl Pts',(-6.42531286892999,12.2,9.04964100355634));
#241078=CARTESIAN_POINT('Ctrl Pts',(-6.42892332940356,12.2,9.05200986446312));
#241079=CARTESIAN_POINT('Ctrl Pts',(-6.4325489052817,12.2,9.05438036537844));
#241080=CARTESIAN_POINT('Ctrl Pts',(-6.43618955981443,12.2,9.05675239445224));
#241081=CARTESIAN_POINT('Ctrl Pts',(-6.43983021385112,12.2,9.05912442320287));
#241082=CARTESIAN_POINT('Ctrl Pts',(-6.44348594688266,12.2,9.06149798139209));
#241083=CARTESIAN_POINT('Ctrl Pts',(-6.44715672104243,12.2,9.06387295687203));
#241084=CARTESIAN_POINT('Ctrl Pts',(-6.45082749570234,12.2,9.06624793267555));
#241085=CARTESIAN_POINT('Ctrl Pts',(-6.4545133114,12.2,9.06862432851192));
#241086=CARTESIAN_POINT('Ctrl Pts',(-6.45821413126935,12.2,9.07100203091937));
#241087=CARTESIAN_POINT('Ctrl Pts',(-6.46191495063446,12.2,9.07337973300286));
#241088=CARTESIAN_POINT('Ctrl Pts',(-6.46563077588266,12.2,9.07575874341663));
#241089=CARTESIAN_POINT('Ctrl Pts',(-6.46936156663168,12.2,9.07813895411081));
#241090=CARTESIAN_POINT('Ctrl Pts',(-6.47309235788902,12.2,9.08051916512929));
#241091=CARTESIAN_POINT('Ctrl Pts',(-6.47683811763048,12.2,9.08290057602204));
#241092=CARTESIAN_POINT('Ctrl Pts',(-6.48059880551923,12.2,9.0852830790516));
#241093=CARTESIAN_POINT('Ctrl Pts',(-6.48341932117959,12.2,9.08706995616146));
#241094=CARTESIAN_POINT('Ctrl Pts',(-6.48624823573766,12.2,9.08885744752187));
#241095=CARTESIAN_POINT('Ctrl Pts',(-6.48908553277242,12.2,9.09064550821503));
#241096=CARTESIAN_POINT('Ctrl Pts',(-6.49192282980717,12.2,9.09243356890818));
#241097=CARTESIAN_POINT('Ctrl Pts',(-6.49476850814347,12.2,9.09422219987002));
#241098=CARTESIAN_POINT('Ctrl Pts',(-6.49762255374738,12.2,9.09601135451331));
#241099=CARTESIAN_POINT('Ctrl Pts',(-6.50047659935128,12.2,9.09780050915658));
#241100=CARTESIAN_POINT('Ctrl Pts',(-6.50333901166296,12.2,9.09959018835817));
#241101=CARTESIAN_POINT('Ctrl Pts',(-6.50620977434918,12.2,9.10138034883473));
#241102=CARTESIAN_POINT('Ctrl Pts',(-6.50908053755692,12.2,9.10317050963649));
#241103=CARTESIAN_POINT('Ctrl Pts',(-6.51195965244202,12.2,9.10496114953008));
#241104=CARTESIAN_POINT('Ctrl Pts',(-6.51484710165447,12.2,9.10675222591543));
#241105=CARTESIAN_POINT('Ctrl Pts',(-6.51773455034236,12.2,9.10854330197542));
#241106=CARTESIAN_POINT('Ctrl Pts',(-6.52063033495474,12.2,9.11033481415555));
#241107=CARTESIAN_POINT('Ctrl Pts',(-6.52353443828695,12.2,9.11212671838834));
#241108=CARTESIAN_POINT('Ctrl Pts',(-6.52643854161916,12.2,9.11391862262114));
#241109=CARTESIAN_POINT('Ctrl Pts',(-6.52935096497388,12.2,9.11571091906048));
#241110=CARTESIAN_POINT('Ctrl Pts',(-6.53227169107683,12.2,9.11750356420372));
#241111=CARTESIAN_POINT('Ctrl Pts',(-6.53519241717978,12.2,9.11929620934696));
#241112=CARTESIAN_POINT('Ctrl Pts',(-6.53812144647338,12.2,9.12108920284848));
#241113=CARTESIAN_POINT('Ctrl Pts',(-6.54105876403333,12.2,9.12288250199165));
#241114=CARTESIAN_POINT('Ctrl Pts',(-6.54399608159328,12.2,9.12467580113483));
#241115=CARTESIAN_POINT('Ctrl Pts',(-6.54694168686957,12.2,9.12646940566967));
#241116=CARTESIAN_POINT('Ctrl Pts',(-6.54989556396983,12.2,9.12826327277112));
#241117=CARTESIAN_POINT('Ctrl Pts',(-6.55284944107009,12.2,9.13005713987257));
#241118=CARTESIAN_POINT('Ctrl Pts',(-6.55581158960254,12.2,9.13185126901174));
#241119=CARTESIAN_POINT('Ctrl Pts',(-6.55878199443371,12.2,9.13364561816116));
#241120=CARTESIAN_POINT('Ctrl Pts',(-6.56175239926489,12.2,9.13543996731057));
#241121=CARTESIAN_POINT('Ctrl Pts',(-6.56473106165852,12.2,9.1372345350573));
#241122=CARTESIAN_POINT('Ctrl Pts',(-6.56771796238219,12.2,9.13902928111706));
#241123=CARTESIAN_POINT('Ctrl Pts',(-6.57070486364848,12.2,9.14082402750287));
#241124=CARTESIAN_POINT('Ctrl Pts',(-6.5737000059838,12.2,9.14261895043041));
#241125=CARTESIAN_POINT('Ctrl Pts',(-6.57670337217141,12.2,9.14441400889964));
#241126=CARTESIAN_POINT('Ctrl Pts',(-6.57970673781341,12.2,9.14620906704277));
#241127=CARTESIAN_POINT('Ctrl Pts',(-6.58271832773829,12.2,9.14800426054422));
#241128=CARTESIAN_POINT('Ctrl Pts',(-6.58573812633763,12.2,9.14979954668734));
#241129=CARTESIAN_POINT('Ctrl Pts',(-6.58875792493697,12.2,9.15159483283046));
#241130=CARTESIAN_POINT('Ctrl Pts',(-6.59178593243258,12.2,9.15339021140869));
#241131=CARTESIAN_POINT('Ctrl Pts',(-6.59482213204442,12.2,9.15518564251828));
#241132=CARTESIAN_POINT('Ctrl Pts',(-6.59887039800967,12.2,9.15757955055568));
#241133=CARTESIAN_POINT('Ctrl Pts',(-6.60293322881538,12.2,9.15997355057371));
#241134=CARTESIAN_POINT('Ctrl Pts',(-6.60701058609168,12.2,9.16236754343356));
#241135=CARTESIAN_POINT('Ctrl Pts',(-6.61006860474332,12.2,9.16416303848616));
#241136=CARTESIAN_POINT('Ctrl Pts',(-6.61313479453896,12.2,9.16595853006379));
#241137=CARTESIAN_POINT('Ctrl Pts',(-6.61620913969521,12.2,9.16775397711639));
#241138=CARTESIAN_POINT('Ctrl Pts',(-6.61928348429296,12.2,9.16954942384282));
#241139=CARTESIAN_POINT('Ctrl Pts',(-6.62236598456526,12.2,9.17134482622757));
#241140=CARTESIAN_POINT('Ctrl Pts',(-6.62545662462036,12.2,9.17314014295401));
#241141=CARTESIAN_POINT('Ctrl Pts',(-6.62854726467546,12.2,9.17493545968046));
#241142=CARTESIAN_POINT('Ctrl Pts',(-6.63164604319621,12.2,9.17673069149854));
#241143=CARTESIAN_POINT('Ctrl Pts',(-6.63475294620833,12.2,9.17852579722499));
#241144=CARTESIAN_POINT('Ctrl Pts',(-6.63785984922046,12.2,9.18032090295143));
#241145=CARTESIAN_POINT('Ctrl Pts',(-6.64097487487391,12.2,9.18211588333622));
#241146=CARTESIAN_POINT('Ctrl Pts',(-6.64409800892637,12.2,9.18391069706268));
#241147=CARTESIAN_POINT('Ctrl Pts',(-6.64722114297884,12.2,9.18570551078914));
#241148=CARTESIAN_POINT('Ctrl Pts',(-6.65035238486753,12.2,9.187500158895));
#241149=CARTESIAN_POINT('Ctrl Pts',(-6.65349171811769,12.2,9.18929460116947));
#241150=CARTESIAN_POINT('Ctrl Pts',(-6.65663105136784,12.2,9.19108904344393));
#241151=CARTESIAN_POINT('Ctrl Pts',(-6.65977847524454,12.2,9.19288327942405));
#241152=CARTESIAN_POINT('Ctrl Pts',(-6.66293397575377,12.2,9.1946772696089));
#241153=CARTESIAN_POINT('Ctrl Pts',(-6.66608947683624,12.2,9.19647126011965));
#241154=CARTESIAN_POINT('Ctrl Pts',(-6.66925305362937,12.2,9.19826500438034));
#241155=CARTESIAN_POINT('Ctrl Pts',(-6.67242468971642,12.2,9.20005846389096));
#241156=CARTESIAN_POINT('Ctrl Pts',(-6.67559632522729,12.2,9.20185192307577));
#241157=CARTESIAN_POINT('Ctrl Pts',(-6.67877601927939,12.2,9.20364509692724));
#241158=CARTESIAN_POINT('Ctrl Pts',(-6.6819637578726,12.2,9.20543794619541));
#241159=CARTESIAN_POINT('Ctrl Pts',(-6.68515149646582,12.2,9.20723079546358));
#241160=CARTESIAN_POINT('Ctrl Pts',(-6.6883472793714,12.2,9.20902332097526));
#241161=CARTESIAN_POINT('Ctrl Pts',(-6.69155108897791,12.2,9.21081548270995));
#241162=CARTESIAN_POINT('Ctrl Pts',(-6.69475489858442,12.2,9.21260764444464));
#241163=CARTESIAN_POINT('Ctrl Pts',(-6.6979667357828,12.2,9.21439944307197));
#241164=CARTESIAN_POINT('Ctrl Pts',(-6.70118658480542,12.2,9.21619083876503));
#241165=CARTESIAN_POINT('Ctrl Pts',(-6.70440643382803,12.2,9.21798223445809));
#241166=CARTESIAN_POINT('Ctrl Pts',(-6.70763429324903,12.2,9.21977322685317));
#241167=CARTESIAN_POINT('Ctrl Pts',(-6.71087014838076,12.2,9.22156377953815));
#241168=CARTESIAN_POINT('Ctrl Pts',(-6.71410600351248,12.2,9.22335433222312));
#241169=CARTESIAN_POINT('Ctrl Pts',(-6.71734985492702,12.2,9.22514444437481));
#241170=CARTESIAN_POINT('Ctrl Pts',(-6.72060168505778,12.2,9.22693407764318));
#241171=CARTESIAN_POINT('Ctrl Pts',(-6.72493745895928,12.2,9.22932025555108));
#241172=CARTESIAN_POINT('Ctrl Pts',(-6.72928742038135,12.2,9.23170558359416));
#241173=CARTESIAN_POINT('Ctrl Pts',(-6.73365152769465,12.2,9.23408996873495));
#241174=CARTESIAN_POINT('Ctrl Pts',(-6.73692460788232,12.2,9.23587825742811));
#241175=CARTESIAN_POINT('Ctrl Pts',(-6.74020564685162,12.2,9.23766601558852));
#241176=CARTESIAN_POINT('Ctrl Pts',(-6.74349462549701,12.2,9.23945320524003));
#241177=CARTESIAN_POINT('Ctrl Pts',(-6.74678360414241,12.2,9.24124039489155));
#241178=CARTESIAN_POINT('Ctrl Pts',(-6.75008052382735,12.2,9.24302701408682));
#241179=CARTESIAN_POINT('Ctrl Pts',(-6.75338537087324,12.2,9.24481303131363));
#241180=CARTESIAN_POINT('Ctrl Pts',(-6.75669021791912,12.2,9.24659904854046));
#241181=CARTESIAN_POINT('Ctrl Pts',(-6.76000299123116,12.2,9.24838446287566));
#241182=CARTESIAN_POINT('Ctrl Pts',(-6.7633236757761,12.2,9.25016923810258));
#241183=CARTESIAN_POINT('Ctrl Pts',(-6.76664436092431,12.2,9.25195401365372));
#241184=CARTESIAN_POINT('Ctrl Pts',(-6.76997295680805,12.2,9.25373815099635));
#241185=CARTESIAN_POINT('Ctrl Pts',(-6.77330944441903,12.2,9.25552160438045));
#241186=CARTESIAN_POINT('Ctrl Pts',(-6.77775809355678,12.2,9.25789954168592));
#241187=CARTESIAN_POINT('Ctrl Pts',(-6.78222076954265,12.2,9.26027625692344));
#241188=CARTESIAN_POINT('Ctrl Pts',(-6.78669743619696,12.2,9.26265166624004));
#241189=CARTESIAN_POINT('Ctrl Pts',(-6.79229326997229,12.2,9.26562092812853));
#241190=CARTESIAN_POINT('Ctrl Pts',(-6.79791095410398,12.2,9.26858815135357));
#241191=CARTESIAN_POINT('Ctrl Pts',(-6.80355049700006,12.2,9.27155330199999));
#241192=CARTESIAN_POINT('Ctrl Pts',(-7.10901226900006,15.2,9.03946594399999));
#241193=CARTESIAN_POINT('Ctrl Pts',(-7.10901226900006,11.6,9.03946594399999));
#241194=CARTESIAN_POINT('Ctrl Pts',(-7.10885083700005,15.2,9.03871859599998));
#241195=CARTESIAN_POINT('Ctrl Pts',(-7.10885083700005,11.6,9.03871859599998));
#241196=CARTESIAN_POINT('Ctrl Pts',(-7.10852778500006,15.2,9.03722439199999));
#241197=CARTESIAN_POINT('Ctrl Pts',(-7.10852778500006,11.6,9.03722439199999));
#241198=CARTESIAN_POINT('Ctrl Pts',(-7.10804264000005,15.2,9.03498456099998));
#241199=CARTESIAN_POINT('Ctrl Pts',(-7.10804264000005,11.6,9.03498456099998));
#241200=CARTESIAN_POINT('Ctrl Pts',(-7.10739465200006,15.2,9.03200107199999));
#241201=CARTESIAN_POINT('Ctrl Pts',(-7.10739465200006,11.6,9.03200107199999));
#241202=CARTESIAN_POINT('Ctrl Pts',(-7.10658278400006,15.2,9.02827662999999));
#241203=CARTESIAN_POINT('Ctrl Pts',(-7.10658278400006,11.6,9.02827662999999));
#241204=CARTESIAN_POINT('Ctrl Pts',(-7.10576903600006,15.2,9.02455710699999));
#241205=CARTESIAN_POINT('Ctrl Pts',(-7.10576903600006,11.6,9.02455710699999));
#241206=CARTESIAN_POINT('Ctrl Pts',(-7.10495340800006,15.2,9.02084250499998));
#241207=CARTESIAN_POINT('Ctrl Pts',(-7.10495340800006,11.6,9.02084250499998));
#241208=CARTESIAN_POINT('Ctrl Pts',(-7.10413590500006,15.2,9.01713282899999));
#241209=CARTESIAN_POINT('Ctrl Pts',(-7.10413590500006,11.6,9.01713282899999));
#241210=CARTESIAN_POINT('Ctrl Pts',(-7.10331652900006,15.2,9.01342808099999));
#241211=CARTESIAN_POINT('Ctrl Pts',(-7.10331652900006,11.6,9.01342808099999));
#241212=CARTESIAN_POINT('Ctrl Pts',(-7.10249528700006,15.2,9.00972826399999));
#241213=CARTESIAN_POINT('Ctrl Pts',(-7.10249528700006,11.6,9.00972826399999));
#241214=CARTESIAN_POINT('Ctrl Pts',(-7.10167218800006,15.2,9.00603338899998));
#241215=CARTESIAN_POINT('Ctrl Pts',(-7.10167218800006,11.6,9.00603338899998));
#241216=CARTESIAN_POINT('Ctrl Pts',(-7.10084724000006,15.2,9.00234345799999));
#241217=CARTESIAN_POINT('Ctrl Pts',(-7.10084724000006,11.6,9.00234345799999));
#241218=CARTESIAN_POINT('Ctrl Pts',(-7.10002045000006,15.2,8.99865848199998));
#241219=CARTESIAN_POINT('Ctrl Pts',(-7.10002045000006,11.6,8.99865848199998));
#241220=CARTESIAN_POINT('Ctrl Pts',(-7.09919183000006,15.2,8.99497846599999));
#241221=CARTESIAN_POINT('Ctrl Pts',(-7.09919183000006,11.6,8.99497846599999));
#241222=CARTESIAN_POINT('Ctrl Pts',(-7.09836138500005,15.2,8.99130341599999));
#241223=CARTESIAN_POINT('Ctrl Pts',(-7.09836138500005,11.6,8.99130341599999));
#241224=CARTESIAN_POINT('Ctrl Pts',(-7.09752912300006,15.2,8.98763333899998));
#241225=CARTESIAN_POINT('Ctrl Pts',(-7.09752912300006,11.6,8.98763333899998));
#241226=CARTESIAN_POINT('Ctrl Pts',(-7.09669505100006,15.2,8.98396823999999));
#241227=CARTESIAN_POINT('Ctrl Pts',(-7.09669505100006,11.6,8.98396823999999));
#241228=CARTESIAN_POINT('Ctrl Pts',(-7.09585917500006,15.2,8.98030812399998));
#241229=CARTESIAN_POINT('Ctrl Pts',(-7.09585917500006,11.6,8.98030812399998));
#241230=CARTESIAN_POINT('Ctrl Pts',(-7.09502150300006,15.2,8.97665299599998));
#241231=CARTESIAN_POINT('Ctrl Pts',(-7.09502150300006,11.6,8.97665299599998));
#241232=CARTESIAN_POINT('Ctrl Pts',(-7.09418204000006,15.2,8.97300286299998));
#241233=CARTESIAN_POINT('Ctrl Pts',(-7.09418204000006,11.6,8.97300286299998));
#241234=CARTESIAN_POINT('Ctrl Pts',(-7.09334079200006,15.2,8.96935772799999));
#241235=CARTESIAN_POINT('Ctrl Pts',(-7.09334079200006,11.6,8.96935772799999));
#241236=CARTESIAN_POINT('Ctrl Pts',(-7.09249776700006,15.2,8.96571759799999));
#241237=CARTESIAN_POINT('Ctrl Pts',(-7.09249776700006,11.6,8.96571759799999));
#241238=CARTESIAN_POINT('Ctrl Pts',(-7.09165297300006,15.2,8.96208247799999));
#241239=CARTESIAN_POINT('Ctrl Pts',(-7.09165297300006,11.6,8.96208247799999));
#241240=CARTESIAN_POINT('Ctrl Pts',(-7.09080641500006,15.2,8.95845237299999));
#241241=CARTESIAN_POINT('Ctrl Pts',(-7.09080641500006,11.6,8.95845237299999));
#241242=CARTESIAN_POINT('Ctrl Pts',(-7.08995810300006,15.2,8.95482729199998));
#241243=CARTESIAN_POINT('Ctrl Pts',(-7.08995810300006,11.6,8.95482729199998));
#241244=CARTESIAN_POINT('Ctrl Pts',(-7.08910804400006,15.2,8.95120723899998));
#241245=CARTESIAN_POINT('Ctrl Pts',(-7.08910804400006,11.6,8.95120723899998));
#241246=CARTESIAN_POINT('Ctrl Pts',(-7.08825624400006,15.2,8.94759221899999));
#241247=CARTESIAN_POINT('Ctrl Pts',(-7.08825624400006,11.6,8.94759221899999));
#241248=CARTESIAN_POINT('Ctrl Pts',(-7.08740271100006,15.2,8.94398223899999));
#241249=CARTESIAN_POINT('Ctrl Pts',(-7.08740271100006,11.6,8.94398223899999));
#241250=CARTESIAN_POINT('Ctrl Pts',(-7.08654745300006,15.2,8.94037730399998));
#241251=CARTESIAN_POINT('Ctrl Pts',(-7.08654745300006,11.6,8.94037730399998));
#241252=CARTESIAN_POINT('Ctrl Pts',(-7.08569047500006,15.2,8.93677742099998));
#241253=CARTESIAN_POINT('Ctrl Pts',(-7.08569047500006,11.6,8.93677742099998));
#241254=CARTESIAN_POINT('Ctrl Pts',(-7.08483178600006,15.2,8.93318259399998));
#241255=CARTESIAN_POINT('Ctrl Pts',(-7.08483178600006,11.6,8.93318259399998));
#241256=CARTESIAN_POINT('Ctrl Pts',(-7.08397139200006,15.2,8.92959282899999));
#241257=CARTESIAN_POINT('Ctrl Pts',(-7.08397139200006,11.6,8.92959282899999));
#241258=CARTESIAN_POINT('Ctrl Pts',(-7.08310930200006,15.2,8.92600813199999));
#241259=CARTESIAN_POINT('Ctrl Pts',(-7.08310930200006,11.6,8.92600813199999));
#241260=CARTESIAN_POINT('Ctrl Pts',(-7.08224552200006,15.2,8.92242850899999));
#241261=CARTESIAN_POINT('Ctrl Pts',(-7.08224552200006,11.6,8.92242850899999));
#241262=CARTESIAN_POINT('Ctrl Pts',(-7.08138005900006,15.2,8.91885396399999));
#241263=CARTESIAN_POINT('Ctrl Pts',(-7.08138005900006,11.6,8.91885396399999));
#241264=CARTESIAN_POINT('Ctrl Pts',(-7.08051292100006,15.2,8.91528450599999));
#241265=CARTESIAN_POINT('Ctrl Pts',(-7.08051292100006,11.6,8.91528450599999));
#241266=CARTESIAN_POINT('Ctrl Pts',(-7.07964411500006,15.2,8.91172013699999));
#241267=CARTESIAN_POINT('Ctrl Pts',(-7.07964411500006,11.6,8.91172013699999));
#241268=CARTESIAN_POINT('Ctrl Pts',(-7.07877364900006,15.2,8.90816086699999));
#241269=CARTESIAN_POINT('Ctrl Pts',(-7.07877364900006,11.6,8.90816086699999));
#241270=CARTESIAN_POINT('Ctrl Pts',(-7.07790153000006,15.2,8.90460669799998));
#241271=CARTESIAN_POINT('Ctrl Pts',(-7.07790153000006,11.6,8.90460669799998));
#241272=CARTESIAN_POINT('Ctrl Pts',(-7.07702776600006,15.2,8.90105763799999));
#241273=CARTESIAN_POINT('Ctrl Pts',(-7.07702776600006,11.6,8.90105763799999));
#241274=CARTESIAN_POINT('Ctrl Pts',(-7.07615236300006,15.2,8.89751369099999));
#241275=CARTESIAN_POINT('Ctrl Pts',(-7.07615236300006,11.6,8.89751369099999));
#241276=CARTESIAN_POINT('Ctrl Pts',(-7.07527533000006,15.2,8.89397486499998));
#241277=CARTESIAN_POINT('Ctrl Pts',(-7.07527533000006,11.6,8.89397486499998));
#241278=CARTESIAN_POINT('Ctrl Pts',(-7.07439667400006,15.2,8.89044116499999));
#241279=CARTESIAN_POINT('Ctrl Pts',(-7.07439667400006,11.6,8.89044116499999));
#241280=CARTESIAN_POINT('Ctrl Pts',(-7.07351640200006,15.2,8.88691259499998));
#241281=CARTESIAN_POINT('Ctrl Pts',(-7.07351640200006,11.6,8.88691259499998));
#241282=CARTESIAN_POINT('Ctrl Pts',(-7.07263452200006,15.2,8.88338916299999));
#241283=CARTESIAN_POINT('Ctrl Pts',(-7.07263452200006,11.6,8.88338916299999));
#241284=CARTESIAN_POINT('Ctrl Pts',(-7.07175104100005,15.2,8.87987087299998));
#241285=CARTESIAN_POINT('Ctrl Pts',(-7.07175104100005,11.6,8.87987087299998));
#241286=CARTESIAN_POINT('Ctrl Pts',(-7.07086596700006,15.2,8.87635773199998));
#241287=CARTESIAN_POINT('Ctrl Pts',(-7.07086596700006,11.6,8.87635773199998));
#241288=CARTESIAN_POINT('Ctrl Pts',(-7.06997930800005,15.2,8.87284974499998));
#241289=CARTESIAN_POINT('Ctrl Pts',(-7.06997930800005,11.6,8.87284974499998));
#241290=CARTESIAN_POINT('Ctrl Pts',(-7.06909107000006,15.2,8.86934691799999));
#241291=CARTESIAN_POINT('Ctrl Pts',(-7.06909107000006,11.6,8.86934691799999));
#241292=CARTESIAN_POINT('Ctrl Pts',(-7.06820126200006,15.2,8.86584925799998));
#241293=CARTESIAN_POINT('Ctrl Pts',(-7.06820126200006,11.6,8.86584925799998));
#241294=CARTESIAN_POINT('Ctrl Pts',(-7.06730989000006,15.2,8.86235676999998));
#241295=CARTESIAN_POINT('Ctrl Pts',(-7.06730989000006,11.6,8.86235676999998));
#241296=CARTESIAN_POINT('Ctrl Pts',(-7.06641696500006,15.2,8.85886945899999));
#241297=CARTESIAN_POINT('Ctrl Pts',(-7.06641696500006,11.6,8.85886945899999));
#241298=CARTESIAN_POINT('Ctrl Pts',(-7.06552249100006,15.2,8.85538733199999));
#241299=CARTESIAN_POINT('Ctrl Pts',(-7.06552249100006,11.6,8.85538733199999));
#241300=CARTESIAN_POINT('Ctrl Pts',(-7.06462647800006,15.2,8.85191039399999));
#241301=CARTESIAN_POINT('Ctrl Pts',(-7.06462647800006,11.6,8.85191039399999));
#241302=CARTESIAN_POINT('Ctrl Pts',(-7.06372893200006,15.2,8.84843865099998));
#241303=CARTESIAN_POINT('Ctrl Pts',(-7.06372893200006,11.6,8.84843865099998));
#241304=CARTESIAN_POINT('Ctrl Pts',(-7.06282986100006,15.2,8.84497210899998));
#241305=CARTESIAN_POINT('Ctrl Pts',(-7.06282986100006,11.6,8.84497210899998));
#241306=CARTESIAN_POINT('Ctrl Pts',(-7.06192927500005,15.2,8.84151077399999));
#241307=CARTESIAN_POINT('Ctrl Pts',(-7.06192927500005,11.6,8.84151077399999));
#241308=CARTESIAN_POINT('Ctrl Pts',(-7.06102717800006,15.2,8.83805465099999));
#241309=CARTESIAN_POINT('Ctrl Pts',(-7.06102717800006,11.6,8.83805465099999));
#241310=CARTESIAN_POINT('Ctrl Pts',(-7.06012358100006,15.2,8.83460374699998));
#241311=CARTESIAN_POINT('Ctrl Pts',(-7.06012358100006,11.6,8.83460374699998));
#241312=CARTESIAN_POINT('Ctrl Pts',(-7.05921849000006,15.2,8.83115806699998));
#241313=CARTESIAN_POINT('Ctrl Pts',(-7.05921849000006,11.6,8.83115806699998));
#241314=CARTESIAN_POINT('Ctrl Pts',(-7.05831191400006,15.2,8.82771761699999));
#241315=CARTESIAN_POINT('Ctrl Pts',(-7.05831191400006,11.6,8.82771761699999));
#241316=CARTESIAN_POINT('Ctrl Pts',(-7.05740385900006,15.2,8.82428240299999));
#241317=CARTESIAN_POINT('Ctrl Pts',(-7.05740385900006,11.6,8.82428240299999));
#241318=CARTESIAN_POINT('Ctrl Pts',(-7.05649433500006,15.2,8.82085243099999));
#241319=CARTESIAN_POINT('Ctrl Pts',(-7.05649433500006,11.6,8.82085243099999));
#241320=CARTESIAN_POINT('Ctrl Pts',(-7.05558334800005,15.2,8.81742770599999));
#241321=CARTESIAN_POINT('Ctrl Pts',(-7.05558334800005,11.6,8.81742770599999));
#241322=CARTESIAN_POINT('Ctrl Pts',(-7.05467090700005,15.2,8.81400823599999));
#241323=CARTESIAN_POINT('Ctrl Pts',(-7.05467090700005,11.6,8.81400823599999));
#241324=CARTESIAN_POINT('Ctrl Pts',(-7.05375701900006,15.2,8.81059402399998));
#241325=CARTESIAN_POINT('Ctrl Pts',(-7.05375701900006,11.6,8.81059402399998));
#241326=CARTESIAN_POINT('Ctrl Pts',(-7.05284169300006,15.2,8.80718507699999));
#241327=CARTESIAN_POINT('Ctrl Pts',(-7.05284169300006,11.6,8.80718507699999));
#241328=CARTESIAN_POINT('Ctrl Pts',(-7.05192493600006,15.2,8.80378140299998));
#241329=CARTESIAN_POINT('Ctrl Pts',(-7.05192493600006,11.6,8.80378140299998));
#241330=CARTESIAN_POINT('Ctrl Pts',(-7.05100675700006,15.2,8.80038300399999));
#241331=CARTESIAN_POINT('Ctrl Pts',(-7.05100675700006,11.6,8.80038300399999));
#241332=CARTESIAN_POINT('Ctrl Pts',(-7.05008716300005,15.2,8.79698988899998));
#241333=CARTESIAN_POINT('Ctrl Pts',(-7.05008716300005,11.6,8.79698988899998));
#241334=CARTESIAN_POINT('Ctrl Pts',(-7.04916616100006,15.2,8.79360206199999));
#241335=CARTESIAN_POINT('Ctrl Pts',(-7.04916616100006,11.6,8.79360206199999));
#241336=CARTESIAN_POINT('Ctrl Pts',(-7.04824376200006,15.2,8.79021952899999));
#241337=CARTESIAN_POINT('Ctrl Pts',(-7.04824376200006,11.6,8.79021952899999));
#241338=CARTESIAN_POINT('Ctrl Pts',(-7.04731997100006,15.2,8.78684229799998));
#241339=CARTESIAN_POINT('Ctrl Pts',(-7.04731997100006,11.6,8.78684229799998));
#241340=CARTESIAN_POINT('Ctrl Pts',(-7.04639479800006,15.2,8.78347037299999));
#241341=CARTESIAN_POINT('Ctrl Pts',(-7.04639479800006,11.6,8.78347037299999));
#241342=CARTESIAN_POINT('Ctrl Pts',(-7.04546825000006,15.2,8.78010376099999));
#241343=CARTESIAN_POINT('Ctrl Pts',(-7.04546825000006,11.6,8.78010376099999));
#241344=CARTESIAN_POINT('Ctrl Pts',(-7.04454033600006,15.2,8.77674246599998));
#241345=CARTESIAN_POINT('Ctrl Pts',(-7.04454033600006,11.6,8.77674246599998));
#241346=CARTESIAN_POINT('Ctrl Pts',(-7.04361106300006,15.2,8.77338649599999));
#241347=CARTESIAN_POINT('Ctrl Pts',(-7.04361106300006,11.6,8.77338649599999));
#241348=CARTESIAN_POINT('Ctrl Pts',(-7.04268044000006,15.2,8.77003585599999));
#241349=CARTESIAN_POINT('Ctrl Pts',(-7.04268044000006,11.6,8.77003585599999));
#241350=CARTESIAN_POINT('Ctrl Pts',(-7.04174847500005,15.2,8.76669055199999));
#241351=CARTESIAN_POINT('Ctrl Pts',(-7.04174847500005,11.6,8.76669055199999));
#241352=CARTESIAN_POINT('Ctrl Pts',(-7.04081517600006,15.2,8.76335058999998));
#241353=CARTESIAN_POINT('Ctrl Pts',(-7.04081517600006,11.6,8.76335058999998));
#241354=CARTESIAN_POINT('Ctrl Pts',(-7.03988055100006,15.2,8.76001597599998));
#241355=CARTESIAN_POINT('Ctrl Pts',(-7.03988055100006,11.6,8.76001597599998));
#241356=CARTESIAN_POINT('Ctrl Pts',(-7.03894460800006,15.2,8.75668671499999));
#241357=CARTESIAN_POINT('Ctrl Pts',(-7.03894460800006,11.6,8.75668671499999));
#241358=CARTESIAN_POINT('Ctrl Pts',(-7.03800735600006,15.2,8.75336281399999));
#241359=CARTESIAN_POINT('Ctrl Pts',(-7.03800735600006,11.6,8.75336281399999));
#241360=CARTESIAN_POINT('Ctrl Pts',(-7.03706880200006,15.2,8.75004427999999));
#241361=CARTESIAN_POINT('Ctrl Pts',(-7.03706880200006,11.6,8.75004427999999));
#241362=CARTESIAN_POINT('Ctrl Pts',(-7.03612895600005,15.2,8.74673111599999));
#241363=CARTESIAN_POINT('Ctrl Pts',(-7.03612895600005,11.6,8.74673111599999));
#241364=CARTESIAN_POINT('Ctrl Pts',(-7.03518782600006,15.2,8.74342332999999));
#241365=CARTESIAN_POINT('Ctrl Pts',(-7.03518782600006,11.6,8.74342332999999));
#241366=CARTESIAN_POINT('Ctrl Pts',(-7.03424541800006,15.2,8.74012092699999));
#241367=CARTESIAN_POINT('Ctrl Pts',(-7.03424541800006,11.6,8.74012092699999));
#241368=CARTESIAN_POINT('Ctrl Pts',(-7.03330174400006,15.2,8.73682391499998));
#241369=CARTESIAN_POINT('Ctrl Pts',(-7.03330174400006,11.6,8.73682391499998));
#241370=CARTESIAN_POINT('Ctrl Pts',(-7.03235680900006,15.2,8.73353229799999));
#241371=CARTESIAN_POINT('Ctrl Pts',(-7.03235680900006,11.6,8.73353229799999));
#241372=CARTESIAN_POINT('Ctrl Pts',(-7.03141062300006,15.2,8.73024608099998));
#241373=CARTESIAN_POINT('Ctrl Pts',(-7.03141062300006,11.6,8.73024608099998));
#241374=CARTESIAN_POINT('Ctrl Pts',(-7.03046319500006,15.2,8.72696527299999));
#241375=CARTESIAN_POINT('Ctrl Pts',(-7.03046319500006,11.6,8.72696527299999));
#241376=CARTESIAN_POINT('Ctrl Pts',(-7.02951453100006,15.2,8.72368987799998));
#241377=CARTESIAN_POINT('Ctrl Pts',(-7.02951453100006,11.6,8.72368987799998));
#241378=CARTESIAN_POINT('Ctrl Pts',(-7.02856464100006,15.2,8.72041990199998));
#241379=CARTESIAN_POINT('Ctrl Pts',(-7.02856464100006,11.6,8.72041990199998));
#241380=CARTESIAN_POINT('Ctrl Pts',(-7.02761353400006,15.2,8.71715535199998));
#241381=CARTESIAN_POINT('Ctrl Pts',(-7.02761353400006,11.6,8.71715535199998));
#241382=CARTESIAN_POINT('Ctrl Pts',(-7.02666121800006,15.2,8.71389623299999));
#241383=CARTESIAN_POINT('Ctrl Pts',(-7.02666121800006,11.6,8.71389623299999));
#241384=CARTESIAN_POINT('Ctrl Pts',(-7.02570770200006,15.2,8.71064255199999));
#241385=CARTESIAN_POINT('Ctrl Pts',(-7.02570770200006,11.6,8.71064255199999));
#241386=CARTESIAN_POINT('Ctrl Pts',(-7.02475299300006,15.2,8.70739431299998));
#241387=CARTESIAN_POINT('Ctrl Pts',(-7.02475299300006,11.6,8.70739431299998));
#241388=CARTESIAN_POINT('Ctrl Pts',(-7.02379710000006,15.2,8.70415152399998));
#241389=CARTESIAN_POINT('Ctrl Pts',(-7.02379710000006,11.6,8.70415152399998));
#241390=CARTESIAN_POINT('Ctrl Pts',(-7.02284003300006,15.2,8.70091419099998));
#241391=CARTESIAN_POINT('Ctrl Pts',(-7.02284003300006,11.6,8.70091419099998));
#241392=CARTESIAN_POINT('Ctrl Pts',(-7.02188179900006,15.2,8.69768231899998));
#241393=CARTESIAN_POINT('Ctrl Pts',(-7.02188179900006,11.6,8.69768231899998));
#241394=CARTESIAN_POINT('Ctrl Pts',(-7.02092240700006,15.2,8.69445591399998));
#241395=CARTESIAN_POINT('Ctrl Pts',(-7.02092240700006,11.6,8.69445591399998));
#241396=CARTESIAN_POINT('Ctrl Pts',(-7.01996186600006,15.2,8.69123498299999));
#241397=CARTESIAN_POINT('Ctrl Pts',(-7.01996186600006,11.6,8.69123498299999));
#241398=CARTESIAN_POINT('Ctrl Pts',(-7.01900018300006,15.2,8.68801953099998));
#241399=CARTESIAN_POINT('Ctrl Pts',(-7.01900018300006,11.6,8.68801953099998));
#241400=CARTESIAN_POINT('Ctrl Pts',(-7.01803737000006,15.2,8.68480956499998));
#241401=CARTESIAN_POINT('Ctrl Pts',(-7.01803737000006,11.6,8.68480956499998));
#241402=CARTESIAN_POINT('Ctrl Pts',(-7.01707343300006,15.2,8.68160509099998));
#241403=CARTESIAN_POINT('Ctrl Pts',(-7.01707343300006,11.6,8.68160509099998));
#241404=CARTESIAN_POINT('Ctrl Pts',(-7.01610838200006,15.2,8.67840611399998));
#241405=CARTESIAN_POINT('Ctrl Pts',(-7.01610838200006,11.6,8.67840611399998));
#241406=CARTESIAN_POINT('Ctrl Pts',(-7.01514222400006,15.2,8.67521264099998));
#241407=CARTESIAN_POINT('Ctrl Pts',(-7.01514222400006,11.6,8.67521264099998));
#241408=CARTESIAN_POINT('Ctrl Pts',(-7.01417497000006,15.2,8.67202467699999));
#241409=CARTESIAN_POINT('Ctrl Pts',(-7.01417497000006,11.6,8.67202467699999));
#241410=CARTESIAN_POINT('Ctrl Pts',(-7.01320662700006,15.2,8.66884222899999));
#241411=CARTESIAN_POINT('Ctrl Pts',(-7.01320662700006,11.6,8.66884222899999));
#241412=CARTESIAN_POINT('Ctrl Pts',(-7.01223720400006,15.2,8.66566530299998));
#241413=CARTESIAN_POINT('Ctrl Pts',(-7.01223720400006,11.6,8.66566530299998));
#241414=CARTESIAN_POINT('Ctrl Pts',(-7.01126671200006,15.2,8.66249390599998));
#241415=CARTESIAN_POINT('Ctrl Pts',(-7.01126671200006,11.6,8.66249390599998));
#241416=CARTESIAN_POINT('Ctrl Pts',(-7.01029515700006,15.2,8.65932804199998));
#241417=CARTESIAN_POINT('Ctrl Pts',(-7.01029515700006,11.6,8.65932804199998));
#241418=CARTESIAN_POINT('Ctrl Pts',(-7.00932254900006,15.2,8.65616771799999));
#241419=CARTESIAN_POINT('Ctrl Pts',(-7.00932254900006,11.6,8.65616771799999));
#241420=CARTESIAN_POINT('Ctrl Pts',(-7.00834889700006,15.2,8.65301293999998));
#241421=CARTESIAN_POINT('Ctrl Pts',(-7.00834889700006,11.6,8.65301293999998));
#241422=CARTESIAN_POINT('Ctrl Pts',(-7.00737421000006,15.2,8.64986371499998));
#241423=CARTESIAN_POINT('Ctrl Pts',(-7.00737421000006,11.6,8.64986371499998));
#241424=CARTESIAN_POINT('Ctrl Pts',(-7.00639849600006,15.2,8.64672004799999));
#241425=CARTESIAN_POINT('Ctrl Pts',(-7.00639849600006,11.6,8.64672004799999));
#241426=CARTESIAN_POINT('Ctrl Pts',(-7.00542176600006,15.2,8.64358194499999));
#241427=CARTESIAN_POINT('Ctrl Pts',(-7.00542176600006,11.6,8.64358194499999));
#241428=CARTESIAN_POINT('Ctrl Pts',(-7.00444402700006,15.2,8.64044941399998));
#241429=CARTESIAN_POINT('Ctrl Pts',(-7.00444402700006,11.6,8.64044941399998));
#241430=CARTESIAN_POINT('Ctrl Pts',(-7.00346528800006,15.2,8.63732245899998));
#241431=CARTESIAN_POINT('Ctrl Pts',(-7.00346528800006,11.6,8.63732245899998));
#241432=CARTESIAN_POINT('Ctrl Pts',(-7.00248556000005,15.2,8.63420108599998));
#241433=CARTESIAN_POINT('Ctrl Pts',(-7.00248556000005,11.6,8.63420108599998));
#241434=CARTESIAN_POINT('Ctrl Pts',(-7.00150484900006,15.2,8.63108530299998));
#241435=CARTESIAN_POINT('Ctrl Pts',(-7.00150484900006,11.6,8.63108530299998));
#241436=CARTESIAN_POINT('Ctrl Pts',(-7.00052316800006,15.2,8.62797511399998));
#241437=CARTESIAN_POINT('Ctrl Pts',(-7.00052316800006,11.6,8.62797511399998));
#241438=CARTESIAN_POINT('Ctrl Pts',(-6.99954052300006,15.2,8.62487052699999));
#241439=CARTESIAN_POINT('Ctrl Pts',(-6.99954052300006,11.6,8.62487052699999));
#241440=CARTESIAN_POINT('Ctrl Pts',(-6.99855692300006,15.2,8.62177154799999));
#241441=CARTESIAN_POINT('Ctrl Pts',(-6.99855692300006,11.6,8.62177154799999));
#241442=CARTESIAN_POINT('Ctrl Pts',(-6.99757237900006,15.2,8.61867818099999));
#241443=CARTESIAN_POINT('Ctrl Pts',(-6.99757237900006,11.6,8.61867818099999));
#241444=CARTESIAN_POINT('Ctrl Pts',(-6.99658689800006,15.2,8.61559043399998));
#241445=CARTESIAN_POINT('Ctrl Pts',(-6.99658689800006,11.6,8.61559043399998));
#241446=CARTESIAN_POINT('Ctrl Pts',(-6.99560049200006,15.2,8.61250831299999));
#241447=CARTESIAN_POINT('Ctrl Pts',(-6.99560049200006,11.6,8.61250831299999));
#241448=CARTESIAN_POINT('Ctrl Pts',(-6.99461316900006,15.2,8.60943182499998));
#241449=CARTESIAN_POINT('Ctrl Pts',(-6.99461316900006,11.6,8.60943182499998));
#241450=CARTESIAN_POINT('Ctrl Pts',(-6.99362493700006,15.2,8.60636097399999));
#241451=CARTESIAN_POINT('Ctrl Pts',(-6.99362493700006,11.6,8.60636097399999));
#241452=CARTESIAN_POINT('Ctrl Pts',(-6.99263580600006,15.2,8.60329576699998));
#241453=CARTESIAN_POINT('Ctrl Pts',(-6.99263580600006,11.6,8.60329576699998));
#241454=CARTESIAN_POINT('Ctrl Pts',(-6.99164578600006,15.2,8.60023621099998));
#241455=CARTESIAN_POINT('Ctrl Pts',(-6.99164578600006,11.6,8.60023621099998));
#241456=CARTESIAN_POINT('Ctrl Pts',(-6.99065488600006,15.2,8.59718231199999));
#241457=CARTESIAN_POINT('Ctrl Pts',(-6.99065488600006,11.6,8.59718231199999));
#241458=CARTESIAN_POINT('Ctrl Pts',(-6.98966311500006,15.2,8.59413407599998));
#241459=CARTESIAN_POINT('Ctrl Pts',(-6.98966311500006,11.6,8.59413407599998));
#241460=CARTESIAN_POINT('Ctrl Pts',(-6.98867048100006,15.2,8.59109150799998));
#241461=CARTESIAN_POINT('Ctrl Pts',(-6.98867048100006,11.6,8.59109150799998));
#241462=CARTESIAN_POINT('Ctrl Pts',(-6.98767699600006,15.2,8.58805461599999));
#241463=CARTESIAN_POINT('Ctrl Pts',(-6.98767699600006,11.6,8.58805461599999));
#241464=CARTESIAN_POINT('Ctrl Pts',(-6.98668266900006,15.2,8.58502340599999));
#241465=CARTESIAN_POINT('Ctrl Pts',(-6.98668266900006,11.6,8.58502340599999));
#241466=CARTESIAN_POINT('Ctrl Pts',(-6.98568750700006,15.2,8.58199788299999));
#241467=CARTESIAN_POINT('Ctrl Pts',(-6.98568750700006,11.6,8.58199788299999));
#241468=CARTESIAN_POINT('Ctrl Pts',(-6.98469152300006,15.2,8.57897805299999));
#241469=CARTESIAN_POINT('Ctrl Pts',(-6.98469152300006,11.6,8.57897805299999));
#241470=CARTESIAN_POINT('Ctrl Pts',(-6.98369472300006,15.2,8.57596392499998));
#241471=CARTESIAN_POINT('Ctrl Pts',(-6.98369472300006,11.6,8.57596392499998));
#241472=CARTESIAN_POINT('Ctrl Pts',(-6.98269711900006,15.2,8.57295550199999));
#241473=CARTESIAN_POINT('Ctrl Pts',(-6.98269711900006,11.6,8.57295550199999));
#241474=CARTESIAN_POINT('Ctrl Pts',(-6.98169871800006,15.2,8.56995279199998));
#241475=CARTESIAN_POINT('Ctrl Pts',(-6.98169871800006,11.6,8.56995279199998));
#241476=CARTESIAN_POINT('Ctrl Pts',(-6.98069953300006,15.2,8.56695580099998));
#241477=CARTESIAN_POINT('Ctrl Pts',(-6.98069953300006,11.6,8.56695580099998));
#241478=CARTESIAN_POINT('Ctrl Pts',(-6.97969957100006,15.2,8.56396453399999));
#241479=CARTESIAN_POINT('Ctrl Pts',(-6.97969957100006,11.6,8.56396453399999));
#241480=CARTESIAN_POINT('Ctrl Pts',(-6.97869884300006,15.2,8.56097899899999));
#241481=CARTESIAN_POINT('Ctrl Pts',(-6.97869884300006,11.6,8.56097899899999));
#241482=CARTESIAN_POINT('Ctrl Pts',(-6.97769735700006,15.2,8.55799920099999));
#241483=CARTESIAN_POINT('Ctrl Pts',(-6.97769735700006,11.6,8.55799920099999));
#241484=CARTESIAN_POINT('Ctrl Pts',(-6.97669512400005,15.2,8.55502514799999));
#241485=CARTESIAN_POINT('Ctrl Pts',(-6.97669512400005,11.6,8.55502514799999));
#241486=CARTESIAN_POINT('Ctrl Pts',(-6.97569215400006,15.2,8.55205684399999));
#241487=CARTESIAN_POINT('Ctrl Pts',(-6.97569215400006,11.6,8.55205684399999));
#241488=CARTESIAN_POINT('Ctrl Pts',(-6.97468845400006,15.2,8.54909429699998));
#241489=CARTESIAN_POINT('Ctrl Pts',(-6.97468845400006,11.6,8.54909429699998));
#241490=CARTESIAN_POINT('Ctrl Pts',(-6.97368403800006,15.2,8.54613751299999));
#241491=CARTESIAN_POINT('Ctrl Pts',(-6.97368403800006,11.6,8.54613751299999));
#241492=CARTESIAN_POINT('Ctrl Pts',(-6.97267891300006,15.2,8.54318649699999));
#241493=CARTESIAN_POINT('Ctrl Pts',(-6.97267891300006,11.6,8.54318649699999));
#241494=CARTESIAN_POINT('Ctrl Pts',(-6.97167308800006,15.2,8.54024125799998));
#241495=CARTESIAN_POINT('Ctrl Pts',(-6.97167308800006,11.6,8.54024125799998));
#241496=CARTESIAN_POINT('Ctrl Pts',(-6.97066657500006,15.2,8.53730179799999));
#241497=CARTESIAN_POINT('Ctrl Pts',(-6.97066657500006,11.6,8.53730179799999));
#241498=CARTESIAN_POINT('Ctrl Pts',(-6.96965938300006,15.2,8.53436812799998));
#241499=CARTESIAN_POINT('Ctrl Pts',(-6.96965938300006,11.6,8.53436812799998));
#241500=CARTESIAN_POINT('Ctrl Pts',(-6.96865152100006,15.2,8.53144025099999));
#241501=CARTESIAN_POINT('Ctrl Pts',(-6.96865152100006,11.6,8.53144025099999));
#241502=CARTESIAN_POINT('Ctrl Pts',(-6.96764300000006,15.2,8.52851817499998));
#241503=CARTESIAN_POINT('Ctrl Pts',(-6.96764300000006,11.6,8.52851817499998));
#241504=CARTESIAN_POINT('Ctrl Pts',(-6.96663383000006,15.2,8.52560190499998));
#241505=CARTESIAN_POINT('Ctrl Pts',(-6.96663383000006,11.6,8.52560190499998));
#241506=CARTESIAN_POINT('Ctrl Pts',(-6.96562402000006,15.2,8.52269144799998));
#241507=CARTESIAN_POINT('Ctrl Pts',(-6.96562402000006,11.6,8.52269144799998));
#241508=CARTESIAN_POINT('Ctrl Pts',(-6.96461358100006,15.2,8.51978681099999));
#241509=CARTESIAN_POINT('Ctrl Pts',(-6.96461358100006,11.6,8.51978681099999));
#241510=CARTESIAN_POINT('Ctrl Pts',(-6.96360252100006,15.2,8.51688799899998));
#241511=CARTESIAN_POINT('Ctrl Pts',(-6.96360252100006,11.6,8.51688799899998));
#241512=CARTESIAN_POINT('Ctrl Pts',(-6.96259085300006,15.2,8.51399501999998));
#241513=CARTESIAN_POINT('Ctrl Pts',(-6.96259085300006,11.6,8.51399501999998));
#241514=CARTESIAN_POINT('Ctrl Pts',(-6.96157858500006,15.2,8.51110787899999));
#241515=CARTESIAN_POINT('Ctrl Pts',(-6.96157858500006,11.6,8.51110787899999));
#241516=CARTESIAN_POINT('Ctrl Pts',(-6.96056572800006,15.2,8.50822658299998));
#241517=CARTESIAN_POINT('Ctrl Pts',(-6.96056572800006,11.6,8.50822658299998));
#241518=CARTESIAN_POINT('Ctrl Pts',(-6.95955229200006,15.2,8.50535113899999));
#241519=CARTESIAN_POINT('Ctrl Pts',(-6.95955229200006,11.6,8.50535113899999));
#241520=CARTESIAN_POINT('Ctrl Pts',(-6.95853828500006,15.2,8.50248155199999));
#241521=CARTESIAN_POINT('Ctrl Pts',(-6.95853828500006,11.6,8.50248155199999));
#241522=CARTESIAN_POINT('Ctrl Pts',(-6.95752372100006,15.2,8.49961782899998));
#241523=CARTESIAN_POINT('Ctrl Pts',(-6.95752372100006,11.6,8.49961782899998));
#241524=CARTESIAN_POINT('Ctrl Pts',(-6.95650860700006,15.2,8.49675997499999));
#241525=CARTESIAN_POINT('Ctrl Pts',(-6.95650860700006,11.6,8.49675997499999));
#241526=CARTESIAN_POINT('Ctrl Pts',(-6.95549295500006,15.2,8.49390799999998));
#241527=CARTESIAN_POINT('Ctrl Pts',(-6.95549295500006,11.6,8.49390799999998));
#241528=CARTESIAN_POINT('Ctrl Pts',(-6.95447677300006,15.2,8.49106190699998));
#241529=CARTESIAN_POINT('Ctrl Pts',(-6.95447677300006,11.6,8.49106190699998));
#241530=CARTESIAN_POINT('Ctrl Pts',(-6.95346007500006,15.2,8.48822170299999));
#241531=CARTESIAN_POINT('Ctrl Pts',(-6.95346007500006,11.6,8.48822170299999));
#241532=CARTESIAN_POINT('Ctrl Pts',(-6.95244286800006,15.2,8.48538739599999));
#241533=CARTESIAN_POINT('Ctrl Pts',(-6.95244286800006,11.6,8.48538739599999));
#241534=CARTESIAN_POINT('Ctrl Pts',(-6.95142516400006,15.2,8.48255898999999));
#241535=CARTESIAN_POINT('Ctrl Pts',(-6.95142516400006,11.6,8.48255898999999));
#241536=CARTESIAN_POINT('Ctrl Pts',(-6.95040697200006,15.2,8.47973649399999));
#241537=CARTESIAN_POINT('Ctrl Pts',(-6.95040697200006,11.6,8.47973649399999));
#241538=CARTESIAN_POINT('Ctrl Pts',(-6.94938830500006,15.2,8.47691991299998));
#241539=CARTESIAN_POINT('Ctrl Pts',(-6.94938830500006,11.6,8.47691991299998));
#241540=CARTESIAN_POINT('Ctrl Pts',(-6.94836917000006,15.2,8.47410925299998));
#241541=CARTESIAN_POINT('Ctrl Pts',(-6.94836917000006,11.6,8.47410925299998));
#241542=CARTESIAN_POINT('Ctrl Pts',(-6.94734957900006,15.2,8.47130452199998));
#241543=CARTESIAN_POINT('Ctrl Pts',(-6.94734957900006,11.6,8.47130452199998));
#241544=CARTESIAN_POINT('Ctrl Pts',(-6.94632954300006,15.2,8.46850572499999));
#241545=CARTESIAN_POINT('Ctrl Pts',(-6.94632954300006,11.6,8.46850572499999));
#241546=CARTESIAN_POINT('Ctrl Pts',(-6.94530907200006,15.2,8.46571286899999));
#241547=CARTESIAN_POINT('Ctrl Pts',(-6.94530907200006,11.6,8.46571286899999));
#241548=CARTESIAN_POINT('Ctrl Pts',(-6.94428817600006,15.2,8.46292595999999));
#241549=CARTESIAN_POINT('Ctrl Pts',(-6.94428817600006,11.6,8.46292595999999));
#241550=CARTESIAN_POINT('Ctrl Pts',(-6.94326686700006,15.2,8.46014500499999));
#241551=CARTESIAN_POINT('Ctrl Pts',(-6.94326686700006,11.6,8.46014500499999));
#241552=CARTESIAN_POINT('Ctrl Pts',(-6.94224515500006,15.2,8.45737001099998));
#241553=CARTESIAN_POINT('Ctrl Pts',(-6.94224515500006,11.6,8.45737001099998));
#241554=CARTESIAN_POINT('Ctrl Pts',(-6.94122304900006,15.2,8.45460098399998));
#241555=CARTESIAN_POINT('Ctrl Pts',(-6.94122304900006,11.6,8.45460098399998));
#241556=CARTESIAN_POINT('Ctrl Pts',(-6.94020056100006,15.2,8.45183792999999));
#241557=CARTESIAN_POINT('Ctrl Pts',(-6.94020056100006,11.6,8.45183792999999));
#241558=CARTESIAN_POINT('Ctrl Pts',(-6.93917770200006,15.2,8.44908085699998));
#241559=CARTESIAN_POINT('Ctrl Pts',(-6.93917770200006,11.6,8.44908085699998));
#241560=CARTESIAN_POINT('Ctrl Pts',(-6.93815448200006,15.2,8.44632976799998));
#241561=CARTESIAN_POINT('Ctrl Pts',(-6.93815448200006,11.6,8.44632976799998));
#241562=CARTESIAN_POINT('Ctrl Pts',(-6.93713091200006,15.2,8.44358467399999));
#241563=CARTESIAN_POINT('Ctrl Pts',(-6.93713091200006,11.6,8.44358467399999));
#241564=CARTESIAN_POINT('Ctrl Pts',(-6.93610700300006,15.2,8.44084557799999));
#241565=CARTESIAN_POINT('Ctrl Pts',(-6.93610700300006,11.6,8.44084557799999));
#241566=CARTESIAN_POINT('Ctrl Pts',(-6.93508276600006,15.2,8.43811248899998));
#241567=CARTESIAN_POINT('Ctrl Pts',(-6.93508276600006,11.6,8.43811248899998));
#241568=CARTESIAN_POINT('Ctrl Pts',(-6.93405821100006,15.2,8.43538541199998));
#241569=CARTESIAN_POINT('Ctrl Pts',(-6.93405821100006,11.6,8.43538541199998));
#241570=CARTESIAN_POINT('Ctrl Pts',(-6.93303334800006,15.2,8.43266435399999));
#241571=CARTESIAN_POINT('Ctrl Pts',(-6.93303334800006,11.6,8.43266435399999));
#241572=CARTESIAN_POINT('Ctrl Pts',(-6.93200819100006,15.2,8.42994932099998));
#241573=CARTESIAN_POINT('Ctrl Pts',(-6.93200819100006,11.6,8.42994932099998));
#241574=CARTESIAN_POINT('Ctrl Pts',(-6.93098274800006,15.2,8.42724032099999));
#241575=CARTESIAN_POINT('Ctrl Pts',(-6.93098274800006,11.6,8.42724032099999));
#241576=CARTESIAN_POINT('Ctrl Pts',(-6.92995703100006,15.2,8.42453735999998));
#241577=CARTESIAN_POINT('Ctrl Pts',(-6.92995703100006,11.6,8.42453735999998));
#241578=CARTESIAN_POINT('Ctrl Pts',(-6.92893105100006,15.2,8.42184044299999));
#241579=CARTESIAN_POINT('Ctrl Pts',(-6.92893105100006,11.6,8.42184044299999));
#241580=CARTESIAN_POINT('Ctrl Pts',(-6.92790481800006,15.2,8.41914957799998));
#241581=CARTESIAN_POINT('Ctrl Pts',(-6.92790481800006,11.6,8.41914957799998));
#241582=CARTESIAN_POINT('Ctrl Pts',(-6.92687834600005,15.2,8.41646477099999));
#241583=CARTESIAN_POINT('Ctrl Pts',(-6.92687834600005,11.6,8.41646477099999));
#241584=CARTESIAN_POINT('Ctrl Pts',(-6.92585164200006,15.2,8.41378602999999));
#241585=CARTESIAN_POINT('Ctrl Pts',(-6.92585164200006,11.6,8.41378602999999));
#241586=CARTESIAN_POINT('Ctrl Pts',(-6.92482471900006,15.2,8.41111335999998));
#241587=CARTESIAN_POINT('Ctrl Pts',(-6.92482471900006,11.6,8.41111335999998));
#241588=CARTESIAN_POINT('Ctrl Pts',(-6.92379759000006,15.2,8.40844676899999));
#241589=CARTESIAN_POINT('Ctrl Pts',(-6.92379759000006,11.6,8.40844676899999));
#241590=CARTESIAN_POINT('Ctrl Pts',(-6.92277026400006,15.2,8.40578626199999));
#241591=CARTESIAN_POINT('Ctrl Pts',(-6.92277026400006,11.6,8.40578626199999));
#241592=CARTESIAN_POINT('Ctrl Pts',(-6.92174275100006,15.2,8.40313184599999));
#241593=CARTESIAN_POINT('Ctrl Pts',(-6.92174275100006,11.6,8.40313184599999));
#241594=CARTESIAN_POINT('Ctrl Pts',(-6.92071506500006,15.2,8.40048352999998));
#241595=CARTESIAN_POINT('Ctrl Pts',(-6.92071506500006,11.6,8.40048352999998));
#241596=CARTESIAN_POINT('Ctrl Pts',(-6.91968721600006,15.2,8.39784131699999));
#241597=CARTESIAN_POINT('Ctrl Pts',(-6.91968721600006,11.6,8.39784131699999));
#241598=CARTESIAN_POINT('Ctrl Pts',(-6.91865921500006,15.2,8.39520521599999));
#241599=CARTESIAN_POINT('Ctrl Pts',(-6.91865921500006,11.6,8.39520521599999));
#241600=CARTESIAN_POINT('Ctrl Pts',(-6.91763107300006,15.2,8.39257523199999));
#241601=CARTESIAN_POINT('Ctrl Pts',(-6.91763107300006,11.6,8.39257523199999));
#241602=CARTESIAN_POINT('Ctrl Pts',(-6.91660280300006,15.2,8.38995137299998));
#241603=CARTESIAN_POINT('Ctrl Pts',(-6.91660280300006,11.6,8.38995137299998));
#241604=CARTESIAN_POINT('Ctrl Pts',(-6.91557441500006,15.2,8.38733364499999));
#241605=CARTESIAN_POINT('Ctrl Pts',(-6.91557441500006,11.6,8.38733364499999));
#241606=CARTESIAN_POINT('Ctrl Pts',(-6.91454592100006,15.2,8.38472205599999));
#241607=CARTESIAN_POINT('Ctrl Pts',(-6.91454592100006,11.6,8.38472205599999));
#241608=CARTESIAN_POINT('Ctrl Pts',(-6.91351733200006,15.2,8.38211661099999));
#241609=CARTESIAN_POINT('Ctrl Pts',(-6.91351733200006,11.6,8.38211661099999));
#241610=CARTESIAN_POINT('Ctrl Pts',(-6.91248866000006,15.2,8.37951731799999));
#241611=CARTESIAN_POINT('Ctrl Pts',(-6.91248866000006,11.6,8.37951731799999));
#241612=CARTESIAN_POINT('Ctrl Pts',(-6.91145991600006,15.2,8.37692418199998));
#241613=CARTESIAN_POINT('Ctrl Pts',(-6.91145991600006,11.6,8.37692418199998));
#241614=CARTESIAN_POINT('Ctrl Pts',(-6.91043111200006,15.2,8.37433721099998));
#241615=CARTESIAN_POINT('Ctrl Pts',(-6.91043111200006,11.6,8.37433721099998));
#241616=CARTESIAN_POINT('Ctrl Pts',(-6.90940225900006,15.2,8.37175641099999));
#241617=CARTESIAN_POINT('Ctrl Pts',(-6.90940225900006,11.6,8.37175641099999));
#241618=CARTESIAN_POINT('Ctrl Pts',(-6.90837336900006,15.2,8.36918178999999));
#241619=CARTESIAN_POINT('Ctrl Pts',(-6.90837336900006,11.6,8.36918178999999));
#241620=CARTESIAN_POINT('Ctrl Pts',(-6.90734445400006,15.2,8.36661335399998));
#241621=CARTESIAN_POINT('Ctrl Pts',(-6.90734445400006,11.6,8.36661335399998));
#241622=CARTESIAN_POINT('Ctrl Pts',(-6.90631552400006,15.2,8.36405110899998));
#241623=CARTESIAN_POINT('Ctrl Pts',(-6.90631552400006,11.6,8.36405110899998));
#241624=CARTESIAN_POINT('Ctrl Pts',(-6.90528659400006,15.2,8.36149506199998));
#241625=CARTESIAN_POINT('Ctrl Pts',(-6.90528659400006,11.6,8.36149506199998));
#241626=CARTESIAN_POINT('Ctrl Pts',(-6.90425767200006,15.2,8.35894522099998));
#241627=CARTESIAN_POINT('Ctrl Pts',(-6.90425767200006,11.6,8.35894522099998));
#241628=CARTESIAN_POINT('Ctrl Pts',(-6.90322877200006,15.2,8.35640159099999));
#241629=CARTESIAN_POINT('Ctrl Pts',(-6.90322877200006,11.6,8.35640159099999));
#241630=CARTESIAN_POINT('Ctrl Pts',(-6.90219990600006,15.2,8.35386418099999));
#241631=CARTESIAN_POINT('Ctrl Pts',(-6.90219990600006,11.6,8.35386418099999));
#241632=CARTESIAN_POINT('Ctrl Pts',(-6.90117108500006,15.2,8.35133299499999));
#241633=CARTESIAN_POINT('Ctrl Pts',(-6.90117108500006,11.6,8.35133299499999));
#241634=CARTESIAN_POINT('Ctrl Pts',(-6.90014232100006,15.2,8.34880804199998));
#241635=CARTESIAN_POINT('Ctrl Pts',(-6.90014232100006,11.6,8.34880804199998));
#241636=CARTESIAN_POINT('Ctrl Pts',(-6.89911362600006,15.2,8.34628932799999));
#241637=CARTESIAN_POINT('Ctrl Pts',(-6.89911362600006,11.6,8.34628932799999));
#241638=CARTESIAN_POINT('Ctrl Pts',(-6.89808501200006,15.2,8.34377685899998));
#241639=CARTESIAN_POINT('Ctrl Pts',(-6.89808501200006,11.6,8.34377685899998));
#241640=CARTESIAN_POINT('Ctrl Pts',(-6.89705649000006,15.2,8.34127064299999));
#241641=CARTESIAN_POINT('Ctrl Pts',(-6.89705649000006,11.6,8.34127064299999));
#241642=CARTESIAN_POINT('Ctrl Pts',(-6.89602807500005,15.2,8.33877068699999));
#241643=CARTESIAN_POINT('Ctrl Pts',(-6.89602807500005,11.6,8.33877068699999));
#241644=CARTESIAN_POINT('Ctrl Pts',(-6.89499977500006,15.2,8.33627699599998));
#241645=CARTESIAN_POINT('Ctrl Pts',(-6.89499977500006,11.6,8.33627699599998));
#241646=CARTESIAN_POINT('Ctrl Pts',(-6.89397160500006,15.2,8.33378957899999));
#241647=CARTESIAN_POINT('Ctrl Pts',(-6.89397160500006,11.6,8.33378957899999));
#241648=CARTESIAN_POINT('Ctrl Pts',(-6.89294357700006,15.2,8.33130844199999));
#241649=CARTESIAN_POINT('Ctrl Pts',(-6.89294357700006,11.6,8.33130844199999));
#241650=CARTESIAN_POINT('Ctrl Pts',(-6.89191570200006,15.2,8.32883359199998));
#241651=CARTESIAN_POINT('Ctrl Pts',(-6.89191570200006,11.6,8.32883359199998));
#241652=CARTESIAN_POINT('Ctrl Pts',(-6.89088799300006,15.2,8.32636503499998));
#241653=CARTESIAN_POINT('Ctrl Pts',(-6.89088799300006,11.6,8.32636503499998));
#241654=CARTESIAN_POINT('Ctrl Pts',(-6.88986046100006,15.2,8.32390277899999));
#241655=CARTESIAN_POINT('Ctrl Pts',(-6.88986046100006,11.6,8.32390277899999));
#241656=CARTESIAN_POINT('Ctrl Pts',(-6.88883312000006,15.2,8.32144682999999));
#241657=CARTESIAN_POINT('Ctrl Pts',(-6.88883312000006,11.6,8.32144682999999));
#241658=CARTESIAN_POINT('Ctrl Pts',(-6.88780598100006,15.2,8.31899719499999));
#241659=CARTESIAN_POINT('Ctrl Pts',(-6.88780598100006,11.6,8.31899719499999));
#241660=CARTESIAN_POINT('Ctrl Pts',(-6.88677905700006,15.2,8.31655388199999));
#241661=CARTESIAN_POINT('Ctrl Pts',(-6.88677905700006,11.6,8.31655388199999));
#241662=CARTESIAN_POINT('Ctrl Pts',(-6.88575236000006,15.2,8.31411689699999));
#241663=CARTESIAN_POINT('Ctrl Pts',(-6.88575236000006,11.6,8.31411689699999));
#241664=CARTESIAN_POINT('Ctrl Pts',(-6.88472590400006,15.2,8.31168624599999));
#241665=CARTESIAN_POINT('Ctrl Pts',(-6.88472590400006,11.6,8.31168624599999));
#241666=CARTESIAN_POINT('Ctrl Pts',(-6.88369969900006,15.2,8.30926193799998));
#241667=CARTESIAN_POINT('Ctrl Pts',(-6.88369969900006,11.6,8.30926193799998));
#241668=CARTESIAN_POINT('Ctrl Pts',(-6.88267376000006,15.2,8.30684397899999));
#241669=CARTESIAN_POINT('Ctrl Pts',(-6.88267376000006,11.6,8.30684397899999));
#241670=CARTESIAN_POINT('Ctrl Pts',(-6.88164809600006,15.2,8.30443237499999));
#241671=CARTESIAN_POINT('Ctrl Pts',(-6.88164809600006,11.6,8.30443237499999));
#241672=CARTESIAN_POINT('Ctrl Pts',(-6.88062272400006,15.2,8.30202713399999));
#241673=CARTESIAN_POINT('Ctrl Pts',(-6.88062272400006,11.6,8.30202713399999));
#241674=CARTESIAN_POINT('Ctrl Pts',(-6.87959765300006,15.2,8.29962826199999));
#241675=CARTESIAN_POINT('Ctrl Pts',(-6.87959765300006,11.6,8.29962826199999));
#241676=CARTESIAN_POINT('Ctrl Pts',(-6.87857289800006,15.2,8.29723576799999));
#241677=CARTESIAN_POINT('Ctrl Pts',(-6.87857289800006,11.6,8.29723576799999));
#241678=CARTESIAN_POINT('Ctrl Pts',(-6.87754847000006,15.2,8.29484965699999));
#241679=CARTESIAN_POINT('Ctrl Pts',(-6.87754847000006,11.6,8.29484965699999));
#241680=CARTESIAN_POINT('Ctrl Pts',(-6.87652438300006,15.2,8.29246993699999));
#241681=CARTESIAN_POINT('Ctrl Pts',(-6.87652438300006,11.6,8.29246993699999));
#241682=CARTESIAN_POINT('Ctrl Pts',(-6.87550064900006,15.2,8.29009661299999));
#241683=CARTESIAN_POINT('Ctrl Pts',(-6.87550064900006,11.6,8.29009661299999));
#241684=CARTESIAN_POINT('Ctrl Pts',(-6.87447728200006,15.2,8.28772969599999));
#241685=CARTESIAN_POINT('Ctrl Pts',(-6.87447728200006,11.6,8.28772969599999));
#241686=CARTESIAN_POINT('Ctrl Pts',(-6.87345429300006,15.2,8.28536918899999));
#241687=CARTESIAN_POINT('Ctrl Pts',(-6.87345429300006,11.6,8.28536918899999));
#241688=CARTESIAN_POINT('Ctrl Pts',(-6.87243169600006,15.2,8.28301510199999));
#241689=CARTESIAN_POINT('Ctrl Pts',(-6.87243169600006,11.6,8.28301510199999));
#241690=CARTESIAN_POINT('Ctrl Pts',(-6.87140950400006,15.2,8.28066743899999));
#241691=CARTESIAN_POINT('Ctrl Pts',(-6.87140950400006,11.6,8.28066743899999));
#241692=CARTESIAN_POINT('Ctrl Pts',(-6.87038772900006,15.2,8.27832621099999));
#241693=CARTESIAN_POINT('Ctrl Pts',(-6.87038772900006,11.6,8.27832621099999));
#241694=CARTESIAN_POINT('Ctrl Pts',(-6.86936638600006,15.2,8.27599142099999));
#241695=CARTESIAN_POINT('Ctrl Pts',(-6.86936638600006,11.6,8.27599142099999));
#241696=CARTESIAN_POINT('Ctrl Pts',(-6.86834548600006,15.2,8.27366307899998));
#241697=CARTESIAN_POINT('Ctrl Pts',(-6.86834548600006,11.6,8.27366307899998));
#241698=CARTESIAN_POINT('Ctrl Pts',(-6.86732504300006,15.2,8.27134118999999));
#241699=CARTESIAN_POINT('Ctrl Pts',(-6.86732504300006,11.6,8.27134118999999));
#241700=CARTESIAN_POINT('Ctrl Pts',(-6.86630507000006,15.2,8.26902576299998));
#241701=CARTESIAN_POINT('Ctrl Pts',(-6.86630507000006,11.6,8.26902576299998));
#241702=CARTESIAN_POINT('Ctrl Pts',(-6.86528558100005,15.2,8.26671680299999));
#241703=CARTESIAN_POINT('Ctrl Pts',(-6.86528558100005,11.6,8.26671680299999));
#241704=CARTESIAN_POINT('Ctrl Pts',(-6.86426658700006,15.2,8.26441431899998));
#241705=CARTESIAN_POINT('Ctrl Pts',(-6.86426658700006,11.6,8.26441431899998));
#241706=CARTESIAN_POINT('Ctrl Pts',(-6.86324810300006,15.2,8.26211831699998));
#241707=CARTESIAN_POINT('Ctrl Pts',(-6.86324810300006,11.6,8.26211831699998));
#241708=CARTESIAN_POINT('Ctrl Pts',(-6.86223014300006,15.2,8.25982880399999));
#241709=CARTESIAN_POINT('Ctrl Pts',(-6.86223014300006,11.6,8.25982880399999));
#241710=CARTESIAN_POINT('Ctrl Pts',(-6.86121271900006,15.2,8.25754578899998));
#241711=CARTESIAN_POINT('Ctrl Pts',(-6.86121271900006,11.6,8.25754578899998));
#241712=CARTESIAN_POINT('Ctrl Pts',(-6.86019584400006,15.2,8.25526927799999));
#241713=CARTESIAN_POINT('Ctrl Pts',(-6.86019584400006,11.6,8.25526927799999));
#241714=CARTESIAN_POINT('Ctrl Pts',(-6.85917953300006,15.2,8.25299927699999));
#241715=CARTESIAN_POINT('Ctrl Pts',(-6.85917953300006,11.6,8.25299927699999));
#241716=CARTESIAN_POINT('Ctrl Pts',(-6.85816379800006,15.2,8.25073579399999));
#241717=CARTESIAN_POINT('Ctrl Pts',(-6.85816379800006,11.6,8.25073579399999));
#241718=CARTESIAN_POINT('Ctrl Pts',(-6.85714865300006,15.2,8.24847883599999));
#241719=CARTESIAN_POINT('Ctrl Pts',(-6.85714865300006,11.6,8.24847883599999));
#241720=CARTESIAN_POINT('Ctrl Pts',(-6.85613411100006,15.2,8.24622841099998));
#241721=CARTESIAN_POINT('Ctrl Pts',(-6.85613411100006,11.6,8.24622841099998));
#241722=CARTESIAN_POINT('Ctrl Pts',(-6.85512018700006,15.2,8.24398452599999));
#241723=CARTESIAN_POINT('Ctrl Pts',(-6.85512018700006,11.6,8.24398452599999));
#241724=CARTESIAN_POINT('Ctrl Pts',(-6.85410689400006,15.2,8.24174718599998));
#241725=CARTESIAN_POINT('Ctrl Pts',(-6.85410689400006,11.6,8.24174718599998));
#241726=CARTESIAN_POINT('Ctrl Pts',(-6.85309424500006,15.2,8.23951640199999));
#241727=CARTESIAN_POINT('Ctrl Pts',(-6.85309424500006,11.6,8.23951640199999));
#241728=CARTESIAN_POINT('Ctrl Pts',(-6.85208225500006,15.2,8.23729217899999));
#241729=CARTESIAN_POINT('Ctrl Pts',(-6.85208225500006,11.6,8.23729217899999));
#241730=CARTESIAN_POINT('Ctrl Pts',(-6.85107093700006,15.2,8.23507452399999));
#241731=CARTESIAN_POINT('Ctrl Pts',(-6.85107093700006,11.6,8.23507452399999));
#241732=CARTESIAN_POINT('Ctrl Pts',(-6.85006030400006,15.2,8.23286344499999));
#241733=CARTESIAN_POINT('Ctrl Pts',(-6.85006030400006,11.6,8.23286344499999));
#241734=CARTESIAN_POINT('Ctrl Pts',(-6.84905037200005,15.2,8.23065894899998));
#241735=CARTESIAN_POINT('Ctrl Pts',(-6.84905037200005,11.6,8.23065894899998));
#241736=CARTESIAN_POINT('Ctrl Pts',(-6.84804115200006,15.2,8.22846104399999));
#241737=CARTESIAN_POINT('Ctrl Pts',(-6.84804115200006,11.6,8.22846104399999));
#241738=CARTESIAN_POINT('Ctrl Pts',(-6.84703266000006,15.2,8.22626973599998));
#241739=CARTESIAN_POINT('Ctrl Pts',(-6.84703266000006,11.6,8.22626973599998));
#241740=CARTESIAN_POINT('Ctrl Pts',(-6.84602491000006,15.2,8.22408503299998));
#241741=CARTESIAN_POINT('Ctrl Pts',(-6.84602491000006,11.6,8.22408503299998));
#241742=CARTESIAN_POINT('Ctrl Pts',(-6.84501791600006,15.2,8.22190694199998));
#241743=CARTESIAN_POINT('Ctrl Pts',(-6.84501791600006,11.6,8.22190694199998));
#241744=CARTESIAN_POINT('Ctrl Pts',(-6.84401169000005,15.2,8.21973546999999));
#241745=CARTESIAN_POINT('Ctrl Pts',(-6.84401169000005,11.6,8.21973546999999));
#241746=CARTESIAN_POINT('Ctrl Pts',(-6.84300624900006,15.2,8.21757062599998));
#241747=CARTESIAN_POINT('Ctrl Pts',(-6.84300624900006,11.6,8.21757062599998));
#241748=CARTESIAN_POINT('Ctrl Pts',(-6.84200160600006,15.2,8.21541241499999));
#241749=CARTESIAN_POINT('Ctrl Pts',(-6.84200160600006,11.6,8.21541241499999));
#241750=CARTESIAN_POINT('Ctrl Pts',(-6.84099777500006,15.2,8.21326084699999));
#241751=CARTESIAN_POINT('Ctrl Pts',(-6.84099777500006,11.6,8.21326084699999));
#241752=CARTESIAN_POINT('Ctrl Pts',(-6.83999477000006,15.2,8.21111592799999));
#241753=CARTESIAN_POINT('Ctrl Pts',(-6.83999477000006,11.6,8.21111592799999));
#241754=CARTESIAN_POINT('Ctrl Pts',(-6.83899260600006,15.2,8.20897766399998));
#241755=CARTESIAN_POINT('Ctrl Pts',(-6.83899260600006,11.6,8.20897766399998));
#241756=CARTESIAN_POINT('Ctrl Pts',(-6.83799129700006,15.2,8.20684606399999));
#241757=CARTESIAN_POINT('Ctrl Pts',(-6.83799129700006,11.6,8.20684606399999));
#241758=CARTESIAN_POINT('Ctrl Pts',(-6.83699085800006,15.2,8.20472113499999));
#241759=CARTESIAN_POINT('Ctrl Pts',(-6.83699085800006,11.6,8.20472113499999));
#241760=CARTESIAN_POINT('Ctrl Pts',(-6.83599130200006,15.2,8.20260288499998));
#241761=CARTESIAN_POINT('Ctrl Pts',(-6.83599130200006,11.6,8.20260288499998));
#241762=CARTESIAN_POINT('Ctrl Pts',(-6.83499264500006,15.2,8.20049131999999));
#241763=CARTESIAN_POINT('Ctrl Pts',(-6.83499264500006,11.6,8.20049131999999));
#241764=CARTESIAN_POINT('Ctrl Pts',(-6.83399490100006,15.2,8.19838644999999));
#241765=CARTESIAN_POINT('Ctrl Pts',(-6.83399490100006,11.6,8.19838644999999));
#241766=CARTESIAN_POINT('Ctrl Pts',(-6.83299808500006,15.2,8.19628827899999));
#241767=CARTESIAN_POINT('Ctrl Pts',(-6.83299808500006,11.6,8.19628827899999));
#241768=CARTESIAN_POINT('Ctrl Pts',(-6.83200221000006,15.2,8.19419681699999));
#241769=CARTESIAN_POINT('Ctrl Pts',(-6.83200221000006,11.6,8.19419681699999));
#241770=CARTESIAN_POINT('Ctrl Pts',(-6.83100729300006,15.2,8.19211206999999));
#241771=CARTESIAN_POINT('Ctrl Pts',(-6.83100729300006,11.6,8.19211206999999));
#241772=CARTESIAN_POINT('Ctrl Pts',(-6.83001334700006,15.2,8.19003404699998));
#241773=CARTESIAN_POINT('Ctrl Pts',(-6.83001334700006,11.6,8.19003404699998));
#241774=CARTESIAN_POINT('Ctrl Pts',(-6.82902038700006,15.2,8.18796275499999));
#241775=CARTESIAN_POINT('Ctrl Pts',(-6.82902038700006,11.6,8.18796275499999));
#241776=CARTESIAN_POINT('Ctrl Pts',(-6.82802842900006,15.2,8.18589820099999));
#241777=CARTESIAN_POINT('Ctrl Pts',(-6.82802842900006,11.6,8.18589820099999));
#241778=CARTESIAN_POINT('Ctrl Pts',(-6.82703748600006,15.2,8.18384039199999));
#241779=CARTESIAN_POINT('Ctrl Pts',(-6.82703748600006,11.6,8.18384039199999));
#241780=CARTESIAN_POINT('Ctrl Pts',(-6.82604757500005,15.2,8.18178933699999));
#241781=CARTESIAN_POINT('Ctrl Pts',(-6.82604757500005,11.6,8.18178933699999));
#241782=CARTESIAN_POINT('Ctrl Pts',(-6.82505871000005,15.2,8.17974504099999));
#241783=CARTESIAN_POINT('Ctrl Pts',(-6.82505871000005,11.6,8.17974504099999));
#241784=CARTESIAN_POINT('Ctrl Pts',(-6.82407090600006,15.2,8.17770751499998));
#241785=CARTESIAN_POINT('Ctrl Pts',(-6.82407090600006,11.6,8.17770751499998));
#241786=CARTESIAN_POINT('Ctrl Pts',(-6.82308417900006,15.2,8.17567676499999));
#241787=CARTESIAN_POINT('Ctrl Pts',(-6.82308417900006,11.6,8.17567676499999));
#241788=CARTESIAN_POINT('Ctrl Pts',(-6.82209854200006,15.2,8.17365279799999));
#241789=CARTESIAN_POINT('Ctrl Pts',(-6.82209854200006,11.6,8.17365279799999));
#241790=CARTESIAN_POINT('Ctrl Pts',(-6.82111401300006,15.2,8.17163562099999));
#241791=CARTESIAN_POINT('Ctrl Pts',(-6.82111401300006,11.6,8.17163562099999));
#241792=CARTESIAN_POINT('Ctrl Pts',(-6.82013060500006,15.2,8.16962524399998));
#241793=CARTESIAN_POINT('Ctrl Pts',(-6.82013060500006,11.6,8.16962524399998));
#241794=CARTESIAN_POINT('Ctrl Pts',(-6.81914833400006,15.2,8.16762167299999));
#241795=CARTESIAN_POINT('Ctrl Pts',(-6.81914833400006,11.6,8.16762167299999));
#241796=CARTESIAN_POINT('Ctrl Pts',(-6.81816721500006,15.2,8.16562491699998));
#241797=CARTESIAN_POINT('Ctrl Pts',(-6.81816721500006,11.6,8.16562491699998));
#241798=CARTESIAN_POINT('Ctrl Pts',(-6.81718726400006,15.2,8.16363498099999));
#241799=CARTESIAN_POINT('Ctrl Pts',(-6.81718726400006,11.6,8.16363498099999));
#241800=CARTESIAN_POINT('Ctrl Pts',(-6.81620849600006,15.2,8.16165187399999));
#241801=CARTESIAN_POINT('Ctrl Pts',(-6.81620849600006,11.6,8.16165187399999));
#241802=CARTESIAN_POINT('Ctrl Pts',(-6.81523092700006,15.2,8.15967560499999));
#241803=CARTESIAN_POINT('Ctrl Pts',(-6.81523092700006,11.6,8.15967560499999));
#241804=CARTESIAN_POINT('Ctrl Pts',(-6.81425457300006,15.2,8.15770617999998));
#241805=CARTESIAN_POINT('Ctrl Pts',(-6.81425457300006,11.6,8.15770617999998));
#241806=CARTESIAN_POINT('Ctrl Pts',(-6.81327944800006,15.2,8.15574360799998));
#241807=CARTESIAN_POINT('Ctrl Pts',(-6.81327944800006,11.6,8.15574360799998));
#241808=CARTESIAN_POINT('Ctrl Pts',(-6.81230556900006,15.2,8.15378789499999));
#241809=CARTESIAN_POINT('Ctrl Pts',(-6.81230556900006,11.6,8.15378789499999));
#241810=CARTESIAN_POINT('Ctrl Pts',(-6.81133295100006,15.2,8.15183904999999));
#241811=CARTESIAN_POINT('Ctrl Pts',(-6.81133295100006,11.6,8.15183904999999));
#241812=CARTESIAN_POINT('Ctrl Pts',(-6.81036161000006,15.2,8.14989708099999));
#241813=CARTESIAN_POINT('Ctrl Pts',(-6.81036161000006,11.6,8.14989708099999));
#241814=CARTESIAN_POINT('Ctrl Pts',(-6.80939156200006,15.2,8.14796199499998));
#241815=CARTESIAN_POINT('Ctrl Pts',(-6.80939156200006,11.6,8.14796199499998));
#241816=CARTESIAN_POINT('Ctrl Pts',(-6.80842282200006,15.2,8.14603380099998));
#241817=CARTESIAN_POINT('Ctrl Pts',(-6.80842282200006,11.6,8.14603380099998));
#241818=CARTESIAN_POINT('Ctrl Pts',(-6.80745540800006,15.2,8.14411250399999));
#241819=CARTESIAN_POINT('Ctrl Pts',(-6.80745540800006,11.6,8.14411250399999));
#241820=CARTESIAN_POINT('Ctrl Pts',(-6.80648933300006,15.2,8.14219811399998));
#241821=CARTESIAN_POINT('Ctrl Pts',(-6.80648933300006,11.6,8.14219811399998));
#241822=CARTESIAN_POINT('Ctrl Pts',(-6.80552461600006,15.2,8.14029063899999));
#241823=CARTESIAN_POINT('Ctrl Pts',(-6.80552461600006,11.6,8.14029063899999));
#241824=CARTESIAN_POINT('Ctrl Pts',(-6.80456127200006,15.2,8.13839008599999));
#241825=CARTESIAN_POINT('Ctrl Pts',(-6.80456127200006,11.6,8.13839008599999));
#241826=CARTESIAN_POINT('Ctrl Pts',(-6.80359931600006,15.2,8.13649646299999));
#241827=CARTESIAN_POINT('Ctrl Pts',(-6.80359931600006,11.6,8.13649646299999));
#241828=CARTESIAN_POINT('Ctrl Pts',(-6.80263876600006,15.2,8.13460977699999));
#241829=CARTESIAN_POINT('Ctrl Pts',(-6.80263876600006,11.6,8.13460977699999));
#241830=CARTESIAN_POINT('Ctrl Pts',(-6.80167963800006,15.2,8.13273003799999));
#241831=CARTESIAN_POINT('Ctrl Pts',(-6.80167963800006,11.6,8.13273003799999));
#241832=CARTESIAN_POINT('Ctrl Pts',(-6.80072194600006,15.2,8.13085725199999));
#241833=CARTESIAN_POINT('Ctrl Pts',(-6.80072194600006,11.6,8.13085725199999));
#241834=CARTESIAN_POINT('Ctrl Pts',(-6.79976571000006,15.2,8.12899142899998));
#241835=CARTESIAN_POINT('Ctrl Pts',(-6.79976571000006,11.6,8.12899142899998));
#241836=CARTESIAN_POINT('Ctrl Pts',(-6.79881094300006,15.2,8.12713257299999));
#241837=CARTESIAN_POINT('Ctrl Pts',(-6.79881094300006,11.6,8.12713257299999));
#241838=CARTESIAN_POINT('Ctrl Pts',(-6.79785766400006,15.2,8.12528069599999));
#241839=CARTESIAN_POINT('Ctrl Pts',(-6.79785766400006,11.6,8.12528069599999));
#241840=CARTESIAN_POINT('Ctrl Pts',(-6.79690588900006,15.2,8.12343580499999));
#241841=CARTESIAN_POINT('Ctrl Pts',(-6.79690588900006,11.6,8.12343580499999));
#241842=CARTESIAN_POINT('Ctrl Pts',(-6.79595563300006,15.2,8.12159790499998));
#241843=CARTESIAN_POINT('Ctrl Pts',(-6.79595563300006,11.6,8.12159790499998));
#241844=CARTESIAN_POINT('Ctrl Pts',(-6.79500691600006,15.2,8.11976700799999));
#241845=CARTESIAN_POINT('Ctrl Pts',(-6.79500691600006,11.6,8.11976700799999));
#241846=CARTESIAN_POINT('Ctrl Pts',(-6.79405975100006,15.2,8.11794311999999));
#241847=CARTESIAN_POINT('Ctrl Pts',(-6.79405975100006,11.6,8.11794311999999));
#241848=CARTESIAN_POINT('Ctrl Pts',(-6.79311415800006,15.2,8.11612624899999));
#241849=CARTESIAN_POINT('Ctrl Pts',(-6.79311415800006,11.6,8.11612624899999));
#241850=CARTESIAN_POINT('Ctrl Pts',(-6.79217015000006,15.2,8.11431640399999));
#241851=CARTESIAN_POINT('Ctrl Pts',(-6.79217015000006,11.6,8.11431640399999));
#241852=CARTESIAN_POINT('Ctrl Pts',(-6.79122774800006,15.2,8.11251359099998));
#241853=CARTESIAN_POINT('Ctrl Pts',(-6.79122774800006,11.6,8.11251359099998));
#241854=CARTESIAN_POINT('Ctrl Pts',(-6.79028696800006,15.2,8.11071782099998));
#241855=CARTESIAN_POINT('Ctrl Pts',(-6.79028696800006,11.6,8.11071782099998));
#241856=CARTESIAN_POINT('Ctrl Pts',(-6.78934782500006,15.2,8.10892909799998));
#241857=CARTESIAN_POINT('Ctrl Pts',(-6.78934782500006,11.6,8.10892909799998));
#241858=CARTESIAN_POINT('Ctrl Pts',(-6.78841033800006,15.2,8.10714743499998));
#241859=CARTESIAN_POINT('Ctrl Pts',(-6.78841033800006,11.6,8.10714743499998));
#241860=CARTESIAN_POINT('Ctrl Pts',(-6.78747452300006,15.2,8.10537283699999));
#241861=CARTESIAN_POINT('Ctrl Pts',(-6.78747452300006,11.6,8.10537283699999));
#241862=CARTESIAN_POINT('Ctrl Pts',(-6.78654039900006,15.2,8.10360531199999));
#241863=CARTESIAN_POINT('Ctrl Pts',(-6.78654039900006,11.6,8.10360531199999));
#241864=CARTESIAN_POINT('Ctrl Pts',(-6.78560798200006,15.2,8.10184486899999));
#241865=CARTESIAN_POINT('Ctrl Pts',(-6.78560798200006,11.6,8.10184486899999));
#241866=CARTESIAN_POINT('Ctrl Pts',(-6.78467728900006,15.2,8.10009151699998));
#241867=CARTESIAN_POINT('Ctrl Pts',(-6.78467728900006,11.6,8.10009151699998));
#241868=CARTESIAN_POINT('Ctrl Pts',(-6.78374833800006,15.2,8.09834526099999));
#241869=CARTESIAN_POINT('Ctrl Pts',(-6.78374833800006,11.6,8.09834526099999));
#241870=CARTESIAN_POINT('Ctrl Pts',(-6.78282114600006,15.2,8.09660611299999));
#241871=CARTESIAN_POINT('Ctrl Pts',(-6.78282114600006,11.6,8.09660611299999));
#241872=CARTESIAN_POINT('Ctrl Pts',(-6.78189573200005,15.2,8.09487407999999));
#241873=CARTESIAN_POINT('Ctrl Pts',(-6.78189573200005,11.6,8.09487407999999));
#241874=CARTESIAN_POINT('Ctrl Pts',(-6.78097211100006,15.2,8.09314916899999));
#241875=CARTESIAN_POINT('Ctrl Pts',(-6.78097211100006,11.6,8.09314916899999));
#241876=CARTESIAN_POINT('Ctrl Pts',(-6.78005030300006,15.2,8.09143138899999));
#241877=CARTESIAN_POINT('Ctrl Pts',(-6.78005030300006,11.6,8.09143138899999));
#241878=CARTESIAN_POINT('Ctrl Pts',(-6.77913032500006,15.2,8.08972074899999));
#241879=CARTESIAN_POINT('Ctrl Pts',(-6.77913032500006,11.6,8.08972074899999));
#241880=CARTESIAN_POINT('Ctrl Pts',(-6.77821219500006,15.2,8.08801725599999));
#241881=CARTESIAN_POINT('Ctrl Pts',(-6.77821219500006,11.6,8.08801725599999));
#241882=CARTESIAN_POINT('Ctrl Pts',(-6.77729593100006,15.2,8.08632091799998));
#241883=CARTESIAN_POINT('Ctrl Pts',(-6.77729593100006,11.6,8.08632091799998));
#241884=CARTESIAN_POINT('Ctrl Pts',(-6.77638155000006,15.2,8.08463174499998));
#241885=CARTESIAN_POINT('Ctrl Pts',(-6.77638155000006,11.6,8.08463174499998));
#241886=CARTESIAN_POINT('Ctrl Pts',(-6.77546907200006,15.2,8.08294974399999));
#241887=CARTESIAN_POINT('Ctrl Pts',(-6.77546907200006,11.6,8.08294974399999));
#241888=CARTESIAN_POINT('Ctrl Pts',(-6.77455851200006,15.2,8.08127492399999));
#241889=CARTESIAN_POINT('Ctrl Pts',(-6.77455851200006,11.6,8.08127492399999));
#241890=CARTESIAN_POINT('Ctrl Pts',(-6.77364989000006,15.2,8.07960729299998));
#241891=CARTESIAN_POINT('Ctrl Pts',(-6.77364989000006,11.6,8.07960729299998));
#241892=CARTESIAN_POINT('Ctrl Pts',(-6.77274322500006,15.2,8.07794685999998));
#241893=CARTESIAN_POINT('Ctrl Pts',(-6.77274322500006,11.6,8.07794685999998));
#241894=CARTESIAN_POINT('Ctrl Pts',(-6.77183853400006,15.2,8.07629363199998));
#241895=CARTESIAN_POINT('Ctrl Pts',(-6.77183853400006,11.6,8.07629363199998));
#241896=CARTESIAN_POINT('Ctrl Pts',(-6.77093583500006,15.2,8.07464761899999));
#241897=CARTESIAN_POINT('Ctrl Pts',(-6.77093583500006,11.6,8.07464761899999));
#241898=CARTESIAN_POINT('Ctrl Pts',(-6.77003514900006,15.2,8.07300882799998));
#241899=CARTESIAN_POINT('Ctrl Pts',(-6.77003514900006,11.6,8.07300882799998));
#241900=CARTESIAN_POINT('Ctrl Pts',(-6.76913649100006,15.2,8.07137726799999));
#241901=CARTESIAN_POINT('Ctrl Pts',(-6.76913649100006,11.6,8.07137726799999));
#241902=CARTESIAN_POINT('Ctrl Pts',(-6.76823988100006,15.2,8.06975294799999));
#241903=CARTESIAN_POINT('Ctrl Pts',(-6.76823988100006,11.6,8.06975294799999));
#241904=CARTESIAN_POINT('Ctrl Pts',(-6.76734533900006,15.2,8.06813587699999));
#241905=CARTESIAN_POINT('Ctrl Pts',(-6.76734533900006,11.6,8.06813587699999));
#241906=CARTESIAN_POINT('Ctrl Pts',(-6.76645288200006,15.2,8.06652606199999));
#241907=CARTESIAN_POINT('Ctrl Pts',(-6.76645288200006,11.6,8.06652606199999));
#241908=CARTESIAN_POINT('Ctrl Pts',(-6.76556252900006,15.2,8.06492351199999));
#241909=CARTESIAN_POINT('Ctrl Pts',(-6.76556252900006,11.6,8.06492351199999));
#241910=CARTESIAN_POINT('Ctrl Pts',(-6.76467429900006,15.2,8.06332823599998));
#241911=CARTESIAN_POINT('Ctrl Pts',(-6.76467429900006,11.6,8.06332823599998));
#241912=CARTESIAN_POINT('Ctrl Pts',(-6.76378821300006,15.2,8.06174024099998));
#241913=CARTESIAN_POINT('Ctrl Pts',(-6.76378821300006,11.6,8.06174024099998));
#241914=CARTESIAN_POINT('Ctrl Pts',(-6.76290428600006,15.2,8.06015953799999));
#241915=CARTESIAN_POINT('Ctrl Pts',(-6.76290428600006,11.6,8.06015953799999));
#241916=CARTESIAN_POINT('Ctrl Pts',(-6.76202253900006,15.2,8.05858613399998));
#241917=CARTESIAN_POINT('Ctrl Pts',(-6.76202253900006,11.6,8.05858613399998));
#241918=CARTESIAN_POINT('Ctrl Pts',(-6.76114299300006,15.2,8.05702003799999));
#241919=CARTESIAN_POINT('Ctrl Pts',(-6.76114299300006,11.6,8.05702003799999));
#241920=CARTESIAN_POINT('Ctrl Pts',(-6.76026566400005,15.2,8.05546125899999));
#241921=CARTESIAN_POINT('Ctrl Pts',(-6.76026566400005,11.6,8.05546125899999));
#241922=CARTESIAN_POINT('Ctrl Pts',(-6.75939057400006,15.2,8.05390980499999));
#241923=CARTESIAN_POINT('Ctrl Pts',(-6.75939057400006,11.6,8.05390980499999));
#241924=CARTESIAN_POINT('Ctrl Pts',(-6.75851774100006,15.2,8.05236568499998));
#241925=CARTESIAN_POINT('Ctrl Pts',(-6.75851774100006,11.6,8.05236568499998));
#241926=CARTESIAN_POINT('Ctrl Pts',(-6.75764718400006,15.2,8.05082890799999));
#241927=CARTESIAN_POINT('Ctrl Pts',(-6.75764718400006,11.6,8.05082890799999));
#241928=CARTESIAN_POINT('Ctrl Pts',(-6.75677892300006,15.2,8.04929948199998));
#241929=CARTESIAN_POINT('Ctrl Pts',(-6.75677892300006,11.6,8.04929948199998));
#241930=CARTESIAN_POINT('Ctrl Pts',(-6.75591297800006,15.2,8.04777741599998));
#241931=CARTESIAN_POINT('Ctrl Pts',(-6.75591297800006,11.6,8.04777741599998));
#241932=CARTESIAN_POINT('Ctrl Pts',(-6.75504936900006,15.2,8.04626271899998));
#241933=CARTESIAN_POINT('Ctrl Pts',(-6.75504936900006,11.6,8.04626271899998));
#241934=CARTESIAN_POINT('Ctrl Pts',(-6.75418811500006,15.2,8.04475539999999));
#241935=CARTESIAN_POINT('Ctrl Pts',(-6.75418811500006,11.6,8.04475539999999));
#241936=CARTESIAN_POINT('Ctrl Pts',(-6.75332923600005,15.2,8.04325546699998));
#241937=CARTESIAN_POINT('Ctrl Pts',(-6.75332923600005,11.6,8.04325546699998));
#241938=CARTESIAN_POINT('Ctrl Pts',(-6.75247275200006,15.2,8.04176292999998));
#241939=CARTESIAN_POINT('Ctrl Pts',(-6.75247275200006,11.6,8.04176292999998));
#241940=CARTESIAN_POINT('Ctrl Pts',(-6.75161868200005,15.2,8.04027779599998));
#241941=CARTESIAN_POINT('Ctrl Pts',(-6.75161868200005,11.6,8.04027779599998));
#241942=CARTESIAN_POINT('Ctrl Pts',(-6.75076704800006,15.2,8.03880007599999));
#241943=CARTESIAN_POINT('Ctrl Pts',(-6.75076704800006,11.6,8.03880007599999));
#241944=CARTESIAN_POINT('Ctrl Pts',(-6.74991786900006,15.2,8.03732977699998));
#241945=CARTESIAN_POINT('Ctrl Pts',(-6.74991786900006,11.6,8.03732977699998));
#241946=CARTESIAN_POINT('Ctrl Pts',(-6.74907116500005,15.2,8.03586690899999));
#241947=CARTESIAN_POINT('Ctrl Pts',(-6.74907116500005,11.6,8.03586690899999));
#241948=CARTESIAN_POINT('Ctrl Pts',(-6.74822695800006,15.2,8.03441148099999));
#241949=CARTESIAN_POINT('Ctrl Pts',(-6.74822695800006,11.6,8.03441148099999));
#241950=CARTESIAN_POINT('Ctrl Pts',(-6.74738526500006,15.2,8.03296350199999));
#241951=CARTESIAN_POINT('Ctrl Pts',(-6.74738526500006,11.6,8.03296350199999));
#241952=CARTESIAN_POINT('Ctrl Pts',(-6.74654611000006,15.2,8.03152297999999));
#241953=CARTESIAN_POINT('Ctrl Pts',(-6.74654611000006,11.6,8.03152297999999));
#241954=CARTESIAN_POINT('Ctrl Pts',(-6.74570951200006,15.2,8.03008992499999));
#241955=CARTESIAN_POINT('Ctrl Pts',(-6.74570951200006,11.6,8.03008992499999));
#241956=CARTESIAN_POINT('Ctrl Pts',(-6.74487549200006,15.2,8.02866434499999));
#241957=CARTESIAN_POINT('Ctrl Pts',(-6.74487549200006,11.6,8.02866434499999));
#241958=CARTESIAN_POINT('Ctrl Pts',(-6.74404407000006,15.2,8.02724625099999));
#241959=CARTESIAN_POINT('Ctrl Pts',(-6.74404407000006,11.6,8.02724625099999));
#241960=CARTESIAN_POINT('Ctrl Pts',(-6.74321526700006,15.2,8.02583564899999));
#241961=CARTESIAN_POINT('Ctrl Pts',(-6.74321526700006,11.6,8.02583564899999));
#241962=CARTESIAN_POINT('Ctrl Pts',(-6.74238910500006,15.2,8.02443255099998));
#241963=CARTESIAN_POINT('Ctrl Pts',(-6.74238910500006,11.6,8.02443255099998));
#241964=CARTESIAN_POINT('Ctrl Pts',(-6.74156560400006,15.2,8.02303696499998));
#241965=CARTESIAN_POINT('Ctrl Pts',(-6.74156560400006,11.6,8.02303696499998));
#241966=CARTESIAN_POINT('Ctrl Pts',(-6.74074478500006,15.2,8.02164889999998));
#241967=CARTESIAN_POINT('Ctrl Pts',(-6.74074478500006,11.6,8.02164889999998));
#241968=CARTESIAN_POINT('Ctrl Pts',(-6.73992667000006,15.2,8.02026836499999));
#241969=CARTESIAN_POINT('Ctrl Pts',(-6.73992667000006,11.6,8.02026836499999));
#241970=CARTESIAN_POINT('Ctrl Pts',(-6.73911127900006,15.2,8.01889536999998));
#241971=CARTESIAN_POINT('Ctrl Pts',(-6.73911127900006,11.6,8.01889536999998));
#241972=CARTESIAN_POINT('Ctrl Pts',(-6.73829863500006,15.2,8.01752992299999));
#241973=CARTESIAN_POINT('Ctrl Pts',(-6.73829863500006,11.6,8.01752992299999));
#241974=CARTESIAN_POINT('Ctrl Pts',(-6.73748875900006,15.2,8.01617203399999));
#241975=CARTESIAN_POINT('Ctrl Pts',(-6.73748875900006,11.6,8.01617203399999));
#241976=CARTESIAN_POINT('Ctrl Pts',(-6.73668167000006,15.2,8.01482171199999));
#241977=CARTESIAN_POINT('Ctrl Pts',(-6.73668167000006,11.6,8.01482171199999));
#241978=CARTESIAN_POINT('Ctrl Pts',(-6.73587739300006,15.2,8.01347896699999));
#241979=CARTESIAN_POINT('Ctrl Pts',(-6.73587739300006,11.6,8.01347896699999));
#241980=CARTESIAN_POINT('Ctrl Pts',(-6.73507594800006,15.2,8.01214380699999));
#241981=CARTESIAN_POINT('Ctrl Pts',(-6.73507594800006,11.6,8.01214380699999));
#241982=CARTESIAN_POINT('Ctrl Pts',(-6.73427735700006,15.2,8.01081624299999));
#241983=CARTESIAN_POINT('Ctrl Pts',(-6.73427735700006,11.6,8.01081624299999));
#241984=CARTESIAN_POINT('Ctrl Pts',(-6.73348164200006,15.2,8.00949628199999));
#241985=CARTESIAN_POINT('Ctrl Pts',(-6.73348164200006,11.6,8.00949628199999));
#241986=CARTESIAN_POINT('Ctrl Pts',(-6.73268882400006,15.2,8.00818393499998));
#241987=CARTESIAN_POINT('Ctrl Pts',(-6.73268882400006,11.6,8.00818393499998));
#241988=CARTESIAN_POINT('Ctrl Pts',(-6.73189892800006,15.2,8.00687921199999));
#241989=CARTESIAN_POINT('Ctrl Pts',(-6.73189892800006,11.6,8.00687921199999));
#241990=CARTESIAN_POINT('Ctrl Pts',(-6.73111197300006,15.2,8.00558212099999));
#241991=CARTESIAN_POINT('Ctrl Pts',(-6.73111197300006,11.6,8.00558212099999));
#241992=CARTESIAN_POINT('Ctrl Pts',(-6.73032798300006,15.2,8.00429267199998));
#241993=CARTESIAN_POINT('Ctrl Pts',(-6.73032798300006,11.6,8.00429267199998));
#241994=CARTESIAN_POINT('Ctrl Pts',(-6.72954697900006,15.2,8.00301087499999));
#241995=CARTESIAN_POINT('Ctrl Pts',(-6.72954697900006,11.6,8.00301087499999));
#241996=CARTESIAN_POINT('Ctrl Pts',(-6.72876898500006,15.2,8.00173673899998));
#241997=CARTESIAN_POINT('Ctrl Pts',(-6.72876898500006,11.6,8.00173673899998));
#241998=CARTESIAN_POINT('Ctrl Pts',(-6.72799402200006,15.2,8.00047027299998));
#241999=CARTESIAN_POINT('Ctrl Pts',(-6.72799402200006,11.6,8.00047027299998));
#242000=CARTESIAN_POINT('Ctrl Pts',(-6.72722211500006,15.2,7.99921148699998));
#242001=CARTESIAN_POINT('Ctrl Pts',(-6.72722211500006,11.6,7.99921148699998));
#242002=CARTESIAN_POINT('Ctrl Pts',(-6.72645328300006,15.2,7.99796039199999));
#242003=CARTESIAN_POINT('Ctrl Pts',(-6.72645328300006,11.6,7.99796039199999));
#242004=CARTESIAN_POINT('Ctrl Pts',(-6.72568755300006,15.2,7.99671699499999));
#242005=CARTESIAN_POINT('Ctrl Pts',(-6.72568755300006,11.6,7.99671699499999));
#242006=CARTESIAN_POINT('Ctrl Pts',(-6.72492494500006,15.2,7.99548130699999));
#242007=CARTESIAN_POINT('Ctrl Pts',(-6.72492494500006,11.6,7.99548130699999));
#242008=CARTESIAN_POINT('Ctrl Pts',(-6.72416548300006,15.2,7.99425333899999));
#242009=CARTESIAN_POINT('Ctrl Pts',(-6.72416548300006,11.6,7.99425333899999));
#242010=CARTESIAN_POINT('Ctrl Pts',(-6.72340919000006,15.2,7.99303309799999));
#242011=CARTESIAN_POINT('Ctrl Pts',(-6.72340919000006,11.6,7.99303309799999));
#242012=CARTESIAN_POINT('Ctrl Pts',(-6.72265609000006,15.2,7.99182059499999));
#242013=CARTESIAN_POINT('Ctrl Pts',(-6.72265609000006,11.6,7.99182059499999));
#242014=CARTESIAN_POINT('Ctrl Pts',(-6.72190620500006,15.2,7.99061584099999));
#242015=CARTESIAN_POINT('Ctrl Pts',(-6.72190620500006,11.6,7.99061584099999));
#242016=CARTESIAN_POINT('Ctrl Pts',(-6.72115955900006,15.2,7.98941884399999));
#242017=CARTESIAN_POINT('Ctrl Pts',(-6.72115955900006,11.6,7.98941884399999));
#242018=CARTESIAN_POINT('Ctrl Pts',(-6.72041617600006,15.2,7.98822961399999));
#242019=CARTESIAN_POINT('Ctrl Pts',(-6.72041617600006,11.6,7.98822961399999));
#242020=CARTESIAN_POINT('Ctrl Pts',(-6.71967608100006,15.2,7.98704816199999));
#242021=CARTESIAN_POINT('Ctrl Pts',(-6.71967608100006,11.6,7.98704816199999));
#242022=CARTESIAN_POINT('Ctrl Pts',(-6.71893929400006,15.2,7.98587449599999));
#242023=CARTESIAN_POINT('Ctrl Pts',(-6.71893929400006,11.6,7.98587449599999));
#242024=CARTESIAN_POINT('Ctrl Pts',(-6.71820584200006,15.2,7.98470862799999));
#242025=CARTESIAN_POINT('Ctrl Pts',(-6.71820584200006,11.6,7.98470862799999));
#242026=CARTESIAN_POINT('Ctrl Pts',(-6.71747574700006,15.2,7.98355056599998));
#242027=CARTESIAN_POINT('Ctrl Pts',(-6.71747574700006,11.6,7.98355056599998));
#242028=CARTESIAN_POINT('Ctrl Pts',(-6.71674903500006,15.2,7.98240032199999));
#242029=CARTESIAN_POINT('Ctrl Pts',(-6.71674903500006,11.6,7.98240032199999));
#242030=CARTESIAN_POINT('Ctrl Pts',(-6.71602572900006,15.2,7.98125790399999));
#242031=CARTESIAN_POINT('Ctrl Pts',(-6.71602572900006,11.6,7.98125790399999));
#242032=CARTESIAN_POINT('Ctrl Pts',(-6.71530585400006,15.2,7.98012332299999));
#242033=CARTESIAN_POINT('Ctrl Pts',(-6.71530585400006,11.6,7.98012332299999));
#242034=CARTESIAN_POINT('Ctrl Pts',(-6.71458943400006,15.2,7.97899658999999));
#242035=CARTESIAN_POINT('Ctrl Pts',(-6.71458943400006,11.6,7.97899658999999));
#242036=CARTESIAN_POINT('Ctrl Pts',(-6.71387649200006,15.2,7.97787771299999));
#242037=CARTESIAN_POINT('Ctrl Pts',(-6.71387649200006,11.6,7.97787771299999));
#242038=CARTESIAN_POINT('Ctrl Pts',(-6.71316705500006,15.2,7.97676670399999));
#242039=CARTESIAN_POINT('Ctrl Pts',(-6.71316705500006,11.6,7.97676670399999));
#242040=CARTESIAN_POINT('Ctrl Pts',(-6.71246114700006,15.2,7.97566357099999));
#242041=CARTESIAN_POINT('Ctrl Pts',(-6.71246114700006,11.6,7.97566357099999));
#242042=CARTESIAN_POINT('Ctrl Pts',(-6.71175879300006,15.2,7.97456832599998));
#242043=CARTESIAN_POINT('Ctrl Pts',(-6.71175879300006,11.6,7.97456832599998));
#242044=CARTESIAN_POINT('Ctrl Pts',(-6.71106001700006,15.2,7.97348097999999));
#242045=CARTESIAN_POINT('Ctrl Pts',(-6.71106001700006,11.6,7.97348097999999));
#242046=CARTESIAN_POINT('Ctrl Pts',(-6.71036484500006,15.2,7.97240153999999));
#242047=CARTESIAN_POINT('Ctrl Pts',(-6.71036484500006,11.6,7.97240153999999));
#242048=CARTESIAN_POINT('Ctrl Pts',(-6.70967330200006,15.2,7.97133001899999));
#242049=CARTESIAN_POINT('Ctrl Pts',(-6.70967330200006,11.6,7.97133001899999));
#242050=CARTESIAN_POINT('Ctrl Pts',(-6.70898541300006,15.2,7.97026642699999));
#242051=CARTESIAN_POINT('Ctrl Pts',(-6.70898541300006,11.6,7.97026642699999));
#242052=CARTESIAN_POINT('Ctrl Pts',(-6.70830120400006,15.2,7.96921077299999));
#242053=CARTESIAN_POINT('Ctrl Pts',(-6.70830120400006,11.6,7.96921077299999));
#242054=CARTESIAN_POINT('Ctrl Pts',(-6.70762070000006,15.2,7.96816306899998));
#242055=CARTESIAN_POINT('Ctrl Pts',(-6.70762070000006,11.6,7.96816306899998));
#242056=CARTESIAN_POINT('Ctrl Pts',(-6.70694392700006,15.2,7.96712332499999));
#242057=CARTESIAN_POINT('Ctrl Pts',(-6.70694392700006,11.6,7.96712332499999));
#242058=CARTESIAN_POINT('Ctrl Pts',(-6.70627091100005,15.2,7.96609154899999));
#242059=CARTESIAN_POINT('Ctrl Pts',(-6.70627091100005,11.6,7.96609154899999));
#242060=CARTESIAN_POINT('Ctrl Pts',(-6.70560167800006,15.2,7.96506775499999));
#242061=CARTESIAN_POINT('Ctrl Pts',(-6.70560167800006,11.6,7.96506775499999));
#242062=CARTESIAN_POINT('Ctrl Pts',(-6.70493625300006,15.2,7.96405195199998));
#242063=CARTESIAN_POINT('Ctrl Pts',(-6.70493625300006,11.6,7.96405195199998));
#242064=CARTESIAN_POINT('Ctrl Pts',(-6.70427466300006,15.2,7.96304415099998));
#242065=CARTESIAN_POINT('Ctrl Pts',(-6.70427466300006,11.6,7.96304415099998));
#242066=CARTESIAN_POINT('Ctrl Pts',(-6.70361693400006,15.2,7.96204436099998));
#242067=CARTESIAN_POINT('Ctrl Pts',(-6.70361693400006,11.6,7.96204436099998));
#242068=CARTESIAN_POINT('Ctrl Pts',(-6.70296309400006,15.2,7.96105259399998));
#242069=CARTESIAN_POINT('Ctrl Pts',(-6.70296309400006,11.6,7.96105259399998));
#242070=CARTESIAN_POINT('Ctrl Pts',(-6.70231316700006,15.2,7.96006886099998));
#242071=CARTESIAN_POINT('Ctrl Pts',(-6.70231316700006,11.6,7.96006886099998));
#242072=CARTESIAN_POINT('Ctrl Pts',(-6.70166718000006,15.2,7.95909317099999));
#242073=CARTESIAN_POINT('Ctrl Pts',(-6.70166718000006,11.6,7.95909317099999));
#242074=CARTESIAN_POINT('Ctrl Pts',(-6.70102516100005,15.2,7.95812553699999));
#242075=CARTESIAN_POINT('Ctrl Pts',(-6.70102516100005,11.6,7.95812553699999));
#242076=CARTESIAN_POINT('Ctrl Pts',(-6.70038713700006,15.2,7.95716596799998));
#242077=CARTESIAN_POINT('Ctrl Pts',(-6.70038713700006,11.6,7.95716596799998));
#242078=CARTESIAN_POINT('Ctrl Pts',(-6.69975313400006,15.2,7.95621447499999));
#242079=CARTESIAN_POINT('Ctrl Pts',(-6.69975313400006,11.6,7.95621447499999));
#242080=CARTESIAN_POINT('Ctrl Pts',(-6.69912317900006,15.2,7.95527106999998));
#242081=CARTESIAN_POINT('Ctrl Pts',(-6.69912317900006,11.6,7.95527106999998));
#242082=CARTESIAN_POINT('Ctrl Pts',(-6.69849730200006,15.2,7.95433576299998));
#242083=CARTESIAN_POINT('Ctrl Pts',(-6.69849730200006,11.6,7.95433576299998));
#242084=CARTESIAN_POINT('Ctrl Pts',(-6.69787552700006,15.2,7.95340856399999));
#242085=CARTESIAN_POINT('Ctrl Pts',(-6.69787552700006,11.6,7.95340856399999));
#242086=CARTESIAN_POINT('Ctrl Pts',(-6.69725788400005,15.2,7.95248948499999));
#242087=CARTESIAN_POINT('Ctrl Pts',(-6.69725788400005,11.6,7.95248948499999));
#242088=CARTESIAN_POINT('Ctrl Pts',(-6.69664439800005,15.2,7.95157853799999));
#242089=CARTESIAN_POINT('Ctrl Pts',(-6.69664439800005,11.6,7.95157853799999));
#242090=CARTESIAN_POINT('Ctrl Pts',(-6.69603510100006,15.2,7.95067573199999));
#242091=CARTESIAN_POINT('Ctrl Pts',(-6.69603510100006,11.6,7.95067573199999));
#242092=CARTESIAN_POINT('Ctrl Pts',(-6.69543001600006,15.2,7.94978107899999));
#242093=CARTESIAN_POINT('Ctrl Pts',(-6.69543001600006,11.6,7.94978107899999));
#242094=CARTESIAN_POINT('Ctrl Pts',(-6.69482917600006,15.2,7.94889459099998));
#242095=CARTESIAN_POINT('Ctrl Pts',(-6.69482917600006,11.6,7.94889459099998));
#242096=CARTESIAN_POINT('Ctrl Pts',(-6.69423260600006,15.2,7.94801627699999));
#242097=CARTESIAN_POINT('Ctrl Pts',(-6.69423260600006,11.6,7.94801627699999));
#242098=CARTESIAN_POINT('Ctrl Pts',(-6.69364033500006,15.2,7.94714614999998));
#242099=CARTESIAN_POINT('Ctrl Pts',(-6.69364033500006,11.6,7.94714614999998));
#242100=CARTESIAN_POINT('Ctrl Pts',(-6.69305239300006,15.2,7.94628422099999));
#242101=CARTESIAN_POINT('Ctrl Pts',(-6.69305239300006,11.6,7.94628422099999));
#242102=CARTESIAN_POINT('Ctrl Pts',(-6.69246880700006,15.2,7.94543049999999));
#242103=CARTESIAN_POINT('Ctrl Pts',(-6.69246880700006,11.6,7.94543049999999));
#242104=CARTESIAN_POINT('Ctrl Pts',(-6.69188960600006,15.2,7.94458499899999));
#242105=CARTESIAN_POINT('Ctrl Pts',(-6.69188960600006,11.6,7.94458499899999));
#242106=CARTESIAN_POINT('Ctrl Pts',(-6.69131482100005,15.2,7.94374772999999));
#242107=CARTESIAN_POINT('Ctrl Pts',(-6.69131482100005,11.6,7.94374772999999));
#242108=CARTESIAN_POINT('Ctrl Pts',(-6.69074447800006,15.2,7.94291870399999));
#242109=CARTESIAN_POINT('Ctrl Pts',(-6.69074447800006,11.6,7.94291870399999));
#242110=CARTESIAN_POINT('Ctrl Pts',(-6.69017860900006,15.2,7.94209793299999));
#242111=CARTESIAN_POINT('Ctrl Pts',(-6.69017860900006,11.6,7.94209793299999));
#242112=CARTESIAN_POINT('Ctrl Pts',(-6.68961724200006,15.2,7.94128542699998));
#242113=CARTESIAN_POINT('Ctrl Pts',(-6.68961724200006,11.6,7.94128542699998));
#242114=CARTESIAN_POINT('Ctrl Pts',(-6.68906040700006,15.2,7.94048119799999));
#242115=CARTESIAN_POINT('Ctrl Pts',(-6.68906040700006,11.6,7.94048119799999));
#242116=CARTESIAN_POINT('Ctrl Pts',(-6.68850813400006,15.2,7.93968525899999));
#242117=CARTESIAN_POINT('Ctrl Pts',(-6.68850813400006,11.6,7.93968525899999));
#242118=CARTESIAN_POINT('Ctrl Pts',(-6.68796045100006,15.2,7.93889761999999));
#242119=CARTESIAN_POINT('Ctrl Pts',(-6.68796045100006,11.6,7.93889761999999));
#242120=CARTESIAN_POINT('Ctrl Pts',(-6.68741739100006,15.2,7.93811829299998));
#242121=CARTESIAN_POINT('Ctrl Pts',(-6.68741739100006,11.6,7.93811829299998));
#242122=CARTESIAN_POINT('Ctrl Pts',(-6.68687898200006,15.2,7.93734728999999));
#242123=CARTESIAN_POINT('Ctrl Pts',(-6.68687898200006,11.6,7.93734728999999));
#242124=CARTESIAN_POINT('Ctrl Pts',(-6.68634525600006,15.2,7.93658462199998));
#242125=CARTESIAN_POINT('Ctrl Pts',(-6.68634525600006,11.6,7.93658462199998));
#242126=CARTESIAN_POINT('Ctrl Pts',(-6.68581928800006,15.2,7.93583464699999));
#242127=CARTESIAN_POINT('Ctrl Pts',(-6.68581928800006,11.6,7.93583464699999));
#242128=CARTESIAN_POINT('Ctrl Pts',(-6.68540286400006,15.2,7.93524212599999));
#242129=CARTESIAN_POINT('Ctrl Pts',(-6.68540286400006,11.6,7.93524212599999));
#242130=CARTESIAN_POINT('Ctrl Pts',(-6.68509340700006,15.2,7.93480250499999));
#242131=CARTESIAN_POINT('Ctrl Pts',(-6.68509340700006,11.6,7.93480250499999));
#242132=CARTESIAN_POINT('Ctrl Pts',(-6.68488903500006,15.2,7.93451247199998));
#242133=CARTESIAN_POINT('Ctrl Pts',(-6.68488903500006,11.6,7.93451247199998));
#242134=CARTESIAN_POINT('Ctrl Pts',(-6.68478856800006,15.2,7.93436996999999));
#242135=CARTESIAN_POINT('Ctrl Pts',(-6.68478856800006,11.6,7.93436996999999));
#242136=CARTESIAN_POINT('',(-6.68478856800006,12.2,7.93436996999999));
#242137=CARTESIAN_POINT('',(-6.68478856800006,15.2,7.93436996999999));
#242138=CARTESIAN_POINT('',(-6.68478856800006,12.2,7.93436996999999));
#242139=CARTESIAN_POINT('Ctrl Pts',(-7.10901226900006,12.2,9.03946594399999));
#242140=CARTESIAN_POINT('Ctrl Pts',(-7.10820510876447,12.2,9.03572920290932));
#242141=CARTESIAN_POINT('Ctrl Pts',(-7.10739512190664,12.2,9.03199984245684));
#242142=CARTESIAN_POINT('Ctrl Pts',(-7.10658231406325,12.2,9.0282778601728));
#242143=CARTESIAN_POINT('Ctrl Pts',(-7.10576950621987,12.2,9.02455587788876));
#242144=CARTESIAN_POINT('Ctrl Pts',(-7.10495387608589,12.2,9.02084127356863));
#242145=CARTESIAN_POINT('Ctrl Pts',(-7.10413543695006,12.2,9.01713406172559));
#242146=CARTESIAN_POINT('Ctrl Pts',(-7.10331699781423,12.2,9.01342684988256));
#242147=CARTESIAN_POINT('Ctrl Pts',(-7.10249574876606,12.2,9.00972702820508));
#242148=CARTESIAN_POINT('Ctrl Pts',(-7.10167172592138,12.2,9.00603462587988));
#242149=CARTESIAN_POINT('Ctrl Pts',(-7.100847702927,12.2,9.0023422228839));
#242150=CARTESIAN_POINT('Ctrl Pts',(-7.10002090567351,12.2,8.99865723969837));
#242151=CARTESIAN_POINT('Ctrl Pts',(-7.09919137359424,12.2,8.99497970670658));
#242152=CARTESIAN_POINT('Ctrl Pts',(-7.09780882032972,12.2,8.98885048594438));
#242153=CARTESIAN_POINT('Ctrl Pts',(-7.09641866681232,12.2,8.9827419607242));
#242154=CARTESIAN_POINT('Ctrl Pts',(-7.0950210550756,12.2,8.97665424392032));
#242155=CARTESIAN_POINT('Ctrl Pts',(-7.09362344349122,12.2,8.97056652778002));
#242156=CARTESIAN_POINT('Ctrl Pts',(-7.09221836699138,12.2,8.96449961652235));
#242157=CARTESIAN_POINT('Ctrl Pts',(-7.09080597665981,12.2,8.95845362974909));
#242158=CARTESIAN_POINT('Ctrl Pts',(-7.08995854224534,12.2,8.95482603676251));
#242159=CARTESIAN_POINT('Ctrl Pts',(-7.0891084765218,12.2,8.95120597821974));
#242160=CARTESIAN_POINT('Ctrl Pts',(-7.08825581056419,12.2,8.94759347819574));
#242161=CARTESIAN_POINT('Ctrl Pts',(-7.08740314476148,12.2,8.94398097882802));
#242162=CARTESIAN_POINT('Ctrl Pts',(-7.08654787997558,12.2,8.94037603907659));
#242163=CARTESIAN_POINT('Ctrl Pts',(-7.08569004713153,12.2,8.93677868462462));
#242164=CARTESIAN_POINT('Ctrl Pts',(-7.08454627005807,12.2,8.93198221223983));
#242165=CARTESIAN_POINT('Ctrl Pts',(-7.08339792922195,12.2,8.92719922369441));
#242166=CARTESIAN_POINT('Ctrl Pts',(-7.08224510142567,12.2,8.92242977923376));
#242167=CARTESIAN_POINT('Ctrl Pts',(-7.08138048053918,12.2,8.9188526957258));
#242168=CARTESIAN_POINT('Ctrl Pts',(-7.08051333552438,12.2,8.9152832313314));
#242169=CARTESIAN_POINT('Ctrl Pts',(-7.07964370018132,12.2,8.91172141245974));
#242170=CARTESIAN_POINT('Ctrl Pts',(-7.07877406468027,12.2,8.90815959294103));
#242171=CARTESIAN_POINT('Ctrl Pts',(-7.07790193908686,12.2,8.90460541902451));
#242172=CARTESIAN_POINT('Ctrl Pts',(-7.07702735608441,12.2,8.90105891551013));
#242173=CARTESIAN_POINT('Ctrl Pts',(-7.07615277324085,12.2,8.89751241264003));
#242174=CARTESIAN_POINT('Ctrl Pts',(-7.07527573325576,12.2,8.89397358151954));
#242175=CARTESIAN_POINT('Ctrl Pts',(-7.0743962699125,12.2,8.8904424471485));
#242176=CARTESIAN_POINT('Ctrl Pts',(-7.07351680656924,12.2,8.88691131277746));
#242177=CARTESIAN_POINT('Ctrl Pts',(-7.0726349195545,12.2,8.88338787511826));
#242178=CARTESIAN_POINT('Ctrl Pts',(-7.07175064274927,12.2,8.87987216023008));
#242179=CARTESIAN_POINT('Ctrl Pts',(-7.07086636594404,12.2,8.8763564453419));
#242180=CARTESIAN_POINT('Ctrl Pts',(-7.06997969982261,12.2,8.8728484526252));
#242181=CARTESIAN_POINT('Ctrl Pts',(-7.06909067747588,12.2,8.86934820973645));
#242182=CARTESIAN_POINT('Ctrl Pts',(-7.06820165512916,12.2,8.8658479668477));
#242183=CARTESIAN_POINT('Ctrl Pts',(-7.06731027678143,12.2,8.86235547373728));
#242184=CARTESIAN_POINT('Ctrl Pts',(-7.06641657789745,12.2,8.85887075536323));
#242185=CARTESIAN_POINT('Ctrl Pts',(-7.06552287901346,12.2,8.85538603698917));
#242186=CARTESIAN_POINT('Ctrl Pts',(-7.06462685867962,12.2,8.85190909388126));
#242187=CARTESIAN_POINT('Ctrl Pts',(-7.06372855096257,12.2,8.8484399520062));
#242188=CARTESIAN_POINT('Ctrl Pts',(-7.06283024308231,12.2,8.84497080950092));
#242189=CARTESIAN_POINT('Ctrl Pts',(-7.06192964918477,12.2,8.84150946848127));
#242190=CARTESIAN_POINT('Ctrl Pts',(-7.06102680276158,12.2,8.83805595498041));
#242191=CARTESIAN_POINT('Ctrl Pts',(-7.06012395650241,12.2,8.83460244210694));
#242192=CARTESIAN_POINT('Ctrl Pts',(-7.05921885898503,12.2,8.83115675699975));
#242193=CARTESIAN_POINT('Ctrl Pts',(-7.05831154418447,12.2,8.82771892562534));
#242194=CARTESIAN_POINT('Ctrl Pts',(-7.05740422938391,12.2,8.82428109425093));
#242195=CARTESIAN_POINT('Ctrl Pts',(-7.05649469778694,12.2,8.82085111663799));
#242196=CARTESIAN_POINT('Ctrl Pts',(-7.05558298448258,12.2,8.81742901970516));
#242197=CARTESIAN_POINT('Ctrl Pts',(-7.05467127117822,12.2,8.81400692277234));
#242198=CARTESIAN_POINT('Ctrl Pts',(-7.05375737607178,12.2,8.81059270517812));
#242199=CARTESIAN_POINT('Ctrl Pts',(-7.05284133526757,12.2,8.80718639520303));
#242200=CARTESIAN_POINT('Ctrl Pts',(-7.05192529446337,12.2,8.80378008522795));
#242201=CARTESIAN_POINT('Ctrl Pts',(-7.05100710835006,12.2,8.80038168184715));
#242202=CARTESIAN_POINT('Ctrl Pts',(-7.05008681113368,12.2,8.79699121138628));
#242203=CARTESIAN_POINT('Ctrl Pts',(-7.04885974806704,12.2,8.7924705836945));
#242204=CARTESIAN_POINT('Ctrl Pts',(-7.04762893401108,12.2,8.78796405849062));
#242205=CARTESIAN_POINT('Ctrl Pts',(-7.04639445416578,12.2,8.78347170085781));
#242206=CARTESIAN_POINT('Ctrl Pts',(-7.0454685943659,12.2,8.78010243293924));
#242207=CARTESIAN_POINT('Ctrl Pts',(-7.044540672753,12.2,8.77674113294025));
#242208=CARTESIAN_POINT('Ctrl Pts',(-7.04361072549089,12.2,8.77338782850523));
#242209=CARTESIAN_POINT('Ctrl Pts',(-7.04237079586439,12.2,8.76891675612827));
#242210=CARTESIAN_POINT('Ctrl Pts',(-7.04112726599888,12.2,8.76445989729794));
#242211=CARTESIAN_POINT('Ctrl Pts',(-7.03988022171229,12.2,8.76001731499296));
#242212=CARTESIAN_POINT('Ctrl Pts',(-7.03894493828496,12.2,8.7566853775076));
#242213=CARTESIAN_POINT('Ctrl Pts',(-7.03800767816541,12.2,8.75336147084121));
#242214=CARTESIAN_POINT('Ctrl Pts',(-7.03706847877865,12.2,8.75004562181874));
#242215=CARTESIAN_POINT('Ctrl Pts',(-7.03612927956251,12.2,8.74672977339866));
#242216=CARTESIAN_POINT('Ctrl Pts',(-7.03518814159647,12.2,8.74342198123646));
#242217=CARTESIAN_POINT('Ctrl Pts',(-7.03424510133891,12.2,8.74012227435707));
#242218=CARTESIAN_POINT('Ctrl Pts',(-7.03330206108135,12.2,8.73682256747767));
#242219=CARTESIAN_POINT('Ctrl Pts',(-7.03235711881911,12.2,8.73353094505917));
#242220=CARTESIAN_POINT('Ctrl Pts',(-7.03141031247421,12.2,8.73024743320529));
#242221=CARTESIAN_POINT('Ctrl Pts',(-7.03046350612931,12.2,8.7269639213514));
#242222=CARTESIAN_POINT('Ctrl Pts',(-7.02951483450403,12.2,8.72368852088237));
#242223=CARTESIAN_POINT('Ctrl Pts',(-7.0285643367426,12.2,8.72042125848624));
#242224=CARTESIAN_POINT('Ctrl Pts',(-7.02761383898117,12.2,8.71715399609011));
#242225=CARTESIAN_POINT('Ctrl Pts',(-7.02666151566921,12.2,8.71389487227034));
#242226=CARTESIAN_POINT('Ctrl Pts',(-7.0257074038707,12.2,8.71064391288775));
#242227=CARTESIAN_POINT('Ctrl Pts',(-7.0247532920722,12.2,8.70739295350516));
#242228=CARTESIAN_POINT('Ctrl Pts',(-7.0237973912738,12.2,8.70415015888866));
#242229=CARTESIAN_POINT('Ctrl Pts',(-7.0228397414755,12.2,8.70091555696341));
#242230=CARTESIAN_POINT('Ctrl Pts',(-7.02188209150322,12.2,8.69768095445053));
#242231=CARTESIAN_POINT('Ctrl Pts',(-7.02092269168046,12.2,8.69445454353162));
#242232=CARTESIAN_POINT('Ctrl Pts',(-7.01996158033221,12.2,8.69123635206505));
#242233=CARTESIAN_POINT('Ctrl Pts',(-7.01900046915858,12.2,8.68801816118312));
#242234=CARTESIAN_POINT('Ctrl Pts',(-7.01803764759345,12.2,8.68480818968989));
#242235=CARTESIAN_POINT('Ctrl Pts',(-7.01707315428845,12.2,8.68160646464722));
#242236=CARTESIAN_POINT('Ctrl Pts',(-7.01578716327352,12.2,8.67733749811756));
#242237=CARTESIAN_POINT('Ctrl Pts',(-7.01449819990541,12.2,8.67308319145381));
#242238=CARTESIAN_POINT('Ctrl Pts',(-7.01320635712231,12.2,8.66884360985499));
#242239=CARTESIAN_POINT('Ctrl Pts',(-7.01191451416321,12.2,8.66460402767853));
#242240=CARTESIAN_POINT('Ctrl Pts',(-7.01061979363152,12.2,8.66037917167046));
#242241=CARTESIAN_POINT('Ctrl Pts',(-7.00932228789397,12.2,8.65616910416423));
#242242=CARTESIAN_POINT('Ctrl Pts',(-7.00802478233321,12.2,8.65195903723164));
#242243=CARTESIAN_POINT('Ctrl Pts',(-7.00672449235858,12.2,8.64776376044167));
#242244=CARTESIAN_POINT('Ctrl Pts',(-7.00542151395579,12.2,8.64358333857328));
#242245=CARTESIAN_POINT('Ctrl Pts',(-7.00411853537546,12.2,8.63940291613529));
#242246=CARTESIAN_POINT('Ctrl Pts',(-7.00281286668399,12.2,8.63523734875263));
#242247=CARTESIAN_POINT('Ctrl Pts',(-7.00150460633476,12.2,8.63108670119408));
#242248=CARTESIAN_POINT('Ctrl Pts',(-7.00019634616377,12.2,8.62693605420107));
#242249=CARTESIAN_POINT('Ctrl Pts',(-6.99888549384329,12.2,8.62280032821055));
#242250=CARTESIAN_POINT('Ctrl Pts',(-6.99757214500646,12.2,8.61867958665701));
#242251=CARTESIAN_POINT('Ctrl Pts',(-6.9962587959907,12.2,8.61455884454202));
#242252=CARTESIAN_POINT('Ctrl Pts',(-6.99494295321589,12.2,8.61045308979414));
#242253=CARTESIAN_POINT('Ctrl Pts',(-6.99362471224917,12.2,8.60636238499715));
#242254=CARTESIAN_POINT('Ctrl Pts',(-6.99230647146207,12.2,8.60227168075752));
#242255=CARTESIAN_POINT('Ctrl Pts',(-6.99098583494687,12.2,8.59819602863621));
#242256=CARTESIAN_POINT('Ctrl Pts',(-6.9896628994997,12.2,8.59413549368883));
#242257=CARTESIAN_POINT('Ctrl Pts',(-6.98833996387227,12.2,8.5900749581882));
#242258=CARTESIAN_POINT('Ctrl Pts',(-6.9870147311252,12.2,8.58602954099459));
#242259=CARTESIAN_POINT('Ctrl Pts',(-6.98568730144173,12.2,8.58199930627492));
#242260=CARTESIAN_POINT('Ctrl Pts',(-6.98402801442784,12.2,8.57696151314989));
#242261=CARTESIAN_POINT('Ctrl Pts',(-6.9823652933734,12.2,8.57194744614203));
#242262=CARTESIAN_POINT('Ctrl Pts',(-6.98069933878249,12.2,8.5669572320222));
#242263=CARTESIAN_POINT('Ctrl Pts',(-6.97936657521871,12.2,8.56296506105269));
#242264=CARTESIAN_POINT('Ctrl Pts',(-6.9780317408897,12.2,8.55898815627535));
#242265=CARTESIAN_POINT('Ctrl Pts',(-6.97669493994363,12.2,8.55502658593098));
#242266=CARTESIAN_POINT('Ctrl Pts',(-6.97535813881543,12.2,8.55106501504685));
#242267=CARTESIAN_POINT('Ctrl Pts',(-6.97401937026479,12.2,8.54711877746137));
#242268=CARTESIAN_POINT('Ctrl Pts',(-6.97267873802507,12.2,8.5431879411916));
#242269=CARTESIAN_POINT('Ctrl Pts',(-6.97133810578533,12.2,8.53925710492183));
#242270=CARTESIAN_POINT('Ctrl Pts',(-6.96999561026206,12.2,8.53534166874273));
#242271=CARTESIAN_POINT('Ctrl Pts',(-6.96865135602194,12.2,8.53144170058729));
#242272=CARTESIAN_POINT('Ctrl Pts',(-6.96730710196498,12.2,8.52754173296322));
#242273=CARTESIAN_POINT('Ctrl Pts',(-6.96596109052192,12.2,8.52365723225668));
#242274=CARTESIAN_POINT('Ctrl Pts',(-6.96461342579265,12.2,8.51978826727756));
#242275=CARTESIAN_POINT('Ctrl Pts',(-6.96326576087975,12.2,8.5159193017713));
#242276=CARTESIAN_POINT('Ctrl Pts',(-6.96191644408631,12.2,8.51206587156335));
#242277=CARTESIAN_POINT('Ctrl Pts',(-6.96056558301253,12.2,8.50822804535579));
#242278=CARTESIAN_POINT('Ctrl Pts',(-6.95921472212282,12.2,8.50439021967113));
#242279=CARTESIAN_POINT('Ctrl Pts',(-6.95786231535552,12.2,8.50056799663723));
#242280=CARTESIAN_POINT('Ctrl Pts',(-6.95650847257739,12.2,8.49676144500292));
#242281=CARTESIAN_POINT('Ctrl Pts',(-6.9551546296148,12.2,8.49295489284995));
#242282=CARTESIAN_POINT('Ctrl Pts',(-6.95379934985484,12.2,8.48916401246561));
#242283=CARTESIAN_POINT('Ctrl Pts',(-6.95244274361415,12.2,8.48538887098312));
#242284=CARTESIAN_POINT('Ctrl Pts',(-6.9510861375583,12.2,8.481613730015));
#242285=CARTESIAN_POINT('Ctrl Pts',(-6.94972820553451,12.2,8.47785432892837));
#242286=CARTESIAN_POINT('Ctrl Pts',(-6.94836905618894,12.2,8.47411073576822));
#242287=CARTESIAN_POINT('Ctrl Pts',(-6.94700990665817,12.2,8.470367142098));
#242288=CARTESIAN_POINT('Ctrl Pts',(-6.94564954147412,12.2,8.46663935695341));
#242289=CARTESIAN_POINT('Ctrl Pts',(-6.94428807262208,12.2,8.46292744819661));
#242290=CARTESIAN_POINT('Ctrl Pts',(-6.94292660395554,12.2,8.45921553994557));
#242291=CARTESIAN_POINT('Ctrl Pts',(-6.9415640318531,12.2,8.45551950956632));
#242292=CARTESIAN_POINT('Ctrl Pts',(-6.94020046846467,12.2,8.45183942580995));
#242293=CARTESIAN_POINT('Ctrl Pts',(-6.93883690489044,12.2,8.44815934155217));
#242294=CARTESIAN_POINT('Ctrl Pts',(-6.93747235057141,12.2,8.444495202485));
#242295=CARTESIAN_POINT('Ctrl Pts',(-6.9361069209908,12.2,8.44084707971411));
#242296=CARTESIAN_POINT('Ctrl Pts',(-6.93474149159622,12.2,8.43719895744027));
#242297=CARTESIAN_POINT('Ctrl Pts',(-6.93337518520063,12.2,8.43356685075275));
#242298=CARTESIAN_POINT('Ctrl Pts',(-6.93200811975691,12.2,8.42995082982447));
#242299=CARTESIAN_POINT('Ctrl Pts',(-6.93064105412692,12.2,8.42633480840351));
#242300=CARTESIAN_POINT('Ctrl Pts',(-6.92927322709964,12.2,8.42273487326746));
#242301=CARTESIAN_POINT('Ctrl Pts',(-6.92790475819173,12.2,8.41915109251658));
#242302=CARTESIAN_POINT('Ctrl Pts',(-6.92653628928381,12.2,8.41556731176571));
#242303=CARTESIAN_POINT('Ctrl Pts',(-6.92516717622027,12.2,8.41199968762786));
#242304=CARTESIAN_POINT('Ctrl Pts',(-6.92379754053446,12.2,8.40844828943595));
#242305=CARTESIAN_POINT('Ctrl Pts',(-6.92242790503526,12.2,8.40489689172791));
#242306=CARTESIAN_POINT('Ctrl Pts',(-6.92105774333963,12.2,8.4013617199196));
#242307=CARTESIAN_POINT('Ctrl Pts',(-6.91968717800099,12.2,8.39784284496899));
#242308=CARTESIAN_POINT('Ctrl Pts',(-6.91831661247562,12.2,8.39432396953894));
#242309=CARTESIAN_POINT('Ctrl Pts',(-6.91694564173117,12.2,8.39082138995437));
#242310=CARTESIAN_POINT('Ctrl Pts',(-6.91557438826753,12.2,8.38733517915494));
#242311=CARTESIAN_POINT('Ctrl Pts',(-6.91420313499071,12.2,8.3838489688305));
#242312=CARTESIAN_POINT('Ctrl Pts',(-6.9128315983806,12.2,8.38037912712338));
#242313=CARTESIAN_POINT('Ctrl Pts',(-6.91145990110386,12.2,8.37692572351573));
#242314=CARTESIAN_POINT('Ctrl Pts',(-6.91008820364023,12.2,8.37347231943755));
#242315=CARTESIAN_POINT('Ctrl Pts',(-6.90871634551375,12.2,8.37003535489566));
#242316=CARTESIAN_POINT('Ctrl Pts',(-6.90734445009265,12.2,8.36661490126201));
#242317=CARTESIAN_POINT('Ctrl Pts',(-6.90597255485848,12.2,8.3631944480944));
#242318=CARTESIAN_POINT('Ctrl Pts',(-6.90460062321396,12.2,8.35979050523729));
#242319=CARTESIAN_POINT('Ctrl Pts',(-6.90322878060387,12.2,8.35640314623532));
#242320=CARTESIAN_POINT('Ctrl Pts',(-6.90151397720106,12.2,8.35216894713671));
#242321=CARTESIAN_POINT('Ctrl Pts',(-6.89979931333997,12.2,8.34796065897496));
#242322=CARTESIAN_POINT('Ctrl Pts',(-6.89808503514551,12.2,8.34377842251527));
#242323=CARTESIAN_POINT('Ctrl Pts',(-6.89671361251519,12.2,8.34043263316517));
#242324=CARTESIAN_POINT('Ctrl Pts',(-6.89534243782485,12.2,8.33710351748334));
#242325=CARTESIAN_POINT('Ctrl Pts',(-6.89397164029282,12.2,8.33379114852771));
#242326=CARTESIAN_POINT('Ctrl Pts',(-6.89260084294755,12.2,8.33047878002339));
#242327=CARTESIAN_POINT('Ctrl Pts',(-6.89123042266955,12.2,8.32718315837063));
#242328=CARTESIAN_POINT('Ctrl Pts',(-6.88986050883705,12.2,8.32390435602645));
#242329=CARTESIAN_POINT('Ctrl Pts',(-6.88849059481791,12.2,8.32062555323553));
#242330=CARTESIAN_POINT('Ctrl Pts',(-6.88712118751272,12.2,8.31736357026887));
#242331=CARTESIAN_POINT('Ctrl Pts',(-6.88575242010483,12.2,8.31411848025979));
#242332=CARTESIAN_POINT('Ctrl Pts',(-6.88438365288343,12.2,8.31087339069285));
#242333=CARTESIAN_POINT('Ctrl Pts',(-6.8830155249773,12.2,8.30764519532095));
#242334=CARTESIAN_POINT('Ctrl Pts',(-6.88164816913181,12.2,8.30443396619933));
#242335=CARTESIAN_POINT('Ctrl Pts',(-6.8802808131,12.2,8.30122273664016));
#242336=CARTESIAN_POINT('Ctrl Pts',(-6.87891423041834,12.2,8.29802847458182));
#242337=CARTESIAN_POINT('Ctrl Pts',(-6.87754855512175,12.2,8.29485125446535));
#242338=CARTESIAN_POINT('Ctrl Pts',(-6.87618288001124,12.2,8.29167403478178));
#242339=CARTESIAN_POINT('Ctrl Pts',(-6.87481811360331,12.2,8.2885138560975));
#242340=CARTESIAN_POINT('Ctrl Pts',(-6.87345439121469,12.2,8.28537079446382));
#242341=CARTESIAN_POINT('Ctrl Pts',(-6.87209066864026,12.2,8.28222773240188));
#242342=CARTESIAN_POINT('Ctrl Pts',(-6.87072799079894,12.2,8.27910178697295));
#242343=CARTESIAN_POINT('Ctrl Pts',(-6.86936649677413,12.2,8.27599303295615));
#242344=CARTESIAN_POINT('Ctrl Pts',(-6.86800500293482,12.2,8.27288427936291));
#242345=CARTESIAN_POINT('Ctrl Pts',(-6.86664469211685,12.2,8.26979271739471));
#242346=CARTESIAN_POINT('Ctrl Pts',(-6.86528570500558,12.2,8.26671842247757));
#242347=CARTESIAN_POINT('Ctrl Pts',(-6.86392671770914,12.2,8.26364412714155));
#242348=CARTESIAN_POINT('Ctrl Pts',(-6.86256905411841,12.2,8.26058709849891));
#242349=CARTESIAN_POINT('Ctrl Pts',(-6.86121285626672,12.2,8.25754741499992));
#242350=CARTESIAN_POINT('Ctrl Pts',(-6.85951760904449,12.2,8.25374781083325));
#242351=CARTESIAN_POINT('Ctrl Pts',(-6.85782465187901,12.2,8.24997530349814));
#242352=CARTESIAN_POINT('Ctrl Pts',(-6.85613426548246,12.2,8.24623004598121));
#242353=CARTESIAN_POINT('Ctrl Pts',(-6.85444387908591,12.2,8.2424847884643));
#242354=CARTESIAN_POINT('Ctrl Pts',(-6.8527560653175,12.2,8.23876677837395));
#242355=CARTESIAN_POINT('Ctrl Pts',(-6.85107110816487,12.2,8.23507616775038));
#242356=CARTESIAN_POINT('Ctrl Pts',(-6.84938615101224,12.2,8.23138555712683));
#242357=CARTESIAN_POINT('Ctrl Pts',(-6.84770405040121,12.2,8.22772234645532));
#242358=CARTESIAN_POINT('Ctrl Pts',(-6.8460250988736,12.2,8.22408668576231));
#242359=CARTESIAN_POINT('Ctrl Pts',(-6.84434614734597,12.2,8.22045102506929));
#242360=CARTESIAN_POINT('Ctrl Pts',(-6.84267034271829,12.2,8.21684291401446));
#242361=CARTESIAN_POINT('Ctrl Pts',(-6.84099798139903,12.2,8.21326250901593));
#242362=CARTESIAN_POINT('Ctrl Pts',(-6.83899114788885,12.2,8.20896602317379));
#242363=CARTESIAN_POINT('Ctrl Pts',(-6.83698927177916,12.2,8.2047094274012));
#242364=CARTESIAN_POINT('Ctrl Pts',(-6.83499287325929,12.2,8.20049299370184));
#242365=CARTESIAN_POINT('Ctrl Pts',(-6.83332920776563,12.2,8.19697929882472));
#242366=CARTESIAN_POINT('Ctrl Pts',(-6.8316693463556,12.2,8.19349349127769));
#242367=CARTESIAN_POINT('Ctrl Pts',(-6.83001359350838,12.2,8.1900357297499));
#242368=CARTESIAN_POINT('Ctrl Pts',(-6.82835784066115,12.2,8.18657796822211));
#242369=CARTESIAN_POINT('Ctrl Pts',(-6.82670619727883,12.2,8.18314825062453));
#242370=CARTESIAN_POINT('Ctrl Pts',(-6.82505897525748,12.2,8.1797467334564));
#242371=CARTESIAN_POINT('Ctrl Pts',(-6.82341175323613,12.2,8.17634521628825));
#242372=CARTESIAN_POINT('Ctrl Pts',(-6.82176895281494,12.2,8.17297190092988));
#242373=CARTESIAN_POINT('Ctrl Pts',(-6.82013088913461,12.2,8.16962694530632));
#242374=CARTESIAN_POINT('Ctrl Pts',(-6.81849282545428,12.2,8.16628198968278));
#242375=CARTESIAN_POINT('Ctrl Pts',(-6.81685949770997,12.2,8.16296539310019));
#242376=CARTESIAN_POINT('Ctrl Pts',(-6.81523123062692,12.2,8.15967731581005));
#242377=CARTESIAN_POINT('Ctrl Pts',(-6.81360296354386,12.2,8.1563892385199));
#242378=CARTESIAN_POINT('Ctrl Pts',(-6.81197975514824,12.2,8.15312967960656));
#242379=CARTESIAN_POINT('Ctrl Pts',(-6.81036193305392,12.2,8.14989880139163));
#242380=CARTESIAN_POINT('Ctrl Pts',(-6.80874411095961,12.2,8.14666792317669));
#242381=CARTESIAN_POINT('Ctrl Pts',(-6.80713167445608,12.2,8.14346572471582));
#242382=CARTESIAN_POINT('Ctrl Pts',(-6.80552495903989,12.2,8.14029236909318));
#242383=CARTESIAN_POINT('Ctrl Pts',(-6.80391824362369,12.2,8.13711901347056));
#242384=CARTESIAN_POINT('Ctrl Pts',(-6.80231724744094,12.2,8.13397449881783));
#242385=CARTESIAN_POINT('Ctrl Pts',(-6.80072230973309,12.2,8.13085899229242));
#242386=CARTESIAN_POINT('Ctrl Pts',(-6.79912737219911,12.2,8.12774348610661));
#242387=CARTESIAN_POINT('Ctrl Pts',(-6.79753849293507,12.2,8.1246569853523));
#242388=CARTESIAN_POINT('Ctrl Pts',(-6.79595601789869,12.2,8.12159965609981));
#242389=CARTESIAN_POINT('Ctrl Pts',(-6.79437354268982,12.2,8.11854232651406));
#242390=CARTESIAN_POINT('Ctrl Pts',(-6.79279746987807,12.2,8.11551417021121));
#242391=CARTESIAN_POINT('Ctrl Pts',(-6.79122815369698,12.2,8.11251535208383));
#242392=CARTESIAN_POINT('Ctrl Pts',(-6.78965883751588,12.2,8.10951653395645));
#242393=CARTESIAN_POINT('Ctrl Pts',(-6.78809627455882,12.2,8.10654705507356));
#242394=CARTESIAN_POINT('Ctrl Pts',(-6.78654082593896,12.2,8.10360708284131));
#242395=CARTESIAN_POINT('Ctrl Pts',(-6.7846742874934,12.2,8.10007911597033));
#242396=CARTESIAN_POINT('Ctrl Pts',(-6.7828179900404,12.2,8.09659364105941));
#242397=CARTESIAN_POINT('Ctrl Pts',(-6.78097256402388,12.2,8.09315095137466));
#242398=CARTESIAN_POINT('Ctrl Pts',(-6.779127138175,12.2,8.08970826200263));
#242399=CARTESIAN_POINT('Ctrl Pts',(-6.77729258656622,12.2,8.08630835871654));
#242400=CARTESIAN_POINT('Ctrl Pts',(-6.77546955154088,12.2,8.08295153924006));
#242401=CARTESIAN_POINT('Ctrl Pts',(-6.77364651651555,12.2,8.07959471976359));
#242402=CARTESIAN_POINT('Ctrl Pts',(-6.77183499715831,12.2,8.0762809853114));
#242403=CARTESIAN_POINT('Ctrl Pts',(-6.77003565613982,12.2,8.07301063592833));
#242404=CARTESIAN_POINT('Ctrl Pts',(-6.7682363149579,12.2,8.0697402862482));
#242405=CARTESIAN_POINT('Ctrl Pts',(-6.76644914785245,12.2,8.06651332560679));
#242406=CARTESIAN_POINT('Ctrl Pts',(-6.76467483475664,12.2,8.06333005593628));
#242407=CARTESIAN_POINT('Ctrl Pts',(-6.76290052182198,12.2,8.06014678655492));
#242408=CARTESIAN_POINT('Ctrl Pts',(-6.76113905801572,12.2,8.05700721071698));
#242409=CARTESIAN_POINT('Ctrl Pts',(-6.75939113816316,12.2,8.05391163833139));
#242410=CARTESIAN_POINT('Ctrl Pts',(-6.7576432183106,12.2,8.05081606594578));
#242411=CARTESIAN_POINT('Ctrl Pts',(-6.75590883844864,12.2,8.04776449707332));
#242412=CARTESIAN_POINT('Ctrl Pts',(-6.75418870884384,12.2,8.04475724668065));
#242413=CARTESIAN_POINT('Ctrl Pts',(-6.75218189086742,12.2,8.0412487877071));
#242414=CARTESIAN_POINT('Ctrl Pts',(-6.75019446584363,12.2,8.03780064964788));
#242415=CARTESIAN_POINT('Ctrl Pts',(-6.74822758646655,12.2,8.03441334308353));
#242416=CARTESIAN_POINT('Ctrl Pts',(-6.74654168994513,12.2,8.03150993760765));
#242417=CARTESIAN_POINT('Ctrl Pts',(-6.74487088876418,12.2,8.02865122335319));
#242418=CARTESIAN_POINT('Ctrl Pts',(-6.74321592732362,12.2,8.02583752512011));
#242419=CARTESIAN_POINT('Ctrl Pts',(-6.74156096573273,12.2,8.02302382663146));
#242420=CARTESIAN_POINT('Ctrl Pts',(-6.73992184356047,12.2,8.02025514675672));
#242421=CARTESIAN_POINT('Ctrl Pts',(-6.73829932680651,12.2,8.01753181219474));
#242422=CARTESIAN_POINT('Ctrl Pts',(-6.73667681019993,12.2,8.01480847788012));
#242423=CARTESIAN_POINT('Ctrl Pts',(-6.73507089530507,12.2,8.0121304915007));
#242424=CARTESIAN_POINT('Ctrl Pts',(-6.73348236619686,12.2,8.00949818534832));
#242425=CARTESIAN_POINT('Ctrl Pts',(-6.73189383708866,12.2,8.00686587919593));
#242426=CARTESIAN_POINT('Ctrl Pts',(-6.73032269597908,12.2,8.00427925697325));
#242427=CARTESIAN_POINT('Ctrl Pts',(-6.72876974286807,12.2,8.00173865664689));
#242428=CARTESIAN_POINT('Ctrl Pts',(-6.72721678975705,12.2,7.99919805632055));
#242429=CARTESIAN_POINT('Ctrl Pts',(-6.72568202645312,12.2,7.99670347846429));
#242430=CARTESIAN_POINT('Ctrl Pts',(-6.72416627542358,12.2,7.99425527105011));
#242431=CARTESIAN_POINT('Ctrl Pts',(-6.72265052425637,12.2,7.99180706341354));
#242432=CARTESIAN_POINT('Ctrl Pts',(-6.72115378614092,12.2,7.98940522486475));
#242433=CARTESIAN_POINT('Ctrl Pts',(-6.71967690797795,12.2,7.98705010840508));
#242434=CARTESIAN_POINT('Ctrl Pts',(-6.71820002994913,12.2,7.98469499215934));
#242435=CARTESIAN_POINT('Ctrl Pts',(-6.71674300878007,12.2,7.98238659732083));
#242436=CARTESIAN_POINT('Ctrl Pts',(-6.71530671774234,12.2,7.98012528497593));
#242437=CARTESIAN_POINT('Ctrl Pts',(-6.71387042670461,12.2,7.97786397263103));
#242438=CARTESIAN_POINT('Ctrl Pts',(-6.71245486184446,12.2,7.97564974104394));
#242439=CARTESIAN_POINT('Ctrl Pts',(-6.71106091814363,12.2,7.9734829567861));
#242440=CARTESIAN_POINT('Ctrl Pts',(-6.70966697431618,12.2,7.97131617233144));
#242441=CARTESIAN_POINT('Ctrl Pts',(-6.70829465092583,12.2,7.96919683522989));
#242442=CARTESIAN_POINT('Ctrl Pts',(-6.7069448661195,12.2,7.96712531684963));
#242443=CARTESIAN_POINT('Ctrl Pts',(-6.70537011736268,12.2,7.96470854568825));
#242444=CARTESIAN_POINT('Ctrl Pts',(-6.70382604637675,12.2,7.96235686321937));
#242445=CARTESIAN_POINT('Ctrl Pts',(-6.70231415214961,12.2,7.96007087199682));
#242446=CARTESIAN_POINT('Ctrl Pts',(-6.70101824266072,12.2,7.95811145072011));
#242447=CARTESIAN_POINT('Ctrl Pts',(-6.69974597505825,12.2,7.95620029419487));
#242448=CARTESIAN_POINT('Ctrl Pts',(-6.69849832742938,12.2,7.95433778983651));
#242449=CARTESIAN_POINT('Ctrl Pts',(-6.69725067991383,12.2,7.95247528564732));
#242450=CARTESIAN_POINT('Ctrl Pts',(-6.69602764898984,12.2,7.95066143463579));
#242451=CARTESIAN_POINT('Ctrl Pts',(-6.69483024353334,12.2,7.94889663453322));
#242452=CARTESIAN_POINT('Ctrl Pts',(-6.69363283807683,12.2,7.94713183443065));
#242453=CARTESIAN_POINT('Ctrl Pts',(-6.69246105484464,12.2,7.94541608402843));
#242454=CARTESIAN_POINT('Ctrl Pts',(-6.69131593166085,12.2,7.94374979091955));
#242455=CARTESIAN_POINT('Ctrl Pts',(-6.69017080837305,12.2,7.94208349765932));
#242456=CARTESIAN_POINT('Ctrl Pts',(-6.68905234456365,12.2,7.94046666191108));
#242457=CARTESIAN_POINT('Ctrl Pts',(-6.68796160658946,12.2,7.93889969782912));
#242458=CARTESIAN_POINT('Ctrl Pts',(-6.68687610346005,12.2,7.93734025417272));
#242459=CARTESIAN_POINT('Ctrl Pts',(-6.68581806471473,12.2,7.93583020411499));
#242460=CARTESIAN_POINT('Ctrl Pts',(-6.68478856800006,12.2,7.93436996999999));
#242461=CARTESIAN_POINT('Ctrl Pts',(-6.68478856800006,15.2,7.93436996999999));
#242462=CARTESIAN_POINT('Ctrl Pts',(-6.68581806471473,15.2,7.93583020411499));
#242463=CARTESIAN_POINT('Ctrl Pts',(-6.68687610346001,15.2,7.93734025417266));
#242464=CARTESIAN_POINT('Ctrl Pts',(-6.68796160658946,15.2,7.93889969782911));
#242465=CARTESIAN_POINT('Ctrl Pts',(-6.68905234456369,15.2,7.94046666191113));
#242466=CARTESIAN_POINT('Ctrl Pts',(-6.69017080837302,15.2,7.94208349765928));
#242467=CARTESIAN_POINT('Ctrl Pts',(-6.69131593166085,15.2,7.94374979091955));
#242468=CARTESIAN_POINT('Ctrl Pts',(-6.69246105484467,15.2,7.94541608402847));
#242469=CARTESIAN_POINT('Ctrl Pts',(-6.69363283807684,15.2,7.94713183443067));
#242470=CARTESIAN_POINT('Ctrl Pts',(-6.69483024353334,15.2,7.94889663453323));
#242471=CARTESIAN_POINT('Ctrl Pts',(-6.69602764898984,15.2,7.95066143463578));
#242472=CARTESIAN_POINT('Ctrl Pts',(-6.69725067991382,15.2,7.9524752856473));
#242473=CARTESIAN_POINT('Ctrl Pts',(-6.69849832742937,15.2,7.9543377898365));
#242474=CARTESIAN_POINT('Ctrl Pts',(-6.69974597505826,15.2,7.95620029419488));
#242475=CARTESIAN_POINT('Ctrl Pts',(-6.70101824266071,15.2,7.95811145072009));
#242476=CARTESIAN_POINT('Ctrl Pts',(-6.70231415214961,15.2,7.96007087199682));
#242477=CARTESIAN_POINT('Ctrl Pts',(-6.7036100615208,15.2,7.96203029309558));
#242478=CARTESIAN_POINT('Ctrl Pts',(-6.70492961203493,15.2,7.9640379764411));
#242479=CARTESIAN_POINT('Ctrl Pts',(-6.7062718567423,15.2,7.96609354445918));
#242480=CARTESIAN_POINT('Ctrl Pts',(-6.70761410144967,15.2,7.96814911247727));
#242481=CARTESIAN_POINT('Ctrl Pts',(-6.70897904139254,15.2,7.97025256060477));
#242482=CARTESIAN_POINT('Ctrl Pts',(-6.71036575217453,15.2,7.97240351960788));
#242483=CARTESIAN_POINT('Ctrl Pts',(-6.71175246308249,15.2,7.97455447880635));
#242484=CARTESIAN_POINT('Ctrl Pts',(-6.71316094577651,15.2,7.97675294581909));
#242485=CARTESIAN_POINT('Ctrl Pts',(-6.71459030368916,15.2,7.97899855427803));
#242486=CARTESIAN_POINT('Ctrl Pts',(-6.71601966147198,15.2,7.98124416253299));
#242487=CARTESIAN_POINT('Ctrl Pts',(-6.71746989292446,15.2,7.98353691334393));
#242488=CARTESIAN_POINT('Ctrl Pts',(-6.71894012778856,15.2,7.98587644559427));
#242489=CARTESIAN_POINT('Ctrl Pts',(-6.72041036265266,15.2,7.9882159778446));
#242490=CARTESIAN_POINT('Ctrl Pts',(-6.72190059904019,15.2,7.99060229029125));
#242491=CARTESIAN_POINT('Ctrl Pts',(-6.72340998815117,15.2,7.99303503236752));
#242492=CARTESIAN_POINT('Ctrl Pts',(-6.72491937726217,15.2,7.99546777444376));
#242493=CARTESIAN_POINT('Ctrl Pts',(-6.72644791950553,15.2,7.99794694257784));
#242494=CARTESIAN_POINT('Ctrl Pts',(-6.72799478578142,15.2,8.000472192733));
#242495=CARTESIAN_POINT('Ctrl Pts',(-6.72954165219784,15.2,8.00299744311753));
#242496=CARTESIAN_POINT('Ctrl Pts',(-6.73110684411601,15.2,8.00556877248147));
#242497=CARTESIAN_POINT('Ctrl Pts',(-6.73268955453636,15.2,8.00818584112606));
#242498=CARTESIAN_POINT('Ctrl Pts',(-6.73427226481293,15.2,8.01080290953295));
#242499=CARTESIAN_POINT('Ctrl Pts',(-6.73587249451741,15.2,8.01346571642655));
#242500=CARTESIAN_POINT('Ctrl Pts',(-6.73748945579929,15.2,8.01617392575701));
#242501=CARTESIAN_POINT('Ctrl Pts',(-6.73910641708119,15.2,8.01888213508748));
#242502=CARTESIAN_POINT('Ctrl Pts',(-6.74074011055623,15.2,8.02163574622458));
#242503=CARTESIAN_POINT('Ctrl Pts',(-6.74238977007855,15.2,8.0244344287032));
#242504=CARTESIAN_POINT('Ctrl Pts',(-6.74403942975074,15.2,8.02723311143604));
#242505=CARTESIAN_POINT('Ctrl Pts',(-6.74570505504111,15.2,8.03007686676484));
#242506=CARTESIAN_POINT('Ctrl Pts',(-6.74738589955004,15.2,8.03296536642419));
#242507=CARTESIAN_POINT('Ctrl Pts',(-6.74906674390628,15.2,8.03585386582117));
#242508=CARTESIAN_POINT('Ctrl Pts',(-6.75076280499531,15.2,8.03878711137662));
#242509=CARTESIAN_POINT('Ctrl Pts',(-6.75247335552426,15.2,8.04176478078189));
#242510=CARTESIAN_POINT('Ctrl Pts',(-6.7541839060532,15.2,8.04474245018717));
#242511=CARTESIAN_POINT('Ctrl Pts',(-6.75590894320798,15.2,8.04776454395514));
#242512=CARTESIAN_POINT('Ctrl Pts',(-6.7576477578105,15.2,8.05083074542404));
#242513=CARTESIAN_POINT('Ctrl Pts',(-6.75938657257097,15.2,8.05389694717145));
#242514=CARTESIAN_POINT('Ctrl Pts',(-6.76113916048569,15.2,8.05700725707316));
#242515=CARTESIAN_POINT('Ctrl Pts',(-6.76290483117087,15.2,8.0601613630718));
#242516=CARTESIAN_POINT('Ctrl Pts',(-6.76467050169567,15.2,8.06331546878394));
#242517=CARTESIAN_POINT('Ctrl Pts',(-6.76644924912344,15.2,8.06651337068433));
#242518=CARTESIAN_POINT('Ctrl Pts',(-6.76824039797503,15.2,8.06975476023324));
#242519=CARTESIAN_POINT('Ctrl Pts',(-6.77003154682663,15.2,8.07299614978215));
#242520=CARTESIAN_POINT('Ctrl Pts',(-6.77183509503376,15.2,8.07628102945192));
#242521=CARTESIAN_POINT('Ctrl Pts',(-6.77365037905779,15.2,8.0796090921614));
#242522=CARTESIAN_POINT('Ctrl Pts',(-6.77546566324672,15.2,8.08293715517317));
#242523=CARTESIAN_POINT('Ctrl Pts',(-6.77729268209943,15.2,8.08630840419134));
#242524=CARTESIAN_POINT('Ctrl Pts',(-6.77913078720039,15.2,8.08972253613039));
#242525=CARTESIAN_POINT('Ctrl Pts',(-6.78096889213439,15.2,8.09313666775932));
#242526=CARTESIAN_POINT('Ctrl Pts',(-6.78281808346832,15.2,8.09659368458767));
#242527=CARTESIAN_POINT('Ctrl Pts',(-6.78467772449255,15.2,8.10009329105984));
#242528=CARTESIAN_POINT('Ctrl Pts',(-6.78653736551678,15.2,8.10359289753202));
#242529=CARTESIAN_POINT('Ctrl Pts',(-6.78840745708302,15.2,8.10713509117849));
#242530=CARTESIAN_POINT('Ctrl Pts',(-6.79028737718096,15.2,8.11071958262974));
#242531=CARTESIAN_POINT('Ctrl Pts',(-6.79185397731949,15.2,8.11370665894764));
#242532=CARTESIAN_POINT('Ctrl Pts',(-6.79342740458042,15.2,8.11672310687465));
#242533=CARTESIAN_POINT('Ctrl Pts',(-6.79500730395509,15.2,8.11976876006757));
#242534=CARTESIAN_POINT('Ctrl Pts',(-6.79658720332974,15.2,8.12281441326048));
#242535=CARTESIAN_POINT('Ctrl Pts',(-6.79817357701418,15.2,8.12588927274531));
#242536=CARTESIAN_POINT('Ctrl Pts',(-6.79976607729917,15.2,8.12899317081489));
#242537=CARTESIAN_POINT('Ctrl Pts',(-6.80167707757174,15.2,8.13271784836305));
#242538=CARTESIAN_POINT('Ctrl Pts',(-6.80359690061049,15.2,8.13648434248437));
#242539=CARTESIAN_POINT('Ctrl Pts',(-6.80552495903989,15.2,8.14029236909319));
#242540=CARTESIAN_POINT('Ctrl Pts',(-6.8071316744561,15.2,8.14346572471585));
#242541=CARTESIAN_POINT('Ctrl Pts',(-6.8087441109596,15.2,8.14666792317666));
#242542=CARTESIAN_POINT('Ctrl Pts',(-6.81036193305392,15.2,8.14989880139162));
#242543=CARTESIAN_POINT('Ctrl Pts',(-6.81197975514825,15.2,8.15312967960658));
#242544=CARTESIAN_POINT('Ctrl Pts',(-6.81360296354384,15.2,8.15638923851985));
#242545=CARTESIAN_POINT('Ctrl Pts',(-6.81523123062692,15.2,8.15967731581005));
#242546=CARTESIAN_POINT('Ctrl Pts',(-6.81718515123309,15.2,8.16362300877331));
#242547=CARTESIAN_POINT('Ctrl Pts',(-6.81914635879852,15.2,8.16760976851666));
#242548=CARTESIAN_POINT('Ctrl Pts',(-6.82111429348955,15.2,8.17163732140559));
#242549=CARTESIAN_POINT('Ctrl Pts',(-6.82275423879728,15.2,8.17499361493095));
#242550=CARTESIAN_POINT('Ctrl Pts',(-6.82439885848668,15.2,8.17837823533896));
#242551=CARTESIAN_POINT('Ctrl Pts',(-6.82604783629269,15.2,8.18179102635353));
#242552=CARTESIAN_POINT('Ctrl Pts',(-6.82769681427845,15.2,8.18520381774011));
#242553=CARTESIAN_POINT('Ctrl Pts',(-6.82935015166137,15.2,8.18864477664291));
#242554=CARTESIAN_POINT('Ctrl Pts',(-6.83100753554992,15.2,8.1921137505295));
#242555=CARTESIAN_POINT('Ctrl Pts',(-6.83299639632458,15.2,8.19627651942028));
#242556=CARTESIAN_POINT('Ctrl Pts',(-6.83499108617596,15.2,8.2004796268649));
#242557=CARTESIAN_POINT('Ctrl Pts',(-6.83699107896854,15.2,8.20472280514382));
#242558=CARTESIAN_POINT('Ctrl Pts',(-6.83899107157944,15.2,8.20896598303733));
#242559=CARTESIAN_POINT('Ctrl Pts',(-6.8409963668314,15.2,8.21324923069861));
#242560=CARTESIAN_POINT('Ctrl Pts',(-6.84300644850838,15.2,8.21757228429157));
#242561=CARTESIAN_POINT('Ctrl Pts',(-6.84501653018537,15.2,8.22189533788455));
#242562=CARTESIAN_POINT('Ctrl Pts',(-6.84703140014528,15.2,8.22625819658269));
#242563=CARTESIAN_POINT('Ctrl Pts',(-6.84905054982163,15.2,8.23066059625339));
#242564=CARTESIAN_POINT('Ctrl Pts',(-6.85073317461305,15.2,8.23432926277894));
#242565=CARTESIAN_POINT('Ctrl Pts',(-6.85241877168104,15.2,8.23802538877811));
#242566=CARTESIAN_POINT('Ctrl Pts',(-6.85410705482074,15.2,8.24174882451777));
#242567=CARTESIAN_POINT('Ctrl Pts',(-6.85579533796045,15.2,8.24547226025744));
#242568=CARTESIAN_POINT('Ctrl Pts',(-6.85748630704498,15.2,8.24922300395439));
#242569=CARTESIAN_POINT('Ctrl Pts',(-6.85917967690599,15.2,8.25300090624468));
#242570=CARTESIAN_POINT('Ctrl Pts',(-6.860873046767,15.2,8.25677880853496));
#242571=CARTESIAN_POINT('Ctrl Pts',(-6.86256881806138,15.2,8.26058386849535));
#242572=CARTESIAN_POINT('Ctrl Pts',(-6.86426671438068,15.2,8.26441593925778));
#242573=CARTESIAN_POINT('Ctrl Pts',(-6.86562503151016,15.2,8.26748159603481));
#242574=CARTESIAN_POINT('Ctrl Pts',(-6.8669847064636,15.2,8.27056453918565));
#242575=CARTESIAN_POINT('Ctrl Pts',(-6.8683456004392,15.2,8.2736646927332));
#242576=CARTESIAN_POINT('Ctrl Pts',(-6.86970649422937,15.2,8.27676484585836));
#242577=CARTESIAN_POINT('Ctrl Pts',(-6.87106860596401,15.2,8.27988220889283));
#242578=CARTESIAN_POINT('Ctrl Pts',(-6.87243179713029,15.2,8.28301670780217));
#242579=CARTESIAN_POINT('Ctrl Pts',(-6.8737949884823,15.2,8.28615120713857));
#242580=CARTESIAN_POINT('Ctrl Pts',(-6.87515925874831,15.2,8.28930284102418));
#242581=CARTESIAN_POINT('Ctrl Pts',(-6.87652447137834,15.2,8.29247153630913));
#242582=CARTESIAN_POINT('Ctrl Pts',(-6.87788968382236,15.2,8.29564023116235));
#242583=CARTESIAN_POINT('Ctrl Pts',(-6.87925583847857,15.2,8.2988259847469));
#242584=CARTESIAN_POINT('Ctrl Pts',(-6.8806227991017,15.2,8.30202872581028));
#242585=CARTESIAN_POINT('Ctrl Pts',(-6.88233150002033,15.2,8.30603215246679));
#242586=CARTESIAN_POINT('Ctrl Pts',(-6.88404146093822,15.2,8.31006211796952));
#242587=CARTESIAN_POINT('Ctrl Pts',(-6.88575242010483,15.2,8.31411848025978));
#242588=CARTESIAN_POINT('Ctrl Pts',(-6.88712118751271,15.2,8.31736357026885));
#242589=CARTESIAN_POINT('Ctrl Pts',(-6.88849059481791,15.2,8.32062555323554));
#242590=CARTESIAN_POINT('Ctrl Pts',(-6.88986050883705,15.2,8.32390435602645));
#242591=CARTESIAN_POINT('Ctrl Pts',(-6.89123042266954,15.2,8.32718315837062));
#242592=CARTESIAN_POINT('Ctrl Pts',(-6.89260084294753,15.2,8.33047878002334));
#242593=CARTESIAN_POINT('Ctrl Pts',(-6.89397164029281,15.2,8.33379114852769));
#242594=CARTESIAN_POINT('Ctrl Pts',(-6.89534243782485,15.2,8.33710351748335));
#242595=CARTESIAN_POINT('Ctrl Pts',(-6.8967136125152,15.2,8.34043263316519));
#242596=CARTESIAN_POINT('Ctrl Pts',(-6.89808503514551,15.2,8.34377842251527));
#242597=CARTESIAN_POINT('Ctrl Pts',(-6.89945645758896,15.2,8.34712421140948));
#242598=CARTESIAN_POINT('Ctrl Pts',(-6.9008281270907,15.2,8.35048667348928));
#242599=CARTESIAN_POINT('Ctrl Pts',(-6.9021999170341,15.2,8.35386573648912));
#242600=CARTESIAN_POINT('Ctrl Pts',(-6.9035717071644,15.2,8.35724479994934));
#242601=CARTESIAN_POINT('Ctrl Pts',(-6.90494361847277,15.2,8.36064046447572));
#242602=CARTESIAN_POINT('Ctrl Pts',(-6.90631552394266,15.2,8.36405265851058));
#242603=CARTESIAN_POINT('Ctrl Pts',(-6.90768742922563,15.2,8.36746485208053));
#242604=CARTESIAN_POINT('Ctrl Pts',(-6.90905932959068,15.2,8.37089357359774));
#242605=CARTESIAN_POINT('Ctrl Pts',(-6.91043109953411,15.2,8.37433875320331));
#242606=CARTESIAN_POINT('Ctrl Pts',(-6.91180286966444,15.2,8.37778393327828));
#242607=CARTESIAN_POINT('Ctrl Pts',(-6.91317450979477,15.2,8.38124556989093));
#242608=CARTESIAN_POINT('Ctrl Pts',(-6.91454589725839,15.2,8.38472359202492));
#242609=CARTESIAN_POINT('Ctrl Pts',(-6.91591728472202,15.2,8.3882016141589));
#242610=CARTESIAN_POINT('Ctrl Pts',(-6.91728841924951,15.2,8.39169602304481));
#242611=CARTESIAN_POINT('Ctrl Pts',(-6.91865917999085,15.2,8.39520674584895));
#242612=CARTESIAN_POINT('Ctrl Pts',(-6.92037263063738,15.2,8.39959514863663));
#242613=CARTESIAN_POINT('Ctrl Pts',(-6.92208549620712,15.2,8.40400904242189));
#242614=CARTESIAN_POINT('Ctrl Pts',(-6.92379754053445,15.2,8.40844828943594));
#242615=CARTESIAN_POINT('Ctrl Pts',(-6.92516717622026,15.2,8.41199968762783));
#242616=CARTESIAN_POINT('Ctrl Pts',(-6.92653628928382,15.2,8.41556731176574));
#242617=CARTESIAN_POINT('Ctrl Pts',(-6.92790475819172,15.2,8.41915109251658));
#242618=CARTESIAN_POINT('Ctrl Pts',(-6.92995746136712,15.2,8.42452676315456));
#242619=CARTESIAN_POINT('Ctrl Pts',(-6.93200871780712,15.2,8.42993878222585));
#242620=CARTESIAN_POINT('Ctrl Pts',(-6.93405813383513,15.2,8.43538691621463));
#242621=CARTESIAN_POINT('Ctrl Pts',(-6.93610755004931,15.2,8.44083505069828));
#242622=CARTESIAN_POINT('Ctrl Pts',(-6.93815512310335,15.2,8.44631929942333));
#242623=CARTESIAN_POINT('Ctrl Pts',(-6.94020046846467,15.2,8.45183942580996));
#242624=CARTESIAN_POINT('Ctrl Pts',(-6.94156403185309,15.2,8.45551950956629));
#242625=CARTESIAN_POINT('Ctrl Pts',(-6.94292660395554,15.2,8.45921553994557));
#242626=CARTESIAN_POINT('Ctrl Pts',(-6.94428807262208,15.2,8.46292744819662));
#242627=CARTESIAN_POINT('Ctrl Pts',(-6.94564954147413,15.2,8.46663935695343));
#242628=CARTESIAN_POINT('Ctrl Pts',(-6.94700990665818,15.2,8.47036714209802));
#242629=CARTESIAN_POINT('Ctrl Pts',(-6.94836905618895,15.2,8.47411073576823));
#242630=CARTESIAN_POINT('Ctrl Pts',(-6.9500679930098,15.2,8.47879022760096));
#242631=CARTESIAN_POINT('Ctrl Pts',(-6.9517650284997,15.2,8.48349441949977));
#242632=CARTESIAN_POINT('Ctrl Pts',(-6.95345994801342,15.2,8.48822317783513));
#242633=CARTESIAN_POINT('Ctrl Pts',(-6.95481588351355,15.2,8.49200618419414));
#242634=CARTESIAN_POINT('Ctrl Pts',(-6.95617046593052,15.2,8.49580491245943));
#242635=CARTESIAN_POINT('Ctrl Pts',(-6.9575235834311,15.2,8.4996192959799));
#242636=CARTESIAN_POINT('Ctrl Pts',(-6.95887670111603,15.2,8.50343368002008));
#242637=CARTESIAN_POINT('Ctrl Pts',(-6.96022835561194,15.2,8.50726371646497));
#242638=CARTESIAN_POINT('Ctrl Pts',(-6.96157843785209,15.2,8.51110934056446));
#242639=CARTESIAN_POINT('Ctrl Pts',(-6.96292851990828,15.2,8.51495496413997));
#242640=CARTESIAN_POINT('Ctrl Pts',(-6.96427703096119,15.2,8.51881617387873));
#242641=CARTESIAN_POINT('Ctrl Pts',(-6.96562386252962,15.2,8.5226929024208));
#242642=CARTESIAN_POINT('Ctrl Pts',(-6.96697069428156,15.2,8.52656963149107));
#242643=CARTESIAN_POINT('Ctrl Pts',(-6.96831584733122,15.2,8.53046187900832));
#242644=CARTESIAN_POINT('Ctrl Pts',(-6.96965921562653,15.2,8.53436957661119));
#242645=CARTESIAN_POINT('Ctrl Pts',(-6.9710025837388,15.2,8.53827727368162));
#242646=CARTESIAN_POINT('Ctrl Pts',(-6.9723441675459,15.2,8.54220042215731));
#242647=CARTESIAN_POINT('Ctrl Pts',(-6.97368386054769,15.2,8.54613895438931));
#242648=CARTESIAN_POINT('Ctrl Pts',(-6.975023553732,15.2,8.55007748715793));
#242649=CARTESIAN_POINT('Ctrl Pts',(-6.97636135866378,15.2,8.55403140365157));
#242650=CARTESIAN_POINT('Ctrl Pts',(-6.97769717024264,15.2,8.5580006372193));
#242651=CARTESIAN_POINT('Ctrl Pts',(-6.97903298163949,15.2,8.56196987024621));
#242652=CARTESIAN_POINT('Ctrl Pts',(-6.98036679895209,15.2,8.56595442136061));
#242653=CARTESIAN_POINT('Ctrl Pts',(-6.98169852173233,15.2,8.56995422108763));
#242654=CARTESIAN_POINT('Ctrl Pts',(-6.98303024469401,15.2,8.57395402135962));
#242655=CARTESIAN_POINT('Ctrl Pts',(-6.98435987175828,15.2,8.57796907155528));
#242656=CARTESIAN_POINT('Ctrl Pts',(-6.98568730144173,15.2,8.58199930627493));
#242657=CARTESIAN_POINT('Ctrl Pts',(-6.98701473112519,15.2,8.58602954099457));
#242658=CARTESIAN_POINT('Ctrl Pts',(-6.98833996387227,15.2,8.59007495818822));
#242659=CARTESIAN_POINT('Ctrl Pts',(-6.9896628994997,15.2,8.59413549368883));
#242660=CARTESIAN_POINT('Ctrl Pts',(-6.99098583494687,15.2,8.5981960286362));
#242661=CARTESIAN_POINT('Ctrl Pts',(-6.99230647146206,15.2,8.6022716807575));
#242662=CARTESIAN_POINT('Ctrl Pts',(-6.99362471224917,15.2,8.60636238499714));
#242663=CARTESIAN_POINT('Ctrl Pts',(-6.99494295321589,15.2,8.61045308979415));
#242664=CARTESIAN_POINT('Ctrl Pts',(-6.9962587959907,15.2,8.61455884454201));
#242665=CARTESIAN_POINT('Ctrl Pts',(-6.99757214500647,15.2,8.61867958665702));
#242666=CARTESIAN_POINT('Ctrl Pts',(-6.99888549384329,15.2,8.62280032821057));
#242667=CARTESIAN_POINT('Ctrl Pts',(-7.00019634616376,15.2,8.62693605420104));
#242668=CARTESIAN_POINT('Ctrl Pts',(-7.00150460633476,15.2,8.63108670119409));
#242669=CARTESIAN_POINT('Ctrl Pts',(-7.002812866684,15.2,8.63523734875266));
#242670=CARTESIAN_POINT('Ctrl Pts',(-7.00411853537548,15.2,8.63940291613535));
#242671=CARTESIAN_POINT('Ctrl Pts',(-7.00542151395579,15.2,8.64358333857328));
#242672=CARTESIAN_POINT('Ctrl Pts',(-7.00672449235856,15.2,8.64776376044163));
#242673=CARTESIAN_POINT('Ctrl Pts',(-7.0080247823332,15.2,8.65195903723162));
#242674=CARTESIAN_POINT('Ctrl Pts',(-7.00932228789397,15.2,8.65616910416422));
#242675=CARTESIAN_POINT('Ctrl Pts',(-7.01126854650029,15.2,8.66248420542356));
#242676=CARTESIAN_POINT('Ctrl Pts',(-7.01320853957256,15.2,8.66883258261215));
#242677=CARTESIAN_POINT('Ctrl Pts',(-7.01514195017748,15.2,8.67521401896219));
#242678=CARTESIAN_POINT('Ctrl Pts',(-7.01643089040514,15.2,8.67946830928259));
#242679=CARTESIAN_POINT('Ctrl Pts',(-7.0177169042149,15.2,8.68373729154168));
#242680=CARTESIAN_POINT('Ctrl Pts',(-7.01899990044919,15.2,8.68802090248868));
#242681=CARTESIAN_POINT('Ctrl Pts',(-7.01996214766861,15.2,8.69123361084483));
#242682=CARTESIAN_POINT('Ctrl Pts',(-7.02092269718022,15.2,8.69445454756615));
#242683=CARTESIAN_POINT('Ctrl Pts',(-7.02188150939553,15.2,8.69768368540642));
#242684=CARTESIAN_POINT('Ctrl Pts',(-7.02284032161084,15.2,8.70091282324669));
#242685=CARTESIAN_POINT('Ctrl Pts',(-7.02379739662628,15.2,8.7041501614781));
#242686=CARTESIAN_POINT('Ctrl Pts',(-7.02475269680015,15.2,8.70739567477574));
#242687=CARTESIAN_POINT('Ctrl Pts',(-7.02570799714756,15.2,8.71064118866297));
#242688=CARTESIAN_POINT('Ctrl Pts',(-7.02666152103614,15.2,8.71389487600254));
#242689=CARTESIAN_POINT('Ctrl Pts',(-7.02761323196587,15.2,8.71715671047769));
#242690=CARTESIAN_POINT('Ctrl Pts',(-7.02919941644535,15.2,8.72259309988696));
#242691=CARTESIAN_POINT('Ctrl Pts',(-7.03078056335973,15.2,8.72805212055449));
#242692=CARTESIAN_POINT('Ctrl Pts',(-7.0323564960356,15.2,8.73353364731628));
#242693=CARTESIAN_POINT('Ctrl Pts',(-7.03330205588161,15.2,8.73682256420984));
#242694=CARTESIAN_POINT('Ctrl Pts',(-7.03424573836877,15.2,8.74011958205567));
#242695=CARTESIAN_POINT('Ctrl Pts',(-7.03518750675538,15.2,8.74342467649546));
#242696=CARTESIAN_POINT('Ctrl Pts',(-7.03612927497089,15.2,8.74672977033481));
#242697=CARTESIAN_POINT('Ctrl Pts',(-7.03706912836985,15.2,8.75004293911539));
#242698=CARTESIAN_POINT('Ctrl Pts',(-7.03800703062727,15.2,8.75336415607875));
#242699=CARTESIAN_POINT('Ctrl Pts',(-7.0392575669137,15.2,8.7577924451621));
#242700=CARTESIAN_POINT('Ctrl Pts',(-7.04050463291439,15.2,8.76223504366289));
#242701=CARTESIAN_POINT('Ctrl Pts',(-7.04174814131961,15.2,8.7666918868533));
#242702=CARTESIAN_POINT('Ctrl Pts',(-7.04268077266588,15.2,8.77003451939792));
#242703=CARTESIAN_POINT('Ctrl Pts',(-7.04361140326443,15.2,8.77338516465752));
#242704=CARTESIAN_POINT('Ctrl Pts',(-7.0445399960643,15.2,8.77674379649274));
#242705=CARTESIAN_POINT('Ctrl Pts',(-7.04577811990992,15.2,8.78122197267979));
#242706=CARTESIAN_POINT('Ctrl Pts',(-7.04701262147466,15.2,8.78571434555435));
#242707=CARTESIAN_POINT('Ctrl Pts',(-7.04824341404174,15.2,8.7902208544666));
#242708=CARTESIAN_POINT('Ctrl Pts',(-7.0491665083832,15.2,8.79360073584377));
#242709=CARTESIAN_POINT('Ctrl Pts',(-7.05008751726641,15.2,8.796988568254));
#242710=CARTESIAN_POINT('Ctrl Pts',(-7.05100640314988,15.2,8.80038432458826));
#242711=CARTESIAN_POINT('Ctrl Pts',(-7.05192528903334,15.2,8.80378008092251));
#242712=CARTESIAN_POINT('Ctrl Pts',(-7.05284205296039,15.2,8.80718376067771));
#242713=CARTESIAN_POINT('Ctrl Pts',(-7.05375665930643,15.2,8.81059533959828));
#242714=CARTESIAN_POINT('Ctrl Pts',(-7.05528100327188,15.2,8.81628130467248));
#242715=CARTESIAN_POINT('Ctrl Pts',(-7.05679935279526,15.2,8.8219892064598));
#242716=CARTESIAN_POINT('Ctrl Pts',(-7.05831154418447,15.2,8.82771892562533));
#242717=CARTESIAN_POINT('Ctrl Pts',(-7.05921885898503,15.2,8.83115675699974));
#242718=CARTESIAN_POINT('Ctrl Pts',(-7.06012395650242,15.2,8.83460244210696));
#242719=CARTESIAN_POINT('Ctrl Pts',(-7.06102680276158,15.2,8.8380559549804));
#242720=CARTESIAN_POINT('Ctrl Pts',(-7.06192964918476,15.2,8.84150946848124));
#242721=CARTESIAN_POINT('Ctrl Pts',(-7.06283024308232,15.2,8.84497080950095));
#242722=CARTESIAN_POINT('Ctrl Pts',(-7.06372855096257,15.2,8.8484399520062));
#242723=CARTESIAN_POINT('Ctrl Pts',(-7.06462685867962,15.2,8.85190909388123));
#242724=CARTESIAN_POINT('Ctrl Pts',(-7.06552287901346,15.2,8.85538603698917));
#242725=CARTESIAN_POINT('Ctrl Pts',(-7.06641657789745,15.2,8.85887075536323));
#242726=CARTESIAN_POINT('Ctrl Pts',(-7.06760817635531,15.2,8.86351704631761));
#242727=CARTESIAN_POINT('Ctrl Pts',(-7.06879564930727,15.2,8.86817715920215));
#242728=CARTESIAN_POINT('Ctrl Pts',(-7.06997891310335,15.2,8.87285103433012));
#242729=CARTESIAN_POINT('Ctrl Pts',(-7.07086636099071,15.2,8.87635644083529));
#242730=CARTESIAN_POINT('Ctrl Pts',(-7.07175144172273,15.2,8.8798695873447));
#242731=CARTESIAN_POINT('Ctrl Pts',(-7.07263412156598,15.2,8.88339044775738));
#242732=CARTESIAN_POINT('Ctrl Pts',(-7.07381102813055,15.2,8.88808492873404));
#242733=CARTESIAN_POINT('Ctrl Pts',(-7.07498366564195,15.2,8.89279312302312));
#242734=CARTESIAN_POINT('Ctrl Pts',(-7.07615195548341,15.2,8.89751497122494));
#242735=CARTESIAN_POINT('Ctrl Pts',(-7.07702817278492,15.2,8.90105635705463));
#242736=CARTESIAN_POINT('Ctrl Pts',(-7.07790194381983,15.2,8.90460542295895));
#242737=CARTESIAN_POINT('Ctrl Pts',(-7.07877323566339,15.2,8.90816214191238));
#242738=CARTESIAN_POINT('Ctrl Pts',(-7.07964452750695,15.2,8.9117188608658));
#242739=CARTESIAN_POINT('Ctrl Pts',(-7.080513340187,15.2,8.9152832339111));
#242740=CARTESIAN_POINT('Ctrl Pts',(-7.08137964007411,15.2,8.91885523500058));
#242741=CARTESIAN_POINT('Ctrl Pts',(-7.08224593996121,15.2,8.92242723609006));
#242742=CARTESIAN_POINT('Ctrl Pts',(-7.08310972644326,15.2,8.92600686484928));
#242743=CARTESIAN_POINT('Ctrl Pts',(-7.08397096778732,15.2,8.92959409521793));
#242744=CARTESIAN_POINT('Ctrl Pts',(-7.0851192896837,15.2,8.93437706947724));
#242745=CARTESIAN_POINT('Ctrl Pts',(-7.08626308638521,15.2,8.93917355733779));
#242746=CARTESIAN_POINT('Ctrl Pts',(-7.08740227972508,15.2,8.9439835002666));
#242747=CARTESIAN_POINT('Ctrl Pts',(-7.08825667465236,15.2,8.94759095713553));
#242748=CARTESIAN_POINT('Ctrl Pts',(-7.08910848122144,15.2,8.95120598212082));
#242749=CARTESIAN_POINT('Ctrl Pts',(-7.08995766614914,15.2,8.95482854861353));
#242750=CARTESIAN_POINT('Ctrl Pts',(-7.09080685107684,15.2,8.95845111510624));
#242751=CARTESIAN_POINT('Ctrl Pts',(-7.09165341559164,15.2,8.96208122516421));
#242752=CARTESIAN_POINT('Ctrl Pts',(-7.09249732456177,15.2,8.96571884979622));
#242753=CARTESIAN_POINT('Ctrl Pts',(-7.09334123353191,15.2,8.96935647442823));
#242754=CARTESIAN_POINT('Ctrl Pts',(-7.09418248806403,15.2,8.97300161397071));
#242755=CARTESIAN_POINT('Ctrl Pts',(-7.0950210550756,15.2,8.97665424392033));
#242756=CARTESIAN_POINT('Ctrl Pts',(-7.0958596222395,15.2,8.98030687453351));
#242757=CARTESIAN_POINT('Ctrl Pts',(-7.09669550409432,15.2,8.98396699618209));
#242758=CARTESIAN_POINT('Ctrl Pts',(-7.09752867067337,15.2,8.98763458429948));
#242759=CARTESIAN_POINT('Ctrl Pts',(-7.09863955919318,15.2,8.99252470067887));
#242760=CARTESIAN_POINT('Ctrl Pts',(-7.09974562193026,15.2,8.99742809292313));
#242761=CARTESIAN_POINT('Ctrl Pts',(-7.10084677945168,15.2,9.00234469629812));
#242762=CARTESIAN_POINT('Ctrl Pts',(-7.10222322646597,15.2,9.00849045101926));
#242763=CARTESIAN_POINT('Ctrl Pts',(-7.10359199720425,15.2,9.01465683859633));
#242764=CARTESIAN_POINT('Ctrl Pts',(-7.10495293922433,15.2,9.02084373647156));
#242765=CARTESIAN_POINT('Ctrl Pts',(-7.10631388124442,15.2,9.02703063434678));
#242766=CARTESIAN_POINT('Ctrl Pts',(-7.10766700189186,15.2,9.03323804195593));
#242767=CARTESIAN_POINT('Ctrl Pts',(-7.10901226900006,15.2,9.03946594399999));
#242768=CARTESIAN_POINT('Origin',(-5.66257110645729E-14,15.2,-1.77635683940025E-14));
#242769=CARTESIAN_POINT('',(-7.01216898600006,15.2,7.64657512399998));
#242770=CARTESIAN_POINT('',(-7.01216898600006,12.2,7.64657512399998));
#242771=CARTESIAN_POINT('',(-7.01216898600006,15.2,7.64657512399998));
#242772=CARTESIAN_POINT('Origin',(-5.66257110645729E-14,12.2,-1.77635683940025E-14));
#242773=CARTESIAN_POINT('Origin',(-5.66257110645729E-14,15.2,-1.77635683940025E-14));
#242774=CARTESIAN_POINT('Origin',(-5.66257110645729E-14,15.2,-1.77635683940025E-14));
#242775=CARTESIAN_POINT('',(-8.05377977200006,15.2,8.20893606999999));
#242776=CARTESIAN_POINT('',(-8.32310290947582,15.2,7.93573928281797));
#242777=CARTESIAN_POINT('Origin',(-5.66257110645729E-14,15.2,-1.77635683940025E-14));
#242778=CARTESIAN_POINT('',(-8.32310290947582,12.2,7.93573928281797));
#242779=CARTESIAN_POINT('',(-8.32310291000006,15.2,7.93573928299999));
#242780=CARTESIAN_POINT('',(-8.05377977200006,12.2,8.20893606999999));
#242781=CARTESIAN_POINT('Origin',(-5.66257110645729E-14,12.2,-1.77635683940025E-14));
#242782=CARTESIAN_POINT('',(-8.05377977200006,15.2,8.20893606999999));
#242783=CARTESIAN_POINT('Ctrl Pts',(-8.32310290900006,15.2,7.93573928299999));
#242784=CARTESIAN_POINT('Ctrl Pts',(-8.32310290900006,11.6,7.93573928299999));
#242785=CARTESIAN_POINT('Ctrl Pts',(-8.32283676100005,15.2,7.93502251699999));
#242786=CARTESIAN_POINT('Ctrl Pts',(-8.32283676100005,11.6,7.93502251699999));
#242787=CARTESIAN_POINT('Ctrl Pts',(-8.32230434900006,15.2,7.93358949599998));
#242788=CARTESIAN_POINT('Ctrl Pts',(-8.32230434900006,11.6,7.93358949599998));
#242789=CARTESIAN_POINT('Ctrl Pts',(-8.32150538200005,15.2,7.93144150699998));
#242790=CARTESIAN_POINT('Ctrl Pts',(-8.32150538200005,11.6,7.93144150699998));
#242791=CARTESIAN_POINT('Ctrl Pts',(-8.32043939300006,15.2,7.92858060399999));
#242792=CARTESIAN_POINT('Ctrl Pts',(-8.32043939300006,11.6,7.92858060399999));
#242793=CARTESIAN_POINT('Ctrl Pts',(-8.31910574600006,15.2,7.92500961199998));
#242794=CARTESIAN_POINT('Ctrl Pts',(-8.31910574600006,11.6,7.92500961199998));
#242795=CARTESIAN_POINT('Ctrl Pts',(-8.31777093800006,15.2,7.92144375699999));
#242796=CARTESIAN_POINT('Ctrl Pts',(-8.31777093800006,11.6,7.92144375699999));
#242797=CARTESIAN_POINT('Ctrl Pts',(-8.31643496900006,15.2,7.91788304099998));
#242798=CARTESIAN_POINT('Ctrl Pts',(-8.31643496900006,11.6,7.91788304099998));
#242799=CARTESIAN_POINT('Ctrl Pts',(-8.31509784400006,15.2,7.91432746599998));
#242800=CARTESIAN_POINT('Ctrl Pts',(-8.31509784400006,11.6,7.91432746599998));
#242801=CARTESIAN_POINT('Ctrl Pts',(-8.31375956800006,15.2,7.91077703599999));
#242802=CARTESIAN_POINT('Ctrl Pts',(-8.31375956800006,11.6,7.91077703599999));
#242803=CARTESIAN_POINT('Ctrl Pts',(-8.31242014800005,15.2,7.90723175399999));
#242804=CARTESIAN_POINT('Ctrl Pts',(-8.31242014800005,11.6,7.90723175399999));
#242805=CARTESIAN_POINT('Ctrl Pts',(-8.31107959100006,15.2,7.90369162599998));
#242806=CARTESIAN_POINT('Ctrl Pts',(-8.31107959100006,11.6,7.90369162599998));
#242807=CARTESIAN_POINT('Ctrl Pts',(-8.30973790700006,15.2,7.90015665599999));
#242808=CARTESIAN_POINT('Ctrl Pts',(-8.30973790700006,11.6,7.90015665599999));
#242809=CARTESIAN_POINT('Ctrl Pts',(-8.30839510700006,15.2,7.89662685099999));
#242810=CARTESIAN_POINT('Ctrl Pts',(-8.30839510700006,11.6,7.89662685099999));
#242811=CARTESIAN_POINT('Ctrl Pts',(-8.30705119900006,15.2,7.89310221799998));
#242812=CARTESIAN_POINT('Ctrl Pts',(-8.30705119900006,11.6,7.89310221799998));
#242813=CARTESIAN_POINT('Ctrl Pts',(-8.30570619200006,15.2,7.88958275899999));
#242814=CARTESIAN_POINT('Ctrl Pts',(-8.30570619200006,11.6,7.88958275899999));
#242815=CARTESIAN_POINT('Ctrl Pts',(-8.30436009500006,15.2,7.88606848099998));
#242816=CARTESIAN_POINT('Ctrl Pts',(-8.30436009500006,11.6,7.88606848099998));
#242817=CARTESIAN_POINT('Ctrl Pts',(-8.30301291400006,15.2,7.88255938899999));
#242818=CARTESIAN_POINT('Ctrl Pts',(-8.30301291400006,11.6,7.88255938899999));
#242819=CARTESIAN_POINT('Ctrl Pts',(-8.30166465900006,15.2,7.87905548499998));
#242820=CARTESIAN_POINT('Ctrl Pts',(-8.30166465900006,11.6,7.87905548499998));
#242821=CARTESIAN_POINT('Ctrl Pts',(-8.30031533400006,15.2,7.87555677499999));
#242822=CARTESIAN_POINT('Ctrl Pts',(-8.30031533400006,11.6,7.87555677499999));
#242823=CARTESIAN_POINT('Ctrl Pts',(-8.29896494600005,15.2,7.87206326199998));
#242824=CARTESIAN_POINT('Ctrl Pts',(-8.29896494600005,11.6,7.87206326199998));
#242825=CARTESIAN_POINT('Ctrl Pts',(-8.29761350500006,15.2,7.86857495199998));
#242826=CARTESIAN_POINT('Ctrl Pts',(-8.29761350500006,11.6,7.86857495199998));
#242827=CARTESIAN_POINT('Ctrl Pts',(-8.29626101600006,15.2,7.86509184699998));
#242828=CARTESIAN_POINT('Ctrl Pts',(-8.29626101600006,11.6,7.86509184699998));
#242829=CARTESIAN_POINT('Ctrl Pts',(-8.29490748900006,15.2,7.86161395399999));
#242830=CARTESIAN_POINT('Ctrl Pts',(-8.29490748900006,11.6,7.86161395399999));
#242831=CARTESIAN_POINT('Ctrl Pts',(-8.29355293100006,15.2,7.85814127699999));
#242832=CARTESIAN_POINT('Ctrl Pts',(-8.29355293100006,11.6,7.85814127699999));
#242833=CARTESIAN_POINT('Ctrl Pts',(-8.29219735000006,15.2,7.85467382099998));
#242834=CARTESIAN_POINT('Ctrl Pts',(-8.29219735000006,11.6,7.85467382099998));
#242835=CARTESIAN_POINT('Ctrl Pts',(-8.29084075600005,15.2,7.85121158999999));
#242836=CARTESIAN_POINT('Ctrl Pts',(-8.29084075600005,11.6,7.85121158999999));
#242837=CARTESIAN_POINT('Ctrl Pts',(-8.28948315500006,15.2,7.84775459099999));
#242838=CARTESIAN_POINT('Ctrl Pts',(-8.28948315500006,11.6,7.84775459099999));
#242839=CARTESIAN_POINT('Ctrl Pts',(-8.28812455600006,15.2,7.84430282599998));
#242840=CARTESIAN_POINT('Ctrl Pts',(-8.28812455600006,11.6,7.84430282599998));
#242841=CARTESIAN_POINT('Ctrl Pts',(-8.28676496700006,15.2,7.84085629999999));
#242842=CARTESIAN_POINT('Ctrl Pts',(-8.28676496700006,11.6,7.84085629999999));
#242843=CARTESIAN_POINT('Ctrl Pts',(-8.28540439600006,15.2,7.83741501799998));
#242844=CARTESIAN_POINT('Ctrl Pts',(-8.28540439600006,11.6,7.83741501799998));
#242845=CARTESIAN_POINT('Ctrl Pts',(-8.28404285000006,15.2,7.83397898599999));
#242846=CARTESIAN_POINT('Ctrl Pts',(-8.28404285000006,11.6,7.83397898599999));
#242847=CARTESIAN_POINT('Ctrl Pts',(-8.28268033800006,15.2,7.83054820599999));
#242848=CARTESIAN_POINT('Ctrl Pts',(-8.28268033800006,11.6,7.83054820599999));
#242849=CARTESIAN_POINT('Ctrl Pts',(-8.28131686600006,15.2,7.82712268499999));
#242850=CARTESIAN_POINT('Ctrl Pts',(-8.28131686600006,11.6,7.82712268499999));
#242851=CARTESIAN_POINT('Ctrl Pts',(-8.27995244500006,15.2,7.82370242499999));
#242852=CARTESIAN_POINT('Ctrl Pts',(-8.27995244500006,11.6,7.82370242499999));
#242853=CARTESIAN_POINT('Ctrl Pts',(-8.27858708000005,15.2,7.82028743299998));
#242854=CARTESIAN_POINT('Ctrl Pts',(-8.27858708000005,11.6,7.82028743299998));
#242855=CARTESIAN_POINT('Ctrl Pts',(-8.27722078100006,15.2,7.81687771299998));
#242856=CARTESIAN_POINT('Ctrl Pts',(-8.27722078100006,11.6,7.81687771299998));
#242857=CARTESIAN_POINT('Ctrl Pts',(-8.27585355600006,15.2,7.81347326899999));
#242858=CARTESIAN_POINT('Ctrl Pts',(-8.27585355600006,11.6,7.81347326899999));
#242859=CARTESIAN_POINT('Ctrl Pts',(-8.27448541300006,15.2,7.81007410599998));
#242860=CARTESIAN_POINT('Ctrl Pts',(-8.27448541300006,11.6,7.81007410599998));
#242861=CARTESIAN_POINT('Ctrl Pts',(-8.27311636000006,15.2,7.80668022899999));
#242862=CARTESIAN_POINT('Ctrl Pts',(-8.27311636000006,11.6,7.80668022899999));
#242863=CARTESIAN_POINT('Ctrl Pts',(-8.27174640600006,15.2,7.80329164399999));
#242864=CARTESIAN_POINT('Ctrl Pts',(-8.27174640600006,11.6,7.80329164399999));
#242865=CARTESIAN_POINT('Ctrl Pts',(-8.27037555700005,15.2,7.79990835199998));
#242866=CARTESIAN_POINT('Ctrl Pts',(-8.27037555700005,11.6,7.79990835199998));
#242867=CARTESIAN_POINT('Ctrl Pts',(-8.26900382400006,15.2,7.79653036099998));
#242868=CARTESIAN_POINT('Ctrl Pts',(-8.26900382400006,11.6,7.79653036099998));
#242869=CARTESIAN_POINT('Ctrl Pts',(-8.26763121300005,15.2,7.79315767299998));
#242870=CARTESIAN_POINT('Ctrl Pts',(-8.26763121300005,11.6,7.79315767299998));
#242871=CARTESIAN_POINT('Ctrl Pts',(-8.26625773300006,15.2,7.78979029499999));
#242872=CARTESIAN_POINT('Ctrl Pts',(-8.26625773300006,11.6,7.78979029499999));
#242873=CARTESIAN_POINT('Ctrl Pts',(-8.26488339300005,15.2,7.78642823099998));
#242874=CARTESIAN_POINT('Ctrl Pts',(-8.26488339300005,11.6,7.78642823099998));
#242875=CARTESIAN_POINT('Ctrl Pts',(-8.26350820000006,15.2,7.78307148499999));
#242876=CARTESIAN_POINT('Ctrl Pts',(-8.26350820000006,11.6,7.78307148499999));
#242877=CARTESIAN_POINT('Ctrl Pts',(-8.26213216200006,15.2,7.77972006199998));
#242878=CARTESIAN_POINT('Ctrl Pts',(-8.26213216200006,11.6,7.77972006199998));
#242879=CARTESIAN_POINT('Ctrl Pts',(-8.26075528800006,15.2,7.77637396599999));
#242880=CARTESIAN_POINT('Ctrl Pts',(-8.26075528800006,11.6,7.77637396599999));
#242881=CARTESIAN_POINT('Ctrl Pts',(-8.25937758800006,15.2,7.77303320299998));
#242882=CARTESIAN_POINT('Ctrl Pts',(-8.25937758800006,11.6,7.77303320299998));
#242883=CARTESIAN_POINT('Ctrl Pts',(-8.25799906800006,15.2,7.76969777699998));
#242884=CARTESIAN_POINT('Ctrl Pts',(-8.25799906800006,11.6,7.76969777699998));
#242885=CARTESIAN_POINT('Ctrl Pts',(-8.25661973700005,15.2,7.76636769199998));
#242886=CARTESIAN_POINT('Ctrl Pts',(-8.25661973700005,11.6,7.76636769199998));
#242887=CARTESIAN_POINT('Ctrl Pts',(-8.25523960300006,15.2,7.76304295399999));
#242888=CARTESIAN_POINT('Ctrl Pts',(-8.25523960300006,11.6,7.76304295399999));
#242889=CARTESIAN_POINT('Ctrl Pts',(-8.25385867600006,15.2,7.75972356699998));
#242890=CARTESIAN_POINT('Ctrl Pts',(-8.25385867600006,11.6,7.75972356699998));
#242891=CARTESIAN_POINT('Ctrl Pts',(-8.25247696300006,15.2,7.75640953499998));
#242892=CARTESIAN_POINT('Ctrl Pts',(-8.25247696300006,11.6,7.75640953499998));
#242893=CARTESIAN_POINT('Ctrl Pts',(-8.25109447200006,15.2,7.75310086299999));
#242894=CARTESIAN_POINT('Ctrl Pts',(-8.25109447200006,11.6,7.75310086299999));
#242895=CARTESIAN_POINT('Ctrl Pts',(-8.24971121300005,15.2,7.74979755699999));
#242896=CARTESIAN_POINT('Ctrl Pts',(-8.24971121300005,11.6,7.74979755699999));
#242897=CARTESIAN_POINT('Ctrl Pts',(-8.24832719300005,15.2,7.74649961999998));
#242898=CARTESIAN_POINT('Ctrl Pts',(-8.24832719300005,11.6,7.74649961999998));
#242899=CARTESIAN_POINT('Ctrl Pts',(-8.24694242100006,15.2,7.74320705699999));
#242900=CARTESIAN_POINT('Ctrl Pts',(-8.24694242100006,11.6,7.74320705699999));
#242901=CARTESIAN_POINT('Ctrl Pts',(-8.24555690700005,15.2,7.73991987299999));
#242902=CARTESIAN_POINT('Ctrl Pts',(-8.24555690700005,11.6,7.73991987299999));
#242903=CARTESIAN_POINT('Ctrl Pts',(-8.24417065700005,15.2,7.73663807299998));
#242904=CARTESIAN_POINT('Ctrl Pts',(-8.24417065700005,11.6,7.73663807299998));
#242905=CARTESIAN_POINT('Ctrl Pts',(-8.24278368100006,15.2,7.73336166199999));
#242906=CARTESIAN_POINT('Ctrl Pts',(-8.24278368100006,11.6,7.73336166199999));
#242907=CARTESIAN_POINT('Ctrl Pts',(-8.24139598700006,15.2,7.73009064299998));
#242908=CARTESIAN_POINT('Ctrl Pts',(-8.24139598700006,11.6,7.73009064299998));
#242909=CARTESIAN_POINT('Ctrl Pts',(-8.24000758500006,15.2,7.72682502199999));
#242910=CARTESIAN_POINT('Ctrl Pts',(-8.24000758500006,11.6,7.72682502199999));
#242911=CARTESIAN_POINT('Ctrl Pts',(-8.23861848100006,15.2,7.72356480299998));
#242912=CARTESIAN_POINT('Ctrl Pts',(-8.23861848100006,11.6,7.72356480299998));
#242913=CARTESIAN_POINT('Ctrl Pts',(-8.23722868600005,15.2,7.72030999099999));
#242914=CARTESIAN_POINT('Ctrl Pts',(-8.23722868600005,11.6,7.72030999099999));
#242915=CARTESIAN_POINT('Ctrl Pts',(-8.23583820700006,15.2,7.71706059099999));
#242916=CARTESIAN_POINT('Ctrl Pts',(-8.23583820700006,11.6,7.71706059099999));
#242917=CARTESIAN_POINT('Ctrl Pts',(-8.23444705400006,15.2,7.71381660699999));
#242918=CARTESIAN_POINT('Ctrl Pts',(-8.23444705400006,11.6,7.71381660699999));
#242919=CARTESIAN_POINT('Ctrl Pts',(-8.23305523500006,15.2,7.71057804499999));
#242920=CARTESIAN_POINT('Ctrl Pts',(-8.23305523500006,11.6,7.71057804499999));
#242921=CARTESIAN_POINT('Ctrl Pts',(-8.23166275900006,15.2,7.70734490799998));
#242922=CARTESIAN_POINT('Ctrl Pts',(-8.23166275900006,11.6,7.70734490799998));
#242923=CARTESIAN_POINT('Ctrl Pts',(-8.23026963300006,15.2,7.70411720099998));
#242924=CARTESIAN_POINT('Ctrl Pts',(-8.23026963300006,11.6,7.70411720099998));
#242925=CARTESIAN_POINT('Ctrl Pts',(-8.22887586900006,15.2,7.70089492999999));
#242926=CARTESIAN_POINT('Ctrl Pts',(-8.22887586900006,11.6,7.70089492999999));
#242927=CARTESIAN_POINT('Ctrl Pts',(-8.22748147400005,15.2,7.69767809899999));
#242928=CARTESIAN_POINT('Ctrl Pts',(-8.22748147400005,11.6,7.69767809899999));
#242929=CARTESIAN_POINT('Ctrl Pts',(-8.22608645600006,15.2,7.69446671199999));
#242930=CARTESIAN_POINT('Ctrl Pts',(-8.22608645600006,11.6,7.69446671199999));
#242931=CARTESIAN_POINT('Ctrl Pts',(-8.22469082500006,15.2,7.69126077399999));
#242932=CARTESIAN_POINT('Ctrl Pts',(-8.22469082500006,11.6,7.69126077399999));
#242933=CARTESIAN_POINT('Ctrl Pts',(-8.22329458800005,15.2,7.68806028999999));
#242934=CARTESIAN_POINT('Ctrl Pts',(-8.22329458800005,11.6,7.68806028999999));
#242935=CARTESIAN_POINT('Ctrl Pts',(-8.22189775700006,15.2,7.68486526499998));
#242936=CARTESIAN_POINT('Ctrl Pts',(-8.22189775700006,11.6,7.68486526499998));
#242937=CARTESIAN_POINT('Ctrl Pts',(-8.22050033900006,15.2,7.68167570299998));
#242938=CARTESIAN_POINT('Ctrl Pts',(-8.22050033900006,11.6,7.68167570299998));
#242939=CARTESIAN_POINT('Ctrl Pts',(-8.21910234200006,15.2,7.67849160899999));
#242940=CARTESIAN_POINT('Ctrl Pts',(-8.21910234200006,11.6,7.67849160899999));
#242941=CARTESIAN_POINT('Ctrl Pts',(-8.21770377700006,15.2,7.67531298799998));
#242942=CARTESIAN_POINT('Ctrl Pts',(-8.21770377700006,11.6,7.67531298799998));
#242943=CARTESIAN_POINT('Ctrl Pts',(-8.21630465100006,15.2,7.67213984399999));
#242944=CARTESIAN_POINT('Ctrl Pts',(-8.21630465100006,11.6,7.67213984399999));
#242945=CARTESIAN_POINT('Ctrl Pts',(-8.21490497400006,15.2,7.66897218199999));
#242946=CARTESIAN_POINT('Ctrl Pts',(-8.21490497400006,11.6,7.66897218199999));
#242947=CARTESIAN_POINT('Ctrl Pts',(-8.21350475500006,15.2,7.66581000699999));
#242948=CARTESIAN_POINT('Ctrl Pts',(-8.21350475500006,11.6,7.66581000699999));
#242949=CARTESIAN_POINT('Ctrl Pts',(-8.21210400200006,15.2,7.66265332299999));
#242950=CARTESIAN_POINT('Ctrl Pts',(-8.21210400200006,11.6,7.66265332299999));
#242951=CARTESIAN_POINT('Ctrl Pts',(-8.21070272500006,15.2,7.65950213599999));
#242952=CARTESIAN_POINT('Ctrl Pts',(-8.21070272500006,11.6,7.65950213599999));
#242953=CARTESIAN_POINT('Ctrl Pts',(-8.20930093300005,15.2,7.65635645099999));
#242954=CARTESIAN_POINT('Ctrl Pts',(-8.20930093300005,11.6,7.65635645099999));
#242955=CARTESIAN_POINT('Ctrl Pts',(-8.20789863500006,15.2,7.65321626999998));
#242956=CARTESIAN_POINT('Ctrl Pts',(-8.20789863500006,11.6,7.65321626999998));
#242957=CARTESIAN_POINT('Ctrl Pts',(-8.20649583900006,15.2,7.65008159999999));
#242958=CARTESIAN_POINT('Ctrl Pts',(-8.20649583900006,11.6,7.65008159999999));
#242959=CARTESIAN_POINT('Ctrl Pts',(-8.20509255500006,15.2,7.64695244499999));
#242960=CARTESIAN_POINT('Ctrl Pts',(-8.20509255500006,11.6,7.64695244499999));
#242961=CARTESIAN_POINT('Ctrl Pts',(-8.20368879300006,15.2,7.64382880899999));
#242962=CARTESIAN_POINT('Ctrl Pts',(-8.20368879300006,11.6,7.64382880899999));
#242963=CARTESIAN_POINT('Ctrl Pts',(-8.20228456100006,15.2,7.64071069899998));
#242964=CARTESIAN_POINT('Ctrl Pts',(-8.20228456100006,11.6,7.64071069899998));
#242965=CARTESIAN_POINT('Ctrl Pts',(-8.20087986700005,15.2,7.63759811799999));
#242966=CARTESIAN_POINT('Ctrl Pts',(-8.20087986700005,11.6,7.63759811799999));
#242967=CARTESIAN_POINT('Ctrl Pts',(-8.19947472300005,15.2,7.63449107099999));
#242968=CARTESIAN_POINT('Ctrl Pts',(-8.19947472300005,11.6,7.63449107099999));
#242969=CARTESIAN_POINT('Ctrl Pts',(-8.19806913600006,15.2,7.63138956199998));
#242970=CARTESIAN_POINT('Ctrl Pts',(-8.19806913600006,11.6,7.63138956199998));
#242971=CARTESIAN_POINT('Ctrl Pts',(-8.19666311600006,15.2,7.62829359599999));
#242972=CARTESIAN_POINT('Ctrl Pts',(-8.19666311600006,11.6,7.62829359599999));
#242973=CARTESIAN_POINT('Ctrl Pts',(-8.19525667200006,15.2,7.62520317899998));
#242974=CARTESIAN_POINT('Ctrl Pts',(-8.19525667200006,11.6,7.62520317899998));
#242975=CARTESIAN_POINT('Ctrl Pts',(-8.19384981300006,15.2,7.62211831499998));
#242976=CARTESIAN_POINT('Ctrl Pts',(-8.19384981300006,11.6,7.62211831499998));
#242977=CARTESIAN_POINT('Ctrl Pts',(-8.19244254900006,15.2,7.61903900799999));
#242978=CARTESIAN_POINT('Ctrl Pts',(-8.19244254900006,11.6,7.61903900799999));
#242979=CARTESIAN_POINT('Ctrl Pts',(-8.19103488900006,15.2,7.61596526399998));
#242980=CARTESIAN_POINT('Ctrl Pts',(-8.19103488900006,11.6,7.61596526399998));
#242981=CARTESIAN_POINT('Ctrl Pts',(-8.18962684300006,15.2,7.61289708599998));
#242982=CARTESIAN_POINT('Ctrl Pts',(-8.18962684300006,11.6,7.61289708599998));
#242983=CARTESIAN_POINT('Ctrl Pts',(-8.18821841900006,15.2,7.60983448099999));
#242984=CARTESIAN_POINT('Ctrl Pts',(-8.18821841900006,11.6,7.60983448099999));
#242985=CARTESIAN_POINT('Ctrl Pts',(-8.18680962700006,15.2,7.60677745299999));
#242986=CARTESIAN_POINT('Ctrl Pts',(-8.18680962700006,11.6,7.60677745299999));
#242987=CARTESIAN_POINT('Ctrl Pts',(-8.18540047700006,15.2,7.60372600499998));
#242988=CARTESIAN_POINT('Ctrl Pts',(-8.18540047700006,11.6,7.60372600499998));
#242989=CARTESIAN_POINT('Ctrl Pts',(-8.18399097600006,15.2,7.60068014299998));
#242990=CARTESIAN_POINT('Ctrl Pts',(-8.18399097600006,11.6,7.60068014299998));
#242991=CARTESIAN_POINT('Ctrl Pts',(-8.18258113700006,15.2,7.59763987299999));
#242992=CARTESIAN_POINT('Ctrl Pts',(-8.18258113700006,11.6,7.59763987299999));
#242993=CARTESIAN_POINT('Ctrl Pts',(-8.18117096700006,15.2,7.59460519799998));
#242994=CARTESIAN_POINT('Ctrl Pts',(-8.18117096700006,11.6,7.59460519799998));
#242995=CARTESIAN_POINT('Ctrl Pts',(-8.17976047700006,15.2,7.59157612299998));
#242996=CARTESIAN_POINT('Ctrl Pts',(-8.17976047700006,11.6,7.59157612299998));
#242997=CARTESIAN_POINT('Ctrl Pts',(-8.17834967600006,15.2,7.58855265399998));
#242998=CARTESIAN_POINT('Ctrl Pts',(-8.17834967600006,11.6,7.58855265399998));
#242999=CARTESIAN_POINT('Ctrl Pts',(-8.17693857200006,15.2,7.58553479399998));
#243000=CARTESIAN_POINT('Ctrl Pts',(-8.17693857200006,11.6,7.58553479399998));
#243001=CARTESIAN_POINT('Ctrl Pts',(-8.17552717500006,15.2,7.58252254799999));
#243002=CARTESIAN_POINT('Ctrl Pts',(-8.17552717500006,11.6,7.58252254799999));
#243003=CARTESIAN_POINT('Ctrl Pts',(-8.17411549700006,15.2,7.57951592199999));
#243004=CARTESIAN_POINT('Ctrl Pts',(-8.17411549700006,11.6,7.57951592199999));
#243005=CARTESIAN_POINT('Ctrl Pts',(-8.17270354500006,15.2,7.57651491999999));
#243006=CARTESIAN_POINT('Ctrl Pts',(-8.17270354500006,11.6,7.57651491999999));
#243007=CARTESIAN_POINT('Ctrl Pts',(-8.17129133000006,15.2,7.57351954699998));
#243008=CARTESIAN_POINT('Ctrl Pts',(-8.17129133000006,11.6,7.57351954699998));
#243009=CARTESIAN_POINT('Ctrl Pts',(-8.16987886100006,15.2,7.57052980599998));
#243010=CARTESIAN_POINT('Ctrl Pts',(-8.16987886100006,11.6,7.57052980599998));
#243011=CARTESIAN_POINT('Ctrl Pts',(-8.16846614700006,15.2,7.56754570599998));
#243012=CARTESIAN_POINT('Ctrl Pts',(-8.16846614700006,11.6,7.56754570599998));
#243013=CARTESIAN_POINT('Ctrl Pts',(-8.16705320000005,15.2,7.56456724699999));
#243014=CARTESIAN_POINT('Ctrl Pts',(-8.16705320000005,11.6,7.56456724699999));
#243015=CARTESIAN_POINT('Ctrl Pts',(-8.16564002800006,15.2,7.56159443599999));
#243016=CARTESIAN_POINT('Ctrl Pts',(-8.16564002800006,11.6,7.56159443599999));
#243017=CARTESIAN_POINT('Ctrl Pts',(-8.16422664000006,15.2,7.55862727799999));
#243018=CARTESIAN_POINT('Ctrl Pts',(-8.16422664000006,11.6,7.55862727799999));
#243019=CARTESIAN_POINT('Ctrl Pts',(-8.16281304700006,15.2,7.55566577799998));
#243020=CARTESIAN_POINT('Ctrl Pts',(-8.16281304700006,11.6,7.55566577799998));
#243021=CARTESIAN_POINT('Ctrl Pts',(-8.16139925900006,15.2,7.55270993999999));
#243022=CARTESIAN_POINT('Ctrl Pts',(-8.16139925900006,11.6,7.55270993999999));
#243023=CARTESIAN_POINT('Ctrl Pts',(-8.15998528500005,15.2,7.54975976799999));
#243024=CARTESIAN_POINT('Ctrl Pts',(-8.15998528500005,11.6,7.54975976799999));
#243025=CARTESIAN_POINT('Ctrl Pts',(-8.15857113400006,15.2,7.54681526899999));
#243026=CARTESIAN_POINT('Ctrl Pts',(-8.15857113400006,11.6,7.54681526899999));
#243027=CARTESIAN_POINT('Ctrl Pts',(-8.15715681900006,15.2,7.54387644599999));
#243028=CARTESIAN_POINT('Ctrl Pts',(-8.15715681900006,11.6,7.54387644599999));
#243029=CARTESIAN_POINT('Ctrl Pts',(-8.15574234600006,15.2,7.54094330399998));
#243030=CARTESIAN_POINT('Ctrl Pts',(-8.15574234600006,11.6,7.54094330399998));
#243031=CARTESIAN_POINT('Ctrl Pts',(-8.15432772800006,15.2,7.53801584699998));
#243032=CARTESIAN_POINT('Ctrl Pts',(-8.15432772800006,11.6,7.53801584699998));
#243033=CARTESIAN_POINT('Ctrl Pts',(-8.15291297300006,15.2,7.53509408299998));
#243034=CARTESIAN_POINT('Ctrl Pts',(-8.15291297300006,11.6,7.53509408299998));
#243035=CARTESIAN_POINT('Ctrl Pts',(-8.15149809100006,15.2,7.53217801399998));
#243036=CARTESIAN_POINT('Ctrl Pts',(-8.15149809100006,11.6,7.53217801399998));
#243037=CARTESIAN_POINT('Ctrl Pts',(-8.15008309400006,15.2,7.52926764499998));
#243038=CARTESIAN_POINT('Ctrl Pts',(-8.15008309400006,11.6,7.52926764499998));
#243039=CARTESIAN_POINT('Ctrl Pts',(-8.14866799000006,15.2,7.52636298099999));
#243040=CARTESIAN_POINT('Ctrl Pts',(-8.14866799000006,11.6,7.52636298099999));
#243041=CARTESIAN_POINT('Ctrl Pts',(-8.14725278900006,15.2,7.52346402699998));
#243042=CARTESIAN_POINT('Ctrl Pts',(-8.14725278900006,11.6,7.52346402699998));
#243043=CARTESIAN_POINT('Ctrl Pts',(-8.14583750200006,15.2,7.52057078799999));
#243044=CARTESIAN_POINT('Ctrl Pts',(-8.14583750200006,11.6,7.52057078799999));
#243045=CARTESIAN_POINT('Ctrl Pts',(-8.14442213800006,15.2,7.51768326799999));
#243046=CARTESIAN_POINT('Ctrl Pts',(-8.14442213800006,11.6,7.51768326799999));
#243047=CARTESIAN_POINT('Ctrl Pts',(-8.14300670900005,15.2,7.51480147299999));
#243048=CARTESIAN_POINT('Ctrl Pts',(-8.14300670900005,11.6,7.51480147299999));
#243049=CARTESIAN_POINT('Ctrl Pts',(-8.14159122400006,15.2,7.51192540699999));
#243050=CARTESIAN_POINT('Ctrl Pts',(-8.14159122400006,11.6,7.51192540699999));
#243051=CARTESIAN_POINT('Ctrl Pts',(-8.14017569100006,15.2,7.50905507499999));
#243052=CARTESIAN_POINT('Ctrl Pts',(-8.14017569100006,11.6,7.50905507499999));
#243053=CARTESIAN_POINT('Ctrl Pts',(-8.13876012400006,15.2,7.50619048199999));
#243054=CARTESIAN_POINT('Ctrl Pts',(-8.13876012400006,11.6,7.50619048199999));
#243055=CARTESIAN_POINT('Ctrl Pts',(-8.13734453100006,15.2,7.50333163199999));
#243056=CARTESIAN_POINT('Ctrl Pts',(-8.13734453100006,11.6,7.50333163199999));
#243057=CARTESIAN_POINT('Ctrl Pts',(-8.13592892200005,15.2,7.50047853099999));
#243058=CARTESIAN_POINT('Ctrl Pts',(-8.13592892200005,11.6,7.50047853099999));
#243059=CARTESIAN_POINT('Ctrl Pts',(-8.13451330900006,15.2,7.49763118299998));
#243060=CARTESIAN_POINT('Ctrl Pts',(-8.13451330900006,11.6,7.49763118299998));
#243061=CARTESIAN_POINT('Ctrl Pts',(-8.13309770000006,15.2,7.49478959299999));
#243062=CARTESIAN_POINT('Ctrl Pts',(-8.13309770000006,11.6,7.49478959299999));
#243063=CARTESIAN_POINT('Ctrl Pts',(-8.13168210600006,15.2,7.49195376499999));
#243064=CARTESIAN_POINT('Ctrl Pts',(-8.13168210600006,11.6,7.49195376499999));
#243065=CARTESIAN_POINT('Ctrl Pts',(-8.13026653800006,15.2,7.48912370499998));
#243066=CARTESIAN_POINT('Ctrl Pts',(-8.13026653800006,11.6,7.48912370499998));
#243067=CARTESIAN_POINT('Ctrl Pts',(-8.12885100600005,15.2,7.48629941799998));
#243068=CARTESIAN_POINT('Ctrl Pts',(-8.12885100600005,11.6,7.48629941799998));
#243069=CARTESIAN_POINT('Ctrl Pts',(-8.12743552100006,15.2,7.48348090799999));
#243070=CARTESIAN_POINT('Ctrl Pts',(-8.12743552100006,11.6,7.48348090799999));
#243071=CARTESIAN_POINT('Ctrl Pts',(-8.12602009300005,15.2,7.48066817999998));
#243072=CARTESIAN_POINT('Ctrl Pts',(-8.12602009300005,11.6,7.48066817999998));
#243073=CARTESIAN_POINT('Ctrl Pts',(-8.12460473100005,15.2,7.47786123899999));
#243074=CARTESIAN_POINT('Ctrl Pts',(-8.12460473100005,11.6,7.47786123899999));
#243075=CARTESIAN_POINT('Ctrl Pts',(-8.12318944800005,15.2,7.47506008999999));
#243076=CARTESIAN_POINT('Ctrl Pts',(-8.12318944800005,11.6,7.47506008999999));
#243077=CARTESIAN_POINT('Ctrl Pts',(-8.12177425200005,15.2,7.47226473699998));
#243078=CARTESIAN_POINT('Ctrl Pts',(-8.12177425200005,11.6,7.47226473699998));
#243079=CARTESIAN_POINT('Ctrl Pts',(-8.12035915500006,15.2,7.46947518499999));
#243080=CARTESIAN_POINT('Ctrl Pts',(-8.12035915500006,11.6,7.46947518499999));
#243081=CARTESIAN_POINT('Ctrl Pts',(-8.11894416700006,15.2,7.46669143999998));
#243082=CARTESIAN_POINT('Ctrl Pts',(-8.11894416700006,11.6,7.46669143999998));
#243083=CARTESIAN_POINT('Ctrl Pts',(-8.11752930000005,15.2,7.46391350499999));
#243084=CARTESIAN_POINT('Ctrl Pts',(-8.11752930000005,11.6,7.46391350499999));
#243085=CARTESIAN_POINT('Ctrl Pts',(-8.11611456200006,15.2,7.46114138799998));
#243086=CARTESIAN_POINT('Ctrl Pts',(-8.11611456200006,11.6,7.46114138799998));
#243087=CARTESIAN_POINT('Ctrl Pts',(-8.11469996500006,15.2,7.45837508899999));
#243088=CARTESIAN_POINT('Ctrl Pts',(-8.11469996500006,11.6,7.45837508899999));
#243089=CARTESIAN_POINT('Ctrl Pts',(-8.11328552000005,15.2,7.45561461699998));
#243090=CARTESIAN_POINT('Ctrl Pts',(-8.11328552000005,11.6,7.45561461699998));
#243091=CARTESIAN_POINT('Ctrl Pts',(-8.11187123600006,15.2,7.45285997599999));
#243092=CARTESIAN_POINT('Ctrl Pts',(-8.11187123600006,11.6,7.45285997599999));
#243093=CARTESIAN_POINT('Ctrl Pts',(-8.11045712500006,15.2,7.45011116899998));
#243094=CARTESIAN_POINT('Ctrl Pts',(-8.11045712500006,11.6,7.45011116899998));
#243095=CARTESIAN_POINT('Ctrl Pts',(-8.10904319900006,15.2,7.44736820399999));
#243096=CARTESIAN_POINT('Ctrl Pts',(-8.10904319900006,11.6,7.44736820399999));
#243097=CARTESIAN_POINT('Ctrl Pts',(-8.10762946700006,15.2,7.44463108199999));
#243098=CARTESIAN_POINT('Ctrl Pts',(-8.10762946700006,11.6,7.44463108199999));
#243099=CARTESIAN_POINT('Ctrl Pts',(-8.10621593800006,15.2,7.44189980999998));
#243100=CARTESIAN_POINT('Ctrl Pts',(-8.10621593800006,11.6,7.44189980999998));
#243101=CARTESIAN_POINT('Ctrl Pts',(-8.10480262700005,15.2,7.43917439399999));
#243102=CARTESIAN_POINT('Ctrl Pts',(-8.10480262700005,11.6,7.43917439399999));
#243103=CARTESIAN_POINT('Ctrl Pts',(-8.10338954200006,15.2,7.43645483599998));
#243104=CARTESIAN_POINT('Ctrl Pts',(-8.10338954200006,11.6,7.43645483599998));
#243105=CARTESIAN_POINT('Ctrl Pts',(-8.10197669400005,15.2,7.43374114299999));
#243106=CARTESIAN_POINT('Ctrl Pts',(-8.10197669400005,11.6,7.43374114299999));
#243107=CARTESIAN_POINT('Ctrl Pts',(-8.10056409600006,15.2,7.43103331899999));
#243108=CARTESIAN_POINT('Ctrl Pts',(-8.10056409600006,11.6,7.43103331899999));
#243109=CARTESIAN_POINT('Ctrl Pts',(-8.09915175600005,15.2,7.42833136899999));
#243110=CARTESIAN_POINT('Ctrl Pts',(-8.09915175600005,11.6,7.42833136899999));
#243111=CARTESIAN_POINT('Ctrl Pts',(-8.09773968600006,15.2,7.42563529799998));
#243112=CARTESIAN_POINT('Ctrl Pts',(-8.09773968600006,11.6,7.42563529799998));
#243113=CARTESIAN_POINT('Ctrl Pts',(-8.09632789800006,15.2,7.42294511099999));
#243114=CARTESIAN_POINT('Ctrl Pts',(-8.09632789800006,11.6,7.42294511099999));
#243115=CARTESIAN_POINT('Ctrl Pts',(-8.09491640200006,15.2,7.42026081299999));
#243116=CARTESIAN_POINT('Ctrl Pts',(-8.09491640200006,11.6,7.42026081299999));
#243117=CARTESIAN_POINT('Ctrl Pts',(-8.09350520800006,15.2,7.41758240799999));
#243118=CARTESIAN_POINT('Ctrl Pts',(-8.09350520800006,11.6,7.41758240799999));
#243119=CARTESIAN_POINT('Ctrl Pts',(-8.09209433000006,15.2,7.41490990199999));
#243120=CARTESIAN_POINT('Ctrl Pts',(-8.09209433000006,11.6,7.41490990199999));
#243121=CARTESIAN_POINT('Ctrl Pts',(-8.09068377600006,15.2,7.41224329899998));
#243122=CARTESIAN_POINT('Ctrl Pts',(-8.09068377600006,11.6,7.41224329899998));
#243123=CARTESIAN_POINT('Ctrl Pts',(-8.08927355900006,15.2,7.40958260399999));
#243124=CARTESIAN_POINT('Ctrl Pts',(-8.08927355900006,11.6,7.40958260399999));
#243125=CARTESIAN_POINT('Ctrl Pts',(-8.08786369000006,15.2,7.40692782299998));
#243126=CARTESIAN_POINT('Ctrl Pts',(-8.08786369000006,11.6,7.40692782299998));
#243127=CARTESIAN_POINT('Ctrl Pts',(-8.08645417900006,15.2,7.40427895899998));
#243128=CARTESIAN_POINT('Ctrl Pts',(-8.08645417900006,11.6,7.40427895899998));
#243129=CARTESIAN_POINT('Ctrl Pts',(-8.08504503800006,15.2,7.40163601799999));
#243130=CARTESIAN_POINT('Ctrl Pts',(-8.08504503800006,11.6,7.40163601799999));
#243131=CARTESIAN_POINT('Ctrl Pts',(-8.08363627800006,15.2,7.39899900499999));
#243132=CARTESIAN_POINT('Ctrl Pts',(-8.08363627800006,11.6,7.39899900499999));
#243133=CARTESIAN_POINT('Ctrl Pts',(-8.08222791000006,15.2,7.39636792399998));
#243134=CARTESIAN_POINT('Ctrl Pts',(-8.08222791000006,11.6,7.39636792399998));
#243135=CARTESIAN_POINT('Ctrl Pts',(-8.08081994700006,15.2,7.39374278199998));
#243136=CARTESIAN_POINT('Ctrl Pts',(-8.08081994700006,11.6,7.39374278199998));
#243137=CARTESIAN_POINT('Ctrl Pts',(-8.07941239800006,15.2,7.39112358099998));
#243138=CARTESIAN_POINT('Ctrl Pts',(-8.07941239800006,11.6,7.39112358099998));
#243139=CARTESIAN_POINT('Ctrl Pts',(-8.07800527500006,15.2,7.38851032799998));
#243140=CARTESIAN_POINT('Ctrl Pts',(-8.07800527500006,11.6,7.38851032799998));
#243141=CARTESIAN_POINT('Ctrl Pts',(-8.07659859000006,15.2,7.38590302699999));
#243142=CARTESIAN_POINT('Ctrl Pts',(-8.07659859000006,11.6,7.38590302699999));
#243143=CARTESIAN_POINT('Ctrl Pts',(-8.07519235300006,15.2,7.38330168299999));
#243144=CARTESIAN_POINT('Ctrl Pts',(-8.07519235300006,11.6,7.38330168299999));
#243145=CARTESIAN_POINT('Ctrl Pts',(-8.07378657800006,15.2,7.38070630199999));
#243146=CARTESIAN_POINT('Ctrl Pts',(-8.07378657800006,11.6,7.38070630199999));
#243147=CARTESIAN_POINT('Ctrl Pts',(-8.07238127500005,15.2,7.37811688599999));
#243148=CARTESIAN_POINT('Ctrl Pts',(-8.07238127500005,11.6,7.37811688599999));
#243149=CARTESIAN_POINT('Ctrl Pts',(-8.07097645400006,15.2,7.37553344299998));
#243150=CARTESIAN_POINT('Ctrl Pts',(-8.07097645400006,11.6,7.37553344299998));
#243151=CARTESIAN_POINT('Ctrl Pts',(-8.06957212900006,15.2,7.37295597699998));
#243152=CARTESIAN_POINT('Ctrl Pts',(-8.06957212900006,11.6,7.37295597699998));
#243153=CARTESIAN_POINT('Ctrl Pts',(-8.06816830900006,15.2,7.37038449199999));
#243154=CARTESIAN_POINT('Ctrl Pts',(-8.06816830900006,11.6,7.37038449199999));
#243155=CARTESIAN_POINT('Ctrl Pts',(-8.06676500800006,15.2,7.36781899399999));
#243156=CARTESIAN_POINT('Ctrl Pts',(-8.06676500800006,11.6,7.36781899399999));
#243157=CARTESIAN_POINT('Ctrl Pts',(-8.06536223700006,15.2,7.36525948799999));
#243158=CARTESIAN_POINT('Ctrl Pts',(-8.06536223700006,11.6,7.36525948799999));
#243159=CARTESIAN_POINT('Ctrl Pts',(-8.06396000700006,15.2,7.36270597899999));
#243160=CARTESIAN_POINT('Ctrl Pts',(-8.06396000700006,11.6,7.36270597899999));
#243161=CARTESIAN_POINT('Ctrl Pts',(-8.06255832900005,15.2,7.36015846999998));
#243162=CARTESIAN_POINT('Ctrl Pts',(-8.06255832900005,11.6,7.36015846999998));
#243163=CARTESIAN_POINT('Ctrl Pts',(-8.06115721700005,15.2,7.35761696699999));
#243164=CARTESIAN_POINT('Ctrl Pts',(-8.06115721700005,11.6,7.35761696699999));
#243165=CARTESIAN_POINT('Ctrl Pts',(-8.05975668100006,15.2,7.35508147699999));
#243166=CARTESIAN_POINT('Ctrl Pts',(-8.05975668100006,11.6,7.35508147699999));
#243167=CARTESIAN_POINT('Ctrl Pts',(-8.05835673200006,15.2,7.35255200199998));
#243168=CARTESIAN_POINT('Ctrl Pts',(-8.05835673200006,11.6,7.35255200199998));
#243169=CARTESIAN_POINT('Ctrl Pts',(-8.05695738400006,15.2,7.35002854799998));
#243170=CARTESIAN_POINT('Ctrl Pts',(-8.05695738400006,11.6,7.35002854799998));
#243171=CARTESIAN_POINT('Ctrl Pts',(-8.05555864800005,15.2,7.34751112099998));
#243172=CARTESIAN_POINT('Ctrl Pts',(-8.05555864800005,11.6,7.34751112099998));
#243173=CARTESIAN_POINT('Ctrl Pts',(-8.05416053400006,15.2,7.34499972499999));
#243174=CARTESIAN_POINT('Ctrl Pts',(-8.05416053400006,11.6,7.34499972499999));
#243175=CARTESIAN_POINT('Ctrl Pts',(-8.05276305700006,15.2,7.34249436299999));
#243176=CARTESIAN_POINT('Ctrl Pts',(-8.05276305700006,11.6,7.34249436299999));
#243177=CARTESIAN_POINT('Ctrl Pts',(-8.05136622600006,15.2,7.33999504399999));
#243178=CARTESIAN_POINT('Ctrl Pts',(-8.05136622600006,11.6,7.33999504399999));
#243179=CARTESIAN_POINT('Ctrl Pts',(-8.04997005600006,15.2,7.33750177099999));
#243180=CARTESIAN_POINT('Ctrl Pts',(-8.04997005600006,11.6,7.33750177099999));
#243181=CARTESIAN_POINT('Ctrl Pts',(-8.04857455600006,15.2,7.33501454799999));
#243182=CARTESIAN_POINT('Ctrl Pts',(-8.04857455600006,11.6,7.33501454799999));
#243183=CARTESIAN_POINT('Ctrl Pts',(-8.04717974000006,15.2,7.33253338099999));
#243184=CARTESIAN_POINT('Ctrl Pts',(-8.04717974000006,11.6,7.33253338099999));
#243185=CARTESIAN_POINT('Ctrl Pts',(-8.04578561900006,15.2,7.33005827499999));
#243186=CARTESIAN_POINT('Ctrl Pts',(-8.04578561900006,11.6,7.33005827499999));
#243187=CARTESIAN_POINT('Ctrl Pts',(-8.04439220600005,15.2,7.32758923399999));
#243188=CARTESIAN_POINT('Ctrl Pts',(-8.04439220600005,11.6,7.32758923399999));
#243189=CARTESIAN_POINT('Ctrl Pts',(-8.04299951200005,15.2,7.32512626399998));
#243190=CARTESIAN_POINT('Ctrl Pts',(-8.04299951200005,11.6,7.32512626399998));
#243191=CARTESIAN_POINT('Ctrl Pts',(-8.04160755100006,15.2,7.32266936999999));
#243192=CARTESIAN_POINT('Ctrl Pts',(-8.04160755100006,11.6,7.32266936999999));
#243193=CARTESIAN_POINT('Ctrl Pts',(-8.04021633200006,15.2,7.32021855699998));
#243194=CARTESIAN_POINT('Ctrl Pts',(-8.04021633200006,11.6,7.32021855699998));
#243195=CARTESIAN_POINT('Ctrl Pts',(-8.03882587100006,15.2,7.31777382799999));
#243196=CARTESIAN_POINT('Ctrl Pts',(-8.03882587100006,11.6,7.31777382799999));
#243197=CARTESIAN_POINT('Ctrl Pts',(-8.03743617700006,15.2,7.31533519099998));
#243198=CARTESIAN_POINT('Ctrl Pts',(-8.03743617700006,11.6,7.31533519099998));
#243199=CARTESIAN_POINT('Ctrl Pts',(-8.03604726400006,15.2,7.31290264899998));
#243200=CARTESIAN_POINT('Ctrl Pts',(-8.03604726400006,11.6,7.31290264899998));
#243201=CARTESIAN_POINT('Ctrl Pts',(-8.03465914400006,15.2,7.31047620699999));
#243202=CARTESIAN_POINT('Ctrl Pts',(-8.03465914400006,11.6,7.31047620699999));
#243203=CARTESIAN_POINT('Ctrl Pts',(-8.03327182900006,15.2,7.30805587199999));
#243204=CARTESIAN_POINT('Ctrl Pts',(-8.03327182900006,11.6,7.30805587199999));
#243205=CARTESIAN_POINT('Ctrl Pts',(-8.03188533300006,15.2,7.30564164699998));
#243206=CARTESIAN_POINT('Ctrl Pts',(-8.03188533300006,11.6,7.30564164699998));
#243207=CARTESIAN_POINT('Ctrl Pts',(-8.03049966600006,15.2,7.30323353699998));
#243208=CARTESIAN_POINT('Ctrl Pts',(-8.03049966600006,11.6,7.30323353699998));
#243209=CARTESIAN_POINT('Ctrl Pts',(-8.02911484200006,15.2,7.30083154799999));
#243210=CARTESIAN_POINT('Ctrl Pts',(-8.02911484200006,11.6,7.30083154799999));
#243211=CARTESIAN_POINT('Ctrl Pts',(-8.02773087300006,15.2,7.29843568399998));
#243212=CARTESIAN_POINT('Ctrl Pts',(-8.02773087300006,11.6,7.29843568399998));
#243213=CARTESIAN_POINT('Ctrl Pts',(-8.02634777100005,15.2,7.29604595099998));
#243214=CARTESIAN_POINT('Ctrl Pts',(-8.02634777100005,11.6,7.29604595099998));
#243215=CARTESIAN_POINT('Ctrl Pts',(-8.02496555000005,15.2,7.29366235399999));
#243216=CARTESIAN_POINT('Ctrl Pts',(-8.02496555000005,11.6,7.29366235399999));
#243217=CARTESIAN_POINT('Ctrl Pts',(-8.02358422100006,15.2,7.29128489699999));
#243218=CARTESIAN_POINT('Ctrl Pts',(-8.02358422100006,11.6,7.29128489699999));
#243219=CARTESIAN_POINT('Ctrl Pts',(-8.02220379800006,15.2,7.28891358499999));
#243220=CARTESIAN_POINT('Ctrl Pts',(-8.02220379800006,11.6,7.28891358499999));
#243221=CARTESIAN_POINT('Ctrl Pts',(-8.02082429300006,15.2,7.28654842499999));
#243222=CARTESIAN_POINT('Ctrl Pts',(-8.02082429300006,11.6,7.28654842499999));
#243223=CARTESIAN_POINT('Ctrl Pts',(-8.01944571900006,15.2,7.28418941999998));
#243224=CARTESIAN_POINT('Ctrl Pts',(-8.01944571900006,11.6,7.28418941999998));
#243225=CARTESIAN_POINT('Ctrl Pts',(-8.01806808700006,15.2,7.28183657599998));
#243226=CARTESIAN_POINT('Ctrl Pts',(-8.01806808700006,11.6,7.28183657599998));
#243227=CARTESIAN_POINT('Ctrl Pts',(-8.01669141300006,15.2,7.27948989599999));
#243228=CARTESIAN_POINT('Ctrl Pts',(-8.01669141300006,11.6,7.27948989599999));
#243229=CARTESIAN_POINT('Ctrl Pts',(-8.01531570700006,15.2,7.27714938799998));
#243230=CARTESIAN_POINT('Ctrl Pts',(-8.01531570700006,11.6,7.27714938799998));
#243231=CARTESIAN_POINT('Ctrl Pts',(-8.01394098300005,15.2,7.27481505599999));
#243232=CARTESIAN_POINT('Ctrl Pts',(-8.01394098300005,11.6,7.27481505599999));
#243233=CARTESIAN_POINT('Ctrl Pts',(-8.01256725300006,15.2,7.27248690499999));
#243234=CARTESIAN_POINT('Ctrl Pts',(-8.01256725300006,11.6,7.27248690499999));
#243235=CARTESIAN_POINT('Ctrl Pts',(-8.01119453200006,15.2,7.27016493799999));
#243236=CARTESIAN_POINT('Ctrl Pts',(-8.01119453200006,11.6,7.27016493799999));
#243237=CARTESIAN_POINT('Ctrl Pts',(-8.00982283100005,15.2,7.26784916399998));
#243238=CARTESIAN_POINT('Ctrl Pts',(-8.00982283100005,11.6,7.26784916399998));
#243239=CARTESIAN_POINT('Ctrl Pts',(-8.00845216400005,15.2,7.26553958499998));
#243240=CARTESIAN_POINT('Ctrl Pts',(-8.00845216400005,11.6,7.26553958499998));
#243241=CARTESIAN_POINT('Ctrl Pts',(-8.00708254300006,15.2,7.26323620699999));
#243242=CARTESIAN_POINT('Ctrl Pts',(-8.00708254300006,11.6,7.26323620699999));
#243243=CARTESIAN_POINT('Ctrl Pts',(-8.00571398200006,15.2,7.26093903499999));
#243244=CARTESIAN_POINT('Ctrl Pts',(-8.00571398200006,11.6,7.26093903499999));
#243245=CARTESIAN_POINT('Ctrl Pts',(-8.00434649400006,15.2,7.25864807299998));
#243246=CARTESIAN_POINT('Ctrl Pts',(-8.00434649400006,11.6,7.25864807299998));
#243247=CARTESIAN_POINT('Ctrl Pts',(-8.00298009200005,15.2,7.25636332799999));
#243248=CARTESIAN_POINT('Ctrl Pts',(-8.00298009200005,11.6,7.25636332799999));
#243249=CARTESIAN_POINT('Ctrl Pts',(-8.00161478800005,15.2,7.25408480499999));
#243250=CARTESIAN_POINT('Ctrl Pts',(-8.00161478800005,11.6,7.25408480499999));
#243251=CARTESIAN_POINT('Ctrl Pts',(-8.00025059700006,15.2,7.25181250799999));
#243252=CARTESIAN_POINT('Ctrl Pts',(-8.00025059700006,11.6,7.25181250799999));
#243253=CARTESIAN_POINT('Ctrl Pts',(-7.99888753100006,15.2,7.24954644099999));
#243254=CARTESIAN_POINT('Ctrl Pts',(-7.99888753100006,11.6,7.24954644099999));
#243255=CARTESIAN_POINT('Ctrl Pts',(-7.99752560500006,15.2,7.24728661199999));
#243256=CARTESIAN_POINT('Ctrl Pts',(-7.99752560500006,11.6,7.24728661199999));
#243257=CARTESIAN_POINT('Ctrl Pts',(-7.99616483100006,15.2,7.24503302299999));
#243258=CARTESIAN_POINT('Ctrl Pts',(-7.99616483100006,11.6,7.24503302299999));
#243259=CARTESIAN_POINT('Ctrl Pts',(-7.99480522200006,15.2,7.24278568099999));
#243260=CARTESIAN_POINT('Ctrl Pts',(-7.99480522200006,11.6,7.24278568099999));
#243261=CARTESIAN_POINT('Ctrl Pts',(-7.99344679200006,15.2,7.24054459099998));
#243262=CARTESIAN_POINT('Ctrl Pts',(-7.99344679200006,11.6,7.24054459099998));
#243263=CARTESIAN_POINT('Ctrl Pts',(-7.99208955400006,15.2,7.23830975799999));
#243264=CARTESIAN_POINT('Ctrl Pts',(-7.99208955400006,11.6,7.23830975799999));
#243265=CARTESIAN_POINT('Ctrl Pts',(-7.99073352200006,15.2,7.23608118599999));
#243266=CARTESIAN_POINT('Ctrl Pts',(-7.99073352200006,11.6,7.23608118599999));
#243267=CARTESIAN_POINT('Ctrl Pts',(-7.98937871000006,15.2,7.23385888199999));
#243268=CARTESIAN_POINT('Ctrl Pts',(-7.98937871000006,11.6,7.23385888199999));
#243269=CARTESIAN_POINT('Ctrl Pts',(-7.98802513000006,15.2,7.23164284899998));
#243270=CARTESIAN_POINT('Ctrl Pts',(-7.98802513000006,11.6,7.23164284899998));
#243271=CARTESIAN_POINT('Ctrl Pts',(-7.98667279800006,15.2,7.22943309299998));
#243272=CARTESIAN_POINT('Ctrl Pts',(-7.98667279800006,11.6,7.22943309299998));
#243273=CARTESIAN_POINT('Ctrl Pts',(-7.98532172500006,15.2,7.22722962099999));
#243274=CARTESIAN_POINT('Ctrl Pts',(-7.98532172500006,11.6,7.22722962099999));
#243275=CARTESIAN_POINT('Ctrl Pts',(-7.98397192700006,15.2,7.22503243499999));
#243276=CARTESIAN_POINT('Ctrl Pts',(-7.98397192700006,11.6,7.22503243499999));
#243277=CARTESIAN_POINT('Ctrl Pts',(-7.98262341500006,15.2,7.22284154199999));
#243278=CARTESIAN_POINT('Ctrl Pts',(-7.98262341500006,11.6,7.22284154199999));
#243279=CARTESIAN_POINT('Ctrl Pts',(-7.98127620500006,15.2,7.22065694499998));
#243280=CARTESIAN_POINT('Ctrl Pts',(-7.98127620500006,11.6,7.22065694499998));
#243281=CARTESIAN_POINT('Ctrl Pts',(-7.97993031100006,15.2,7.21847865199998));
#243282=CARTESIAN_POINT('Ctrl Pts',(-7.97993031100006,11.6,7.21847865199998));
#243283=CARTESIAN_POINT('Ctrl Pts',(-7.97858574500006,15.2,7.21630666699999));
#243284=CARTESIAN_POINT('Ctrl Pts',(-7.97858574500006,11.6,7.21630666699999));
#243285=CARTESIAN_POINT('Ctrl Pts',(-7.97724252100006,15.2,7.21414099499999));
#243286=CARTESIAN_POINT('Ctrl Pts',(-7.97724252100006,11.6,7.21414099499999));
#243287=CARTESIAN_POINT('Ctrl Pts',(-7.97590065500006,15.2,7.21198164099999));
#243288=CARTESIAN_POINT('Ctrl Pts',(-7.97590065500006,11.6,7.21198164099999));
#243289=CARTESIAN_POINT('Ctrl Pts',(-7.97456015900006,15.2,7.20982860999998));
#243290=CARTESIAN_POINT('Ctrl Pts',(-7.97456015900006,11.6,7.20982860999998));
#243291=CARTESIAN_POINT('Ctrl Pts',(-7.97322104900006,15.2,7.20768190799999));
#243292=CARTESIAN_POINT('Ctrl Pts',(-7.97322104900006,11.6,7.20768190799999));
#243293=CARTESIAN_POINT('Ctrl Pts',(-7.97188333700006,15.2,7.20554153799998));
#243294=CARTESIAN_POINT('Ctrl Pts',(-7.97188333700006,11.6,7.20554153799998));
#243295=CARTESIAN_POINT('Ctrl Pts',(-7.97054703800006,15.2,7.20340750799998));
#243296=CARTESIAN_POINT('Ctrl Pts',(-7.97054703800006,11.6,7.20340750799998));
#243297=CARTESIAN_POINT('Ctrl Pts',(-7.96921216600006,15.2,7.20127982099999));
#243298=CARTESIAN_POINT('Ctrl Pts',(-7.96921216600006,11.6,7.20127982099999));
#243299=CARTESIAN_POINT('Ctrl Pts',(-7.96787873500006,15.2,7.19915848399998));
#243300=CARTESIAN_POINT('Ctrl Pts',(-7.96787873500006,11.6,7.19915848399998));
#243301=CARTESIAN_POINT('Ctrl Pts',(-7.96654675900006,15.2,7.19704350199999));
#243302=CARTESIAN_POINT('Ctrl Pts',(-7.96654675900006,11.6,7.19704350199999));
#243303=CARTESIAN_POINT('Ctrl Pts',(-7.96521625400005,15.2,7.19493487699999));
#243304=CARTESIAN_POINT('Ctrl Pts',(-7.96521625400005,11.6,7.19493487699999));
#243305=CARTESIAN_POINT('Ctrl Pts',(-7.96388723200005,15.2,7.19283261799998));
#243306=CARTESIAN_POINT('Ctrl Pts',(-7.96388723200005,11.6,7.19283261799998));
#243307=CARTESIAN_POINT('Ctrl Pts',(-7.96255970800006,15.2,7.19073672799999));
#243308=CARTESIAN_POINT('Ctrl Pts',(-7.96255970800006,11.6,7.19073672799999));
#243309=CARTESIAN_POINT('Ctrl Pts',(-7.96123369800006,15.2,7.18864721399999));
#243310=CARTESIAN_POINT('Ctrl Pts',(-7.96123369800006,11.6,7.18864721399999));
#243311=CARTESIAN_POINT('Ctrl Pts',(-7.95990921500006,15.2,7.18656407799998));
#243312=CARTESIAN_POINT('Ctrl Pts',(-7.95990921500006,11.6,7.18656407799998));
#243313=CARTESIAN_POINT('Ctrl Pts',(-7.95858627200006,15.2,7.18448732899999));
#243314=CARTESIAN_POINT('Ctrl Pts',(-7.95858627200006,11.6,7.18448732899999));
#243315=CARTESIAN_POINT('Ctrl Pts',(-7.95726488600006,15.2,7.18241696899998));
#243316=CARTESIAN_POINT('Ctrl Pts',(-7.95726488600006,11.6,7.18241696899998));
#243317=CARTESIAN_POINT('Ctrl Pts',(-7.95594507200006,15.2,7.18035300599999));
#243318=CARTESIAN_POINT('Ctrl Pts',(-7.95594507200006,11.6,7.18035300599999));
#243319=CARTESIAN_POINT('Ctrl Pts',(-7.95462684200006,15.2,7.17829544299998));
#243320=CARTESIAN_POINT('Ctrl Pts',(-7.95462684200006,11.6,7.17829544299998));
#243321=CARTESIAN_POINT('Ctrl Pts',(-7.95331021200005,15.2,7.17624428699998));
#243322=CARTESIAN_POINT('Ctrl Pts',(-7.95331021200005,11.6,7.17624428699998));
#243323=CARTESIAN_POINT('Ctrl Pts',(-7.95199519600006,15.2,7.17419954199999));
#243324=CARTESIAN_POINT('Ctrl Pts',(-7.95199519600006,11.6,7.17419954199999));
#243325=CARTESIAN_POINT('Ctrl Pts',(-7.95068181100006,15.2,7.17216121299998));
#243326=CARTESIAN_POINT('Ctrl Pts',(-7.95068181100006,11.6,7.17216121299998));
#243327=CARTESIAN_POINT('Ctrl Pts',(-7.94937007000006,15.2,7.17012930599999));
#243328=CARTESIAN_POINT('Ctrl Pts',(-7.94937007000006,11.6,7.17012930599999));
#243329=CARTESIAN_POINT('Ctrl Pts',(-7.94805998700006,15.2,7.16810382499999));
#243330=CARTESIAN_POINT('Ctrl Pts',(-7.94805998700006,11.6,7.16810382499999));
#243331=CARTESIAN_POINT('Ctrl Pts',(-7.94675157900006,15.2,7.16608477799999));
#243332=CARTESIAN_POINT('Ctrl Pts',(-7.94675157900006,11.6,7.16608477799999));
#243333=CARTESIAN_POINT('Ctrl Pts',(-7.94544485900006,15.2,7.16407216699999));
#243334=CARTESIAN_POINT('Ctrl Pts',(-7.94544485900006,11.6,7.16407216699999));
#243335=CARTESIAN_POINT('Ctrl Pts',(-7.94413984400006,15.2,7.16206599799998));
#243336=CARTESIAN_POINT('Ctrl Pts',(-7.94413984400006,11.6,7.16206599799998));
#243337=CARTESIAN_POINT('Ctrl Pts',(-7.94283654700005,15.2,7.16006627799998));
#243338=CARTESIAN_POINT('Ctrl Pts',(-7.94283654700005,11.6,7.16006627799998));
#243339=CARTESIAN_POINT('Ctrl Pts',(-7.94153498400006,15.2,7.15807301099999));
#243340=CARTESIAN_POINT('Ctrl Pts',(-7.94153498400006,11.6,7.15807301099999));
#243341=CARTESIAN_POINT('Ctrl Pts',(-7.94023517100006,15.2,7.15608620199998));
#243342=CARTESIAN_POINT('Ctrl Pts',(-7.94023517100006,11.6,7.15608620199998));
#243343=CARTESIAN_POINT('Ctrl Pts',(-7.93893712100005,15.2,7.15410585699999));
#243344=CARTESIAN_POINT('Ctrl Pts',(-7.93893712100005,11.6,7.15410585699999));
#243345=CARTESIAN_POINT('Ctrl Pts',(-7.93764085100006,15.2,7.15213197999999));
#243346=CARTESIAN_POINT('Ctrl Pts',(-7.93764085100006,11.6,7.15213197999999));
#243347=CARTESIAN_POINT('Ctrl Pts',(-7.93634637600006,15.2,7.15016457899999));
#243348=CARTESIAN_POINT('Ctrl Pts',(-7.93634637600006,11.6,7.15016457899999));
#243349=CARTESIAN_POINT('Ctrl Pts',(-7.93505371000006,15.2,7.14820365599999));
#243350=CARTESIAN_POINT('Ctrl Pts',(-7.93505371000006,11.6,7.14820365599999));
#243351=CARTESIAN_POINT('Ctrl Pts',(-7.93376287100005,15.2,7.14624921799999));
#243352=CARTESIAN_POINT('Ctrl Pts',(-7.93376287100005,11.6,7.14624921799999));
#243353=CARTESIAN_POINT('Ctrl Pts',(-7.93247387100006,15.2,7.14430126999999));
#243354=CARTESIAN_POINT('Ctrl Pts',(-7.93247387100006,11.6,7.14430126999999));
#243355=CARTESIAN_POINT('Ctrl Pts',(-7.93118672800006,15.2,7.14235981699999));
#243356=CARTESIAN_POINT('Ctrl Pts',(-7.93118672800006,11.6,7.14235981699999));
#243357=CARTESIAN_POINT('Ctrl Pts',(-7.92990145700006,15.2,7.14042486499999));
#243358=CARTESIAN_POINT('Ctrl Pts',(-7.92990145700006,11.6,7.14042486499999));
#243359=CARTESIAN_POINT('Ctrl Pts',(-7.92861807300006,15.2,7.13849641899999));
#243360=CARTESIAN_POINT('Ctrl Pts',(-7.92861807300006,11.6,7.13849641899999));
#243361=CARTESIAN_POINT('Ctrl Pts',(-7.92733659200006,15.2,7.13657448399999));
#243362=CARTESIAN_POINT('Ctrl Pts',(-7.92733659200006,11.6,7.13657448399999));
#243363=CARTESIAN_POINT('Ctrl Pts',(-7.92605703000006,15.2,7.13465906499999));
#243364=CARTESIAN_POINT('Ctrl Pts',(-7.92605703000006,11.6,7.13465906499999));
#243365=CARTESIAN_POINT('Ctrl Pts',(-7.92477940100006,15.2,7.13275016799999));
#243366=CARTESIAN_POINT('Ctrl Pts',(-7.92477940100006,11.6,7.13275016799999));
#243367=CARTESIAN_POINT('Ctrl Pts',(-7.92350372300006,15.2,7.13084779799999));
#243368=CARTESIAN_POINT('Ctrl Pts',(-7.92350372300006,11.6,7.13084779799999));
#243369=CARTESIAN_POINT('Ctrl Pts',(-7.92223001100006,15.2,7.12895196099999));
#243370=CARTESIAN_POINT('Ctrl Pts',(-7.92223001100006,11.6,7.12895196099999));
#243371=CARTESIAN_POINT('Ctrl Pts',(-7.92095828000006,15.2,7.12706266099998));
#243372=CARTESIAN_POINT('Ctrl Pts',(-7.92095828000006,11.6,7.12706266099998));
#243373=CARTESIAN_POINT('Ctrl Pts',(-7.91968854700006,15.2,7.12517990399999));
#243374=CARTESIAN_POINT('Ctrl Pts',(-7.91968854700006,11.6,7.12517990399999));
#243375=CARTESIAN_POINT('Ctrl Pts',(-7.91842082700006,15.2,7.12330369699998));
#243376=CARTESIAN_POINT('Ctrl Pts',(-7.91842082700006,11.6,7.12330369699998));
#243377=CARTESIAN_POINT('Ctrl Pts',(-7.91715513700006,15.2,7.12143404199999));
#243378=CARTESIAN_POINT('Ctrl Pts',(-7.91715513700006,11.6,7.12143404199999));
#243379=CARTESIAN_POINT('Ctrl Pts',(-7.91589149200006,15.2,7.11957094699999));
#243380=CARTESIAN_POINT('Ctrl Pts',(-7.91589149200006,11.6,7.11957094699999));
#243381=CARTESIAN_POINT('Ctrl Pts',(-7.91462990900006,15.2,7.11771441599999));
#243382=CARTESIAN_POINT('Ctrl Pts',(-7.91462990900006,11.6,7.11771441599999));
#243383=CARTESIAN_POINT('Ctrl Pts',(-7.91337040500006,15.2,7.11586445499999));
#243384=CARTESIAN_POINT('Ctrl Pts',(-7.91337040500006,11.6,7.11586445499999));
#243385=CARTESIAN_POINT('Ctrl Pts',(-7.91211299300006,15.2,7.11402106899998));
#243386=CARTESIAN_POINT('Ctrl Pts',(-7.91211299300006,11.6,7.11402106899998));
#243387=CARTESIAN_POINT('Ctrl Pts',(-7.91085769300006,15.2,7.11218426399999));
#243388=CARTESIAN_POINT('Ctrl Pts',(-7.91085769300006,11.6,7.11218426399999));
#243389=CARTESIAN_POINT('Ctrl Pts',(-7.90960451900006,15.2,7.11035404499999));
#243390=CARTESIAN_POINT('Ctrl Pts',(-7.90960451900006,11.6,7.11035404499999));
#243391=CARTESIAN_POINT('Ctrl Pts',(-7.90835348900006,15.2,7.10853041599999));
#243392=CARTESIAN_POINT('Ctrl Pts',(-7.90835348900006,11.6,7.10853041599999));
#243393=CARTESIAN_POINT('Ctrl Pts',(-7.90710461800006,15.2,7.10671338599998));
#243394=CARTESIAN_POINT('Ctrl Pts',(-7.90710461800006,11.6,7.10671338599998));
#243395=CARTESIAN_POINT('Ctrl Pts',(-7.90585792200006,15.2,7.10490295699999));
#243396=CARTESIAN_POINT('Ctrl Pts',(-7.90585792200006,11.6,7.10490295699999));
#243397=CARTESIAN_POINT('Ctrl Pts',(-7.90461341900006,15.2,7.10309913499999));
#243398=CARTESIAN_POINT('Ctrl Pts',(-7.90461341900006,11.6,7.10309913499999));
#243399=CARTESIAN_POINT('Ctrl Pts',(-7.90337112600006,15.2,7.10130192599999));
#243400=CARTESIAN_POINT('Ctrl Pts',(-7.90337112600006,11.6,7.10130192599999));
#243401=CARTESIAN_POINT('Ctrl Pts',(-7.90213105800006,15.2,7.09951133599999));
#243402=CARTESIAN_POINT('Ctrl Pts',(-7.90213105800006,11.6,7.09951133599999));
#243403=CARTESIAN_POINT('Ctrl Pts',(-7.90089323400006,15.2,7.09772736899998));
#243404=CARTESIAN_POINT('Ctrl Pts',(-7.90089323400006,11.6,7.09772736899998));
#243405=CARTESIAN_POINT('Ctrl Pts',(-7.89965766800006,15.2,7.09595003199999));
#243406=CARTESIAN_POINT('Ctrl Pts',(-7.89965766800006,11.6,7.09595003199999));
#243407=CARTESIAN_POINT('Ctrl Pts',(-7.89842437800005,15.2,7.09417932899999));
#243408=CARTESIAN_POINT('Ctrl Pts',(-7.89842437800005,11.6,7.09417932899999));
#243409=CARTESIAN_POINT('Ctrl Pts',(-7.89719338100006,15.2,7.09241526599998));
#243410=CARTESIAN_POINT('Ctrl Pts',(-7.89719338100006,11.6,7.09241526599998));
#243411=CARTESIAN_POINT('Ctrl Pts',(-7.89596469400006,15.2,7.09065784899998));
#243412=CARTESIAN_POINT('Ctrl Pts',(-7.89596469400006,11.6,7.09065784899998));
#243413=CARTESIAN_POINT('Ctrl Pts',(-7.89473833400006,15.2,7.08890708299998));
#243414=CARTESIAN_POINT('Ctrl Pts',(-7.89473833400006,11.6,7.08890708299998));
#243415=CARTESIAN_POINT('Ctrl Pts',(-7.89351431800006,15.2,7.08716297299999));
#243416=CARTESIAN_POINT('Ctrl Pts',(-7.89351431800006,11.6,7.08716297299999));
#243417=CARTESIAN_POINT('Ctrl Pts',(-7.89229266400006,15.2,7.08542552399998));
#243418=CARTESIAN_POINT('Ctrl Pts',(-7.89229266400006,11.6,7.08542552399998));
#243419=CARTESIAN_POINT('Ctrl Pts',(-7.89107338700005,15.2,7.08369474399999));
#243420=CARTESIAN_POINT('Ctrl Pts',(-7.89107338700005,11.6,7.08369474399999));
#243421=CARTESIAN_POINT('Ctrl Pts',(-7.88985650600005,15.2,7.08197063499998));
#243422=CARTESIAN_POINT('Ctrl Pts',(-7.88985650600005,11.6,7.08197063499998));
#243423=CARTESIAN_POINT('Ctrl Pts',(-7.88864203800006,15.2,7.08025320599998));
#243424=CARTESIAN_POINT('Ctrl Pts',(-7.88864203800006,11.6,7.08025320599998));
#243425=CARTESIAN_POINT('Ctrl Pts',(-7.88743000000006,15.2,7.07854245999999));
#243426=CARTESIAN_POINT('Ctrl Pts',(-7.88743000000006,11.6,7.07854245999999));
#243427=CARTESIAN_POINT('Ctrl Pts',(-7.88622040900006,15.2,7.07683840299998));
#243428=CARTESIAN_POINT('Ctrl Pts',(-7.88622040900006,11.6,7.07683840299998));
#243429=CARTESIAN_POINT('Ctrl Pts',(-7.88501328300006,15.2,7.07514104099998));
#243430=CARTESIAN_POINT('Ctrl Pts',(-7.88501328300006,11.6,7.07514104099998));
#243431=CARTESIAN_POINT('Ctrl Pts',(-7.88380864000005,15.2,7.07345037899999));
#243432=CARTESIAN_POINT('Ctrl Pts',(-7.88380864000005,11.6,7.07345037899999));
#243433=CARTESIAN_POINT('Ctrl Pts',(-7.88260649600005,15.2,7.07176642199999));
#243434=CARTESIAN_POINT('Ctrl Pts',(-7.88260649600005,11.6,7.07176642199999));
#243435=CARTESIAN_POINT('Ctrl Pts',(-7.88140687100006,15.2,7.07008917799998));
#243436=CARTESIAN_POINT('Ctrl Pts',(-7.88140687100006,11.6,7.07008917799998));
#243437=CARTESIAN_POINT('Ctrl Pts',(-7.88020978100005,15.2,7.06841864999999));
#243438=CARTESIAN_POINT('Ctrl Pts',(-7.88020978100005,11.6,7.06841864999999));
#243439=CARTESIAN_POINT('Ctrl Pts',(-7.87901524500005,15.2,7.06675484299998));
#243440=CARTESIAN_POINT('Ctrl Pts',(-7.87901524500005,11.6,7.06675484299998));
#243441=CARTESIAN_POINT('Ctrl Pts',(-7.87782327800005,15.2,7.06509776599999));
#243442=CARTESIAN_POINT('Ctrl Pts',(-7.87782327800005,11.6,7.06509776599999));
#243443=CARTESIAN_POINT('Ctrl Pts',(-7.87663390200006,15.2,7.06344742199998));
#243444=CARTESIAN_POINT('Ctrl Pts',(-7.87663390200006,11.6,7.06344742199998));
#243445=CARTESIAN_POINT('Ctrl Pts',(-7.87544713200005,15.2,7.06180381599999));
#243446=CARTESIAN_POINT('Ctrl Pts',(-7.87544713200005,11.6,7.06180381599999));
#243447=CARTESIAN_POINT('Ctrl Pts',(-7.87426298700005,15.2,7.06016695499999));
#243448=CARTESIAN_POINT('Ctrl Pts',(-7.87426298700005,11.6,7.06016695499999));
#243449=CARTESIAN_POINT('Ctrl Pts',(-7.87308148500006,15.2,7.05853684399998));
#243450=CARTESIAN_POINT('Ctrl Pts',(-7.87308148500006,11.6,7.05853684399998));
#243451=CARTESIAN_POINT('Ctrl Pts',(-7.87190264400006,15.2,7.05691348899999));
#243452=CARTESIAN_POINT('Ctrl Pts',(-7.87190264400006,11.6,7.05691348899999));
#243453=CARTESIAN_POINT('Ctrl Pts',(-7.87072648300006,15.2,7.05529689499999));
#243454=CARTESIAN_POINT('Ctrl Pts',(-7.87072648300006,11.6,7.05529689499999));
#243455=CARTESIAN_POINT('Ctrl Pts',(-7.86955301900005,15.2,7.05368706799998));
#243456=CARTESIAN_POINT('Ctrl Pts',(-7.86955301900005,11.6,7.05368706799998));
#243457=CARTESIAN_POINT('Ctrl Pts',(-7.86838227000005,15.2,7.05208401299998));
#243458=CARTESIAN_POINT('Ctrl Pts',(-7.86838227000005,11.6,7.05208401299998));
#243459=CARTESIAN_POINT('Ctrl Pts',(-7.86721425700006,15.2,7.05048773599999));
#243460=CARTESIAN_POINT('Ctrl Pts',(-7.86721425700006,11.6,7.05048773599999));
#243461=CARTESIAN_POINT('Ctrl Pts',(-7.86604899600006,15.2,7.04889824399999));
#243462=CARTESIAN_POINT('Ctrl Pts',(-7.86604899600006,11.6,7.04889824399999));
#243463=CARTESIAN_POINT('Ctrl Pts',(-7.86488650700005,15.2,7.04731553999999));
#243464=CARTESIAN_POINT('Ctrl Pts',(-7.86488650700005,11.6,7.04731553999999));
#243465=CARTESIAN_POINT('Ctrl Pts',(-7.86372680800006,15.2,7.04573962999999));
#243466=CARTESIAN_POINT('Ctrl Pts',(-7.86372680800006,11.6,7.04573962999999));
#243467=CARTESIAN_POINT('Ctrl Pts',(-7.86256991700006,15.2,7.04417052199998));
#243468=CARTESIAN_POINT('Ctrl Pts',(-7.86256991700006,11.6,7.04417052199998));
#243469=CARTESIAN_POINT('Ctrl Pts',(-7.86141585400006,15.2,7.04260821999998));
#243470=CARTESIAN_POINT('Ctrl Pts',(-7.86141585400006,11.6,7.04260821999998));
#243471=CARTESIAN_POINT('Ctrl Pts',(-7.86026463600006,15.2,7.04105272899999));
#243472=CARTESIAN_POINT('Ctrl Pts',(-7.86026463600006,11.6,7.04105272899999));
#243473=CARTESIAN_POINT('Ctrl Pts',(-7.85911628400005,15.2,7.03950405599999));
#243474=CARTESIAN_POINT('Ctrl Pts',(-7.85911628400005,11.6,7.03950405599999));
#243475=CARTESIAN_POINT('Ctrl Pts',(-7.85797081600006,15.2,7.03796220599998));
#243476=CARTESIAN_POINT('Ctrl Pts',(-7.85797081600006,11.6,7.03796220599998));
#243477=CARTESIAN_POINT('Ctrl Pts',(-7.85682825100006,15.2,7.03642718499999));
#243478=CARTESIAN_POINT('Ctrl Pts',(-7.85682825100006,11.6,7.03642718499999));
#243479=CARTESIAN_POINT('Ctrl Pts',(-7.85568860800005,15.2,7.03489899899999));
#243480=CARTESIAN_POINT('Ctrl Pts',(-7.85568860800005,11.6,7.03489899899999));
#243481=CARTESIAN_POINT('Ctrl Pts',(-7.85455190600005,15.2,7.03337765199999));
#243482=CARTESIAN_POINT('Ctrl Pts',(-7.85455190600005,11.6,7.03337765199999));
#243483=CARTESIAN_POINT('Ctrl Pts',(-7.85341816500006,15.2,7.03186315199999));
#243484=CARTESIAN_POINT('Ctrl Pts',(-7.85341816500006,11.6,7.03186315199999));
#243485=CARTESIAN_POINT('Ctrl Pts',(-7.85228740400005,15.2,7.03035550199999));
#243486=CARTESIAN_POINT('Ctrl Pts',(-7.85228740400005,11.6,7.03035550199999));
#243487=CARTESIAN_POINT('Ctrl Pts',(-7.85115964100005,15.2,7.02885470999998));
#243488=CARTESIAN_POINT('Ctrl Pts',(-7.85115964100005,11.6,7.02885470999998));
#243489=CARTESIAN_POINT('Ctrl Pts',(-7.85003489800006,15.2,7.02736078099999));
#243490=CARTESIAN_POINT('Ctrl Pts',(-7.85003489800006,11.6,7.02736078099999));
#243491=CARTESIAN_POINT('Ctrl Pts',(-7.84891319200005,15.2,7.02587372099998));
#243492=CARTESIAN_POINT('Ctrl Pts',(-7.84891319200005,11.6,7.02587372099998));
#243493=CARTESIAN_POINT('Ctrl Pts',(-7.84779454400006,15.2,7.02439353499998));
#243494=CARTESIAN_POINT('Ctrl Pts',(-7.84779454400006,11.6,7.02439353499998));
#243495=CARTESIAN_POINT('Ctrl Pts',(-7.84667897300006,15.2,7.02292022999998));
#243496=CARTESIAN_POINT('Ctrl Pts',(-7.84667897300006,11.6,7.02292022999998));
#243497=CARTESIAN_POINT('Ctrl Pts',(-7.84556650000006,15.2,7.02145380999998));
#243498=CARTESIAN_POINT('Ctrl Pts',(-7.84556650000006,11.6,7.02145380999998));
#243499=CARTESIAN_POINT('Ctrl Pts',(-7.84445714300006,15.2,7.01999428199999));
#243500=CARTESIAN_POINT('Ctrl Pts',(-7.84445714300006,11.6,7.01999428199999));
#243501=CARTESIAN_POINT('Ctrl Pts',(-7.84335092300006,15.2,7.01854165199999));
#243502=CARTESIAN_POINT('Ctrl Pts',(-7.84335092300006,11.6,7.01854165199999));
#243503=CARTESIAN_POINT('Ctrl Pts',(-7.84224785900006,15.2,7.01709592399999));
#243504=CARTESIAN_POINT('Ctrl Pts',(-7.84224785900006,11.6,7.01709592399999));
#243505=CARTESIAN_POINT('Ctrl Pts',(-7.84114797200005,15.2,7.01565710699998));
#243506=CARTESIAN_POINT('Ctrl Pts',(-7.84114797200005,11.6,7.01565710699998));
#243507=CARTESIAN_POINT('Ctrl Pts',(-7.84005128300005,15.2,7.01422520199999));
#243508=CARTESIAN_POINT('Ctrl Pts',(-7.84005128300005,11.6,7.01422520199999));
#243509=CARTESIAN_POINT('Ctrl Pts',(-7.83895781000006,15.2,7.01280021999998));
#243510=CARTESIAN_POINT('Ctrl Pts',(-7.83895781000006,11.6,7.01280021999998));
#243511=CARTESIAN_POINT('Ctrl Pts',(-7.83786757400006,15.2,7.01138216399999));
#243512=CARTESIAN_POINT('Ctrl Pts',(-7.83786757400006,11.6,7.01138216399999));
#243513=CARTESIAN_POINT('Ctrl Pts',(-7.83678059600006,15.2,7.00997103999998));
#243514=CARTESIAN_POINT('Ctrl Pts',(-7.83678059600006,11.6,7.00997103999998));
#243515=CARTESIAN_POINT('Ctrl Pts',(-7.83569689500006,15.2,7.00856685299998));
#243516=CARTESIAN_POINT('Ctrl Pts',(-7.83569689500006,11.6,7.00856685299998));
#243517=CARTESIAN_POINT('Ctrl Pts',(-7.83461649300006,15.2,7.00716961199999));
#243518=CARTESIAN_POINT('Ctrl Pts',(-7.83461649300006,11.6,7.00716961199999));
#243519=CARTESIAN_POINT('Ctrl Pts',(-7.83353941100006,15.2,7.00577931999998));
#243520=CARTESIAN_POINT('Ctrl Pts',(-7.83353941100006,11.6,7.00577931999998));
#243521=CARTESIAN_POINT('Ctrl Pts',(-7.83246566700005,15.2,7.00439598299998));
#243522=CARTESIAN_POINT('Ctrl Pts',(-7.83246566700005,11.6,7.00439598299998));
#243523=CARTESIAN_POINT('Ctrl Pts',(-7.83139528400006,15.2,7.00301960799998));
#243524=CARTESIAN_POINT('Ctrl Pts',(-7.83139528400006,11.6,7.00301960799998));
#243525=CARTESIAN_POINT('Ctrl Pts',(-7.83032828200006,15.2,7.00165019999999));
#243526=CARTESIAN_POINT('Ctrl Pts',(-7.83032828200006,11.6,7.00165019999999));
#243527=CARTESIAN_POINT('Ctrl Pts',(-7.82926468300006,15.2,7.00028776499998));
#243528=CARTESIAN_POINT('Ctrl Pts',(-7.82926468300006,11.6,7.00028776499998));
#243529=CARTESIAN_POINT('Ctrl Pts',(-7.82820450700005,15.2,6.99893230999999));
#243530=CARTESIAN_POINT('Ctrl Pts',(-7.82820450700005,11.6,6.99893230999999));
#243531=CARTESIAN_POINT('Ctrl Pts',(-7.82714777400006,15.2,6.99758383999999));
#243532=CARTESIAN_POINT('Ctrl Pts',(-7.82714777400006,11.6,6.99758383999999));
#243533=CARTESIAN_POINT('Ctrl Pts',(-7.82609450600006,15.2,6.99624236099999));
#243534=CARTESIAN_POINT('Ctrl Pts',(-7.82609450600006,11.6,6.99624236099999));
#243535=CARTESIAN_POINT('Ctrl Pts',(-7.82504472500006,15.2,6.99490787899999));
#243536=CARTESIAN_POINT('Ctrl Pts',(-7.82504472500006,11.6,6.99490787899999));
#243537=CARTESIAN_POINT('Ctrl Pts',(-7.82399845200005,15.2,6.99358039999999));
#243538=CARTESIAN_POINT('Ctrl Pts',(-7.82399845200005,11.6,6.99358039999999));
#243539=CARTESIAN_POINT('Ctrl Pts',(-7.82295570800006,15.2,6.99225992899999));
#243540=CARTESIAN_POINT('Ctrl Pts',(-7.82295570800006,11.6,6.99225992899999));
#243541=CARTESIAN_POINT('Ctrl Pts',(-7.82191651400005,15.2,6.99094647299999));
#243542=CARTESIAN_POINT('Ctrl Pts',(-7.82191651400005,11.6,6.99094647299999));
#243543=CARTESIAN_POINT('Ctrl Pts',(-7.82088089200006,15.2,6.98964003799999));
#243544=CARTESIAN_POINT('Ctrl Pts',(-7.82088089200006,11.6,6.98964003799999));
#243545=CARTESIAN_POINT('Ctrl Pts',(-7.81984886500006,15.2,6.98834062899999));
#243546=CARTESIAN_POINT('Ctrl Pts',(-7.81984886500006,11.6,6.98834062899999));
#243547=CARTESIAN_POINT('Ctrl Pts',(-7.81882045200006,15.2,6.98704825399999));
#243548=CARTESIAN_POINT('Ctrl Pts',(-7.81882045200006,11.6,6.98704825399999));
#243549=CARTESIAN_POINT('Ctrl Pts',(-7.81779567800006,15.2,6.98576291699998));
#243550=CARTESIAN_POINT('Ctrl Pts',(-7.81779567800006,11.6,6.98576291699998));
#243551=CARTESIAN_POINT('Ctrl Pts',(-7.81677456100006,15.2,6.98448462499999));
#243552=CARTESIAN_POINT('Ctrl Pts',(-7.81677456100006,11.6,6.98448462499999));
#243553=CARTESIAN_POINT('Ctrl Pts',(-7.81575712600005,15.2,6.98321338399998));
#243554=CARTESIAN_POINT('Ctrl Pts',(-7.81575712600005,11.6,6.98321338399998));
#243555=CARTESIAN_POINT('Ctrl Pts',(-7.81474339500006,15.2,6.98194919799998));
#243556=CARTESIAN_POINT('Ctrl Pts',(-7.81474339500006,11.6,6.98194919799998));
#243557=CARTESIAN_POINT('Ctrl Pts',(-7.81373338800006,15.2,6.98069207599998));
#243558=CARTESIAN_POINT('Ctrl Pts',(-7.81373338800006,11.6,6.98069207599998));
#243559=CARTESIAN_POINT('Ctrl Pts',(-7.81272713000006,15.2,6.97944202399999));
#243560=CARTESIAN_POINT('Ctrl Pts',(-7.81272713000006,11.6,6.97944202399999));
#243561=CARTESIAN_POINT('Ctrl Pts',(-7.81172464100005,15.2,6.97819904499998));
#243562=CARTESIAN_POINT('Ctrl Pts',(-7.81172464100005,11.6,6.97819904499998));
#243563=CARTESIAN_POINT('Ctrl Pts',(-7.81072594600006,15.2,6.97696314799998));
#243564=CARTESIAN_POINT('Ctrl Pts',(-7.81072594600006,11.6,6.97696314799998));
#243565=CARTESIAN_POINT('Ctrl Pts',(-7.80973106400006,15.2,6.97573433799998));
#243566=CARTESIAN_POINT('Ctrl Pts',(-7.80973106400006,11.6,6.97573433799998));
#243567=CARTESIAN_POINT('Ctrl Pts',(-7.80874002000005,15.2,6.97451262099998));
#243568=CARTESIAN_POINT('Ctrl Pts',(-7.80874002000005,11.6,6.97451262099998));
#243569=CARTESIAN_POINT('Ctrl Pts',(-7.80775283700006,15.2,6.97329800299999));
#243570=CARTESIAN_POINT('Ctrl Pts',(-7.80775283700006,11.6,6.97329800299999));
#243571=CARTESIAN_POINT('Ctrl Pts',(-7.80676953600006,15.2,6.97209049099998));
#243572=CARTESIAN_POINT('Ctrl Pts',(-7.80676953600006,11.6,6.97209049099998));
#243573=CARTESIAN_POINT('Ctrl Pts',(-7.80579014100006,15.2,6.97089009099999));
#243574=CARTESIAN_POINT('Ctrl Pts',(-7.80579014100006,11.6,6.97089009099999));
#243575=CARTESIAN_POINT('Ctrl Pts',(-7.80481467600006,15.2,6.96969680799998));
#243576=CARTESIAN_POINT('Ctrl Pts',(-7.80481467600006,11.6,6.96969680799998));
#243577=CARTESIAN_POINT('Ctrl Pts',(-7.80384316200006,15.2,6.96851064799999));
#243578=CARTESIAN_POINT('Ctrl Pts',(-7.80384316200006,11.6,6.96851064799999));
#243579=CARTESIAN_POINT('Ctrl Pts',(-7.80287562300006,15.2,6.96733161899999));
#243580=CARTESIAN_POINT('Ctrl Pts',(-7.80287562300006,11.6,6.96733161899999));
#243581=CARTESIAN_POINT('Ctrl Pts',(-7.80191208300005,15.2,6.96615972599999));
#243582=CARTESIAN_POINT('Ctrl Pts',(-7.80191208300005,11.6,6.96615972599999));
#243583=CARTESIAN_POINT('Ctrl Pts',(-7.80095256500006,15.2,6.96499497499998));
#243584=CARTESIAN_POINT('Ctrl Pts',(-7.80095256500006,11.6,6.96499497499998));
#243585=CARTESIAN_POINT('Ctrl Pts',(-7.79999709200006,15.2,6.96383737299998));
#243586=CARTESIAN_POINT('Ctrl Pts',(-7.79999709200006,11.6,6.96383737299998));
#243587=CARTESIAN_POINT('Ctrl Pts',(-7.79904568800006,15.2,6.96268692599999));
#243588=CARTESIAN_POINT('Ctrl Pts',(-7.79904568800006,11.6,6.96268692599999));
#243589=CARTESIAN_POINT('Ctrl Pts',(-7.79809837800006,15.2,6.96154363999998));
#243590=CARTESIAN_POINT('Ctrl Pts',(-7.79809837800006,11.6,6.96154363999998));
#243591=CARTESIAN_POINT('Ctrl Pts',(-7.79715518200006,15.2,6.96040752099999));
#243592=CARTESIAN_POINT('Ctrl Pts',(-7.79715518200006,11.6,6.96040752099999));
#243593=CARTESIAN_POINT('Ctrl Pts',(-7.79621612700005,15.2,6.95927857499999));
#243594=CARTESIAN_POINT('Ctrl Pts',(-7.79621612700005,11.6,6.95927857499999));
#243595=CARTESIAN_POINT('Ctrl Pts',(-7.79528123700005,15.2,6.95815680999999));
#243596=CARTESIAN_POINT('Ctrl Pts',(-7.79528123700005,11.6,6.95815680999999));
#243597=CARTESIAN_POINT('Ctrl Pts',(-7.79435053400006,15.2,6.95704223099998));
#243598=CARTESIAN_POINT('Ctrl Pts',(-7.79435053400006,11.6,6.95704223099998));
#243599=CARTESIAN_POINT('Ctrl Pts',(-7.79342404400006,15.2,6.95593484299999));
#243600=CARTESIAN_POINT('Ctrl Pts',(-7.79342404400006,11.6,6.95593484299999));
#243601=CARTESIAN_POINT('Ctrl Pts',(-7.79250179200006,15.2,6.95483465499999));
#243602=CARTESIAN_POINT('Ctrl Pts',(-7.79250179200006,11.6,6.95483465499999));
#243603=CARTESIAN_POINT('Ctrl Pts',(-7.79158380000006,15.2,6.95374166999999));
#243604=CARTESIAN_POINT('Ctrl Pts',(-7.79158380000006,11.6,6.95374166999999));
#243605=CARTESIAN_POINT('Ctrl Pts',(-7.79067009400006,15.2,6.95265589799998));
#243606=CARTESIAN_POINT('Ctrl Pts',(-7.79067009400006,11.6,6.95265589799998));
#243607=CARTESIAN_POINT('Ctrl Pts',(-7.78976069700006,15.2,6.95157734299999));
#243608=CARTESIAN_POINT('Ctrl Pts',(-7.78976069700006,11.6,6.95157734299999));
#243609=CARTESIAN_POINT('Ctrl Pts',(-7.78885563500006,15.2,6.95050601399998));
#243610=CARTESIAN_POINT('Ctrl Pts',(-7.78885563500006,11.6,6.95050601399998));
#243611=CARTESIAN_POINT('Ctrl Pts',(-7.78795493400006,15.2,6.94944191199999));
#243612=CARTESIAN_POINT('Ctrl Pts',(-7.78795493400006,11.6,6.94944191199999));
#243613=CARTESIAN_POINT('Ctrl Pts',(-7.78705861700006,15.2,6.94838504899998));
#243614=CARTESIAN_POINT('Ctrl Pts',(-7.78705861700006,11.6,6.94838504899998));
#243615=CARTESIAN_POINT('Ctrl Pts',(-7.78616671000006,15.2,6.94733542799998));
#243616=CARTESIAN_POINT('Ctrl Pts',(-7.78616671000006,11.6,6.94733542799998));
#243617=CARTESIAN_POINT('Ctrl Pts',(-7.78527923800005,15.2,6.94629305799998));
#243618=CARTESIAN_POINT('Ctrl Pts',(-7.78527923800005,11.6,6.94629305799998));
#243619=CARTESIAN_POINT('Ctrl Pts',(-7.78439622500006,15.2,6.94525794299999));
#243620=CARTESIAN_POINT('Ctrl Pts',(-7.78439622500006,11.6,6.94525794299999));
#243621=CARTESIAN_POINT('Ctrl Pts',(-7.78351769900006,15.2,6.94423009099999));
#243622=CARTESIAN_POINT('Ctrl Pts',(-7.78351769900006,11.6,6.94423009099999));
#243623=CARTESIAN_POINT('Ctrl Pts',(-7.78264368300006,15.2,6.94320950799998));
#243624=CARTESIAN_POINT('Ctrl Pts',(-7.78264368300006,11.6,6.94320950799998));
#243625=CARTESIAN_POINT('Ctrl Pts',(-7.78177420300005,15.2,6.94219619999998));
#243626=CARTESIAN_POINT('Ctrl Pts',(-7.78177420300005,11.6,6.94219619999998));
#243627=CARTESIAN_POINT('Ctrl Pts',(-7.78090928600006,15.2,6.94119017399998));
#243628=CARTESIAN_POINT('Ctrl Pts',(-7.78090928600006,11.6,6.94119017399998));
#243629=CARTESIAN_POINT('Ctrl Pts',(-7.78004895800006,15.2,6.94019143699999));
#243630=CARTESIAN_POINT('Ctrl Pts',(-7.78004895800006,11.6,6.94019143699999));
#243631=CARTESIAN_POINT('Ctrl Pts',(-7.77919324200005,15.2,6.93919999399998));
#243632=CARTESIAN_POINT('Ctrl Pts',(-7.77919324200005,11.6,6.93919999399998));
#243633=CARTESIAN_POINT('Ctrl Pts',(-7.77834216700005,15.2,6.93821585299998));
#243634=CARTESIAN_POINT('Ctrl Pts',(-7.77834216700005,11.6,6.93821585299998));
#243635=CARTESIAN_POINT('Ctrl Pts',(-7.77749575900006,15.2,6.93723901999999));
#243636=CARTESIAN_POINT('Ctrl Pts',(-7.77749575900006,11.6,6.93723901999999));
#243637=CARTESIAN_POINT('Ctrl Pts',(-7.77665404200006,15.2,6.93626949999998));
#243638=CARTESIAN_POINT('Ctrl Pts',(-7.77665404200006,11.6,6.93626949999998));
#243639=CARTESIAN_POINT('Ctrl Pts',(-7.77581704500006,15.2,6.93530730299998));
#243640=CARTESIAN_POINT('Ctrl Pts',(-7.77581704500006,11.6,6.93530730299998));
#243641=CARTESIAN_POINT('Ctrl Pts',(-7.77498479200006,15.2,6.93435243299999));
#243642=CARTESIAN_POINT('Ctrl Pts',(-7.77498479200006,11.6,6.93435243299999));
#243643=CARTESIAN_POINT('Ctrl Pts',(-7.77415731300006,15.2,6.93340489699998));
#243644=CARTESIAN_POINT('Ctrl Pts',(-7.77415731300006,11.6,6.93340489699998));
#243645=CARTESIAN_POINT('Ctrl Pts',(-7.77333463200006,15.2,6.93246470299999));
#243646=CARTESIAN_POINT('Ctrl Pts',(-7.77333463200006,11.6,6.93246470299999));
#243647=CARTESIAN_POINT('Ctrl Pts',(-7.77251677700006,15.2,6.93153185599999));
#243648=CARTESIAN_POINT('Ctrl Pts',(-7.77251677700006,11.6,6.93153185599999));
#243649=CARTESIAN_POINT('Ctrl Pts',(-7.77170377400005,15.2,6.93060636399998));
#243650=CARTESIAN_POINT('Ctrl Pts',(-7.77170377400005,11.6,6.93060636399998));
#243651=CARTESIAN_POINT('Ctrl Pts',(-7.77089565100006,15.2,6.92968823199998));
#243652=CARTESIAN_POINT('Ctrl Pts',(-7.77089565100006,11.6,6.92968823199998));
#243653=CARTESIAN_POINT('Ctrl Pts',(-7.77009243600006,15.2,6.92877746799999));
#243654=CARTESIAN_POINT('Ctrl Pts',(-7.77009243600006,11.6,6.92877746799999));
#243655=CARTESIAN_POINT('Ctrl Pts',(-7.76929415400006,15.2,6.92787407899999));
#243656=CARTESIAN_POINT('Ctrl Pts',(-7.76929415400006,11.6,6.92787407899999));
#243657=CARTESIAN_POINT('Ctrl Pts',(-7.76850083500006,15.2,6.92697806999998));
#243658=CARTESIAN_POINT('Ctrl Pts',(-7.76850083500006,11.6,6.92697806999998));
#243659=CARTESIAN_POINT('Ctrl Pts',(-7.76771250600006,15.2,6.92608944899998));
#243660=CARTESIAN_POINT('Ctrl Pts',(-7.76771250600006,11.6,6.92608944899998));
#243661=CARTESIAN_POINT('Ctrl Pts',(-7.76692919400006,15.2,6.92520822299999));
#243662=CARTESIAN_POINT('Ctrl Pts',(-7.76692919400006,11.6,6.92520822299999));
#243663=CARTESIAN_POINT('Ctrl Pts',(-7.76615092800006,15.2,6.92433439799998));
#243664=CARTESIAN_POINT('Ctrl Pts',(-7.76615092800006,11.6,6.92433439799998));
#243665=CARTESIAN_POINT('Ctrl Pts',(-7.76537773500006,15.2,6.92346798199999));
#243666=CARTESIAN_POINT('Ctrl Pts',(-7.76537773500006,11.6,6.92346798199999));
#243667=CARTESIAN_POINT('Ctrl Pts',(-7.76460964500006,15.2,6.92260897999999));
#243668=CARTESIAN_POINT('Ctrl Pts',(-7.76460964500006,11.6,6.92260897999999));
#243669=CARTESIAN_POINT('Ctrl Pts',(-7.76384668300006,15.2,6.92175739999998));
#243670=CARTESIAN_POINT('Ctrl Pts',(-7.76384668300006,11.6,6.92175739999998));
#243671=CARTESIAN_POINT('Ctrl Pts',(-7.76308888000005,15.2,6.92091324899998));
#243672=CARTESIAN_POINT('Ctrl Pts',(-7.76308888000005,11.6,6.92091324899998));
#243673=CARTESIAN_POINT('Ctrl Pts',(-7.76233626500006,15.2,6.92007653299999));
#243674=CARTESIAN_POINT('Ctrl Pts',(-7.76233626500006,11.6,6.92007653299999));
#243675=CARTESIAN_POINT('Ctrl Pts',(-7.76158886500006,15.2,6.91924725999999));
#243676=CARTESIAN_POINT('Ctrl Pts',(-7.76158886500006,11.6,6.91924725999999));
#243677=CARTESIAN_POINT('Ctrl Pts',(-7.76084671000006,15.2,6.91842543699998));
#243678=CARTESIAN_POINT('Ctrl Pts',(-7.76084671000006,11.6,6.91842543699998));
#243679=CARTESIAN_POINT('Ctrl Pts',(-7.76010982700006,15.2,6.91761106899998));
#243680=CARTESIAN_POINT('Ctrl Pts',(-7.76010982700006,11.6,6.91761106899998));
#243681=CARTESIAN_POINT('Ctrl Pts',(-7.75937824900006,15.2,6.91680416399999));
#243682=CARTESIAN_POINT('Ctrl Pts',(-7.75937824900006,11.6,6.91680416399999));
#243683=CARTESIAN_POINT('Ctrl Pts',(-7.75865200200006,15.2,6.91600473099999));
#243684=CARTESIAN_POINT('Ctrl Pts',(-7.75865200200006,11.6,6.91600473099999));
#243685=CARTESIAN_POINT('Ctrl Pts',(-7.75793111600006,15.2,6.91521277299999));
#243686=CARTESIAN_POINT('Ctrl Pts',(-7.75793111600006,11.6,6.91521277299999));
#243687=CARTESIAN_POINT('Ctrl Pts',(-7.75721562100006,15.2,6.91442829999998));
#243688=CARTESIAN_POINT('Ctrl Pts',(-7.75721562100006,11.6,6.91442829999998));
#243689=CARTESIAN_POINT('Ctrl Pts',(-7.75650554800006,15.2,6.91365131899998));
#243690=CARTESIAN_POINT('Ctrl Pts',(-7.75650554800006,11.6,6.91365131899998));
#243691=CARTESIAN_POINT('Ctrl Pts',(-7.75580092400006,15.2,6.91288183599998));
#243692=CARTESIAN_POINT('Ctrl Pts',(-7.75580092400006,11.6,6.91288183599998));
#243693=CARTESIAN_POINT('Ctrl Pts',(-7.75510178000006,15.2,6.91211985699999));
#243694=CARTESIAN_POINT('Ctrl Pts',(-7.75510178000006,11.6,6.91211985699999));
#243695=CARTESIAN_POINT('Ctrl Pts',(-7.75440814900006,15.2,6.91136539199999));
#243696=CARTESIAN_POINT('Ctrl Pts',(-7.75440814900006,11.6,6.91136539199999));
#243697=CARTESIAN_POINT('Ctrl Pts',(-7.75372005700006,15.2,6.91061844599999));
#243698=CARTESIAN_POINT('Ctrl Pts',(-7.75372005700006,11.6,6.91061844599999));
#243699=CARTESIAN_POINT('Ctrl Pts',(-7.75303753800006,15.2,6.90987902599999));
#243700=CARTESIAN_POINT('Ctrl Pts',(-7.75303753800006,11.6,6.90987902599999));
#243701=CARTESIAN_POINT('Ctrl Pts',(-7.75236062000006,15.2,6.90914714099998));
#243702=CARTESIAN_POINT('Ctrl Pts',(-7.75236062000006,11.6,6.90914714099998));
#243703=CARTESIAN_POINT('Ctrl Pts',(-7.75168933500006,15.2,6.90842279499999));
#243704=CARTESIAN_POINT('Ctrl Pts',(-7.75168933500006,11.6,6.90842279499999));
#243705=CARTESIAN_POINT('Ctrl Pts',(-7.75102371400005,15.2,6.90770599899999));
#243706=CARTESIAN_POINT('Ctrl Pts',(-7.75102371400005,11.6,6.90770599899999));
#243707=CARTESIAN_POINT('Ctrl Pts',(-7.75036378800006,15.2,6.90699675799999));
#243708=CARTESIAN_POINT('Ctrl Pts',(-7.75036378800006,11.6,6.90699675799999));
#243709=CARTESIAN_POINT('Ctrl Pts',(-7.74970958800005,15.2,6.90629507899998));
#243710=CARTESIAN_POINT('Ctrl Pts',(-7.74970958800005,11.6,6.90629507899998));
#243711=CARTESIAN_POINT('Ctrl Pts',(-7.74906114600006,15.2,6.90560096999998));
#243712=CARTESIAN_POINT('Ctrl Pts',(-7.74906114600006,11.6,6.90560096999998));
#243713=CARTESIAN_POINT('Ctrl Pts',(-7.74841849100006,15.2,6.90491443799999));
#243714=CARTESIAN_POINT('Ctrl Pts',(-7.74841849100006,11.6,6.90491443799999));
#243715=CARTESIAN_POINT('Ctrl Pts',(-7.74778165900005,15.2,6.90423549099999));
#243716=CARTESIAN_POINT('Ctrl Pts',(-7.74778165900005,11.6,6.90423549099999));
#243717=CARTESIAN_POINT('Ctrl Pts',(-7.74715431200006,15.2,6.90356800199999));
#243718=CARTESIAN_POINT('Ctrl Pts',(-7.74715431200006,11.6,6.90356800199999));
#243719=CARTESIAN_POINT('Ctrl Pts',(-7.74665780200006,15.2,6.90304077499999));
#243720=CARTESIAN_POINT('Ctrl Pts',(-7.74665780200006,11.6,6.90304077499999));
#243721=CARTESIAN_POINT('Ctrl Pts',(-7.74628893100005,15.2,6.90264966899999));
#243722=CARTESIAN_POINT('Ctrl Pts',(-7.74628893100005,11.6,6.90264966899999));
#243723=CARTESIAN_POINT('Ctrl Pts',(-7.74604536300006,15.2,6.90239167399999));
#243724=CARTESIAN_POINT('Ctrl Pts',(-7.74604536300006,11.6,6.90239167399999));
#243725=CARTESIAN_POINT('Ctrl Pts',(-7.74592563800006,15.2,6.90226491999999));
#243726=CARTESIAN_POINT('Ctrl Pts',(-7.74592563800006,11.6,6.90226491999999));
#243727=CARTESIAN_POINT('',(-7.74592563733583,12.2,6.90226492000216));
#243728=CARTESIAN_POINT('',(-7.74592563733583,15.2,6.90226492000216));
#243729=CARTESIAN_POINT('',(-7.74592563700006,12.2,6.90226491999999));
#243730=CARTESIAN_POINT('Ctrl Pts',(-8.32310290900006,12.2,7.93573928299999));
#243731=CARTESIAN_POINT('Ctrl Pts',(-8.3217721687583,12.2,7.93215545234894));
#243732=CARTESIAN_POINT('Ctrl Pts',(-8.32043968335571,12.2,7.92857931992112));
#243733=CARTESIAN_POINT('Ctrl Pts',(-8.31910545589695,12.2,7.92501089665198));
#243734=CARTESIAN_POINT('Ctrl Pts',(-8.31777122843819,12.2,7.92144247338284));
#243735=CARTESIAN_POINT('Ctrl Pts',(-8.31643525654356,12.2,7.91788175518672));
#243736=CARTESIAN_POINT('Ctrl Pts',(-8.31509755652553,12.2,7.91432875292909));
#243737=CARTESIAN_POINT('Ctrl Pts',(-8.31375985650751,12.2,7.91077575067146));
#243738=CARTESIAN_POINT('Ctrl Pts',(-8.31242042912681,12.2,7.90723046471033));
#243739=CARTESIAN_POINT('Ctrl Pts',(-8.31107930955076,12.2,7.90369291629612));
#243740=CARTESIAN_POINT('Ctrl Pts',(-8.30973818973107,12.2,7.90015536723925));
#243741=CARTESIAN_POINT('Ctrl Pts',(-8.3083953809026,12.2,7.89662555690962));
#243742=CARTESIAN_POINT('Ctrl Pts',(-8.30705092395697,12.2,7.89310351077379));
#243743=CARTESIAN_POINT('Ctrl Pts',(-8.30570646725559,12.2,7.88958146527781));
#243744=CARTESIAN_POINT('Ctrl Pts',(-8.30436036267098,12.2,7.88606718318977));
#243745=CARTESIAN_POINT('Ctrl Pts',(-8.30301264530314,12.2,7.88256068565118));
#243746=CARTESIAN_POINT('Ctrl Pts',(-8.3016649279353,12.2,7.8790541881126));
#243747=CARTESIAN_POINT('Ctrl Pts',(-8.30031559653923,12.2,7.87555547376907));
#243748=CARTESIAN_POINT('Ctrl Pts',(-8.29896468270717,12.2,7.87206456271343));
#243749=CARTESIAN_POINT('Ctrl Pts',(-8.29761376887511,12.2,7.86857365165778));
#243750=CARTESIAN_POINT('Ctrl Pts',(-8.29626127309158,12.2,7.86509054252597));
#243751=CARTESIAN_POINT('Ctrl Pts',(-8.29490723125963,12.2,7.86161525801142));
#243752=CARTESIAN_POINT('Ctrl Pts',(-8.29355318942768,12.2,7.85813997349687));
#243753=CARTESIAN_POINT('Ctrl Pts',(-8.29219760124853,12.2,7.85467251283548));
#243754=CARTESIAN_POINT('Ctrl Pts',(-8.29084050442296,12.2,7.85121289833549));
#243755=CARTESIAN_POINT('Ctrl Pts',(-8.2894834075974,12.2,7.8477532838355));
#243756=CARTESIAN_POINT('Ctrl Pts',(-8.28812480111361,12.2,7.84430151517664));
#243757=CARTESIAN_POINT('Ctrl Pts',(-8.28676472178823,12.2,7.84085761175903));
#243758=CARTESIAN_POINT('Ctrl Pts',(-8.28540464221577,12.2,7.83741370771578));
#243759=CARTESIAN_POINT('Ctrl Pts',(-8.28404308923455,12.2,7.83397767058309));
#243760=CARTESIAN_POINT('Ctrl Pts',(-8.2826800977446,12.2,7.83054951996093));
#243761=CARTESIAN_POINT('Ctrl Pts',(-8.28131710650225,12.2,7.82712136996156));
#243762=CARTESIAN_POINT('Ctrl Pts',(-8.2799526774879,12.2,7.82370110605206));
#243763=CARTESIAN_POINT('Ctrl Pts',(-8.27858684621913,12.2,7.8202887503398));
#243764=CARTESIAN_POINT('Ctrl Pts',(-8.27722101495035,12.2,7.81687639462754));
#243765=CARTESIAN_POINT('Ctrl Pts',(-8.27585378260126,12.2,7.81347194655575));
#243766=CARTESIAN_POINT('Ctrl Pts',(-8.2744851853592,12.2,7.81007542713818));
#243767=CARTESIAN_POINT('Ctrl Pts',(-8.27266038911933,12.2,7.80554673478709));
#243768=CARTESIAN_POINT('Ctrl Pts',(-8.27083316650773,12.2,7.80103213932765));
#243769=CARTESIAN_POINT('Ctrl Pts',(-8.2690036048242,12.2,7.79653168752742));
#243770=CARTESIAN_POINT('Ctrl Pts',(-8.26717404289138,12.2,7.79203123511401));
#243771=CARTESIAN_POINT('Ctrl Pts',(-8.26534214192101,12.2,7.78754492816924));
#243772=CARTESIAN_POINT('Ctrl Pts',(-8.26350798875715,12.2,7.78307281573856));
#243773=CARTESIAN_POINT('Ctrl Pts',(-8.2621323740092,12.2,7.77971873172021));
#243774=CARTESIAN_POINT('Ctrl Pts',(-8.2607554923575,12.2,7.77637263131356));
#243775=CARTESIAN_POINT('Ctrl Pts',(-8.25937738302632,12.2,7.77303453725297));
#243776=CARTESIAN_POINT('Ctrl Pts',(-8.25799927369513,12.2,7.76969644319238));
#243777=CARTESIAN_POINT('Ctrl Pts',(-8.25661993461692,12.2,7.76636635415884));
#243778=CARTESIAN_POINT('Ctrl Pts',(-8.25523940487552,12.2,7.76304429211217));
#243779=CARTESIAN_POINT('Ctrl Pts',(-8.25385887513412,12.2,7.7597222300655));
#243780=CARTESIAN_POINT('Ctrl Pts',(-8.25247715451779,12.2,7.75640819370163));
#243781=CARTESIAN_POINT('Ctrl Pts',(-8.25109428027653,12.2,7.75310220519564));
#243782=CARTESIAN_POINT('Ctrl Pts',(-8.24971140578403,12.2,7.74979621608907));
#243783=CARTESIAN_POINT('Ctrl Pts',(-8.24832737769956,12.2,7.74649827459311));
#243784=CARTESIAN_POINT('Ctrl Pts',(-8.24694223516477,12.2,7.74320840103276));
#243785=CARTESIAN_POINT('Ctrl Pts',(-8.24555709288163,12.2,7.73991852807006));
#243786=CARTESIAN_POINT('Ctrl Pts',(-8.24417083556518,12.2,7.7366367241736));
#243787=CARTESIAN_POINT('Ctrl Pts',(-8.24278350136549,12.2,7.73336300966823));
#243788=CARTESIAN_POINT('Ctrl Pts',(-8.2413961671658,12.2,7.73008929516287));
#243789=CARTESIAN_POINT('Ctrl Pts',(-8.24000775692131,12.2,7.72682366972671));
#243790=CARTESIAN_POINT('Ctrl Pts',(-8.23861830821548,12.2,7.72356615474699));
#243791=CARTESIAN_POINT('Ctrl Pts',(-8.23722885950965,12.2,7.72030863976728));
#243792=CARTESIAN_POINT('Ctrl Pts',(-8.23583837275708,12.2,7.71705923499986));
#243793=CARTESIAN_POINT('Ctrl Pts',(-8.23444688750966,12.2,7.71381796247788));
#243794=CARTESIAN_POINT('Ctrl Pts',(-8.23305540226224,12.2,7.7105766899559));
#243795=CARTESIAN_POINT('Ctrl Pts',(-8.23166291776788,12.2,7.70734354880179));
#243796=CARTESIAN_POINT('Ctrl Pts',(-8.23026947361026,12.2,7.70411856033491));
#243797=CARTESIAN_POINT('Ctrl Pts',(-8.22887602945264,12.2,7.70089357186803));
#243798=CARTESIAN_POINT('Ctrl Pts',(-8.2274816267701,12.2,7.6976767369173));
#243799=CARTESIAN_POINT('Ctrl Pts',(-8.22608630302924,12.2,7.69446807494942));
#243800=CARTESIAN_POINT('Ctrl Pts',(-8.22469097903491,12.2,7.69125941239863));
#243801=CARTESIAN_POINT('Ctrl Pts',(-8.223294734032,12.2,7.68805892365019));
#243802=CARTESIAN_POINT('Ctrl Pts',(-8.22189760995382,12.2,7.68486663006234));
#243803=CARTESIAN_POINT('Ctrl Pts',(-8.22050048612946,12.2,7.68167433705444));
#243804=CARTESIAN_POINT('Ctrl Pts',(-8.21910248131524,12.2,7.6784902388112));
#243805=CARTESIAN_POINT('Ctrl Pts',(-8.21770363650441,12.2,7.67531435664389));
#243806=CARTESIAN_POINT('Ctrl Pts',(-8.21583851017469,12.2,7.67107984727978));
#243807=CARTESIAN_POINT('Ctrl Pts',(-8.21397188993607,12.2,7.66685994396491));
#243808=CARTESIAN_POINT('Ctrl Pts',(-8.21210387114443,12.2,7.66265469758552));
#243809=CARTESIAN_POINT('Ctrl Pts',(-8.21070285698707,12.2,7.65950076265773));
#243810=CARTESIAN_POINT('Ctrl Pts',(-8.20930105702143,12.2,7.65635507333771));
#243811=CARTESIAN_POINT('Ctrl Pts',(-8.20789851082248,12.2,7.6532176484089));
#243812=CARTESIAN_POINT('Ctrl Pts',(-8.20649596436875,12.2,7.65008022291012));
#243813=CARTESIAN_POINT('Ctrl Pts',(-8.20509267173139,12.2,7.64695106282185));
#243814=CARTESIAN_POINT('Ctrl Pts',(-8.20368867519391,12.2,7.64383018978608));
#243815=CARTESIAN_POINT('Ctrl Pts',(-8.20228467891149,12.2,7.64070931731727));
#243816=CARTESIAN_POINT('Ctrl Pts',(-8.20087997681404,12.2,7.63759673257408));
#243817=CARTESIAN_POINT('Ctrl Pts',(-8.19947461200315,12.2,7.63449245490774));
#243818=CARTESIAN_POINT('Ctrl Pts',(-8.19806924719226,12.2,7.6313881772414));
#243819=CARTESIAN_POINT('Ctrl Pts',(-8.19666321876234,12.2,7.62829220696728));
#243820=CARTESIAN_POINT('Ctrl Pts',(-8.19525656810506,12.2,7.62520456691351));
#243821=CARTESIAN_POINT('Ctrl Pts',(-8.19384991744778,12.2,7.62211692685975));
#243822=CARTESIAN_POINT('Ctrl Pts',(-8.19244264468225,12.2,7.61903761600502));
#243823=CARTESIAN_POINT('Ctrl Pts',(-8.19103479248339,12.2,7.61596665553325));
#243824=CARTESIAN_POINT('Ctrl Pts',(-8.18962694028454,12.2,7.61289569506149));
#243825=CARTESIAN_POINT('Ctrl Pts',(-8.18821850786906,12.2,7.60983308587275));
#243826=CARTESIAN_POINT('Ctrl Pts',(-8.18680953762863,12.2,7.60677884835798));
#243827=CARTESIAN_POINT('Ctrl Pts',(-8.18540056738819,12.2,7.6037246108432));
#243828=CARTESIAN_POINT('Ctrl Pts',(-8.18399105832535,12.2,7.60067874456338));
#243829=CARTESIAN_POINT('Ctrl Pts',(-8.18258105455619,12.2,7.59764127235435));
#243830=CARTESIAN_POINT('Ctrl Pts',(-8.18117105078703,12.2,7.59460380014533));
#243831=CARTESIAN_POINT('Ctrl Pts',(-8.17976055227297,12.2,7.59157472098313));
#243832=CARTESIAN_POINT('Ctrl Pts',(-8.17834960057431,12.2,7.5885540569251));
#243833=CARTESIAN_POINT('Ctrl Pts',(-8.17646833147189,12.2,7.58452650448189));
#243834=CARTESIAN_POINT('Ctrl Pts',(-8.17458625622489,12.2,7.58051391034001));
#243835=CARTESIAN_POINT('Ctrl Pts',(-8.1727034792334,12.2,7.57651632723326));
#243836=CARTESIAN_POINT('Ctrl Pts',(-8.17082070224191,12.2,7.57251874412652));
#243837=CARTESIAN_POINT('Ctrl Pts',(-8.16893722194197,12.2,7.56853617121593));
#243838=CARTESIAN_POINT('Ctrl Pts',(-8.16705314345035,12.2,7.56456865833459));
#243839=CARTESIAN_POINT('Ctrl Pts',(-8.16516906521542,12.2,7.56060114599381));
#243840=CARTESIAN_POINT('Ctrl Pts',(-8.16328438602245,12.2,7.55664869561255));
#243841=CARTESIAN_POINT('Ctrl Pts',(-8.16139921250134,12.2,7.55271135652761));
#243842=CARTESIAN_POINT('Ctrl Pts',(-8.15951403872337,12.2,7.5487740169062));
#243843=CARTESIAN_POINT('Ctrl Pts',(-8.15762836900285,12.2,7.54485179018918));
#243844=CARTESIAN_POINT('Ctrl Pts',(-8.15574230940002,12.2,7.54094472464446));
#243845=CARTESIAN_POINT('Ctrl Pts',(-8.15385625005417,12.2,7.53703765963208));
#243846=CARTESIAN_POINT('Ctrl Pts',(-8.15196980026671,12.2,7.53314575936217));
#243847=CARTESIAN_POINT('Ctrl Pts',(-8.15008306742096,12.2,7.52926907156699));
#243848=CARTESIAN_POINT('Ctrl Pts',(-8.14819633431816,12.2,7.52539238324361));
#243849=CARTESIAN_POINT('Ctrl Pts',(-8.14630931581502,12.2,7.5215309085201));
#243850=CARTESIAN_POINT('Ctrl Pts',(-8.14442212145121,12.2,7.51768469867524));
#243851=CARTESIAN_POINT('Ctrl Pts',(-8.14253492734454,12.2,7.51383848935443));
#243852=CARTESIAN_POINT('Ctrl Pts',(-8.14064755651672,12.2,7.51000754587886));
#243853=CARTESIAN_POINT('Ctrl Pts',(-8.13876011767102,12.2,7.50619191807866));
#243854=CARTESIAN_POINT('Ctrl Pts',(-8.13687267856815,12.2,7.50237628975859));
#243855=CARTESIAN_POINT('Ctrl Pts',(-8.13498517114307,12.2,7.49857597819037));
#243856=CARTESIAN_POINT('Ctrl Pts',(-8.13309770359576,12.2,7.49479103320733));
#243857=CARTESIAN_POINT('Ctrl Pts',(-8.13121023630563,12.2,7.49100608873999));
#243858=CARTESIAN_POINT('Ctrl Pts',(-8.12932280973336,12.2,7.48723651203785));
#243859=CARTESIAN_POINT('Ctrl Pts',(-8.12743553551558,12.2,7.48348235404476));
#243860=CARTESIAN_POINT('Ctrl Pts',(-8.1250764425505,12.2,7.47878965616977));
#243861=CARTESIAN_POINT('Ctrl Pts',(-8.12271758505987,12.2,7.47412105057175));
#243862=CARTESIAN_POINT('Ctrl Pts',(-8.12035918242096,12.2,7.46947663702881));
#243863=CARTESIAN_POINT('Ctrl Pts',(-8.118472460207,12.2,7.46576110599196));
#243864=CARTESIAN_POINT('Ctrl Pts',(-8.11658602982086,12.2,7.46206105888477));
#243865=CARTESIAN_POINT('Ctrl Pts',(-8.11470000282921,12.2,7.45837654540719));
#243866=CARTESIAN_POINT('Ctrl Pts',(-8.11281397609452,12.2,7.45469203243164));
#243867=CARTESIAN_POINT('Ctrl Pts',(-8.11092835204705,12.2,7.45102305610424));
#243868=CARTESIAN_POINT('Ctrl Pts',(-8.10904324777359,12.2,7.44736966533013));
#243869=CARTESIAN_POINT('Ctrl Pts',(-8.10668686723912,12.2,7.44280292648915));
#243870=CARTESIAN_POINT('Ctrl Pts',(-8.10433129348742,12.2,7.43826054076349));
#243871=CARTESIAN_POINT('Ctrl Pts',(-8.10197675661237,12.2,7.43374261055386));
#243872=CARTESIAN_POINT('Ctrl Pts',(-8.10009312700967,12.2,7.43012826618918));
#243873=CARTESIAN_POINT('Ctrl Pts',(-8.09821015917093,12.2,7.42652957264305));
#243874=CARTESIAN_POINT('Ctrl Pts',(-8.0963279708462,12.2,7.42294658294883));
#243875=CARTESIAN_POINT('Ctrl Pts',(-8.0944457827779,12.2,7.41936359374279));
#243876=CARTESIAN_POINT('Ctrl Pts',(-8.09256437305387,12.2,7.41579630768909));
#243877=CARTESIAN_POINT('Ctrl Pts',(-8.09068386054085,12.2,7.41224477658894));
#243878=CARTESIAN_POINT('Ctrl Pts',(-8.08880334777161,12.2,7.4086932450049));
#243879=CARTESIAN_POINT('Ctrl Pts',(-8.08692373280415,12.2,7.40515746903032));
#243880=CARTESIAN_POINT('Ctrl Pts',(-8.08504513324877,12.2,7.40163749998919));
#243881=CARTESIAN_POINT('Ctrl Pts',(-8.08269688393254,12.2,7.39723753892757));
#243882=CARTESIAN_POINT('Ctrl Pts',(-8.08035022280215,12.2,7.39286227676422));
#243883=CARTESIAN_POINT('Ctrl Pts',(-8.07800538433004,12.2,7.38851181572388));
#243884=CARTESIAN_POINT('Ctrl Pts',(-8.0761295137057,12.2,7.38503144717613));
#243885=CARTESIAN_POINT('Ctrl Pts',(-8.07425481035335,12.2,7.38156695150017));
#243886=CARTESIAN_POINT('Ctrl Pts',(-8.07238139583969,12.2,7.37811837978044));
#243887=CARTESIAN_POINT('Ctrl Pts',(-8.07050798107078,12.2,7.37466980759083));
#243888=CARTESIAN_POINT('Ctrl Pts',(-8.06863585405367,12.2,7.37123716097705));
#243889=CARTESIAN_POINT('Ctrl Pts',(-8.06676514049878,12.2,7.3678204919976));
#243890=CARTESIAN_POINT('Ctrl Pts',(-8.06489442719877,12.2,7.36440382348368));
#243891=CARTESIAN_POINT('Ctrl Pts',(-8.06302512532789,12.2,7.36100313198659));
#243892=CARTESIAN_POINT('Ctrl Pts',(-8.06115736131376,12.2,7.35761847076166));
#243893=CARTESIAN_POINT('Ctrl Pts',(-8.05928959704514,12.2,7.35423380907556));
#243894=CARTESIAN_POINT('Ctrl Pts',(-8.05742336892112,12.2,7.35086517720208));
#243895=CARTESIAN_POINT('Ctrl Pts',(-8.05555880354172,12.2,7.34751262874158));
#243896=CARTESIAN_POINT('Ctrl Pts',(-8.05369423816231,12.2,7.34416008028108));
#243897=CARTESIAN_POINT('Ctrl Pts',(-8.05183133539423,12.2,7.34082361326415));
#243898=CARTESIAN_POINT('Ctrl Pts',(-8.04997022323743,12.2,7.33750328297372));
#243899=CARTESIAN_POINT('Ctrl Pts',(-8.0481091113342,12.2,7.3341829531357));
#243900=CARTESIAN_POINT('Ctrl Pts',(-8.04624978891069,12.2,7.33087875821226));
#243901=CARTESIAN_POINT('Ctrl Pts',(-8.04439238577632,12.2,7.32759075174384));
#243902=CARTESIAN_POINT('Ctrl Pts',(-8.04253498238886,12.2,7.32430274482742));
#243903=CARTESIAN_POINT('Ctrl Pts',(-8.04067949797838,12.2,7.32103092732398));
#243904=CARTESIAN_POINT('Ctrl Pts',(-8.03882606248868,12.2,7.31777535042598));
#243905=CARTESIAN_POINT('Ctrl Pts',(-8.03697262725152,12.2,7.31451977397156));
#243906=CARTESIAN_POINT('Ctrl Pts',(-8.03512123971688,12.2,7.31128043907337));
#243907=CARTESIAN_POINT('Ctrl Pts',(-8.03327203386791,12.2,7.30805739978022));
#243908=CARTESIAN_POINT('Ctrl Pts',(-8.03142282776697,12.2,7.30483436004793));
#243909=CARTESIAN_POINT('Ctrl Pts',(-8.02957580224709,12.2,7.30162761399944));
#243910=CARTESIAN_POINT('Ctrl Pts',(-8.02773108949905,12.2,7.29843721627873));
#243911=CARTESIAN_POINT('Ctrl Pts',(-8.02588637700236,12.2,7.29524681899272));
#243912=CARTESIAN_POINT('Ctrl Pts',(-8.02404397811968,12.2,7.29207277041229));
#243913=CARTESIAN_POINT('Ctrl Pts',(-8.02220402765882,12.2,7.28891512322488));
#243914=CARTESIAN_POINT('Ctrl Pts',(-8.02036407694725,12.2,7.28575747560723));
#243915=CARTESIAN_POINT('Ctrl Pts',(-8.01852657364991,12.2,7.28261623021387));
#243916=CARTESIAN_POINT('Ctrl Pts',(-8.0166916548834,12.2,7.2794914387113));
#243917=CARTESIAN_POINT('Ctrl Pts',(-8.01485673636691,12.2,7.27636664763448));
#243918=CARTESIAN_POINT('Ctrl Pts',(-8.0130244005104,12.2,7.27325831326569));
#243919=CARTESIAN_POINT('Ctrl Pts',(-8.01119478729054,12.2,7.27016648664032));
#243920=CARTESIAN_POINT('Ctrl Pts',(-8.0093651738214,12.2,7.26707465959368));
#243921=CARTESIAN_POINT('Ctrl Pts',(-8.0075382814224,12.2,7.26399934282954));
#243922=CARTESIAN_POINT('Ctrl Pts',(-8.00571425010096,12.2,7.26094058727503));
#243923=CARTESIAN_POINT('Ctrl Pts',(-8.00389021902804,12.2,7.25788183213727));
#243924=CARTESIAN_POINT('Ctrl Pts',(-8.00206904825732,12.2,7.25483964111564));
#243925=CARTESIAN_POINT('Ctrl Pts',(-8.00025087857232,12.2,7.25181406602794));
#243926=CARTESIAN_POINT('Ctrl Pts',(-7.99843270863958,12.2,7.248788490528));
#243927=CARTESIAN_POINT('Ctrl Pts',(-7.99661754134745,12.2,7.24577953161895));
#243928=CARTESIAN_POINT('Ctrl Pts',(-7.99480551674048,12.2,7.24278724399789));
#243929=CARTESIAN_POINT('Ctrl Pts',(-7.99299349238039,12.2,7.23979495678451));
#243930=CARTESIAN_POINT('Ctrl Pts',(-7.99118461129244,12.2,7.23681934085188));
#243931=CARTESIAN_POINT('Ctrl Pts',(-7.9893790183286,12.2,7.23386045025871));
#243932=CARTESIAN_POINT('Ctrl Pts',(-7.98757342511873,12.2,7.23090155926239));
#243933=CARTESIAN_POINT('Ctrl Pts',(-7.98577112047308,12.2,7.22795939382046));
#243934=CARTESIAN_POINT('Ctrl Pts',(-7.98397224854171,12.2,7.2250340082166));
#243935=CARTESIAN_POINT('Ctrl Pts',(-7.98217337661035,12.2,7.22210862261273));
#243936=CARTESIAN_POINT('Ctrl Pts',(-7.98037793865436,12.2,7.21920001571076));
#243937=CARTESIAN_POINT('Ctrl Pts',(-7.97858608022374,12.2,7.21630824477712));
#243938=CARTESIAN_POINT('Ctrl Pts',(-7.97679422203727,12.2,7.21341647423748));
#243939=CARTESIAN_POINT('Ctrl Pts',(-7.97500594488848,12.2,7.2105415382118));
#243940=CARTESIAN_POINT('Ctrl Pts',(-7.97322139852626,12.2,7.20768349104354));
#243941=CARTESIAN_POINT('Ctrl Pts',(-7.9714368519209,12.2,7.20482544348586));
#243942=CARTESIAN_POINT('Ctrl Pts',(-7.96965603490598,12.2,7.20198428469316));
#243943=CARTESIAN_POINT('Ctrl Pts',(-7.96787909847618,12.2,7.19916007226317));
#243944=CARTESIAN_POINT('Ctrl Pts',(-7.96565792805999,12.2,7.19562980691809));
#243945=CARTESIAN_POINT('Ctrl Pts',(-7.96344282182177,12.2,7.19212601567076));
#243946=CARTESIAN_POINT('Ctrl Pts',(-7.96123407946114,12.2,7.18864880810345));
#243947=CARTESIAN_POINT('Ctrl Pts',(-7.95902533734128,12.2,7.18517160091515));
#243948=CARTESIAN_POINT('Ctrl Pts',(-7.9568229566151,12.2,7.18172097653783));
#243949=CARTESIAN_POINT('Ctrl Pts',(-7.95462724227057,12.2,7.17829704517277));
#243950=CARTESIAN_POINT('Ctrl Pts',(-7.95243152768672,12.2,7.17487311343451));
#243951=CARTESIAN_POINT('Ctrl Pts',(-7.95024247975272,12.2,7.17147587319856));
#243952=CARTESIAN_POINT('Ctrl Pts',(-7.94806040600212,12.2,7.16810543389078));
#243953=CARTESIAN_POINT('Ctrl Pts',(-7.94587833225154,12.2,7.164734994583));
#243954=CARTESIAN_POINT('Ctrl Pts',(-7.94370323307863,12.2,7.1613913551804));
#243955=CARTESIAN_POINT('Ctrl Pts',(-7.94153542175859,12.2,7.15807462594209));
#243956=CARTESIAN_POINT('Ctrl Pts',(-7.93806692369378,12.2,7.15276785923307));
#243957=CARTESIAN_POINT('Ctrl Pts',(-7.93461707823475,12.2,7.14752998137508));
#243958=CARTESIAN_POINT('Ctrl Pts',(-7.93118719628043,12.2,7.14236144266412));
#243959=CARTESIAN_POINT('Ctrl Pts',(-7.92904352002977,12.2,7.13913110592575));
#243960=CARTESIAN_POINT('Ctrl Pts',(-7.92690764254568,12.2,7.13592785524537));
#243961=CARTESIAN_POINT('Ctrl Pts',(-7.92477988900335,12.2,7.13275180017369));
#243962=CARTESIAN_POINT('Ctrl Pts',(-7.922652135461,12.2,7.129575745102));
#243963=CARTESIAN_POINT('Ctrl Pts',(-7.92053250761231,12.2,7.12642688654244));
#243964=CARTESIAN_POINT('Ctrl Pts',(-7.91842133472847,12.2,7.12330533541238));
#243965=CARTESIAN_POINT('Ctrl Pts',(-7.91631016184464,12.2,7.12018378428232));
#243966=CARTESIAN_POINT('Ctrl Pts',(-7.91420744539304,12.2,7.11708953951319));
#243967=CARTESIAN_POINT('Ctrl Pts',(-7.91211352108703,12.2,7.11402271444232));
#243968=CARTESIAN_POINT('Ctrl Pts',(-7.91001959678102,12.2,7.11095588937146));
#243969=CARTESIAN_POINT('Ctrl Pts',(-7.90793446711411,12.2,7.10791648394849));
#243970=CARTESIAN_POINT('Ctrl Pts',(-7.90585847037751,12.2,7.10490460894705));
#243971=CARTESIAN_POINT('Ctrl Pts',(-7.90378247364092,12.2,7.1018927339456));
#243972=CARTESIAN_POINT('Ctrl Pts',(-7.90171561457166,12.2,7.09890838983727));
#243973=CARTESIAN_POINT('Ctrl Pts',(-7.89965823699282,12.2,7.0959516905182));
#243974=CARTESIAN_POINT('Ctrl Pts',(-7.897600859414,12.2,7.09299499119913));
#243975=CARTESIAN_POINT('Ctrl Pts',(-7.89555296451672,12.2,7.09006593653882));
#243976=CARTESIAN_POINT('Ctrl Pts',(-7.89351490847503,12.2,7.08716463827492));
#243977=CARTESIAN_POINT('Ctrl Pts',(-7.89147685243335,12.2,7.08426334001101));
#243978=CARTESIAN_POINT('Ctrl Pts',(-7.88944863350252,12.2,7.08138980059456));
#243979=CARTESIAN_POINT('Ctrl Pts',(-7.88743061175726,12.2,7.07854413224837));
#243980=CARTESIAN_POINT('Ctrl Pts',(-7.88541259001201,12.2,7.07569846390218));
#243981=CARTESIAN_POINT('Ctrl Pts',(-7.88340476471337,12.2,7.07288066627728));
#243982=CARTESIAN_POINT('Ctrl Pts',(-7.88140750464447,12.2,7.0700908568343));
#243983=CARTESIAN_POINT('Ctrl Pts',(-7.87941024457558,12.2,7.06730104739132));
#243984=CARTESIAN_POINT('Ctrl Pts',(-7.87742354804253,12.2,7.06453922371985));
#243985=CARTESIAN_POINT('Ctrl Pts',(-7.87544778811255,12.2,7.06180550205463));
#243986=CARTESIAN_POINT('Ctrl Pts',(-7.87347202818255,12.2,7.05907178038943));
#243987=CARTESIAN_POINT('Ctrl Pts',(-7.8715072057701,12.2,7.05636616173211));
#243988=CARTESIAN_POINT('Ctrl Pts',(-7.86955369754829,12.2,7.05368876069754));
#243989=CARTESIAN_POINT('Ctrl Pts',(-7.8672094877673,12.2,7.05047587957279));
#243990=CARTESIAN_POINT('Ctrl Pts',(-7.86488157480772,12.2,7.04730363264447));
#243991=CARTESIAN_POINT('Ctrl Pts',(-7.86257062397502,12.2,7.04417222350824));
#243992=CARTESIAN_POINT('Ctrl Pts',(-7.86025967314232,12.2,7.04104081437201));
#243993=CARTESIAN_POINT('Ctrl Pts',(-7.85796568526065,12.2,7.03795024112229));
#243994=CARTESIAN_POINT('Ctrl Pts',(-7.85568934347861,12.2,7.03490070907836));
#243995=CARTESIAN_POINT('Ctrl Pts',(-7.85341300148981,12.2,7.03185117675743));
#243996=CARTESIAN_POINT('Ctrl Pts',(-7.85115430702667,12.2,7.02884268435205));
#243997=CARTESIAN_POINT('Ctrl Pts',(-7.84891395623916,12.2,7.02587543919316));
#243998=CARTESIAN_POINT('Ctrl Pts',(-7.84667360565515,12.2,7.02290819430378));
#243999=CARTESIAN_POINT('Ctrl Pts',(-7.84445160067892,12.2,7.01998219575677));
#244000=CARTESIAN_POINT('Ctrl Pts',(-7.84224865324902,12.2,7.01709765168194));
#244001=CARTESIAN_POINT('Ctrl Pts',(-7.84004570581913,12.2,7.0142131076071));
#244002=CARTESIAN_POINT('Ctrl Pts',(-7.83786181919861,12.2,7.01137001650279));
#244003=CARTESIAN_POINT('Ctrl Pts',(-7.83569771985971,12.2,7.00856858960276));
#244004=CARTESIAN_POINT('Ctrl Pts',(-7.83353362032424,12.2,7.00576716244827));
#244005=CARTESIAN_POINT('Ctrl Pts',(-7.83138931029956,12.2,7.00300739883229));
#244006=CARTESIAN_POINT('Ctrl Pts',(-7.82926553851853,12.2,7.000289509687));
#244007=CARTESIAN_POINT('Ctrl Pts',(-7.82714176693041,12.2,6.9975716207886));
#244008=CARTESIAN_POINT('Ctrl Pts',(-7.82503852973505,12.2,6.99489560841732));
#244009=CARTESIAN_POINT('Ctrl Pts',(-7.82295659539498,12.2,6.99226168259821));
#244010=CARTESIAN_POINT('Ctrl Pts',(-7.82087466105491,12.2,6.98962775677911));
#244011=CARTESIAN_POINT('Ctrl Pts',(-7.81881402959643,12.2,6.98703591994823));
#244012=CARTESIAN_POINT('Ctrl Pts',(-7.81677548158621,12.2,6.98448638787237));
#244013=CARTESIAN_POINT('Ctrl Pts',(-7.81473693339083,12.2,6.98193685556494));
#244014=CARTESIAN_POINT('Ctrl Pts',(-7.81272047252316,12.2,6.97942962570439));
#244015=CARTESIAN_POINT('Ctrl Pts',(-7.81072689908272,12.2,6.9769649194896));
#244016=CARTESIAN_POINT('Ctrl Pts',(-7.80873332582335,12.2,6.97450021349869));
#244017=CARTESIAN_POINT('Ctrl Pts',(-7.80676263884723,12.2,6.97207803038208));
#244018=CARTESIAN_POINT('Ctrl Pts',(-7.80481566366901,12.2,6.96969858863709));
#244019=CARTESIAN_POINT('Ctrl Pts',(-7.80286868849079,12.2,6.96731914689208));
#244020=CARTESIAN_POINT('Ctrl Pts',(-7.800945421744,12.2,6.96498244829361));
#244021=CARTESIAN_POINT('Ctrl Pts',(-7.79904671156193,12.2,6.9626887163751));
#244022=CARTESIAN_POINT('Ctrl Pts',(-7.79714800137986,12.2,6.96039498445658));
#244023=CARTESIAN_POINT('Ctrl Pts',(-7.79527384169444,12.2,6.95814421811329));
#244024=CARTESIAN_POINT('Ctrl Pts',(-7.79342510367653,12.2,6.95593664319055));
#244025=CARTESIAN_POINT('Ctrl Pts',(-7.79157636549069,12.2,6.95372906806728));
#244026=CARTESIAN_POINT('Ctrl Pts',(-7.78975304394064,12.2,6.95156468542317));
#244027=CARTESIAN_POINT('Ctrl Pts',(-7.78795602992718,12.2,6.9494437215595));
#244028=CARTESIAN_POINT('Ctrl Pts',(-7.78615901607696,12.2,6.94732275788846));
#244029=CARTESIAN_POINT('Ctrl Pts',(-7.78438830853713,12.2,6.9452452166113));
#244030=CARTESIAN_POINT('Ctrl Pts',(-7.78264481700914,12.2,6.94321132675917));
#244031=CARTESIAN_POINT('Ctrl Pts',(-7.78090132548115,12.2,6.94117743690704));
#244032=CARTESIAN_POINT('Ctrl Pts',(-7.77918505249957,12.2,6.93918720018598));
#244033=CARTESIAN_POINT('Ctrl Pts',(-7.77749693197569,12.2,6.93724084850374));
#244034=CARTESIAN_POINT('Ctrl Pts',(-7.77580881129846,12.2,6.93529449664471));
#244035=CARTESIAN_POINT('Ctrl Pts',(-7.77414884352764,12.2,6.93339203265347));
#244036=CARTESIAN_POINT('Ctrl Pts',(-7.77251798985898,12.2,6.93153369454525));
#244037=CARTESIAN_POINT('Ctrl Pts',(-7.77088713633846,12.2,6.92967535660584));
#244038=CARTESIAN_POINT('Ctrl Pts',(-7.7692853965429,12.2,6.92786114359393));
#244039=CARTESIAN_POINT('Ctrl Pts',(-7.76771376026667,12.2,6.92609129774157));
#244040=CARTESIAN_POINT('Ctrl Pts',(-7.76614212399044,12.2,6.92432145188921));
#244041=CARTESIAN_POINT('Ctrl Pts',(-7.76460059048524,12.2,6.92259597378809));
#244042=CARTESIAN_POINT('Ctrl Pts',(-7.76309017712953,12.2,6.92091510792929));
#244043=CARTESIAN_POINT('Ctrl Pts',(-7.76157976363662,12.2,6.91923424191781));
#244044=CARTESIAN_POINT('Ctrl Pts',(-7.76010047016895,12.2,6.91759798963515));
#244045=CARTESIAN_POINT('Ctrl Pts',(-7.75865334209226,12.2,6.91600659963478));
#244046=CARTESIAN_POINT('Ctrl Pts',(-7.75720621414701,12.2,6.91441520977898));
#244047=CARTESIAN_POINT('Ctrl Pts',(-7.75579125177202,12.2,6.91286868171804));
#244048=CARTESIAN_POINT('Ctrl Pts',(-7.75440953381604,12.2,6.9113672717659));
#244049=CARTESIAN_POINT('Ctrl Pts',(-7.75302781586007,12.2,6.90986586181377));
#244050=CARTESIAN_POINT('Ctrl Pts',(-7.75167934028384,12.2,6.90840956728605));
#244051=CARTESIAN_POINT('Ctrl Pts',(-7.75036521958009,12.2,6.90699864858533));
#244052=CARTESIAN_POINT('Ctrl Pts',(-7.74883838549972,12.2,6.90535934806235));
#244053=CARTESIAN_POINT('Ctrl Pts',(-7.74735792437416,12.2,6.90378129525211));
#244054=CARTESIAN_POINT('Ctrl Pts',(-7.74592563800006,12.2,6.90226491999999));
#244055=CARTESIAN_POINT('Ctrl Pts',(-7.74592563800006,15.2,6.90226491999999));
#244056=CARTESIAN_POINT('Ctrl Pts',(-7.74715246678865,15.2,6.90356377534571));
#244057=CARTESIAN_POINT('Ctrl Pts',(-7.74841464217223,15.2,6.90490788340064));
#244058=CARTESIAN_POINT('Ctrl Pts',(-7.74971102733301,15.2,6.90629697133944));
#244059=CARTESIAN_POINT('Ctrl Pts',(-7.75101366431833,15.2,6.90769275816243));
#244060=CARTESIAN_POINT('Ctrl Pts',(-7.75235084435424,15.2,6.90913396283592));
#244061=CARTESIAN_POINT('Ctrl Pts',(-7.75372145033267,15.2,6.91062032766048));
#244062=CARTESIAN_POINT('Ctrl Pts',(-7.75532049045411,15.2,6.91235441975326));
#244063=CARTESIAN_POINT('Ctrl Pts',(-7.75696502619996,15.2,6.91414997818454));
#244064=CARTESIAN_POINT('Ctrl Pts',(-7.75865334209227,15.2,6.91600659963479));
#244065=CARTESIAN_POINT('Ctrl Pts',(-7.76010047016897,15.2,6.91759798963517));
#244066=CARTESIAN_POINT('Ctrl Pts',(-7.7615797636366,15.2,6.91923424191777));
#244067=CARTESIAN_POINT('Ctrl Pts',(-7.76309017712953,15.2,6.92091510792929));
#244068=CARTESIAN_POINT('Ctrl Pts',(-7.76460059048527,15.2,6.92259597378812));
#244069=CARTESIAN_POINT('Ctrl Pts',(-7.76614212399043,15.2,6.9243214518892));
#244070=CARTESIAN_POINT('Ctrl Pts',(-7.76771376026667,15.2,6.92609129774157));
#244071=CARTESIAN_POINT('Ctrl Pts',(-7.76928539654291,15.2,6.92786114359394));
#244072=CARTESIAN_POINT('Ctrl Pts',(-7.77088713633845,15.2,6.92967535660582));
#244073=CARTESIAN_POINT('Ctrl Pts',(-7.77251798985898,15.2,6.93153369454525));
#244074=CARTESIAN_POINT('Ctrl Pts',(-7.77414884352765,15.2,6.93339203265348));
#244075=CARTESIAN_POINT('Ctrl Pts',(-7.77580881129845,15.2,6.93529449664469));
#244076=CARTESIAN_POINT('Ctrl Pts',(-7.77749693197568,15.2,6.93724084850373));
#244077=CARTESIAN_POINT('Ctrl Pts',(-7.77918505249957,15.2,6.93918720018598));
#244078=CARTESIAN_POINT('Ctrl Pts',(-7.78090132548116,15.2,6.94117743690705));
#244079=CARTESIAN_POINT('Ctrl Pts',(-7.78264481700914,15.2,6.94321132675917));
#244080=CARTESIAN_POINT('Ctrl Pts',(-7.78438830853712,15.2,6.94524521661129));
#244081=CARTESIAN_POINT('Ctrl Pts',(-7.78615901607696,15.2,6.94732275788845));
#244082=CARTESIAN_POINT('Ctrl Pts',(-7.78795602992718,15.2,6.9494437215595));
#244083=CARTESIAN_POINT('Ctrl Pts',(-7.78975304394065,15.2,6.95156468542318));
#244084=CARTESIAN_POINT('Ctrl Pts',(-7.79157636549068,15.2,6.95372906806727));
#244085=CARTESIAN_POINT('Ctrl Pts',(-7.79342510367653,15.2,6.95593664319054));
#244086=CARTESIAN_POINT('Ctrl Pts',(-7.79527384169445,15.2,6.9581442181133));
#244087=CARTESIAN_POINT('Ctrl Pts',(-7.79714800137984,15.2,6.96039498445656));
#244088=CARTESIAN_POINT('Ctrl Pts',(-7.79904671156193,15.2,6.9626887163751));
#244089=CARTESIAN_POINT('Ctrl Pts',(-7.80094542174402,15.2,6.96498244829363));
#244090=CARTESIAN_POINT('Ctrl Pts',(-7.80286868849078,15.2,6.96731914689208));
#244091=CARTESIAN_POINT('Ctrl Pts',(-7.804815663669,15.2,6.96969858863707));
#244092=CARTESIAN_POINT('Ctrl Pts',(-7.80676263884721,15.2,6.97207803038206));
#244093=CARTESIAN_POINT('Ctrl Pts',(-7.80873332582338,15.2,6.97450021349873));
#244094=CARTESIAN_POINT('Ctrl Pts',(-7.81072689908272,15.2,6.9769649194896));
#244095=CARTESIAN_POINT('Ctrl Pts',(-7.81272047252313,15.2,6.97942962570435));
#244096=CARTESIAN_POINT('Ctrl Pts',(-7.81473693339078,15.2,6.98193685556488));
#244097=CARTESIAN_POINT('Ctrl Pts',(-7.81677548158621,15.2,6.98448638787237));
#244098=CARTESIAN_POINT('Ctrl Pts',(-7.81881402959647,15.2,6.98703591994829));
#244099=CARTESIAN_POINT('Ctrl Pts',(-7.82087466105487,15.2,6.98962775677906));
#244100=CARTESIAN_POINT('Ctrl Pts',(-7.82295659539498,15.2,6.99226168259821));
#244101=CARTESIAN_POINT('Ctrl Pts',(-7.82503852973509,15.2,6.99489560841737));
#244102=CARTESIAN_POINT('Ctrl Pts',(-7.82714176693043,15.2,6.99757162078863));
#244103=CARTESIAN_POINT('Ctrl Pts',(-7.82926553851854,15.2,7.00028950968701));
#244104=CARTESIAN_POINT('Ctrl Pts',(-7.83138931029955,15.2,7.00300739883227));
#244105=CARTESIAN_POINT('Ctrl Pts',(-7.83353362032421,15.2,7.00576716244823));
#244106=CARTESIAN_POINT('Ctrl Pts',(-7.83569771985971,15.2,7.00856858960276));
#244107=CARTESIAN_POINT('Ctrl Pts',(-7.83786181919864,15.2,7.01137001650283));
#244108=CARTESIAN_POINT('Ctrl Pts',(-7.84004570581912,15.2,7.0142131076071));
#244109=CARTESIAN_POINT('Ctrl Pts',(-7.84224865324903,15.2,7.01709765168194));
#244110=CARTESIAN_POINT('Ctrl Pts',(-7.84445160067893,15.2,7.01998219575679));
#244111=CARTESIAN_POINT('Ctrl Pts',(-7.84667360565514,15.2,7.02290819430377));
#244112=CARTESIAN_POINT('Ctrl Pts',(-7.84891395623916,15.2,7.02587543919316));
#244113=CARTESIAN_POINT('Ctrl Pts',(-7.85115430702668,15.2,7.02884268435206));
#244114=CARTESIAN_POINT('Ctrl Pts',(-7.8534130014898,15.2,7.03185117675742));
#244115=CARTESIAN_POINT('Ctrl Pts',(-7.85568934347861,15.2,7.03490070907836));
#244116=CARTESIAN_POINT('Ctrl Pts',(-7.85796568526066,15.2,7.0379502411223));
#244117=CARTESIAN_POINT('Ctrl Pts',(-7.86025967314234,15.2,7.04104081437204));
#244118=CARTESIAN_POINT('Ctrl Pts',(-7.86257062397502,15.2,7.04417222350824));
#244119=CARTESIAN_POINT('Ctrl Pts',(-7.8648815748077,15.2,7.04730363264444));
#244120=CARTESIAN_POINT('Ctrl Pts',(-7.86720948776729,15.2,7.05047587957277));
#244121=CARTESIAN_POINT('Ctrl Pts',(-7.86955369754829,15.2,7.05368876069754));
#244122=CARTESIAN_POINT('Ctrl Pts',(-7.87150720577011,15.2,7.05636616173213));
#244123=CARTESIAN_POINT('Ctrl Pts',(-7.87347202818256,15.2,7.05907178038944));
#244124=CARTESIAN_POINT('Ctrl Pts',(-7.87544778811255,15.2,7.06180550205465));
#244125=CARTESIAN_POINT('Ctrl Pts',(-7.87742354804254,15.2,7.06453922371986));
#244126=CARTESIAN_POINT('Ctrl Pts',(-7.87941024457559,15.2,7.06730104739134));
#244127=CARTESIAN_POINT('Ctrl Pts',(-7.88140750464447,15.2,7.07009085683429));
#244128=CARTESIAN_POINT('Ctrl Pts',(-7.88420366878443,15.2,7.07399659011525));
#244129=CARTESIAN_POINT('Ctrl Pts',(-7.88702053880993,15.2,7.0779571785731));
#244130=CARTESIAN_POINT('Ctrl Pts',(-7.8898571093826,15.2,7.08197230513765));
#244131=CARTESIAN_POINT('Ctrl Pts',(-7.89228845546155,15.2,7.08541384201434));
#244132=CARTESIAN_POINT('Ctrl Pts',(-7.89473427728936,15.2,7.08889544834617));
#244133=CARTESIAN_POINT('Ctrl Pts',(-7.89719395836603,15.2,7.09241692729982));
#244134=CARTESIAN_POINT('Ctrl Pts',(-7.89924369267107,15.2,7.09535149320116));
#244135=CARTESIAN_POINT('Ctrl Pts',(-7.90130305046732,15.2,7.09831374891258));
#244136=CARTESIAN_POINT('Ctrl Pts',(-7.90337168228224,15.2,7.10130358073163));
#244137=CARTESIAN_POINT('Ctrl Pts',(-7.90585404036996,15.2,7.10489137878413));
#244138=CARTESIAN_POINT('Ctrl Pts',(-7.90834975301863,15.2,7.10851888697784));
#244139=CARTESIAN_POINT('Ctrl Pts',(-7.91085822425995,15.2,7.11218591009188));
#244140=CARTESIAN_POINT('Ctrl Pts',(-7.91336669572912,15.2,7.11585293353903));
#244141=CARTESIAN_POINT('Ctrl Pts',(-7.91588792712977,15.2,7.11955947385212));
#244142=CARTESIAN_POINT('Ctrl Pts',(-7.91842133472847,15.2,7.12330533541238));
#244143=CARTESIAN_POINT('Ctrl Pts',(-7.92137697658178,15.2,7.12767550672231));
#244144=CARTESIAN_POINT('Ctrl Pts',(-7.9243491910579,15.2,7.13209920094139));
#244145=CARTESIAN_POINT('Ctrl Pts',(-7.92733707145422,15.2,7.13657611258999));
#244146=CARTESIAN_POINT('Ctrl Pts',(-7.93032495208318,15.2,7.14105302458716));
#244147=CARTESIAN_POINT('Ctrl Pts',(-7.93332850016596,15.2,7.14558315465606));
#244148=CARTESIAN_POINT('Ctrl Pts',(-7.9363468282822,15.2,7.1501661985398));
#244149=CARTESIAN_POINT('Ctrl Pts',(-7.93850277690308,15.2,7.15343980126294));
#244150=CARTESIAN_POINT('Ctrl Pts',(-7.94066626605559,15.2,7.15674040271658));
#244151=CARTESIAN_POINT('Ctrl Pts',(-7.94283698050004,15.2,7.16006789125824));
#244152=CARTESIAN_POINT('Ctrl Pts',(-7.94544183773873,15.2,7.16406087736317));
#244153=CARTESIAN_POINT('Ctrl Pts',(-7.94805709806829,15.2,7.16809258302344));
#244154=CARTESIAN_POINT('Ctrl Pts',(-7.95068222172223,15.2,7.1721628180396));
#244155=CARTESIAN_POINT('Ctrl Pts',(-7.95286982484666,15.2,7.1755546806763));
#244156=CARTESIAN_POINT('Ctrl Pts',(-7.95506428048505,15.2,7.17897329923534));
#244157=CARTESIAN_POINT('Ctrl Pts',(-7.95726527871956,15.2,7.1824185678084));
#244158=CARTESIAN_POINT('Ctrl Pts',(-7.95946627695407,15.2,7.18586383638145));
#244159=CARTESIAN_POINT('Ctrl Pts',(-7.9616738201834,15.2,7.18933575325045));
#244160=CARTESIAN_POINT('Ctrl Pts',(-7.96388760636363,15.2,7.19283421005461));
#244161=CARTESIAN_POINT('Ctrl Pts',(-7.96654414992467,15.2,7.1970323584484));
#244162=CARTESIAN_POINT('Ctrl Pts',(-7.96920968180351,15.2,7.20126872410527));
#244163=CARTESIAN_POINT('Ctrl Pts',(-7.97188369053318,15.2,7.20554312342417));
#244164=CARTESIAN_POINT('Ctrl Pts',(-7.97366636277674,15.2,7.20839272258186));
#244165=CARTESIAN_POINT('Ctrl Pts',(-7.97545280215928,15.2,7.21125922460953));
#244166=CARTESIAN_POINT('Ctrl Pts',(-7.97724286046549,15.2,7.21414257449796));
#244167=CARTESIAN_POINT('Ctrl Pts',(-7.97903291901561,15.2,7.21702592477925));
#244168=CARTESIAN_POINT('Ctrl Pts',(-7.9808265943456,15.2,7.21992612363562));
#244169=CARTESIAN_POINT('Ctrl Pts',(-7.98262374077721,15.2,7.22284311651852));
#244170=CARTESIAN_POINT('Ctrl Pts',(-7.98442088696397,15.2,7.22576010900398));
#244171=CARTESIAN_POINT('Ctrl Pts',(-7.98622150212531,15.2,7.22869389298174));
#244172=CARTESIAN_POINT('Ctrl Pts',(-7.98802544181093,15.2,7.2316444180172));
#244173=CARTESIAN_POINT('Ctrl Pts',(-7.98982938174235,15.2,7.23459494345466));
#244174=CARTESIAN_POINT('Ctrl Pts',(-7.99163664624837,15.2,7.23756220719483));
#244175=CARTESIAN_POINT('Ctrl Pts',(-7.9934470902711,15.2,7.24054615567467));
#244176=CARTESIAN_POINT('Ctrl Pts',(-7.99525753404717,15.2,7.24353010374794));
#244177=CARTESIAN_POINT('Ctrl Pts',(-7.99707115614192,15.2,7.24653073700669));
#244178=CARTESIAN_POINT('Ctrl Pts',(-7.99888781582656,15.2,7.2495480002034));
#244179=CARTESIAN_POINT('Ctrl Pts',(-8.00115864061799,15.2,7.25331957950761));
#244180=CARTESIAN_POINT('Ctrl Pts',(-8.00343421107341,15.2,7.25711714304025));
#244181=CARTESIAN_POINT('Ctrl Pts',(-8.00571425010096,15.2,7.26094058727502));
#244182=CARTESIAN_POINT('Ctrl Pts',(-8.0075382814224,15.2,7.26399934282954));
#244183=CARTESIAN_POINT('Ctrl Pts',(-8.00936517382141,15.2,7.2670746595937));
#244184=CARTESIAN_POINT('Ctrl Pts',(-8.01119478729055,15.2,7.27016648664033));
#244185=CARTESIAN_POINT('Ctrl Pts',(-8.0130244005104,15.2,7.27325831326569));
#244186=CARTESIAN_POINT('Ctrl Pts',(-8.01485673636691,15.2,7.27636664763449));
#244187=CARTESIAN_POINT('Ctrl Pts',(-8.0166916548834,15.2,7.27949143871129));
#244188=CARTESIAN_POINT('Ctrl Pts',(-8.01852657364989,15.2,7.28261623021384));
#244189=CARTESIAN_POINT('Ctrl Pts',(-8.02036407694727,15.2,7.28575747560727));
#244190=CARTESIAN_POINT('Ctrl Pts',(-8.02220402765882,15.2,7.28891512322488));
#244191=CARTESIAN_POINT('Ctrl Pts',(-8.02404397811966,15.2,7.29207277041225));
#244192=CARTESIAN_POINT('Ctrl Pts',(-8.02588637700234,15.2,7.2952468189927));
#244193=CARTESIAN_POINT('Ctrl Pts',(-8.02773108949904,15.2,7.29843721627872));
#244194=CARTESIAN_POINT('Ctrl Pts',(-8.02957580224709,15.2,7.30162761399944));
#244195=CARTESIAN_POINT('Ctrl Pts',(-8.03142282776698,15.2,7.30483436004793));
#244196=CARTESIAN_POINT('Ctrl Pts',(-8.03327203386791,15.2,7.30805739978023));
#244197=CARTESIAN_POINT('Ctrl Pts',(-8.03512123971688,15.2,7.31128043907338));
#244198=CARTESIAN_POINT('Ctrl Pts',(-8.03697262725151,15.2,7.31451977397155));
#244199=CARTESIAN_POINT('Ctrl Pts',(-8.03882606248868,15.2,7.31777535042597));
#244200=CARTESIAN_POINT('Ctrl Pts',(-8.04067949797837,15.2,7.32103092732396));
#244201=CARTESIAN_POINT('Ctrl Pts',(-8.04253498238887,15.2,7.32430274482745));
#244202=CARTESIAN_POINT('Ctrl Pts',(-8.04439238577631,15.2,7.32759075174384));
#244203=CARTESIAN_POINT('Ctrl Pts',(-8.04624978891068,15.2,7.33087875821224));
#244204=CARTESIAN_POINT('Ctrl Pts',(-8.0481091113342,15.2,7.3341829531357));
#244205=CARTESIAN_POINT('Ctrl Pts',(-8.04997022323742,15.2,7.33750328297372));
#244206=CARTESIAN_POINT('Ctrl Pts',(-8.05183133539422,15.2,7.34082361326413));
#244207=CARTESIAN_POINT('Ctrl Pts',(-8.05369423816233,15.2,7.34416008028111));
#244208=CARTESIAN_POINT('Ctrl Pts',(-8.05555880354172,15.2,7.34751262874159));
#244209=CARTESIAN_POINT('Ctrl Pts',(-8.05742336892111,15.2,7.35086517720206));
#244210=CARTESIAN_POINT('Ctrl Pts',(-8.05928959704515,15.2,7.35423380907557));
#244211=CARTESIAN_POINT('Ctrl Pts',(-8.06115736131377,15.2,7.35761847076166));
#244212=CARTESIAN_POINT('Ctrl Pts',(-8.06302512532789,15.2,7.3610031319866));
#244213=CARTESIAN_POINT('Ctrl Pts',(-8.06489442719878,15.2,7.36440382348369));
#244214=CARTESIAN_POINT('Ctrl Pts',(-8.06676514049877,15.2,7.36782049199759));
#244215=CARTESIAN_POINT('Ctrl Pts',(-8.06863585405365,15.2,7.37123716097702));
#244216=CARTESIAN_POINT('Ctrl Pts',(-8.07050798107081,15.2,7.37466980759088));
#244217=CARTESIAN_POINT('Ctrl Pts',(-8.07238139583969,15.2,7.37811837978044));
#244218=CARTESIAN_POINT('Ctrl Pts',(-8.07425481035332,15.2,7.38156695150012));
#244219=CARTESIAN_POINT('Ctrl Pts',(-8.07612951370569,15.2,7.3850314471761));
#244220=CARTESIAN_POINT('Ctrl Pts',(-8.07800538433004,15.2,7.38851181572388));
#244221=CARTESIAN_POINT('Ctrl Pts',(-8.07988125520997,15.2,7.39199218474584));
#244222=CARTESIAN_POINT('Ctrl Pts',(-8.08175829209296,15.2,7.39548842611083));
#244223=CARTESIAN_POINT('Ctrl Pts',(-8.08363637628925,15.2,7.39900048853464));
#244224=CARTESIAN_POINT('Ctrl Pts',(-8.08598398140665,15.2,7.40339056632514));
#244225=CARTESIAN_POINT('Ctrl Pts',(-8.08833321970741,15.2,7.40780536235083));
#244226=CARTESIAN_POINT('Ctrl Pts',(-8.09068386054085,15.2,7.41224477658895));
#244227=CARTESIAN_POINT('Ctrl Pts',(-8.09256437305388,15.2,7.4157963076891));
#244228=CARTESIAN_POINT('Ctrl Pts',(-8.09444578277789,15.2,7.41936359374276));
#244229=CARTESIAN_POINT('Ctrl Pts',(-8.09632797084619,15.2,7.42294658294883));
#244230=CARTESIAN_POINT('Ctrl Pts',(-8.09821015917094,15.2,7.42652957264307));
#244231=CARTESIAN_POINT('Ctrl Pts',(-8.10009312700966,15.2,7.43012826618917));
#244232=CARTESIAN_POINT('Ctrl Pts',(-8.10197675661238,15.2,7.43374261055389));
#244233=CARTESIAN_POINT('Ctrl Pts',(-8.10386038595845,15.2,7.43735695442614));
#244234=CARTESIAN_POINT('Ctrl Pts',(-8.10574467825319,15.2,7.44098694880214));
#244235=CARTESIAN_POINT('Ctrl Pts',(-8.10762951752655,15.2,7.44463254396267));
#244236=CARTESIAN_POINT('Ctrl Pts',(-8.10951435705672,15.2,7.44827813961991));
#244237=CARTESIAN_POINT('Ctrl Pts',(-8.11139974215976,15.2,7.45193933322982));
#244238=CARTESIAN_POINT('Ctrl Pts',(-8.11328556042922,15.2,7.4556160750423));
#244239=CARTESIAN_POINT('Ctrl Pts',(-8.11517137844174,15.2,7.45929281635384));
#244240=CARTESIAN_POINT('Ctrl Pts',(-8.11705762817364,15.2,7.46298510618451));
#244241=CARTESIAN_POINT('Ctrl Pts',(-8.11894419690827,15.2,7.46669289193537));
#244242=CARTESIAN_POINT('Ctrl Pts',(-8.12083076589994,15.2,7.47040067819143));
#244243=CARTESIAN_POINT('Ctrl Pts',(-8.12271765509825,15.2,7.47412396060668));
#244244=CARTESIAN_POINT('Ctrl Pts',(-8.12460475070967,15.2,7.47786268699414));
#244245=CARTESIAN_POINT('Ctrl Pts',(-8.12649184606397,15.2,7.48160141287219));
#244246=CARTESIAN_POINT('Ctrl Pts',(-8.12837914802076,15.2,7.48535558376832));
#244247=CARTESIAN_POINT('Ctrl Pts',(-8.1302665466998,15.2,7.48912514762527));
#244248=CARTESIAN_POINT('Ctrl Pts',(-8.13215394563599,15.2,7.49289471199582));
#244249=CARTESIAN_POINT('Ctrl Pts',(-8.13404144064164,15.2,7.49667967021783));
#244250=CARTESIAN_POINT('Ctrl Pts',(-8.13592892096672,15.2,7.50047996925826));
#244251=CARTESIAN_POINT('Ctrl Pts',(-8.13876014119718,15.2,7.50618041730114));
#244252=CARTESIAN_POINT('Ctrl Pts',(-8.14159133016264,15.2,7.51191538443199));
#244253=CARTESIAN_POINT('Ctrl Pts',(-8.14442212145121,15.2,7.51768469867524));
#244254=CARTESIAN_POINT('Ctrl Pts',(-8.14630931581501,15.2,7.52153090852009));
#244255=CARTESIAN_POINT('Ctrl Pts',(-8.14819633431816,15.2,7.52539238324361));
#244256=CARTESIAN_POINT('Ctrl Pts',(-8.15008306742097,15.2,7.52926907156699));
#244257=CARTESIAN_POINT('Ctrl Pts',(-8.15196980026671,15.2,7.53314575936217));
#244258=CARTESIAN_POINT('Ctrl Pts',(-8.15385625005416,15.2,7.53703765963207));
#244259=CARTESIAN_POINT('Ctrl Pts',(-8.15574230940002,15.2,7.54094472464445));
#244260=CARTESIAN_POINT('Ctrl Pts',(-8.15762836900285,15.2,7.54485179018917));
#244261=CARTESIAN_POINT('Ctrl Pts',(-8.15951403872337,15.2,7.54877401690621));
#244262=CARTESIAN_POINT('Ctrl Pts',(-8.16139921250134,15.2,7.55271135652762));
#244263=CARTESIAN_POINT('Ctrl Pts',(-8.16328438602246,15.2,7.55664869561256));
#244264=CARTESIAN_POINT('Ctrl Pts',(-8.16516906521542,15.2,7.56060114599382));
#244265=CARTESIAN_POINT('Ctrl Pts',(-8.16705314345034,15.2,7.56456865833458));
#244266=CARTESIAN_POINT('Ctrl Pts',(-8.16893722194196,15.2,7.56853617121591));
#244267=CARTESIAN_POINT('Ctrl Pts',(-8.1708207022419,15.2,7.57251874412651));
#244268=CARTESIAN_POINT('Ctrl Pts',(-8.17270347923339,15.2,7.57651632723326));
#244269=CARTESIAN_POINT('Ctrl Pts',(-8.17458625622489,15.2,7.58051391034001));
#244270=CARTESIAN_POINT('Ctrl Pts',(-8.17646833147188,15.2,7.58452650448186));
#244271=CARTESIAN_POINT('Ctrl Pts',(-8.17834960057431,15.2,7.5885540569251));
#244272=CARTESIAN_POINT('Ctrl Pts',(-8.17976055227298,15.2,7.59157472098315));
#244273=CARTESIAN_POINT('Ctrl Pts',(-8.18117105078704,15.2,7.59460380014535));
#244274=CARTESIAN_POINT('Ctrl Pts',(-8.18258105455619,15.2,7.59764127235435));
#244275=CARTESIAN_POINT('Ctrl Pts',(-8.18446105949633,15.2,7.60169123511575));
#244276=CARTESIAN_POINT('Ctrl Pts',(-8.1863401841111,15.2,7.60575612029827));
#244277=CARTESIAN_POINT('Ctrl Pts',(-8.18821832684651,15.2,7.60983587490822));
#244278=CARTESIAN_POINT('Ctrl Pts',(-8.18962693396205,15.2,7.61289569100464));
#244279=CARTESIAN_POINT('Ctrl Pts',(-8.19103498854429,15.2,7.61596387304216));
#244280=CARTESIAN_POINT('Ctrl Pts',(-8.19244244970157,15.2,7.61904039805425));
#244281=CARTESIAN_POINT('Ctrl Pts',(-8.19384991111453,15.2,7.62211692362523));
#244282=CARTESIAN_POINT('Ctrl Pts',(-8.19525677885234,15.2,7.62520179237357));
#244283=CARTESIAN_POINT('Ctrl Pts',(-8.19666301030662,15.2,7.62829498390759));
#244284=CARTESIAN_POINT('Ctrl Pts',(-8.19806924150545,15.2,7.63138817487968));
#244285=CARTESIAN_POINT('Ctrl Pts',(-8.19947483650281,15.2,7.63448968842502));
#244286=CARTESIAN_POINT('Ctrl Pts',(-8.2008797547302,15.2,7.63759950209335));
#244287=CARTESIAN_POINT('Ctrl Pts',(-8.2022846729576,15.2,7.64070931576167));
#244288=CARTESIAN_POINT('Ctrl Pts',(-8.20368891343743,15.2,7.64382743018705));
#244289=CARTESIAN_POINT('Ctrl Pts',(-8.20509243563637,15.2,7.64695382511584));
#244290=CARTESIAN_POINT('Ctrl Pts',(-8.20743163938625,15.2,7.65216448351981));
#244291=CARTESIAN_POINT('Ctrl Pts',(-8.20976884746398,15.2,7.65739813918152));
#244292=CARTESIAN_POINT('Ctrl Pts',(-8.21210387114443,15.2,7.66265469758551));
#244293=CARTESIAN_POINT('Ctrl Pts',(-8.21350488530179,15.2,7.66580863251331));
#244294=CARTESIAN_POINT('Ctrl Pts',(-8.21490511257916,15.2,7.66897081202024));
#244295=CARTESIAN_POINT('Ctrl Pts',(-8.216304513243,15.2,7.67214121450282));
#244296=CARTESIAN_POINT('Ctrl Pts',(-8.21817038071004,15.2,7.67636841762092));
#244297=CARTESIAN_POINT('Ctrl Pts',(-8.2200347782726,15.2,7.68061023957843));
#244298=CARTESIAN_POINT('Ctrl Pts',(-8.22189760995382,15.2,7.68486663006234));
#244299=CARTESIAN_POINT('Ctrl Pts',(-8.223294734032,15.2,7.6880589236502));
#244300=CARTESIAN_POINT('Ctrl Pts',(-8.22469097903492,15.2,7.69125941239865));
#244301=CARTESIAN_POINT('Ctrl Pts',(-8.22608630302924,15.2,7.69446807494943));
#244302=CARTESIAN_POINT('Ctrl Pts',(-8.22748162677009,15.2,7.69767673691729));
#244303=CARTESIAN_POINT('Ctrl Pts',(-8.22887602945265,15.2,7.70089357186806));
#244304=CARTESIAN_POINT('Ctrl Pts',(-8.23026947361027,15.2,7.70411856033493));
#244305=CARTESIAN_POINT('Ctrl Pts',(-8.23212739906937,15.2,7.70841854476211));
#244306=CARTESIAN_POINT('Ctrl Pts',(-8.23398361793977,15.2,7.71273302241631));
#244307=CARTESIAN_POINT('Ctrl Pts',(-8.2358380382143,15.2,7.71706194438852));
#244308=CARTESIAN_POINT('Ctrl Pts',(-8.23722885348336,15.2,7.72030863601513));
#244309=CARTESIAN_POINT('Ctrl Pts',(-8.23861865699762,15.2,7.7235634522916));
#244310=CARTESIAN_POINT('Ctrl Pts',(-8.24000740923898,15.2,7.72682637179695));
#244311=CARTESIAN_POINT('Ctrl Pts',(-8.242321996392,15.2,7.73226457117011));
#244312=CARTESIAN_POINT('Ctrl Pts',(-8.24463366460899,15.2,7.73772527922906));
#244313=CARTESIAN_POINT('Ctrl Pts',(-8.24694223516477,15.2,7.74320840103274));
#244314=CARTESIAN_POINT('Ctrl Pts',(-8.24832737769955,15.2,7.74649827459308));
#244315=CARTESIAN_POINT('Ctrl Pts',(-8.24971140578404,15.2,7.74979621608907));
#244316=CARTESIAN_POINT('Ctrl Pts',(-8.25109428027653,15.2,7.75310220519565));
#244317=CARTESIAN_POINT('Ctrl Pts',(-8.2524771545178,15.2,7.75640819370164));
#244318=CARTESIAN_POINT('Ctrl Pts',(-8.25385887513413,15.2,7.75972223006552));
#244319=CARTESIAN_POINT('Ctrl Pts',(-8.25523940487552,15.2,7.76304429211217));
#244320=CARTESIAN_POINT('Ctrl Pts',(-8.25708011111378,15.2,7.7674737079732));
#244321=CARTESIAN_POINT('Ctrl Pts',(-8.25891869948066,15.2,7.771917393285));
#244322=CARTESIAN_POINT('Ctrl Pts',(-8.26075508120025,15.2,7.77637529858647));
#244323=CARTESIAN_POINT('Ctrl Pts',(-8.26259146317004,15.2,7.78083320449532));
#244324=CARTESIAN_POINT('Ctrl Pts',(-8.26442563892233,15.2,7.78530532939918));
#244325=CARTESIAN_POINT('Ctrl Pts',(-8.26625751813313,15.2,7.78979162386682));
#244326=CARTESIAN_POINT('Ctrl Pts',(-8.26808939709433,15.2,7.79427791772318));
#244327=CARTESIAN_POINT('Ctrl Pts',(-8.26991898108655,15.2,7.79877838277397));
#244328=CARTESIAN_POINT('Ctrl Pts',(-8.27174618199298,15.2,7.80329296657013));
#244329=CARTESIAN_POINT('Ctrl Pts',(-8.27357338314836,15.2,7.8078075509814));
#244330=CARTESIAN_POINT('Ctrl Pts',(-8.27539820094928,15.2,7.8123362562431));
#244331=CARTESIAN_POINT('Ctrl Pts',(-8.2772205495013,15.2,7.81687903201136));
#244332=CARTESIAN_POINT('Ctrl Pts',(-8.27858731079118,15.2,7.82028611352807));
#244333=CARTESIAN_POINT('Ctrl Pts',(-8.27995268290886,15.2,7.82370111027236));
#244334=CARTESIAN_POINT('Ctrl Pts',(-8.28131662869883,15.2,7.82712400028849));
#244335=CARTESIAN_POINT('Ctrl Pts',(-8.28313522325065,15.2,7.83168785405788));
#244336=CARTESIAN_POINT('Ctrl Pts',(-8.284951282523,15.2,7.83626574011846));
#244337=CARTESIAN_POINT('Ctrl Pts',(-8.28676472178823,15.2,7.84085761175904));
#244338=CARTESIAN_POINT('Ctrl Pts',(-8.28812480111362,15.2,7.84430151517665));
#244339=CARTESIAN_POINT('Ctrl Pts',(-8.2894834075974,15.2,7.8477532838355));
#244340=CARTESIAN_POINT('Ctrl Pts',(-8.29084050442296,15.2,7.85121289833549));
#244341=CARTESIAN_POINT('Ctrl Pts',(-8.29219760124853,15.2,7.85467251283547));
#244342=CARTESIAN_POINT('Ctrl Pts',(-8.29355318942768,15.2,7.85813997349688));
#244343=CARTESIAN_POINT('Ctrl Pts',(-8.29490723125963,15.2,7.86161525801142));
#244344=CARTESIAN_POINT('Ctrl Pts',(-8.29626127309158,15.2,7.86509054252597));
#244345=CARTESIAN_POINT('Ctrl Pts',(-8.29761376887511,15.2,7.86857365165778));
#244346=CARTESIAN_POINT('Ctrl Pts',(-8.29896468270717,15.2,7.87206456271343));
#244347=CARTESIAN_POINT('Ctrl Pts',(-8.30031559653923,15.2,7.87555547376907));
#244348=CARTESIAN_POINT('Ctrl Pts',(-8.3016649279353,15.2,7.8790541881126));
#244349=CARTESIAN_POINT('Ctrl Pts',(-8.30301264530314,15.2,7.88256068565119));
#244350=CARTESIAN_POINT('Ctrl Pts',(-8.30436036267098,15.2,7.88606718318977));
#244351=CARTESIAN_POINT('Ctrl Pts',(-8.3057064672556,15.2,7.88958146527782));
#244352=CARTESIAN_POINT('Ctrl Pts',(-8.30705092395697,15.2,7.89310351077379));
#244353=CARTESIAN_POINT('Ctrl Pts',(-8.30839538090259,15.2,7.89662555690959));
#244354=CARTESIAN_POINT('Ctrl Pts',(-8.30973818973108,15.2,7.90015536723927));
#244355=CARTESIAN_POINT('Ctrl Pts',(-8.31107930955076,15.2,7.90369291629613));
#244356=CARTESIAN_POINT('Ctrl Pts',(-8.31331450868175,15.2,7.90958882989137));
#244357=CARTESIAN_POINT('Ctrl Pts',(-8.31554500059004,15.2,7.91550623273332));
#244358=CARTESIAN_POINT('Ctrl Pts',(-8.31777064750062,15.2,7.92144504097314));
#244359=CARTESIAN_POINT('Ctrl Pts',(-8.3195511653202,15.2,7.92619608834179));
#244360=CARTESIAN_POINT('Ctrl Pts',(-8.32132858851655,15.2,7.93096084169788));
#244361=CARTESIAN_POINT('Ctrl Pts',(-8.32310290900006,15.2,7.93573928299999));
#244362=CARTESIAN_POINT('Ctrl Pts',(-7.01216898600006,15.2,7.64657512399998));
#244363=CARTESIAN_POINT('Ctrl Pts',(-7.01216898600006,11.6,7.64657512399998));
#244364=CARTESIAN_POINT('Ctrl Pts',(-7.01229743800006,15.2,7.64669302599999));
#244365=CARTESIAN_POINT('Ctrl Pts',(-7.01229743800006,11.6,7.64669302599999));
#244366=CARTESIAN_POINT('Ctrl Pts',(-7.01255888500006,15.2,7.64693288599998));
#244367=CARTESIAN_POINT('Ctrl Pts',(-7.01255888500006,11.6,7.64693288599998));
#244368=CARTESIAN_POINT('Ctrl Pts',(-7.01295521800006,15.2,7.64729613499998));
#244369=CARTESIAN_POINT('Ctrl Pts',(-7.01295521800006,11.6,7.64729613499998));
#244370=CARTESIAN_POINT('Ctrl Pts',(-7.01348948000006,15.2,7.64778506499999));
#244371=CARTESIAN_POINT('Ctrl Pts',(-7.01348948000006,11.6,7.64778506499999));
#244372=CARTESIAN_POINT('Ctrl Pts',(-7.01416585900006,15.2,7.64840281599999));
#244373=CARTESIAN_POINT('Ctrl Pts',(-7.01416585900006,11.6,7.64840281599999));
#244374=CARTESIAN_POINT('Ctrl Pts',(-7.01485383100006,15.2,7.64902988999999));
#244375=CARTESIAN_POINT('Ctrl Pts',(-7.01485383100006,11.6,7.64902988999999));
#244376=CARTESIAN_POINT('Ctrl Pts',(-7.01554947000006,15.2,7.64966267399998));
#244377=CARTESIAN_POINT('Ctrl Pts',(-7.01554947000006,11.6,7.64966267399998));
#244378=CARTESIAN_POINT('Ctrl Pts',(-7.01625276700006,15.2,7.65030113899999));
#244379=CARTESIAN_POINT('Ctrl Pts',(-7.01625276700006,11.6,7.65030113899999));
#244380=CARTESIAN_POINT('Ctrl Pts',(-7.01696371600006,15.2,7.65094525299999));
#244381=CARTESIAN_POINT('Ctrl Pts',(-7.01696371600006,11.6,7.65094525299999));
#244382=CARTESIAN_POINT('Ctrl Pts',(-7.01768230900006,15.2,7.65159498499998));
#244383=CARTESIAN_POINT('Ctrl Pts',(-7.01768230900006,11.6,7.65159498499998));
#244384=CARTESIAN_POINT('Ctrl Pts',(-7.01840853600006,15.2,7.65225030299998));
#244385=CARTESIAN_POINT('Ctrl Pts',(-7.01840853600006,11.6,7.65225030299998));
#244386=CARTESIAN_POINT('Ctrl Pts',(-7.01914239300006,15.2,7.65291117499999));
#244387=CARTESIAN_POINT('Ctrl Pts',(-7.01914239300006,11.6,7.65291117499999));
#244388=CARTESIAN_POINT('Ctrl Pts',(-7.01988387000006,15.2,7.65357757299999));
#244389=CARTESIAN_POINT('Ctrl Pts',(-7.01988387000006,11.6,7.65357757299999));
#244390=CARTESIAN_POINT('Ctrl Pts',(-7.02063296000006,15.2,7.65424946399998));
#244391=CARTESIAN_POINT('Ctrl Pts',(-7.02063296000006,11.6,7.65424946399998));
#244392=CARTESIAN_POINT('Ctrl Pts',(-7.02138965700006,15.2,7.65492681899998));
#244393=CARTESIAN_POINT('Ctrl Pts',(-7.02138965700006,11.6,7.65492681899998));
#244394=CARTESIAN_POINT('Ctrl Pts',(-7.02215395000006,15.2,7.65560960799998));
#244395=CARTESIAN_POINT('Ctrl Pts',(-7.02215395000006,11.6,7.65560960799998));
#244396=CARTESIAN_POINT('Ctrl Pts',(-7.02292583400006,15.2,7.65629779899999));
#244397=CARTESIAN_POINT('Ctrl Pts',(-7.02292583400006,11.6,7.65629779899999));
#244398=CARTESIAN_POINT('Ctrl Pts',(-7.02370530000006,15.2,7.65699136299999));
#244399=CARTESIAN_POINT('Ctrl Pts',(-7.02370530000006,11.6,7.65699136299999));
#244400=CARTESIAN_POINT('Ctrl Pts',(-7.02449234200006,15.2,7.65769026899999));
#244401=CARTESIAN_POINT('Ctrl Pts',(-7.02449234200006,11.6,7.65769026899999));
#244402=CARTESIAN_POINT('Ctrl Pts',(-7.02528695100006,15.2,7.65839448899998));
#244403=CARTESIAN_POINT('Ctrl Pts',(-7.02528695100006,11.6,7.65839448899998));
#244404=CARTESIAN_POINT('Ctrl Pts',(-7.02608912200006,15.2,7.65910399299998));
#244405=CARTESIAN_POINT('Ctrl Pts',(-7.02608912200006,11.6,7.65910399299998));
#244406=CARTESIAN_POINT('Ctrl Pts',(-7.02689884500006,15.2,7.65981874999999));
#244407=CARTESIAN_POINT('Ctrl Pts',(-7.02689884500006,11.6,7.65981874999999));
#244408=CARTESIAN_POINT('Ctrl Pts',(-7.02771611300006,15.2,7.66053873299998));
#244409=CARTESIAN_POINT('Ctrl Pts',(-7.02771611300006,11.6,7.66053873299998));
#244410=CARTESIAN_POINT('Ctrl Pts',(-7.02854092000006,15.2,7.66126390999998));
#244411=CARTESIAN_POINT('Ctrl Pts',(-7.02854092000006,11.6,7.66126390999998));
#244412=CARTESIAN_POINT('Ctrl Pts',(-7.02937325800006,15.2,7.66199425499998));
#244413=CARTESIAN_POINT('Ctrl Pts',(-7.02937325800006,11.6,7.66199425499998));
#244414=CARTESIAN_POINT('Ctrl Pts',(-7.03021311900006,15.2,7.66272973699999));
#244415=CARTESIAN_POINT('Ctrl Pts',(-7.03021311900006,11.6,7.66272973699999));
#244416=CARTESIAN_POINT('Ctrl Pts',(-7.03106049600006,15.2,7.66347032799998));
#244417=CARTESIAN_POINT('Ctrl Pts',(-7.03106049600006,11.6,7.66347032799998));
#244418=CARTESIAN_POINT('Ctrl Pts',(-7.03191538200006,15.2,7.66421599899999));
#244419=CARTESIAN_POINT('Ctrl Pts',(-7.03191538200006,11.6,7.66421599899999));
#244420=CARTESIAN_POINT('Ctrl Pts',(-7.03277777000006,15.2,7.66496672199998));
#244421=CARTESIAN_POINT('Ctrl Pts',(-7.03277777000006,11.6,7.66496672199998));
#244422=CARTESIAN_POINT('Ctrl Pts',(-7.03364765200006,15.2,7.66572246899998));
#244423=CARTESIAN_POINT('Ctrl Pts',(-7.03364765200006,11.6,7.66572246899998));
#244424=CARTESIAN_POINT('Ctrl Pts',(-7.03452502100006,15.2,7.66648321099999));
#244425=CARTESIAN_POINT('Ctrl Pts',(-7.03452502100006,11.6,7.66648321099999));
#244426=CARTESIAN_POINT('Ctrl Pts',(-7.03540987000006,15.2,7.66724892099998));
#244427=CARTESIAN_POINT('Ctrl Pts',(-7.03540987000006,11.6,7.66724892099998));
#244428=CARTESIAN_POINT('Ctrl Pts',(-7.03630219100006,15.2,7.66801956799998));
#244429=CARTESIAN_POINT('Ctrl Pts',(-7.03630219100006,11.6,7.66801956799998));
#244430=CARTESIAN_POINT('Ctrl Pts',(-7.03720197800005,15.2,7.66879512799999));
#244431=CARTESIAN_POINT('Ctrl Pts',(-7.03720197800005,11.6,7.66879512799999));
#244432=CARTESIAN_POINT('Ctrl Pts',(-7.03810922400006,15.2,7.66957557299998));
#244433=CARTESIAN_POINT('Ctrl Pts',(-7.03810922400006,11.6,7.66957557299998));
#244434=CARTESIAN_POINT('Ctrl Pts',(-7.03902392100006,15.2,7.67036087199998));
#244435=CARTESIAN_POINT('Ctrl Pts',(-7.03902392100006,11.6,7.67036087199998));
#244436=CARTESIAN_POINT('Ctrl Pts',(-7.03994606100006,15.2,7.67115099999998));
#244437=CARTESIAN_POINT('Ctrl Pts',(-7.03994606100006,11.6,7.67115099999998));
#244438=CARTESIAN_POINT('Ctrl Pts',(-7.04087563900006,15.2,7.67194592999999));
#244439=CARTESIAN_POINT('Ctrl Pts',(-7.04087563900006,11.6,7.67194592999999));
#244440=CARTESIAN_POINT('Ctrl Pts',(-7.04181264600006,15.2,7.67274563399998));
#244441=CARTESIAN_POINT('Ctrl Pts',(-7.04181264600006,11.6,7.67274563399998));
#244442=CARTESIAN_POINT('Ctrl Pts',(-7.04275707700006,15.2,7.67355008599999));
#244443=CARTESIAN_POINT('Ctrl Pts',(-7.04275707700006,11.6,7.67355008599999));
#244444=CARTESIAN_POINT('Ctrl Pts',(-7.04370892200005,15.2,7.67435925699999));
#244445=CARTESIAN_POINT('Ctrl Pts',(-7.04370892200005,11.6,7.67435925699999));
#244446=CARTESIAN_POINT('Ctrl Pts',(-7.04466817800006,15.2,7.67517312299999));
#244447=CARTESIAN_POINT('Ctrl Pts',(-7.04466817800006,11.6,7.67517312299999));
#244448=CARTESIAN_POINT('Ctrl Pts',(-7.04563483400006,15.2,7.67599165499998));
#244449=CARTESIAN_POINT('Ctrl Pts',(-7.04563483400006,11.6,7.67599165499998));
#244450=CARTESIAN_POINT('Ctrl Pts',(-7.04660888600006,15.2,7.67681482699999));
#244451=CARTESIAN_POINT('Ctrl Pts',(-7.04660888600006,11.6,7.67681482699999));
#244452=CARTESIAN_POINT('Ctrl Pts',(-7.04759032400006,15.2,7.67764261299998));
#244453=CARTESIAN_POINT('Ctrl Pts',(-7.04759032400006,11.6,7.67764261299998));
#244454=CARTESIAN_POINT('Ctrl Pts',(-7.04857914400006,15.2,7.67847498699999));
#244455=CARTESIAN_POINT('Ctrl Pts',(-7.04857914400006,11.6,7.67847498699999));
#244456=CARTESIAN_POINT('Ctrl Pts',(-7.04957533900005,15.2,7.67931192299999));
#244457=CARTESIAN_POINT('Ctrl Pts',(-7.04957533900005,11.6,7.67931192299999));
#244458=CARTESIAN_POINT('Ctrl Pts',(-7.05057890000006,15.2,7.68015339299998));
#244459=CARTESIAN_POINT('Ctrl Pts',(-7.05057890000006,11.6,7.68015339299998));
#244460=CARTESIAN_POINT('Ctrl Pts',(-7.05158982000006,15.2,7.68099937399998));
#244461=CARTESIAN_POINT('Ctrl Pts',(-7.05158982000006,11.6,7.68099937399998));
#244462=CARTESIAN_POINT('Ctrl Pts',(-7.05260809400006,15.2,7.68184983699999));
#244463=CARTESIAN_POINT('Ctrl Pts',(-7.05260809400006,11.6,7.68184983699999));
#244464=CARTESIAN_POINT('Ctrl Pts',(-7.05363371500006,15.2,7.68270475799999));
#244465=CARTESIAN_POINT('Ctrl Pts',(-7.05363371500006,11.6,7.68270475799999));
#244466=CARTESIAN_POINT('Ctrl Pts',(-7.05466667400006,15.2,7.68356411099998));
#244467=CARTESIAN_POINT('Ctrl Pts',(-7.05466667400006,11.6,7.68356411099998));
#244468=CARTESIAN_POINT('Ctrl Pts',(-7.05570696700006,15.2,7.68442787099998));
#244469=CARTESIAN_POINT('Ctrl Pts',(-7.05570696700006,11.6,7.68442787099998));
#244470=CARTESIAN_POINT('Ctrl Pts',(-7.05675458400005,15.2,7.68529601199998));
#244471=CARTESIAN_POINT('Ctrl Pts',(-7.05675458400005,11.6,7.68529601199998));
#244472=CARTESIAN_POINT('Ctrl Pts',(-7.05780952100006,15.2,7.68616850899999));
#244473=CARTESIAN_POINT('Ctrl Pts',(-7.05780952100006,11.6,7.68616850899999));
#244474=CARTESIAN_POINT('Ctrl Pts',(-7.05887177100006,15.2,7.68704533799998));
#244475=CARTESIAN_POINT('Ctrl Pts',(-7.05887177100006,11.6,7.68704533799998));
#244476=CARTESIAN_POINT('Ctrl Pts',(-7.05994132500006,15.2,7.68792647199999));
#244477=CARTESIAN_POINT('Ctrl Pts',(-7.05994132500006,11.6,7.68792647199999));
#244478=CARTESIAN_POINT('Ctrl Pts',(-7.06101817900006,15.2,7.68881188699999));
#244479=CARTESIAN_POINT('Ctrl Pts',(-7.06101817900006,11.6,7.68881188699999));
#244480=CARTESIAN_POINT('Ctrl Pts',(-7.06210232400006,15.2,7.68970155699999));
#244481=CARTESIAN_POINT('Ctrl Pts',(-7.06210232400006,11.6,7.68970155699999));
#244482=CARTESIAN_POINT('Ctrl Pts',(-7.06319375500006,15.2,7.69059545999998));
#244483=CARTESIAN_POINT('Ctrl Pts',(-7.06319375500006,11.6,7.69059545999998));
#244484=CARTESIAN_POINT('Ctrl Pts',(-7.06429246300006,15.2,7.69149356899998));
#244485=CARTESIAN_POINT('Ctrl Pts',(-7.06429246300006,11.6,7.69149356899998));
#244486=CARTESIAN_POINT('Ctrl Pts',(-7.06539844400006,15.2,7.69239585999999));
#244487=CARTESIAN_POINT('Ctrl Pts',(-7.06539844400006,11.6,7.69239585999999));
#244488=CARTESIAN_POINT('Ctrl Pts',(-7.06651169000006,15.2,7.69330230899998));
#244489=CARTESIAN_POINT('Ctrl Pts',(-7.06651169000006,11.6,7.69330230899998));
#244490=CARTESIAN_POINT('Ctrl Pts',(-7.06763219400006,15.2,7.69421289099999));
#244491=CARTESIAN_POINT('Ctrl Pts',(-7.06763219400006,11.6,7.69421289099999));
#244492=CARTESIAN_POINT('Ctrl Pts',(-7.06875995000006,15.2,7.69512758399999));
#244493=CARTESIAN_POINT('Ctrl Pts',(-7.06875995000006,11.6,7.69512758399999));
#244494=CARTESIAN_POINT('Ctrl Pts',(-7.06989495100006,15.2,7.69604635999999));
#244495=CARTESIAN_POINT('Ctrl Pts',(-7.06989495100006,11.6,7.69604635999999));
#244496=CARTESIAN_POINT('Ctrl Pts',(-7.07103719100005,15.2,7.69696919799999));
#244497=CARTESIAN_POINT('Ctrl Pts',(-7.07103719100005,11.6,7.69696919799999));
#244498=CARTESIAN_POINT('Ctrl Pts',(-7.07218666200006,15.2,7.69789607499998));
#244499=CARTESIAN_POINT('Ctrl Pts',(-7.07218666200006,11.6,7.69789607499998));
#244500=CARTESIAN_POINT('Ctrl Pts',(-7.07334335900006,15.2,7.69882696299998));
#244501=CARTESIAN_POINT('Ctrl Pts',(-7.07334335900006,11.6,7.69882696299998));
#244502=CARTESIAN_POINT('Ctrl Pts',(-7.07450727400006,15.2,7.69976184299999));
#244503=CARTESIAN_POINT('Ctrl Pts',(-7.07450727400006,11.6,7.69976184299999));
#244504=CARTESIAN_POINT('Ctrl Pts',(-7.07567840200006,15.2,7.70070068799999));
#244505=CARTESIAN_POINT('Ctrl Pts',(-7.07567840200006,11.6,7.70070068799999));
#244506=CARTESIAN_POINT('Ctrl Pts',(-7.07685673500006,15.2,7.70164347599999));
#244507=CARTESIAN_POINT('Ctrl Pts',(-7.07685673500006,11.6,7.70164347599999));
#244508=CARTESIAN_POINT('Ctrl Pts',(-7.07804226800006,15.2,7.70259018399998));
#244509=CARTESIAN_POINT('Ctrl Pts',(-7.07804226800006,11.6,7.70259018399998));
#244510=CARTESIAN_POINT('Ctrl Pts',(-7.07923499300006,15.2,7.70354078799999));
#244511=CARTESIAN_POINT('Ctrl Pts',(-7.07923499300006,11.6,7.70354078799999));
#244512=CARTESIAN_POINT('Ctrl Pts',(-7.08043490300006,15.2,7.70449526499998));
#244513=CARTESIAN_POINT('Ctrl Pts',(-7.08043490300006,11.6,7.70449526499998));
#244514=CARTESIAN_POINT('Ctrl Pts',(-7.08164199400006,15.2,7.70545359099999));
#244515=CARTESIAN_POINT('Ctrl Pts',(-7.08164199400006,11.6,7.70545359099999));
#244516=CARTESIAN_POINT('Ctrl Pts',(-7.08285625800006,15.2,7.70641574499999));
#244517=CARTESIAN_POINT('Ctrl Pts',(-7.08285625800006,11.6,7.70641574499999));
#244518=CARTESIAN_POINT('Ctrl Pts',(-7.08407768800006,15.2,7.70738170199999));
#244519=CARTESIAN_POINT('Ctrl Pts',(-7.08407768800006,11.6,7.70738170199999));
#244520=CARTESIAN_POINT('Ctrl Pts',(-7.08530627800006,15.2,7.70835144099999));
#244521=CARTESIAN_POINT('Ctrl Pts',(-7.08530627800006,11.6,7.70835144099999));
#244522=CARTESIAN_POINT('Ctrl Pts',(-7.08654202200006,15.2,7.70932493899998));
#244523=CARTESIAN_POINT('Ctrl Pts',(-7.08654202200006,11.6,7.70932493899998));
#244524=CARTESIAN_POINT('Ctrl Pts',(-7.08778491400006,15.2,7.71030217199999));
#244525=CARTESIAN_POINT('Ctrl Pts',(-7.08778491400006,11.6,7.71030217199999));
#244526=CARTESIAN_POINT('Ctrl Pts',(-7.08903494500006,15.2,7.71128311899999));
#244527=CARTESIAN_POINT('Ctrl Pts',(-7.08903494500006,11.6,7.71128311899999));
#244528=CARTESIAN_POINT('Ctrl Pts',(-7.09029211200006,15.2,7.71226775599998));
#244529=CARTESIAN_POINT('Ctrl Pts',(-7.09029211200006,11.6,7.71226775599998));
#244530=CARTESIAN_POINT('Ctrl Pts',(-7.09155640600006,15.2,7.71325606199999));
#244531=CARTESIAN_POINT('Ctrl Pts',(-7.09155640600006,11.6,7.71325606199999));
#244532=CARTESIAN_POINT('Ctrl Pts',(-7.09282782300006,15.2,7.71424801399998));
#244533=CARTESIAN_POINT('Ctrl Pts',(-7.09282782300006,11.6,7.71424801399998));
#244534=CARTESIAN_POINT('Ctrl Pts',(-7.09410635400006,15.2,7.71524359099999));
#244535=CARTESIAN_POINT('Ctrl Pts',(-7.09410635400006,11.6,7.71524359099999));
#244536=CARTESIAN_POINT('Ctrl Pts',(-7.09539199400006,15.2,7.71624276799999));
#244537=CARTESIAN_POINT('Ctrl Pts',(-7.09539199400006,11.6,7.71624276799999));
#244538=CARTESIAN_POINT('Ctrl Pts',(-7.09668473700006,15.2,7.71724552699999));
#244539=CARTESIAN_POINT('Ctrl Pts',(-7.09668473700006,11.6,7.71724552699999));
#244540=CARTESIAN_POINT('Ctrl Pts',(-7.09798457700006,15.2,7.71825184399999));
#244541=CARTESIAN_POINT('Ctrl Pts',(-7.09798457700006,11.6,7.71825184399999));
#244542=CARTESIAN_POINT('Ctrl Pts',(-7.09929150500006,15.2,7.71926169699999));
#244543=CARTESIAN_POINT('Ctrl Pts',(-7.09929150500006,11.6,7.71926169699999));
#244544=CARTESIAN_POINT('Ctrl Pts',(-7.10060551800006,15.2,7.72027506499998));
#244545=CARTESIAN_POINT('Ctrl Pts',(-7.10060551800006,11.6,7.72027506499998));
#244546=CARTESIAN_POINT('Ctrl Pts',(-7.10192660800006,15.2,7.72129192499998));
#244547=CARTESIAN_POINT('Ctrl Pts',(-7.10192660800006,11.6,7.72129192499998));
#244548=CARTESIAN_POINT('Ctrl Pts',(-7.10325476900006,15.2,7.72231225799998));
#244549=CARTESIAN_POINT('Ctrl Pts',(-7.10325476900006,11.6,7.72231225799998));
#244550=CARTESIAN_POINT('Ctrl Pts',(-7.10458999400006,15.2,7.72333603999999));
#244551=CARTESIAN_POINT('Ctrl Pts',(-7.10458999400006,11.6,7.72333603999999));
#244552=CARTESIAN_POINT('Ctrl Pts',(-7.10593227900006,15.2,7.72436325099999));
#244553=CARTESIAN_POINT('Ctrl Pts',(-7.10593227900006,11.6,7.72436325099999));
#244554=CARTESIAN_POINT('Ctrl Pts',(-7.10728161500006,15.2,7.72539386899999));
#244555=CARTESIAN_POINT('Ctrl Pts',(-7.10728161500006,11.6,7.72539386899999));
#244556=CARTESIAN_POINT('Ctrl Pts',(-7.10863799800006,15.2,7.72642787299999));
#244557=CARTESIAN_POINT('Ctrl Pts',(-7.10863799800006,11.6,7.72642787299999));
#244558=CARTESIAN_POINT('Ctrl Pts',(-7.11000142000006,15.2,7.72746524299999));
#244559=CARTESIAN_POINT('Ctrl Pts',(-7.11000142000006,11.6,7.72746524299999));
#244560=CARTESIAN_POINT('Ctrl Pts',(-7.11137187600006,15.2,7.72850595599999));
#244561=CARTESIAN_POINT('Ctrl Pts',(-7.11137187600006,11.6,7.72850595599999));
#244562=CARTESIAN_POINT('Ctrl Pts',(-7.11274935900006,15.2,7.72954999299999));
#244563=CARTESIAN_POINT('Ctrl Pts',(-7.11274935900006,11.6,7.72954999299999));
#244564=CARTESIAN_POINT('Ctrl Pts',(-7.11413386400006,15.2,7.73059733099998));
#244565=CARTESIAN_POINT('Ctrl Pts',(-7.11413386400006,11.6,7.73059733099998));
#244566=CARTESIAN_POINT('Ctrl Pts',(-7.11552538300006,15.2,7.73164795099999));
#244567=CARTESIAN_POINT('Ctrl Pts',(-7.11552538300006,11.6,7.73164795099999));
#244568=CARTESIAN_POINT('Ctrl Pts',(-7.11692391100006,15.2,7.73270183099999));
#244569=CARTESIAN_POINT('Ctrl Pts',(-7.11692391100006,11.6,7.73270183099999));
#244570=CARTESIAN_POINT('Ctrl Pts',(-7.11832944100006,15.2,7.73375895199998));
#244571=CARTESIAN_POINT('Ctrl Pts',(-7.11832944100006,11.6,7.73375895199998));
#244572=CARTESIAN_POINT('Ctrl Pts',(-7.11974196900006,15.2,7.73481929199999));
#244573=CARTESIAN_POINT('Ctrl Pts',(-7.11974196900006,11.6,7.73481929199999));
#244574=CARTESIAN_POINT('Ctrl Pts',(-7.12116148600006,15.2,7.73588283099999));
#244575=CARTESIAN_POINT('Ctrl Pts',(-7.12116148600006,11.6,7.73588283099999));
#244576=CARTESIAN_POINT('Ctrl Pts',(-7.12258798800006,15.2,7.73694954699998));
#244577=CARTESIAN_POINT('Ctrl Pts',(-7.12258798800006,11.6,7.73694954699998));
#244578=CARTESIAN_POINT('Ctrl Pts',(-7.12402146800006,15.2,7.73801942399999));
#244579=CARTESIAN_POINT('Ctrl Pts',(-7.12402146800006,11.6,7.73801942399999));
#244580=CARTESIAN_POINT('Ctrl Pts',(-7.12546192000006,15.2,7.73909243699999));
#244581=CARTESIAN_POINT('Ctrl Pts',(-7.12546192000006,11.6,7.73909243699999));
#244582=CARTESIAN_POINT('Ctrl Pts',(-7.12690933700006,15.2,7.74016856899999));
#244583=CARTESIAN_POINT('Ctrl Pts',(-7.12690933700006,11.6,7.74016856899999));
#244584=CARTESIAN_POINT('Ctrl Pts',(-7.12836371400006,15.2,7.74124779699999));
#244585=CARTESIAN_POINT('Ctrl Pts',(-7.12836371400006,11.6,7.74124779699999));
#244586=CARTESIAN_POINT('Ctrl Pts',(-7.12982504600006,15.2,7.74233010399998));
#244587=CARTESIAN_POINT('Ctrl Pts',(-7.12982504600006,11.6,7.74233010399998));
#244588=CARTESIAN_POINT('Ctrl Pts',(-7.13129332400006,15.2,7.74341546899999));
#244589=CARTESIAN_POINT('Ctrl Pts',(-7.13129332400006,11.6,7.74341546899999));
#244590=CARTESIAN_POINT('Ctrl Pts',(-7.13276854400006,15.2,7.74450386999998));
#244591=CARTESIAN_POINT('Ctrl Pts',(-7.13276854400006,11.6,7.74450386999998));
#244592=CARTESIAN_POINT('Ctrl Pts',(-7.13425070000006,15.2,7.74559529099999));
#244593=CARTESIAN_POINT('Ctrl Pts',(-7.13425070000006,11.6,7.74559529099999));
#244594=CARTESIAN_POINT('Ctrl Pts',(-7.13573978500006,15.2,7.74668970999999));
#244595=CARTESIAN_POINT('Ctrl Pts',(-7.13573978500006,11.6,7.74668970999999));
#244596=CARTESIAN_POINT('Ctrl Pts',(-7.13723579400006,15.2,7.74778710799998));
#244597=CARTESIAN_POINT('Ctrl Pts',(-7.13723579400006,11.6,7.74778710799998));
#244598=CARTESIAN_POINT('Ctrl Pts',(-7.13873872000006,15.2,7.74888746499999));
#244599=CARTESIAN_POINT('Ctrl Pts',(-7.13873872000006,11.6,7.74888746499999));
#244600=CARTESIAN_POINT('Ctrl Pts',(-7.14024855600006,15.2,7.74999076199999));
#244601=CARTESIAN_POINT('Ctrl Pts',(-7.14024855600006,11.6,7.74999076199999));
#244602=CARTESIAN_POINT('Ctrl Pts',(-7.14176530000006,15.2,7.75109697799999));
#244603=CARTESIAN_POINT('Ctrl Pts',(-7.14176530000006,11.6,7.75109697799999));
#244604=CARTESIAN_POINT('Ctrl Pts',(-7.14328894200006,15.2,7.75220609499998));
#244605=CARTESIAN_POINT('Ctrl Pts',(-7.14328894200006,11.6,7.75220609499998));
#244606=CARTESIAN_POINT('Ctrl Pts',(-7.14481947700006,15.2,7.75331809499999));
#244607=CARTESIAN_POINT('Ctrl Pts',(-7.14481947700006,11.6,7.75331809499999));
#244608=CARTESIAN_POINT('Ctrl Pts',(-7.14635690000006,15.2,7.75443295699999));
#244609=CARTESIAN_POINT('Ctrl Pts',(-7.14635690000006,11.6,7.75443295699999));
#244610=CARTESIAN_POINT('Ctrl Pts',(-7.14790120500005,15.2,7.75555066199999));
#244611=CARTESIAN_POINT('Ctrl Pts',(-7.14790120500005,11.6,7.75555066199999));
#244612=CARTESIAN_POINT('Ctrl Pts',(-7.14945238500006,15.2,7.75667119099998));
#244613=CARTESIAN_POINT('Ctrl Pts',(-7.14945238500006,11.6,7.75667119099998));
#244614=CARTESIAN_POINT('Ctrl Pts',(-7.15101043300006,15.2,7.75779452499999));
#244615=CARTESIAN_POINT('Ctrl Pts',(-7.15101043300006,11.6,7.75779452499999));
#244616=CARTESIAN_POINT('Ctrl Pts',(-7.15257534700006,15.2,7.75892064699998));
#244617=CARTESIAN_POINT('Ctrl Pts',(-7.15257534700006,11.6,7.75892064699998));
#244618=CARTESIAN_POINT('Ctrl Pts',(-7.15414711700006,15.2,7.76004953499999));
#244619=CARTESIAN_POINT('Ctrl Pts',(-7.15414711700006,11.6,7.76004953499999));
#244620=CARTESIAN_POINT('Ctrl Pts',(-7.15572573900006,15.2,7.76118117199999));
#244621=CARTESIAN_POINT('Ctrl Pts',(-7.15572573900006,11.6,7.76118117199999));
#244622=CARTESIAN_POINT('Ctrl Pts',(-7.15731120800006,15.2,7.76231553799998));
#244623=CARTESIAN_POINT('Ctrl Pts',(-7.15731120800006,11.6,7.76231553799998));
#244624=CARTESIAN_POINT('Ctrl Pts',(-7.15890351700006,15.2,7.76345261699999));
#244625=CARTESIAN_POINT('Ctrl Pts',(-7.15890351700006,11.6,7.76345261699999));
#244626=CARTESIAN_POINT('Ctrl Pts',(-7.16050265800006,15.2,7.76459238699999));
#244627=CARTESIAN_POINT('Ctrl Pts',(-7.16050265800006,11.6,7.76459238699999));
#244628=CARTESIAN_POINT('Ctrl Pts',(-7.16210862800006,15.2,7.76573483199999));
#244629=CARTESIAN_POINT('Ctrl Pts',(-7.16210862800006,11.6,7.76573483199999));
#244630=CARTESIAN_POINT('Ctrl Pts',(-7.16372142100006,15.2,7.76687993299999));
#244631=CARTESIAN_POINT('Ctrl Pts',(-7.16372142100006,11.6,7.76687993299999));
#244632=CARTESIAN_POINT('Ctrl Pts',(-7.16534103000006,15.2,7.76802766999998));
#244633=CARTESIAN_POINT('Ctrl Pts',(-7.16534103000006,11.6,7.76802766999998));
#244634=CARTESIAN_POINT('Ctrl Pts',(-7.16696745000006,15.2,7.76917802599999));
#244635=CARTESIAN_POINT('Ctrl Pts',(-7.16696745000006,11.6,7.76917802599999));
#244636=CARTESIAN_POINT('Ctrl Pts',(-7.16860067400006,15.2,7.77033098499999));
#244637=CARTESIAN_POINT('Ctrl Pts',(-7.16860067400006,11.6,7.77033098499999));
#244638=CARTESIAN_POINT('Ctrl Pts',(-7.17024069700006,15.2,7.77148652499999));
#244639=CARTESIAN_POINT('Ctrl Pts',(-7.17024069700006,11.6,7.77148652499999));
#244640=CARTESIAN_POINT('Ctrl Pts',(-7.17188751300006,15.2,7.77264462899999));
#244641=CARTESIAN_POINT('Ctrl Pts',(-7.17188751300006,11.6,7.77264462899999));
#244642=CARTESIAN_POINT('Ctrl Pts',(-7.17354111600006,15.2,7.77380527999998));
#244643=CARTESIAN_POINT('Ctrl Pts',(-7.17354111600006,11.6,7.77380527999998));
#244644=CARTESIAN_POINT('Ctrl Pts',(-7.17520150000006,15.2,7.77496845799998));
#244645=CARTESIAN_POINT('Ctrl Pts',(-7.17520150000006,11.6,7.77496845799998));
#244646=CARTESIAN_POINT('Ctrl Pts',(-7.17686866000006,15.2,7.77613414899999));
#244647=CARTESIAN_POINT('Ctrl Pts',(-7.17686866000006,11.6,7.77613414899999));
#244648=CARTESIAN_POINT('Ctrl Pts',(-7.17854259000006,15.2,7.77730232999998));
#244649=CARTESIAN_POINT('Ctrl Pts',(-7.17854259000006,11.6,7.77730232999998));
#244650=CARTESIAN_POINT('Ctrl Pts',(-7.18022328300005,15.2,7.77847298699999));
#244651=CARTESIAN_POINT('Ctrl Pts',(-7.18022328300005,11.6,7.77847298699999));
#244652=CARTESIAN_POINT('Ctrl Pts',(-7.18191073400006,15.2,7.77964609999999));
#244653=CARTESIAN_POINT('Ctrl Pts',(-7.18191073400006,11.6,7.77964609999999));
#244654=CARTESIAN_POINT('Ctrl Pts',(-7.18360493800006,15.2,7.78082165399999));
#244655=CARTESIAN_POINT('Ctrl Pts',(-7.18360493800006,11.6,7.78082165399999));
#244656=CARTESIAN_POINT('Ctrl Pts',(-7.18530588900006,15.2,7.78199962799999));
#244657=CARTESIAN_POINT('Ctrl Pts',(-7.18530588900006,11.6,7.78199962799999));
#244658=CARTESIAN_POINT('Ctrl Pts',(-7.18701358000006,15.2,7.78318000699999));
#244659=CARTESIAN_POINT('Ctrl Pts',(-7.18701358000006,11.6,7.78318000699999));
#244660=CARTESIAN_POINT('Ctrl Pts',(-7.18872800700006,15.2,7.78436277199998));
#244661=CARTESIAN_POINT('Ctrl Pts',(-7.18872800700006,11.6,7.78436277199998));
#244662=CARTESIAN_POINT('Ctrl Pts',(-7.19044916200006,15.2,7.78554790599999));
#244663=CARTESIAN_POINT('Ctrl Pts',(-7.19044916200006,11.6,7.78554790599999));
#244664=CARTESIAN_POINT('Ctrl Pts',(-7.19217704100005,15.2,7.78673539199998));
#244665=CARTESIAN_POINT('Ctrl Pts',(-7.19217704100005,11.6,7.78673539199998));
#244666=CARTESIAN_POINT('Ctrl Pts',(-7.19391163700006,15.2,7.78792521199998));
#244667=CARTESIAN_POINT('Ctrl Pts',(-7.19391163700006,11.6,7.78792521199998));
#244668=CARTESIAN_POINT('Ctrl Pts',(-7.19565294600006,15.2,7.78911734999999));
#244669=CARTESIAN_POINT('Ctrl Pts',(-7.19565294600006,11.6,7.78911734999999));
#244670=CARTESIAN_POINT('Ctrl Pts',(-7.19740096200006,15.2,7.79031178799999));
#244671=CARTESIAN_POINT('Ctrl Pts',(-7.19740096200006,11.6,7.79031178799999));
#244672=CARTESIAN_POINT('Ctrl Pts',(-7.19915567700006,15.2,7.79150850799999));
#244673=CARTESIAN_POINT('Ctrl Pts',(-7.19915567700006,11.6,7.79150850799999));
#244674=CARTESIAN_POINT('Ctrl Pts',(-7.20091708800005,15.2,7.79270749399998));
#244675=CARTESIAN_POINT('Ctrl Pts',(-7.20091708800005,11.6,7.79270749399998));
#244676=CARTESIAN_POINT('Ctrl Pts',(-7.20268518700006,15.2,7.79390872899998));
#244677=CARTESIAN_POINT('Ctrl Pts',(-7.20268518700006,11.6,7.79390872899998));
#244678=CARTESIAN_POINT('Ctrl Pts',(-7.20445997000006,15.2,7.79511219599998));
#244679=CARTESIAN_POINT('Ctrl Pts',(-7.20445997000006,11.6,7.79511219599998));
#244680=CARTESIAN_POINT('Ctrl Pts',(-7.20624143100006,15.2,7.79631787699999));
#244681=CARTESIAN_POINT('Ctrl Pts',(-7.20624143100006,11.6,7.79631787699999));
#244682=CARTESIAN_POINT('Ctrl Pts',(-7.20802956400005,15.2,7.79752575699998));
#244683=CARTESIAN_POINT('Ctrl Pts',(-7.20802956400005,11.6,7.79752575699998));
#244684=CARTESIAN_POINT('Ctrl Pts',(-7.20982436400006,15.2,7.79873581599999));
#244685=CARTESIAN_POINT('Ctrl Pts',(-7.20982436400006,11.6,7.79873581599999));
#244686=CARTESIAN_POINT('Ctrl Pts',(-7.21162582400006,15.2,7.79994804199998));
#244687=CARTESIAN_POINT('Ctrl Pts',(-7.21162582400006,11.6,7.79994804199998));
#244688=CARTESIAN_POINT('Ctrl Pts',(-7.21343393900006,15.2,7.80116241399998));
#244689=CARTESIAN_POINT('Ctrl Pts',(-7.21343393900006,11.6,7.80116241399998));
#244690=CARTESIAN_POINT('Ctrl Pts',(-7.21524870400006,15.2,7.80237891799998));
#244691=CARTESIAN_POINT('Ctrl Pts',(-7.21524870400006,11.6,7.80237891799998));
#244692=CARTESIAN_POINT('Ctrl Pts',(-7.21707011300006,15.2,7.80359753599999));
#244693=CARTESIAN_POINT('Ctrl Pts',(-7.21707011300006,11.6,7.80359753599999));
#244694=CARTESIAN_POINT('Ctrl Pts',(-7.21889815900006,15.2,7.80481825199999));
#244695=CARTESIAN_POINT('Ctrl Pts',(-7.21889815900006,11.6,7.80481825199999));
#244696=CARTESIAN_POINT('Ctrl Pts',(-7.22073283800006,15.2,7.80604104899999));
#244697=CARTESIAN_POINT('Ctrl Pts',(-7.22073283800006,11.6,7.80604104899999));
#244698=CARTESIAN_POINT('Ctrl Pts',(-7.22257414400006,15.2,7.80726591199999));
#244699=CARTESIAN_POINT('Ctrl Pts',(-7.22257414400006,11.6,7.80726591199999));
#244700=CARTESIAN_POINT('Ctrl Pts',(-7.22442207200006,15.2,7.80849282399998));
#244701=CARTESIAN_POINT('Ctrl Pts',(-7.22442207200006,11.6,7.80849282399998));
#244702=CARTESIAN_POINT('Ctrl Pts',(-7.22627661400006,15.2,7.80972176699999));
#244703=CARTESIAN_POINT('Ctrl Pts',(-7.22627661400006,11.6,7.80972176699999));
#244704=CARTESIAN_POINT('Ctrl Pts',(-7.22813776800006,15.2,7.81095272699999));
#244705=CARTESIAN_POINT('Ctrl Pts',(-7.22813776800006,11.6,7.81095272699999));
#244706=CARTESIAN_POINT('Ctrl Pts',(-7.23000552500006,15.2,7.81218568699998));
#244707=CARTESIAN_POINT('Ctrl Pts',(-7.23000552500006,11.6,7.81218568699998));
#244708=CARTESIAN_POINT('Ctrl Pts',(-7.23187988200006,15.2,7.81342063099999));
#244709=CARTESIAN_POINT('Ctrl Pts',(-7.23187988200006,11.6,7.81342063099999));
#244710=CARTESIAN_POINT('Ctrl Pts',(-7.23376083100006,15.2,7.81465754299998));
#244711=CARTESIAN_POINT('Ctrl Pts',(-7.23376083100006,11.6,7.81465754299998));
#244712=CARTESIAN_POINT('Ctrl Pts',(-7.23564836800006,15.2,7.81589640599999));
#244713=CARTESIAN_POINT('Ctrl Pts',(-7.23564836800006,11.6,7.81589640599999));
#244714=CARTESIAN_POINT('Ctrl Pts',(-7.23754248700006,15.2,7.81713720599999));
#244715=CARTESIAN_POINT('Ctrl Pts',(-7.23754248700006,11.6,7.81713720599999));
#244716=CARTESIAN_POINT('Ctrl Pts',(-7.23944318300005,15.2,7.81837992399999));
#244717=CARTESIAN_POINT('Ctrl Pts',(-7.23944318300005,11.6,7.81837992399999));
#244718=CARTESIAN_POINT('Ctrl Pts',(-7.24135045000006,15.2,7.81962454799999));
#244719=CARTESIAN_POINT('Ctrl Pts',(-7.24135045000006,11.6,7.81962454799999));
#244720=CARTESIAN_POINT('Ctrl Pts',(-7.24326428200006,15.2,7.82087105799998));
#244721=CARTESIAN_POINT('Ctrl Pts',(-7.24326428200006,11.6,7.82087105799998));
#244722=CARTESIAN_POINT('Ctrl Pts',(-7.24518467300006,15.2,7.82211944199998));
#244723=CARTESIAN_POINT('Ctrl Pts',(-7.24518467300006,11.6,7.82211944199998));
#244724=CARTESIAN_POINT('Ctrl Pts',(-7.24711162000006,15.2,7.82336968199999));
#244725=CARTESIAN_POINT('Ctrl Pts',(-7.24711162000006,11.6,7.82336968199999));
#244726=CARTESIAN_POINT('Ctrl Pts',(-7.24904511400006,15.2,7.82462176199999));
#244727=CARTESIAN_POINT('Ctrl Pts',(-7.24904511400006,11.6,7.82462176199999));
#244728=CARTESIAN_POINT('Ctrl Pts',(-7.25098515300005,15.2,7.82587566899998));
#244729=CARTESIAN_POINT('Ctrl Pts',(-7.25098515300005,11.6,7.82587566899998));
#244730=CARTESIAN_POINT('Ctrl Pts',(-7.25293172800006,15.2,7.82713138499999));
#244731=CARTESIAN_POINT('Ctrl Pts',(-7.25293172800006,11.6,7.82713138499999));
#244732=CARTESIAN_POINT('Ctrl Pts',(-7.25488483700006,15.2,7.82838889399999));
#244733=CARTESIAN_POINT('Ctrl Pts',(-7.25488483700006,11.6,7.82838889399999));
#244734=CARTESIAN_POINT('Ctrl Pts',(-7.25684447100006,15.2,7.82964818299998));
#244735=CARTESIAN_POINT('Ctrl Pts',(-7.25684447100006,11.6,7.82964818299998));
#244736=CARTESIAN_POINT('Ctrl Pts',(-7.25881062600005,15.2,7.83090923599998));
#244737=CARTESIAN_POINT('Ctrl Pts',(-7.25881062600005,11.6,7.83090923599998));
#244738=CARTESIAN_POINT('Ctrl Pts',(-7.26078329800006,15.2,7.83217203499999));
#244739=CARTESIAN_POINT('Ctrl Pts',(-7.26078329800006,11.6,7.83217203499999));
#244740=CARTESIAN_POINT('Ctrl Pts',(-7.26276247900006,15.2,7.83343656799998));
#244741=CARTESIAN_POINT('Ctrl Pts',(-7.26276247900006,11.6,7.83343656799998));
#244742=CARTESIAN_POINT('Ctrl Pts',(-7.26474816500006,15.2,7.83470281899999));
#244743=CARTESIAN_POINT('Ctrl Pts',(-7.26474816500006,11.6,7.83470281899999));
#244744=CARTESIAN_POINT('Ctrl Pts',(-7.26674035000006,15.2,7.83597076999998));
#244745=CARTESIAN_POINT('Ctrl Pts',(-7.26674035000006,11.6,7.83597076999998));
#244746=CARTESIAN_POINT('Ctrl Pts',(-7.26873902900006,15.2,7.83724040899998));
#244747=CARTESIAN_POINT('Ctrl Pts',(-7.26873902900006,11.6,7.83724040899998));
#244748=CARTESIAN_POINT('Ctrl Pts',(-7.27074419600005,15.2,7.83851171899999));
#244749=CARTESIAN_POINT('Ctrl Pts',(-7.27074419600005,11.6,7.83851171899999));
#244750=CARTESIAN_POINT('Ctrl Pts',(-7.27275584500005,15.2,7.83978468699999));
#244751=CARTESIAN_POINT('Ctrl Pts',(-7.27275584500005,11.6,7.83978468699999));
#244752=CARTESIAN_POINT('Ctrl Pts',(-7.27477397200006,15.2,7.84105929599999));
#244753=CARTESIAN_POINT('Ctrl Pts',(-7.27477397200006,11.6,7.84105929599999));
#244754=CARTESIAN_POINT('Ctrl Pts',(-7.27679857000005,15.2,7.84233553099998));
#244755=CARTESIAN_POINT('Ctrl Pts',(-7.27679857000005,11.6,7.84233553099998));
#244756=CARTESIAN_POINT('Ctrl Pts',(-7.27882963600006,15.2,7.84361337899998));
#244757=CARTESIAN_POINT('Ctrl Pts',(-7.27882963600006,11.6,7.84361337899998));
#244758=CARTESIAN_POINT('Ctrl Pts',(-7.28086716200006,15.2,7.84489282299998));
#244759=CARTESIAN_POINT('Ctrl Pts',(-7.28086716200006,11.6,7.84489282299998));
#244760=CARTESIAN_POINT('Ctrl Pts',(-7.28291114200006,15.2,7.84617384799999));
#244761=CARTESIAN_POINT('Ctrl Pts',(-7.28291114200006,11.6,7.84617384799999));
#244762=CARTESIAN_POINT('Ctrl Pts',(-7.28496157300006,15.2,7.84745644199998));
#244763=CARTESIAN_POINT('Ctrl Pts',(-7.28496157300006,11.6,7.84745644199998));
#244764=CARTESIAN_POINT('Ctrl Pts',(-7.28701844900006,15.2,7.84874058699998));
#244765=CARTESIAN_POINT('Ctrl Pts',(-7.28701844900006,11.6,7.84874058699998));
#244766=CARTESIAN_POINT('Ctrl Pts',(-7.28908176300005,15.2,7.85002626999999));
#244767=CARTESIAN_POINT('Ctrl Pts',(-7.28908176300005,11.6,7.85002626999999));
#244768=CARTESIAN_POINT('Ctrl Pts',(-7.29115151200006,15.2,7.85131347699998));
#244769=CARTESIAN_POINT('Ctrl Pts',(-7.29115151200006,11.6,7.85131347699998));
#244770=CARTESIAN_POINT('Ctrl Pts',(-7.29322768800006,15.2,7.85260219099998));
#244771=CARTESIAN_POINT('Ctrl Pts',(-7.29322768800006,11.6,7.85260219099998));
#244772=CARTESIAN_POINT('Ctrl Pts',(-7.29531028700006,15.2,7.85389239899998));
#244773=CARTESIAN_POINT('Ctrl Pts',(-7.29531028700006,11.6,7.85389239899998));
#244774=CARTESIAN_POINT('Ctrl Pts',(-7.29739930400005,15.2,7.85518408599999));
#244775=CARTESIAN_POINT('Ctrl Pts',(-7.29739930400005,11.6,7.85518408599999));
#244776=CARTESIAN_POINT('Ctrl Pts',(-7.29949473300006,15.2,7.85647723899999));
#244777=CARTESIAN_POINT('Ctrl Pts',(-7.29949473300006,11.6,7.85647723899999));
#244778=CARTESIAN_POINT('Ctrl Pts',(-7.30159656800006,15.2,7.85777184099998));
#244779=CARTESIAN_POINT('Ctrl Pts',(-7.30159656800006,11.6,7.85777184099998));
#244780=CARTESIAN_POINT('Ctrl Pts',(-7.30370480500006,15.2,7.85906787899999));
#244781=CARTESIAN_POINT('Ctrl Pts',(-7.30370480500006,11.6,7.85906787899999));
#244782=CARTESIAN_POINT('Ctrl Pts',(-7.30581943700006,15.2,7.86036533899999));
#244783=CARTESIAN_POINT('Ctrl Pts',(-7.30581943700006,11.6,7.86036533899999));
#244784=CARTESIAN_POINT('Ctrl Pts',(-7.30794046000006,15.2,7.86166420599999));
#244785=CARTESIAN_POINT('Ctrl Pts',(-7.30794046000006,11.6,7.86166420599999));
#244786=CARTESIAN_POINT('Ctrl Pts',(-7.31006786800006,15.2,7.86296446599999));
#244787=CARTESIAN_POINT('Ctrl Pts',(-7.31006786800006,11.6,7.86296446599999));
#244788=CARTESIAN_POINT('Ctrl Pts',(-7.31220165500006,15.2,7.86426610399998));
#244789=CARTESIAN_POINT('Ctrl Pts',(-7.31220165500006,11.6,7.86426610399998));
#244790=CARTESIAN_POINT('Ctrl Pts',(-7.31434181800006,15.2,7.86556910899999));
#244791=CARTESIAN_POINT('Ctrl Pts',(-7.31434181800006,11.6,7.86556910899999));
#244792=CARTESIAN_POINT('Ctrl Pts',(-7.31648834800006,15.2,7.86687346199999));
#244793=CARTESIAN_POINT('Ctrl Pts',(-7.31648834800006,11.6,7.86687346199999));
#244794=CARTESIAN_POINT('Ctrl Pts',(-7.31864124200006,15.2,7.86817915199999));
#244795=CARTESIAN_POINT('Ctrl Pts',(-7.31864124200006,11.6,7.86817915199999));
#244796=CARTESIAN_POINT('Ctrl Pts',(-7.32080049400006,15.2,7.86948616399999));
#244797=CARTESIAN_POINT('Ctrl Pts',(-7.32080049400006,11.6,7.86948616399999));
#244798=CARTESIAN_POINT('Ctrl Pts',(-7.32296610000006,15.2,7.87079448499998));
#244799=CARTESIAN_POINT('Ctrl Pts',(-7.32296610000006,11.6,7.87079448499998));
#244800=CARTESIAN_POINT('Ctrl Pts',(-7.32513805400006,15.2,7.87210409899998));
#244801=CARTESIAN_POINT('Ctrl Pts',(-7.32513805400006,11.6,7.87210409899998));
#244802=CARTESIAN_POINT('Ctrl Pts',(-7.32731634900006,15.2,7.87341499399999));
#244803=CARTESIAN_POINT('Ctrl Pts',(-7.32731634900006,11.6,7.87341499399999));
#244804=CARTESIAN_POINT('Ctrl Pts',(-7.32950098000006,15.2,7.87472715499998));
#244805=CARTESIAN_POINT('Ctrl Pts',(-7.32950098000006,11.6,7.87472715499998));
#244806=CARTESIAN_POINT('Ctrl Pts',(-7.33169194400006,15.2,7.87604056899998));
#244807=CARTESIAN_POINT('Ctrl Pts',(-7.33169194400006,11.6,7.87604056899998));
#244808=CARTESIAN_POINT('Ctrl Pts',(-7.33388923300006,15.2,7.87735522199998));
#244809=CARTESIAN_POINT('Ctrl Pts',(-7.33388923300006,11.6,7.87735522199998));
#244810=CARTESIAN_POINT('Ctrl Pts',(-7.33609284400006,15.2,7.87867109999999));
#244811=CARTESIAN_POINT('Ctrl Pts',(-7.33609284400006,11.6,7.87867109999999));
#244812=CARTESIAN_POINT('Ctrl Pts',(-7.33830277000005,15.2,7.87998818899998));
#244813=CARTESIAN_POINT('Ctrl Pts',(-7.33830277000005,11.6,7.87998818899998));
#244814=CARTESIAN_POINT('Ctrl Pts',(-7.34051900600006,15.2,7.88130647499998));
#244815=CARTESIAN_POINT('Ctrl Pts',(-7.34051900600006,11.6,7.88130647499998));
#244816=CARTESIAN_POINT('Ctrl Pts',(-7.34274154700006,15.2,7.88262594599999));
#244817=CARTESIAN_POINT('Ctrl Pts',(-7.34274154700006,11.6,7.88262594599999));
#244818=CARTESIAN_POINT('Ctrl Pts',(-7.34497038800006,15.2,7.88394658699998));
#244819=CARTESIAN_POINT('Ctrl Pts',(-7.34497038800006,11.6,7.88394658699998));
#244820=CARTESIAN_POINT('Ctrl Pts',(-7.34720552300006,15.2,7.88526838399999));
#244821=CARTESIAN_POINT('Ctrl Pts',(-7.34720552300006,11.6,7.88526838399999));
#244822=CARTESIAN_POINT('Ctrl Pts',(-7.34944694700006,15.2,7.88659132499999));
#244823=CARTESIAN_POINT('Ctrl Pts',(-7.34944694700006,11.6,7.88659132499999));
#244824=CARTESIAN_POINT('Ctrl Pts',(-7.35169465500006,15.2,7.88791539599998));
#244825=CARTESIAN_POINT('Ctrl Pts',(-7.35169465500006,11.6,7.88791539599998));
#244826=CARTESIAN_POINT('Ctrl Pts',(-7.35394864100006,15.2,7.88924058299998));
#244827=CARTESIAN_POINT('Ctrl Pts',(-7.35394864100006,11.6,7.88924058299998));
#244828=CARTESIAN_POINT('Ctrl Pts',(-7.35620890000006,15.2,7.89056687299999));
#244829=CARTESIAN_POINT('Ctrl Pts',(-7.35620890000006,11.6,7.89056687299999));
#244830=CARTESIAN_POINT('Ctrl Pts',(-7.35847542700006,15.2,7.89189425299998));
#244831=CARTESIAN_POINT('Ctrl Pts',(-7.35847542700006,11.6,7.89189425299998));
#244832=CARTESIAN_POINT('Ctrl Pts',(-7.36074821700006,15.2,7.89322270699999));
#244833=CARTESIAN_POINT('Ctrl Pts',(-7.36074821700006,11.6,7.89322270699999));
#244834=CARTESIAN_POINT('Ctrl Pts',(-7.36302726400006,15.2,7.89455222599998));
#244835=CARTESIAN_POINT('Ctrl Pts',(-7.36302726400006,11.6,7.89455222599998));
#244836=CARTESIAN_POINT('Ctrl Pts',(-7.36531256300006,15.2,7.89588279499998));
#244837=CARTESIAN_POINT('Ctrl Pts',(-7.36531256300006,11.6,7.89588279499998));
#244838=CARTESIAN_POINT('Ctrl Pts',(-7.36760410800006,15.2,7.89721439899999));
#244839=CARTESIAN_POINT('Ctrl Pts',(-7.36760410800006,11.6,7.89721439899999));
#244840=CARTESIAN_POINT('Ctrl Pts',(-7.36990189600006,15.2,7.89854702799998));
#244841=CARTESIAN_POINT('Ctrl Pts',(-7.36990189600006,11.6,7.89854702799998));
#244842=CARTESIAN_POINT('Ctrl Pts',(-7.37220591900006,15.2,7.89988066499999));
#244843=CARTESIAN_POINT('Ctrl Pts',(-7.37220591900006,11.6,7.89988066499999));
#244844=CARTESIAN_POINT('Ctrl Pts',(-7.37451617400006,15.2,7.90121529999999));
#244845=CARTESIAN_POINT('Ctrl Pts',(-7.37451617400006,11.6,7.90121529999999));
#244846=CARTESIAN_POINT('Ctrl Pts',(-7.37683265400006,15.2,7.90255091899999));
#244847=CARTESIAN_POINT('Ctrl Pts',(-7.37683265400006,11.6,7.90255091899999));
#244848=CARTESIAN_POINT('Ctrl Pts',(-7.37915535500006,15.2,7.90388750999998));
#244849=CARTESIAN_POINT('Ctrl Pts',(-7.37915535500006,11.6,7.90388750999998));
#244850=CARTESIAN_POINT('Ctrl Pts',(-7.38148427100006,15.2,7.90522505699998));
#244851=CARTESIAN_POINT('Ctrl Pts',(-7.38148427100006,11.6,7.90522505699998));
#244852=CARTESIAN_POINT('Ctrl Pts',(-7.38381939700006,15.2,7.90656354999999));
#244853=CARTESIAN_POINT('Ctrl Pts',(-7.38381939700006,11.6,7.90656354999999));
#244854=CARTESIAN_POINT('Ctrl Pts',(-7.38616072800006,15.2,7.90790297499999));
#244855=CARTESIAN_POINT('Ctrl Pts',(-7.38616072800006,11.6,7.90790297499999));
#244856=CARTESIAN_POINT('Ctrl Pts',(-7.38850825800006,15.2,7.90924331999998));
#244857=CARTESIAN_POINT('Ctrl Pts',(-7.38850825800006,11.6,7.90924331999998));
#244858=CARTESIAN_POINT('Ctrl Pts',(-7.39086198300006,15.2,7.91058456999998));
#244859=CARTESIAN_POINT('Ctrl Pts',(-7.39086198300006,11.6,7.91058456999998));
#244860=CARTESIAN_POINT('Ctrl Pts',(-7.39322189600006,15.2,7.91192671399998));
#244861=CARTESIAN_POINT('Ctrl Pts',(-7.39322189600006,11.6,7.91192671399998));
#244862=CARTESIAN_POINT('Ctrl Pts',(-7.39558799400006,15.2,7.91326973999999));
#244863=CARTESIAN_POINT('Ctrl Pts',(-7.39558799400006,11.6,7.91326973999999));
#244864=CARTESIAN_POINT('Ctrl Pts',(-7.39796027100006,15.2,7.91461363299998));
#244865=CARTESIAN_POINT('Ctrl Pts',(-7.39796027100006,11.6,7.91461363299998));
#244866=CARTESIAN_POINT('Ctrl Pts',(-7.40033872100006,15.2,7.91595838099998));
#244867=CARTESIAN_POINT('Ctrl Pts',(-7.40033872100006,11.6,7.91595838099998));
#244868=CARTESIAN_POINT('Ctrl Pts',(-7.40272333900006,15.2,7.91730397299999));
#244869=CARTESIAN_POINT('Ctrl Pts',(-7.40272333900006,11.6,7.91730397299999));
#244870=CARTESIAN_POINT('Ctrl Pts',(-7.40511412000005,15.2,7.91865039499999));
#244871=CARTESIAN_POINT('Ctrl Pts',(-7.40511412000005,11.6,7.91865039499999));
#244872=CARTESIAN_POINT('Ctrl Pts',(-7.40751105900006,15.2,7.91999763299999));
#244873=CARTESIAN_POINT('Ctrl Pts',(-7.40751105900006,11.6,7.91999763299999));
#244874=CARTESIAN_POINT('Ctrl Pts',(-7.40991415200006,15.2,7.92134567699998));
#244875=CARTESIAN_POINT('Ctrl Pts',(-7.40991415200006,11.6,7.92134567699998));
#244876=CARTESIAN_POINT('Ctrl Pts',(-7.41232339100006,15.2,7.92269451299998));
#244877=CARTESIAN_POINT('Ctrl Pts',(-7.41232339100006,11.6,7.92269451299998));
#244878=CARTESIAN_POINT('Ctrl Pts',(-7.41473877300006,15.2,7.92404412999999));
#244879=CARTESIAN_POINT('Ctrl Pts',(-7.41473877300006,11.6,7.92404412999999));
#244880=CARTESIAN_POINT('Ctrl Pts',(-7.41716029100006,15.2,7.92539451399998));
#244881=CARTESIAN_POINT('Ctrl Pts',(-7.41716029100006,11.6,7.92539451399998));
#244882=CARTESIAN_POINT('Ctrl Pts',(-7.41958794200006,15.2,7.92674565199999));
#244883=CARTESIAN_POINT('Ctrl Pts',(-7.41958794200006,11.6,7.92674565199999));
#244884=CARTESIAN_POINT('Ctrl Pts',(-7.42202171900006,15.2,7.92809753399998));
#244885=CARTESIAN_POINT('Ctrl Pts',(-7.42202171900006,11.6,7.92809753399998));
#244886=CARTESIAN_POINT('Ctrl Pts',(-7.42446161900006,15.2,7.92945014599999));
#244887=CARTESIAN_POINT('Ctrl Pts',(-7.42446161900006,11.6,7.92945014599999));
#244888=CARTESIAN_POINT('Ctrl Pts',(-7.42690763400006,15.2,7.93080347599999));
#244889=CARTESIAN_POINT('Ctrl Pts',(-7.42690763400006,11.6,7.93080347599999));
#244890=CARTESIAN_POINT('Ctrl Pts',(-7.42935976100005,15.2,7.93215751199998));
#244891=CARTESIAN_POINT('Ctrl Pts',(-7.42935976100005,11.6,7.93215751199998));
#244892=CARTESIAN_POINT('Ctrl Pts',(-7.43181799400006,15.2,7.93351224099998));
#244893=CARTESIAN_POINT('Ctrl Pts',(-7.43181799400006,11.6,7.93351224099998));
#244894=CARTESIAN_POINT('Ctrl Pts',(-7.43428232700006,15.2,7.93486765199999));
#244895=CARTESIAN_POINT('Ctrl Pts',(-7.43428232700006,11.6,7.93486765199999));
#244896=CARTESIAN_POINT('Ctrl Pts',(-7.43675275700006,15.2,7.93622373199998));
#244897=CARTESIAN_POINT('Ctrl Pts',(-7.43675275700006,11.6,7.93622373199998));
#244898=CARTESIAN_POINT('Ctrl Pts',(-7.43922927800006,15.2,7.93758046899999));
#244899=CARTESIAN_POINT('Ctrl Pts',(-7.43922927800006,11.6,7.93758046899999));
#244900=CARTESIAN_POINT('Ctrl Pts',(-7.44171188300006,15.2,7.93893784999998));
#244901=CARTESIAN_POINT('Ctrl Pts',(-7.44171188300006,11.6,7.93893784999998));
#244902=CARTESIAN_POINT('Ctrl Pts',(-7.44420057000006,15.2,7.94029586499998));
#244903=CARTESIAN_POINT('Ctrl Pts',(-7.44420057000006,11.6,7.94029586499998));
#244904=CARTESIAN_POINT('Ctrl Pts',(-7.44669533100006,15.2,7.94165450099998));
#244905=CARTESIAN_POINT('Ctrl Pts',(-7.44669533100006,11.6,7.94165450099998));
#244906=CARTESIAN_POINT('Ctrl Pts',(-7.44919616200006,15.2,7.94301374399998));
#244907=CARTESIAN_POINT('Ctrl Pts',(-7.44919616200006,11.6,7.94301374399998));
#244908=CARTESIAN_POINT('Ctrl Pts',(-7.45170305800006,15.2,7.94437358599998));
#244909=CARTESIAN_POINT('Ctrl Pts',(-7.45170305800006,11.6,7.94437358599998));
#244910=CARTESIAN_POINT('Ctrl Pts',(-7.45421601400006,15.2,7.94573401099999));
#244911=CARTESIAN_POINT('Ctrl Pts',(-7.45421601400006,11.6,7.94573401099999));
#244912=CARTESIAN_POINT('Ctrl Pts',(-7.45673502500006,15.2,7.94709500999998));
#244913=CARTESIAN_POINT('Ctrl Pts',(-7.45673502500006,11.6,7.94709500999998));
#244914=CARTESIAN_POINT('Ctrl Pts',(-7.45926008500006,15.2,7.94845657099999));
#244915=CARTESIAN_POINT('Ctrl Pts',(-7.45926008500006,11.6,7.94845657099999));
#244916=CARTESIAN_POINT('Ctrl Pts',(-7.46179119000006,15.2,7.94981867899998));
#244917=CARTESIAN_POINT('Ctrl Pts',(-7.46179119000006,11.6,7.94981867899998));
#244918=CARTESIAN_POINT('Ctrl Pts',(-7.46432833400006,15.2,7.95118132499999));
#244919=CARTESIAN_POINT('Ctrl Pts',(-7.46432833400006,11.6,7.95118132499999));
#244920=CARTESIAN_POINT('Ctrl Pts',(-7.46687151300006,15.2,7.95254449699998));
#244921=CARTESIAN_POINT('Ctrl Pts',(-7.46687151300006,11.6,7.95254449699998));
#244922=CARTESIAN_POINT('Ctrl Pts',(-7.46942072000006,15.2,7.95390818299998));
#244923=CARTESIAN_POINT('Ctrl Pts',(-7.46942072000006,11.6,7.95390818299998));
#244924=CARTESIAN_POINT('Ctrl Pts',(-7.47197595100006,15.2,7.95527237099999));
#244925=CARTESIAN_POINT('Ctrl Pts',(-7.47197595100006,11.6,7.95527237099999));
#244926=CARTESIAN_POINT('Ctrl Pts',(-7.47453720200006,15.2,7.95663704999999));
#244927=CARTESIAN_POINT('Ctrl Pts',(-7.47453720200006,11.6,7.95663704999999));
#244928=CARTESIAN_POINT('Ctrl Pts',(-7.47710446500006,15.2,7.95800220799999));
#244929=CARTESIAN_POINT('Ctrl Pts',(-7.47710446500006,11.6,7.95800220799999));
#244930=CARTESIAN_POINT('Ctrl Pts',(-7.47967773800006,15.2,7.95936783099998));
#244931=CARTESIAN_POINT('Ctrl Pts',(-7.47967773800006,11.6,7.95936783099998));
#244932=CARTESIAN_POINT('Ctrl Pts',(-7.48225701500006,15.2,7.96073391199998));
#244933=CARTESIAN_POINT('Ctrl Pts',(-7.48225701500006,11.6,7.96073391199998));
#244934=CARTESIAN_POINT('Ctrl Pts',(-7.48484228800006,15.2,7.96210043599999));
#244935=CARTESIAN_POINT('Ctrl Pts',(-7.48484228800006,11.6,7.96210043599999));
#244936=CARTESIAN_POINT('Ctrl Pts',(-7.48743355700006,15.2,7.96346739199999));
#244937=CARTESIAN_POINT('Ctrl Pts',(-7.48743355700006,11.6,7.96346739199999));
#244938=CARTESIAN_POINT('Ctrl Pts',(-7.49003081300006,15.2,7.96483476999998));
#244939=CARTESIAN_POINT('Ctrl Pts',(-7.49003081300006,11.6,7.96483476999998));
#244940=CARTESIAN_POINT('Ctrl Pts',(-7.49263405300006,15.2,7.96620255599999));
#244941=CARTESIAN_POINT('Ctrl Pts',(-7.49263405300006,11.6,7.96620255599999));
#244942=CARTESIAN_POINT('Ctrl Pts',(-7.49524327100006,15.2,7.96757074199999));
#244943=CARTESIAN_POINT('Ctrl Pts',(-7.49524327100006,11.6,7.96757074199999));
#244944=CARTESIAN_POINT('Ctrl Pts',(-7.49785846200006,15.2,7.96893931299999));
#244945=CARTESIAN_POINT('Ctrl Pts',(-7.49785846200006,11.6,7.96893931299999));
#244946=CARTESIAN_POINT('Ctrl Pts',(-7.50047962100006,15.2,7.97030825999999));
#244947=CARTESIAN_POINT('Ctrl Pts',(-7.50047962100006,11.6,7.97030825999999));
#244948=CARTESIAN_POINT('Ctrl Pts',(-7.50310674300006,15.2,7.97167757099999));
#244949=CARTESIAN_POINT('Ctrl Pts',(-7.50310674300006,11.6,7.97167757099999));
#244950=CARTESIAN_POINT('Ctrl Pts',(-7.50573982300006,15.2,7.97304723499998));
#244951=CARTESIAN_POINT('Ctrl Pts',(-7.50573982300006,11.6,7.97304723499998));
#244952=CARTESIAN_POINT('Ctrl Pts',(-7.50837885500006,15.2,7.97441723899999));
#244953=CARTESIAN_POINT('Ctrl Pts',(-7.50837885500006,11.6,7.97441723899999));
#244954=CARTESIAN_POINT('Ctrl Pts',(-7.51102383600006,15.2,7.97578757299998));
#244955=CARTESIAN_POINT('Ctrl Pts',(-7.51102383600006,11.6,7.97578757299998));
#244956=CARTESIAN_POINT('Ctrl Pts',(-7.51367475900006,15.2,7.97715822699999));
#244957=CARTESIAN_POINT('Ctrl Pts',(-7.51367475900006,11.6,7.97715822699999));
#244958=CARTESIAN_POINT('Ctrl Pts',(-7.51633162000005,15.2,7.97852918799999));
#244959=CARTESIAN_POINT('Ctrl Pts',(-7.51633162000005,11.6,7.97852918799999));
#244960=CARTESIAN_POINT('Ctrl Pts',(-7.51899441200005,15.2,7.97990044499999));
#244961=CARTESIAN_POINT('Ctrl Pts',(-7.51899441200005,11.6,7.97990044499999));
#244962=CARTESIAN_POINT('Ctrl Pts',(-7.52166313300006,15.2,7.98127198799998));
#244963=CARTESIAN_POINT('Ctrl Pts',(-7.52166313300006,11.6,7.98127198799998));
#244964=CARTESIAN_POINT('Ctrl Pts',(-7.52433777600006,15.2,7.98264380499998));
#244965=CARTESIAN_POINT('Ctrl Pts',(-7.52433777600006,11.6,7.98264380499998));
#244966=CARTESIAN_POINT('Ctrl Pts',(-7.52701833700005,15.2,7.98401588399998));
#244967=CARTESIAN_POINT('Ctrl Pts',(-7.52701833700005,11.6,7.98401588399998));
#244968=CARTESIAN_POINT('Ctrl Pts',(-7.52970481000006,15.2,7.98538821699999));
#244969=CARTESIAN_POINT('Ctrl Pts',(-7.52970481000006,11.6,7.98538821699999));
#244970=CARTESIAN_POINT('Ctrl Pts',(-7.53239719100005,15.2,7.98676078899998));
#244971=CARTESIAN_POINT('Ctrl Pts',(-7.53239719100005,11.6,7.98676078899998));
#244972=CARTESIAN_POINT('Ctrl Pts',(-7.53509547300006,15.2,7.98813359199999));
#244973=CARTESIAN_POINT('Ctrl Pts',(-7.53509547300006,11.6,7.98813359199999));
#244974=CARTESIAN_POINT('Ctrl Pts',(-7.53779965400006,15.2,7.98950661499998));
#244975=CARTESIAN_POINT('Ctrl Pts',(-7.53779965400006,11.6,7.98950661499998));
#244976=CARTESIAN_POINT('Ctrl Pts',(-7.54050972500006,15.2,7.99087984499998));
#244977=CARTESIAN_POINT('Ctrl Pts',(-7.54050972500006,11.6,7.99087984499998));
#244978=CARTESIAN_POINT('Ctrl Pts',(-7.54322568500006,15.2,7.99225327099998));
#244979=CARTESIAN_POINT('Ctrl Pts',(-7.54322568500006,11.6,7.99225327099998));
#244980=CARTESIAN_POINT('Ctrl Pts',(-7.54594752700006,15.2,7.99362688499999));
#244981=CARTESIAN_POINT('Ctrl Pts',(-7.54594752700006,11.6,7.99362688499999));
#244982=CARTESIAN_POINT('Ctrl Pts',(-7.54867524600006,15.2,7.99500067299999));
#244983=CARTESIAN_POINT('Ctrl Pts',(-7.54867524600006,11.6,7.99500067299999));
#244984=CARTESIAN_POINT('Ctrl Pts',(-7.55140883700006,15.2,7.99637462699998));
#244985=CARTESIAN_POINT('Ctrl Pts',(-7.55140883700006,11.6,7.99637462699998));
#244986=CARTESIAN_POINT('Ctrl Pts',(-7.55414829500006,15.2,7.99774873399999));
#244987=CARTESIAN_POINT('Ctrl Pts',(-7.55414829500006,11.6,7.99774873399999));
#244988=CARTESIAN_POINT('Ctrl Pts',(-7.55689361600006,15.2,7.99912298399998));
#244989=CARTESIAN_POINT('Ctrl Pts',(-7.55689361600006,11.6,7.99912298399998));
#244990=CARTESIAN_POINT('Ctrl Pts',(-7.55964479300006,15.2,8.00049736599998));
#244991=CARTESIAN_POINT('Ctrl Pts',(-7.55964479300006,11.6,8.00049736599998));
#244992=CARTESIAN_POINT('Ctrl Pts',(-7.56240182300005,15.2,8.00187187099999));
#244993=CARTESIAN_POINT('Ctrl Pts',(-7.56240182300005,11.6,8.00187187099999));
#244994=CARTESIAN_POINT('Ctrl Pts',(-7.56516470000006,15.2,8.00324648399998));
#244995=CARTESIAN_POINT('Ctrl Pts',(-7.56516470000006,11.6,8.00324648399998));
#244996=CARTESIAN_POINT('Ctrl Pts',(-7.56793341800006,15.2,8.00462119899999));
#244997=CARTESIAN_POINT('Ctrl Pts',(-7.56793341800006,11.6,8.00462119899999));
#244998=CARTESIAN_POINT('Ctrl Pts',(-7.57070797500005,15.2,8.00599600399998));
#244999=CARTESIAN_POINT('Ctrl Pts',(-7.57070797500005,11.6,8.00599600399998));
#245000=CARTESIAN_POINT('Ctrl Pts',(-7.57348836300006,15.2,8.00737088699999));
#245001=CARTESIAN_POINT('Ctrl Pts',(-7.57348836300006,11.6,8.00737088699999));
#245002=CARTESIAN_POINT('Ctrl Pts',(-7.57627457800006,15.2,8.00874583799999));
#245003=CARTESIAN_POINT('Ctrl Pts',(-7.57627457800006,11.6,8.00874583799999));
#245004=CARTESIAN_POINT('Ctrl Pts',(-7.57906661600006,15.2,8.01012084699998));
#245005=CARTESIAN_POINT('Ctrl Pts',(-7.57906661600006,11.6,8.01012084699998));
#245006=CARTESIAN_POINT('Ctrl Pts',(-7.58186447000006,15.2,8.01149590299998));
#245007=CARTESIAN_POINT('Ctrl Pts',(-7.58186447000006,11.6,8.01149590299998));
#245008=CARTESIAN_POINT('Ctrl Pts',(-7.58466813600006,15.2,8.01287099699999));
#245009=CARTESIAN_POINT('Ctrl Pts',(-7.58466813600006,11.6,8.01287099699999));
#245010=CARTESIAN_POINT('Ctrl Pts',(-7.58747761100006,15.2,8.01424611599998));
#245011=CARTESIAN_POINT('Ctrl Pts',(-7.58747761100006,11.6,8.01424611599998));
#245012=CARTESIAN_POINT('Ctrl Pts',(-7.59029288700006,15.2,8.01562125099998));
#245013=CARTESIAN_POINT('Ctrl Pts',(-7.59029288700006,11.6,8.01562125099998));
#245014=CARTESIAN_POINT('Ctrl Pts',(-7.59311396000006,15.2,8.01699639099999));
#245015=CARTESIAN_POINT('Ctrl Pts',(-7.59311396000006,11.6,8.01699639099999));
#245016=CARTESIAN_POINT('Ctrl Pts',(-7.59594082600006,15.2,8.01837152699999));
#245017=CARTESIAN_POINT('Ctrl Pts',(-7.59594082600006,11.6,8.01837152699999));
#245018=CARTESIAN_POINT('Ctrl Pts',(-7.59877347800006,15.2,8.01974664699999));
#245019=CARTESIAN_POINT('Ctrl Pts',(-7.59877347800006,11.6,8.01974664699999));
#245020=CARTESIAN_POINT('Ctrl Pts',(-7.60161191400006,15.2,8.02112174099998));
#245021=CARTESIAN_POINT('Ctrl Pts',(-7.60161191400006,11.6,8.02112174099998));
#245022=CARTESIAN_POINT('Ctrl Pts',(-7.60445612600006,15.2,8.02249679899998));
#245023=CARTESIAN_POINT('Ctrl Pts',(-7.60445612600006,11.6,8.02249679899998));
#245024=CARTESIAN_POINT('Ctrl Pts',(-7.60730611100006,15.2,8.02387180999999));
#245025=CARTESIAN_POINT('Ctrl Pts',(-7.60730611100006,11.6,8.02387180999999));
#245026=CARTESIAN_POINT('Ctrl Pts',(-7.61016186300005,15.2,8.02524676499999));
#245027=CARTESIAN_POINT('Ctrl Pts',(-7.61016186300005,11.6,8.02524676499999));
#245028=CARTESIAN_POINT('Ctrl Pts',(-7.61302337700006,15.2,8.02662165399998));
#245029=CARTESIAN_POINT('Ctrl Pts',(-7.61302337700006,11.6,8.02662165399998));
#245030=CARTESIAN_POINT('Ctrl Pts',(-7.61589065000006,15.2,8.02799646399999));
#245031=CARTESIAN_POINT('Ctrl Pts',(-7.61589065000006,11.6,8.02799646399999));
#245032=CARTESIAN_POINT('Ctrl Pts',(-7.61876367500006,15.2,8.02937118799999));
#245033=CARTESIAN_POINT('Ctrl Pts',(-7.61876367500006,11.6,8.02937118799999));
#245034=CARTESIAN_POINT('Ctrl Pts',(-7.62164244700006,15.2,8.03074581399999));
#245035=CARTESIAN_POINT('Ctrl Pts',(-7.62164244700006,11.6,8.03074581399999));
#245036=CARTESIAN_POINT('Ctrl Pts',(-7.62452696100006,15.2,8.03212033199999));
#245037=CARTESIAN_POINT('Ctrl Pts',(-7.62452696100006,11.6,8.03212033199999));
#245038=CARTESIAN_POINT('Ctrl Pts',(-7.62741721300006,15.2,8.03349473299999));
#245039=CARTESIAN_POINT('Ctrl Pts',(-7.62741721300006,11.6,8.03349473299999));
#245040=CARTESIAN_POINT('Ctrl Pts',(-7.63031319900006,15.2,8.03486900599999));
#245041=CARTESIAN_POINT('Ctrl Pts',(-7.63031319900006,11.6,8.03486900599999));
#245042=CARTESIAN_POINT('Ctrl Pts',(-7.63321491200006,15.2,8.03624313999999));
#245043=CARTESIAN_POINT('Ctrl Pts',(-7.63321491200006,11.6,8.03624313999999));
#245044=CARTESIAN_POINT('Ctrl Pts',(-7.63612234700006,15.2,8.03761712699998));
#245045=CARTESIAN_POINT('Ctrl Pts',(-7.63612234700006,11.6,8.03761712699998));
#245046=CARTESIAN_POINT('Ctrl Pts',(-7.63903550100006,15.2,8.03899095599999));
#245047=CARTESIAN_POINT('Ctrl Pts',(-7.63903550100006,11.6,8.03899095599999));
#245048=CARTESIAN_POINT('Ctrl Pts',(-7.64195436800006,15.2,8.04036461599999));
#245049=CARTESIAN_POINT('Ctrl Pts',(-7.64195436800006,11.6,8.04036461599999));
#245050=CARTESIAN_POINT('Ctrl Pts',(-7.64487894200006,15.2,8.04173809899999));
#245051=CARTESIAN_POINT('Ctrl Pts',(-7.64487894200006,11.6,8.04173809899999));
#245052=CARTESIAN_POINT('Ctrl Pts',(-7.64780922000006,15.2,8.04311139499998));
#245053=CARTESIAN_POINT('Ctrl Pts',(-7.64780922000006,11.6,8.04311139499998));
#245054=CARTESIAN_POINT('Ctrl Pts',(-7.65074519600006,15.2,8.04448449199998));
#245055=CARTESIAN_POINT('Ctrl Pts',(-7.65074519600006,11.6,8.04448449199998));
#245056=CARTESIAN_POINT('Ctrl Pts',(-7.65368686500006,15.2,8.04585738099998));
#245057=CARTESIAN_POINT('Ctrl Pts',(-7.65368686500006,11.6,8.04585738099998));
#245058=CARTESIAN_POINT('Ctrl Pts',(-7.65663422300006,15.2,8.04723005299999));
#245059=CARTESIAN_POINT('Ctrl Pts',(-7.65663422300006,11.6,8.04723005299999));
#245060=CARTESIAN_POINT('Ctrl Pts',(-7.65958726300005,15.2,8.04860249699999));
#245061=CARTESIAN_POINT('Ctrl Pts',(-7.65958726300005,11.6,8.04860249699999));
#245062=CARTESIAN_POINT('Ctrl Pts',(-7.66254598200005,15.2,8.04997470299998));
#245063=CARTESIAN_POINT('Ctrl Pts',(-7.66254598200005,11.6,8.04997470299998));
#245064=CARTESIAN_POINT('Ctrl Pts',(-7.66551037500006,15.2,8.05134666399999));
#245065=CARTESIAN_POINT('Ctrl Pts',(-7.66551037500006,11.6,8.05134666399999));
#245066=CARTESIAN_POINT('Ctrl Pts',(-7.66848043700006,15.2,8.05271836699998));
#245067=CARTESIAN_POINT('Ctrl Pts',(-7.66848043700006,11.6,8.05271836699998));
#245068=CARTESIAN_POINT('Ctrl Pts',(-7.67145616200006,15.2,8.05408980299998));
#245069=CARTESIAN_POINT('Ctrl Pts',(-7.67145616200006,11.6,8.05408980299998));
#245070=CARTESIAN_POINT('Ctrl Pts',(-7.67443754600006,15.2,8.05546096299998));
#245071=CARTESIAN_POINT('Ctrl Pts',(-7.67443754600006,11.6,8.05546096299998));
#245072=CARTESIAN_POINT('Ctrl Pts',(-7.67742458300006,15.2,8.05683183699998));
#245073=CARTESIAN_POINT('Ctrl Pts',(-7.67742458300006,11.6,8.05683183699998));
#245074=CARTESIAN_POINT('Ctrl Pts',(-7.68041727000006,15.2,8.05820241499998));
#245075=CARTESIAN_POINT('Ctrl Pts',(-7.68041727000006,11.6,8.05820241499998));
#245076=CARTESIAN_POINT('Ctrl Pts',(-7.68341560100006,15.2,8.05957268799999));
#245077=CARTESIAN_POINT('Ctrl Pts',(-7.68341560100006,11.6,8.05957268799999));
#245078=CARTESIAN_POINT('Ctrl Pts',(-7.68641957100006,15.2,8.06094264599999));
#245079=CARTESIAN_POINT('Ctrl Pts',(-7.68641957100006,11.6,8.06094264599999));
#245080=CARTESIAN_POINT('Ctrl Pts',(-7.68942917500006,15.2,8.06231227899998));
#245081=CARTESIAN_POINT('Ctrl Pts',(-7.68942917500006,11.6,8.06231227899998));
#245082=CARTESIAN_POINT('Ctrl Pts',(-7.69244440900006,15.2,8.06368157799999));
#245083=CARTESIAN_POINT('Ctrl Pts',(-7.69244440900006,11.6,8.06368157799999));
#245084=CARTESIAN_POINT('Ctrl Pts',(-7.69546526600006,15.2,8.06505053299999));
#245085=CARTESIAN_POINT('Ctrl Pts',(-7.69546526600006,11.6,8.06505053299999));
#245086=CARTESIAN_POINT('Ctrl Pts',(-7.69849174400005,15.2,8.06641913399999));
#245087=CARTESIAN_POINT('Ctrl Pts',(-7.69849174400005,11.6,8.06641913399999));
#245088=CARTESIAN_POINT('Ctrl Pts',(-7.70152383600006,15.2,8.06778737399998));
#245089=CARTESIAN_POINT('Ctrl Pts',(-7.70152383600006,11.6,8.06778737399998));
#245090=CARTESIAN_POINT('Ctrl Pts',(-7.70456153900006,15.2,8.06915523999999));
#245091=CARTESIAN_POINT('Ctrl Pts',(-7.70456153900006,11.6,8.06915523999999));
#245092=CARTESIAN_POINT('Ctrl Pts',(-7.70760484600006,15.2,8.07052272399999));
#245093=CARTESIAN_POINT('Ctrl Pts',(-7.70760484600006,11.6,8.07052272399999));
#245094=CARTESIAN_POINT('Ctrl Pts',(-7.71065375300005,15.2,8.07188981699999));
#245095=CARTESIAN_POINT('Ctrl Pts',(-7.71065375300005,11.6,8.07188981699999));
#245096=CARTESIAN_POINT('Ctrl Pts',(-7.71370825500006,15.2,8.07325650899998));
#245097=CARTESIAN_POINT('Ctrl Pts',(-7.71370825500006,11.6,8.07325650899998));
#245098=CARTESIAN_POINT('Ctrl Pts',(-7.71676834800005,15.2,8.07462279199999));
#245099=CARTESIAN_POINT('Ctrl Pts',(-7.71676834800005,11.6,8.07462279199999));
#245100=CARTESIAN_POINT('Ctrl Pts',(-7.71983402500006,15.2,8.07598865399999));
#245101=CARTESIAN_POINT('Ctrl Pts',(-7.71983402500006,11.6,8.07598865399999));
#245102=CARTESIAN_POINT('Ctrl Pts',(-7.72290528400006,15.2,8.07735408899998));
#245103=CARTESIAN_POINT('Ctrl Pts',(-7.72290528400006,11.6,8.07735408899998));
#245104=CARTESIAN_POINT('Ctrl Pts',(-7.72598211700006,15.2,8.07871908399999));
#245105=CARTESIAN_POINT('Ctrl Pts',(-7.72598211700006,11.6,8.07871908399999));
#245106=CARTESIAN_POINT('Ctrl Pts',(-7.72906452200005,15.2,8.08008363199999));
#245107=CARTESIAN_POINT('Ctrl Pts',(-7.72906452200005,11.6,8.08008363199999));
#245108=CARTESIAN_POINT('Ctrl Pts',(-7.73215249300006,15.2,8.08144772299999));
#245109=CARTESIAN_POINT('Ctrl Pts',(-7.73215249300006,11.6,8.08144772299999));
#245110=CARTESIAN_POINT('Ctrl Pts',(-7.73524602400006,15.2,8.08281134799999));
#245111=CARTESIAN_POINT('Ctrl Pts',(-7.73524602400006,11.6,8.08281134799999));
#245112=CARTESIAN_POINT('Ctrl Pts',(-7.73834511100005,15.2,8.08417449699999));
#245113=CARTESIAN_POINT('Ctrl Pts',(-7.73834511100005,11.6,8.08417449699999));
#245114=CARTESIAN_POINT('Ctrl Pts',(-7.74144975100005,15.2,8.08553716199999));
#245115=CARTESIAN_POINT('Ctrl Pts',(-7.74144975100005,11.6,8.08553716199999));
#245116=CARTESIAN_POINT('Ctrl Pts',(-7.74455993600006,15.2,8.08689933299998));
#245117=CARTESIAN_POINT('Ctrl Pts',(-7.74455993600006,11.6,8.08689933299998));
#245118=CARTESIAN_POINT('Ctrl Pts',(-7.74767566300006,15.2,8.08826100099999));
#245119=CARTESIAN_POINT('Ctrl Pts',(-7.74767566300006,11.6,8.08826100099999));
#245120=CARTESIAN_POINT('Ctrl Pts',(-7.75079692700006,15.2,8.08962215699999));
#245121=CARTESIAN_POINT('Ctrl Pts',(-7.75079692700006,11.6,8.08962215699999));
#245122=CARTESIAN_POINT('Ctrl Pts',(-7.75392372200006,15.2,8.09098279099998));
#245123=CARTESIAN_POINT('Ctrl Pts',(-7.75392372200006,11.6,8.09098279099998));
#245124=CARTESIAN_POINT('Ctrl Pts',(-7.75705604400006,15.2,8.09234289499998));
#245125=CARTESIAN_POINT('Ctrl Pts',(-7.75705604400006,11.6,8.09234289499998));
#245126=CARTESIAN_POINT('Ctrl Pts',(-7.76019388900006,15.2,8.09370245899999));
#245127=CARTESIAN_POINT('Ctrl Pts',(-7.76019388900006,11.6,8.09370245899999));
#245128=CARTESIAN_POINT('Ctrl Pts',(-7.76333725000006,15.2,8.09506147499999));
#245129=CARTESIAN_POINT('Ctrl Pts',(-7.76333725000006,11.6,8.09506147499999));
#245130=CARTESIAN_POINT('Ctrl Pts',(-7.76648612500006,15.2,8.09641993199998));
#245131=CARTESIAN_POINT('Ctrl Pts',(-7.76648612500006,11.6,8.09641993199998));
#245132=CARTESIAN_POINT('Ctrl Pts',(-7.76964050600006,15.2,8.09777782399999));
#245133=CARTESIAN_POINT('Ctrl Pts',(-7.76964050600006,11.6,8.09777782399999));
#245134=CARTESIAN_POINT('Ctrl Pts',(-7.77280039100006,15.2,8.09913513899998));
#245135=CARTESIAN_POINT('Ctrl Pts',(-7.77280039100006,11.6,8.09913513899998));
#245136=CARTESIAN_POINT('Ctrl Pts',(-7.77596577300006,15.2,8.10049186899998));
#245137=CARTESIAN_POINT('Ctrl Pts',(-7.77596577300006,11.6,8.10049186899998));
#245138=CARTESIAN_POINT('Ctrl Pts',(-7.77913664800005,15.2,8.10184800599998));
#245139=CARTESIAN_POINT('Ctrl Pts',(-7.77913664800005,11.6,8.10184800599998));
#245140=CARTESIAN_POINT('Ctrl Pts',(-7.78231301200006,15.2,8.10320353899998));
#245141=CARTESIAN_POINT('Ctrl Pts',(-7.78231301200006,11.6,8.10320353899998));
#245142=CARTESIAN_POINT('Ctrl Pts',(-7.78549485900006,15.2,8.10455846299998));
#245143=CARTESIAN_POINT('Ctrl Pts',(-7.78549485900006,11.6,8.10455846299998));
#245144=CARTESIAN_POINT('Ctrl Pts',(-7.78868218500006,15.2,8.10591276399999));
#245145=CARTESIAN_POINT('Ctrl Pts',(-7.78868218500006,11.6,8.10591276399999));
#245146=CARTESIAN_POINT('Ctrl Pts',(-7.79187498300006,15.2,8.10726643599999));
#245147=CARTESIAN_POINT('Ctrl Pts',(-7.79187498300006,11.6,8.10726643599999));
#245148=CARTESIAN_POINT('Ctrl Pts',(-7.79507325100005,15.2,8.10861946999999));
#245149=CARTESIAN_POINT('Ctrl Pts',(-7.79507325100005,11.6,8.10861946999999));
#245150=CARTESIAN_POINT('Ctrl Pts',(-7.79827698300006,15.2,8.10997185699998));
#245151=CARTESIAN_POINT('Ctrl Pts',(-7.79827698300006,11.6,8.10997185699998));
#245152=CARTESIAN_POINT('Ctrl Pts',(-7.80148617400006,15.2,8.11132358799998));
#245153=CARTESIAN_POINT('Ctrl Pts',(-7.80148617400006,11.6,8.11132358799998));
#245154=CARTESIAN_POINT('Ctrl Pts',(-7.80470082000006,15.2,8.11267465299998));
#245155=CARTESIAN_POINT('Ctrl Pts',(-7.80470082000006,11.6,8.11267465299998));
#245156=CARTESIAN_POINT('Ctrl Pts',(-7.80792091500006,15.2,8.11402504599998));
#245157=CARTESIAN_POINT('Ctrl Pts',(-7.80792091500006,11.6,8.11402504599998));
#245158=CARTESIAN_POINT('Ctrl Pts',(-7.81114645400006,15.2,8.11537475499998));
#245159=CARTESIAN_POINT('Ctrl Pts',(-7.81114645400006,11.6,8.11537475499998));
#245160=CARTESIAN_POINT('Ctrl Pts',(-7.81437743500006,15.2,8.11672377399999));
#245161=CARTESIAN_POINT('Ctrl Pts',(-7.81437743500006,11.6,8.11672377399999));
#245162=CARTESIAN_POINT('Ctrl Pts',(-7.81761384900006,15.2,8.11807209299998));
#245163=CARTESIAN_POINT('Ctrl Pts',(-7.81761384900006,11.6,8.11807209299998));
#245164=CARTESIAN_POINT('Ctrl Pts',(-7.82085569500006,15.2,8.11941970299999));
#245165=CARTESIAN_POINT('Ctrl Pts',(-7.82085569500006,11.6,8.11941970299999));
#245166=CARTESIAN_POINT('Ctrl Pts',(-7.82410296500006,15.2,8.12076659599999));
#245167=CARTESIAN_POINT('Ctrl Pts',(-7.82410296500006,11.6,8.12076659599999));
#245168=CARTESIAN_POINT('Ctrl Pts',(-7.82735565600006,15.2,8.12211276299998));
#245169=CARTESIAN_POINT('Ctrl Pts',(-7.82735565600006,11.6,8.12211276299998));
#245170=CARTESIAN_POINT('Ctrl Pts',(-7.83061376200005,15.2,8.12345819399999));
#245171=CARTESIAN_POINT('Ctrl Pts',(-7.83061376200005,11.6,8.12345819399999));
#245172=CARTESIAN_POINT('Ctrl Pts',(-7.83387728100006,15.2,8.12480288399998));
#245173=CARTESIAN_POINT('Ctrl Pts',(-7.83387728100006,11.6,8.12480288399998));
#245174=CARTESIAN_POINT('Ctrl Pts',(-7.83714620400006,15.2,8.12614681999998));
#245175=CARTESIAN_POINT('Ctrl Pts',(-7.83714620400006,11.6,8.12614681999998));
#245176=CARTESIAN_POINT('Ctrl Pts',(-7.84042053000006,15.2,8.12748999699998));
#245177=CARTESIAN_POINT('Ctrl Pts',(-7.84042053000006,11.6,8.12748999699998));
#245178=CARTESIAN_POINT('Ctrl Pts',(-7.84370025300006,15.2,8.12883240399999));
#245179=CARTESIAN_POINT('Ctrl Pts',(-7.84370025300006,11.6,8.12883240399999));
#245180=CARTESIAN_POINT('Ctrl Pts',(-7.84698536600006,15.2,8.13017403499998));
#245181=CARTESIAN_POINT('Ctrl Pts',(-7.84698536600006,11.6,8.13017403499998));
#245182=CARTESIAN_POINT('Ctrl Pts',(-7.85027586700006,15.2,8.13151487799999));
#245183=CARTESIAN_POINT('Ctrl Pts',(-7.85027586700006,11.6,8.13151487799999));
#245184=CARTESIAN_POINT('Ctrl Pts',(-7.85357175000006,15.2,8.13285492699999));
#245185=CARTESIAN_POINT('Ctrl Pts',(-7.85357175000006,11.6,8.13285492699999));
#245186=CARTESIAN_POINT('Ctrl Pts',(-7.85687301000006,15.2,8.13419417299999));
#245187=CARTESIAN_POINT('Ctrl Pts',(-7.85687301000006,11.6,8.13419417299999));
#245188=CARTESIAN_POINT('Ctrl Pts',(-7.86017964300005,15.2,8.13553260699998));
#245189=CARTESIAN_POINT('Ctrl Pts',(-7.86017964300005,11.6,8.13553260699998));
#245190=CARTESIAN_POINT('Ctrl Pts',(-7.86349164400006,15.2,8.13687022099998));
#245191=CARTESIAN_POINT('Ctrl Pts',(-7.86349164400006,11.6,8.13687022099998));
#245192=CARTESIAN_POINT('Ctrl Pts',(-7.86680900800006,15.2,8.13820700699999));
#245193=CARTESIAN_POINT('Ctrl Pts',(-7.86680900800006,11.6,8.13820700699999));
#245194=CARTESIAN_POINT('Ctrl Pts',(-7.87013173000006,15.2,8.13954295599999));
#245195=CARTESIAN_POINT('Ctrl Pts',(-7.87013173000006,11.6,8.13954295599999));
#245196=CARTESIAN_POINT('Ctrl Pts',(-7.87345980500006,15.2,8.14087805999998));
#245197=CARTESIAN_POINT('Ctrl Pts',(-7.87345980500006,11.6,8.14087805999998));
#245198=CARTESIAN_POINT('Ctrl Pts',(-7.87679322900006,15.2,8.14221230999999));
#245199=CARTESIAN_POINT('Ctrl Pts',(-7.87679322900006,11.6,8.14221230999999));
#245200=CARTESIAN_POINT('Ctrl Pts',(-7.88013199700006,15.2,8.14354569699999));
#245201=CARTESIAN_POINT('Ctrl Pts',(-7.88013199700006,11.6,8.14354569699999));
#245202=CARTESIAN_POINT('Ctrl Pts',(-7.88347610400006,15.2,8.14487821399998));
#245203=CARTESIAN_POINT('Ctrl Pts',(-7.88347610400006,11.6,8.14487821399998));
#245204=CARTESIAN_POINT('Ctrl Pts',(-7.88682554500006,15.2,8.14620985299998));
#245205=CARTESIAN_POINT('Ctrl Pts',(-7.88682554500006,11.6,8.14620985299998));
#245206=CARTESIAN_POINT('Ctrl Pts',(-7.89018031600006,15.2,8.14754060399999));
#245207=CARTESIAN_POINT('Ctrl Pts',(-7.89018031600006,11.6,8.14754060399999));
#245208=CARTESIAN_POINT('Ctrl Pts',(-7.89354041200006,15.2,8.14887045999999));
#245209=CARTESIAN_POINT('Ctrl Pts',(-7.89354041200006,11.6,8.14887045999999));
#245210=CARTESIAN_POINT('Ctrl Pts',(-7.89690582700005,15.2,8.15019941199999));
#245211=CARTESIAN_POINT('Ctrl Pts',(-7.89690582700005,11.6,8.15019941199999));
#245212=CARTESIAN_POINT('Ctrl Pts',(-7.90027655700006,15.2,8.15152745299999));
#245213=CARTESIAN_POINT('Ctrl Pts',(-7.90027655700006,11.6,8.15152745299999));
#245214=CARTESIAN_POINT('Ctrl Pts',(-7.90365259800006,15.2,8.15285457299998));
#245215=CARTESIAN_POINT('Ctrl Pts',(-7.90365259800006,11.6,8.15285457299998));
#245216=CARTESIAN_POINT('Ctrl Pts',(-7.90703394500006,15.2,8.15418076499999));
#245217=CARTESIAN_POINT('Ctrl Pts',(-7.90703394500006,11.6,8.15418076499999));
#245218=CARTESIAN_POINT('Ctrl Pts',(-7.91042059300005,15.2,8.15550602099999));
#245219=CARTESIAN_POINT('Ctrl Pts',(-7.91042059300005,11.6,8.15550602099999));
#245220=CARTESIAN_POINT('Ctrl Pts',(-7.91381253600005,15.2,8.15683033199999));
#245221=CARTESIAN_POINT('Ctrl Pts',(-7.91381253600005,11.6,8.15683033199999));
#245222=CARTESIAN_POINT('Ctrl Pts',(-7.91720977000006,15.2,8.15815368899998));
#245223=CARTESIAN_POINT('Ctrl Pts',(-7.91720977000006,11.6,8.15815368899998));
#245224=CARTESIAN_POINT('Ctrl Pts',(-7.92061229100005,15.2,8.15947608599998));
#245225=CARTESIAN_POINT('Ctrl Pts',(-7.92061229100005,11.6,8.15947608599998));
#245226=CARTESIAN_POINT('Ctrl Pts',(-7.92402009400006,15.2,8.16079751399998));
#245227=CARTESIAN_POINT('Ctrl Pts',(-7.92402009400006,11.6,8.16079751399998));
#245228=CARTESIAN_POINT('Ctrl Pts',(-7.92743317500006,15.2,8.16211796399998));
#245229=CARTESIAN_POINT('Ctrl Pts',(-7.92743317500006,11.6,8.16211796399998));
#245230=CARTESIAN_POINT('Ctrl Pts',(-7.93085152700005,15.2,8.16343742899999));
#245231=CARTESIAN_POINT('Ctrl Pts',(-7.93085152700005,11.6,8.16343742899999));
#245232=CARTESIAN_POINT('Ctrl Pts',(-7.93427514700006,15.2,8.16475590099999));
#245233=CARTESIAN_POINT('Ctrl Pts',(-7.93427514700006,11.6,8.16475590099999));
#245234=CARTESIAN_POINT('Ctrl Pts',(-7.93770402900006,15.2,8.16607337199999));
#245235=CARTESIAN_POINT('Ctrl Pts',(-7.93770402900006,11.6,8.16607337199999));
#245236=CARTESIAN_POINT('Ctrl Pts',(-7.94113817000006,15.2,8.16738983299999));
#245237=CARTESIAN_POINT('Ctrl Pts',(-7.94113817000006,11.6,8.16738983299999));
#245238=CARTESIAN_POINT('Ctrl Pts',(-7.94457756400006,15.2,8.16870527599999));
#245239=CARTESIAN_POINT('Ctrl Pts',(-7.94457756400006,11.6,8.16870527599999));
#245240=CARTESIAN_POINT('Ctrl Pts',(-7.94802220600006,15.2,8.17001969299999));
#245241=CARTESIAN_POINT('Ctrl Pts',(-7.94802220600006,11.6,8.17001969299999));
#245242=CARTESIAN_POINT('Ctrl Pts',(-7.95147209200006,15.2,8.17133307699999));
#245243=CARTESIAN_POINT('Ctrl Pts',(-7.95147209200006,11.6,8.17133307699999));
#245244=CARTESIAN_POINT('Ctrl Pts',(-7.95492721600005,15.2,8.17264541999998));
#245245=CARTESIAN_POINT('Ctrl Pts',(-7.95492721600005,11.6,8.17264541999998));
#245246=CARTESIAN_POINT('Ctrl Pts',(-7.95838757500006,15.2,8.17395671299998));
#245247=CARTESIAN_POINT('Ctrl Pts',(-7.95838757500006,11.6,8.17395671299998));
#245248=CARTESIAN_POINT('Ctrl Pts',(-7.96185316300006,15.2,8.17526694799999));
#245249=CARTESIAN_POINT('Ctrl Pts',(-7.96185316300006,11.6,8.17526694799999));
#245250=CARTESIAN_POINT('Ctrl Pts',(-7.96532397700006,15.2,8.17657611899998));
#245251=CARTESIAN_POINT('Ctrl Pts',(-7.96532397700006,11.6,8.17657611899998));
#245252=CARTESIAN_POINT('Ctrl Pts',(-7.96880001000006,15.2,8.17788421699999));
#245253=CARTESIAN_POINT('Ctrl Pts',(-7.96880001000006,11.6,8.17788421699999));
#245254=CARTESIAN_POINT('Ctrl Pts',(-7.97228126000006,15.2,8.17919123499999));
#245255=CARTESIAN_POINT('Ctrl Pts',(-7.97228126000006,11.6,8.17919123499999));
#245256=CARTESIAN_POINT('Ctrl Pts',(-7.97576771900006,15.2,8.18049716399998));
#245257=CARTESIAN_POINT('Ctrl Pts',(-7.97576771900006,11.6,8.18049716399998));
#245258=CARTESIAN_POINT('Ctrl Pts',(-7.97925938500006,15.2,8.18180199599999));
#245259=CARTESIAN_POINT('Ctrl Pts',(-7.97925938500006,11.6,8.18180199599999));
#245260=CARTESIAN_POINT('Ctrl Pts',(-7.98275625000005,15.2,8.18310572199999));
#245261=CARTESIAN_POINT('Ctrl Pts',(-7.98275625000005,11.6,8.18310572199999));
#245262=CARTESIAN_POINT('Ctrl Pts',(-7.98625831300006,15.2,8.18440833599999));
#245263=CARTESIAN_POINT('Ctrl Pts',(-7.98625831300006,11.6,8.18440833599999));
#245264=CARTESIAN_POINT('Ctrl Pts',(-7.98976556600006,15.2,8.18570982799999));
#245265=CARTESIAN_POINT('Ctrl Pts',(-7.98976556600006,11.6,8.18570982799999));
#245266=CARTESIAN_POINT('Ctrl Pts',(-7.99327800400006,15.2,8.18701019299999));
#245267=CARTESIAN_POINT('Ctrl Pts',(-7.99327800400006,11.6,8.18701019299999));
#245268=CARTESIAN_POINT('Ctrl Pts',(-7.99679562600006,15.2,8.18830942099999));
#245269=CARTESIAN_POINT('Ctrl Pts',(-7.99679562600006,11.6,8.18830942099999));
#245270=CARTESIAN_POINT('Ctrl Pts',(-8.00031842500006,15.2,8.18960750499999));
#245271=CARTESIAN_POINT('Ctrl Pts',(-8.00031842500006,11.6,8.18960750499999));
#245272=CARTESIAN_POINT('Ctrl Pts',(-8.00384639600006,15.2,8.19090443999999));
#245273=CARTESIAN_POINT('Ctrl Pts',(-8.00384639600006,11.6,8.19090443999999));
#245274=CARTESIAN_POINT('Ctrl Pts',(-8.00737953700006,15.2,8.19220021799998));
#245275=CARTESIAN_POINT('Ctrl Pts',(-8.00737953700006,11.6,8.19220021799998));
#245276=CARTESIAN_POINT('Ctrl Pts',(-8.01091784300005,15.2,8.19349483199998));
#245277=CARTESIAN_POINT('Ctrl Pts',(-8.01091784300005,11.6,8.19349483199998));
#245278=CARTESIAN_POINT('Ctrl Pts',(-8.01446130800005,15.2,8.19478827199998));
#245279=CARTESIAN_POINT('Ctrl Pts',(-8.01446130800005,11.6,8.19478827199998));
#245280=CARTESIAN_POINT('Ctrl Pts',(-8.01800992700005,15.2,8.19608053199998));
#245281=CARTESIAN_POINT('Ctrl Pts',(-8.01800992700005,11.6,8.19608053199998));
#245282=CARTESIAN_POINT('Ctrl Pts',(-8.02156369500005,15.2,8.19737160199999));
#245283=CARTESIAN_POINT('Ctrl Pts',(-8.02156369500005,11.6,8.19737160199999));
#245284=CARTESIAN_POINT('Ctrl Pts',(-8.02512260400006,15.2,8.19866146999999));
#245285=CARTESIAN_POINT('Ctrl Pts',(-8.02512260400006,11.6,8.19866146999999));
#245286=CARTESIAN_POINT('Ctrl Pts',(-8.02868665100006,15.2,8.19995012899999));
#245287=CARTESIAN_POINT('Ctrl Pts',(-8.02868665100006,11.6,8.19995012899999));
#245288=CARTESIAN_POINT('Ctrl Pts',(-8.03225583000006,15.2,8.20123757099999));
#245289=CARTESIAN_POINT('Ctrl Pts',(-8.03225583000006,11.6,8.20123757099999));
#245290=CARTESIAN_POINT('Ctrl Pts',(-8.03583013500005,15.2,8.20252378799999));
#245291=CARTESIAN_POINT('Ctrl Pts',(-8.03583013500005,11.6,8.20252378799999));
#245292=CARTESIAN_POINT('Ctrl Pts',(-8.03940956400006,15.2,8.20380877499998));
#245293=CARTESIAN_POINT('Ctrl Pts',(-8.03940956400006,11.6,8.20380877499998));
#245294=CARTESIAN_POINT('Ctrl Pts',(-8.04299411600006,15.2,8.20509252899999));
#245295=CARTESIAN_POINT('Ctrl Pts',(-8.04299411600006,11.6,8.20509252899999));
#245296=CARTESIAN_POINT('Ctrl Pts',(-8.04658378800006,15.2,8.20637504799999));
#245297=CARTESIAN_POINT('Ctrl Pts',(-8.04658378800006,11.6,8.20637504799999));
#245298=CARTESIAN_POINT('Ctrl Pts',(-8.04945962200006,15.2,8.20740007499998));
#245299=CARTESIAN_POINT('Ctrl Pts',(-8.04945962200006,11.6,8.20740007499998));
#245300=CARTESIAN_POINT('Ctrl Pts',(-8.05161880100006,15.2,8.20816828899999));
#245301=CARTESIAN_POINT('Ctrl Pts',(-8.05161880100006,11.6,8.20816828899999));
#245302=CARTESIAN_POINT('Ctrl Pts',(-8.05305927800006,15.2,8.20868018399998));
#245303=CARTESIAN_POINT('Ctrl Pts',(-8.05305927800006,11.6,8.20868018399998));
#245304=CARTESIAN_POINT('Ctrl Pts',(-8.05377977200006,15.2,8.20893606999999));
#245305=CARTESIAN_POINT('Ctrl Pts',(-8.05377977200006,11.6,8.20893606999999));
#245306=CARTESIAN_POINT('Ctrl Pts',(-7.01216898600006,15.2,7.64657512399998));
#245307=CARTESIAN_POINT('Ctrl Pts',(-7.01229743700006,15.2,7.64669302599999));
#245308=CARTESIAN_POINT('Ctrl Pts',(-7.01255888300006,15.2,7.64693288499998));
#245309=CARTESIAN_POINT('Ctrl Pts',(-7.01295521800006,15.2,7.64729613499998));
#245310=CARTESIAN_POINT('Ctrl Pts',(-7.01348948000006,15.2,7.64778506499999));
#245311=CARTESIAN_POINT('Ctrl Pts',(-7.01416585900006,15.2,7.64840281599999));
#245312=CARTESIAN_POINT('Ctrl Pts',(-7.01485383100006,15.2,7.64902988999999));
#245313=CARTESIAN_POINT('Ctrl Pts',(-7.01554947000006,15.2,7.64966267399998));
#245314=CARTESIAN_POINT('Ctrl Pts',(-7.01625276700006,15.2,7.65030113899999));
#245315=CARTESIAN_POINT('Ctrl Pts',(-7.01696371600006,15.2,7.65094525299999));
#245316=CARTESIAN_POINT('Ctrl Pts',(-7.01768230900006,15.2,7.65159498499998));
#245317=CARTESIAN_POINT('Ctrl Pts',(-7.01840853600006,15.2,7.65225030299998));
#245318=CARTESIAN_POINT('Ctrl Pts',(-7.01914239300006,15.2,7.65291117499999));
#245319=CARTESIAN_POINT('Ctrl Pts',(-7.01988387000006,15.2,7.65357757299999));
#245320=CARTESIAN_POINT('Ctrl Pts',(-7.02063296000006,15.2,7.65424946399998));
#245321=CARTESIAN_POINT('Ctrl Pts',(-7.02138965700006,15.2,7.65492681899998));
#245322=CARTESIAN_POINT('Ctrl Pts',(-7.02215395000006,15.2,7.65560960799998));
#245323=CARTESIAN_POINT('Ctrl Pts',(-7.02292583400006,15.2,7.65629779899999));
#245324=CARTESIAN_POINT('Ctrl Pts',(-7.02370530000006,15.2,7.65699136299999));
#245325=CARTESIAN_POINT('Ctrl Pts',(-7.02449234200006,15.2,7.65769026899999));
#245326=CARTESIAN_POINT('Ctrl Pts',(-7.02528695100006,15.2,7.65839448899998));
#245327=CARTESIAN_POINT('Ctrl Pts',(-7.02608912200006,15.2,7.65910399299998));
#245328=CARTESIAN_POINT('Ctrl Pts',(-7.02689884500006,15.2,7.65981874999999));
#245329=CARTESIAN_POINT('Ctrl Pts',(-7.02771611300006,15.2,7.66053873299998));
#245330=CARTESIAN_POINT('Ctrl Pts',(-7.02854092000006,15.2,7.66126390999998));
#245331=CARTESIAN_POINT('Ctrl Pts',(-7.02937325800006,15.2,7.66199425499998));
#245332=CARTESIAN_POINT('Ctrl Pts',(-7.03021311900006,15.2,7.66272973699999));
#245333=CARTESIAN_POINT('Ctrl Pts',(-7.03106049600006,15.2,7.66347032799998));
#245334=CARTESIAN_POINT('Ctrl Pts',(-7.03191538200006,15.2,7.66421599899999));
#245335=CARTESIAN_POINT('Ctrl Pts',(-7.03277777000006,15.2,7.66496672199998));
#245336=CARTESIAN_POINT('Ctrl Pts',(-7.03364765200006,15.2,7.66572246899998));
#245337=CARTESIAN_POINT('Ctrl Pts',(-7.03452502100006,15.2,7.66648321099999));
#245338=CARTESIAN_POINT('Ctrl Pts',(-7.03540987000006,15.2,7.66724892099998));
#245339=CARTESIAN_POINT('Ctrl Pts',(-7.03630219100006,15.2,7.66801956799998));
#245340=CARTESIAN_POINT('Ctrl Pts',(-7.03720197800005,15.2,7.66879512799999));
#245341=CARTESIAN_POINT('Ctrl Pts',(-7.03810922400006,15.2,7.66957557299998));
#245342=CARTESIAN_POINT('Ctrl Pts',(-7.03902392100006,15.2,7.67036087199998));
#245343=CARTESIAN_POINT('Ctrl Pts',(-7.03994606100006,15.2,7.67115099999998));
#245344=CARTESIAN_POINT('Ctrl Pts',(-7.04087563900006,15.2,7.67194592999999));
#245345=CARTESIAN_POINT('Ctrl Pts',(-7.04181264600006,15.2,7.67274563399998));
#245346=CARTESIAN_POINT('Ctrl Pts',(-7.04275707700006,15.2,7.67355008599999));
#245347=CARTESIAN_POINT('Ctrl Pts',(-7.04370892200005,15.2,7.67435925699999));
#245348=CARTESIAN_POINT('Ctrl Pts',(-7.04466817800006,15.2,7.67517312299999));
#245349=CARTESIAN_POINT('Ctrl Pts',(-7.04563483400006,15.2,7.67599165499998));
#245350=CARTESIAN_POINT('Ctrl Pts',(-7.04660888600006,15.2,7.67681482699999));
#245351=CARTESIAN_POINT('Ctrl Pts',(-7.04759032400006,15.2,7.67764261299998));
#245352=CARTESIAN_POINT('Ctrl Pts',(-7.04857914400006,15.2,7.67847498699999));
#245353=CARTESIAN_POINT('Ctrl Pts',(-7.04957533900005,15.2,7.67931192299999));
#245354=CARTESIAN_POINT('Ctrl Pts',(-7.05057890000006,15.2,7.68015339299998));
#245355=CARTESIAN_POINT('Ctrl Pts',(-7.05158982000006,15.2,7.68099937399998));
#245356=CARTESIAN_POINT('Ctrl Pts',(-7.05260809400006,15.2,7.68184983699999));
#245357=CARTESIAN_POINT('Ctrl Pts',(-7.05363371500006,15.2,7.68270475799999));
#245358=CARTESIAN_POINT('Ctrl Pts',(-7.05466667400006,15.2,7.68356411099998));
#245359=CARTESIAN_POINT('Ctrl Pts',(-7.05570696700006,15.2,7.68442787099998));
#245360=CARTESIAN_POINT('Ctrl Pts',(-7.05675458400005,15.2,7.68529601199998));
#245361=CARTESIAN_POINT('Ctrl Pts',(-7.05780952100006,15.2,7.68616850899999));
#245362=CARTESIAN_POINT('Ctrl Pts',(-7.05887177100006,15.2,7.68704533799998));
#245363=CARTESIAN_POINT('Ctrl Pts',(-7.05994132500006,15.2,7.68792647199999));
#245364=CARTESIAN_POINT('Ctrl Pts',(-7.06101817900006,15.2,7.68881188699999));
#245365=CARTESIAN_POINT('Ctrl Pts',(-7.06210232400006,15.2,7.68970155699999));
#245366=CARTESIAN_POINT('Ctrl Pts',(-7.06319375500006,15.2,7.69059545999998));
#245367=CARTESIAN_POINT('Ctrl Pts',(-7.06429246300006,15.2,7.69149356899998));
#245368=CARTESIAN_POINT('Ctrl Pts',(-7.06539844400006,15.2,7.69239585999999));
#245369=CARTESIAN_POINT('Ctrl Pts',(-7.06651169000006,15.2,7.69330230899998));
#245370=CARTESIAN_POINT('Ctrl Pts',(-7.06763219400006,15.2,7.69421289099999));
#245371=CARTESIAN_POINT('Ctrl Pts',(-7.06875995000006,15.2,7.69512758399999));
#245372=CARTESIAN_POINT('Ctrl Pts',(-7.06989495100006,15.2,7.69604635999999));
#245373=CARTESIAN_POINT('Ctrl Pts',(-7.07103719100005,15.2,7.69696919799999));
#245374=CARTESIAN_POINT('Ctrl Pts',(-7.07218666200006,15.2,7.69789607499998));
#245375=CARTESIAN_POINT('Ctrl Pts',(-7.07334335900006,15.2,7.69882696299998));
#245376=CARTESIAN_POINT('Ctrl Pts',(-7.07450727400006,15.2,7.69976184299999));
#245377=CARTESIAN_POINT('Ctrl Pts',(-7.07567840200006,15.2,7.70070068799999));
#245378=CARTESIAN_POINT('Ctrl Pts',(-7.07685673500006,15.2,7.70164347599999));
#245379=CARTESIAN_POINT('Ctrl Pts',(-7.07804226800006,15.2,7.70259018399998));
#245380=CARTESIAN_POINT('Ctrl Pts',(-7.07923499300006,15.2,7.70354078799999));
#245381=CARTESIAN_POINT('Ctrl Pts',(-7.08043490300006,15.2,7.70449526499998));
#245382=CARTESIAN_POINT('Ctrl Pts',(-7.08164199400006,15.2,7.70545359099999));
#245383=CARTESIAN_POINT('Ctrl Pts',(-7.08285625800006,15.2,7.70641574499999));
#245384=CARTESIAN_POINT('Ctrl Pts',(-7.08407768800006,15.2,7.70738170199999));
#245385=CARTESIAN_POINT('Ctrl Pts',(-7.08530627800006,15.2,7.70835144099999));
#245386=CARTESIAN_POINT('Ctrl Pts',(-7.08654202200006,15.2,7.70932493899998));
#245387=CARTESIAN_POINT('Ctrl Pts',(-7.08778491400006,15.2,7.71030217199999));
#245388=CARTESIAN_POINT('Ctrl Pts',(-7.08903494500006,15.2,7.71128311899999));
#245389=CARTESIAN_POINT('Ctrl Pts',(-7.09029211200006,15.2,7.71226775599998));
#245390=CARTESIAN_POINT('Ctrl Pts',(-7.09155640600006,15.2,7.71325606199999));
#245391=CARTESIAN_POINT('Ctrl Pts',(-7.09282782300006,15.2,7.71424801399998));
#245392=CARTESIAN_POINT('Ctrl Pts',(-7.09410635400006,15.2,7.71524359099999));
#245393=CARTESIAN_POINT('Ctrl Pts',(-7.09539199400006,15.2,7.71624276799999));
#245394=CARTESIAN_POINT('Ctrl Pts',(-7.09668473700006,15.2,7.71724552699999));
#245395=CARTESIAN_POINT('Ctrl Pts',(-7.09798457700006,15.2,7.71825184399999));
#245396=CARTESIAN_POINT('Ctrl Pts',(-7.09929150500006,15.2,7.71926169699999));
#245397=CARTESIAN_POINT('Ctrl Pts',(-7.10060551800006,15.2,7.72027506499998));
#245398=CARTESIAN_POINT('Ctrl Pts',(-7.10192660800006,15.2,7.72129192499998));
#245399=CARTESIAN_POINT('Ctrl Pts',(-7.10325476900006,15.2,7.72231225799998));
#245400=CARTESIAN_POINT('Ctrl Pts',(-7.10458999400006,15.2,7.72333603999999));
#245401=CARTESIAN_POINT('Ctrl Pts',(-7.10593227900006,15.2,7.72436325099999));
#245402=CARTESIAN_POINT('Ctrl Pts',(-7.10728161500006,15.2,7.72539386899999));
#245403=CARTESIAN_POINT('Ctrl Pts',(-7.10863799800006,15.2,7.72642787299999));
#245404=CARTESIAN_POINT('Ctrl Pts',(-7.11000142000006,15.2,7.72746524299999));
#245405=CARTESIAN_POINT('Ctrl Pts',(-7.11137187600006,15.2,7.72850595599999));
#245406=CARTESIAN_POINT('Ctrl Pts',(-7.11274935900006,15.2,7.72954999299999));
#245407=CARTESIAN_POINT('Ctrl Pts',(-7.11413386400006,15.2,7.73059733099998));
#245408=CARTESIAN_POINT('Ctrl Pts',(-7.11552538300006,15.2,7.73164795099999));
#245409=CARTESIAN_POINT('Ctrl Pts',(-7.11692391100006,15.2,7.73270183099999));
#245410=CARTESIAN_POINT('Ctrl Pts',(-7.11832944100006,15.2,7.73375895199998));
#245411=CARTESIAN_POINT('Ctrl Pts',(-7.11974196900006,15.2,7.73481929199999));
#245412=CARTESIAN_POINT('Ctrl Pts',(-7.12116148600006,15.2,7.73588283099999));
#245413=CARTESIAN_POINT('Ctrl Pts',(-7.12258798800006,15.2,7.73694954699998));
#245414=CARTESIAN_POINT('Ctrl Pts',(-7.12402146800006,15.2,7.73801942399999));
#245415=CARTESIAN_POINT('Ctrl Pts',(-7.12546192000006,15.2,7.73909243699999));
#245416=CARTESIAN_POINT('Ctrl Pts',(-7.12690933700006,15.2,7.74016856899999));
#245417=CARTESIAN_POINT('Ctrl Pts',(-7.12836371400006,15.2,7.74124779699999));
#245418=CARTESIAN_POINT('Ctrl Pts',(-7.12982504600006,15.2,7.74233010399998));
#245419=CARTESIAN_POINT('Ctrl Pts',(-7.13129332400006,15.2,7.74341546899999));
#245420=CARTESIAN_POINT('Ctrl Pts',(-7.13276854400006,15.2,7.74450386999998));
#245421=CARTESIAN_POINT('Ctrl Pts',(-7.13425070000006,15.2,7.74559529099999));
#245422=CARTESIAN_POINT('Ctrl Pts',(-7.13573978500006,15.2,7.74668970999999));
#245423=CARTESIAN_POINT('Ctrl Pts',(-7.13723579400006,15.2,7.74778710799998));
#245424=CARTESIAN_POINT('Ctrl Pts',(-7.13873872000006,15.2,7.74888746499999));
#245425=CARTESIAN_POINT('Ctrl Pts',(-7.14024855600006,15.2,7.74999076199999));
#245426=CARTESIAN_POINT('Ctrl Pts',(-7.14176530000006,15.2,7.75109697799999));
#245427=CARTESIAN_POINT('Ctrl Pts',(-7.14328894200006,15.2,7.75220609499998));
#245428=CARTESIAN_POINT('Ctrl Pts',(-7.14481947700006,15.2,7.75331809499999));
#245429=CARTESIAN_POINT('Ctrl Pts',(-7.14635690000006,15.2,7.75443295699999));
#245430=CARTESIAN_POINT('Ctrl Pts',(-7.14790120500005,15.2,7.75555066199999));
#245431=CARTESIAN_POINT('Ctrl Pts',(-7.14945238500006,15.2,7.75667119099998));
#245432=CARTESIAN_POINT('Ctrl Pts',(-7.15101043300006,15.2,7.75779452499999));
#245433=CARTESIAN_POINT('Ctrl Pts',(-7.15257534700006,15.2,7.75892064699998));
#245434=CARTESIAN_POINT('Ctrl Pts',(-7.15414711700006,15.2,7.76004953499999));
#245435=CARTESIAN_POINT('Ctrl Pts',(-7.15572573900006,15.2,7.76118117199999));
#245436=CARTESIAN_POINT('Ctrl Pts',(-7.15731120800006,15.2,7.76231553799998));
#245437=CARTESIAN_POINT('Ctrl Pts',(-7.15890351700006,15.2,7.76345261699999));
#245438=CARTESIAN_POINT('Ctrl Pts',(-7.16050265800006,15.2,7.76459238699999));
#245439=CARTESIAN_POINT('Ctrl Pts',(-7.16210862800006,15.2,7.76573483199999));
#245440=CARTESIAN_POINT('Ctrl Pts',(-7.16372142100006,15.2,7.76687993299999));
#245441=CARTESIAN_POINT('Ctrl Pts',(-7.16534103000006,15.2,7.76802766999998));
#245442=CARTESIAN_POINT('Ctrl Pts',(-7.16696745000006,15.2,7.76917802599999));
#245443=CARTESIAN_POINT('Ctrl Pts',(-7.16860067400006,15.2,7.77033098499999));
#245444=CARTESIAN_POINT('Ctrl Pts',(-7.17024069700006,15.2,7.77148652499999));
#245445=CARTESIAN_POINT('Ctrl Pts',(-7.17188751300006,15.2,7.77264462899999));
#245446=CARTESIAN_POINT('Ctrl Pts',(-7.17354111600006,15.2,7.77380527999998));
#245447=CARTESIAN_POINT('Ctrl Pts',(-7.17520150000006,15.2,7.77496845799998));
#245448=CARTESIAN_POINT('Ctrl Pts',(-7.17686866000006,15.2,7.77613414899999));
#245449=CARTESIAN_POINT('Ctrl Pts',(-7.17854259000006,15.2,7.77730232999998));
#245450=CARTESIAN_POINT('Ctrl Pts',(-7.18022328300005,15.2,7.77847298699999));
#245451=CARTESIAN_POINT('Ctrl Pts',(-7.18191073400006,15.2,7.77964609999999));
#245452=CARTESIAN_POINT('Ctrl Pts',(-7.18360493800006,15.2,7.78082165399999));
#245453=CARTESIAN_POINT('Ctrl Pts',(-7.18530588900006,15.2,7.78199962799999));
#245454=CARTESIAN_POINT('Ctrl Pts',(-7.18701358000006,15.2,7.78318000699999));
#245455=CARTESIAN_POINT('Ctrl Pts',(-7.18872800700006,15.2,7.78436277199998));
#245456=CARTESIAN_POINT('Ctrl Pts',(-7.19044916200006,15.2,7.78554790599999));
#245457=CARTESIAN_POINT('Ctrl Pts',(-7.19217704100005,15.2,7.78673539199998));
#245458=CARTESIAN_POINT('Ctrl Pts',(-7.19391163700006,15.2,7.78792521199998));
#245459=CARTESIAN_POINT('Ctrl Pts',(-7.19565294600006,15.2,7.78911734999999));
#245460=CARTESIAN_POINT('Ctrl Pts',(-7.19740096200006,15.2,7.79031178799999));
#245461=CARTESIAN_POINT('Ctrl Pts',(-7.19915567700006,15.2,7.79150850799999));
#245462=CARTESIAN_POINT('Ctrl Pts',(-7.20091708800005,15.2,7.79270749399998));
#245463=CARTESIAN_POINT('Ctrl Pts',(-7.20268518700006,15.2,7.79390872899998));
#245464=CARTESIAN_POINT('Ctrl Pts',(-7.20445997000006,15.2,7.79511219599998));
#245465=CARTESIAN_POINT('Ctrl Pts',(-7.20624143100006,15.2,7.79631787699999));
#245466=CARTESIAN_POINT('Ctrl Pts',(-7.20802956400005,15.2,7.79752575699998));
#245467=CARTESIAN_POINT('Ctrl Pts',(-7.20982436400006,15.2,7.79873581599999));
#245468=CARTESIAN_POINT('Ctrl Pts',(-7.21162582400006,15.2,7.79994804199998));
#245469=CARTESIAN_POINT('Ctrl Pts',(-7.21343393900006,15.2,7.80116241399998));
#245470=CARTESIAN_POINT('Ctrl Pts',(-7.21524870400006,15.2,7.80237891799998));
#245471=CARTESIAN_POINT('Ctrl Pts',(-7.21707011300006,15.2,7.80359753599999));
#245472=CARTESIAN_POINT('Ctrl Pts',(-7.21889815900006,15.2,7.80481825199999));
#245473=CARTESIAN_POINT('Ctrl Pts',(-7.22073283800006,15.2,7.80604104899999));
#245474=CARTESIAN_POINT('Ctrl Pts',(-7.22257414400006,15.2,7.80726591199999));
#245475=CARTESIAN_POINT('Ctrl Pts',(-7.22442207200006,15.2,7.80849282399998));
#245476=CARTESIAN_POINT('Ctrl Pts',(-7.22627661400006,15.2,7.80972176699999));
#245477=CARTESIAN_POINT('Ctrl Pts',(-7.22813776800006,15.2,7.81095272699999));
#245478=CARTESIAN_POINT('Ctrl Pts',(-7.23000552500006,15.2,7.81218568699998));
#245479=CARTESIAN_POINT('Ctrl Pts',(-7.23187988200006,15.2,7.81342063099999));
#245480=CARTESIAN_POINT('Ctrl Pts',(-7.23376083100006,15.2,7.81465754299998));
#245481=CARTESIAN_POINT('Ctrl Pts',(-7.23564836800006,15.2,7.81589640599999));
#245482=CARTESIAN_POINT('Ctrl Pts',(-7.23754248700006,15.2,7.81713720599999));
#245483=CARTESIAN_POINT('Ctrl Pts',(-7.23944318300005,15.2,7.81837992399999));
#245484=CARTESIAN_POINT('Ctrl Pts',(-7.24135045000006,15.2,7.81962454799999));
#245485=CARTESIAN_POINT('Ctrl Pts',(-7.24326428200006,15.2,7.82087105799998));
#245486=CARTESIAN_POINT('Ctrl Pts',(-7.24518467300006,15.2,7.82211944199998));
#245487=CARTESIAN_POINT('Ctrl Pts',(-7.24711162000006,15.2,7.82336968199999));
#245488=CARTESIAN_POINT('Ctrl Pts',(-7.24904511400006,15.2,7.82462176199999));
#245489=CARTESIAN_POINT('Ctrl Pts',(-7.25098515300005,15.2,7.82587566899998));
#245490=CARTESIAN_POINT('Ctrl Pts',(-7.25293172800006,15.2,7.82713138499999));
#245491=CARTESIAN_POINT('Ctrl Pts',(-7.25488483700006,15.2,7.82838889399999));
#245492=CARTESIAN_POINT('Ctrl Pts',(-7.25684447100006,15.2,7.82964818299998));
#245493=CARTESIAN_POINT('Ctrl Pts',(-7.25881062600005,15.2,7.83090923599998));
#245494=CARTESIAN_POINT('Ctrl Pts',(-7.26078329800006,15.2,7.83217203499999));
#245495=CARTESIAN_POINT('Ctrl Pts',(-7.26276247900006,15.2,7.83343656799998));
#245496=CARTESIAN_POINT('Ctrl Pts',(-7.26474816500006,15.2,7.83470281899999));
#245497=CARTESIAN_POINT('Ctrl Pts',(-7.26674035000006,15.2,7.83597076999998));
#245498=CARTESIAN_POINT('Ctrl Pts',(-7.26873902900006,15.2,7.83724040899998));
#245499=CARTESIAN_POINT('Ctrl Pts',(-7.27074419600005,15.2,7.83851171899999));
#245500=CARTESIAN_POINT('Ctrl Pts',(-7.27275584500005,15.2,7.83978468699999));
#245501=CARTESIAN_POINT('Ctrl Pts',(-7.27477397200006,15.2,7.84105929599999));
#245502=CARTESIAN_POINT('Ctrl Pts',(-7.27679857000005,15.2,7.84233553099998));
#245503=CARTESIAN_POINT('Ctrl Pts',(-7.27882963600006,15.2,7.84361337899998));
#245504=CARTESIAN_POINT('Ctrl Pts',(-7.28086716200006,15.2,7.84489282299998));
#245505=CARTESIAN_POINT('Ctrl Pts',(-7.28291114200006,15.2,7.84617384799999));
#245506=CARTESIAN_POINT('Ctrl Pts',(-7.28496157300006,15.2,7.84745644199998));
#245507=CARTESIAN_POINT('Ctrl Pts',(-7.28701844900006,15.2,7.84874058699998));
#245508=CARTESIAN_POINT('Ctrl Pts',(-7.28908176300005,15.2,7.85002626999999));
#245509=CARTESIAN_POINT('Ctrl Pts',(-7.29115151200006,15.2,7.85131347699998));
#245510=CARTESIAN_POINT('Ctrl Pts',(-7.29322768800006,15.2,7.85260219099998));
#245511=CARTESIAN_POINT('Ctrl Pts',(-7.29531028700006,15.2,7.85389239899998));
#245512=CARTESIAN_POINT('Ctrl Pts',(-7.29739930400005,15.2,7.85518408599999));
#245513=CARTESIAN_POINT('Ctrl Pts',(-7.29949473300006,15.2,7.85647723899999));
#245514=CARTESIAN_POINT('Ctrl Pts',(-7.30159656800006,15.2,7.85777184099998));
#245515=CARTESIAN_POINT('Ctrl Pts',(-7.30370480500006,15.2,7.85906787899999));
#245516=CARTESIAN_POINT('Ctrl Pts',(-7.30581943700006,15.2,7.86036533899999));
#245517=CARTESIAN_POINT('Ctrl Pts',(-7.30794046000006,15.2,7.86166420599999));
#245518=CARTESIAN_POINT('Ctrl Pts',(-7.31006786800006,15.2,7.86296446599999));
#245519=CARTESIAN_POINT('Ctrl Pts',(-7.31220165500006,15.2,7.86426610399998));
#245520=CARTESIAN_POINT('Ctrl Pts',(-7.31434181800006,15.2,7.86556910899999));
#245521=CARTESIAN_POINT('Ctrl Pts',(-7.31648834800006,15.2,7.86687346199999));
#245522=CARTESIAN_POINT('Ctrl Pts',(-7.31864124200006,15.2,7.86817915199999));
#245523=CARTESIAN_POINT('Ctrl Pts',(-7.32080049400006,15.2,7.86948616399999));
#245524=CARTESIAN_POINT('Ctrl Pts',(-7.32296610000006,15.2,7.87079448499998));
#245525=CARTESIAN_POINT('Ctrl Pts',(-7.32513805400006,15.2,7.87210409899998));
#245526=CARTESIAN_POINT('Ctrl Pts',(-7.32731634900006,15.2,7.87341499399999));
#245527=CARTESIAN_POINT('Ctrl Pts',(-7.32950098000006,15.2,7.87472715499998));
#245528=CARTESIAN_POINT('Ctrl Pts',(-7.33169194400006,15.2,7.87604056899998));
#245529=CARTESIAN_POINT('Ctrl Pts',(-7.33388923300006,15.2,7.87735522199998));
#245530=CARTESIAN_POINT('Ctrl Pts',(-7.33609284400006,15.2,7.87867109999999));
#245531=CARTESIAN_POINT('Ctrl Pts',(-7.33830277000005,15.2,7.87998818899998));
#245532=CARTESIAN_POINT('Ctrl Pts',(-7.34051900600006,15.2,7.88130647499998));
#245533=CARTESIAN_POINT('Ctrl Pts',(-7.34274154700006,15.2,7.88262594599999));
#245534=CARTESIAN_POINT('Ctrl Pts',(-7.34497038800006,15.2,7.88394658699998));
#245535=CARTESIAN_POINT('Ctrl Pts',(-7.34720552300006,15.2,7.88526838399999));
#245536=CARTESIAN_POINT('Ctrl Pts',(-7.34944694700006,15.2,7.88659132499999));
#245537=CARTESIAN_POINT('Ctrl Pts',(-7.35169465500006,15.2,7.88791539599998));
#245538=CARTESIAN_POINT('Ctrl Pts',(-7.35394864100006,15.2,7.88924058299998));
#245539=CARTESIAN_POINT('Ctrl Pts',(-7.35620890000006,15.2,7.89056687299999));
#245540=CARTESIAN_POINT('Ctrl Pts',(-7.35847542700006,15.2,7.89189425299998));
#245541=CARTESIAN_POINT('Ctrl Pts',(-7.36074821700006,15.2,7.89322270699999));
#245542=CARTESIAN_POINT('Ctrl Pts',(-7.36302726400006,15.2,7.89455222599998));
#245543=CARTESIAN_POINT('Ctrl Pts',(-7.36531256300006,15.2,7.89588279499998));
#245544=CARTESIAN_POINT('Ctrl Pts',(-7.36760410800006,15.2,7.89721439899999));
#245545=CARTESIAN_POINT('Ctrl Pts',(-7.36990189600006,15.2,7.89854702799998));
#245546=CARTESIAN_POINT('Ctrl Pts',(-7.37220591900006,15.2,7.89988066499999));
#245547=CARTESIAN_POINT('Ctrl Pts',(-7.37451617400006,15.2,7.90121529999999));
#245548=CARTESIAN_POINT('Ctrl Pts',(-7.37683265400006,15.2,7.90255091899999));
#245549=CARTESIAN_POINT('Ctrl Pts',(-7.37915535500006,15.2,7.90388750999998));
#245550=CARTESIAN_POINT('Ctrl Pts',(-7.38148427100006,15.2,7.90522505699998));
#245551=CARTESIAN_POINT('Ctrl Pts',(-7.38381939700006,15.2,7.90656354999999));
#245552=CARTESIAN_POINT('Ctrl Pts',(-7.38616072800006,15.2,7.90790297499999));
#245553=CARTESIAN_POINT('Ctrl Pts',(-7.38850825800006,15.2,7.90924331999998));
#245554=CARTESIAN_POINT('Ctrl Pts',(-7.39086198300006,15.2,7.91058456999998));
#245555=CARTESIAN_POINT('Ctrl Pts',(-7.39322189600006,15.2,7.91192671399998));
#245556=CARTESIAN_POINT('Ctrl Pts',(-7.39558799400006,15.2,7.91326973999999));
#245557=CARTESIAN_POINT('Ctrl Pts',(-7.39796027100006,15.2,7.91461363299998));
#245558=CARTESIAN_POINT('Ctrl Pts',(-7.40033872100006,15.2,7.91595838099998));
#245559=CARTESIAN_POINT('Ctrl Pts',(-7.40272333900006,15.2,7.91730397299999));
#245560=CARTESIAN_POINT('Ctrl Pts',(-7.40511412000005,15.2,7.91865039499999));
#245561=CARTESIAN_POINT('Ctrl Pts',(-7.40751105900006,15.2,7.91999763299999));
#245562=CARTESIAN_POINT('Ctrl Pts',(-7.40991415200006,15.2,7.92134567699998));
#245563=CARTESIAN_POINT('Ctrl Pts',(-7.41232339100006,15.2,7.92269451299998));
#245564=CARTESIAN_POINT('Ctrl Pts',(-7.41473877300006,15.2,7.92404412999999));
#245565=CARTESIAN_POINT('Ctrl Pts',(-7.41716029100006,15.2,7.92539451399998));
#245566=CARTESIAN_POINT('Ctrl Pts',(-7.41958794200006,15.2,7.92674565199999));
#245567=CARTESIAN_POINT('Ctrl Pts',(-7.42202171900006,15.2,7.92809753399998));
#245568=CARTESIAN_POINT('Ctrl Pts',(-7.42446161900006,15.2,7.92945014599999));
#245569=CARTESIAN_POINT('Ctrl Pts',(-7.42690763400006,15.2,7.93080347599999));
#245570=CARTESIAN_POINT('Ctrl Pts',(-7.42935976100005,15.2,7.93215751199998));
#245571=CARTESIAN_POINT('Ctrl Pts',(-7.43181799400006,15.2,7.93351224099998));
#245572=CARTESIAN_POINT('Ctrl Pts',(-7.43428232700006,15.2,7.93486765199999));
#245573=CARTESIAN_POINT('Ctrl Pts',(-7.43675275700006,15.2,7.93622373199998));
#245574=CARTESIAN_POINT('Ctrl Pts',(-7.43922927800006,15.2,7.93758046899999));
#245575=CARTESIAN_POINT('Ctrl Pts',(-7.44171188300006,15.2,7.93893784999998));
#245576=CARTESIAN_POINT('Ctrl Pts',(-7.44420057000006,15.2,7.94029586499998));
#245577=CARTESIAN_POINT('Ctrl Pts',(-7.44669533100006,15.2,7.94165450099998));
#245578=CARTESIAN_POINT('Ctrl Pts',(-7.44919616200006,15.2,7.94301374399998));
#245579=CARTESIAN_POINT('Ctrl Pts',(-7.45170305800006,15.2,7.94437358599998));
#245580=CARTESIAN_POINT('Ctrl Pts',(-7.45421601400006,15.2,7.94573401099999));
#245581=CARTESIAN_POINT('Ctrl Pts',(-7.45673502500006,15.2,7.94709500999998));
#245582=CARTESIAN_POINT('Ctrl Pts',(-7.45926008500006,15.2,7.94845657099999));
#245583=CARTESIAN_POINT('Ctrl Pts',(-7.46179119000006,15.2,7.94981867899998));
#245584=CARTESIAN_POINT('Ctrl Pts',(-7.46432833400006,15.2,7.95118132499999));
#245585=CARTESIAN_POINT('Ctrl Pts',(-7.46687151300006,15.2,7.95254449699998));
#245586=CARTESIAN_POINT('Ctrl Pts',(-7.46942072000006,15.2,7.95390818299998));
#245587=CARTESIAN_POINT('Ctrl Pts',(-7.47197595100006,15.2,7.95527237099999));
#245588=CARTESIAN_POINT('Ctrl Pts',(-7.47453720200006,15.2,7.95663704999999));
#245589=CARTESIAN_POINT('Ctrl Pts',(-7.47710446500006,15.2,7.95800220799999));
#245590=CARTESIAN_POINT('Ctrl Pts',(-7.47967773800006,15.2,7.95936783099998));
#245591=CARTESIAN_POINT('Ctrl Pts',(-7.48225701500006,15.2,7.96073391199998));
#245592=CARTESIAN_POINT('Ctrl Pts',(-7.48484228800006,15.2,7.96210043599999));
#245593=CARTESIAN_POINT('Ctrl Pts',(-7.48743355700006,15.2,7.96346739199999));
#245594=CARTESIAN_POINT('Ctrl Pts',(-7.49003081300006,15.2,7.96483476999998));
#245595=CARTESIAN_POINT('Ctrl Pts',(-7.49263405300006,15.2,7.96620255599999));
#245596=CARTESIAN_POINT('Ctrl Pts',(-7.49524327100006,15.2,7.96757074199999));
#245597=CARTESIAN_POINT('Ctrl Pts',(-7.49785846200006,15.2,7.96893931299999));
#245598=CARTESIAN_POINT('Ctrl Pts',(-7.50047962100006,15.2,7.97030825999999));
#245599=CARTESIAN_POINT('Ctrl Pts',(-7.50310674300006,15.2,7.97167757099999));
#245600=CARTESIAN_POINT('Ctrl Pts',(-7.50573982300006,15.2,7.97304723499998));
#245601=CARTESIAN_POINT('Ctrl Pts',(-7.50837885500006,15.2,7.97441723899999));
#245602=CARTESIAN_POINT('Ctrl Pts',(-7.51102383600006,15.2,7.97578757299998));
#245603=CARTESIAN_POINT('Ctrl Pts',(-7.51367475900006,15.2,7.97715822699999));
#245604=CARTESIAN_POINT('Ctrl Pts',(-7.51633162000005,15.2,7.97852918799999));
#245605=CARTESIAN_POINT('Ctrl Pts',(-7.51899441200005,15.2,7.97990044499999));
#245606=CARTESIAN_POINT('Ctrl Pts',(-7.52166313300006,15.2,7.98127198799998));
#245607=CARTESIAN_POINT('Ctrl Pts',(-7.52433777600006,15.2,7.98264380499998));
#245608=CARTESIAN_POINT('Ctrl Pts',(-7.52701833700005,15.2,7.98401588399998));
#245609=CARTESIAN_POINT('Ctrl Pts',(-7.52970481000006,15.2,7.98538821699999));
#245610=CARTESIAN_POINT('Ctrl Pts',(-7.53239719100005,15.2,7.98676078899998));
#245611=CARTESIAN_POINT('Ctrl Pts',(-7.53509547300006,15.2,7.98813359199999));
#245612=CARTESIAN_POINT('Ctrl Pts',(-7.53779965400006,15.2,7.98950661499998));
#245613=CARTESIAN_POINT('Ctrl Pts',(-7.54050972500006,15.2,7.99087984499998));
#245614=CARTESIAN_POINT('Ctrl Pts',(-7.54322568500006,15.2,7.99225327099998));
#245615=CARTESIAN_POINT('Ctrl Pts',(-7.54594752700006,15.2,7.99362688499999));
#245616=CARTESIAN_POINT('Ctrl Pts',(-7.54867524600006,15.2,7.99500067299999));
#245617=CARTESIAN_POINT('Ctrl Pts',(-7.55140883700006,15.2,7.99637462699998));
#245618=CARTESIAN_POINT('Ctrl Pts',(-7.55414829500006,15.2,7.99774873399999));
#245619=CARTESIAN_POINT('Ctrl Pts',(-7.55689361600006,15.2,7.99912298399998));
#245620=CARTESIAN_POINT('Ctrl Pts',(-7.55964479300006,15.2,8.00049736599998));
#245621=CARTESIAN_POINT('Ctrl Pts',(-7.56240182300005,15.2,8.00187187099999));
#245622=CARTESIAN_POINT('Ctrl Pts',(-7.56516470000006,15.2,8.00324648399998));
#245623=CARTESIAN_POINT('Ctrl Pts',(-7.56793341800006,15.2,8.00462119899999));
#245624=CARTESIAN_POINT('Ctrl Pts',(-7.57070797500005,15.2,8.00599600399998));
#245625=CARTESIAN_POINT('Ctrl Pts',(-7.57348836300006,15.2,8.00737088699999));
#245626=CARTESIAN_POINT('Ctrl Pts',(-7.57627457800006,15.2,8.00874583799999));
#245627=CARTESIAN_POINT('Ctrl Pts',(-7.57906661600006,15.2,8.01012084699998));
#245628=CARTESIAN_POINT('Ctrl Pts',(-7.58186447000006,15.2,8.01149590299998));
#245629=CARTESIAN_POINT('Ctrl Pts',(-7.58466813600006,15.2,8.01287099699999));
#245630=CARTESIAN_POINT('Ctrl Pts',(-7.58747761100006,15.2,8.01424611599998));
#245631=CARTESIAN_POINT('Ctrl Pts',(-7.59029288700006,15.2,8.01562125099998));
#245632=CARTESIAN_POINT('Ctrl Pts',(-7.59311396000006,15.2,8.01699639099999));
#245633=CARTESIAN_POINT('Ctrl Pts',(-7.59594082600006,15.2,8.01837152699999));
#245634=CARTESIAN_POINT('Ctrl Pts',(-7.59877347800006,15.2,8.01974664699999));
#245635=CARTESIAN_POINT('Ctrl Pts',(-7.60161191400006,15.2,8.02112174099998));
#245636=CARTESIAN_POINT('Ctrl Pts',(-7.60445612600006,15.2,8.02249679899998));
#245637=CARTESIAN_POINT('Ctrl Pts',(-7.60730611100006,15.2,8.02387180999999));
#245638=CARTESIAN_POINT('Ctrl Pts',(-7.61016186300005,15.2,8.02524676499999));
#245639=CARTESIAN_POINT('Ctrl Pts',(-7.61302337700006,15.2,8.02662165399998));
#245640=CARTESIAN_POINT('Ctrl Pts',(-7.61589065000006,15.2,8.02799646399999));
#245641=CARTESIAN_POINT('Ctrl Pts',(-7.61876367500006,15.2,8.02937118799999));
#245642=CARTESIAN_POINT('Ctrl Pts',(-7.62164244700006,15.2,8.03074581399999));
#245643=CARTESIAN_POINT('Ctrl Pts',(-7.62452696100006,15.2,8.03212033199999));
#245644=CARTESIAN_POINT('Ctrl Pts',(-7.62741721300006,15.2,8.03349473299999));
#245645=CARTESIAN_POINT('Ctrl Pts',(-7.63031319900006,15.2,8.03486900599999));
#245646=CARTESIAN_POINT('Ctrl Pts',(-7.63321491200006,15.2,8.03624313999999));
#245647=CARTESIAN_POINT('Ctrl Pts',(-7.63612234700006,15.2,8.03761712699998));
#245648=CARTESIAN_POINT('Ctrl Pts',(-7.63903550100006,15.2,8.03899095599999));
#245649=CARTESIAN_POINT('Ctrl Pts',(-7.64195436800006,15.2,8.04036461599999));
#245650=CARTESIAN_POINT('Ctrl Pts',(-7.64487894200006,15.2,8.04173809899999));
#245651=CARTESIAN_POINT('Ctrl Pts',(-7.64780922000006,15.2,8.04311139499998));
#245652=CARTESIAN_POINT('Ctrl Pts',(-7.65074519600006,15.2,8.04448449199998));
#245653=CARTESIAN_POINT('Ctrl Pts',(-7.65368686500006,15.2,8.04585738099998));
#245654=CARTESIAN_POINT('Ctrl Pts',(-7.65663422300006,15.2,8.04723005299999));
#245655=CARTESIAN_POINT('Ctrl Pts',(-7.65958726300005,15.2,8.04860249699999));
#245656=CARTESIAN_POINT('Ctrl Pts',(-7.66254598200005,15.2,8.04997470299998));
#245657=CARTESIAN_POINT('Ctrl Pts',(-7.66551037500006,15.2,8.05134666399999));
#245658=CARTESIAN_POINT('Ctrl Pts',(-7.66848043700006,15.2,8.05271836699998));
#245659=CARTESIAN_POINT('Ctrl Pts',(-7.67145616200006,15.2,8.05408980299998));
#245660=CARTESIAN_POINT('Ctrl Pts',(-7.67443754600006,15.2,8.05546096299998));
#245661=CARTESIAN_POINT('Ctrl Pts',(-7.67742458300006,15.2,8.05683183699998));
#245662=CARTESIAN_POINT('Ctrl Pts',(-7.68041727000006,15.2,8.05820241499998));
#245663=CARTESIAN_POINT('Ctrl Pts',(-7.68341560100006,15.2,8.05957268799999));
#245664=CARTESIAN_POINT('Ctrl Pts',(-7.68641957100006,15.2,8.06094264599999));
#245665=CARTESIAN_POINT('Ctrl Pts',(-7.68942917500006,15.2,8.06231227899998));
#245666=CARTESIAN_POINT('Ctrl Pts',(-7.69244440900006,15.2,8.06368157799999));
#245667=CARTESIAN_POINT('Ctrl Pts',(-7.69546526600006,15.2,8.06505053299999));
#245668=CARTESIAN_POINT('Ctrl Pts',(-7.69849174400005,15.2,8.06641913399999));
#245669=CARTESIAN_POINT('Ctrl Pts',(-7.70152383600006,15.2,8.06778737399998));
#245670=CARTESIAN_POINT('Ctrl Pts',(-7.70456153900006,15.2,8.06915523999999));
#245671=CARTESIAN_POINT('Ctrl Pts',(-7.70760484600006,15.2,8.07052272399999));
#245672=CARTESIAN_POINT('Ctrl Pts',(-7.71065375300005,15.2,8.07188981699999));
#245673=CARTESIAN_POINT('Ctrl Pts',(-7.71370825500006,15.2,8.07325650899998));
#245674=CARTESIAN_POINT('Ctrl Pts',(-7.71676834800005,15.2,8.07462279199999));
#245675=CARTESIAN_POINT('Ctrl Pts',(-7.71983402500006,15.2,8.07598865399999));
#245676=CARTESIAN_POINT('Ctrl Pts',(-7.72290528400006,15.2,8.07735408899998));
#245677=CARTESIAN_POINT('Ctrl Pts',(-7.72598211700006,15.2,8.07871908399999));
#245678=CARTESIAN_POINT('Ctrl Pts',(-7.72906452200005,15.2,8.08008363199999));
#245679=CARTESIAN_POINT('Ctrl Pts',(-7.73215249300006,15.2,8.08144772299999));
#245680=CARTESIAN_POINT('Ctrl Pts',(-7.73524602400006,15.2,8.08281134799999));
#245681=CARTESIAN_POINT('Ctrl Pts',(-7.73834511100005,15.2,8.08417449699999));
#245682=CARTESIAN_POINT('Ctrl Pts',(-7.74144975100005,15.2,8.08553716199999));
#245683=CARTESIAN_POINT('Ctrl Pts',(-7.74455993600006,15.2,8.08689933299998));
#245684=CARTESIAN_POINT('Ctrl Pts',(-7.74767566300006,15.2,8.08826100099999));
#245685=CARTESIAN_POINT('Ctrl Pts',(-7.75079692700006,15.2,8.08962215699999));
#245686=CARTESIAN_POINT('Ctrl Pts',(-7.75392372200006,15.2,8.09098279099998));
#245687=CARTESIAN_POINT('Ctrl Pts',(-7.75705604400006,15.2,8.09234289499998));
#245688=CARTESIAN_POINT('Ctrl Pts',(-7.76019388900006,15.2,8.09370245899999));
#245689=CARTESIAN_POINT('Ctrl Pts',(-7.76333725000006,15.2,8.09506147499999));
#245690=CARTESIAN_POINT('Ctrl Pts',(-7.76648612500006,15.2,8.09641993199998));
#245691=CARTESIAN_POINT('Ctrl Pts',(-7.76964050600006,15.2,8.09777782399999));
#245692=CARTESIAN_POINT('Ctrl Pts',(-7.77280039100006,15.2,8.09913513899998));
#245693=CARTESIAN_POINT('Ctrl Pts',(-7.77596577300006,15.2,8.10049186899998));
#245694=CARTESIAN_POINT('Ctrl Pts',(-7.77913664800005,15.2,8.10184800599998));
#245695=CARTESIAN_POINT('Ctrl Pts',(-7.78231301200006,15.2,8.10320353899998));
#245696=CARTESIAN_POINT('Ctrl Pts',(-7.78549485900006,15.2,8.10455846299998));
#245697=CARTESIAN_POINT('Ctrl Pts',(-7.78868218500006,15.2,8.10591276399999));
#245698=CARTESIAN_POINT('Ctrl Pts',(-7.79187498300006,15.2,8.10726643599999));
#245699=CARTESIAN_POINT('Ctrl Pts',(-7.79507325100005,15.2,8.10861946999999));
#245700=CARTESIAN_POINT('Ctrl Pts',(-7.79827698300006,15.2,8.10997185699998));
#245701=CARTESIAN_POINT('Ctrl Pts',(-7.80148617400006,15.2,8.11132358799998));
#245702=CARTESIAN_POINT('Ctrl Pts',(-7.80470082000006,15.2,8.11267465299998));
#245703=CARTESIAN_POINT('Ctrl Pts',(-7.80792091500006,15.2,8.11402504599998));
#245704=CARTESIAN_POINT('Ctrl Pts',(-7.81114645400006,15.2,8.11537475499998));
#245705=CARTESIAN_POINT('Ctrl Pts',(-7.81437743500006,15.2,8.11672377399999));
#245706=CARTESIAN_POINT('Ctrl Pts',(-7.81761384900006,15.2,8.11807209299998));
#245707=CARTESIAN_POINT('Ctrl Pts',(-7.82085569500006,15.2,8.11941970299999));
#245708=CARTESIAN_POINT('Ctrl Pts',(-7.82410296500006,15.2,8.12076659599999));
#245709=CARTESIAN_POINT('Ctrl Pts',(-7.82735565600006,15.2,8.12211276299998));
#245710=CARTESIAN_POINT('Ctrl Pts',(-7.83061376200005,15.2,8.12345819399999));
#245711=CARTESIAN_POINT('Ctrl Pts',(-7.83387728100006,15.2,8.12480288399998));
#245712=CARTESIAN_POINT('Ctrl Pts',(-7.83714620400006,15.2,8.12614681999998));
#245713=CARTESIAN_POINT('Ctrl Pts',(-7.84042053000006,15.2,8.12748999699998));
#245714=CARTESIAN_POINT('Ctrl Pts',(-7.84370025300006,15.2,8.12883240399999));
#245715=CARTESIAN_POINT('Ctrl Pts',(-7.84698536600006,15.2,8.13017403499998));
#245716=CARTESIAN_POINT('Ctrl Pts',(-7.85027586700006,15.2,8.13151487799999));
#245717=CARTESIAN_POINT('Ctrl Pts',(-7.85357175000006,15.2,8.13285492699999));
#245718=CARTESIAN_POINT('Ctrl Pts',(-7.85687301000006,15.2,8.13419417299999));
#245719=CARTESIAN_POINT('Ctrl Pts',(-7.86017964300005,15.2,8.13553260699998));
#245720=CARTESIAN_POINT('Ctrl Pts',(-7.86349164400006,15.2,8.13687022099998));
#245721=CARTESIAN_POINT('Ctrl Pts',(-7.86680900800006,15.2,8.13820700699999));
#245722=CARTESIAN_POINT('Ctrl Pts',(-7.87013173000006,15.2,8.13954295599999));
#245723=CARTESIAN_POINT('Ctrl Pts',(-7.87345980500006,15.2,8.14087805999998));
#245724=CARTESIAN_POINT('Ctrl Pts',(-7.87679322900006,15.2,8.14221230999999));
#245725=CARTESIAN_POINT('Ctrl Pts',(-7.88013199700006,15.2,8.14354569699999));
#245726=CARTESIAN_POINT('Ctrl Pts',(-7.88347610400006,15.2,8.14487821399998));
#245727=CARTESIAN_POINT('Ctrl Pts',(-7.88682554500006,15.2,8.14620985299998));
#245728=CARTESIAN_POINT('Ctrl Pts',(-7.89018031600006,15.2,8.14754060399999));
#245729=CARTESIAN_POINT('Ctrl Pts',(-7.89354041200006,15.2,8.14887045999999));
#245730=CARTESIAN_POINT('Ctrl Pts',(-7.89690582700005,15.2,8.15019941199999));
#245731=CARTESIAN_POINT('Ctrl Pts',(-7.90027655700006,15.2,8.15152745299999));
#245732=CARTESIAN_POINT('Ctrl Pts',(-7.90365259800006,15.2,8.15285457299998));
#245733=CARTESIAN_POINT('Ctrl Pts',(-7.90703394500006,15.2,8.15418076499999));
#245734=CARTESIAN_POINT('Ctrl Pts',(-7.91042059300005,15.2,8.15550602099999));
#245735=CARTESIAN_POINT('Ctrl Pts',(-7.91381253600005,15.2,8.15683033199999));
#245736=CARTESIAN_POINT('Ctrl Pts',(-7.91720977000006,15.2,8.15815368899998));
#245737=CARTESIAN_POINT('Ctrl Pts',(-7.92061229100005,15.2,8.15947608599998));
#245738=CARTESIAN_POINT('Ctrl Pts',(-7.92402009400006,15.2,8.16079751399998));
#245739=CARTESIAN_POINT('Ctrl Pts',(-7.92743317500006,15.2,8.16211796399998));
#245740=CARTESIAN_POINT('Ctrl Pts',(-7.93085152700005,15.2,8.16343742899999));
#245741=CARTESIAN_POINT('Ctrl Pts',(-7.93427514700006,15.2,8.16475590099999));
#245742=CARTESIAN_POINT('Ctrl Pts',(-7.93770402900006,15.2,8.16607337199999));
#245743=CARTESIAN_POINT('Ctrl Pts',(-7.94113817000006,15.2,8.16738983299999));
#245744=CARTESIAN_POINT('Ctrl Pts',(-7.94457756400006,15.2,8.16870527599999));
#245745=CARTESIAN_POINT('Ctrl Pts',(-7.94802220600006,15.2,8.17001969299999));
#245746=CARTESIAN_POINT('Ctrl Pts',(-7.95147209200006,15.2,8.17133307699999));
#245747=CARTESIAN_POINT('Ctrl Pts',(-7.95492721600005,15.2,8.17264541999998));
#245748=CARTESIAN_POINT('Ctrl Pts',(-7.95838757500006,15.2,8.17395671299998));
#245749=CARTESIAN_POINT('Ctrl Pts',(-7.96185316300006,15.2,8.17526694799999));
#245750=CARTESIAN_POINT('Ctrl Pts',(-7.96532397700006,15.2,8.17657611899998));
#245751=CARTESIAN_POINT('Ctrl Pts',(-7.96880001000006,15.2,8.17788421699999));
#245752=CARTESIAN_POINT('Ctrl Pts',(-7.97228126000006,15.2,8.17919123499999));
#245753=CARTESIAN_POINT('Ctrl Pts',(-7.97576771900006,15.2,8.18049716399998));
#245754=CARTESIAN_POINT('Ctrl Pts',(-7.97925938500006,15.2,8.18180199599999));
#245755=CARTESIAN_POINT('Ctrl Pts',(-7.98275625000005,15.2,8.18310572199999));
#245756=CARTESIAN_POINT('Ctrl Pts',(-7.98625831300006,15.2,8.18440833599999));
#245757=CARTESIAN_POINT('Ctrl Pts',(-7.98976556600006,15.2,8.18570982799999));
#245758=CARTESIAN_POINT('Ctrl Pts',(-7.99327800400006,15.2,8.18701019299999));
#245759=CARTESIAN_POINT('Ctrl Pts',(-7.99679562600006,15.2,8.18830942099999));
#245760=CARTESIAN_POINT('Ctrl Pts',(-8.00031842500006,15.2,8.18960750499999));
#245761=CARTESIAN_POINT('Ctrl Pts',(-8.00384639600006,15.2,8.19090443999999));
#245762=CARTESIAN_POINT('Ctrl Pts',(-8.00737953700006,15.2,8.19220021799998));
#245763=CARTESIAN_POINT('Ctrl Pts',(-8.01091784300005,15.2,8.19349483199998));
#245764=CARTESIAN_POINT('Ctrl Pts',(-8.01446130800005,15.2,8.19478827199998));
#245765=CARTESIAN_POINT('Ctrl Pts',(-8.01800992700005,15.2,8.19608053199998));
#245766=CARTESIAN_POINT('Ctrl Pts',(-8.02156369500005,15.2,8.19737160199999));
#245767=CARTESIAN_POINT('Ctrl Pts',(-8.02512260400006,15.2,8.19866146999999));
#245768=CARTESIAN_POINT('Ctrl Pts',(-8.02868665100006,15.2,8.19995012899999));
#245769=CARTESIAN_POINT('Ctrl Pts',(-8.03225583000006,15.2,8.20123757099999));
#245770=CARTESIAN_POINT('Ctrl Pts',(-8.03583013500005,15.2,8.20252378799999));
#245771=CARTESIAN_POINT('Ctrl Pts',(-8.03940956400006,15.2,8.20380877499998));
#245772=CARTESIAN_POINT('Ctrl Pts',(-8.04299411600006,15.2,8.20509252899999));
#245773=CARTESIAN_POINT('Ctrl Pts',(-8.04658378800006,15.2,8.20637504799999));
#245774=CARTESIAN_POINT('Ctrl Pts',(-8.04945962200006,15.2,8.20740007499998));
#245775=CARTESIAN_POINT('Ctrl Pts',(-8.05161880100006,15.2,8.20816828899999));
#245776=CARTESIAN_POINT('Ctrl Pts',(-8.05305927800006,15.2,8.20868018399998));
#245777=CARTESIAN_POINT('Ctrl Pts',(-8.05377977200006,15.2,8.20893606999999));
#245778=CARTESIAN_POINT('Ctrl Pts',(-7.01216898600006,12.2,7.64657512399998));
#245779=CARTESIAN_POINT('Ctrl Pts',(-7.01229743700006,12.2,7.64669302599999));
#245780=CARTESIAN_POINT('Ctrl Pts',(-7.01255888300006,12.2,7.64693288499998));
#245781=CARTESIAN_POINT('Ctrl Pts',(-7.01295521800006,12.2,7.64729613499998));
#245782=CARTESIAN_POINT('Ctrl Pts',(-7.01348948000006,12.2,7.64778506499999));
#245783=CARTESIAN_POINT('Ctrl Pts',(-7.01416585900006,12.2,7.64840281599999));
#245784=CARTESIAN_POINT('Ctrl Pts',(-7.01485383100006,12.2,7.64902988999999));
#245785=CARTESIAN_POINT('Ctrl Pts',(-7.01554947000006,12.2,7.64966267399998));
#245786=CARTESIAN_POINT('Ctrl Pts',(-7.01625276700006,12.2,7.65030113899999));
#245787=CARTESIAN_POINT('Ctrl Pts',(-7.01696371600006,12.2,7.65094525299999));
#245788=CARTESIAN_POINT('Ctrl Pts',(-7.01768230900006,12.2,7.65159498499998));
#245789=CARTESIAN_POINT('Ctrl Pts',(-7.01840853600006,12.2,7.65225030299998));
#245790=CARTESIAN_POINT('Ctrl Pts',(-7.01914239300006,12.2,7.65291117499999));
#245791=CARTESIAN_POINT('Ctrl Pts',(-7.01988387000006,12.2,7.65357757299999));
#245792=CARTESIAN_POINT('Ctrl Pts',(-7.02063296000006,12.2,7.65424946399998));
#245793=CARTESIAN_POINT('Ctrl Pts',(-7.02138965700006,12.2,7.65492681899998));
#245794=CARTESIAN_POINT('Ctrl Pts',(-7.02215395000006,12.2,7.65560960799998));
#245795=CARTESIAN_POINT('Ctrl Pts',(-7.02292583400006,12.2,7.65629779899999));
#245796=CARTESIAN_POINT('Ctrl Pts',(-7.02370530000006,12.2,7.65699136299999));
#245797=CARTESIAN_POINT('Ctrl Pts',(-7.02449234200006,12.2,7.65769026899999));
#245798=CARTESIAN_POINT('Ctrl Pts',(-7.02528695100006,12.2,7.65839448899998));
#245799=CARTESIAN_POINT('Ctrl Pts',(-7.02608912200006,12.2,7.65910399299998));
#245800=CARTESIAN_POINT('Ctrl Pts',(-7.02689884500006,12.2,7.65981874999999));
#245801=CARTESIAN_POINT('Ctrl Pts',(-7.02771611300006,12.2,7.66053873299998));
#245802=CARTESIAN_POINT('Ctrl Pts',(-7.02854092000006,12.2,7.66126390999998));
#245803=CARTESIAN_POINT('Ctrl Pts',(-7.02937325800006,12.2,7.66199425499998));
#245804=CARTESIAN_POINT('Ctrl Pts',(-7.03021311900006,12.2,7.66272973699999));
#245805=CARTESIAN_POINT('Ctrl Pts',(-7.03106049600006,12.2,7.66347032799998));
#245806=CARTESIAN_POINT('Ctrl Pts',(-7.03191538200006,12.2,7.66421599899999));
#245807=CARTESIAN_POINT('Ctrl Pts',(-7.03277777000006,12.2,7.66496672199998));
#245808=CARTESIAN_POINT('Ctrl Pts',(-7.03364765200006,12.2,7.66572246899998));
#245809=CARTESIAN_POINT('Ctrl Pts',(-7.03452502100006,12.2,7.66648321099999));
#245810=CARTESIAN_POINT('Ctrl Pts',(-7.03540987000006,12.2,7.66724892099998));
#245811=CARTESIAN_POINT('Ctrl Pts',(-7.03630219100006,12.2,7.66801956799998));
#245812=CARTESIAN_POINT('Ctrl Pts',(-7.03720197800005,12.2,7.66879512799999));
#245813=CARTESIAN_POINT('Ctrl Pts',(-7.03810922400006,12.2,7.66957557299998));
#245814=CARTESIAN_POINT('Ctrl Pts',(-7.03902392100006,12.2,7.67036087199998));
#245815=CARTESIAN_POINT('Ctrl Pts',(-7.03994606100006,12.2,7.67115099999998));
#245816=CARTESIAN_POINT('Ctrl Pts',(-7.04087563900006,12.2,7.67194592999999));
#245817=CARTESIAN_POINT('Ctrl Pts',(-7.04181264600006,12.2,7.67274563399998));
#245818=CARTESIAN_POINT('Ctrl Pts',(-7.04275707700006,12.2,7.67355008599999));
#245819=CARTESIAN_POINT('Ctrl Pts',(-7.04370892200005,12.2,7.67435925699999));
#245820=CARTESIAN_POINT('Ctrl Pts',(-7.04466817800006,12.2,7.67517312299999));
#245821=CARTESIAN_POINT('Ctrl Pts',(-7.04563483400006,12.2,7.67599165499998));
#245822=CARTESIAN_POINT('Ctrl Pts',(-7.04660888600006,12.2,7.67681482699999));
#245823=CARTESIAN_POINT('Ctrl Pts',(-7.04759032400006,12.2,7.67764261299998));
#245824=CARTESIAN_POINT('Ctrl Pts',(-7.04857914400006,12.2,7.67847498699999));
#245825=CARTESIAN_POINT('Ctrl Pts',(-7.04957533900005,12.2,7.67931192299999));
#245826=CARTESIAN_POINT('Ctrl Pts',(-7.05057890000006,12.2,7.68015339299998));
#245827=CARTESIAN_POINT('Ctrl Pts',(-7.05158982000006,12.2,7.68099937399998));
#245828=CARTESIAN_POINT('Ctrl Pts',(-7.05260809400006,12.2,7.68184983699999));
#245829=CARTESIAN_POINT('Ctrl Pts',(-7.05363371500006,12.2,7.68270475799999));
#245830=CARTESIAN_POINT('Ctrl Pts',(-7.05466667400006,12.2,7.68356411099998));
#245831=CARTESIAN_POINT('Ctrl Pts',(-7.05570696700006,12.2,7.68442787099998));
#245832=CARTESIAN_POINT('Ctrl Pts',(-7.05675458400005,12.2,7.68529601199998));
#245833=CARTESIAN_POINT('Ctrl Pts',(-7.05780952100006,12.2,7.68616850899999));
#245834=CARTESIAN_POINT('Ctrl Pts',(-7.05887177100006,12.2,7.68704533799998));
#245835=CARTESIAN_POINT('Ctrl Pts',(-7.05994132500006,12.2,7.68792647199999));
#245836=CARTESIAN_POINT('Ctrl Pts',(-7.06101817900006,12.2,7.68881188699999));
#245837=CARTESIAN_POINT('Ctrl Pts',(-7.06210232400006,12.2,7.68970155699999));
#245838=CARTESIAN_POINT('Ctrl Pts',(-7.06319375500006,12.2,7.69059545999998));
#245839=CARTESIAN_POINT('Ctrl Pts',(-7.06429246300006,12.2,7.69149356899998));
#245840=CARTESIAN_POINT('Ctrl Pts',(-7.06539844400006,12.2,7.69239585999999));
#245841=CARTESIAN_POINT('Ctrl Pts',(-7.06651169000006,12.2,7.69330230899998));
#245842=CARTESIAN_POINT('Ctrl Pts',(-7.06763219400006,12.2,7.69421289099999));
#245843=CARTESIAN_POINT('Ctrl Pts',(-7.06875995000006,12.2,7.69512758399999));
#245844=CARTESIAN_POINT('Ctrl Pts',(-7.06989495100006,12.2,7.69604635999999));
#245845=CARTESIAN_POINT('Ctrl Pts',(-7.07103719100005,12.2,7.69696919799999));
#245846=CARTESIAN_POINT('Ctrl Pts',(-7.07218666200006,12.2,7.69789607499998));
#245847=CARTESIAN_POINT('Ctrl Pts',(-7.07334335900006,12.2,7.69882696299998));
#245848=CARTESIAN_POINT('Ctrl Pts',(-7.07450727400006,12.2,7.69976184299999));
#245849=CARTESIAN_POINT('Ctrl Pts',(-7.07567840200006,12.2,7.70070068799999));
#245850=CARTESIAN_POINT('Ctrl Pts',(-7.07685673500006,12.2,7.70164347599999));
#245851=CARTESIAN_POINT('Ctrl Pts',(-7.07804226800006,12.2,7.70259018399998));
#245852=CARTESIAN_POINT('Ctrl Pts',(-7.07923499300006,12.2,7.70354078799999));
#245853=CARTESIAN_POINT('Ctrl Pts',(-7.08043490300006,12.2,7.70449526499998));
#245854=CARTESIAN_POINT('Ctrl Pts',(-7.08164199400006,12.2,7.70545359099999));
#245855=CARTESIAN_POINT('Ctrl Pts',(-7.08285625800006,12.2,7.70641574499999));
#245856=CARTESIAN_POINT('Ctrl Pts',(-7.08407768800006,12.2,7.70738170199999));
#245857=CARTESIAN_POINT('Ctrl Pts',(-7.08530627800006,12.2,7.70835144099999));
#245858=CARTESIAN_POINT('Ctrl Pts',(-7.08654202200006,12.2,7.70932493899998));
#245859=CARTESIAN_POINT('Ctrl Pts',(-7.08778491400006,12.2,7.71030217199999));
#245860=CARTESIAN_POINT('Ctrl Pts',(-7.08903494500006,12.2,7.71128311899999));
#245861=CARTESIAN_POINT('Ctrl Pts',(-7.09029211200006,12.2,7.71226775599998));
#245862=CARTESIAN_POINT('Ctrl Pts',(-7.09155640600006,12.2,7.71325606199999));
#245863=CARTESIAN_POINT('Ctrl Pts',(-7.09282782300006,12.2,7.71424801399998));
#245864=CARTESIAN_POINT('Ctrl Pts',(-7.09410635400006,12.2,7.71524359099999));
#245865=CARTESIAN_POINT('Ctrl Pts',(-7.09539199400006,12.2,7.71624276799999));
#245866=CARTESIAN_POINT('Ctrl Pts',(-7.09668473700006,12.2,7.71724552699999));
#245867=CARTESIAN_POINT('Ctrl Pts',(-7.09798457700006,12.2,7.71825184399999));
#245868=CARTESIAN_POINT('Ctrl Pts',(-7.09929150500006,12.2,7.71926169699999));
#245869=CARTESIAN_POINT('Ctrl Pts',(-7.10060551800006,12.2,7.72027506499998));
#245870=CARTESIAN_POINT('Ctrl Pts',(-7.10192660800006,12.2,7.72129192499998));
#245871=CARTESIAN_POINT('Ctrl Pts',(-7.10325476900006,12.2,7.72231225799998));
#245872=CARTESIAN_POINT('Ctrl Pts',(-7.10458999400006,12.2,7.72333603999999));
#245873=CARTESIAN_POINT('Ctrl Pts',(-7.10593227900006,12.2,7.72436325099999));
#245874=CARTESIAN_POINT('Ctrl Pts',(-7.10728161500006,12.2,7.72539386899999));
#245875=CARTESIAN_POINT('Ctrl Pts',(-7.10863799800006,12.2,7.72642787299999));
#245876=CARTESIAN_POINT('Ctrl Pts',(-7.11000142000006,12.2,7.72746524299999));
#245877=CARTESIAN_POINT('Ctrl Pts',(-7.11137187600006,12.2,7.72850595599999));
#245878=CARTESIAN_POINT('Ctrl Pts',(-7.11274935900006,12.2,7.72954999299999));
#245879=CARTESIAN_POINT('Ctrl Pts',(-7.11413386400006,12.2,7.73059733099998));
#245880=CARTESIAN_POINT('Ctrl Pts',(-7.11552538300006,12.2,7.73164795099999));
#245881=CARTESIAN_POINT('Ctrl Pts',(-7.11692391100006,12.2,7.73270183099999));
#245882=CARTESIAN_POINT('Ctrl Pts',(-7.11832944100006,12.2,7.73375895199998));
#245883=CARTESIAN_POINT('Ctrl Pts',(-7.11974196900006,12.2,7.73481929199999));
#245884=CARTESIAN_POINT('Ctrl Pts',(-7.12116148600006,12.2,7.73588283099999));
#245885=CARTESIAN_POINT('Ctrl Pts',(-7.12258798800006,12.2,7.73694954699998));
#245886=CARTESIAN_POINT('Ctrl Pts',(-7.12402146800006,12.2,7.73801942399999));
#245887=CARTESIAN_POINT('Ctrl Pts',(-7.12546192000006,12.2,7.73909243699999));
#245888=CARTESIAN_POINT('Ctrl Pts',(-7.12690933700006,12.2,7.74016856899999));
#245889=CARTESIAN_POINT('Ctrl Pts',(-7.12836371400006,12.2,7.74124779699999));
#245890=CARTESIAN_POINT('Ctrl Pts',(-7.12982504600006,12.2,7.74233010399998));
#245891=CARTESIAN_POINT('Ctrl Pts',(-7.13129332400006,12.2,7.74341546899999));
#245892=CARTESIAN_POINT('Ctrl Pts',(-7.13276854400006,12.2,7.74450386999998));
#245893=CARTESIAN_POINT('Ctrl Pts',(-7.13425070000006,12.2,7.74559529099999));
#245894=CARTESIAN_POINT('Ctrl Pts',(-7.13573978500006,12.2,7.74668970999999));
#245895=CARTESIAN_POINT('Ctrl Pts',(-7.13723579400006,12.2,7.74778710799998));
#245896=CARTESIAN_POINT('Ctrl Pts',(-7.13873872000006,12.2,7.74888746499999));
#245897=CARTESIAN_POINT('Ctrl Pts',(-7.14024855600006,12.2,7.74999076199999));
#245898=CARTESIAN_POINT('Ctrl Pts',(-7.14176530000006,12.2,7.75109697799999));
#245899=CARTESIAN_POINT('Ctrl Pts',(-7.14328894200006,12.2,7.75220609499998));
#245900=CARTESIAN_POINT('Ctrl Pts',(-7.14481947700006,12.2,7.75331809499999));
#245901=CARTESIAN_POINT('Ctrl Pts',(-7.14635690000006,12.2,7.75443295699999));
#245902=CARTESIAN_POINT('Ctrl Pts',(-7.14790120500005,12.2,7.75555066199999));
#245903=CARTESIAN_POINT('Ctrl Pts',(-7.14945238500006,12.2,7.75667119099998));
#245904=CARTESIAN_POINT('Ctrl Pts',(-7.15101043300006,12.2,7.75779452499999));
#245905=CARTESIAN_POINT('Ctrl Pts',(-7.15257534700006,12.2,7.75892064699998));
#245906=CARTESIAN_POINT('Ctrl Pts',(-7.15414711700006,12.2,7.76004953499999));
#245907=CARTESIAN_POINT('Ctrl Pts',(-7.15572573900006,12.2,7.76118117199999));
#245908=CARTESIAN_POINT('Ctrl Pts',(-7.15731120800006,12.2,7.76231553799998));
#245909=CARTESIAN_POINT('Ctrl Pts',(-7.15890351700006,12.2,7.76345261699999));
#245910=CARTESIAN_POINT('Ctrl Pts',(-7.16050265800006,12.2,7.76459238699999));
#245911=CARTESIAN_POINT('Ctrl Pts',(-7.16210862800006,12.2,7.76573483199999));
#245912=CARTESIAN_POINT('Ctrl Pts',(-7.16372142100006,12.2,7.76687993299999));
#245913=CARTESIAN_POINT('Ctrl Pts',(-7.16534103000006,12.2,7.76802766999998));
#245914=CARTESIAN_POINT('Ctrl Pts',(-7.16696745000006,12.2,7.76917802599999));
#245915=CARTESIAN_POINT('Ctrl Pts',(-7.16860067400006,12.2,7.77033098499999));
#245916=CARTESIAN_POINT('Ctrl Pts',(-7.17024069700006,12.2,7.77148652499999));
#245917=CARTESIAN_POINT('Ctrl Pts',(-7.17188751300006,12.2,7.77264462899999));
#245918=CARTESIAN_POINT('Ctrl Pts',(-7.17354111600006,12.2,7.77380527999998));
#245919=CARTESIAN_POINT('Ctrl Pts',(-7.17520150000006,12.2,7.77496845799998));
#245920=CARTESIAN_POINT('Ctrl Pts',(-7.17686866000006,12.2,7.77613414899999));
#245921=CARTESIAN_POINT('Ctrl Pts',(-7.17854259000006,12.2,7.77730232999998));
#245922=CARTESIAN_POINT('Ctrl Pts',(-7.18022328300005,12.2,7.77847298699999));
#245923=CARTESIAN_POINT('Ctrl Pts',(-7.18191073400006,12.2,7.77964609999999));
#245924=CARTESIAN_POINT('Ctrl Pts',(-7.18360493800006,12.2,7.78082165399999));
#245925=CARTESIAN_POINT('Ctrl Pts',(-7.18530588900006,12.2,7.78199962799999));
#245926=CARTESIAN_POINT('Ctrl Pts',(-7.18701358000006,12.2,7.78318000699999));
#245927=CARTESIAN_POINT('Ctrl Pts',(-7.18872800700006,12.2,7.78436277199998));
#245928=CARTESIAN_POINT('Ctrl Pts',(-7.19044916200006,12.2,7.78554790599999));
#245929=CARTESIAN_POINT('Ctrl Pts',(-7.19217704100005,12.2,7.78673539199998));
#245930=CARTESIAN_POINT('Ctrl Pts',(-7.19391163700006,12.2,7.78792521199998));
#245931=CARTESIAN_POINT('Ctrl Pts',(-7.19565294600006,12.2,7.78911734999999));
#245932=CARTESIAN_POINT('Ctrl Pts',(-7.19740096200006,12.2,7.79031178799999));
#245933=CARTESIAN_POINT('Ctrl Pts',(-7.19915567700006,12.2,7.79150850799999));
#245934=CARTESIAN_POINT('Ctrl Pts',(-7.20091708800005,12.2,7.79270749399998));
#245935=CARTESIAN_POINT('Ctrl Pts',(-7.20268518700006,12.2,7.79390872899998));
#245936=CARTESIAN_POINT('Ctrl Pts',(-7.20445997000006,12.2,7.79511219599998));
#245937=CARTESIAN_POINT('Ctrl Pts',(-7.20624143100006,12.2,7.79631787699999));
#245938=CARTESIAN_POINT('Ctrl Pts',(-7.20802956400005,12.2,7.79752575699998));
#245939=CARTESIAN_POINT('Ctrl Pts',(-7.20982436400006,12.2,7.79873581599999));
#245940=CARTESIAN_POINT('Ctrl Pts',(-7.21162582400006,12.2,7.79994804199998));
#245941=CARTESIAN_POINT('Ctrl Pts',(-7.21343393900006,12.2,7.80116241399998));
#245942=CARTESIAN_POINT('Ctrl Pts',(-7.21524870400006,12.2,7.80237891799998));
#245943=CARTESIAN_POINT('Ctrl Pts',(-7.21707011300006,12.2,7.80359753599999));
#245944=CARTESIAN_POINT('Ctrl Pts',(-7.21889815900006,12.2,7.80481825199999));
#245945=CARTESIAN_POINT('Ctrl Pts',(-7.22073283800006,12.2,7.80604104899999));
#245946=CARTESIAN_POINT('Ctrl Pts',(-7.22257414400006,12.2,7.80726591199999));
#245947=CARTESIAN_POINT('Ctrl Pts',(-7.22442207200006,12.2,7.80849282399998));
#245948=CARTESIAN_POINT('Ctrl Pts',(-7.22627661400006,12.2,7.80972176699999));
#245949=CARTESIAN_POINT('Ctrl Pts',(-7.22813776800006,12.2,7.81095272699999));
#245950=CARTESIAN_POINT('Ctrl Pts',(-7.23000552500006,12.2,7.81218568699998));
#245951=CARTESIAN_POINT('Ctrl Pts',(-7.23187988200006,12.2,7.81342063099999));
#245952=CARTESIAN_POINT('Ctrl Pts',(-7.23376083100006,12.2,7.81465754299998));
#245953=CARTESIAN_POINT('Ctrl Pts',(-7.23564836800006,12.2,7.81589640599999));
#245954=CARTESIAN_POINT('Ctrl Pts',(-7.23754248700006,12.2,7.81713720599999));
#245955=CARTESIAN_POINT('Ctrl Pts',(-7.23944318300005,12.2,7.81837992399999));
#245956=CARTESIAN_POINT('Ctrl Pts',(-7.24135045000006,12.2,7.81962454799999));
#245957=CARTESIAN_POINT('Ctrl Pts',(-7.24326428200006,12.2,7.82087105799998));
#245958=CARTESIAN_POINT('Ctrl Pts',(-7.24518467300006,12.2,7.82211944199998));
#245959=CARTESIAN_POINT('Ctrl Pts',(-7.24711162000006,12.2,7.82336968199999));
#245960=CARTESIAN_POINT('Ctrl Pts',(-7.24904511400006,12.2,7.82462176199999));
#245961=CARTESIAN_POINT('Ctrl Pts',(-7.25098515300005,12.2,7.82587566899998));
#245962=CARTESIAN_POINT('Ctrl Pts',(-7.25293172800006,12.2,7.82713138499999));
#245963=CARTESIAN_POINT('Ctrl Pts',(-7.25488483700006,12.2,7.82838889399999));
#245964=CARTESIAN_POINT('Ctrl Pts',(-7.25684447100006,12.2,7.82964818299998));
#245965=CARTESIAN_POINT('Ctrl Pts',(-7.25881062600005,12.2,7.83090923599998));
#245966=CARTESIAN_POINT('Ctrl Pts',(-7.26078329800006,12.2,7.83217203499999));
#245967=CARTESIAN_POINT('Ctrl Pts',(-7.26276247900006,12.2,7.83343656799998));
#245968=CARTESIAN_POINT('Ctrl Pts',(-7.26474816500006,12.2,7.83470281899999));
#245969=CARTESIAN_POINT('Ctrl Pts',(-7.26674035000006,12.2,7.83597076999998));
#245970=CARTESIAN_POINT('Ctrl Pts',(-7.26873902900006,12.2,7.83724040899998));
#245971=CARTESIAN_POINT('Ctrl Pts',(-7.27074419600005,12.2,7.83851171899999));
#245972=CARTESIAN_POINT('Ctrl Pts',(-7.27275584500005,12.2,7.83978468699999));
#245973=CARTESIAN_POINT('Ctrl Pts',(-7.27477397200006,12.2,7.84105929599999));
#245974=CARTESIAN_POINT('Ctrl Pts',(-7.27679857000005,12.2,7.84233553099998));
#245975=CARTESIAN_POINT('Ctrl Pts',(-7.27882963600006,12.2,7.84361337899998));
#245976=CARTESIAN_POINT('Ctrl Pts',(-7.28086716200006,12.2,7.84489282299998));
#245977=CARTESIAN_POINT('Ctrl Pts',(-7.28291114200006,12.2,7.84617384799999));
#245978=CARTESIAN_POINT('Ctrl Pts',(-7.28496157300006,12.2,7.84745644199998));
#245979=CARTESIAN_POINT('Ctrl Pts',(-7.28701844900006,12.2,7.84874058699998));
#245980=CARTESIAN_POINT('Ctrl Pts',(-7.28908176300005,12.2,7.85002626999999));
#245981=CARTESIAN_POINT('Ctrl Pts',(-7.29115151200006,12.2,7.85131347699998));
#245982=CARTESIAN_POINT('Ctrl Pts',(-7.29322768800006,12.2,7.85260219099998));
#245983=CARTESIAN_POINT('Ctrl Pts',(-7.29531028700006,12.2,7.85389239899998));
#245984=CARTESIAN_POINT('Ctrl Pts',(-7.29739930400005,12.2,7.85518408599999));
#245985=CARTESIAN_POINT('Ctrl Pts',(-7.29949473300006,12.2,7.85647723899999));
#245986=CARTESIAN_POINT('Ctrl Pts',(-7.30159656800006,12.2,7.85777184099998));
#245987=CARTESIAN_POINT('Ctrl Pts',(-7.30370480500006,12.2,7.85906787899999));
#245988=CARTESIAN_POINT('Ctrl Pts',(-7.30581943700006,12.2,7.86036533899999));
#245989=CARTESIAN_POINT('Ctrl Pts',(-7.30794046000006,12.2,7.86166420599999));
#245990=CARTESIAN_POINT('Ctrl Pts',(-7.31006786800006,12.2,7.86296446599999));
#245991=CARTESIAN_POINT('Ctrl Pts',(-7.31220165500006,12.2,7.86426610399998));
#245992=CARTESIAN_POINT('Ctrl Pts',(-7.31434181800006,12.2,7.86556910899999));
#245993=CARTESIAN_POINT('Ctrl Pts',(-7.31648834800006,12.2,7.86687346199999));
#245994=CARTESIAN_POINT('Ctrl Pts',(-7.31864124200006,12.2,7.86817915199999));
#245995=CARTESIAN_POINT('Ctrl Pts',(-7.32080049400006,12.2,7.86948616399999));
#245996=CARTESIAN_POINT('Ctrl Pts',(-7.32296610000006,12.2,7.87079448499998));
#245997=CARTESIAN_POINT('Ctrl Pts',(-7.32513805400006,12.2,7.87210409899998));
#245998=CARTESIAN_POINT('Ctrl Pts',(-7.32731634900006,12.2,7.87341499399999));
#245999=CARTESIAN_POINT('Ctrl Pts',(-7.32950098000006,12.2,7.87472715499998));
#246000=CARTESIAN_POINT('Ctrl Pts',(-7.33169194400006,12.2,7.87604056899998));
#246001=CARTESIAN_POINT('Ctrl Pts',(-7.33388923300006,12.2,7.87735522199998));
#246002=CARTESIAN_POINT('Ctrl Pts',(-7.33609284400006,12.2,7.87867109999999));
#246003=CARTESIAN_POINT('Ctrl Pts',(-7.33830277000005,12.2,7.87998818899998));
#246004=CARTESIAN_POINT('Ctrl Pts',(-7.34051900600006,12.2,7.88130647499998));
#246005=CARTESIAN_POINT('Ctrl Pts',(-7.34274154700006,12.2,7.88262594599999));
#246006=CARTESIAN_POINT('Ctrl Pts',(-7.34497038800006,12.2,7.88394658699998));
#246007=CARTESIAN_POINT('Ctrl Pts',(-7.34720552300006,12.2,7.88526838399999));
#246008=CARTESIAN_POINT('Ctrl Pts',(-7.34944694700006,12.2,7.88659132499999));
#246009=CARTESIAN_POINT('Ctrl Pts',(-7.35169465500006,12.2,7.88791539599998));
#246010=CARTESIAN_POINT('Ctrl Pts',(-7.35394864100006,12.2,7.88924058299998));
#246011=CARTESIAN_POINT('Ctrl Pts',(-7.35620890000006,12.2,7.89056687299999));
#246012=CARTESIAN_POINT('Ctrl Pts',(-7.35847542700006,12.2,7.89189425299998));
#246013=CARTESIAN_POINT('Ctrl Pts',(-7.36074821700006,12.2,7.89322270699999));
#246014=CARTESIAN_POINT('Ctrl Pts',(-7.36302726400006,12.2,7.89455222599998));
#246015=CARTESIAN_POINT('Ctrl Pts',(-7.36531256300006,12.2,7.89588279499998));
#246016=CARTESIAN_POINT('Ctrl Pts',(-7.36760410800006,12.2,7.89721439899999));
#246017=CARTESIAN_POINT('Ctrl Pts',(-7.36990189600006,12.2,7.89854702799998));
#246018=CARTESIAN_POINT('Ctrl Pts',(-7.37220591900006,12.2,7.89988066499999));
#246019=CARTESIAN_POINT('Ctrl Pts',(-7.37451617400006,12.2,7.90121529999999));
#246020=CARTESIAN_POINT('Ctrl Pts',(-7.37683265400006,12.2,7.90255091899999));
#246021=CARTESIAN_POINT('Ctrl Pts',(-7.37915535500006,12.2,7.90388750999998));
#246022=CARTESIAN_POINT('Ctrl Pts',(-7.38148427100006,12.2,7.90522505699998));
#246023=CARTESIAN_POINT('Ctrl Pts',(-7.38381939700006,12.2,7.90656354999999));
#246024=CARTESIAN_POINT('Ctrl Pts',(-7.38616072800006,12.2,7.90790297499999));
#246025=CARTESIAN_POINT('Ctrl Pts',(-7.38850825800006,12.2,7.90924331999998));
#246026=CARTESIAN_POINT('Ctrl Pts',(-7.39086198300006,12.2,7.91058456999998));
#246027=CARTESIAN_POINT('Ctrl Pts',(-7.39322189600006,12.2,7.91192671399998));
#246028=CARTESIAN_POINT('Ctrl Pts',(-7.39558799400006,12.2,7.91326973999999));
#246029=CARTESIAN_POINT('Ctrl Pts',(-7.39796027100006,12.2,7.91461363299998));
#246030=CARTESIAN_POINT('Ctrl Pts',(-7.40033872100006,12.2,7.91595838099998));
#246031=CARTESIAN_POINT('Ctrl Pts',(-7.40272333900006,12.2,7.91730397299999));
#246032=CARTESIAN_POINT('Ctrl Pts',(-7.40511412000005,12.2,7.91865039499999));
#246033=CARTESIAN_POINT('Ctrl Pts',(-7.40751105900006,12.2,7.91999763299999));
#246034=CARTESIAN_POINT('Ctrl Pts',(-7.40991415200006,12.2,7.92134567699998));
#246035=CARTESIAN_POINT('Ctrl Pts',(-7.41232339100006,12.2,7.92269451299998));
#246036=CARTESIAN_POINT('Ctrl Pts',(-7.41473877300006,12.2,7.92404412999999));
#246037=CARTESIAN_POINT('Ctrl Pts',(-7.41716029100006,12.2,7.92539451399998));
#246038=CARTESIAN_POINT('Ctrl Pts',(-7.41958794200006,12.2,7.92674565199999));
#246039=CARTESIAN_POINT('Ctrl Pts',(-7.42202171900006,12.2,7.92809753399998));
#246040=CARTESIAN_POINT('Ctrl Pts',(-7.42446161900006,12.2,7.92945014599999));
#246041=CARTESIAN_POINT('Ctrl Pts',(-7.42690763400006,12.2,7.93080347599999));
#246042=CARTESIAN_POINT('Ctrl Pts',(-7.42935976100005,12.2,7.93215751199998));
#246043=CARTESIAN_POINT('Ctrl Pts',(-7.43181799400006,12.2,7.93351224099998));
#246044=CARTESIAN_POINT('Ctrl Pts',(-7.43428232700006,12.2,7.93486765199999));
#246045=CARTESIAN_POINT('Ctrl Pts',(-7.43675275700006,12.2,7.93622373199998));
#246046=CARTESIAN_POINT('Ctrl Pts',(-7.43922927800006,12.2,7.93758046899999));
#246047=CARTESIAN_POINT('Ctrl Pts',(-7.44171188300006,12.2,7.93893784999998));
#246048=CARTESIAN_POINT('Ctrl Pts',(-7.44420057000006,12.2,7.94029586499998));
#246049=CARTESIAN_POINT('Ctrl Pts',(-7.44669533100006,12.2,7.94165450099998));
#246050=CARTESIAN_POINT('Ctrl Pts',(-7.44919616200006,12.2,7.94301374399998));
#246051=CARTESIAN_POINT('Ctrl Pts',(-7.45170305800006,12.2,7.94437358599998));
#246052=CARTESIAN_POINT('Ctrl Pts',(-7.45421601400006,12.2,7.94573401099999));
#246053=CARTESIAN_POINT('Ctrl Pts',(-7.45673502500006,12.2,7.94709500999998));
#246054=CARTESIAN_POINT('Ctrl Pts',(-7.45926008500006,12.2,7.94845657099999));
#246055=CARTESIAN_POINT('Ctrl Pts',(-7.46179119000006,12.2,7.94981867899998));
#246056=CARTESIAN_POINT('Ctrl Pts',(-7.46432833400006,12.2,7.95118132499999));
#246057=CARTESIAN_POINT('Ctrl Pts',(-7.46687151300006,12.2,7.95254449699998));
#246058=CARTESIAN_POINT('Ctrl Pts',(-7.46942072000006,12.2,7.95390818299998));
#246059=CARTESIAN_POINT('Ctrl Pts',(-7.47197595100006,12.2,7.95527237099999));
#246060=CARTESIAN_POINT('Ctrl Pts',(-7.47453720200006,12.2,7.95663704999999));
#246061=CARTESIAN_POINT('Ctrl Pts',(-7.47710446500006,12.2,7.95800220799999));
#246062=CARTESIAN_POINT('Ctrl Pts',(-7.47967773800006,12.2,7.95936783099998));
#246063=CARTESIAN_POINT('Ctrl Pts',(-7.48225701500006,12.2,7.96073391199998));
#246064=CARTESIAN_POINT('Ctrl Pts',(-7.48484228800006,12.2,7.96210043599999));
#246065=CARTESIAN_POINT('Ctrl Pts',(-7.48743355700006,12.2,7.96346739199999));
#246066=CARTESIAN_POINT('Ctrl Pts',(-7.49003081300006,12.2,7.96483476999998));
#246067=CARTESIAN_POINT('Ctrl Pts',(-7.49263405300006,12.2,7.96620255599999));
#246068=CARTESIAN_POINT('Ctrl Pts',(-7.49524327100006,12.2,7.96757074199999));
#246069=CARTESIAN_POINT('Ctrl Pts',(-7.49785846200006,12.2,7.96893931299999));
#246070=CARTESIAN_POINT('Ctrl Pts',(-7.50047962100006,12.2,7.97030825999999));
#246071=CARTESIAN_POINT('Ctrl Pts',(-7.50310674300006,12.2,7.97167757099999));
#246072=CARTESIAN_POINT('Ctrl Pts',(-7.50573982300006,12.2,7.97304723499998));
#246073=CARTESIAN_POINT('Ctrl Pts',(-7.50837885500006,12.2,7.97441723899999));
#246074=CARTESIAN_POINT('Ctrl Pts',(-7.51102383600006,12.2,7.97578757299998));
#246075=CARTESIAN_POINT('Ctrl Pts',(-7.51367475900006,12.2,7.97715822699999));
#246076=CARTESIAN_POINT('Ctrl Pts',(-7.51633162000005,12.2,7.97852918799999));
#246077=CARTESIAN_POINT('Ctrl Pts',(-7.51899441200005,12.2,7.97990044499999));
#246078=CARTESIAN_POINT('Ctrl Pts',(-7.52166313300006,12.2,7.98127198799998));
#246079=CARTESIAN_POINT('Ctrl Pts',(-7.52433777600006,12.2,7.98264380499998));
#246080=CARTESIAN_POINT('Ctrl Pts',(-7.52701833700005,12.2,7.98401588399998));
#246081=CARTESIAN_POINT('Ctrl Pts',(-7.52970481000006,12.2,7.98538821699999));
#246082=CARTESIAN_POINT('Ctrl Pts',(-7.53239719100005,12.2,7.98676078899998));
#246083=CARTESIAN_POINT('Ctrl Pts',(-7.53509547300006,12.2,7.98813359199999));
#246084=CARTESIAN_POINT('Ctrl Pts',(-7.53779965400006,12.2,7.98950661499998));
#246085=CARTESIAN_POINT('Ctrl Pts',(-7.54050972500006,12.2,7.99087984499998));
#246086=CARTESIAN_POINT('Ctrl Pts',(-7.54322568500006,12.2,7.99225327099998));
#246087=CARTESIAN_POINT('Ctrl Pts',(-7.54594752700006,12.2,7.99362688499999));
#246088=CARTESIAN_POINT('Ctrl Pts',(-7.54867524600006,12.2,7.99500067299999));
#246089=CARTESIAN_POINT('Ctrl Pts',(-7.55140883700006,12.2,7.99637462699998));
#246090=CARTESIAN_POINT('Ctrl Pts',(-7.55414829500006,12.2,7.99774873399999));
#246091=CARTESIAN_POINT('Ctrl Pts',(-7.55689361600006,12.2,7.99912298399998));
#246092=CARTESIAN_POINT('Ctrl Pts',(-7.55964479300006,12.2,8.00049736599998));
#246093=CARTESIAN_POINT('Ctrl Pts',(-7.56240182300005,12.2,8.00187187099999));
#246094=CARTESIAN_POINT('Ctrl Pts',(-7.56516470000006,12.2,8.00324648399998));
#246095=CARTESIAN_POINT('Ctrl Pts',(-7.56793341800006,12.2,8.00462119899999));
#246096=CARTESIAN_POINT('Ctrl Pts',(-7.57070797500005,12.2,8.00599600399998));
#246097=CARTESIAN_POINT('Ctrl Pts',(-7.57348836300006,12.2,8.00737088699999));
#246098=CARTESIAN_POINT('Ctrl Pts',(-7.57627457800006,12.2,8.00874583799999));
#246099=CARTESIAN_POINT('Ctrl Pts',(-7.57906661600006,12.2,8.01012084699998));
#246100=CARTESIAN_POINT('Ctrl Pts',(-7.58186447000006,12.2,8.01149590299998));
#246101=CARTESIAN_POINT('Ctrl Pts',(-7.58466813600006,12.2,8.01287099699999));
#246102=CARTESIAN_POINT('Ctrl Pts',(-7.58747761100006,12.2,8.01424611599998));
#246103=CARTESIAN_POINT('Ctrl Pts',(-7.59029288700006,12.2,8.01562125099998));
#246104=CARTESIAN_POINT('Ctrl Pts',(-7.59311396000006,12.2,8.01699639099999));
#246105=CARTESIAN_POINT('Ctrl Pts',(-7.59594082600006,12.2,8.01837152699999));
#246106=CARTESIAN_POINT('Ctrl Pts',(-7.59877347800006,12.2,8.01974664699999));
#246107=CARTESIAN_POINT('Ctrl Pts',(-7.60161191400006,12.2,8.02112174099998));
#246108=CARTESIAN_POINT('Ctrl Pts',(-7.60445612600006,12.2,8.02249679899998));
#246109=CARTESIAN_POINT('Ctrl Pts',(-7.60730611100006,12.2,8.02387180999999));
#246110=CARTESIAN_POINT('Ctrl Pts',(-7.61016186300005,12.2,8.02524676499999));
#246111=CARTESIAN_POINT('Ctrl Pts',(-7.61302337700006,12.2,8.02662165399998));
#246112=CARTESIAN_POINT('Ctrl Pts',(-7.61589065000006,12.2,8.02799646399999));
#246113=CARTESIAN_POINT('Ctrl Pts',(-7.61876367500006,12.2,8.02937118799999));
#246114=CARTESIAN_POINT('Ctrl Pts',(-7.62164244700006,12.2,8.03074581399999));
#246115=CARTESIAN_POINT('Ctrl Pts',(-7.62452696100006,12.2,8.03212033199999));
#246116=CARTESIAN_POINT('Ctrl Pts',(-7.62741721300006,12.2,8.03349473299999));
#246117=CARTESIAN_POINT('Ctrl Pts',(-7.63031319900006,12.2,8.03486900599999));
#246118=CARTESIAN_POINT('Ctrl Pts',(-7.63321491200006,12.2,8.03624313999999));
#246119=CARTESIAN_POINT('Ctrl Pts',(-7.63612234700006,12.2,8.03761712699998));
#246120=CARTESIAN_POINT('Ctrl Pts',(-7.63903550100006,12.2,8.03899095599999));
#246121=CARTESIAN_POINT('Ctrl Pts',(-7.64195436800006,12.2,8.04036461599999));
#246122=CARTESIAN_POINT('Ctrl Pts',(-7.64487894200006,12.2,8.04173809899999));
#246123=CARTESIAN_POINT('Ctrl Pts',(-7.64780922000006,12.2,8.04311139499998));
#246124=CARTESIAN_POINT('Ctrl Pts',(-7.65074519600006,12.2,8.04448449199998));
#246125=CARTESIAN_POINT('Ctrl Pts',(-7.65368686500006,12.2,8.04585738099998));
#246126=CARTESIAN_POINT('Ctrl Pts',(-7.65663422300006,12.2,8.04723005299999));
#246127=CARTESIAN_POINT('Ctrl Pts',(-7.65958726300005,12.2,8.04860249699999));
#246128=CARTESIAN_POINT('Ctrl Pts',(-7.66254598200005,12.2,8.04997470299998));
#246129=CARTESIAN_POINT('Ctrl Pts',(-7.66551037500006,12.2,8.05134666399999));
#246130=CARTESIAN_POINT('Ctrl Pts',(-7.66848043700006,12.2,8.05271836699998));
#246131=CARTESIAN_POINT('Ctrl Pts',(-7.67145616200006,12.2,8.05408980299998));
#246132=CARTESIAN_POINT('Ctrl Pts',(-7.67443754600006,12.2,8.05546096299998));
#246133=CARTESIAN_POINT('Ctrl Pts',(-7.67742458300006,12.2,8.05683183699998));
#246134=CARTESIAN_POINT('Ctrl Pts',(-7.68041727000006,12.2,8.05820241499998));
#246135=CARTESIAN_POINT('Ctrl Pts',(-7.68341560100006,12.2,8.05957268799999));
#246136=CARTESIAN_POINT('Ctrl Pts',(-7.68641957100006,12.2,8.06094264599999));
#246137=CARTESIAN_POINT('Ctrl Pts',(-7.68942917500006,12.2,8.06231227899998));
#246138=CARTESIAN_POINT('Ctrl Pts',(-7.69244440900006,12.2,8.06368157799999));
#246139=CARTESIAN_POINT('Ctrl Pts',(-7.69546526600006,12.2,8.06505053299999));
#246140=CARTESIAN_POINT('Ctrl Pts',(-7.69849174400005,12.2,8.06641913399999));
#246141=CARTESIAN_POINT('Ctrl Pts',(-7.70152383600006,12.2,8.06778737399998));
#246142=CARTESIAN_POINT('Ctrl Pts',(-7.70456153900006,12.2,8.06915523999999));
#246143=CARTESIAN_POINT('Ctrl Pts',(-7.70760484600006,12.2,8.07052272399999));
#246144=CARTESIAN_POINT('Ctrl Pts',(-7.71065375300005,12.2,8.07188981699999));
#246145=CARTESIAN_POINT('Ctrl Pts',(-7.71370825500006,12.2,8.07325650899998));
#246146=CARTESIAN_POINT('Ctrl Pts',(-7.71676834800005,12.2,8.07462279199999));
#246147=CARTESIAN_POINT('Ctrl Pts',(-7.71983402500006,12.2,8.07598865399999));
#246148=CARTESIAN_POINT('Ctrl Pts',(-7.72290528400006,12.2,8.07735408899998));
#246149=CARTESIAN_POINT('Ctrl Pts',(-7.72598211700006,12.2,8.07871908399999));
#246150=CARTESIAN_POINT('Ctrl Pts',(-7.72906452200005,12.2,8.08008363199999));
#246151=CARTESIAN_POINT('Ctrl Pts',(-7.73215249300006,12.2,8.08144772299999));
#246152=CARTESIAN_POINT('Ctrl Pts',(-7.73524602400006,12.2,8.08281134799999));
#246153=CARTESIAN_POINT('Ctrl Pts',(-7.73834511100005,12.2,8.08417449699999));
#246154=CARTESIAN_POINT('Ctrl Pts',(-7.74144975100005,12.2,8.08553716199999));
#246155=CARTESIAN_POINT('Ctrl Pts',(-7.74455993600006,12.2,8.08689933299998));
#246156=CARTESIAN_POINT('Ctrl Pts',(-7.74767566300006,12.2,8.08826100099999));
#246157=CARTESIAN_POINT('Ctrl Pts',(-7.75079692700006,12.2,8.08962215699999));
#246158=CARTESIAN_POINT('Ctrl Pts',(-7.75392372200006,12.2,8.09098279099998));
#246159=CARTESIAN_POINT('Ctrl Pts',(-7.75705604400006,12.2,8.09234289499998));
#246160=CARTESIAN_POINT('Ctrl Pts',(-7.76019388900006,12.2,8.09370245899999));
#246161=CARTESIAN_POINT('Ctrl Pts',(-7.76333725000006,12.2,8.09506147499999));
#246162=CARTESIAN_POINT('Ctrl Pts',(-7.76648612500006,12.2,8.09641993199998));
#246163=CARTESIAN_POINT('Ctrl Pts',(-7.76964050600006,12.2,8.09777782399999));
#246164=CARTESIAN_POINT('Ctrl Pts',(-7.77280039100006,12.2,8.09913513899998));
#246165=CARTESIAN_POINT('Ctrl Pts',(-7.77596577300006,12.2,8.10049186899998));
#246166=CARTESIAN_POINT('Ctrl Pts',(-7.77913664800005,12.2,8.10184800599998));
#246167=CARTESIAN_POINT('Ctrl Pts',(-7.78231301200006,12.2,8.10320353899998));
#246168=CARTESIAN_POINT('Ctrl Pts',(-7.78549485900006,12.2,8.10455846299998));
#246169=CARTESIAN_POINT('Ctrl Pts',(-7.78868218500006,12.2,8.10591276399999));
#246170=CARTESIAN_POINT('Ctrl Pts',(-7.79187498300006,12.2,8.10726643599999));
#246171=CARTESIAN_POINT('Ctrl Pts',(-7.79507325100005,12.2,8.10861946999999));
#246172=CARTESIAN_POINT('Ctrl Pts',(-7.79827698300006,12.2,8.10997185699998));
#246173=CARTESIAN_POINT('Ctrl Pts',(-7.80148617400006,12.2,8.11132358799998));
#246174=CARTESIAN_POINT('Ctrl Pts',(-7.80470082000006,12.2,8.11267465299998));
#246175=CARTESIAN_POINT('Ctrl Pts',(-7.80792091500006,12.2,8.11402504599998));
#246176=CARTESIAN_POINT('Ctrl Pts',(-7.81114645400006,12.2,8.11537475499998));
#246177=CARTESIAN_POINT('Ctrl Pts',(-7.81437743500006,12.2,8.11672377399999));
#246178=CARTESIAN_POINT('Ctrl Pts',(-7.81761384900006,12.2,8.11807209299998));
#246179=CARTESIAN_POINT('Ctrl Pts',(-7.82085569500006,12.2,8.11941970299999));
#246180=CARTESIAN_POINT('Ctrl Pts',(-7.82410296500006,12.2,8.12076659599999));
#246181=CARTESIAN_POINT('Ctrl Pts',(-7.82735565600006,12.2,8.12211276299998));
#246182=CARTESIAN_POINT('Ctrl Pts',(-7.83061376200005,12.2,8.12345819399999));
#246183=CARTESIAN_POINT('Ctrl Pts',(-7.83387728100006,12.2,8.12480288399998));
#246184=CARTESIAN_POINT('Ctrl Pts',(-7.83714620400006,12.2,8.12614681999998));
#246185=CARTESIAN_POINT('Ctrl Pts',(-7.84042053000006,12.2,8.12748999699998));
#246186=CARTESIAN_POINT('Ctrl Pts',(-7.84370025300006,12.2,8.12883240399999));
#246187=CARTESIAN_POINT('Ctrl Pts',(-7.84698536600006,12.2,8.13017403499998));
#246188=CARTESIAN_POINT('Ctrl Pts',(-7.85027586700006,12.2,8.13151487799999));
#246189=CARTESIAN_POINT('Ctrl Pts',(-7.85357175000006,12.2,8.13285492699999));
#246190=CARTESIAN_POINT('Ctrl Pts',(-7.85687301000006,12.2,8.13419417299999));
#246191=CARTESIAN_POINT('Ctrl Pts',(-7.86017964300005,12.2,8.13553260699998));
#246192=CARTESIAN_POINT('Ctrl Pts',(-7.86349164400006,12.2,8.13687022099998));
#246193=CARTESIAN_POINT('Ctrl Pts',(-7.86680900800006,12.2,8.13820700699999));
#246194=CARTESIAN_POINT('Ctrl Pts',(-7.87013173000006,12.2,8.13954295599999));
#246195=CARTESIAN_POINT('Ctrl Pts',(-7.87345980500006,12.2,8.14087805999998));
#246196=CARTESIAN_POINT('Ctrl Pts',(-7.87679322900006,12.2,8.14221230999999));
#246197=CARTESIAN_POINT('Ctrl Pts',(-7.88013199700006,12.2,8.14354569699999));
#246198=CARTESIAN_POINT('Ctrl Pts',(-7.88347610400006,12.2,8.14487821399998));
#246199=CARTESIAN_POINT('Ctrl Pts',(-7.88682554500006,12.2,8.14620985299998));
#246200=CARTESIAN_POINT('Ctrl Pts',(-7.89018031600006,12.2,8.14754060399999));
#246201=CARTESIAN_POINT('Ctrl Pts',(-7.89354041200006,12.2,8.14887045999999));
#246202=CARTESIAN_POINT('Ctrl Pts',(-7.89690582700005,12.2,8.15019941199999));
#246203=CARTESIAN_POINT('Ctrl Pts',(-7.90027655700006,12.2,8.15152745299999));
#246204=CARTESIAN_POINT('Ctrl Pts',(-7.90365259800006,12.2,8.15285457299998));
#246205=CARTESIAN_POINT('Ctrl Pts',(-7.90703394500006,12.2,8.15418076499999));
#246206=CARTESIAN_POINT('Ctrl Pts',(-7.91042059300005,12.2,8.15550602099999));
#246207=CARTESIAN_POINT('Ctrl Pts',(-7.91381253600005,12.2,8.15683033199999));
#246208=CARTESIAN_POINT('Ctrl Pts',(-7.91720977000006,12.2,8.15815368899998));
#246209=CARTESIAN_POINT('Ctrl Pts',(-7.92061229100005,12.2,8.15947608599998));
#246210=CARTESIAN_POINT('Ctrl Pts',(-7.92402009400006,12.2,8.16079751399998));
#246211=CARTESIAN_POINT('Ctrl Pts',(-7.92743317500006,12.2,8.16211796399998));
#246212=CARTESIAN_POINT('Ctrl Pts',(-7.93085152700005,12.2,8.16343742899999));
#246213=CARTESIAN_POINT('Ctrl Pts',(-7.93427514700006,12.2,8.16475590099999));
#246214=CARTESIAN_POINT('Ctrl Pts',(-7.93770402900006,12.2,8.16607337199999));
#246215=CARTESIAN_POINT('Ctrl Pts',(-7.94113817000006,12.2,8.16738983299999));
#246216=CARTESIAN_POINT('Ctrl Pts',(-7.94457756400006,12.2,8.16870527599999));
#246217=CARTESIAN_POINT('Ctrl Pts',(-7.94802220600006,12.2,8.17001969299999));
#246218=CARTESIAN_POINT('Ctrl Pts',(-7.95147209200006,12.2,8.17133307699999));
#246219=CARTESIAN_POINT('Ctrl Pts',(-7.95492721600005,12.2,8.17264541999998));
#246220=CARTESIAN_POINT('Ctrl Pts',(-7.95838757500006,12.2,8.17395671299998));
#246221=CARTESIAN_POINT('Ctrl Pts',(-7.96185316300006,12.2,8.17526694799999));
#246222=CARTESIAN_POINT('Ctrl Pts',(-7.96532397700006,12.2,8.17657611899998));
#246223=CARTESIAN_POINT('Ctrl Pts',(-7.96880001000006,12.2,8.17788421699999));
#246224=CARTESIAN_POINT('Ctrl Pts',(-7.97228126000006,12.2,8.17919123499999));
#246225=CARTESIAN_POINT('Ctrl Pts',(-7.97576771900006,12.2,8.18049716399998));
#246226=CARTESIAN_POINT('Ctrl Pts',(-7.97925938500006,12.2,8.18180199599999));
#246227=CARTESIAN_POINT('Ctrl Pts',(-7.98275625000005,12.2,8.18310572199999));
#246228=CARTESIAN_POINT('Ctrl Pts',(-7.98625831300006,12.2,8.18440833599999));
#246229=CARTESIAN_POINT('Ctrl Pts',(-7.98976556600006,12.2,8.18570982799999));
#246230=CARTESIAN_POINT('Ctrl Pts',(-7.99327800400006,12.2,8.18701019299999));
#246231=CARTESIAN_POINT('Ctrl Pts',(-7.99679562600006,12.2,8.18830942099999));
#246232=CARTESIAN_POINT('Ctrl Pts',(-8.00031842500006,12.2,8.18960750499999));
#246233=CARTESIAN_POINT('Ctrl Pts',(-8.00384639600006,12.2,8.19090443999999));
#246234=CARTESIAN_POINT('Ctrl Pts',(-8.00737953700006,12.2,8.19220021799998));
#246235=CARTESIAN_POINT('Ctrl Pts',(-8.01091784300005,12.2,8.19349483199998));
#246236=CARTESIAN_POINT('Ctrl Pts',(-8.01446130800005,12.2,8.19478827199998));
#246237=CARTESIAN_POINT('Ctrl Pts',(-8.01800992700005,12.2,8.19608053199998));
#246238=CARTESIAN_POINT('Ctrl Pts',(-8.02156369500005,12.2,8.19737160199999));
#246239=CARTESIAN_POINT('Ctrl Pts',(-8.02512260400006,12.2,8.19866146999999));
#246240=CARTESIAN_POINT('Ctrl Pts',(-8.02868665100006,12.2,8.19995012899999));
#246241=CARTESIAN_POINT('Ctrl Pts',(-8.03225583000006,12.2,8.20123757099999));
#246242=CARTESIAN_POINT('Ctrl Pts',(-8.03583013500005,12.2,8.20252378799999));
#246243=CARTESIAN_POINT('Ctrl Pts',(-8.03940956400006,12.2,8.20380877499998));
#246244=CARTESIAN_POINT('Ctrl Pts',(-8.04299411600006,12.2,8.20509252899999));
#246245=CARTESIAN_POINT('Ctrl Pts',(-8.04658378800006,12.2,8.20637504799999));
#246246=CARTESIAN_POINT('Ctrl Pts',(-8.04945962200006,12.2,8.20740007499998));
#246247=CARTESIAN_POINT('Ctrl Pts',(-8.05161880100006,12.2,8.20816828899999));
#246248=CARTESIAN_POINT('Ctrl Pts',(-8.05305927800006,12.2,8.20868018399998));
#246249=CARTESIAN_POINT('Ctrl Pts',(-8.05377977200006,12.2,8.20893606999999));
#246250=CARTESIAN_POINT('Origin',(-5.66257110645729E-14,15.2,-1.77635683940025E-14));
#246251=CARTESIAN_POINT('',(-8.02901631900006,15.2,6.57080831899999));
#246252=CARTESIAN_POINT('',(-8.02901631900006,12.2,6.57080831899999));
#246253=CARTESIAN_POINT('',(-8.02901631900006,15.2,6.57080831899999));
#246254=CARTESIAN_POINT('Origin',(-5.66257110645729E-14,12.2,-1.77635683940025E-14));
#246255=CARTESIAN_POINT('Origin',(-5.66257110645729E-14,15.2,-1.77635683940025E-14));
#246256=CARTESIAN_POINT('Origin',(-5.66257110645729E-14,15.2,-1.77635683940025E-14));
#246257=CARTESIAN_POINT('',(-9.14005731500006,15.2,6.97920857099999));
#246258=CARTESIAN_POINT('',(-9.36775917500006,15.2,6.67046385499999));
#246259=CARTESIAN_POINT('Origin',(-5.66257110645729E-14,15.2,-1.77635683940025E-14));
#246260=CARTESIAN_POINT('',(-9.36775917500006,12.2,6.67046385499999));
#246261=CARTESIAN_POINT('',(-9.36775917500006,15.2,6.67046385499999));
#246262=CARTESIAN_POINT('',(-9.14005731500006,12.2,6.97920857099999));
#246263=CARTESIAN_POINT('Origin',(-5.66257110645729E-14,12.2,-1.77635683940025E-14));
#246264=CARTESIAN_POINT('',(-9.14005731500006,15.2,6.97920857099999));
#246265=CARTESIAN_POINT('Ctrl Pts',(-8.02901631900006,15.2,6.57080831899999));
#246266=CARTESIAN_POINT('Ctrl Pts',(-8.02901631900006,11.6,6.57080831899999));
#246267=CARTESIAN_POINT('Ctrl Pts',(-8.02916024200006,15.2,6.57090674099998));
#246268=CARTESIAN_POINT('Ctrl Pts',(-8.02916024200006,11.6,6.57090674099998));
#246269=CARTESIAN_POINT('Ctrl Pts',(-8.02945316300006,15.2,6.57110695199999));
#246270=CARTESIAN_POINT('Ctrl Pts',(-8.02945316300006,11.6,6.57110695199999));
#246271=CARTESIAN_POINT('Ctrl Pts',(-8.02989715800006,15.2,6.57141009799999));
#246272=CARTESIAN_POINT('Ctrl Pts',(-8.02989715800006,11.6,6.57141009799999));
#246273=CARTESIAN_POINT('Ctrl Pts',(-8.03049556400006,15.2,6.57181801999998));
#246274=CARTESIAN_POINT('Ctrl Pts',(-8.03049556400006,11.6,6.57181801999998));
#246275=CARTESIAN_POINT('Ctrl Pts',(-8.03125297400006,15.2,6.57233322399998));
#246276=CARTESIAN_POINT('Ctrl Pts',(-8.03125297400006,11.6,6.57233322399998));
#246277=CARTESIAN_POINT('Ctrl Pts',(-8.03202318500006,15.2,6.57285600599998));
#246278=CARTESIAN_POINT('Ctrl Pts',(-8.03202318500006,11.6,6.57285600599998));
#246279=CARTESIAN_POINT('Ctrl Pts',(-8.03280179800005,15.2,6.57338334999999));
#246280=CARTESIAN_POINT('Ctrl Pts',(-8.03280179800005,11.6,6.57338334999999));
#246281=CARTESIAN_POINT('Ctrl Pts',(-8.03358880000006,15.2,6.57391522699999));
#246282=CARTESIAN_POINT('Ctrl Pts',(-8.03358880000006,11.6,6.57391522699999));
#246283=CARTESIAN_POINT('Ctrl Pts',(-8.03438417900006,15.2,6.57445160599998));
#246284=CARTESIAN_POINT('Ctrl Pts',(-8.03438417900006,11.6,6.57445160599998));
#246285=CARTESIAN_POINT('Ctrl Pts',(-8.03518792400006,15.2,6.57499245799999));
#246286=CARTESIAN_POINT('Ctrl Pts',(-8.03518792400006,11.6,6.57499245799999));
#246287=CARTESIAN_POINT('Ctrl Pts',(-8.03600002200006,15.2,6.57553775199998));
#246288=CARTESIAN_POINT('Ctrl Pts',(-8.03600002200006,11.6,6.57553775199998));
#246289=CARTESIAN_POINT('Ctrl Pts',(-8.03682046100005,15.2,6.57608745999998));
#246290=CARTESIAN_POINT('Ctrl Pts',(-8.03682046100005,11.6,6.57608745999998));
#246291=CARTESIAN_POINT('Ctrl Pts',(-8.03764922900006,15.2,6.57664155099998));
#246292=CARTESIAN_POINT('Ctrl Pts',(-8.03764922900006,11.6,6.57664155099998));
#246293=CARTESIAN_POINT('Ctrl Pts',(-8.03848631400006,15.2,6.57719999799999));
#246294=CARTESIAN_POINT('Ctrl Pts',(-8.03848631400006,11.6,6.57719999799999));
#246295=CARTESIAN_POINT('Ctrl Pts',(-8.03933170600006,15.2,6.57776276899998));
#246296=CARTESIAN_POINT('Ctrl Pts',(-8.03933170600006,11.6,6.57776276899998));
#246297=CARTESIAN_POINT('Ctrl Pts',(-8.04018539100005,15.2,6.57832983699999));
#246298=CARTESIAN_POINT('Ctrl Pts',(-8.04018539100005,11.6,6.57832983699999));
#246299=CARTESIAN_POINT('Ctrl Pts',(-8.04104735700006,15.2,6.57890117299999));
#246300=CARTESIAN_POINT('Ctrl Pts',(-8.04104735700006,11.6,6.57890117299999));
#246301=CARTESIAN_POINT('Ctrl Pts',(-8.04191759500006,15.2,6.57947674699999));
#246302=CARTESIAN_POINT('Ctrl Pts',(-8.04191759500006,11.6,6.57947674699999));
#246303=CARTESIAN_POINT('Ctrl Pts',(-8.04279609000006,15.2,6.58005653299998));
#246304=CARTESIAN_POINT('Ctrl Pts',(-8.04279609000006,11.6,6.58005653299998));
#246305=CARTESIAN_POINT('Ctrl Pts',(-8.04368283300006,15.2,6.58064049899998));
#246306=CARTESIAN_POINT('Ctrl Pts',(-8.04368283300006,11.6,6.58064049899998));
#246307=CARTESIAN_POINT('Ctrl Pts',(-8.04457781100006,15.2,6.58122862099999));
#246308=CARTESIAN_POINT('Ctrl Pts',(-8.04457781100006,11.6,6.58122862099999));
#246309=CARTESIAN_POINT('Ctrl Pts',(-8.04548101300006,15.2,6.58182086699998));
#246310=CARTESIAN_POINT('Ctrl Pts',(-8.04548101300006,11.6,6.58182086699998));
#246311=CARTESIAN_POINT('Ctrl Pts',(-8.04639242800006,15.2,6.58241721199998));
#246312=CARTESIAN_POINT('Ctrl Pts',(-8.04639242800006,11.6,6.58241721199998));
#246313=CARTESIAN_POINT('Ctrl Pts',(-8.04731204200005,15.2,6.58301762599999));
#246314=CARTESIAN_POINT('Ctrl Pts',(-8.04731204200005,11.6,6.58301762599999));
#246315=CARTESIAN_POINT('Ctrl Pts',(-8.04823984700005,15.2,6.58362208299998));
#246316=CARTESIAN_POINT('Ctrl Pts',(-8.04823984700005,11.6,6.58362208299998));
#246317=CARTESIAN_POINT('Ctrl Pts',(-8.04917582900006,15.2,6.58423055499998));
#246318=CARTESIAN_POINT('Ctrl Pts',(-8.04917582900006,11.6,6.58423055499998));
#246319=CARTESIAN_POINT('Ctrl Pts',(-8.05011997800005,15.2,6.58484301199999));
#246320=CARTESIAN_POINT('Ctrl Pts',(-8.05011997800005,11.6,6.58484301199999));
#246321=CARTESIAN_POINT('Ctrl Pts',(-8.05107228300006,15.2,6.58545943199999));
#246322=CARTESIAN_POINT('Ctrl Pts',(-8.05107228300006,11.6,6.58545943199999));
#246323=CARTESIAN_POINT('Ctrl Pts',(-8.05203273200006,15.2,6.58607978299998));
#246324=CARTESIAN_POINT('Ctrl Pts',(-8.05203273200006,11.6,6.58607978299998));
#246325=CARTESIAN_POINT('Ctrl Pts',(-8.05300131400006,15.2,6.58670403999999));
#246326=CARTESIAN_POINT('Ctrl Pts',(-8.05300131400006,11.6,6.58670403999999));
#246327=CARTESIAN_POINT('Ctrl Pts',(-8.05397801800006,15.2,6.58733217599998));
#246328=CARTESIAN_POINT('Ctrl Pts',(-8.05397801800006,11.6,6.58733217599998));
#246329=CARTESIAN_POINT('Ctrl Pts',(-8.05496283200006,15.2,6.58796416399999));
#246330=CARTESIAN_POINT('Ctrl Pts',(-8.05496283200006,11.6,6.58796416399999));
#246331=CARTESIAN_POINT('Ctrl Pts',(-8.05595574600006,15.2,6.58859997699999));
#246332=CARTESIAN_POINT('Ctrl Pts',(-8.05595574600006,11.6,6.58859997699999));
#246333=CARTESIAN_POINT('Ctrl Pts',(-8.05695674700006,15.2,6.58923959099998));
#246334=CARTESIAN_POINT('Ctrl Pts',(-8.05695674700006,11.6,6.58923959099998));
#246335=CARTESIAN_POINT('Ctrl Pts',(-8.05796582700006,15.2,6.58988297599999));
#246336=CARTESIAN_POINT('Ctrl Pts',(-8.05796582700006,11.6,6.58988297599999));
#246337=CARTESIAN_POINT('Ctrl Pts',(-8.05898297300006,15.2,6.59053010699999));
#246338=CARTESIAN_POINT('Ctrl Pts',(-8.05898297300006,11.6,6.59053010699999));
#246339=CARTESIAN_POINT('Ctrl Pts',(-8.06000817500006,15.2,6.59118095899998));
#246340=CARTESIAN_POINT('Ctrl Pts',(-8.06000817500006,11.6,6.59118095899998));
#246341=CARTESIAN_POINT('Ctrl Pts',(-8.06104142100006,15.2,6.59183550499999));
#246342=CARTESIAN_POINT('Ctrl Pts',(-8.06104142100006,11.6,6.59183550499999));
#246343=CARTESIAN_POINT('Ctrl Pts',(-8.06208270100005,15.2,6.59249371899998));
#246344=CARTESIAN_POINT('Ctrl Pts',(-8.06208270100005,11.6,6.59249371899998));
#246345=CARTESIAN_POINT('Ctrl Pts',(-8.06313200300006,15.2,6.59315557599999));
#246346=CARTESIAN_POINT('Ctrl Pts',(-8.06313200300006,11.6,6.59315557599999));
#246347=CARTESIAN_POINT('Ctrl Pts',(-8.06418931900006,15.2,6.59382104899999));
#246348=CARTESIAN_POINT('Ctrl Pts',(-8.06418931900006,11.6,6.59382104899999));
#246349=CARTESIAN_POINT('Ctrl Pts',(-8.06525463500006,15.2,6.59449011399998));
#246350=CARTESIAN_POINT('Ctrl Pts',(-8.06525463500006,11.6,6.59449011399998));
#246351=CARTESIAN_POINT('Ctrl Pts',(-8.06632794200006,15.2,6.59516274499998));
#246352=CARTESIAN_POINT('Ctrl Pts',(-8.06632794200006,11.6,6.59516274499998));
#246353=CARTESIAN_POINT('Ctrl Pts',(-8.06740922800006,15.2,6.59583891799999));
#246354=CARTESIAN_POINT('Ctrl Pts',(-8.06740922800006,11.6,6.59583891799999));
#246355=CARTESIAN_POINT('Ctrl Pts',(-8.06849848300006,15.2,6.59651860499999));
#246356=CARTESIAN_POINT('Ctrl Pts',(-8.06849848300006,11.6,6.59651860499999));
#246357=CARTESIAN_POINT('Ctrl Pts',(-8.06959569800006,15.2,6.59720178299998));
#246358=CARTESIAN_POINT('Ctrl Pts',(-8.06959569800006,11.6,6.59720178299998));
#246359=CARTESIAN_POINT('Ctrl Pts',(-8.07070086000006,15.2,6.59788842599998));
#246360=CARTESIAN_POINT('Ctrl Pts',(-8.07070086000006,11.6,6.59788842599998));
#246361=CARTESIAN_POINT('Ctrl Pts',(-8.07181396000006,15.2,6.59857850899999));
#246362=CARTESIAN_POINT('Ctrl Pts',(-8.07181396000006,11.6,6.59857850899999));
#246363=CARTESIAN_POINT('Ctrl Pts',(-8.07293498600006,15.2,6.59927200999999));
#246364=CARTESIAN_POINT('Ctrl Pts',(-8.07293498600006,11.6,6.59927200999999));
#246365=CARTESIAN_POINT('Ctrl Pts',(-8.07406393000005,15.2,6.59996890099999));
#246366=CARTESIAN_POINT('Ctrl Pts',(-8.07406393000005,11.6,6.59996890099999));
#246367=CARTESIAN_POINT('Ctrl Pts',(-8.07520077900006,15.2,6.60066915999998));
#246368=CARTESIAN_POINT('Ctrl Pts',(-8.07520077900006,11.6,6.60066915999998));
#246369=CARTESIAN_POINT('Ctrl Pts',(-8.07634552300006,15.2,6.60137276099999));
#246370=CARTESIAN_POINT('Ctrl Pts',(-8.07634552300006,11.6,6.60137276099999));
#246371=CARTESIAN_POINT('Ctrl Pts',(-8.07749815200006,15.2,6.60207967899999));
#246372=CARTESIAN_POINT('Ctrl Pts',(-8.07749815200006,11.6,6.60207967899999));
#246373=CARTESIAN_POINT('Ctrl Pts',(-8.07865865700006,15.2,6.60278989299999));
#246374=CARTESIAN_POINT('Ctrl Pts',(-8.07865865700006,11.6,6.60278989299999));
#246375=CARTESIAN_POINT('Ctrl Pts',(-8.07982702600006,15.2,6.60350337599999));
#246376=CARTESIAN_POINT('Ctrl Pts',(-8.07982702600006,11.6,6.60350337599999));
#246377=CARTESIAN_POINT('Ctrl Pts',(-8.08100324800006,15.2,6.60422010599999));
#246378=CARTESIAN_POINT('Ctrl Pts',(-8.08100324800006,11.6,6.60422010599999));
#246379=CARTESIAN_POINT('Ctrl Pts',(-8.08218731400006,15.2,6.60494005799999));
#246380=CARTESIAN_POINT('Ctrl Pts',(-8.08218731400006,11.6,6.60494005799999));
#246381=CARTESIAN_POINT('Ctrl Pts',(-8.08337921500006,15.2,6.60566320799998));
#246382=CARTESIAN_POINT('Ctrl Pts',(-8.08337921500006,11.6,6.60566320799998));
#246383=CARTESIAN_POINT('Ctrl Pts',(-8.08457893900006,15.2,6.60638953299999));
#246384=CARTESIAN_POINT('Ctrl Pts',(-8.08457893900006,11.6,6.60638953299999));
#246385=CARTESIAN_POINT('Ctrl Pts',(-8.08578647500006,15.2,6.60711900999999));
#246386=CARTESIAN_POINT('Ctrl Pts',(-8.08578647500006,11.6,6.60711900999999));
#246387=CARTESIAN_POINT('Ctrl Pts',(-8.08700181600006,15.2,6.60785161499999));
#246388=CARTESIAN_POINT('Ctrl Pts',(-8.08700181600006,11.6,6.60785161499999));
#246389=CARTESIAN_POINT('Ctrl Pts',(-8.08822494800006,15.2,6.60858732499998));
#246390=CARTESIAN_POINT('Ctrl Pts',(-8.08822494800006,11.6,6.60858732499998));
#246391=CARTESIAN_POINT('Ctrl Pts',(-8.08945586400006,15.2,6.60932611599998));
#246392=CARTESIAN_POINT('Ctrl Pts',(-8.08945586400006,11.6,6.60932611599998));
#246393=CARTESIAN_POINT('Ctrl Pts',(-8.09069455200006,15.2,6.61006796499999));
#246394=CARTESIAN_POINT('Ctrl Pts',(-8.09069455200006,11.6,6.61006796499999));
#246395=CARTESIAN_POINT('Ctrl Pts',(-8.09194100400006,15.2,6.61081285099999));
#246396=CARTESIAN_POINT('Ctrl Pts',(-8.09194100400006,11.6,6.61081285099999));
#246397=CARTESIAN_POINT('Ctrl Pts',(-8.09319520700006,15.2,6.61156074899999));
#246398=CARTESIAN_POINT('Ctrl Pts',(-8.09319520700006,11.6,6.61156074899999));
#246399=CARTESIAN_POINT('Ctrl Pts',(-8.09445715400006,15.2,6.61231163599999));
#246400=CARTESIAN_POINT('Ctrl Pts',(-8.09445715400006,11.6,6.61231163599999));
#246401=CARTESIAN_POINT('Ctrl Pts',(-8.09572683400006,15.2,6.61306549099999));
#246402=CARTESIAN_POINT('Ctrl Pts',(-8.09572683400006,11.6,6.61306549099999));
#246403=CARTESIAN_POINT('Ctrl Pts',(-8.09700423700006,15.2,6.61382228999998));
#246404=CARTESIAN_POINT('Ctrl Pts',(-8.09700423700006,11.6,6.61382228999998));
#246405=CARTESIAN_POINT('Ctrl Pts',(-8.09828935300006,15.2,6.61458201099999));
#246406=CARTESIAN_POINT('Ctrl Pts',(-8.09828935300006,11.6,6.61458201099999));
#246407=CARTESIAN_POINT('Ctrl Pts',(-8.09958217100006,15.2,6.61534463099999));
#246408=CARTESIAN_POINT('Ctrl Pts',(-8.09958217100006,11.6,6.61534463099999));
#246409=CARTESIAN_POINT('Ctrl Pts',(-8.10088268300006,15.2,6.61611012799998));
#246410=CARTESIAN_POINT('Ctrl Pts',(-8.10088268300006,11.6,6.61611012799998));
#246411=CARTESIAN_POINT('Ctrl Pts',(-8.10219087900006,15.2,6.61687848099999));
#246412=CARTESIAN_POINT('Ctrl Pts',(-8.10219087900006,11.6,6.61687848099999));
#246413=CARTESIAN_POINT('Ctrl Pts',(-8.10350674900005,15.2,6.61764966799999));
#246414=CARTESIAN_POINT('Ctrl Pts',(-8.10350674900005,11.6,6.61764966799999));
#246415=CARTESIAN_POINT('Ctrl Pts',(-8.10483028300006,15.2,6.61842366399998));
#246416=CARTESIAN_POINT('Ctrl Pts',(-8.10483028300006,11.6,6.61842366399998));
#246417=CARTESIAN_POINT('Ctrl Pts',(-8.10616147100006,15.2,6.61920044899999));
#246418=CARTESIAN_POINT('Ctrl Pts',(-8.10616147100006,11.6,6.61920044899999));
#246419=CARTESIAN_POINT('Ctrl Pts',(-8.10750030400006,15.2,6.61998000199999));
#246420=CARTESIAN_POINT('Ctrl Pts',(-8.10750030400006,11.6,6.61998000199999));
#246421=CARTESIAN_POINT('Ctrl Pts',(-8.10884677200006,15.2,6.62076229999998));
#246422=CARTESIAN_POINT('Ctrl Pts',(-8.10884677200006,11.6,6.62076229999998));
#246423=CARTESIAN_POINT('Ctrl Pts',(-8.11020086500006,15.2,6.62154732099999));
#246424=CARTESIAN_POINT('Ctrl Pts',(-8.11020086500006,11.6,6.62154732099999));
#246425=CARTESIAN_POINT('Ctrl Pts',(-8.11156257400006,15.2,6.62233504499999));
#246426=CARTESIAN_POINT('Ctrl Pts',(-8.11156257400006,11.6,6.62233504499999));
#246427=CARTESIAN_POINT('Ctrl Pts',(-8.11293189000006,15.2,6.62312544999998));
#246428=CARTESIAN_POINT('Ctrl Pts',(-8.11293189000006,11.6,6.62312544999998));
#246429=CARTESIAN_POINT('Ctrl Pts',(-8.11430880100006,15.2,6.62391851299999));
#246430=CARTESIAN_POINT('Ctrl Pts',(-8.11430880100006,11.6,6.62391851299999));
#246431=CARTESIAN_POINT('Ctrl Pts',(-8.11569330000006,15.2,6.62471421499998));
#246432=CARTESIAN_POINT('Ctrl Pts',(-8.11569330000006,11.6,6.62471421499998));
#246433=CARTESIAN_POINT('Ctrl Pts',(-8.11708537600006,15.2,6.62551253399998));
#246434=CARTESIAN_POINT('Ctrl Pts',(-8.11708537600006,11.6,6.62551253399998));
#246435=CARTESIAN_POINT('Ctrl Pts',(-8.11848502100006,15.2,6.62631344799999));
#246436=CARTESIAN_POINT('Ctrl Pts',(-8.11848502100006,11.6,6.62631344799999));
#246437=CARTESIAN_POINT('Ctrl Pts',(-8.11989222400006,15.2,6.62711693599999));
#246438=CARTESIAN_POINT('Ctrl Pts',(-8.11989222400006,11.6,6.62711693599999));
#246439=CARTESIAN_POINT('Ctrl Pts',(-8.12130697600006,15.2,6.62792297899998));
#246440=CARTESIAN_POINT('Ctrl Pts',(-8.12130697600006,11.6,6.62792297899998));
#246441=CARTESIAN_POINT('Ctrl Pts',(-8.12272926800006,15.2,6.62873155499998));
#246442=CARTESIAN_POINT('Ctrl Pts',(-8.12272926800006,11.6,6.62873155499998));
#246443=CARTESIAN_POINT('Ctrl Pts',(-8.12415909100006,15.2,6.62954264199998));
#246444=CARTESIAN_POINT('Ctrl Pts',(-8.12415909100006,11.6,6.62954264199998));
#246445=CARTESIAN_POINT('Ctrl Pts',(-8.12559643300006,15.2,6.63035622099999));
#246446=CARTESIAN_POINT('Ctrl Pts',(-8.12559643300006,11.6,6.63035622099999));
#246447=CARTESIAN_POINT('Ctrl Pts',(-8.12704128900006,15.2,6.63117227099999));
#246448=CARTESIAN_POINT('Ctrl Pts',(-8.12704128900006,11.6,6.63117227099999));
#246449=CARTESIAN_POINT('Ctrl Pts',(-8.12849364700006,15.2,6.63199077099998));
#246450=CARTESIAN_POINT('Ctrl Pts',(-8.12849364700006,11.6,6.63199077099998));
#246451=CARTESIAN_POINT('Ctrl Pts',(-8.12995349700006,15.2,6.63281169999999));
#246452=CARTESIAN_POINT('Ctrl Pts',(-8.12995349700006,11.6,6.63281169999999));
#246453=CARTESIAN_POINT('Ctrl Pts',(-8.13142083200006,15.2,6.63363503899999));
#246454=CARTESIAN_POINT('Ctrl Pts',(-8.13142083200006,11.6,6.63363503899999));
#246455=CARTESIAN_POINT('Ctrl Pts',(-8.13289564100005,15.2,6.63446076699999));
#246456=CARTESIAN_POINT('Ctrl Pts',(-8.13289564100005,11.6,6.63446076699999));
#246457=CARTESIAN_POINT('Ctrl Pts',(-8.13437791500006,15.2,6.63528886499999));
#246458=CARTESIAN_POINT('Ctrl Pts',(-8.13437791500006,11.6,6.63528886499999));
#246459=CARTESIAN_POINT('Ctrl Pts',(-8.13586764600006,15.2,6.63611931099998));
#246460=CARTESIAN_POINT('Ctrl Pts',(-8.13586764600006,11.6,6.63611931099998));
#246461=CARTESIAN_POINT('Ctrl Pts',(-8.13736482400006,15.2,6.63695208599999));
#246462=CARTESIAN_POINT('Ctrl Pts',(-8.13736482400006,11.6,6.63695208599999));
#246463=CARTESIAN_POINT('Ctrl Pts',(-8.13886943900006,15.2,6.63778716999998));
#246464=CARTESIAN_POINT('Ctrl Pts',(-8.13886943900006,11.6,6.63778716999998));
#246465=CARTESIAN_POINT('Ctrl Pts',(-8.14038148300006,15.2,6.63862454399998));
#246466=CARTESIAN_POINT('Ctrl Pts',(-8.14038148300006,11.6,6.63862454399998));
#246467=CARTESIAN_POINT('Ctrl Pts',(-8.14190094800006,15.2,6.63946418699998));
#246468=CARTESIAN_POINT('Ctrl Pts',(-8.14190094800006,11.6,6.63946418699998));
#246469=CARTESIAN_POINT('Ctrl Pts',(-8.14342782200006,15.2,6.64030607899999));
#246470=CARTESIAN_POINT('Ctrl Pts',(-8.14342782200006,11.6,6.64030607899999));
#246471=CARTESIAN_POINT('Ctrl Pts',(-8.14496209800006,15.2,6.64115020099998));
#246472=CARTESIAN_POINT('Ctrl Pts',(-8.14496209800006,11.6,6.64115020099998));
#246473=CARTESIAN_POINT('Ctrl Pts',(-8.14650376600006,15.2,6.64199653299999));
#246474=CARTESIAN_POINT('Ctrl Pts',(-8.14650376600006,11.6,6.64199653299999));
#246475=CARTESIAN_POINT('Ctrl Pts',(-8.14805281800006,15.2,6.64284505699998));
#246476=CARTESIAN_POINT('Ctrl Pts',(-8.14805281800006,11.6,6.64284505699998));
#246477=CARTESIAN_POINT('Ctrl Pts',(-8.14960924300006,15.2,6.64369575199999));
#246478=CARTESIAN_POINT('Ctrl Pts',(-8.14960924300006,11.6,6.64369575199999));
#246479=CARTESIAN_POINT('Ctrl Pts',(-8.15117303600006,15.2,6.64454859999999));
#246480=CARTESIAN_POINT('Ctrl Pts',(-8.15117303600006,11.6,6.64454859999999));
#246481=CARTESIAN_POINT('Ctrl Pts',(-8.15274418400006,15.2,6.64540357999999));
#246482=CARTESIAN_POINT('Ctrl Pts',(-8.15274418400006,11.6,6.64540357999999));
#246483=CARTESIAN_POINT('Ctrl Pts',(-8.15432267900006,15.2,6.64626067399999));
#246484=CARTESIAN_POINT('Ctrl Pts',(-8.15432267900006,11.6,6.64626067399999));
#246485=CARTESIAN_POINT('Ctrl Pts',(-8.15590851400006,15.2,6.64711986299999));
#246486=CARTESIAN_POINT('Ctrl Pts',(-8.15590851400006,11.6,6.64711986299999));
#246487=CARTESIAN_POINT('Ctrl Pts',(-8.15750167800006,15.2,6.64798112699999));
#246488=CARTESIAN_POINT('Ctrl Pts',(-8.15750167800006,11.6,6.64798112699999));
#246489=CARTESIAN_POINT('Ctrl Pts',(-8.15910216400006,15.2,6.64884444899998));
#246490=CARTESIAN_POINT('Ctrl Pts',(-8.15910216400006,11.6,6.64884444899998));
#246491=CARTESIAN_POINT('Ctrl Pts',(-8.16070996000006,15.2,6.64970980799998));
#246492=CARTESIAN_POINT('Ctrl Pts',(-8.16070996000006,11.6,6.64970980799998));
#246493=CARTESIAN_POINT('Ctrl Pts',(-8.16232506100006,15.2,6.65057718599999));
#246494=CARTESIAN_POINT('Ctrl Pts',(-8.16232506100006,11.6,6.65057718599999));
#246495=CARTESIAN_POINT('Ctrl Pts',(-8.16394745600006,15.2,6.65144656499999));
#246496=CARTESIAN_POINT('Ctrl Pts',(-8.16394745600006,11.6,6.65144656499999));
#246497=CARTESIAN_POINT('Ctrl Pts',(-8.16557713600006,15.2,6.65231792599998));
#246498=CARTESIAN_POINT('Ctrl Pts',(-8.16557713600006,11.6,6.65231792599998));
#246499=CARTESIAN_POINT('Ctrl Pts',(-8.16721409300006,15.2,6.65319124899998));
#246500=CARTESIAN_POINT('Ctrl Pts',(-8.16721409300006,11.6,6.65319124899998));
#246501=CARTESIAN_POINT('Ctrl Pts',(-8.16885831800005,15.2,6.65406651699998));
#246502=CARTESIAN_POINT('Ctrl Pts',(-8.16885831800005,11.6,6.65406651699998));
#246503=CARTESIAN_POINT('Ctrl Pts',(-8.17050980300005,15.2,6.65494371199999));
#246504=CARTESIAN_POINT('Ctrl Pts',(-8.17050980300005,11.6,6.65494371199999));
#246505=CARTESIAN_POINT('Ctrl Pts',(-8.17216853900005,15.2,6.65582281399999));
#246506=CARTESIAN_POINT('Ctrl Pts',(-8.17216853900005,11.6,6.65582281399999));
#246507=CARTESIAN_POINT('Ctrl Pts',(-8.17383451600006,15.2,6.65670380499999));
#246508=CARTESIAN_POINT('Ctrl Pts',(-8.17383451600006,11.6,6.65670380499999));
#246509=CARTESIAN_POINT('Ctrl Pts',(-8.17550772700006,15.2,6.65758666799999));
#246510=CARTESIAN_POINT('Ctrl Pts',(-8.17550772700006,11.6,6.65758666799999));
#246511=CARTESIAN_POINT('Ctrl Pts',(-8.17718816300006,15.2,6.65847138399998));
#246512=CARTESIAN_POINT('Ctrl Pts',(-8.17718816300006,11.6,6.65847138399998));
#246513=CARTESIAN_POINT('Ctrl Pts',(-8.17887581500005,15.2,6.65935793499998));
#246514=CARTESIAN_POINT('Ctrl Pts',(-8.17887581500005,11.6,6.65935793499998));
#246515=CARTESIAN_POINT('Ctrl Pts',(-8.18057067400006,15.2,6.66024630299999));
#246516=CARTESIAN_POINT('Ctrl Pts',(-8.18057067400006,11.6,6.66024630299999));
#246517=CARTESIAN_POINT('Ctrl Pts',(-8.18227273200005,15.2,6.66113646999998));
#246518=CARTESIAN_POINT('Ctrl Pts',(-8.18227273200005,11.6,6.66113646999998));
#246519=CARTESIAN_POINT('Ctrl Pts',(-8.18398198000006,15.2,6.66202841799999));
#246520=CARTESIAN_POINT('Ctrl Pts',(-8.18398198000006,11.6,6.66202841799999));
#246521=CARTESIAN_POINT('Ctrl Pts',(-8.18569841000006,15.2,6.66292212999998));
#246522=CARTESIAN_POINT('Ctrl Pts',(-8.18569841000006,11.6,6.66292212999998));
#246523=CARTESIAN_POINT('Ctrl Pts',(-8.18742201200006,15.2,6.66381758699998));
#246524=CARTESIAN_POINT('Ctrl Pts',(-8.18742201200006,11.6,6.66381758699998));
#246525=CARTESIAN_POINT('Ctrl Pts',(-8.18915278100006,15.2,6.66471477199998));
#246526=CARTESIAN_POINT('Ctrl Pts',(-8.18915278100006,11.6,6.66471477199998));
#246527=CARTESIAN_POINT('Ctrl Pts',(-8.19089070500005,15.2,6.66561366699998));
#246528=CARTESIAN_POINT('Ctrl Pts',(-8.19089070500005,11.6,6.66561366699998));
#246529=CARTESIAN_POINT('Ctrl Pts',(-8.19263577500006,15.2,6.66651425499998));
#246530=CARTESIAN_POINT('Ctrl Pts',(-8.19263577500006,11.6,6.66651425499998));
#246531=CARTESIAN_POINT('Ctrl Pts',(-8.19438798700006,15.2,6.66741651699999));
#246532=CARTESIAN_POINT('Ctrl Pts',(-8.19438798700006,11.6,6.66741651699999));
#246533=CARTESIAN_POINT('Ctrl Pts',(-8.19614732800006,15.2,6.66832043799998));
#246534=CARTESIAN_POINT('Ctrl Pts',(-8.19614732800006,11.6,6.66832043799998));
#246535=CARTESIAN_POINT('Ctrl Pts',(-8.19791379200005,15.2,6.66922599899999));
#246536=CARTESIAN_POINT('Ctrl Pts',(-8.19791379200005,11.6,6.66922599899999));
#246537=CARTESIAN_POINT('Ctrl Pts',(-8.19968736900006,15.2,6.67013318399999));
#246538=CARTESIAN_POINT('Ctrl Pts',(-8.19968736900006,11.6,6.67013318399999));
#246539=CARTESIAN_POINT('Ctrl Pts',(-8.20146805300006,15.2,6.67104197399999));
#246540=CARTESIAN_POINT('Ctrl Pts',(-8.20146805300006,11.6,6.67104197399999));
#246541=CARTESIAN_POINT('Ctrl Pts',(-8.20325583300006,15.2,6.67195235199999));
#246542=CARTESIAN_POINT('Ctrl Pts',(-8.20325583300006,11.6,6.67195235199999));
#246543=CARTESIAN_POINT('Ctrl Pts',(-8.20505070200005,15.2,6.67286430199999));
#246544=CARTESIAN_POINT('Ctrl Pts',(-8.20505070200005,11.6,6.67286430199999));
#246545=CARTESIAN_POINT('Ctrl Pts',(-8.20685265200006,15.2,6.67377780699999));
#246546=CARTESIAN_POINT('Ctrl Pts',(-8.20685265200006,11.6,6.67377780699999));
#246547=CARTESIAN_POINT('Ctrl Pts',(-8.20866167300006,15.2,6.67469284899998));
#246548=CARTESIAN_POINT('Ctrl Pts',(-8.20866167300006,11.6,6.67469284899998));
#246549=CARTESIAN_POINT('Ctrl Pts',(-8.21047775900006,15.2,6.67560941199999));
#246550=CARTESIAN_POINT('Ctrl Pts',(-8.21047775900006,11.6,6.67560941199999));
#246551=CARTESIAN_POINT('Ctrl Pts',(-8.21230090000006,15.2,6.67652747899999));
#246552=CARTESIAN_POINT('Ctrl Pts',(-8.21230090000006,11.6,6.67652747899999));
#246553=CARTESIAN_POINT('Ctrl Pts',(-8.21413108800006,15.2,6.67744703199999));
#246554=CARTESIAN_POINT('Ctrl Pts',(-8.21413108800006,11.6,6.67744703199999));
#246555=CARTESIAN_POINT('Ctrl Pts',(-8.21596831500005,15.2,6.67836805599999));
#246556=CARTESIAN_POINT('Ctrl Pts',(-8.21596831500005,11.6,6.67836805599999));
#246557=CARTESIAN_POINT('Ctrl Pts',(-8.21781257400006,15.2,6.67929053299999));
#246558=CARTESIAN_POINT('Ctrl Pts',(-8.21781257400006,11.6,6.67929053299999));
#246559=CARTESIAN_POINT('Ctrl Pts',(-8.21966385400006,15.2,6.68021444699999));
#246560=CARTESIAN_POINT('Ctrl Pts',(-8.21966385400006,11.6,6.68021444699999));
#246561=CARTESIAN_POINT('Ctrl Pts',(-8.22152214900006,15.2,6.68113978099999));
#246562=CARTESIAN_POINT('Ctrl Pts',(-8.22152214900006,11.6,6.68113978099999));
#246563=CARTESIAN_POINT('Ctrl Pts',(-8.22338745000006,15.2,6.68206651899999));
#246564=CARTESIAN_POINT('Ctrl Pts',(-8.22338745000006,11.6,6.68206651899999));
#246565=CARTESIAN_POINT('Ctrl Pts',(-8.22525974800006,15.2,6.68299464499999));
#246566=CARTESIAN_POINT('Ctrl Pts',(-8.22525974800006,11.6,6.68299464499999));
#246567=CARTESIAN_POINT('Ctrl Pts',(-8.22713903600006,15.2,6.68392414099999));
#246568=CARTESIAN_POINT('Ctrl Pts',(-8.22713903600006,11.6,6.68392414099999));
#246569=CARTESIAN_POINT('Ctrl Pts',(-8.22902530700006,15.2,6.68485499099998));
#246570=CARTESIAN_POINT('Ctrl Pts',(-8.22902530700006,11.6,6.68485499099998));
#246571=CARTESIAN_POINT('Ctrl Pts',(-8.23091855000006,15.2,6.68578718099998));
#246572=CARTESIAN_POINT('Ctrl Pts',(-8.23091855000006,11.6,6.68578718099998));
#246573=CARTESIAN_POINT('Ctrl Pts',(-8.23281876000006,15.2,6.68672069299999));
#246574=CARTESIAN_POINT('Ctrl Pts',(-8.23281876000006,11.6,6.68672069299999));
#246575=CARTESIAN_POINT('Ctrl Pts',(-8.23472592500006,15.2,6.68765550999999));
#246576=CARTESIAN_POINT('Ctrl Pts',(-8.23472592500006,11.6,6.68765550999999));
#246577=CARTESIAN_POINT('Ctrl Pts',(-8.23664004100005,15.2,6.68859161699999));
#246578=CARTESIAN_POINT('Ctrl Pts',(-8.23664004100005,11.6,6.68859161699999));
#246579=CARTESIAN_POINT('Ctrl Pts',(-8.23856109700005,15.2,6.68952899899999));
#246580=CARTESIAN_POINT('Ctrl Pts',(-8.23856109700005,11.6,6.68952899899999));
#246581=CARTESIAN_POINT('Ctrl Pts',(-8.24048908700006,15.2,6.69046763799999));
#246582=CARTESIAN_POINT('Ctrl Pts',(-8.24048908700006,11.6,6.69046763799999));
#246583=CARTESIAN_POINT('Ctrl Pts',(-8.24242400200006,15.2,6.69140751899998));
#246584=CARTESIAN_POINT('Ctrl Pts',(-8.24242400200006,11.6,6.69140751899998));
#246585=CARTESIAN_POINT('Ctrl Pts',(-8.24436583300006,15.2,6.69234862599998));
#246586=CARTESIAN_POINT('Ctrl Pts',(-8.24436583300006,11.6,6.69234862599998));
#246587=CARTESIAN_POINT('Ctrl Pts',(-8.24631457400006,15.2,6.69329094299999));
#246588=CARTESIAN_POINT('Ctrl Pts',(-8.24631457400006,11.6,6.69329094299999));
#246589=CARTESIAN_POINT('Ctrl Pts',(-8.24827021500005,15.2,6.69423445399998));
#246590=CARTESIAN_POINT('Ctrl Pts',(-8.24827021500005,11.6,6.69423445399998));
#246591=CARTESIAN_POINT('Ctrl Pts',(-8.25023275000006,15.2,6.69517914499998));
#246592=CARTESIAN_POINT('Ctrl Pts',(-8.25023275000006,11.6,6.69517914499998));
#246593=CARTESIAN_POINT('Ctrl Pts',(-8.25220216900006,15.2,6.69612499799998));
#246594=CARTESIAN_POINT('Ctrl Pts',(-8.25220216900006,11.6,6.69612499799998));
#246595=CARTESIAN_POINT('Ctrl Pts',(-8.25417846600006,15.2,6.69707199899998));
#246596=CARTESIAN_POINT('Ctrl Pts',(-8.25417846600006,11.6,6.69707199899998));
#246597=CARTESIAN_POINT('Ctrl Pts',(-8.25616163200005,15.2,6.69802013199998));
#246598=CARTESIAN_POINT('Ctrl Pts',(-8.25616163200005,11.6,6.69802013199998));
#246599=CARTESIAN_POINT('Ctrl Pts',(-8.25815165800006,15.2,6.69896937999999));
#246600=CARTESIAN_POINT('Ctrl Pts',(-8.25815165800006,11.6,6.69896937999999));
#246601=CARTESIAN_POINT('Ctrl Pts',(-8.26014853900006,15.2,6.69991973099999));
#246602=CARTESIAN_POINT('Ctrl Pts',(-8.26014853900006,11.6,6.69991973099999));
#246603=CARTESIAN_POINT('Ctrl Pts',(-8.26215226500005,15.2,6.70087116699998));
#246604=CARTESIAN_POINT('Ctrl Pts',(-8.26215226500005,11.6,6.70087116699998));
#246605=CARTESIAN_POINT('Ctrl Pts',(-8.26416282900006,15.2,6.70182367299999));
#246606=CARTESIAN_POINT('Ctrl Pts',(-8.26416282900006,11.6,6.70182367299999));
#246607=CARTESIAN_POINT('Ctrl Pts',(-8.26618022200006,15.2,6.70277723399998));
#246608=CARTESIAN_POINT('Ctrl Pts',(-8.26618022200006,11.6,6.70277723399998));
#246609=CARTESIAN_POINT('Ctrl Pts',(-8.26820443600005,15.2,6.70373183399998));
#246610=CARTESIAN_POINT('Ctrl Pts',(-8.26820443600005,11.6,6.70373183399998));
#246611=CARTESIAN_POINT('Ctrl Pts',(-8.27023546500006,15.2,6.70468745899999));
#246612=CARTESIAN_POINT('Ctrl Pts',(-8.27023546500006,11.6,6.70468745899999));
#246613=CARTESIAN_POINT('Ctrl Pts',(-8.27227330000006,15.2,6.70564409399999));
#246614=CARTESIAN_POINT('Ctrl Pts',(-8.27227330000006,11.6,6.70564409399999));
#246615=CARTESIAN_POINT('Ctrl Pts',(-8.27431793400006,15.2,6.70660172299999));
#246616=CARTESIAN_POINT('Ctrl Pts',(-8.27431793400006,11.6,6.70660172299999));
#246617=CARTESIAN_POINT('Ctrl Pts',(-8.27636935800006,15.2,6.70756033199999));
#246618=CARTESIAN_POINT('Ctrl Pts',(-8.27636935800006,11.6,6.70756033199999));
#246619=CARTESIAN_POINT('Ctrl Pts',(-8.27842756500005,15.2,6.70851990399999));
#246620=CARTESIAN_POINT('Ctrl Pts',(-8.27842756500005,11.6,6.70851990399999));
#246621=CARTESIAN_POINT('Ctrl Pts',(-8.28049254600005,15.2,6.70948042599999));
#246622=CARTESIAN_POINT('Ctrl Pts',(-8.28049254600005,11.6,6.70948042599999));
#246623=CARTESIAN_POINT('Ctrl Pts',(-8.28256429600006,15.2,6.71044188299999));
#246624=CARTESIAN_POINT('Ctrl Pts',(-8.28256429600006,11.6,6.71044188299999));
#246625=CARTESIAN_POINT('Ctrl Pts',(-8.28464280400006,15.2,6.71140425899999));
#246626=CARTESIAN_POINT('Ctrl Pts',(-8.28464280400006,11.6,6.71140425899999));
#246627=CARTESIAN_POINT('Ctrl Pts',(-8.28672806400006,15.2,6.71236754099999));
#246628=CARTESIAN_POINT('Ctrl Pts',(-8.28672806400006,11.6,6.71236754099999));
#246629=CARTESIAN_POINT('Ctrl Pts',(-8.28882006800006,15.2,6.71333171199999));
#246630=CARTESIAN_POINT('Ctrl Pts',(-8.28882006800006,11.6,6.71333171199999));
#246631=CARTESIAN_POINT('Ctrl Pts',(-8.29091880900006,15.2,6.71429675899999));
#246632=CARTESIAN_POINT('Ctrl Pts',(-8.29091880900006,11.6,6.71429675899999));
#246633=CARTESIAN_POINT('Ctrl Pts',(-8.29302427900006,15.2,6.71526266699999));
#246634=CARTESIAN_POINT('Ctrl Pts',(-8.29302427900006,11.6,6.71526266699999));
#246635=CARTESIAN_POINT('Ctrl Pts',(-8.29513646900006,15.2,6.71622942099999));
#246636=CARTESIAN_POINT('Ctrl Pts',(-8.29513646900006,11.6,6.71622942099999));
#246637=CARTESIAN_POINT('Ctrl Pts',(-8.29725537200006,15.2,6.71719700699998));
#246638=CARTESIAN_POINT('Ctrl Pts',(-8.29725537200006,11.6,6.71719700699998));
#246639=CARTESIAN_POINT('Ctrl Pts',(-8.29938098200006,15.2,6.71816541099999));
#246640=CARTESIAN_POINT('Ctrl Pts',(-8.29938098200006,11.6,6.71816541099999));
#246641=CARTESIAN_POINT('Ctrl Pts',(-8.30151329000006,15.2,6.71913461699998));
#246642=CARTESIAN_POINT('Ctrl Pts',(-8.30151329000006,11.6,6.71913461699998));
#246643=CARTESIAN_POINT('Ctrl Pts',(-8.30365228800006,15.2,6.72010461099998));
#246644=CARTESIAN_POINT('Ctrl Pts',(-8.30365228800006,11.6,6.72010461099998));
#246645=CARTESIAN_POINT('Ctrl Pts',(-8.30579796800006,15.2,6.72107537999998));
#246646=CARTESIAN_POINT('Ctrl Pts',(-8.30579796800006,11.6,6.72107537999998));
#246647=CARTESIAN_POINT('Ctrl Pts',(-8.30795032400006,15.2,6.72204690899999));
#246648=CARTESIAN_POINT('Ctrl Pts',(-8.30795032400006,11.6,6.72204690899999));
#246649=CARTESIAN_POINT('Ctrl Pts',(-8.31010934700006,15.2,6.72301918299999));
#246650=CARTESIAN_POINT('Ctrl Pts',(-8.31010934700006,11.6,6.72301918299999));
#246651=CARTESIAN_POINT('Ctrl Pts',(-8.31227503200006,15.2,6.72399218899999));
#246652=CARTESIAN_POINT('Ctrl Pts',(-8.31227503200006,11.6,6.72399218899999));
#246653=CARTESIAN_POINT('Ctrl Pts',(-8.31444736700006,15.2,6.72496591099998));
#246654=CARTESIAN_POINT('Ctrl Pts',(-8.31444736700006,11.6,6.72496591099998));
#246655=CARTESIAN_POINT('Ctrl Pts',(-8.31662634800006,15.2,6.72594033599999));
#246656=CARTESIAN_POINT('Ctrl Pts',(-8.31662634800006,11.6,6.72594033599999));
#246657=CARTESIAN_POINT('Ctrl Pts',(-8.31881196700006,15.2,6.72691545099998));
#246658=CARTESIAN_POINT('Ctrl Pts',(-8.31881196700006,11.6,6.72691545099998));
#246659=CARTESIAN_POINT('Ctrl Pts',(-8.32100421400006,15.2,6.72789124199999));
#246660=CARTESIAN_POINT('Ctrl Pts',(-8.32100421400006,11.6,6.72789124199999));
#246661=CARTESIAN_POINT('Ctrl Pts',(-8.32320308600006,15.2,6.72886769299998));
#246662=CARTESIAN_POINT('Ctrl Pts',(-8.32320308600006,11.6,6.72886769299998));
#246663=CARTESIAN_POINT('Ctrl Pts',(-8.32540857100006,15.2,6.72984479099998));
#246664=CARTESIAN_POINT('Ctrl Pts',(-8.32540857100006,11.6,6.72984479099998));
#246665=CARTESIAN_POINT('Ctrl Pts',(-8.32762066300005,15.2,6.73082252199999));
#246666=CARTESIAN_POINT('Ctrl Pts',(-8.32762066300005,11.6,6.73082252199999));
#246667=CARTESIAN_POINT('Ctrl Pts',(-8.32983935500006,15.2,6.73180087299999));
#246668=CARTESIAN_POINT('Ctrl Pts',(-8.32983935500006,11.6,6.73180087299999));
#246669=CARTESIAN_POINT('Ctrl Pts',(-8.33206464000006,15.2,6.73277982899998));
#246670=CARTESIAN_POINT('Ctrl Pts',(-8.33206464000006,11.6,6.73277982899998));
#246671=CARTESIAN_POINT('Ctrl Pts',(-8.33429651000005,15.2,6.73375937799998));
#246672=CARTESIAN_POINT('Ctrl Pts',(-8.33429651000005,11.6,6.73375937799998));
#246673=CARTESIAN_POINT('Ctrl Pts',(-8.33653495700006,15.2,6.73473950399998));
#246674=CARTESIAN_POINT('Ctrl Pts',(-8.33653495700006,11.6,6.73473950399998));
#246675=CARTESIAN_POINT('Ctrl Pts',(-8.33877997400006,15.2,6.73572019399998));
#246676=CARTESIAN_POINT('Ctrl Pts',(-8.33877997400006,11.6,6.73572019399998));
#246677=CARTESIAN_POINT('Ctrl Pts',(-8.34103155400006,15.2,6.73670143699999));
#246678=CARTESIAN_POINT('Ctrl Pts',(-8.34103155400006,11.6,6.73670143699999));
#246679=CARTESIAN_POINT('Ctrl Pts',(-8.34328968900006,15.2,6.73768321599999));
#246680=CARTESIAN_POINT('Ctrl Pts',(-8.34328968900006,11.6,6.73768321599999));
#246681=CARTESIAN_POINT('Ctrl Pts',(-8.34555437200006,15.2,6.73866551899999));
#246682=CARTESIAN_POINT('Ctrl Pts',(-8.34555437200006,11.6,6.73866551899999));
#246683=CARTESIAN_POINT('Ctrl Pts',(-8.34782559500006,15.2,6.73964833199998));
#246684=CARTESIAN_POINT('Ctrl Pts',(-8.34782559500006,11.6,6.73964833199998));
#246685=CARTESIAN_POINT('Ctrl Pts',(-8.35010335200005,15.2,6.74063164199998));
#246686=CARTESIAN_POINT('Ctrl Pts',(-8.35010335200005,11.6,6.74063164199998));
#246687=CARTESIAN_POINT('Ctrl Pts',(-8.35238763300006,15.2,6.74161543599999));
#246688=CARTESIAN_POINT('Ctrl Pts',(-8.35238763300006,11.6,6.74161543599999));
#246689=CARTESIAN_POINT('Ctrl Pts',(-8.35467843300006,15.2,6.74259969899998));
#246690=CARTESIAN_POINT('Ctrl Pts',(-8.35467843300006,11.6,6.74259969899998));
#246691=CARTESIAN_POINT('Ctrl Pts',(-8.35697574500006,15.2,6.74358441899999));
#246692=CARTESIAN_POINT('Ctrl Pts',(-8.35697574500006,11.6,6.74358441899999));
#246693=CARTESIAN_POINT('Ctrl Pts',(-8.35927956000006,15.2,6.74456958299999));
#246694=CARTESIAN_POINT('Ctrl Pts',(-8.35927956000006,11.6,6.74456958299999));
#246695=CARTESIAN_POINT('Ctrl Pts',(-8.36158987100006,15.2,6.74555517699999));
#246696=CARTESIAN_POINT('Ctrl Pts',(-8.36158987100006,11.6,6.74555517699999));
#246697=CARTESIAN_POINT('Ctrl Pts',(-8.36390667000006,15.2,6.74654118799998));
#246698=CARTESIAN_POINT('Ctrl Pts',(-8.36390667000006,11.6,6.74654118799998));
#246699=CARTESIAN_POINT('Ctrl Pts',(-8.36622995200005,15.2,6.74752760299998));
#246700=CARTESIAN_POINT('Ctrl Pts',(-8.36622995200005,11.6,6.74752760299998));
#246701=CARTESIAN_POINT('Ctrl Pts',(-8.36855970800006,15.2,6.74851440899998));
#246702=CARTESIAN_POINT('Ctrl Pts',(-8.36855970800006,11.6,6.74851440899998));
#246703=CARTESIAN_POINT('Ctrl Pts',(-8.37089593200006,15.2,6.74950159299998));
#246704=CARTESIAN_POINT('Ctrl Pts',(-8.37089593200006,11.6,6.74950159299998));
#246705=CARTESIAN_POINT('Ctrl Pts',(-8.37323861500006,15.2,6.75048914099998));
#246706=CARTESIAN_POINT('Ctrl Pts',(-8.37323861500006,11.6,6.75048914099998));
#246707=CARTESIAN_POINT('Ctrl Pts',(-8.37558775000005,15.2,6.75147704099999));
#246708=CARTESIAN_POINT('Ctrl Pts',(-8.37558775000005,11.6,6.75147704099999));
#246709=CARTESIAN_POINT('Ctrl Pts',(-8.37794333100006,15.2,6.75246527999998));
#246710=CARTESIAN_POINT('Ctrl Pts',(-8.37794333100006,11.6,6.75246527999998));
#246711=CARTESIAN_POINT('Ctrl Pts',(-8.38030535100006,15.2,6.75345384399999));
#246712=CARTESIAN_POINT('Ctrl Pts',(-8.38030535100006,11.6,6.75345384399999));
#246713=CARTESIAN_POINT('Ctrl Pts',(-8.38267379900006,15.2,6.75444272199999));
#246714=CARTESIAN_POINT('Ctrl Pts',(-8.38267379900006,11.6,6.75444272199999));
#246715=CARTESIAN_POINT('Ctrl Pts',(-8.38504867400006,15.2,6.75543189999999));
#246716=CARTESIAN_POINT('Ctrl Pts',(-8.38504867400006,11.6,6.75543189999999));
#246717=CARTESIAN_POINT('Ctrl Pts',(-8.38742996300006,15.2,6.75642136499999));
#246718=CARTESIAN_POINT('Ctrl Pts',(-8.38742996300006,11.6,6.75642136499999));
#246719=CARTESIAN_POINT('Ctrl Pts',(-8.38981766300006,15.2,6.75741110399999));
#246720=CARTESIAN_POINT('Ctrl Pts',(-8.38981766300006,11.6,6.75741110399999));
#246721=CARTESIAN_POINT('Ctrl Pts',(-8.39221176300006,15.2,6.75840110599999));
#246722=CARTESIAN_POINT('Ctrl Pts',(-8.39221176300006,11.6,6.75840110599999));
#246723=CARTESIAN_POINT('Ctrl Pts',(-8.39461225900006,15.2,6.75939135599998));
#246724=CARTESIAN_POINT('Ctrl Pts',(-8.39461225900006,11.6,6.75939135599998));
#246725=CARTESIAN_POINT('Ctrl Pts',(-8.39701914300005,15.2,6.76038184399999));
#246726=CARTESIAN_POINT('Ctrl Pts',(-8.39701914300005,11.6,6.76038184399999));
#246727=CARTESIAN_POINT('Ctrl Pts',(-8.39943240800006,15.2,6.76137255499999));
#246728=CARTESIAN_POINT('Ctrl Pts',(-8.39943240800006,11.6,6.76137255499999));
#246729=CARTESIAN_POINT('Ctrl Pts',(-8.40185204500006,15.2,6.76236347699999));
#246730=CARTESIAN_POINT('Ctrl Pts',(-8.40185204500006,11.6,6.76236347699999));
#246731=CARTESIAN_POINT('Ctrl Pts',(-8.40427804900006,15.2,6.76335459899998));
#246732=CARTESIAN_POINT('Ctrl Pts',(-8.40427804900006,11.6,6.76335459899998));
#246733=CARTESIAN_POINT('Ctrl Pts',(-8.40671041200006,15.2,6.76434590699999));
#246734=CARTESIAN_POINT('Ctrl Pts',(-8.40671041200006,11.6,6.76434590699999));
#246735=CARTESIAN_POINT('Ctrl Pts',(-8.40914912700006,15.2,6.76533738899998));
#246736=CARTESIAN_POINT('Ctrl Pts',(-8.40914912700006,11.6,6.76533738899998));
#246737=CARTESIAN_POINT('Ctrl Pts',(-8.41159418600006,15.2,6.76632903299998));
#246738=CARTESIAN_POINT('Ctrl Pts',(-8.41159418600006,11.6,6.76632903299998));
#246739=CARTESIAN_POINT('Ctrl Pts',(-8.41404558400006,15.2,6.76732082599998));
#246740=CARTESIAN_POINT('Ctrl Pts',(-8.41404558400006,11.6,6.76732082599998));
#246741=CARTESIAN_POINT('Ctrl Pts',(-8.41650331200006,15.2,6.76831275599999));
#246742=CARTESIAN_POINT('Ctrl Pts',(-8.41650331200006,11.6,6.76831275599999));
#246743=CARTESIAN_POINT('Ctrl Pts',(-8.41896736400006,15.2,6.76930480999999));
#246744=CARTESIAN_POINT('Ctrl Pts',(-8.41896736400006,11.6,6.76930480999999));
#246745=CARTESIAN_POINT('Ctrl Pts',(-8.42143773200006,15.2,6.77029697699999));
#246746=CARTESIAN_POINT('Ctrl Pts',(-8.42143773200006,11.6,6.77029697699999));
#246747=CARTESIAN_POINT('Ctrl Pts',(-8.42391441000006,15.2,6.77128924499999));
#246748=CARTESIAN_POINT('Ctrl Pts',(-8.42391441000006,11.6,6.77128924499999));
#246749=CARTESIAN_POINT('Ctrl Pts',(-8.42639739000006,15.2,6.77228159899999));
#246750=CARTESIAN_POINT('Ctrl Pts',(-8.42639739000006,11.6,6.77228159899999));
#246751=CARTESIAN_POINT('Ctrl Pts',(-8.42888666600006,15.2,6.77327402999998));
#246752=CARTESIAN_POINT('Ctrl Pts',(-8.42888666600006,11.6,6.77327402999998));
#246753=CARTESIAN_POINT('Ctrl Pts',(-8.43138223000006,15.2,6.77426652399999));
#246754=CARTESIAN_POINT('Ctrl Pts',(-8.43138223000006,11.6,6.77426652399999));
#246755=CARTESIAN_POINT('Ctrl Pts',(-8.43388407600006,15.2,6.77525906999998));
#246756=CARTESIAN_POINT('Ctrl Pts',(-8.43388407600006,11.6,6.77525906999998));
#246757=CARTESIAN_POINT('Ctrl Pts',(-8.43639219500006,15.2,6.77625165599999));
#246758=CARTESIAN_POINT('Ctrl Pts',(-8.43639219500006,11.6,6.77625165599999));
#246759=CARTESIAN_POINT('Ctrl Pts',(-8.43890658200005,15.2,6.77724426899999));
#246760=CARTESIAN_POINT('Ctrl Pts',(-8.43890658200005,11.6,6.77724426899999));
#246761=CARTESIAN_POINT('Ctrl Pts',(-8.44142722800006,15.2,6.77823689799999));
#246762=CARTESIAN_POINT('Ctrl Pts',(-8.44142722800006,11.6,6.77823689799999));
#246763=CARTESIAN_POINT('Ctrl Pts',(-8.44395412900005,15.2,6.77922952999998));
#246764=CARTESIAN_POINT('Ctrl Pts',(-8.44395412900005,11.6,6.77922952999998));
#246765=CARTESIAN_POINT('Ctrl Pts',(-8.44648727500006,15.2,6.78022215499999));
#246766=CARTESIAN_POINT('Ctrl Pts',(-8.44648727500006,11.6,6.78022215499999));
#246767=CARTESIAN_POINT('Ctrl Pts',(-8.44902666200005,15.2,6.78121475899999));
#246768=CARTESIAN_POINT('Ctrl Pts',(-8.44902666200005,11.6,6.78121475899999));
#246769=CARTESIAN_POINT('Ctrl Pts',(-8.45157228000006,15.2,6.78220733099998));
#246770=CARTESIAN_POINT('Ctrl Pts',(-8.45157228000006,11.6,6.78220733099998));
#246771=CARTESIAN_POINT('Ctrl Pts',(-8.45412412400006,15.2,6.78319985899999));
#246772=CARTESIAN_POINT('Ctrl Pts',(-8.45412412400006,11.6,6.78319985899999));
#246773=CARTESIAN_POINT('Ctrl Pts',(-8.45668218700006,15.2,6.78419233299999));
#246774=CARTESIAN_POINT('Ctrl Pts',(-8.45668218700006,11.6,6.78419233299999));
#246775=CARTESIAN_POINT('Ctrl Pts',(-8.45924646000006,15.2,6.78518473899998));
#246776=CARTESIAN_POINT('Ctrl Pts',(-8.45924646000006,11.6,6.78518473899998));
#246777=CARTESIAN_POINT('Ctrl Pts',(-8.46181693900006,15.2,6.78617706599999));
#246778=CARTESIAN_POINT('Ctrl Pts',(-8.46181693900006,11.6,6.78617706599999));
#246779=CARTESIAN_POINT('Ctrl Pts',(-8.46439361500006,15.2,6.78716930199998));
#246780=CARTESIAN_POINT('Ctrl Pts',(-8.46439361500006,11.6,6.78716930199998));
#246781=CARTESIAN_POINT('Ctrl Pts',(-8.46697648200006,15.2,6.78816143599998));
#246782=CARTESIAN_POINT('Ctrl Pts',(-8.46697648200006,11.6,6.78816143599998));
#246783=CARTESIAN_POINT('Ctrl Pts',(-8.46956553300006,15.2,6.78915345699998));
#246784=CARTESIAN_POINT('Ctrl Pts',(-8.46956553300006,11.6,6.78915345699998));
#246785=CARTESIAN_POINT('Ctrl Pts',(-8.47216076100005,15.2,6.79014535399999));
#246786=CARTESIAN_POINT('Ctrl Pts',(-8.47216076100005,11.6,6.79014535399999));
#246787=CARTESIAN_POINT('Ctrl Pts',(-8.47476215800006,15.2,6.79113711099999));
#246788=CARTESIAN_POINT('Ctrl Pts',(-8.47476215800006,11.6,6.79113711099999));
#246789=CARTESIAN_POINT('Ctrl Pts',(-8.47736972000006,15.2,6.79212872199999));
#246790=CARTESIAN_POINT('Ctrl Pts',(-8.47736972000006,11.6,6.79212872199999));
#246791=CARTESIAN_POINT('Ctrl Pts',(-8.47998343700005,15.2,6.79312017299999));
#246792=CARTESIAN_POINT('Ctrl Pts',(-8.47998343700005,11.6,6.79312017299999));
#246793=CARTESIAN_POINT('Ctrl Pts',(-8.48260330400005,15.2,6.79411145299999));
#246794=CARTESIAN_POINT('Ctrl Pts',(-8.48260330400005,11.6,6.79411145299999));
#246795=CARTESIAN_POINT('Ctrl Pts',(-8.48522931400005,15.2,6.79510254999999));
#246796=CARTESIAN_POINT('Ctrl Pts',(-8.48522931400005,11.6,6.79510254999999));
#246797=CARTESIAN_POINT('Ctrl Pts',(-8.48786146000006,15.2,6.79609345399999));
#246798=CARTESIAN_POINT('Ctrl Pts',(-8.48786146000006,11.6,6.79609345399999));
#246799=CARTESIAN_POINT('Ctrl Pts',(-8.49049973400006,15.2,6.79708415199999));
#246800=CARTESIAN_POINT('Ctrl Pts',(-8.49049973400006,11.6,6.79708415199999));
#246801=CARTESIAN_POINT('Ctrl Pts',(-8.49314413000006,15.2,6.79807463399998));
#246802=CARTESIAN_POINT('Ctrl Pts',(-8.49314413000006,11.6,6.79807463399998));
#246803=CARTESIAN_POINT('Ctrl Pts',(-8.49579464300006,15.2,6.79906488799999));
#246804=CARTESIAN_POINT('Ctrl Pts',(-8.49579464300006,11.6,6.79906488799999));
#246805=CARTESIAN_POINT('Ctrl Pts',(-8.49845126200006,15.2,6.80005490199999));
#246806=CARTESIAN_POINT('Ctrl Pts',(-8.49845126200006,11.6,6.80005490199999));
#246807=CARTESIAN_POINT('Ctrl Pts',(-8.50111398500006,15.2,6.80104466699999));
#246808=CARTESIAN_POINT('Ctrl Pts',(-8.50111398500006,11.6,6.80104466699999));
#246809=CARTESIAN_POINT('Ctrl Pts',(-8.50378280200006,15.2,6.80203417099998));
#246810=CARTESIAN_POINT('Ctrl Pts',(-8.50378280200006,11.6,6.80203417099998));
#246811=CARTESIAN_POINT('Ctrl Pts',(-8.50645770800006,15.2,6.80302340199999));
#246812=CARTESIAN_POINT('Ctrl Pts',(-8.50645770800006,11.6,6.80302340199999));
#246813=CARTESIAN_POINT('Ctrl Pts',(-8.50913869400006,15.2,6.80401234999999));
#246814=CARTESIAN_POINT('Ctrl Pts',(-8.50913869400006,11.6,6.80401234999999));
#246815=CARTESIAN_POINT('Ctrl Pts',(-8.51182575500006,15.2,6.80500100299999));
#246816=CARTESIAN_POINT('Ctrl Pts',(-8.51182575500006,11.6,6.80500100299999));
#246817=CARTESIAN_POINT('Ctrl Pts',(-8.51451888400005,15.2,6.80598934999999));
#246818=CARTESIAN_POINT('Ctrl Pts',(-8.51451888400005,11.6,6.80598934999999));
#246819=CARTESIAN_POINT('Ctrl Pts',(-8.51721807400006,15.2,6.80697738099998));
#246820=CARTESIAN_POINT('Ctrl Pts',(-8.51721807400006,11.6,6.80697738099998));
#246821=CARTESIAN_POINT('Ctrl Pts',(-8.51992331900006,15.2,6.80796508499999));
#246822=CARTESIAN_POINT('Ctrl Pts',(-8.51992331900006,11.6,6.80796508499999));
#246823=CARTESIAN_POINT('Ctrl Pts',(-8.52263461100006,15.2,6.80895244999999));
#246824=CARTESIAN_POINT('Ctrl Pts',(-8.52263461100006,11.6,6.80895244999999));
#246825=CARTESIAN_POINT('Ctrl Pts',(-8.52535194400006,15.2,6.80993946599998));
#246826=CARTESIAN_POINT('Ctrl Pts',(-8.52535194400006,11.6,6.80993946599998));
#246827=CARTESIAN_POINT('Ctrl Pts',(-8.52807531100006,15.2,6.81092612099999));
#246828=CARTESIAN_POINT('Ctrl Pts',(-8.52807531100006,11.6,6.81092612099999));
#246829=CARTESIAN_POINT('Ctrl Pts',(-8.53080470500006,15.2,6.81191240399999));
#246830=CARTESIAN_POINT('Ctrl Pts',(-8.53080470500006,11.6,6.81191240399999));
#246831=CARTESIAN_POINT('Ctrl Pts',(-8.53354012000005,15.2,6.81289830599999));
#246832=CARTESIAN_POINT('Ctrl Pts',(-8.53354012000005,11.6,6.81289830599999));
#246833=CARTESIAN_POINT('Ctrl Pts',(-8.53628154900005,15.2,6.81388381599999));
#246834=CARTESIAN_POINT('Ctrl Pts',(-8.53628154900005,11.6,6.81388381599999));
#246835=CARTESIAN_POINT('Ctrl Pts',(-8.53902898600005,15.2,6.81486892199998));
#246836=CARTESIAN_POINT('Ctrl Pts',(-8.53902898600005,11.6,6.81486892199998));
#246837=CARTESIAN_POINT('Ctrl Pts',(-8.54178242300006,15.2,6.81585361399998));
#246838=CARTESIAN_POINT('Ctrl Pts',(-8.54178242300006,11.6,6.81585361399998));
#246839=CARTESIAN_POINT('Ctrl Pts',(-8.54454185400006,15.2,6.81683788099999));
#246840=CARTESIAN_POINT('Ctrl Pts',(-8.54454185400006,11.6,6.81683788099999));
#246841=CARTESIAN_POINT('Ctrl Pts',(-8.54730727200005,15.2,6.81782171199998));
#246842=CARTESIAN_POINT('Ctrl Pts',(-8.54730727200005,11.6,6.81782171199998));
#246843=CARTESIAN_POINT('Ctrl Pts',(-8.55007867000005,15.2,6.81880509699998));
#246844=CARTESIAN_POINT('Ctrl Pts',(-8.55007867000005,11.6,6.81880509699998));
#246845=CARTESIAN_POINT('Ctrl Pts',(-8.55285604400006,15.2,6.81978802599998));
#246846=CARTESIAN_POINT('Ctrl Pts',(-8.55285604400006,11.6,6.81978802599998));
#246847=CARTESIAN_POINT('Ctrl Pts',(-8.55563938300006,15.2,6.82077048699998));
#246848=CARTESIAN_POINT('Ctrl Pts',(-8.55563938300006,11.6,6.82077048699998));
#246849=CARTESIAN_POINT('Ctrl Pts',(-8.55842868500006,15.2,6.82175246999999));
#246850=CARTESIAN_POINT('Ctrl Pts',(-8.55842868500006,11.6,6.82175246999999));
#246851=CARTESIAN_POINT('Ctrl Pts',(-8.56122393900005,15.2,6.82273396399999));
#246852=CARTESIAN_POINT('Ctrl Pts',(-8.56122393900005,11.6,6.82273396399999));
#246853=CARTESIAN_POINT('Ctrl Pts',(-8.56402514200006,15.2,6.82371496099999));
#246854=CARTESIAN_POINT('Ctrl Pts',(-8.56402514200006,11.6,6.82371496099999));
#246855=CARTESIAN_POINT('Ctrl Pts',(-8.56683228400006,15.2,6.82469544699998));
#246856=CARTESIAN_POINT('Ctrl Pts',(-8.56683228400006,11.6,6.82469544699998));
#246857=CARTESIAN_POINT('Ctrl Pts',(-8.56964536200006,15.2,6.82567541399998));
#246858=CARTESIAN_POINT('Ctrl Pts',(-8.56964536200006,11.6,6.82567541399998));
#246859=CARTESIAN_POINT('Ctrl Pts',(-8.57246436700006,15.2,6.82665484999998));
#246860=CARTESIAN_POINT('Ctrl Pts',(-8.57246436700006,11.6,6.82665484999998));
#246861=CARTESIAN_POINT('Ctrl Pts',(-8.57528929200006,15.2,6.82763374599999));
#246862=CARTESIAN_POINT('Ctrl Pts',(-8.57528929200006,11.6,6.82763374599999));
#246863=CARTESIAN_POINT('Ctrl Pts',(-8.57812013200006,15.2,6.82861209099999));
#246864=CARTESIAN_POINT('Ctrl Pts',(-8.57812013200006,11.6,6.82861209099999));
#246865=CARTESIAN_POINT('Ctrl Pts',(-8.58095688000006,15.2,6.82958987499998));
#246866=CARTESIAN_POINT('Ctrl Pts',(-8.58095688000006,11.6,6.82958987499998));
#246867=CARTESIAN_POINT('Ctrl Pts',(-8.58379953000006,15.2,6.83056708799998));
#246868=CARTESIAN_POINT('Ctrl Pts',(-8.58379953000006,11.6,6.83056708799998));
#246869=CARTESIAN_POINT('Ctrl Pts',(-8.58664807300006,15.2,6.83154371699998));
#246870=CARTESIAN_POINT('Ctrl Pts',(-8.58664807300006,11.6,6.83154371699998));
#246871=CARTESIAN_POINT('Ctrl Pts',(-8.58950250400006,15.2,6.83251975699999));
#246872=CARTESIAN_POINT('Ctrl Pts',(-8.58950250400006,11.6,6.83251975699999));
#246873=CARTESIAN_POINT('Ctrl Pts',(-8.59236281800005,15.2,6.83349519299998));
#246874=CARTESIAN_POINT('Ctrl Pts',(-8.59236281800005,11.6,6.83349519299998));
#246875=CARTESIAN_POINT('Ctrl Pts',(-8.59522900700006,15.2,6.83447001699999));
#246876=CARTESIAN_POINT('Ctrl Pts',(-8.59522900700006,11.6,6.83447001699999));
#246877=CARTESIAN_POINT('Ctrl Pts',(-8.59810106400005,15.2,6.83544421899998));
#246878=CARTESIAN_POINT('Ctrl Pts',(-8.59810106400005,11.6,6.83544421899998));
#246879=CARTESIAN_POINT('Ctrl Pts',(-8.60097898200006,15.2,6.83641778699998));
#246880=CARTESIAN_POINT('Ctrl Pts',(-8.60097898200006,11.6,6.83641778699998));
#246881=CARTESIAN_POINT('Ctrl Pts',(-8.60386275600005,15.2,6.83739071399999));
#246882=CARTESIAN_POINT('Ctrl Pts',(-8.60386275600005,11.6,6.83739071399999));
#246883=CARTESIAN_POINT('Ctrl Pts',(-8.60675237900006,15.2,6.83836298699998));
#246884=CARTESIAN_POINT('Ctrl Pts',(-8.60675237900006,11.6,6.83836298699998));
#246885=CARTESIAN_POINT('Ctrl Pts',(-8.60964784400006,15.2,6.83933459799999));
#246886=CARTESIAN_POINT('Ctrl Pts',(-8.60964784400006,11.6,6.83933459799999));
#246887=CARTESIAN_POINT('Ctrl Pts',(-8.61254914500006,15.2,6.84030553499999));
#246888=CARTESIAN_POINT('Ctrl Pts',(-8.61254914500006,11.6,6.84030553499999));
#246889=CARTESIAN_POINT('Ctrl Pts',(-8.61545627500006,15.2,6.84127579099999));
#246890=CARTESIAN_POINT('Ctrl Pts',(-8.61545627500006,11.6,6.84127579099999));
#246891=CARTESIAN_POINT('Ctrl Pts',(-8.61836922900006,15.2,6.84224535299998));
#246892=CARTESIAN_POINT('Ctrl Pts',(-8.61836922900006,11.6,6.84224535299998));
#246893=CARTESIAN_POINT('Ctrl Pts',(-8.62128799900006,15.2,6.84321421299998));
#246894=CARTESIAN_POINT('Ctrl Pts',(-8.62128799900006,11.6,6.84321421299998));
#246895=CARTESIAN_POINT('Ctrl Pts',(-8.62421257700005,15.2,6.84418235999999));
#246896=CARTESIAN_POINT('Ctrl Pts',(-8.62421257700005,11.6,6.84418235999999));
#246897=CARTESIAN_POINT('Ctrl Pts',(-8.62714296000006,15.2,6.84514978399999));
#246898=CARTESIAN_POINT('Ctrl Pts',(-8.62714296000006,11.6,6.84514978399999));
#246899=CARTESIAN_POINT('Ctrl Pts',(-8.63007914000006,15.2,6.84611647699998));
#246900=CARTESIAN_POINT('Ctrl Pts',(-8.63007914000006,11.6,6.84611647699998));
#246901=CARTESIAN_POINT('Ctrl Pts',(-8.63302111000005,15.2,6.84708242699998));
#246902=CARTESIAN_POINT('Ctrl Pts',(-8.63302111000005,11.6,6.84708242699998));
#246903=CARTESIAN_POINT('Ctrl Pts',(-8.63596886400006,15.2,6.84804762499999));
#246904=CARTESIAN_POINT('Ctrl Pts',(-8.63596886400006,11.6,6.84804762499999));
#246905=CARTESIAN_POINT('Ctrl Pts',(-8.63892239600006,15.2,6.84901206199999));
#246906=CARTESIAN_POINT('Ctrl Pts',(-8.63892239600006,11.6,6.84901206199999));
#246907=CARTESIAN_POINT('Ctrl Pts',(-8.64188169900006,15.2,6.84997572699999));
#246908=CARTESIAN_POINT('Ctrl Pts',(-8.64188169900006,11.6,6.84997572699999));
#246909=CARTESIAN_POINT('Ctrl Pts',(-8.64484676600006,15.2,6.85093861099999));
#246910=CARTESIAN_POINT('Ctrl Pts',(-8.64484676600006,11.6,6.85093861099999));
#246911=CARTESIAN_POINT('Ctrl Pts',(-8.64781759100006,15.2,6.85190070499999));
#246912=CARTESIAN_POINT('Ctrl Pts',(-8.64781759100006,11.6,6.85190070499999));
#246913=CARTESIAN_POINT('Ctrl Pts',(-8.65079416900006,15.2,6.85286199699998));
#246914=CARTESIAN_POINT('Ctrl Pts',(-8.65079416900006,11.6,6.85286199699998));
#246915=CARTESIAN_POINT('Ctrl Pts',(-8.65377649100006,15.2,6.85382247999998));
#246916=CARTESIAN_POINT('Ctrl Pts',(-8.65377649100006,11.6,6.85382247999998));
#246917=CARTESIAN_POINT('Ctrl Pts',(-8.65676455400006,15.2,6.85478214199998));
#246918=CARTESIAN_POINT('Ctrl Pts',(-8.65676455400006,11.6,6.85478214199998));
#246919=CARTESIAN_POINT('Ctrl Pts',(-8.65975834800006,15.2,6.85574097599999));
#246920=CARTESIAN_POINT('Ctrl Pts',(-8.65975834800006,11.6,6.85574097599999));
#246921=CARTESIAN_POINT('Ctrl Pts',(-8.66275786800006,15.2,6.85669897099999));
#246922=CARTESIAN_POINT('Ctrl Pts',(-8.66275786800006,11.6,6.85669897099999));
#246923=CARTESIAN_POINT('Ctrl Pts',(-8.66576310800006,15.2,6.85765611699999));
#246924=CARTESIAN_POINT('Ctrl Pts',(-8.66576310800006,11.6,6.85765611699999));
#246925=CARTESIAN_POINT('Ctrl Pts',(-8.66877406100006,15.2,6.85861240499998));
#246926=CARTESIAN_POINT('Ctrl Pts',(-8.66877406100006,11.6,6.85861240499998));
#246927=CARTESIAN_POINT('Ctrl Pts',(-8.67179072300006,15.2,6.85956782599998));
#246928=CARTESIAN_POINT('Ctrl Pts',(-8.67179072300006,11.6,6.85956782599998));
#246929=CARTESIAN_POINT('Ctrl Pts',(-8.67481308300006,15.2,6.86052236899998));
#246930=CARTESIAN_POINT('Ctrl Pts',(-8.67481308300006,11.6,6.86052236899998));
#246931=CARTESIAN_POINT('Ctrl Pts',(-8.67784113900005,15.2,6.86147602699998));
#246932=CARTESIAN_POINT('Ctrl Pts',(-8.67784113900005,11.6,6.86147602699998));
#246933=CARTESIAN_POINT('Ctrl Pts',(-8.68087488300005,15.2,6.86242878899999));
#246934=CARTESIAN_POINT('Ctrl Pts',(-8.68087488300005,11.6,6.86242878899999));
#246935=CARTESIAN_POINT('Ctrl Pts',(-8.68391430700006,15.2,6.86338064599998));
#246936=CARTESIAN_POINT('Ctrl Pts',(-8.68391430700006,11.6,6.86338064599998));
#246937=CARTESIAN_POINT('Ctrl Pts',(-8.68695940700006,15.2,6.86433158899998));
#246938=CARTESIAN_POINT('Ctrl Pts',(-8.68695940700006,11.6,6.86433158899998));
#246939=CARTESIAN_POINT('Ctrl Pts',(-8.69001017600005,15.2,6.86528160699999));
#246940=CARTESIAN_POINT('Ctrl Pts',(-8.69001017600005,11.6,6.86528160699999));
#246941=CARTESIAN_POINT('Ctrl Pts',(-8.69306660800006,15.2,6.86623069199998));
#246942=CARTESIAN_POINT('Ctrl Pts',(-8.69306660800006,11.6,6.86623069199998));
#246943=CARTESIAN_POINT('Ctrl Pts',(-8.69612869600006,15.2,6.86717883599999));
#246944=CARTESIAN_POINT('Ctrl Pts',(-8.69612869600006,11.6,6.86717883599999));
#246945=CARTESIAN_POINT('Ctrl Pts',(-8.69919643300006,15.2,6.86812602599999));
#246946=CARTESIAN_POINT('Ctrl Pts',(-8.69919643300006,11.6,6.86812602599999));
#246947=CARTESIAN_POINT('Ctrl Pts',(-8.70226981400006,15.2,6.86907225699999));
#246948=CARTESIAN_POINT('Ctrl Pts',(-8.70226981400006,11.6,6.86907225699999));
#246949=CARTESIAN_POINT('Ctrl Pts',(-8.70534883200006,15.2,6.87001751699999));
#246950=CARTESIAN_POINT('Ctrl Pts',(-8.70534883200006,11.6,6.87001751699999));
#246951=CARTESIAN_POINT('Ctrl Pts',(-8.70843348100006,15.2,6.87096179799998));
#246952=CARTESIAN_POINT('Ctrl Pts',(-8.70843348100006,11.6,6.87096179799998));
#246953=CARTESIAN_POINT('Ctrl Pts',(-8.71152375500006,15.2,6.87190509099998));
#246954=CARTESIAN_POINT('Ctrl Pts',(-8.71152375500006,11.6,6.87190509099998));
#246955=CARTESIAN_POINT('Ctrl Pts',(-8.71461964700006,15.2,6.87284738499999));
#246956=CARTESIAN_POINT('Ctrl Pts',(-8.71461964700006,11.6,6.87284738499999));
#246957=CARTESIAN_POINT('Ctrl Pts',(-8.71772115100006,15.2,6.87378867299999));
#246958=CARTESIAN_POINT('Ctrl Pts',(-8.71772115100006,11.6,6.87378867299999));
#246959=CARTESIAN_POINT('Ctrl Pts',(-8.72082826000005,15.2,6.87472894499999));
#246960=CARTESIAN_POINT('Ctrl Pts',(-8.72082826000005,11.6,6.87472894499999));
#246961=CARTESIAN_POINT('Ctrl Pts',(-8.72394096900006,15.2,6.87566819299998));
#246962=CARTESIAN_POINT('Ctrl Pts',(-8.72394096900006,11.6,6.87566819299998));
#246963=CARTESIAN_POINT('Ctrl Pts',(-8.72705927100006,15.2,6.87660640599999));
#246964=CARTESIAN_POINT('Ctrl Pts',(-8.72705927100006,11.6,6.87660640599999));
#246965=CARTESIAN_POINT('Ctrl Pts',(-8.73018316100006,15.2,6.87754357599999));
#246966=CARTESIAN_POINT('Ctrl Pts',(-8.73018316100006,11.6,6.87754357599999));
#246967=CARTESIAN_POINT('Ctrl Pts',(-8.73331263100006,15.2,6.87847969399999));
#246968=CARTESIAN_POINT('Ctrl Pts',(-8.73331263100006,11.6,6.87847969399999));
#246969=CARTESIAN_POINT('Ctrl Pts',(-8.73644767400006,15.2,6.87941475199998));
#246970=CARTESIAN_POINT('Ctrl Pts',(-8.73644767400006,11.6,6.87941475199998));
#246971=CARTESIAN_POINT('Ctrl Pts',(-8.73958828700006,15.2,6.88034873899999));
#246972=CARTESIAN_POINT('Ctrl Pts',(-8.73958828700006,11.6,6.88034873899999));
#246973=CARTESIAN_POINT('Ctrl Pts',(-8.74273446100006,15.2,6.88128164799998));
#246974=CARTESIAN_POINT('Ctrl Pts',(-8.74273446100006,11.6,6.88128164799998));
#246975=CARTESIAN_POINT('Ctrl Pts',(-8.74588619100006,15.2,6.88221346799998));
#246976=CARTESIAN_POINT('Ctrl Pts',(-8.74588619100006,11.6,6.88221346799998));
#246977=CARTESIAN_POINT('Ctrl Pts',(-8.74904346900006,15.2,6.88314419199998));
#246978=CARTESIAN_POINT('Ctrl Pts',(-8.74904346900006,11.6,6.88314419199998));
#246979=CARTESIAN_POINT('Ctrl Pts',(-8.75220629200006,15.2,6.88407381099999));
#246980=CARTESIAN_POINT('Ctrl Pts',(-8.75220629200006,11.6,6.88407381099999));
#246981=CARTESIAN_POINT('Ctrl Pts',(-8.75537465200006,15.2,6.88500231499999));
#246982=CARTESIAN_POINT('Ctrl Pts',(-8.75537465200006,11.6,6.88500231499999));
#246983=CARTESIAN_POINT('Ctrl Pts',(-8.75854854200006,15.2,6.88592969499998));
#246984=CARTESIAN_POINT('Ctrl Pts',(-8.75854854200006,11.6,6.88592969499998));
#246985=CARTESIAN_POINT('Ctrl Pts',(-8.76172795600005,15.2,6.88685594399999));
#246986=CARTESIAN_POINT('Ctrl Pts',(-8.76172795600005,11.6,6.88685594399999));
#246987=CARTESIAN_POINT('Ctrl Pts',(-8.76491288800005,15.2,6.88778105199999));
#246988=CARTESIAN_POINT('Ctrl Pts',(-8.76491288800005,11.6,6.88778105199999));
#246989=CARTESIAN_POINT('Ctrl Pts',(-8.76810333300006,15.2,6.88870501099998));
#246990=CARTESIAN_POINT('Ctrl Pts',(-8.76810333300006,11.6,6.88870501099998));
#246991=CARTESIAN_POINT('Ctrl Pts',(-8.77129928400005,15.2,6.88962781099999));
#246992=CARTESIAN_POINT('Ctrl Pts',(-8.77129928400005,11.6,6.88962781099999));
#246993=CARTESIAN_POINT('Ctrl Pts',(-8.77450073400006,15.2,6.89054944399999));
#246994=CARTESIAN_POINT('Ctrl Pts',(-8.77450073400006,11.6,6.89054944399999));
#246995=CARTESIAN_POINT('Ctrl Pts',(-8.77770767800006,15.2,6.89146990199998));
#246996=CARTESIAN_POINT('Ctrl Pts',(-8.77770767800006,11.6,6.89146990199998));
#246997=CARTESIAN_POINT('Ctrl Pts',(-8.78092011000006,15.2,6.89238917599998));
#246998=CARTESIAN_POINT('Ctrl Pts',(-8.78092011000006,11.6,6.89238917599998));
#246999=CARTESIAN_POINT('Ctrl Pts',(-8.78413802200006,15.2,6.89330725599999));
#247000=CARTESIAN_POINT('Ctrl Pts',(-8.78413802200006,11.6,6.89330725599999));
#247001=CARTESIAN_POINT('Ctrl Pts',(-8.78736140900006,15.2,6.89422413499998));
#247002=CARTESIAN_POINT('Ctrl Pts',(-8.78736140900006,11.6,6.89422413499998));
#247003=CARTESIAN_POINT('Ctrl Pts',(-8.79059026600006,15.2,6.89513980399998));
#247004=CARTESIAN_POINT('Ctrl Pts',(-8.79059026600006,11.6,6.89513980399998));
#247005=CARTESIAN_POINT('Ctrl Pts',(-8.79382458400006,15.2,6.89605425399999));
#247006=CARTESIAN_POINT('Ctrl Pts',(-8.79382458400006,11.6,6.89605425399999));
#247007=CARTESIAN_POINT('Ctrl Pts',(-8.79706435900006,15.2,6.89696747699998));
#247008=CARTESIAN_POINT('Ctrl Pts',(-8.79706435900006,11.6,6.89696747699998));
#247009=CARTESIAN_POINT('Ctrl Pts',(-8.80030958500006,15.2,6.89787946299998));
#247010=CARTESIAN_POINT('Ctrl Pts',(-8.80030958500006,11.6,6.89787946299998));
#247011=CARTESIAN_POINT('Ctrl Pts',(-8.80356025500006,15.2,6.89879020499998));
#247012=CARTESIAN_POINT('Ctrl Pts',(-8.80356025500006,11.6,6.89879020499998));
#247013=CARTESIAN_POINT('Ctrl Pts',(-8.80681636300006,15.2,6.89969969599999));
#247014=CARTESIAN_POINT('Ctrl Pts',(-8.80681636300006,11.6,6.89969969599999));
#247015=CARTESIAN_POINT('Ctrl Pts',(-8.81007790200006,15.2,6.90060792399999));
#247016=CARTESIAN_POINT('Ctrl Pts',(-8.81007790200006,11.6,6.90060792399999));
#247017=CARTESIAN_POINT('Ctrl Pts',(-8.81334486800006,15.2,6.90151488299998));
#247018=CARTESIAN_POINT('Ctrl Pts',(-8.81334486800006,11.6,6.90151488299998));
#247019=CARTESIAN_POINT('Ctrl Pts',(-8.81661725300006,15.2,6.90242056299999));
#247020=CARTESIAN_POINT('Ctrl Pts',(-8.81661725300006,11.6,6.90242056299999));
#247021=CARTESIAN_POINT('Ctrl Pts',(-8.81989505200006,15.2,6.90332495799999));
#247022=CARTESIAN_POINT('Ctrl Pts',(-8.81989505200006,11.6,6.90332495799999));
#247023=CARTESIAN_POINT('Ctrl Pts',(-8.82317825900006,15.2,6.90422805599999));
#247024=CARTESIAN_POINT('Ctrl Pts',(-8.82317825900006,11.6,6.90422805599999));
#247025=CARTESIAN_POINT('Ctrl Pts',(-8.82646686600006,15.2,6.90512985099998));
#247026=CARTESIAN_POINT('Ctrl Pts',(-8.82646686600006,11.6,6.90512985099998));
#247027=CARTESIAN_POINT('Ctrl Pts',(-8.82976086800005,15.2,6.90603033599999));
#247028=CARTESIAN_POINT('Ctrl Pts',(-8.82976086800005,11.6,6.90603033599999));
#247029=CARTESIAN_POINT('Ctrl Pts',(-8.83306026000006,15.2,6.90692949999999));
#247030=CARTESIAN_POINT('Ctrl Pts',(-8.83306026000006,11.6,6.90692949999999));
#247031=CARTESIAN_POINT('Ctrl Pts',(-8.83636503500006,15.2,6.90782733499999));
#247032=CARTESIAN_POINT('Ctrl Pts',(-8.83636503500006,11.6,6.90782733499999));
#247033=CARTESIAN_POINT('Ctrl Pts',(-8.83967518800005,15.2,6.90872383499999));
#247034=CARTESIAN_POINT('Ctrl Pts',(-8.83967518800005,11.6,6.90872383499999));
#247035=CARTESIAN_POINT('Ctrl Pts',(-8.84299071000006,15.2,6.90961898899998));
#247036=CARTESIAN_POINT('Ctrl Pts',(-8.84299071000006,11.6,6.90961898899998));
#247037=CARTESIAN_POINT('Ctrl Pts',(-8.84631159700006,15.2,6.91051278999999));
#247038=CARTESIAN_POINT('Ctrl Pts',(-8.84631159700006,11.6,6.91051278999999));
#247039=CARTESIAN_POINT('Ctrl Pts',(-8.84963784400006,15.2,6.91140523099998));
#247040=CARTESIAN_POINT('Ctrl Pts',(-8.84963784400006,11.6,6.91140523099998));
#247041=CARTESIAN_POINT('Ctrl Pts',(-8.85296944200006,15.2,6.91229630099999));
#247042=CARTESIAN_POINT('Ctrl Pts',(-8.85296944200006,11.6,6.91229630099999));
#247043=CARTESIAN_POINT('Ctrl Pts',(-8.85630638700006,15.2,6.91318599399998));
#247044=CARTESIAN_POINT('Ctrl Pts',(-8.85630638700006,11.6,6.91318599399998));
#247045=CARTESIAN_POINT('Ctrl Pts',(-8.85964867400006,15.2,6.91407430099999));
#247046=CARTESIAN_POINT('Ctrl Pts',(-8.85964867400006,11.6,6.91407430099999));
#247047=CARTESIAN_POINT('Ctrl Pts',(-8.86299629400006,15.2,6.91496121399998));
#247048=CARTESIAN_POINT('Ctrl Pts',(-8.86299629400006,11.6,6.91496121399998));
#247049=CARTESIAN_POINT('Ctrl Pts',(-8.86634924200006,15.2,6.91584672599999));
#247050=CARTESIAN_POINT('Ctrl Pts',(-8.86634924200006,11.6,6.91584672599999));
#247051=CARTESIAN_POINT('Ctrl Pts',(-8.86970751300005,15.2,6.91673082599999));
#247052=CARTESIAN_POINT('Ctrl Pts',(-8.86970751300005,11.6,6.91673082599999));
#247053=CARTESIAN_POINT('Ctrl Pts',(-8.87307110100006,15.2,6.91761350899998));
#247054=CARTESIAN_POINT('Ctrl Pts',(-8.87307110100006,11.6,6.91761350899998));
#247055=CARTESIAN_POINT('Ctrl Pts',(-8.87643999800006,15.2,6.91849476499999));
#247056=CARTESIAN_POINT('Ctrl Pts',(-8.87643999800006,11.6,6.91849476499999));
#247057=CARTESIAN_POINT('Ctrl Pts',(-8.87981420000006,15.2,6.91937458799998));
#247058=CARTESIAN_POINT('Ctrl Pts',(-8.87981420000006,11.6,6.91937458799998));
#247059=CARTESIAN_POINT('Ctrl Pts',(-8.88319370000006,15.2,6.92025296799999));
#247060=CARTESIAN_POINT('Ctrl Pts',(-8.88319370000006,11.6,6.92025296799999));
#247061=CARTESIAN_POINT('Ctrl Pts',(-8.88657849200006,15.2,6.92112989699999));
#247062=CARTESIAN_POINT('Ctrl Pts',(-8.88657849200006,11.6,6.92112989699999));
#247063=CARTESIAN_POINT('Ctrl Pts',(-8.88996857100006,15.2,6.92200536799999));
#247064=CARTESIAN_POINT('Ctrl Pts',(-8.88996857100006,11.6,6.92200536799999));
#247065=CARTESIAN_POINT('Ctrl Pts',(-8.89336393000006,15.2,6.92287937299999));
#247066=CARTESIAN_POINT('Ctrl Pts',(-8.89336393000006,11.6,6.92287937299999));
#247067=CARTESIAN_POINT('Ctrl Pts',(-8.89676456200006,15.2,6.92375190499998));
#247068=CARTESIAN_POINT('Ctrl Pts',(-8.89676456200006,11.6,6.92375190499998));
#247069=CARTESIAN_POINT('Ctrl Pts',(-8.90017046300006,15.2,6.92462295199999));
#247070=CARTESIAN_POINT('Ctrl Pts',(-8.90017046300006,11.6,6.92462295199999));
#247071=CARTESIAN_POINT('Ctrl Pts',(-8.90358162600006,15.2,6.92549251099998));
#247072=CARTESIAN_POINT('Ctrl Pts',(-8.90358162600006,11.6,6.92549251099998));
#247073=CARTESIAN_POINT('Ctrl Pts',(-8.90699804400005,15.2,6.92636057199999));
#247074=CARTESIAN_POINT('Ctrl Pts',(-8.90699804400005,11.6,6.92636057199999));
#247075=CARTESIAN_POINT('Ctrl Pts',(-8.91041971400006,15.2,6.92722712699998));
#247076=CARTESIAN_POINT('Ctrl Pts',(-8.91041971400006,11.6,6.92722712699998));
#247077=CARTESIAN_POINT('Ctrl Pts',(-8.91384662700006,15.2,6.92809216799999));
#247078=CARTESIAN_POINT('Ctrl Pts',(-8.91384662700006,11.6,6.92809216799999));
#247079=CARTESIAN_POINT('Ctrl Pts',(-8.91727877800006,15.2,6.92895568799998));
#247080=CARTESIAN_POINT('Ctrl Pts',(-8.91727877800006,11.6,6.92895568799998));
#247081=CARTESIAN_POINT('Ctrl Pts',(-8.92071616200005,15.2,6.92981767899998));
#247082=CARTESIAN_POINT('Ctrl Pts',(-8.92071616200005,11.6,6.92981767899998));
#247083=CARTESIAN_POINT('Ctrl Pts',(-8.92415877200006,15.2,6.93067813199999));
#247084=CARTESIAN_POINT('Ctrl Pts',(-8.92415877200006,11.6,6.93067813199999));
#247085=CARTESIAN_POINT('Ctrl Pts',(-8.92760660200006,15.2,6.93153704099998));
#247086=CARTESIAN_POINT('Ctrl Pts',(-8.92760660200006,11.6,6.93153704099998));
#247087=CARTESIAN_POINT('Ctrl Pts',(-8.93105964700006,15.2,6.93239439799999));
#247088=CARTESIAN_POINT('Ctrl Pts',(-8.93105964700006,11.6,6.93239439799999));
#247089=CARTESIAN_POINT('Ctrl Pts',(-8.93451790000006,15.2,6.93325019299999));
#247090=CARTESIAN_POINT('Ctrl Pts',(-8.93451790000006,11.6,6.93325019299999));
#247091=CARTESIAN_POINT('Ctrl Pts',(-8.93798135500005,15.2,6.93410442099999));
#247092=CARTESIAN_POINT('Ctrl Pts',(-8.93798135500005,11.6,6.93410442099999));
#247093=CARTESIAN_POINT('Ctrl Pts',(-8.94145000700006,15.2,6.93495707399999));
#247094=CARTESIAN_POINT('Ctrl Pts',(-8.94145000700006,11.6,6.93495707399999));
#247095=CARTESIAN_POINT('Ctrl Pts',(-8.94492384900006,15.2,6.93580814299998));
#247096=CARTESIAN_POINT('Ctrl Pts',(-8.94492384900006,11.6,6.93580814299998));
#247097=CARTESIAN_POINT('Ctrl Pts',(-8.94840287600006,15.2,6.93665762099998));
#247098=CARTESIAN_POINT('Ctrl Pts',(-8.94840287600006,11.6,6.93665762099998));
#247099=CARTESIAN_POINT('Ctrl Pts',(-8.95188708200006,15.2,6.93750550099999));
#247100=CARTESIAN_POINT('Ctrl Pts',(-8.95188708200006,11.6,6.93750550099999));
#247101=CARTESIAN_POINT('Ctrl Pts',(-8.95537645900006,15.2,6.93835177399999));
#247102=CARTESIAN_POINT('Ctrl Pts',(-8.95537645900006,11.6,6.93835177399999));
#247103=CARTESIAN_POINT('Ctrl Pts',(-8.95887100500006,15.2,6.93919643299999));
#247104=CARTESIAN_POINT('Ctrl Pts',(-8.95887100500006,11.6,6.93919643299999));
#247105=CARTESIAN_POINT('Ctrl Pts',(-8.96237071000006,15.2,6.94003947099999));
#247106=CARTESIAN_POINT('Ctrl Pts',(-8.96237071000006,11.6,6.94003947099999));
#247107=CARTESIAN_POINT('Ctrl Pts',(-8.96587557000006,15.2,6.94088087999998));
#247108=CARTESIAN_POINT('Ctrl Pts',(-8.96587557000006,11.6,6.94088087999998));
#247109=CARTESIAN_POINT('Ctrl Pts',(-8.96938558000006,15.2,6.94172065299998));
#247110=CARTESIAN_POINT('Ctrl Pts',(-8.96938558000006,11.6,6.94172065299998));
#247111=CARTESIAN_POINT('Ctrl Pts',(-8.97290073400006,15.2,6.94255878199999));
#247112=CARTESIAN_POINT('Ctrl Pts',(-8.97290073400006,11.6,6.94255878199999));
#247113=CARTESIAN_POINT('Ctrl Pts',(-8.97642102300006,15.2,6.94339525799998));
#247114=CARTESIAN_POINT('Ctrl Pts',(-8.97642102300006,11.6,6.94339525799998));
#247115=CARTESIAN_POINT('Ctrl Pts',(-8.97994644400006,15.2,6.94423007599998));
#247116=CARTESIAN_POINT('Ctrl Pts',(-8.97994644400006,11.6,6.94423007599998));
#247117=CARTESIAN_POINT('Ctrl Pts',(-8.98347699100006,15.2,6.94506322799998));
#247118=CARTESIAN_POINT('Ctrl Pts',(-8.98347699100006,11.6,6.94506322799998));
#247119=CARTESIAN_POINT('Ctrl Pts',(-8.98701265700005,15.2,6.94589470499999));
#247120=CARTESIAN_POINT('Ctrl Pts',(-8.98701265700005,11.6,6.94589470499999));
#247121=CARTESIAN_POINT('Ctrl Pts',(-8.99055343700006,15.2,6.94672450099999));
#247122=CARTESIAN_POINT('Ctrl Pts',(-8.99055343700006,11.6,6.94672450099999));
#247123=CARTESIAN_POINT('Ctrl Pts',(-8.99409932400006,15.2,6.94755260799998));
#247124=CARTESIAN_POINT('Ctrl Pts',(-8.99409932400006,11.6,6.94755260799998));
#247125=CARTESIAN_POINT('Ctrl Pts',(-8.99765031400005,15.2,6.94837901999998));
#247126=CARTESIAN_POINT('Ctrl Pts',(-8.99765031400005,11.6,6.94837901999998));
#247127=CARTESIAN_POINT('Ctrl Pts',(-9.00120639900006,15.2,6.94920372699999));
#247128=CARTESIAN_POINT('Ctrl Pts',(-9.00120639900006,11.6,6.94920372699999));
#247129=CARTESIAN_POINT('Ctrl Pts',(-9.00476757400006,15.2,6.95002672299999));
#247130=CARTESIAN_POINT('Ctrl Pts',(-9.00476757400006,11.6,6.95002672299999));
#247131=CARTESIAN_POINT('Ctrl Pts',(-9.00833383300006,15.2,6.95084800199999));
#247132=CARTESIAN_POINT('Ctrl Pts',(-9.00833383300006,11.6,6.95084800199999));
#247133=CARTESIAN_POINT('Ctrl Pts',(-9.01190517100006,15.2,6.95166755499999));
#247134=CARTESIAN_POINT('Ctrl Pts',(-9.01190517100006,11.6,6.95166755499999));
#247135=CARTESIAN_POINT('Ctrl Pts',(-9.01548158200006,15.2,6.95248537499998));
#247136=CARTESIAN_POINT('Ctrl Pts',(-9.01548158200006,11.6,6.95248537499998));
#247137=CARTESIAN_POINT('Ctrl Pts',(-9.01906305900006,15.2,6.95330145399998));
#247138=CARTESIAN_POINT('Ctrl Pts',(-9.01906305900006,11.6,6.95330145399998));
#247139=CARTESIAN_POINT('Ctrl Pts',(-9.02264959700006,15.2,6.95411578599998));
#247140=CARTESIAN_POINT('Ctrl Pts',(-9.02264959700006,11.6,6.95411578599998));
#247141=CARTESIAN_POINT('Ctrl Pts',(-9.02624119000006,15.2,6.95492836299999));
#247142=CARTESIAN_POINT('Ctrl Pts',(-9.02624119000006,11.6,6.95492836299999));
#247143=CARTESIAN_POINT('Ctrl Pts',(-9.02983783100006,15.2,6.95573917899999));
#247144=CARTESIAN_POINT('Ctrl Pts',(-9.02983783100006,11.6,6.95573917899999));
#247145=CARTESIAN_POINT('Ctrl Pts',(-9.03343951600006,15.2,6.95654822399998));
#247146=CARTESIAN_POINT('Ctrl Pts',(-9.03343951600006,11.6,6.95654822399998));
#247147=CARTESIAN_POINT('Ctrl Pts',(-9.03704623800006,15.2,6.95735549299999));
#247148=CARTESIAN_POINT('Ctrl Pts',(-9.03704623800006,11.6,6.95735549299999));
#247149=CARTESIAN_POINT('Ctrl Pts',(-9.04065799200006,15.2,6.95816097899999));
#247150=CARTESIAN_POINT('Ctrl Pts',(-9.04065799200006,11.6,6.95816097899999));
#247151=CARTESIAN_POINT('Ctrl Pts',(-9.04427477200005,15.2,6.95896467299999));
#247152=CARTESIAN_POINT('Ctrl Pts',(-9.04427477200005,11.6,6.95896467299999));
#247153=CARTESIAN_POINT('Ctrl Pts',(-9.04789657200006,15.2,6.95976657099998));
#247154=CARTESIAN_POINT('Ctrl Pts',(-9.04789657200006,11.6,6.95976657099998));
#247155=CARTESIAN_POINT('Ctrl Pts',(-9.05152338600006,15.2,6.96056666299998));
#247156=CARTESIAN_POINT('Ctrl Pts',(-9.05152338600006,11.6,6.96056666299998));
#247157=CARTESIAN_POINT('Ctrl Pts',(-9.05515520900006,15.2,6.96136494399998));
#247158=CARTESIAN_POINT('Ctrl Pts',(-9.05515520900006,11.6,6.96136494399998));
#247159=CARTESIAN_POINT('Ctrl Pts',(-9.05879203500006,15.2,6.96216140399999));
#247160=CARTESIAN_POINT('Ctrl Pts',(-9.05879203500006,11.6,6.96216140399999));
#247161=CARTESIAN_POINT('Ctrl Pts',(-9.06243385700006,15.2,6.96295603899999));
#247162=CARTESIAN_POINT('Ctrl Pts',(-9.06243385700006,11.6,6.96295603899999));
#247163=CARTESIAN_POINT('Ctrl Pts',(-9.06608067000005,15.2,6.96374884099999));
#247164=CARTESIAN_POINT('Ctrl Pts',(-9.06608067000005,11.6,6.96374884099999));
#247165=CARTESIAN_POINT('Ctrl Pts',(-9.06973246700005,15.2,6.96453979999998));
#247166=CARTESIAN_POINT('Ctrl Pts',(-9.06973246700005,11.6,6.96453979999998));
#247167=CARTESIAN_POINT('Ctrl Pts',(-9.07338924200005,15.2,6.96532891099999));
#247168=CARTESIAN_POINT('Ctrl Pts',(-9.07338924200005,11.6,6.96532891099999));
#247169=CARTESIAN_POINT('Ctrl Pts',(-9.07705099100006,15.2,6.96611616699998));
#247170=CARTESIAN_POINT('Ctrl Pts',(-9.07705099100006,11.6,6.96611616699998));
#247171=CARTESIAN_POINT('Ctrl Pts',(-9.08071770800005,15.2,6.96690156099999));
#247172=CARTESIAN_POINT('Ctrl Pts',(-9.08071770800005,11.6,6.96690156099999));
#247173=CARTESIAN_POINT('Ctrl Pts',(-9.08438938600005,15.2,6.96768508699999));
#247174=CARTESIAN_POINT('Ctrl Pts',(-9.08438938600005,11.6,6.96768508699999));
#247175=CARTESIAN_POINT('Ctrl Pts',(-9.08806602100006,15.2,6.96846673699999));
#247176=CARTESIAN_POINT('Ctrl Pts',(-9.08806602100006,11.6,6.96846673699999));
#247177=CARTESIAN_POINT('Ctrl Pts',(-9.09174760800006,15.2,6.96924650799998));
#247178=CARTESIAN_POINT('Ctrl Pts',(-9.09174760800006,11.6,6.96924650799998));
#247179=CARTESIAN_POINT('Ctrl Pts',(-9.09543414200006,15.2,6.97002439099998));
#247180=CARTESIAN_POINT('Ctrl Pts',(-9.09543414200006,11.6,6.97002439099998));
#247181=CARTESIAN_POINT('Ctrl Pts',(-9.09912561600006,15.2,6.97080037899998));
#247182=CARTESIAN_POINT('Ctrl Pts',(-9.09912561600006,11.6,6.97080037899998));
#247183=CARTESIAN_POINT('Ctrl Pts',(-9.10282202200005,15.2,6.97157446399999));
#247184=CARTESIAN_POINT('Ctrl Pts',(-9.10282202200005,11.6,6.97157446399999));
#247185=CARTESIAN_POINT('Ctrl Pts',(-9.10652335600006,15.2,6.97234663799998));
#247186=CARTESIAN_POINT('Ctrl Pts',(-9.10652335600006,11.6,6.97234663799998));
#247187=CARTESIAN_POINT('Ctrl Pts',(-9.11022960900005,15.2,6.97311689299998));
#247188=CARTESIAN_POINT('Ctrl Pts',(-9.11022960900005,11.6,6.97311689299998));
#247189=CARTESIAN_POINT('Ctrl Pts',(-9.11394077400006,15.2,6.97388521799999));
#247190=CARTESIAN_POINT('Ctrl Pts',(-9.11394077400006,11.6,6.97388521799999));
#247191=CARTESIAN_POINT('Ctrl Pts',(-9.11765684500006,15.2,6.97465160799998));
#247192=CARTESIAN_POINT('Ctrl Pts',(-9.11765684500006,11.6,6.97465160799998));
#247193=CARTESIAN_POINT('Ctrl Pts',(-9.12137781700006,15.2,6.97541605599999));
#247194=CARTESIAN_POINT('Ctrl Pts',(-9.12137781700006,11.6,6.97541605599999));
#247195=CARTESIAN_POINT('Ctrl Pts',(-9.12510368600006,15.2,6.97617855899999));
#247196=CARTESIAN_POINT('Ctrl Pts',(-9.12510368600006,11.6,6.97617855899999));
#247197=CARTESIAN_POINT('Ctrl Pts',(-9.12883445000006,15.2,6.97693911099999));
#247198=CARTESIAN_POINT('Ctrl Pts',(-9.12883445000006,11.6,6.97693911099999));
#247199=CARTESIAN_POINT('Ctrl Pts',(-9.13257010500006,15.2,6.97769771199999));
#247200=CARTESIAN_POINT('Ctrl Pts',(-9.13257010500006,11.6,6.97769771199999));
#247201=CARTESIAN_POINT('Ctrl Pts',(-9.13556254400006,15.2,6.97830303199999));
#247202=CARTESIAN_POINT('Ctrl Pts',(-9.13556254400006,11.6,6.97830303199999));
#247203=CARTESIAN_POINT('Ctrl Pts',(-9.13780907400006,15.2,6.97875614399998));
#247204=CARTESIAN_POINT('Ctrl Pts',(-9.13780907400006,11.6,6.97875614399998));
#247205=CARTESIAN_POINT('Ctrl Pts',(-9.13930773800006,15.2,6.97905782699999));
#247206=CARTESIAN_POINT('Ctrl Pts',(-9.13930773800006,11.6,6.97905782699999));
#247207=CARTESIAN_POINT('Ctrl Pts',(-9.14005731500006,15.2,6.97920857099999));
#247208=CARTESIAN_POINT('Ctrl Pts',(-9.14005731500006,11.6,6.97920857099999));
#247209=CARTESIAN_POINT('Ctrl Pts',(-8.02901631900006,15.2,6.57080831899999));
#247210=CARTESIAN_POINT('Ctrl Pts',(-8.03049110446229,15.2,6.57181685366614));
#247211=CARTESIAN_POINT('Ctrl Pts',(-8.0320161093278,15.2,6.57285322826574));
#247212=CARTESIAN_POINT('Ctrl Pts',(-8.03359089408583,15.2,6.57391635240017));
#247213=CARTESIAN_POINT('Ctrl Pts',(-8.03517327325199,15.2,6.57498460345654));
#247214=CARTESIAN_POINT('Ctrl Pts',(-8.03680591570089,15.2,6.57607986594818));
#247215=CARTESIAN_POINT('Ctrl Pts',(-8.03848839087952,15.2,6.57720107915013));
#247216=CARTESIAN_POINT('Ctrl Pts',(-8.04017086590532,15.2,6.57832229225026));
#247217=CARTESIAN_POINT('Ctrl Pts',(-8.04190317283137,15.2,6.57946945464252));
#247218=CARTESIAN_POINT('Ctrl Pts',(-8.04368489176663,15.2,6.58064153793327));
#247219=CARTESIAN_POINT('Ctrl Pts',(-8.04546661070189,15.2,6.58181362122402));
#247220=CARTESIAN_POINT('Ctrl Pts',(-8.04729774128707,15.2,6.58301062651662));
#247221=CARTESIAN_POINT('Ctrl Pts',(-8.04917787055988,15.2,6.58423155119856));
#247222=CARTESIAN_POINT('Ctrl Pts',(-8.05105800000347,15.2,6.58545247599141));
#247223=CARTESIAN_POINT('Ctrl Pts',(-8.05298713099614,15.2,6.58669732359249));
#247224=CARTESIAN_POINT('Ctrl Pts',(-8.05496485719055,15.2,6.58796512041314));
#247225=CARTESIAN_POINT('Ctrl Pts',(-8.05694258320533,15.2,6.58923291711864));
#247226=CARTESIAN_POINT('Ctrl Pts',(-8.05896890538341,15.2,6.59052366630055));
#247227=CARTESIAN_POINT('Ctrl Pts',(-8.06104342948425,15.2,6.59183642200888));
#247228=CARTESIAN_POINT('Ctrl Pts',(-8.06311795358509,15.2,6.59314917771721));
#247229=CARTESIAN_POINT('Ctrl Pts',(-8.0652406808045,15.2,6.59448394076801));
#247230=CARTESIAN_POINT('Ctrl Pts',(-8.06741122014022,15.2,6.59583979646781));
#247231=CARTESIAN_POINT('Ctrl Pts',(-8.06958175967308,15.2,6.59719565229079));
#247232=CARTESIAN_POINT('Ctrl Pts',(-8.0718001153119,15.2,6.5985725970414));
#247233=CARTESIAN_POINT('Ctrl Pts',(-8.07406590652196,15.2,6.59996974311891));
#247234=CARTESIAN_POINT('Ctrl Pts',(-8.0763316975262,15.2,6.60136688906953));
#247235=CARTESIAN_POINT('Ctrl Pts',(-8.07864492271251,15.2,6.60278423372136));
#247236=CARTESIAN_POINT('Ctrl Pts',(-8.0810052091288,15.2,6.60422091158666));
#247237=CARTESIAN_POINT('Ctrl Pts',(-8.08336549554508,15.2,6.60565758945196));
#247238=CARTESIAN_POINT('Ctrl Pts',(-8.08577284749928,15.2,6.60711359814904));
#247239=CARTESIAN_POINT('Ctrl Pts',(-8.08822689382476,15.2,6.608588095178));
#247240=CARTESIAN_POINT('Ctrl Pts',(-8.09068094015023,15.2,6.61006259220696));
#247241=CARTESIAN_POINT('Ctrl Pts',(-8.09318168323473,15.2,6.6115555767414));
#247242=CARTESIAN_POINT('Ctrl Pts',(-8.09572876447236,15.2,6.61306622685197));
#247243=CARTESIAN_POINT('Ctrl Pts',(-8.09827584594135,15.2,6.61457687709976));
#247244=CARTESIAN_POINT('Ctrl Pts',(-8.10086926266481,15.2,6.61610519104097));
#247245=CARTESIAN_POINT('Ctrl Pts',(-8.10350866514402,15.2,6.61765037037591));
#247246=CARTESIAN_POINT('Ctrl Pts',(-8.10614806738348,15.2,6.61919554957051));
#247247=CARTESIAN_POINT('Ctrl Pts',(-8.10883345256066,15.2,6.62075759004112));
#247248=CARTESIAN_POINT('Ctrl Pts',(-8.11156447572374,15.2,6.62233571524091));
#247249=CARTESIAN_POINT('Ctrl Pts',(-8.11429549888682,15.2,6.6239138404407));
#247250=CARTESIAN_POINT('Ctrl Pts',(-8.11707215754802,15.2,6.62550804702571));
#247251=CARTESIAN_POINT('Ctrl Pts',(-8.1198941109424,15.2,6.62711757454952));
#247252=CARTESIAN_POINT('Ctrl Pts',(-8.1227160645931,15.2,6.62872710221953));
#247253=CARTESIAN_POINT('Ctrl Pts',(-8.12558331343989,15.2,6.63035195259939));
#247254=CARTESIAN_POINT('Ctrl Pts',(-8.12849552018388,15.2,6.63199137835604));
#247255=CARTESIAN_POINT('Ctrl Pts',(-8.13140772666334,15.2,6.63363080396376));
#247256=CARTESIAN_POINT('Ctrl Pts',(-8.13436489186082,15.2,6.63528480756059));
#247257=CARTESIAN_POINT('Ctrl Pts',(-8.13736668326528,15.2,6.63695266325754));
#247258=CARTESIAN_POINT('Ctrl Pts',(-8.14036847466976,15.2,6.63862051895448));
#247259=CARTESIAN_POINT('Ctrl Pts',(-8.14341489333673,15.2,6.6403022281027));
#247260=CARTESIAN_POINT('Ctrl Pts',(-8.14650561163811,15.2,6.64199708079023));
#247261=CARTESIAN_POINT('Ctrl Pts',(-8.14959633022023,15.2,6.64369193363172));
#247262=CARTESIAN_POINT('Ctrl Pts',(-8.15273134875635,15.2,6.64539993184433));
#247263=CARTESIAN_POINT('Ctrl Pts',(-8.15591034659095,15.2,6.64712038194143));
#247264=CARTESIAN_POINT('Ctrl Pts',(-8.15908934413678,15.2,6.64884083188225));
#247265=CARTESIAN_POINT('Ctrl Pts',(-8.16231231977699,15.2,6.65057373567169));
#247266=CARTESIAN_POINT('Ctrl Pts',(-8.16557895524164,15.2,6.65231841652496));
#247267=CARTESIAN_POINT('Ctrl Pts',(-8.16884559070628,15.2,6.65406309737823));
#247268=CARTESIAN_POINT('Ctrl Pts',(-8.17215588738246,15.2,6.65581955514721));
#247269=CARTESIAN_POINT('Ctrl Pts',(-8.17550953292566,15.2,6.65758713108734));
#247270=CARTESIAN_POINT('Ctrl Pts',(-8.17886317877349,15.2,6.65935470718801));
#247271=CARTESIAN_POINT('Ctrl Pts',(-8.18226017247622,15.2,6.66113340036345));
#247272=CARTESIAN_POINT('Ctrl Pts',(-8.18570020341662,15.2,6.66292256646165));
#247273=CARTESIAN_POINT('Ctrl Pts',(-8.18914023404455,15.2,6.66471173239735));
#247274=CARTESIAN_POINT('Ctrl Pts',(-8.19262330516359,15.2,6.66651136899997));
#247275=CARTESIAN_POINT('Ctrl Pts',(-8.19614910871825,15.2,6.66832084802579));
#247276=CARTESIAN_POINT('Ctrl Pts',(-8.19967491227291,15.2,6.67013032705162));
#247277=CARTESIAN_POINT('Ctrl Pts',(-8.20324345005307,15.2,6.6719496470672));
#247278=CARTESIAN_POINT('Ctrl Pts',(-8.2068544195867,15.2,6.67377819116702));
#247279=CARTESIAN_POINT('Ctrl Pts',(-8.20986356097405,15.2,6.67530197797224));
#247280=CARTESIAN_POINT('Ctrl Pts',(-8.21290216901772,15.2,6.6768321706943));
#247281=CARTESIAN_POINT('Ctrl Pts',(-8.21597007276618,15.2,6.6783684191662));
#247282=CARTESIAN_POINT('Ctrl Pts',(-8.21903797651465,15.2,6.6799046676381));
#247283=CARTESIAN_POINT('Ctrl Pts',(-8.22213517478973,15.2,6.68144697153657));
#247284=CARTESIAN_POINT('Ctrl Pts',(-8.22526149549829,15.2,6.6829949875158));
#247285=CARTESIAN_POINT('Ctrl Pts',(-8.22838781620684,15.2,6.68454300349504));
#247286=CARTESIAN_POINT('Ctrl Pts',(-8.23154326289995,15.2,6.68609673124996));
#247287=CARTESIAN_POINT('Ctrl Pts',(-8.23472766269164,15.2,6.68765583249997));
#247288=CARTESIAN_POINT('Ctrl Pts',(-8.23854894230283,15.2,6.68952675393201));
#247289=CARTESIAN_POINT('Ctrl Pts',(-8.24241191793825,15.2,6.69140541580895));
#247290=CARTESIAN_POINT('Ctrl Pts',(-8.24631629865572,15.2,6.69329124133423));
#247291=CARTESIAN_POINT('Ctrl Pts',(-8.24956994937182,15.2,6.69486276266239));
#247292=CARTESIAN_POINT('Ctrl Pts',(-8.25285235445733,15.2,6.69643926186906));
#247293=CARTESIAN_POINT('Ctrl Pts',(-8.25616334681695,15.2,6.69802041068826));
#247294=CARTESIAN_POINT('Ctrl Pts',(-8.25947433917657,15.2,6.69960155950747));
#247295=CARTESIAN_POINT('Ctrl Pts',(-8.26281392218693,15.2,6.70118736157957));
#247296=CARTESIAN_POINT('Ctrl Pts',(-8.26618192704656,15.2,6.70277749366267));
#247297=CARTESIAN_POINT('Ctrl Pts',(-8.26954993190617,15.2,6.70436762574578));
#247298=CARTESIAN_POINT('Ctrl Pts',(-8.27294636232709,15.2,6.70596209069186));
#247299=CARTESIAN_POINT('Ctrl Pts',(-8.27637105373145,15.2,6.70756057278244));
#247300=CARTESIAN_POINT('Ctrl Pts',(-8.27979574513583,15.2,6.70915905487303));
#247301=CARTESIAN_POINT('Ctrl Pts',(-8.28324869771664,15.2,6.71076155453331));
#247302=CARTESIAN_POINT('Ctrl Pts',(-8.28672975000832,15.2,6.71236776328331));
#247303=CARTESIAN_POINT('Ctrl Pts',(-8.29021080229998,15.2,6.71397397203331));
#247304=CARTESIAN_POINT('Ctrl Pts',(-8.29371995558578,15.2,6.71558388856019));
#247305=CARTESIAN_POINT('Ctrl Pts',(-8.29725704872691,15.2,6.71719721148419));
#247306=CARTESIAN_POINT('Ctrl Pts',(-8.30079414186805,15.2,6.71881053440819));
#247307=CARTESIAN_POINT('Ctrl Pts',(-8.30435917615591,15.2,6.72042726148355));
#247308=CARTESIAN_POINT('Ctrl Pts',(-8.30795199101846,15.2,6.7220470953726));
#247309=CARTESIAN_POINT('Ctrl Pts',(-8.31154480588101,15.2,6.72366692926165));
#247310=CARTESIAN_POINT('Ctrl Pts',(-8.31516540353176,15.2,6.72528986717284));
#247311=CARTESIAN_POINT('Ctrl Pts',(-8.31881362429708,15.2,6.72691562008965));
#247312=CARTESIAN_POINT('Ctrl Pts',(-8.3224618450624,15.2,6.72854137300647));
#247313=CARTESIAN_POINT('Ctrl Pts',(-8.32613769035757,15.2,6.73016993708987));
#247314=CARTESIAN_POINT('Ctrl Pts',(-8.32984100348402,15.2,6.73180102438167));
#247315=CARTESIAN_POINT('Ctrl Pts',(-8.33354431661046,15.2,6.73343211167347));
#247316=CARTESIAN_POINT('Ctrl Pts',(-8.33727509821339,15.2,6.7350657214969));
#247317=CARTESIAN_POINT('Ctrl Pts',(-8.34103319319468,15.2,6.73670157123155));
#247318=CARTESIAN_POINT('Ctrl Pts',(-8.34479128817596,15.2,6.73833742096621));
#247319=CARTESIAN_POINT('Ctrl Pts',(-8.34857669656313,15.2,6.73997550786434));
#247320=CARTESIAN_POINT('Ctrl Pts',(-8.35238926323202,15.2,6.7416155534895));
#247321=CARTESIAN_POINT('Ctrl Pts',(-8.35620182990089,15.2,6.74325559911466));
#247322=CARTESIAN_POINT('Ctrl Pts',(-8.36004155802578,15.2,6.74489760268706));
#247323=CARTESIAN_POINT('Ctrl Pts',(-8.36390829122243,15.2,6.74654128921497));
#247324=CARTESIAN_POINT('Ctrl Pts',(-8.36700167752687,15.2,6.7478562383298));
#247325=CARTESIAN_POINT('Ctrl Pts',(-8.37011235030333,15.2,6.74917226514799));
#247326=CARTESIAN_POINT('Ctrl Pts',(-8.37324022800619,15.2,6.75048922899075));
#247327=CARTESIAN_POINT('Ctrl Pts',(-8.37636810613523,15.2,6.75180619301294));
#247328=CARTESIAN_POINT('Ctrl Pts',(-8.37951319143738,15.2,6.75312409465198));
#247329=CARTESIAN_POINT('Ctrl Pts',(-8.38267540616702,15.2,6.75444279722393));
#247330=CARTESIAN_POINT('Ctrl Pts',(-8.38583762046581,15.2,6.75576149961619));
#247331=CARTESIAN_POINT('Ctrl Pts',(-8.38901696530126,15.2,6.75708100143059));
#247332=CARTESIAN_POINT('Ctrl Pts',(-8.39221336170551,15.2,6.75840116793373));
#247333=CARTESIAN_POINT('Ctrl Pts',(-8.39540975854526,15.2,6.75972133461675));
#247334=CARTESIAN_POINT('Ctrl Pts',(-8.39862321024381,15.2,6.76104216575087));
#247335=CARTESIAN_POINT('Ctrl Pts',(-8.40185363719384,15.2,6.76236352716673));
#247336=CARTESIAN_POINT('Ctrl Pts',(-8.40508406370374,15.2,6.76368488840255));
#247337=CARTESIAN_POINT('Ctrl Pts',(-8.40833146682903,15.2,6.76500678031389));
#247338=CARTESIAN_POINT('Ctrl Pts',(-8.41159577044996,15.2,6.76632907015022));
#247339=CARTESIAN_POINT('Ctrl Pts',(-8.41486007451564,15.2,6.76765136016671));
#247340=CARTESIAN_POINT('Ctrl Pts',(-8.41814127968336,15.2,6.76897404709436));
#247341=CARTESIAN_POINT('Ctrl Pts',(-8.4214393097531,15.2,6.77029700233314));
#247342=CARTESIAN_POINT('Ctrl Pts',(-8.42473733937348,15.2,6.77161995739168));
#247343=CARTESIAN_POINT('Ctrl Pts',(-8.42805219426569,15.2,6.77294317811949));
#247344=CARTESIAN_POINT('Ctrl Pts',(-8.43138379999164,15.2,6.77426653679962));
#247345=CARTESIAN_POINT('Ctrl Pts',(-8.43471540617151,15.2,6.77558989566006));
#247346=CARTESIAN_POINT('Ctrl Pts',(-8.4380637612352,15.2,6.77691339275549));
#247347=CARTESIAN_POINT('Ctrl Pts',(-8.44142879197524,15.2,6.77823689888318));
#247348=CARTESIAN_POINT('Ctrl Pts',(-8.44563508017105,15.2,6.77989128145262));
#247349=CARTESIAN_POINT('Ctrl Pts',(-8.4498674242884,15.2,6.78154567890817));
#247350=CARTESIAN_POINT('Ctrl Pts',(-8.45412567901197,15.2,6.78319984557483));
#247351=CARTESIAN_POINT('Ctrl Pts',(-8.45753228251232,15.2,6.78452317879997));
#247352=CARTESIAN_POINT('Ctrl Pts',(-8.46095546774228,15.2,6.78584636423894));
#247353=CARTESIAN_POINT('Ctrl Pts',(-8.46439516224262,15.2,6.78716927630802));
#247354=CARTESIAN_POINT('Ctrl Pts',(-8.46783485721161,15.2,6.78849218855734));
#247355=CARTESIAN_POINT('Ctrl Pts',(-8.47129106073814,15.2,6.78981483024714));
#247356=CARTESIAN_POINT('Ctrl Pts',(-8.47476369948404,15.2,6.79113707454141));
#247357=CARTESIAN_POINT('Ctrl Pts',(-8.47823633775679,15.2,6.79245931865553));
#247358=CARTESIAN_POINT('Ctrl Pts',(-8.48172541120677,15.2,6.79378116889469));
#247359=CARTESIAN_POINT('Ctrl Pts',(-8.48523084741852,15.2,6.79510250150895));
#247360=CARTESIAN_POINT('Ctrl Pts',(-8.48961264304142,15.2,6.79675416741179));
#247361=CARTESIAN_POINT('Ctrl Pts',(-8.49402000303247,15.2,6.79840502507597));
#247362=CARTESIAN_POINT('Ctrl Pts',(-8.49845278741884,15.2,6.80005483953347));
#247363=CARTESIAN_POINT('Ctrl Pts',(-8.5028855718052,15.2,6.80170465399096));
#247364=CARTESIAN_POINT('Ctrl Pts',(-8.50734378101378,15.2,6.80335342785883));
#247365=CARTESIAN_POINT('Ctrl Pts',(-8.51182727170693,15.2,6.80500092640057));
#247366=CARTESIAN_POINT('Ctrl Pts',(-8.51631076240006,15.2,6.8066484249423));
#247367=CARTESIAN_POINT('Ctrl Pts',(-8.52081953651052,15.2,6.80829465141456));
#247368=CARTESIAN_POINT('Ctrl Pts',(-8.52535345220363,15.2,6.80993937565075));
#247369=CARTESIAN_POINT('Ctrl Pts',(-8.52988736789674,15.2,6.81158409988694));
#247370=CARTESIAN_POINT('Ctrl Pts',(-8.534446425299,15.2,6.81322732160831));
#247371=CARTESIAN_POINT('Ctrl Pts',(-8.53903048601416,15.2,6.81486881849076));
#247372=CARTESIAN_POINT('Ctrl Pts',(-8.54269773478616,15.2,6.81618201606829));
#247373=CARTESIAN_POINT('Ctrl Pts',(-8.54638098384325,15.2,6.81749410834855));
#247374=CARTESIAN_POINT('Ctrl Pts',(-8.55008016454649,15.2,6.81880498319765));
#247375=CARTESIAN_POINT('Ctrl Pts',(-8.5537793447457,15.2,6.82011585786814));
#247376=CARTESIAN_POINT('Ctrl Pts',(-8.55749445558174,15.2,6.82142551358878));
#247377=CARTESIAN_POINT('Ctrl Pts',(-8.5612254258868,15.2,6.82273383959303));
#247378=CARTESIAN_POINT('Ctrl Pts',(-8.5649563967002,15.2,6.82404216577552));
#247379=CARTESIAN_POINT('Ctrl Pts',(-8.56870322783498,15.2,6.82534916148094));
#247380=CARTESIAN_POINT('Ctrl Pts',(-8.57246584756273,15.2,6.82665471517276));
#247381=CARTESIAN_POINT('Ctrl Pts',(-8.57622846677783,15.2,6.82796026868669));
#247382=CARTESIAN_POINT('Ctrl Pts',(-8.58000687539563,15.2,6.82926438173321));
#247383=CARTESIAN_POINT('Ctrl Pts',(-8.5838010029733,15.2,6.83056694196016));
#247384=CARTESIAN_POINT('Ctrl Pts',(-8.58949219511525,15.2,6.83252078256678));
#247385=CARTESIAN_POINT('Ctrl Pts',(-8.59521875529496,15.2,6.83447113347301));
#247386=CARTESIAN_POINT('Ctrl Pts',(-8.60098044661137,15.2,6.83641762691216));
#247387=CARTESIAN_POINT('Ctrl Pts',(-8.60482157363228,15.2,6.83771528902813));
#247388=CARTESIAN_POINT('Ctrl Pts',(-8.60867831560116,15.2,6.83901123714431));
#247389=CARTESIAN_POINT('Ctrl Pts',(-8.61255060195025,15.2,6.84030536459418));
#247390=CARTESIAN_POINT('Ctrl Pts',(-8.61642288882695,15.2,6.84159949222039));
#247391=CARTESIAN_POINT('Ctrl Pts',(-8.62031072164352,15.2,6.8428917996526));
#247392=CARTESIAN_POINT('Ctrl Pts',(-8.62421402877481,15.2,6.84418217945389));
#247393=CARTESIAN_POINT('Ctrl Pts',(-8.62909316242302,15.2,6.84579515411761));
#247394=CARTESIAN_POINT('Ctrl Pts',(-8.63399647786476,15.2,6.84740511894931));
#247395=CARTESIAN_POINT('Ctrl Pts',(-8.6389238393945,15.2,6.84901186922683));
#247396=CARTESIAN_POINT('Ctrl Pts',(-8.64286572829605,15.2,6.85029726934376));
#247397=CARTESIAN_POINT('Ctrl Pts',(-8.6468230057178,15.2,6.85158061243038));
#247398=CARTESIAN_POINT('Ctrl Pts',(-8.65079560472538,15.2,6.85286179460357));
#247399=CARTESIAN_POINT('Ctrl Pts',(-8.65476820427422,15.2,6.85414297695131));
#247400=CARTESIAN_POINT('Ctrl Pts',(-8.65875612554205,15.2,6.8554219991993));
#247401=CARTESIAN_POINT('Ctrl Pts',(-8.66275929857264,15.2,6.85669875894358));
#247402=CARTESIAN_POINT('Ctrl Pts',(-8.66876405757309,15.2,6.85861389838604));
#247403=CARTESIAN_POINT('Ctrl Pts',(-8.67480313625397,15.2,6.86052394531918));
#247404=CARTESIAN_POINT('Ctrl Pts',(-8.68087630303333,15.2,6.86242856275));
#247405=CARTESIAN_POINT('Ctrl Pts',(-8.684925081254,15.2,6.86369830781921));
#247406=CARTESIAN_POINT('Ctrl Pts',(-8.68898900988754,15.2,6.86496563867979));
#247407=CARTESIAN_POINT('Ctrl Pts',(-8.69306802266692,15.2,6.86623045691512));
#247408=CARTESIAN_POINT('Ctrl Pts',(-8.6981667878075,15.2,6.86781147945079));
#247409=CARTESIAN_POINT('Ctrl Pts',(-8.70328911886753,15.2,6.86938857400425));
#247410=CARTESIAN_POINT('Ctrl Pts',(-8.7084348865686,15.2,6.87096155077758));
#247411=CARTESIAN_POINT('Ctrl Pts',(-8.71460980881948,15.2,6.87284912321417));
#247412=CARTESIAN_POINT('Ctrl Pts',(-8.72081847705701,15.2,6.87473076365857));
#247413=CARTESIAN_POINT('Ctrl Pts',(-8.72706066831535,15.2,6.87660614534385));
#247414=CARTESIAN_POINT('Ctrl Pts',(-8.73122212858724,15.2,6.87785639963035));
#247415=CARTESIAN_POINT('Ctrl Pts',(-8.73539848625421,15.2,6.87910387299203));
#247416=CARTESIAN_POINT('Ctrl Pts',(-8.73958967667525,15.2,6.88034846928605));
#247417=CARTESIAN_POINT('Ctrl Pts',(-8.74378086766732,15.2,6.88159306574964));
#247418=CARTESIAN_POINT('Ctrl Pts',(-8.7479868885392,15.2,6.88283478468114));
#247419=CARTESIAN_POINT('Ctrl Pts',(-8.75220767660352,15.2,6.88407353235957));
#247420=CARTESIAN_POINT('Ctrl Pts',(-8.75642846409276,15.2,6.88531227986922));
#247421=CARTESIAN_POINT('Ctrl Pts',(-8.76066401522073,15.2,6.88654805429891));
#247422=CARTESIAN_POINT('Ctrl Pts',(-8.76491426553842,15.2,6.88778076453178));
#247423=CARTESIAN_POINT('Ctrl Pts',(-8.7691645164352,15.2,6.88901347493261));
#247424=CARTESIAN_POINT('Ctrl Pts',(-8.77342946651131,15.2,6.89024311897565));
#247425=CARTESIAN_POINT('Ctrl Pts',(-8.77770904998625,15.2,6.8914696059925));
#247426=CARTESIAN_POINT('Ctrl Pts',(-8.78091873730091,15.2,6.89238947117158));
#247427=CARTESIAN_POINT('Ctrl Pts',(-8.78413665514967,15.2,6.89330755927829));
#247428=CARTESIAN_POINT('Ctrl Pts',(-8.78736277646374,15.2,6.89422383249916));
#247429=CARTESIAN_POINT('Ctrl Pts',(-8.7905888977778,15.2,6.89514010572004));
#247430=CARTESIAN_POINT('Ctrl Pts',(-8.79382322154856,15.2,6.89605456391682));
#247431=CARTESIAN_POINT('Ctrl Pts',(-8.79706572138837,15.2,6.89696716767549));
#247432=CARTESIAN_POINT('Ctrl Pts',(-8.80138905490083,15.2,6.89818397279758));
#247433=CARTESIAN_POINT('Ctrl Pts',(-8.80572692283445,15.2,6.89939748297205));
#247434=CARTESIAN_POINT('Ctrl Pts',(-8.81007925907261,15.2,6.90060760681556));
#247435=CARTESIAN_POINT('Ctrl Pts',(-8.81334351095472,15.2,6.90151519961575));
#247436=CARTESIAN_POINT('Ctrl Pts',(-8.81661590167391,15.2,6.90242088807956));
#247437=CARTESIAN_POINT('Ctrl Pts',(-8.81989640398631,15.2,6.90332463380082));
#247438=CARTESIAN_POINT('Ctrl Pts',(-8.82427040687088,15.2,6.90452962804111));
#247439=CARTESIAN_POINT('Ctrl Pts',(-8.82865882807488,15.2,6.9057311691128));
#247440=CARTESIAN_POINT('Ctrl Pts',(-8.83306160504682,15.2,6.90692916757079));
#247441=CARTESIAN_POINT('Ctrl Pts',(-8.83636368852562,15.2,6.90782766661832));
#247442=CARTESIAN_POINT('Ctrl Pts',(-8.8396738473567,15.2,6.90872417389861));
#247443=CARTESIAN_POINT('Ctrl Pts',(-8.84299205196505,15.2,6.90961865094499));
#247444=CARTESIAN_POINT('Ctrl Pts',(-8.8463102559706,15.2,6.91051312782888));
#247445=CARTESIAN_POINT('Ctrl Pts',(-8.84963650810069,15.2,6.91140557597954));
#247446=CARTESIAN_POINT('Ctrl Pts',(-8.85297077910524,15.2,6.91229595682202));
#247447=CARTESIAN_POINT('Ctrl Pts',(-8.85630505010979,15.2,6.91318633766449));
#247448=CARTESIAN_POINT('Ctrl Pts',(-8.85964734252619,15.2,6.91407465199566));
#247449=CARTESIAN_POINT('Ctrl Pts',(-8.86299762600305,15.2,6.91496086371747));
#247450=CARTESIAN_POINT('Ctrl Pts',(-8.86634790947992,15.2,6.91584707543929));
#247451=CARTESIAN_POINT('Ctrl Pts',(-8.86970618638733,15.2,6.91673118347723));
#247452=CARTESIAN_POINT('Ctrl Pts',(-8.87307242828028,15.2,6.91761315228253));
#247453=CARTESIAN_POINT('Ctrl Pts',(-8.87643867017324,15.2,6.91849512108784));
#247454=CARTESIAN_POINT('Ctrl Pts',(-8.87981287722173,15.2,6.91937495131933));
#247455=CARTESIAN_POINT('Ctrl Pts',(-8.88319502263981,15.2,6.92025260516263));
#247456=CARTESIAN_POINT('Ctrl Pts',(-8.88657716805789,15.2,6.92113025900594));
#247457=CARTESIAN_POINT('Ctrl Pts',(-8.88996725261712,15.2,6.92200573684105));
#247458=CARTESIAN_POINT('Ctrl Pts',(-8.89336524753424,15.2,6.92287900451796));
#247459=CARTESIAN_POINT('Ctrl Pts',(-8.89676324306866,15.2,6.9237522723535));
#247460=CARTESIAN_POINT('Ctrl Pts',(-8.900169149947,15.2,6.9246233273301));
#247461=CARTESIAN_POINT('Ctrl Pts',(-8.90358294052755,15.2,6.92549213670606));
#247462=CARTESIAN_POINT('Ctrl Pts',(-8.90927259004805,15.2,6.92694015196439));
#247463=CARTESIAN_POINT('Ctrl Pts',(-8.91498414095459,15.2,6.92838192553484));
#247464=CARTESIAN_POINT('Ctrl Pts',(-8.92071746775842,15.2,6.92981729433725));
#247465=CARTESIAN_POINT('Ctrl Pts',(-8.9253041299514,15.2,6.93096558956692));
#247466=CARTESIAN_POINT('Ctrl Pts',(-8.92990472886795,15.2,6.93210978655176));
#247467=CARTESIAN_POINT('Ctrl Pts',(-8.93451920050833,15.2,6.93324980122501));
#247468=CARTESIAN_POINT('Ctrl Pts',(-8.93798005392426,15.2,6.93410481215228));
#247469=CARTESIAN_POINT('Ctrl Pts',(-8.94144871094819,15.2,6.9349574722713));
#247470=CARTESIAN_POINT('Ctrl Pts',(-8.94492514486286,15.2,6.93580774515728));
#247471=CARTESIAN_POINT('Ctrl Pts',(-8.94956039050346,15.2,6.93694144244157));
#247472=CARTESIAN_POINT('Ctrl Pts',(-8.95420946170408,15.2,6.93807089727257));
#247473=CARTESIAN_POINT('Ctrl Pts',(-8.95887229518132,15.2,6.93919602783361));
#247474=CARTESIAN_POINT('Ctrl Pts',(-8.96353512802323,15.2,6.94032115824135));
#247475=CARTESIAN_POINT('Ctrl Pts',(-8.96821172260313,15.2,6.94144196610087));
#247476=CARTESIAN_POINT('Ctrl Pts',(-8.97290201711949,15.2,6.94255836862131));
#247477=CARTESIAN_POINT('Ctrl Pts',(-8.97641973816652,15.2,6.94339567054968));
#247478=CARTESIAN_POINT('Ctrl Pts',(-8.97994516412586,15.2,6.94423049524845));
#247479=CARTESIAN_POINT('Ctrl Pts',(-8.98347826999646,15.2,6.94506280909356));
#247480=CARTESIAN_POINT('Ctrl Pts',(-8.9870113765089,15.2,6.94589512308986));
#247481=CARTESIAN_POINT('Ctrl Pts',(-8.99055216197349,15.2,6.9467249254438));
#247482=CARTESIAN_POINT('Ctrl Pts',(-8.99410060049023,15.2,6.94755218439701));
#247483=CARTESIAN_POINT('Ctrl Pts',(-8.9988318507715,15.2,6.94865519608415));
#247484=CARTESIAN_POINT('Ctrl Pts',(-9.00357670535378,15.2,6.94975368340521));
#247485=CARTESIAN_POINT('Ctrl Pts',(-9.0083351023528,15.2,6.95084757042721));
#247486=CARTESIAN_POINT('Ctrl Pts',(-9.01190390026415,15.2,6.95166798573096));
#247487=CARTESIAN_POINT('Ctrl Pts',(-9.01548031645871,15.2,6.95248581214751));
#247488=CARTESIAN_POINT('Ctrl Pts',(-9.01906432354832,15.2,6.95330101707559));
#247489=CARTESIAN_POINT('Ctrl Pts',(-9.02264833063795,15.2,6.95411622200366));
#247490=CARTESIAN_POINT('Ctrl Pts',(-9.02623992878052,15.2,6.95492880626917));
#247491=CARTESIAN_POINT('Ctrl Pts',(-9.02983909119039,15.2,6.9557387361151));
#247492=CARTESIAN_POINT('Ctrl Pts',(-9.0334382542541,15.2,6.95654866610817));
#247493=CARTESIAN_POINT('Ctrl Pts',(-9.03704498226163,15.2,6.95735594164217));
#247494=CARTESIAN_POINT('Ctrl Pts',(-9.04065924928792,15.2,6.95816053121707));
#247495=CARTESIAN_POINT('Ctrl Pts',(-9.04427351565762,15.2,6.9589651206458));
#247496=CARTESIAN_POINT('Ctrl Pts',(-9.04789532072694,15.2,6.95976702444967));
#247497=CARTESIAN_POINT('Ctrl Pts',(-9.05152463863739,15.2,6.9605662102954));
#247498=CARTESIAN_POINT('Ctrl Pts',(-9.05515395654783,15.2,6.96136539614112));
#247499=CARTESIAN_POINT('Ctrl Pts',(-9.05879078785248,15.2,6.96216186300931));
#247500=CARTESIAN_POINT('Ctrl Pts',(-9.06243510473666,15.2,6.96295558073406));
#247501=CARTESIAN_POINT('Ctrl Pts',(-9.06607942162084,15.2,6.96374929845882));
#247502=CARTESIAN_POINT('Ctrl Pts',(-9.06973122401306,15.2,6.96454026435767));
#247503=CARTESIAN_POINT('Ctrl Pts',(-9.07339048548002,15.2,6.96532844724929));
#247504=CARTESIAN_POINT('Ctrl Pts',(-9.07704974694698,15.2,6.96611663014091));
#247505=CARTESIAN_POINT('Ctrl Pts',(-9.08071646885045,15.2,6.96690203044285));
#247506=CARTESIAN_POINT('Ctrl Pts',(-9.08439062484131,15.2,6.96768461795632));
#247507=CARTESIAN_POINT('Ctrl Pts',(-9.08806478083216,15.2,6.9684672054698));
#247508=CARTESIAN_POINT('Ctrl Pts',(-9.09174637294751,15.2,6.96924698222514));
#247509=CARTESIAN_POINT('Ctrl Pts',(-9.09543537618747,15.2,6.9700239170723));
#247510=CARTESIAN_POINT('Ctrl Pts',(-9.09912438009759,15.2,6.97080085206061));
#247511=CARTESIAN_POINT('Ctrl Pts',(-9.10282079320149,15.2,6.9715749445731));
#247512=CARTESIAN_POINT('Ctrl Pts',(-9.10652458657411,15.2,6.97234615839313));
#247513=CARTESIAN_POINT('Ctrl Pts',(-9.11022837927387,15.2,6.97311737207304));
#247514=CARTESIAN_POINT('Ctrl Pts',(-9.11393954980134,15.2,6.97388570408798));
#247515=CARTESIAN_POINT('Ctrl Pts',(-9.11765807097785,15.2,6.9746511226814));
#247516=CARTESIAN_POINT('Ctrl Pts',(-9.12137659215437,15.2,6.97541654127482));
#247517=CARTESIAN_POINT('Ctrl Pts',(-9.12510246390719,15.2,6.97617904686198));
#247518=CARTESIAN_POINT('Ctrl Pts',(-9.1288356732116,15.2,6.97693862333241));
#247519=CARTESIAN_POINT('Ctrl Pts',(-9.13256888251601,15.2,6.97769819980284));
#247520=CARTESIAN_POINT('Ctrl Pts',(-9.13630942931919,15.2,6.97845485086305));
#247521=CARTESIAN_POINT('Ctrl Pts',(-9.14005731500006,15.2,6.97920857099999));
#247522=CARTESIAN_POINT('Ctrl Pts',(-8.02901631900006,12.2,6.57080831899999));
#247523=CARTESIAN_POINT('Ctrl Pts',(-8.03049110446229,12.2,6.57181685366614));
#247524=CARTESIAN_POINT('Ctrl Pts',(-8.0320161093278,12.2,6.57285322826574));
#247525=CARTESIAN_POINT('Ctrl Pts',(-8.03359089408583,12.2,6.57391635240017));
#247526=CARTESIAN_POINT('Ctrl Pts',(-8.03517327325199,12.2,6.57498460345654));
#247527=CARTESIAN_POINT('Ctrl Pts',(-8.03680591570089,12.2,6.57607986594818));
#247528=CARTESIAN_POINT('Ctrl Pts',(-8.03848839087952,12.2,6.57720107915013));
#247529=CARTESIAN_POINT('Ctrl Pts',(-8.04017086590532,12.2,6.57832229225026));
#247530=CARTESIAN_POINT('Ctrl Pts',(-8.04190317283137,12.2,6.57946945464252));
#247531=CARTESIAN_POINT('Ctrl Pts',(-8.04368489176663,12.2,6.58064153793327));
#247532=CARTESIAN_POINT('Ctrl Pts',(-8.04546661070189,12.2,6.58181362122402));
#247533=CARTESIAN_POINT('Ctrl Pts',(-8.04729774128707,12.2,6.58301062651662));
#247534=CARTESIAN_POINT('Ctrl Pts',(-8.04917787055988,12.2,6.58423155119856));
#247535=CARTESIAN_POINT('Ctrl Pts',(-8.05105800000347,12.2,6.58545247599141));
#247536=CARTESIAN_POINT('Ctrl Pts',(-8.05298713099614,12.2,6.58669732359249));
#247537=CARTESIAN_POINT('Ctrl Pts',(-8.05496485719055,12.2,6.58796512041314));
#247538=CARTESIAN_POINT('Ctrl Pts',(-8.05694258320533,12.2,6.58923291711864));
#247539=CARTESIAN_POINT('Ctrl Pts',(-8.05896890538341,12.2,6.59052366630055));
#247540=CARTESIAN_POINT('Ctrl Pts',(-8.06104342948425,12.2,6.59183642200888));
#247541=CARTESIAN_POINT('Ctrl Pts',(-8.06311795358509,12.2,6.59314917771721));
#247542=CARTESIAN_POINT('Ctrl Pts',(-8.0652406808045,12.2,6.59448394076801));
#247543=CARTESIAN_POINT('Ctrl Pts',(-8.06741122014022,12.2,6.59583979646781));
#247544=CARTESIAN_POINT('Ctrl Pts',(-8.06958175967308,12.2,6.59719565229079));
#247545=CARTESIAN_POINT('Ctrl Pts',(-8.0718001153119,12.2,6.5985725970414));
#247546=CARTESIAN_POINT('Ctrl Pts',(-8.07406590652196,12.2,6.59996974311891));
#247547=CARTESIAN_POINT('Ctrl Pts',(-8.0763316975262,12.2,6.60136688906953));
#247548=CARTESIAN_POINT('Ctrl Pts',(-8.07864492271251,12.2,6.60278423372136));
#247549=CARTESIAN_POINT('Ctrl Pts',(-8.0810052091288,12.2,6.60422091158666));
#247550=CARTESIAN_POINT('Ctrl Pts',(-8.08336549554508,12.2,6.60565758945196));
#247551=CARTESIAN_POINT('Ctrl Pts',(-8.08577284749928,12.2,6.60711359814904));
#247552=CARTESIAN_POINT('Ctrl Pts',(-8.08822689382476,12.2,6.608588095178));
#247553=CARTESIAN_POINT('Ctrl Pts',(-8.09068094015023,12.2,6.61006259220696));
#247554=CARTESIAN_POINT('Ctrl Pts',(-8.09318168323473,12.2,6.6115555767414));
#247555=CARTESIAN_POINT('Ctrl Pts',(-8.09572876447236,12.2,6.61306622685197));
#247556=CARTESIAN_POINT('Ctrl Pts',(-8.09827584594135,12.2,6.61457687709976));
#247557=CARTESIAN_POINT('Ctrl Pts',(-8.10086926266482,12.2,6.61610519104097));
#247558=CARTESIAN_POINT('Ctrl Pts',(-8.10350866514402,12.2,6.61765037037591));
#247559=CARTESIAN_POINT('Ctrl Pts',(-8.10614806738348,12.2,6.61919554957051));
#247560=CARTESIAN_POINT('Ctrl Pts',(-8.10883345256066,12.2,6.62075759004112));
#247561=CARTESIAN_POINT('Ctrl Pts',(-8.11156447572374,12.2,6.62233571524091));
#247562=CARTESIAN_POINT('Ctrl Pts',(-8.11429549888682,12.2,6.6239138404407));
#247563=CARTESIAN_POINT('Ctrl Pts',(-8.11707215754802,12.2,6.62550804702571));
#247564=CARTESIAN_POINT('Ctrl Pts',(-8.1198941109424,12.2,6.62711757454952));
#247565=CARTESIAN_POINT('Ctrl Pts',(-8.1227160645931,12.2,6.62872710221953));
#247566=CARTESIAN_POINT('Ctrl Pts',(-8.12558331343989,12.2,6.63035195259939));
#247567=CARTESIAN_POINT('Ctrl Pts',(-8.12849552018388,12.2,6.63199137835604));
#247568=CARTESIAN_POINT('Ctrl Pts',(-8.13140772666334,12.2,6.63363080396375));
#247569=CARTESIAN_POINT('Ctrl Pts',(-8.13436489186082,12.2,6.63528480756059));
#247570=CARTESIAN_POINT('Ctrl Pts',(-8.13736668326528,12.2,6.63695266325754));
#247571=CARTESIAN_POINT('Ctrl Pts',(-8.14036847466976,12.2,6.63862051895448));
#247572=CARTESIAN_POINT('Ctrl Pts',(-8.14341489333673,12.2,6.6403022281027));
#247573=CARTESIAN_POINT('Ctrl Pts',(-8.14650561163811,12.2,6.64199708079023));
#247574=CARTESIAN_POINT('Ctrl Pts',(-8.14959633022023,12.2,6.64369193363172));
#247575=CARTESIAN_POINT('Ctrl Pts',(-8.15273134875633,12.2,6.64539993184432));
#247576=CARTESIAN_POINT('Ctrl Pts',(-8.15591034659093,12.2,6.64712038194142));
#247577=CARTESIAN_POINT('Ctrl Pts',(-8.15908934413677,12.2,6.64884083188224));
#247578=CARTESIAN_POINT('Ctrl Pts',(-8.16231231977698,12.2,6.65057373567168));
#247579=CARTESIAN_POINT('Ctrl Pts',(-8.16557895524163,12.2,6.65231841652496));
#247580=CARTESIAN_POINT('Ctrl Pts',(-8.16884559070627,12.2,6.65406309737823));
#247581=CARTESIAN_POINT('Ctrl Pts',(-8.17215588738246,12.2,6.65581955514721));
#247582=CARTESIAN_POINT('Ctrl Pts',(-8.17550953292566,12.2,6.65758713108734));
#247583=CARTESIAN_POINT('Ctrl Pts',(-8.17886317877349,12.2,6.65935470718801));
#247584=CARTESIAN_POINT('Ctrl Pts',(-8.18226017247621,12.2,6.66113340036344));
#247585=CARTESIAN_POINT('Ctrl Pts',(-8.18570020341661,12.2,6.66292256646165));
#247586=CARTESIAN_POINT('Ctrl Pts',(-8.18914023404453,12.2,6.66471173239735));
#247587=CARTESIAN_POINT('Ctrl Pts',(-8.19262330516359,12.2,6.66651136899997));
#247588=CARTESIAN_POINT('Ctrl Pts',(-8.19614910871825,12.2,6.66832084802579));
#247589=CARTESIAN_POINT('Ctrl Pts',(-8.19967491227291,12.2,6.67013032705162));
#247590=CARTESIAN_POINT('Ctrl Pts',(-8.20324345005308,12.2,6.6719496470672));
#247591=CARTESIAN_POINT('Ctrl Pts',(-8.20685441958671,12.2,6.67377819116703));
#247592=CARTESIAN_POINT('Ctrl Pts',(-8.20986356097406,12.2,6.67530197797225));
#247593=CARTESIAN_POINT('Ctrl Pts',(-8.21290216901772,12.2,6.6768321706943));
#247594=CARTESIAN_POINT('Ctrl Pts',(-8.21597007276618,12.2,6.6783684191662));
#247595=CARTESIAN_POINT('Ctrl Pts',(-8.21903797651465,12.2,6.6799046676381));
#247596=CARTESIAN_POINT('Ctrl Pts',(-8.22213517478972,12.2,6.68144697153656));
#247597=CARTESIAN_POINT('Ctrl Pts',(-8.22526149549828,12.2,6.68299498751579));
#247598=CARTESIAN_POINT('Ctrl Pts',(-8.22838781620684,12.2,6.68454300349503));
#247599=CARTESIAN_POINT('Ctrl Pts',(-8.23154326289995,12.2,6.68609673124996));
#247600=CARTESIAN_POINT('Ctrl Pts',(-8.23472766269165,12.2,6.68765583249997));
#247601=CARTESIAN_POINT('Ctrl Pts',(-8.23791206248333,12.2,6.68921493374999));
#247602=CARTESIAN_POINT('Ctrl Pts',(-8.24112541823138,12.2,6.6907794107159));
#247603=CARTESIAN_POINT('Ctrl Pts',(-8.24436756046842,12.2,6.69234892850083));
#247604=CARTESIAN_POINT('Ctrl Pts',(-8.24760970270545,12.2,6.69391844628575));
#247605=CARTESIAN_POINT('Ctrl Pts',(-8.25088063221447,12.2,6.69549300605304));
#247606=CARTESIAN_POINT('Ctrl Pts',(-8.25418018346594,12.2,6.69707228209495));
#247607=CARTESIAN_POINT('Ctrl Pts',(-8.25747973471739,12.2,6.69865155813684));
#247608=CARTESIAN_POINT('Ctrl Pts',(-8.26080790682374,12.2,6.70023554983142));
#247609=CARTESIAN_POINT('Ctrl Pts',(-8.26416453647801,12.2,6.70182393684555));
#247610=CARTESIAN_POINT('Ctrl Pts',(-8.26752116613229,12.2,6.70341232385966));
#247611=CARTESIAN_POINT('Ctrl Pts',(-8.27090625118495,12.2,6.70500510523308));
#247612=CARTESIAN_POINT('Ctrl Pts',(-8.27431963191299,12.2,6.70660196816036));
#247613=CARTESIAN_POINT('Ctrl Pts',(-8.27773301264105,12.2,6.70819883108764));
#247614=CARTESIAN_POINT('Ctrl Pts',(-8.28117468674043,12.2,6.70979977275957));
#247615=CARTESIAN_POINT('Ctrl Pts',(-8.28464449243718,12.2,6.71140448567654));
#247616=CARTESIAN_POINT('Ctrl Pts',(-8.28811429813392,12.2,6.71300919859351));
#247617=CARTESIAN_POINT('Ctrl Pts',(-8.2916122377867,12.2,6.71461768115499));
#247618=CARTESIAN_POINT('Ctrl Pts',(-8.29513814771951,12.2,6.71622962921083));
#247619=CARTESIAN_POINT('Ctrl Pts',(-8.29866405726801,12.2,6.71784157709094));
#247620=CARTESIAN_POINT('Ctrl Pts',(-8.3022179412742,12.2,6.71945699038162));
#247621=CARTESIAN_POINT('Ctrl Pts',(-8.30579963650651,12.2,6.72107556978827));
#247622=CARTESIAN_POINT('Ctrl Pts',(-8.30938133212924,12.2,6.72269414937134));
#247623=CARTESIAN_POINT('Ctrl Pts',(-8.3129908415932,12.2,6.72431589348772));
#247624=CARTESIAN_POINT('Ctrl Pts',(-8.31662800700758,12.2,6.72594050827915));
#247625=CARTESIAN_POINT('Ctrl Pts',(-8.32099260574272,12.2,6.7278900461351));
#247626=CARTESIAN_POINT('Ctrl Pts',(-8.32539702749008,12.2,6.72984371952484));
#247627=CARTESIAN_POINT('Ctrl Pts',(-8.32984100348402,12.2,6.73180102438167));
#247628=CARTESIAN_POINT('Ctrl Pts',(-8.33354431661046,12.2,6.73343211167347));
#247629=CARTESIAN_POINT('Ctrl Pts',(-8.33727509821339,12.2,6.7350657214969));
#247630=CARTESIAN_POINT('Ctrl Pts',(-8.34103319319468,12.2,6.73670157123155));
#247631=CARTESIAN_POINT('Ctrl Pts',(-8.34479128817596,12.2,6.73833742096621));
#247632=CARTESIAN_POINT('Ctrl Pts',(-8.34857669656313,12.2,6.73997550786434));
#247633=CARTESIAN_POINT('Ctrl Pts',(-8.35238926323202,12.2,6.7416155534895));
#247634=CARTESIAN_POINT('Ctrl Pts',(-8.35543931631778,12.2,6.74292758988237));
#247635=CARTESIAN_POINT('Ctrl Pts',(-8.35850675374851,12.2,6.74424087936118));
#247636=CARTESIAN_POINT('Ctrl Pts',(-8.36159149277297,12.2,6.74555528114254));
#247637=CARTESIAN_POINT('Ctrl Pts',(-8.36467623221773,12.2,6.74686968310298));
#247638=CARTESIAN_POINT('Ctrl Pts',(-8.36777827644761,12.2,6.74818519751453));
#247639=CARTESIAN_POINT('Ctrl Pts',(-8.37089754721938,12.2,6.74950168420768));
#247640=CARTESIAN_POINT('Ctrl Pts',(-8.37401681756615,12.2,6.75081817072147));
#247641=CARTESIAN_POINT('Ctrl Pts',(-8.37715331341794,12.2,6.75213562919726));
#247642=CARTESIAN_POINT('Ctrl Pts',(-8.38030695782567,12.2,6.75345392236722));
#247643=CARTESIAN_POINT('Ctrl Pts',(-8.38346060266309,12.2,6.75477221571679));
#247644=CARTESIAN_POINT('Ctrl Pts',(-8.38663139731092,12.2,6.7560913438637));
#247645=CARTESIAN_POINT('Ctrl Pts',(-8.38981926331909,12.2,6.75741116982455));
#247646=CARTESIAN_POINT('Ctrl Pts',(-8.39300712889291,12.2,6.75873099560558));
#247647=CARTESIAN_POINT('Ctrl Pts',(-8.3962120667809,12.2,6.76005152021978));
#247648=CARTESIAN_POINT('Ctrl Pts',(-8.3994340005659,12.2,6.76137260756663));
#247649=CARTESIAN_POINT('Ctrl Pts',(-8.40265593478988,12.2,6.76269369509347));
#247650=CARTESIAN_POINT('Ctrl Pts',(-8.40589486450167,12.2,6.76401534691654));
#247651=CARTESIAN_POINT('Ctrl Pts',(-8.40915071329132,12.2,6.76533742959974));
#247652=CARTESIAN_POINT('Ctrl Pts',(-8.41240656163736,12.2,6.76665951210279));
#247653=CARTESIAN_POINT('Ctrl Pts',(-8.41567933019394,12.2,6.76798202541133));
#247654=CARTESIAN_POINT('Ctrl Pts',(-8.41896894247882,12.2,6.76930483802538));
#247655=CARTESIAN_POINT('Ctrl Pts',(-8.42225855521192,12.2,6.77062765081966));
#247656=CARTESIAN_POINT('Ctrl Pts',(-8.42556501193377,12.2,6.77195076375331));
#247657=CARTESIAN_POINT('Ctrl Pts',(-8.42888823801892,12.2,6.77327404577588));
#247658=CARTESIAN_POINT('Ctrl Pts',(-8.43221146365128,12.2,6.77459732761816));
#247659=CARTESIAN_POINT('Ctrl Pts',(-8.43555145857452,12.2,6.77592077954181));
#247660=CARTESIAN_POINT('Ctrl Pts',(-8.43890814624284,12.2,6.77724427276693));
#247661=CARTESIAN_POINT('Ctrl Pts',(-8.44226483436849,12.2,6.77856776617238));
#247662=CARTESIAN_POINT('Ctrl Pts',(-8.44563821710689,12.2,6.77989130153064));
#247663=CARTESIAN_POINT('Ctrl Pts',(-8.44902821979165,12.2,6.78121475099165));
#247664=CARTESIAN_POINT('Ctrl Pts',(-8.45241822247642,12.2,6.78253820045268));
#247665=CARTESIAN_POINT('Ctrl Pts',(-8.455824844552,12.2,6.78386156533035));
#247666=CARTESIAN_POINT('Ctrl Pts',(-8.45924801201803,12.2,6.78518471945799));
#247667=CARTESIAN_POINT('Ctrl Pts',(-8.46267117901766,12.2,6.78650787340536));
#247668=CARTESIAN_POINT('Ctrl Pts',(-8.46611089233953,12.2,6.78783081555953));
#247669=CARTESIAN_POINT('Ctrl Pts',(-8.46956707723931,12.2,6.78915342595742));
#247670=CARTESIAN_POINT('Ctrl Pts',(-8.47302326261,12.2,6.79047603653552));
#247671=CARTESIAN_POINT('Ctrl Pts',(-8.47649591952865,12.2,6.7917983109969));
#247672=CARTESIAN_POINT('Ctrl Pts',(-8.4799849750538,12.2,6.79312013045777));
#247673=CARTESIAN_POINT('Ctrl Pts',(-8.48347403010358,12.2,6.79444194973855));
#247674=CARTESIAN_POINT('Ctrl Pts',(-8.48697948512065,12.2,6.79576331253883));
#247675=CARTESIAN_POINT('Ctrl Pts',(-8.49050126422058,12.2,6.79708409787534));
#247676=CARTESIAN_POINT('Ctrl Pts',(-8.49402304380035,12.2,6.79840488339181));
#247677=CARTESIAN_POINT('Ctrl Pts',(-8.49756114951816,12.2,6.79972509047035));
#247678=CARTESIAN_POINT('Ctrl Pts',(-8.50111550905751,12.2,6.80104460194146));
#247679=CARTESIAN_POINT('Ctrl Pts',(-8.50466986811258,12.2,6.80236411323277));
#247680=CARTESIAN_POINT('Ctrl Pts',(-8.50824047944563,12.2,6.80368292767492));
#247681=CARTESIAN_POINT('Ctrl Pts',(-8.51182727170693,12.2,6.80500092640057));
#247682=CARTESIAN_POINT('Ctrl Pts',(-8.51541406445691,12.2,6.80631892530578));
#247683=CARTESIAN_POINT('Ctrl Pts',(-8.51901703872827,12.2,6.80763610999146));
#247684=CARTESIAN_POINT('Ctrl Pts',(-8.52263612153768,12.2,6.80895236284092));
#247685=CARTESIAN_POINT('Ctrl Pts',(-8.52625520385399,12.2,6.81026861551103));
#247686=CARTESIAN_POINT('Ctrl Pts',(-8.52989039448496,12.2,6.81158393445375));
#247687=CARTESIAN_POINT('Ctrl Pts',(-8.53354162297859,12.2,6.81289820780094));
#247688=CARTESIAN_POINT('Ctrl Pts',(-8.53810565896874,12.2,6.81454104961924));
#247689=CARTESIAN_POINT('Ctrl Pts',(-8.54269475415526,12.2,6.8161822551149));
#247690=CARTESIAN_POINT('Ctrl Pts',(-8.54730876672338,12.2,6.81782160039276));
#247691=CARTESIAN_POINT('Ctrl Pts',(-8.55099997697905,12.2,6.81913307668653));
#247692=CARTESIAN_POINT('Ctrl Pts',(-8.55470713661169,12.2,6.82044336419962));
#247693=CARTESIAN_POINT('Ctrl Pts',(-8.55843017337117,12.2,6.82175234788199));
#247694=CARTESIAN_POINT('Ctrl Pts',(-8.56215320962339,12.2,6.823061331386));
#247695=CARTESIAN_POINT('Ctrl Pts',(-8.56589212223155,12.2,6.82436901362683));
#247696=CARTESIAN_POINT('Ctrl Pts',(-8.56964684322191,12.2,6.82567528108543));
#247697=CARTESIAN_POINT('Ctrl Pts',(-8.57340156472385,12.2,6.826981548722));
#247698=CARTESIAN_POINT('Ctrl Pts',(-8.5771720910773,12.2,6.82828640220504));
#247699=CARTESIAN_POINT('Ctrl Pts',(-8.58095835578467,12.2,6.82958973233152));
#247700=CARTESIAN_POINT('Ctrl Pts',(-8.58474461997617,12.2,6.83089306228044));
#247701=CARTESIAN_POINT('Ctrl Pts',(-8.5885466186145,12.2,6.83219486754353));
#247702=CARTESIAN_POINT('Ctrl Pts',(-8.59236428613413,12.2,6.83349503977074));
#247703=CARTESIAN_POINT('Ctrl Pts',(-8.59618195417391,12.2,6.83479521217509));
#247704=CARTESIAN_POINT('Ctrl Pts',(-8.60001528748467,12.2,6.83609375163766));
#247705=CARTESIAN_POINT('Ctrl Pts',(-8.60386421824999,12.2,6.83739055054166));
#247706=CARTESIAN_POINT('Ctrl Pts',(-8.60771314901532,12.2,6.83868734944567));
#247707=CARTESIAN_POINT('Ctrl Pts',(-8.61157767611857,12.2,6.83998240684948));
#247708=CARTESIAN_POINT('Ctrl Pts',(-8.61545773160939,12.2,6.8412756177531));
#247709=CARTESIAN_POINT('Ctrl Pts',(-8.61933778657157,12.2,6.84256882848053));
#247710=CARTESIAN_POINT('Ctrl Pts',(-8.62323336839101,12.2,6.84386019109311));
#247711=CARTESIAN_POINT('Ctrl Pts',(-8.62714440925567,12.2,6.84514960121578));
#247712=CARTESIAN_POINT('Ctrl Pts',(-8.6310554506532,12.2,6.84643901151414));
#247713=CARTESIAN_POINT('Ctrl Pts',(-8.63498194995588,12.2,6.84772646893476));
#247714=CARTESIAN_POINT('Ctrl Pts',(-8.6389238393945,12.2,6.84901186922683));
#247715=CARTESIAN_POINT('Ctrl Pts',(-8.64286572829605,12.2,6.85029726934376));
#247716=CARTESIAN_POINT('Ctrl Pts',(-8.6468230057178,12.2,6.85158061243038));
#247717=CARTESIAN_POINT('Ctrl Pts',(-8.65079560472538,12.2,6.85286179460357));
#247718=CARTESIAN_POINT('Ctrl Pts',(-8.65675450350738,12.2,6.85478356795062));
#247719=CARTESIAN_POINT('Ctrl Pts',(-8.66274787400597,12.2,6.85670048076072));
#247720=CARTESIAN_POINT('Ctrl Pts',(-8.66877548753467,12.2,6.85861218802495));
#247721=CARTESIAN_POINT('Ctrl Pts',(-8.67279389691878,12.2,6.8598866596502));
#247722=CARTESIAN_POINT('Ctrl Pts',(-8.67682752481266,12.2,6.86115881768079));
#247723=CARTESIAN_POINT('Ctrl Pts',(-8.68087630303333,12.2,6.86242856275));
#247724=CARTESIAN_POINT('Ctrl Pts',(-8.684925081254,12.2,6.86369830781921));
#247725=CARTESIAN_POINT('Ctrl Pts',(-8.68898900988754,12.2,6.86496563867979));
#247726=CARTESIAN_POINT('Ctrl Pts',(-8.69306802266692,12.2,6.86623045691512));
#247727=CARTESIAN_POINT('Ctrl Pts',(-8.6981667878075,12.2,6.86781147945079));
#247728=CARTESIAN_POINT('Ctrl Pts',(-8.70328911886753,12.2,6.86938857400426));
#247729=CARTESIAN_POINT('Ctrl Pts',(-8.70843488656861,12.2,6.87096155077758));
#247730=CARTESIAN_POINT('Ctrl Pts',(-8.71255150140253,12.2,6.87221993240198));
#247731=CARTESIAN_POINT('Ctrl Pts',(-8.71668311509067,12.2,6.87347567662893));
#247732=CARTESIAN_POINT('Ctrl Pts',(-8.72082965998333,12.2,6.874728688975));
#247733=CARTESIAN_POINT('Ctrl Pts',(-8.72497620487598,12.2,6.87598170132107));
#247734=CARTESIAN_POINT('Ctrl Pts',(-8.72913768329261,12.2,6.87723197950015));
#247735=CARTESIAN_POINT('Ctrl Pts',(-8.73331402496617,12.2,6.87847942917895));
#247736=CARTESIAN_POINT('Ctrl Pts',(-8.7374903660707,12.2,6.87972687868779));
#247737=CARTESIAN_POINT('Ctrl Pts',(-8.74168157364137,12.2,6.88097149896723));
#247738=CARTESIAN_POINT('Ctrl Pts',(-8.7458875780388,12.2,6.88221319398248));
#247739=CARTESIAN_POINT('Ctrl Pts',(-8.75009358300931,12.2,6.88345488916692));
#247740=CARTESIAN_POINT('Ctrl Pts',(-8.75431438812685,12.2,6.88469366063778));
#247741=CARTESIAN_POINT('Ctrl Pts',(-8.75854992369252,12.2,6.88592941242704));
#247742=CARTESIAN_POINT('Ctrl Pts',(-8.7627854586811,12.2,6.88716516404793));
#247743=CARTESIAN_POINT('Ctrl Pts',(-8.76703572543441,12.2,6.88839789813865));
#247744=CARTESIAN_POINT('Ctrl Pts',(-8.77130065841814,12.2,6.88962751914945));
#247745=CARTESIAN_POINT('Ctrl Pts',(-8.77449935830122,12.2,6.89054973494943));
#247746=CARTESIAN_POINT('Ctrl Pts',(-8.77770630790183,12.2,6.89147020104284));
#247747=CARTESIAN_POINT('Ctrl Pts',(-8.78092147940302,12.2,6.89238887734724));
#247748=CARTESIAN_POINT('Ctrl Pts',(-8.78413665090421,12.2,6.89330755365163));
#247749=CARTESIAN_POINT('Ctrl Pts',(-8.7873600437474,12.2,6.89422444030018));
#247750=CARTESIAN_POINT('Ctrl Pts',(-8.79059163058719,12.2,6.89513949905885));
#247751=CARTESIAN_POINT('Ctrl Pts',(-8.79382321801404,12.2,6.89605455798375));
#247752=CARTESIAN_POINT('Ctrl Pts',(-8.79706299878493,12.2,6.89696778864981));
#247753=CARTESIAN_POINT('Ctrl Pts',(-8.8003109467164,12.2,6.89787915219867));
#247754=CARTESIAN_POINT('Ctrl Pts',(-8.80355889405783,12.2,6.89879051558197));
#247755=CARTESIAN_POINT('Ctrl Pts',(-8.80681500719049,12.2,6.89970001401537));
#247756=CARTESIAN_POINT('Ctrl Pts',(-8.81007925907261,12.2,6.90060760681556));
#247757=CARTESIAN_POINT('Ctrl Pts',(-8.81443159471776,12.2,6.90181773049419));
#247758=CARTESIAN_POINT('Ctrl Pts',(-8.81879839991876,12.2,6.90302446882722));
#247759=CARTESIAN_POINT('Ctrl Pts',(-8.82317960838934,12.2,6.90422773006705));
#247760=CARTESIAN_POINT('Ctrl Pts',(-8.82646551489151,12.2,6.9051301760379));
#247761=CARTESIAN_POINT('Ctrl Pts',(-8.82975952216789,12.2,6.90603066868649));
#247762=CARTESIAN_POINT('Ctrl Pts',(-8.83306160504682,12.2,6.90692916757079));
#247763=CARTESIAN_POINT('Ctrl Pts',(-8.83636368852561,12.2,6.90782766661832));
#247764=CARTESIAN_POINT('Ctrl Pts',(-8.8396738473567,12.2,6.90872417389861));
#247765=CARTESIAN_POINT('Ctrl Pts',(-8.84299205196505,12.2,6.90961865094499));
#247766=CARTESIAN_POINT('Ctrl Pts',(-8.8463102559706,12.2,6.91051312782888));
#247767=CARTESIAN_POINT('Ctrl Pts',(-8.84963650810069,12.2,6.91140557597954));
#247768=CARTESIAN_POINT('Ctrl Pts',(-8.85297077910524,12.2,6.91229595682202));
#247769=CARTESIAN_POINT('Ctrl Pts',(-8.85630505010979,12.2,6.91318633766449));
#247770=CARTESIAN_POINT('Ctrl Pts',(-8.85964734252618,12.2,6.91407465199566));
#247771=CARTESIAN_POINT('Ctrl Pts',(-8.86299762600305,12.2,6.91496086371747));
#247772=CARTESIAN_POINT('Ctrl Pts',(-8.86634790947992,12.2,6.91584707543929));
#247773=CARTESIAN_POINT('Ctrl Pts',(-8.86970618638733,12.2,6.91673118347723));
#247774=CARTESIAN_POINT('Ctrl Pts',(-8.87307242828028,12.2,6.91761315228253));
#247775=CARTESIAN_POINT('Ctrl Pts',(-8.87643867017324,12.2,6.91849512108784));
#247776=CARTESIAN_POINT('Ctrl Pts',(-8.87981287722173,12.2,6.91937495131933));
#247777=CARTESIAN_POINT('Ctrl Pts',(-8.88319502263981,12.2,6.92025260516263));
#247778=CARTESIAN_POINT('Ctrl Pts',(-8.88657716805789,12.2,6.92113025900594));
#247779=CARTESIAN_POINT('Ctrl Pts',(-8.88996725261712,12.2,6.92200573684105));
#247780=CARTESIAN_POINT('Ctrl Pts',(-8.89336524753424,12.2,6.92287900451796));
#247781=CARTESIAN_POINT('Ctrl Pts',(-8.89676324306866,12.2,6.9237522723535));
#247782=CARTESIAN_POINT('Ctrl Pts',(-8.900169149947,12.2,6.9246233273301));
#247783=CARTESIAN_POINT('Ctrl Pts',(-8.90358294052755,12.2,6.92549213670606));
#247784=CARTESIAN_POINT('Ctrl Pts',(-8.90927259004805,12.2,6.92694015196439));
#247785=CARTESIAN_POINT('Ctrl Pts',(-8.91498414095459,12.2,6.92838192553484));
#247786=CARTESIAN_POINT('Ctrl Pts',(-8.92071746775843,12.2,6.92981729433725));
#247787=CARTESIAN_POINT('Ctrl Pts',(-8.9253041299514,12.2,6.93096558956692));
#247788=CARTESIAN_POINT('Ctrl Pts',(-8.92990472886795,12.2,6.93210978655176));
#247789=CARTESIAN_POINT('Ctrl Pts',(-8.93451920050833,12.2,6.93324980122501));
#247790=CARTESIAN_POINT('Ctrl Pts',(-8.93798005392426,12.2,6.93410481215228));
#247791=CARTESIAN_POINT('Ctrl Pts',(-8.94144871094819,12.2,6.9349574722713));
#247792=CARTESIAN_POINT('Ctrl Pts',(-8.94492514486286,12.2,6.93580774515728));
#247793=CARTESIAN_POINT('Ctrl Pts',(-8.94840157877754,12.2,6.93665801804326));
#247794=CARTESIAN_POINT('Ctrl Pts',(-8.95188578955003,12.2,6.93750590492941));
#247795=CARTESIAN_POINT('Ctrl Pts',(-8.95537775042209,12.2,6.93835137031569));
#247796=CARTESIAN_POINT('Ctrl Pts',(-8.95886971192853,12.2,6.93919683585556));
#247797=CARTESIAN_POINT('Ctrl Pts',(-8.96236942320384,12.2,6.94003988067809));
#247798=CARTESIAN_POINT('Ctrl Pts',(-8.9658768582563,12.2,6.94088047117491));
#247799=CARTESIAN_POINT('Ctrl Pts',(-8.96938429267157,12.2,6.94172106151903));
#247800=CARTESIAN_POINT('Ctrl Pts',(-8.97289945198276,12.2,6.94255919716723));
#247801=CARTESIAN_POINT('Ctrl Pts',(-8.97642230665666,12.2,6.94339484363665));
#247802=CARTESIAN_POINT('Ctrl Pts',(-8.98111944600853,12.2,6.94450903887863));
#247803=CARTESIAN_POINT('Ctrl Pts',(-8.98583026972047,12.2,6.94561881087745));
#247804=CARTESIAN_POINT('Ctrl Pts',(-8.99055471338891,12.2,6.94672407867627));
#247805=CARTESIAN_POINT('Ctrl Pts',(-8.99409804630116,12.2,6.94755302956303));
#247806=CARTESIAN_POINT('Ctrl Pts',(-8.99764904130456,12.2,6.94837944809998));
#247807=CARTESIAN_POINT('Ctrl Pts',(-9.00120767071589,12.2,6.9492032990704));
#247808=CARTESIAN_POINT('Ctrl Pts',(-9.00476630077371,12.2,6.95002715019049));
#247809=CARTESIAN_POINT('Ctrl Pts',(-9.00833256554203,12.2,6.95084843592652));
#247810=CARTESIAN_POINT('Ctrl Pts',(-9.01190644002079,12.2,6.95166712192015));
#247811=CARTESIAN_POINT('Ctrl Pts',(-9.0154803138503,12.2,6.95248580776504));
#247812=CARTESIAN_POINT('Ctrl Pts',(-9.01906179642801,12.2,6.95330189349657));
#247813=CARTESIAN_POINT('Ctrl Pts',(-9.02265086143614,12.2,6.95411534742403));
#247814=CARTESIAN_POINT('Ctrl Pts',(-9.02623992644427,12.2,6.95492880135148));
#247815=CARTESIAN_POINT('Ctrl Pts',(-9.02983657278995,12.2,6.95573962360097));
#247816=CARTESIAN_POINT('Ctrl Pts',(-9.03344077565966,12.2,6.95654778007138));
#247817=CARTESIAN_POINT('Ctrl Pts',(-9.03704497852936,12.2,6.95735593654179));
#247818=CARTESIAN_POINT('Ctrl Pts',(-9.04065673763151,12.2,6.95816142856251));
#247819=CARTESIAN_POINT('Ctrl Pts',(-9.044276027,12.2,6.95896422395001));
#247820=CARTESIAN_POINT('Ctrl Pts',(-9.04789531636849,12.2,6.9597670193375));
#247821=CARTESIAN_POINT('Ctrl Pts',(-9.05152213552004,12.2,6.96056711882511));
#247822=CARTESIAN_POINT('Ctrl Pts',(-9.05515645934565,12.2,6.96136448871304));
#247823=CARTESIAN_POINT('Ctrl Pts',(-9.05879078317127,12.2,6.96216185860098));
#247824=CARTESIAN_POINT('Ctrl Pts',(-9.06243261079517,12.2,6.96295650025233));
#247825=CARTESIAN_POINT('Ctrl Pts',(-9.06608191530235,12.2,6.96374838013843));
#247826=CARTESIAN_POINT('Ctrl Pts',(-9.06973121980953,12.2,6.96454026002454));
#247827=CARTESIAN_POINT('Ctrl Pts',(-9.07338799986868,12.2,6.96532937690677));
#247828=CARTESIAN_POINT('Ctrl Pts',(-9.07705223219287,12.2,6.96611570133692));
#247829=CARTESIAN_POINT('Ctrl Pts',(-9.08071646518273,12.2,6.96690202590991));
#247830=CARTESIAN_POINT('Ctrl Pts',(-9.08438814868303,12.2,6.96768555725712));
#247831=CARTESIAN_POINT('Ctrl Pts',(-9.08806725980206,12.2,6.9684662673702));
#247832=CARTESIAN_POINT('Ctrl Pts',(-9.09174637025272,12.2,6.96924697734145));
#247833=CARTESIAN_POINT('Ctrl Pts',(-9.09543291006968,12.2,6.97002486752951));
#247834=CARTESIAN_POINT('Ctrl Pts',(-9.0991268494361,12.2,6.97079990333443));
#247835=CARTESIAN_POINT('Ctrl Pts',(-9.10282078880253,12.2,6.97157493913936));
#247836=CARTESIAN_POINT('Ctrl Pts',(-9.10652212867126,12.2,6.97234712124184));
#247837=CARTESIAN_POINT('Ctrl Pts',(-9.11023083701171,12.2,6.9731164105507));
#247838=CARTESIAN_POINT('Ctrl Pts',(-9.11641201780371,12.2,6.97439855944539));
#247839=CARTESIAN_POINT('Ctrl Pts',(-9.12261365747818,12.2,6.97567266250236));
#247840=CARTESIAN_POINT('Ctrl Pts',(-9.1288356732116,12.2,6.97693862333241));
#247841=CARTESIAN_POINT('Ctrl Pts',(-9.13256888251601,12.2,6.97769819980284));
#247842=CARTESIAN_POINT('Ctrl Pts',(-9.13630942931919,12.2,6.97845485086305));
#247843=CARTESIAN_POINT('Ctrl Pts',(-9.14005731500006,12.2,6.97920857099999));
#247844=CARTESIAN_POINT('Ctrl Pts',(-9.36775917500006,15.2,6.67046385499999));
#247845=CARTESIAN_POINT('Ctrl Pts',(-9.36775917500006,11.6,6.67046385499999));
#247846=CARTESIAN_POINT('Ctrl Pts',(-9.36739373000006,15.2,6.66979226099999));
#247847=CARTESIAN_POINT('Ctrl Pts',(-9.36739373000006,11.6,6.66979226099999));
#247848=CARTESIAN_POINT('Ctrl Pts',(-9.36666279600006,15.2,6.66844959699999));
#247849=CARTESIAN_POINT('Ctrl Pts',(-9.36666279600006,11.6,6.66844959699999));
#247850=CARTESIAN_POINT('Ctrl Pts',(-9.36556627000006,15.2,6.66643717599998));
#247851=CARTESIAN_POINT('Ctrl Pts',(-9.36556627000006,11.6,6.66643717599998));
#247852=CARTESIAN_POINT('Ctrl Pts',(-9.36410398400006,15.2,6.66375709899999));
#247853=CARTESIAN_POINT('Ctrl Pts',(-9.36410398400006,11.6,6.66375709899999));
#247854=CARTESIAN_POINT('Ctrl Pts',(-9.36227570600006,15.2,6.66041225199999));
#247855=CARTESIAN_POINT('Ctrl Pts',(-9.36227570600006,11.6,6.66041225199999));
#247856=CARTESIAN_POINT('Ctrl Pts',(-9.36044701000006,15.2,6.65707265499999));
#247857=CARTESIAN_POINT('Ctrl Pts',(-9.36044701000006,11.6,6.65707265499999));
#247858=CARTESIAN_POINT('Ctrl Pts',(-9.35861789700006,15.2,6.65373830999999));
#247859=CARTESIAN_POINT('Ctrl Pts',(-9.35861789700006,11.6,6.65373830999999));
#247860=CARTESIAN_POINT('Ctrl Pts',(-9.35678837100006,15.2,6.65040921899998));
#247861=CARTESIAN_POINT('Ctrl Pts',(-9.35678837100006,11.6,6.65040921899998));
#247862=CARTESIAN_POINT('Ctrl Pts',(-9.35495843800006,15.2,6.64708538399999));
#247863=CARTESIAN_POINT('Ctrl Pts',(-9.35495843800006,11.6,6.64708538399999));
#247864=CARTESIAN_POINT('Ctrl Pts',(-9.35312810400006,15.2,6.64376680699998));
#247865=CARTESIAN_POINT('Ctrl Pts',(-9.35312810400006,11.6,6.64376680699998));
#247866=CARTESIAN_POINT('Ctrl Pts',(-9.35129738000006,15.2,6.64045349299998));
#247867=CARTESIAN_POINT('Ctrl Pts',(-9.35129738000006,11.6,6.64045349299998));
#247868=CARTESIAN_POINT('Ctrl Pts',(-9.34946627400006,15.2,6.63714544599999));
#247869=CARTESIAN_POINT('Ctrl Pts',(-9.34946627400006,11.6,6.63714544599999));
#247870=CARTESIAN_POINT('Ctrl Pts',(-9.34763479800005,15.2,6.63384267099998));
#247871=CARTESIAN_POINT('Ctrl Pts',(-9.34763479800005,11.6,6.63384267099998));
#247872=CARTESIAN_POINT('Ctrl Pts',(-9.34580296100006,15.2,6.63054516999999));
#247873=CARTESIAN_POINT('Ctrl Pts',(-9.34580296100006,11.6,6.63054516999999));
#247874=CARTESIAN_POINT('Ctrl Pts',(-9.34397077300006,15.2,6.62725294899998));
#247875=CARTESIAN_POINT('Ctrl Pts',(-9.34397077300006,11.6,6.62725294899998));
#247876=CARTESIAN_POINT('Ctrl Pts',(-9.34213824300006,15.2,6.62396601199998));
#247877=CARTESIAN_POINT('Ctrl Pts',(-9.34213824300006,11.6,6.62396601199998));
#247878=CARTESIAN_POINT('Ctrl Pts',(-9.34030538000006,15.2,6.62068435999998));
#247879=CARTESIAN_POINT('Ctrl Pts',(-9.34030538000006,11.6,6.62068435999998));
#247880=CARTESIAN_POINT('Ctrl Pts',(-9.33847218900006,15.2,6.61740799699999));
#247881=CARTESIAN_POINT('Ctrl Pts',(-9.33847218900006,11.6,6.61740799699999));
#247882=CARTESIAN_POINT('Ctrl Pts',(-9.33663868100006,15.2,6.61413692899998));
#247883=CARTESIAN_POINT('Ctrl Pts',(-9.33663868100006,11.6,6.61413692899998));
#247884=CARTESIAN_POINT('Ctrl Pts',(-9.33480486000006,15.2,6.61087115499999));
#247885=CARTESIAN_POINT('Ctrl Pts',(-9.33480486000006,11.6,6.61087115499999));
#247886=CARTESIAN_POINT('Ctrl Pts',(-9.33297073500006,15.2,6.60761067999999));
#247887=CARTESIAN_POINT('Ctrl Pts',(-9.33297073500006,11.6,6.60761067999999));
#247888=CARTESIAN_POINT('Ctrl Pts',(-9.33113631600006,15.2,6.60435550799999));
#247889=CARTESIAN_POINT('Ctrl Pts',(-9.33113631600006,11.6,6.60435550799999));
#247890=CARTESIAN_POINT('Ctrl Pts',(-9.32930160900005,15.2,6.60110564199999));
#247891=CARTESIAN_POINT('Ctrl Pts',(-9.32930160900005,11.6,6.60110564199999));
#247892=CARTESIAN_POINT('Ctrl Pts',(-9.32746662500006,15.2,6.59786108599998));
#247893=CARTESIAN_POINT('Ctrl Pts',(-9.32746662500006,11.6,6.59786108599998));
#247894=CARTESIAN_POINT('Ctrl Pts',(-9.32563137200006,15.2,6.59462184199998));
#247895=CARTESIAN_POINT('Ctrl Pts',(-9.32563137200006,11.6,6.59462184199998));
#247896=CARTESIAN_POINT('Ctrl Pts',(-9.32379585900006,15.2,6.59138791599998));
#247897=CARTESIAN_POINT('Ctrl Pts',(-9.32379585900006,11.6,6.59138791599998));
#247898=CARTESIAN_POINT('Ctrl Pts',(-9.32196009400006,15.2,6.58815930999998));
#247899=CARTESIAN_POINT('Ctrl Pts',(-9.32196009400006,11.6,6.58815930999998));
#247900=CARTESIAN_POINT('Ctrl Pts',(-9.32012408700006,15.2,6.58493602799999));
#247901=CARTESIAN_POINT('Ctrl Pts',(-9.32012408700006,11.6,6.58493602799999));
#247902=CARTESIAN_POINT('Ctrl Pts',(-9.31828784500006,15.2,6.58171807199999));
#247903=CARTESIAN_POINT('Ctrl Pts',(-9.31828784500006,11.6,6.58171807199999));
#247904=CARTESIAN_POINT('Ctrl Pts',(-9.31645137600006,15.2,6.57850544799999));
#247905=CARTESIAN_POINT('Ctrl Pts',(-9.31645137600006,11.6,6.57850544799999));
#247906=CARTESIAN_POINT('Ctrl Pts',(-9.31461469100006,15.2,6.57529815699998));
#247907=CARTESIAN_POINT('Ctrl Pts',(-9.31461469100006,11.6,6.57529815699998));
#247908=CARTESIAN_POINT('Ctrl Pts',(-9.31277779500006,15.2,6.57209620299999));
#247909=CARTESIAN_POINT('Ctrl Pts',(-9.31277779500006,11.6,6.57209620299999));
#247910=CARTESIAN_POINT('Ctrl Pts',(-9.31094070000006,15.2,6.56889958999999));
#247911=CARTESIAN_POINT('Ctrl Pts',(-9.31094070000006,11.6,6.56889958999999));
#247912=CARTESIAN_POINT('Ctrl Pts',(-9.30910341200006,15.2,6.56570832299998));
#247913=CARTESIAN_POINT('Ctrl Pts',(-9.30910341200006,11.6,6.56570832299998));
#247914=CARTESIAN_POINT('Ctrl Pts',(-9.30726594100006,15.2,6.56252240099998));
#247915=CARTESIAN_POINT('Ctrl Pts',(-9.30726594100006,11.6,6.56252240099998));
#247916=CARTESIAN_POINT('Ctrl Pts',(-9.30542829600006,15.2,6.55934183199999));
#247917=CARTESIAN_POINT('Ctrl Pts',(-9.30542829600006,11.6,6.55934183199999));
#247918=CARTESIAN_POINT('Ctrl Pts',(-9.30359048400006,15.2,6.55616661699998));
#247919=CARTESIAN_POINT('Ctrl Pts',(-9.30359048400006,11.6,6.55616661699998));
#247920=CARTESIAN_POINT('Ctrl Pts',(-9.30175251500006,15.2,6.55299675999998));
#247921=CARTESIAN_POINT('Ctrl Pts',(-9.30175251500006,11.6,6.55299675999998));
#247922=CARTESIAN_POINT('Ctrl Pts',(-9.29991439900006,15.2,6.54983226399998));
#247923=CARTESIAN_POINT('Ctrl Pts',(-9.29991439900006,11.6,6.54983226399998));
#247924=CARTESIAN_POINT('Ctrl Pts',(-9.29807614200006,15.2,6.54667313399998));
#247925=CARTESIAN_POINT('Ctrl Pts',(-9.29807614200006,11.6,6.54667313399998));
#247926=CARTESIAN_POINT('Ctrl Pts',(-9.29623775500006,15.2,6.54351937099998));
#247927=CARTESIAN_POINT('Ctrl Pts',(-9.29623775500006,11.6,6.54351937099998));
#247928=CARTESIAN_POINT('Ctrl Pts',(-9.29439924500005,15.2,6.54037098099998));
#247929=CARTESIAN_POINT('Ctrl Pts',(-9.29439924500005,11.6,6.54037098099998));
#247930=CARTESIAN_POINT('Ctrl Pts',(-9.29256062200006,15.2,6.53722796599999));
#247931=CARTESIAN_POINT('Ctrl Pts',(-9.29256062200006,11.6,6.53722796599999));
#247932=CARTESIAN_POINT('Ctrl Pts',(-9.29072189500006,15.2,6.53409032999999));
#247933=CARTESIAN_POINT('Ctrl Pts',(-9.29072189500006,11.6,6.53409032999999));
#247934=CARTESIAN_POINT('Ctrl Pts',(-9.28888307100006,15.2,6.53095807499999));
#247935=CARTESIAN_POINT('Ctrl Pts',(-9.28888307100006,11.6,6.53095807499999));
#247936=CARTESIAN_POINT('Ctrl Pts',(-9.28704416000006,15.2,6.52783120699999));
#247937=CARTESIAN_POINT('Ctrl Pts',(-9.28704416000006,11.6,6.52783120699999));
#247938=CARTESIAN_POINT('Ctrl Pts',(-9.28520517200005,15.2,6.52470972599998));
#247939=CARTESIAN_POINT('Ctrl Pts',(-9.28520517200005,11.6,6.52470972599998));
#247940=CARTESIAN_POINT('Ctrl Pts',(-9.28336611400006,15.2,6.52159363899998));
#247941=CARTESIAN_POINT('Ctrl Pts',(-9.28336611400006,11.6,6.52159363899998));
#247942=CARTESIAN_POINT('Ctrl Pts',(-9.28152699600006,15.2,6.51848294699998));
#247943=CARTESIAN_POINT('Ctrl Pts',(-9.28152699600006,11.6,6.51848294699998));
#247944=CARTESIAN_POINT('Ctrl Pts',(-9.27968782700006,15.2,6.51537765499998));
#247945=CARTESIAN_POINT('Ctrl Pts',(-9.27968782700006,11.6,6.51537765499998));
#247946=CARTESIAN_POINT('Ctrl Pts',(-9.27784861500006,15.2,6.51227776499999));
#247947=CARTESIAN_POINT('Ctrl Pts',(-9.27784861500006,11.6,6.51227776499999));
#247948=CARTESIAN_POINT('Ctrl Pts',(-9.27600936900006,15.2,6.50918328099999));
#247949=CARTESIAN_POINT('Ctrl Pts',(-9.27600936900006,11.6,6.50918328099999));
#247950=CARTESIAN_POINT('Ctrl Pts',(-9.27417010000006,15.2,6.50609420699999));
#247951=CARTESIAN_POINT('Ctrl Pts',(-9.27417010000006,11.6,6.50609420699999));
#247952=CARTESIAN_POINT('Ctrl Pts',(-9.27233081400006,15.2,6.50301054499998));
#247953=CARTESIAN_POINT('Ctrl Pts',(-9.27233081400006,11.6,6.50301054499998));
#247954=CARTESIAN_POINT('Ctrl Pts',(-9.27049152300006,15.2,6.49993229999998));
#247955=CARTESIAN_POINT('Ctrl Pts',(-9.27049152300006,11.6,6.49993229999998));
#247956=CARTESIAN_POINT('Ctrl Pts',(-9.26865223400006,15.2,6.49685947499999));
#247957=CARTESIAN_POINT('Ctrl Pts',(-9.26865223400006,11.6,6.49685947499999));
#247958=CARTESIAN_POINT('Ctrl Pts',(-9.26681295600006,15.2,6.49379207299998));
#247959=CARTESIAN_POINT('Ctrl Pts',(-9.26681295600006,11.6,6.49379207299998));
#247960=CARTESIAN_POINT('Ctrl Pts',(-9.26497369900006,15.2,6.49073009799999));
#247961=CARTESIAN_POINT('Ctrl Pts',(-9.26497369900006,11.6,6.49073009799999));
#247962=CARTESIAN_POINT('Ctrl Pts',(-9.26313447100006,15.2,6.48767355199999));
#247963=CARTESIAN_POINT('Ctrl Pts',(-9.26313447100006,11.6,6.48767355199999));
#247964=CARTESIAN_POINT('Ctrl Pts',(-9.26129528300006,15.2,6.48462243999998));
#247965=CARTESIAN_POINT('Ctrl Pts',(-9.26129528300006,11.6,6.48462243999998));
#247966=CARTESIAN_POINT('Ctrl Pts',(-9.25945614200005,15.2,6.48157676499999));
#247967=CARTESIAN_POINT('Ctrl Pts',(-9.25945614200005,11.6,6.48157676499999));
#247968=CARTESIAN_POINT('Ctrl Pts',(-9.25761705900005,15.2,6.47853652899999));
#247969=CARTESIAN_POINT('Ctrl Pts',(-9.25761705900005,11.6,6.47853652899999));
#247970=CARTESIAN_POINT('Ctrl Pts',(-9.25577804200006,15.2,6.47550173699998));
#247971=CARTESIAN_POINT('Ctrl Pts',(-9.25577804200006,11.6,6.47550173699998));
#247972=CARTESIAN_POINT('Ctrl Pts',(-9.25393910000006,15.2,6.47247239299999));
#247973=CARTESIAN_POINT('Ctrl Pts',(-9.25393910000006,11.6,6.47247239299999));
#247974=CARTESIAN_POINT('Ctrl Pts',(-9.25210024300006,15.2,6.46944849899998));
#247975=CARTESIAN_POINT('Ctrl Pts',(-9.25210024300006,11.6,6.46944849899998));
#247976=CARTESIAN_POINT('Ctrl Pts',(-9.25026148000006,15.2,6.46643005899998));
#247977=CARTESIAN_POINT('Ctrl Pts',(-9.25026148000006,11.6,6.46643005899998));
#247978=CARTESIAN_POINT('Ctrl Pts',(-9.24842281900006,15.2,6.46341707599999));
#247979=CARTESIAN_POINT('Ctrl Pts',(-9.24842281900006,11.6,6.46341707599999));
#247980=CARTESIAN_POINT('Ctrl Pts',(-9.24658427100006,15.2,6.46040955399998));
#247981=CARTESIAN_POINT('Ctrl Pts',(-9.24658427100006,11.6,6.46040955399998));
#247982=CARTESIAN_POINT('Ctrl Pts',(-9.24474584400006,15.2,6.45740749499998));
#247983=CARTESIAN_POINT('Ctrl Pts',(-9.24474584400006,11.6,6.45740749499998));
#247984=CARTESIAN_POINT('Ctrl Pts',(-9.24290754900005,15.2,6.45441090499999));
#247985=CARTESIAN_POINT('Ctrl Pts',(-9.24290754900005,11.6,6.45441090499999));
#247986=CARTESIAN_POINT('Ctrl Pts',(-9.24106939500006,15.2,6.45141978499999));
#247987=CARTESIAN_POINT('Ctrl Pts',(-9.24106939500006,11.6,6.45141978499999));
#247988=CARTESIAN_POINT('Ctrl Pts',(-9.23923138900006,15.2,6.44843413999999));
#247989=CARTESIAN_POINT('Ctrl Pts',(-9.23923138900006,11.6,6.44843413999999));
#247990=CARTESIAN_POINT('Ctrl Pts',(-9.23739354200006,15.2,6.44545397099999));
#247991=CARTESIAN_POINT('Ctrl Pts',(-9.23739354200006,11.6,6.44545397099999));
#247992=CARTESIAN_POINT('Ctrl Pts',(-9.23555586400006,15.2,6.44247928399999));
#247993=CARTESIAN_POINT('Ctrl Pts',(-9.23555586400006,11.6,6.44247928399999));
#247994=CARTESIAN_POINT('Ctrl Pts',(-9.23371836400005,15.2,6.43951008199998));
#247995=CARTESIAN_POINT('Ctrl Pts',(-9.23371836400005,11.6,6.43951008199998));
#247996=CARTESIAN_POINT('Ctrl Pts',(-9.23188105000006,15.2,6.43654636699999));
#247997=CARTESIAN_POINT('Ctrl Pts',(-9.23188105000006,11.6,6.43654636699999));
#247998=CARTESIAN_POINT('Ctrl Pts',(-9.23004393400005,15.2,6.43358814399999));
#247999=CARTESIAN_POINT('Ctrl Pts',(-9.23004393400005,11.6,6.43358814399999));
#248000=CARTESIAN_POINT('Ctrl Pts',(-9.22820702300006,15.2,6.43063541499998));
#248001=CARTESIAN_POINT('Ctrl Pts',(-9.22820702300006,11.6,6.43063541499998));
#248002=CARTESIAN_POINT('Ctrl Pts',(-9.22637032800005,15.2,6.42768818399999));
#248003=CARTESIAN_POINT('Ctrl Pts',(-9.22637032800005,11.6,6.42768818399999));
#248004=CARTESIAN_POINT('Ctrl Pts',(-9.22453385800006,15.2,6.42474645499998));
#248005=CARTESIAN_POINT('Ctrl Pts',(-9.22453385800006,11.6,6.42474645499998));
#248006=CARTESIAN_POINT('Ctrl Pts',(-9.22269762200006,15.2,6.42181023099998));
#248007=CARTESIAN_POINT('Ctrl Pts',(-9.22269762200006,11.6,6.42181023099998));
#248008=CARTESIAN_POINT('Ctrl Pts',(-9.22086163000005,15.2,6.41887951399998));
#248009=CARTESIAN_POINT('Ctrl Pts',(-9.22086163000005,11.6,6.41887951399998));
#248010=CARTESIAN_POINT('Ctrl Pts',(-9.21902589300006,15.2,6.41595430899999));
#248011=CARTESIAN_POINT('Ctrl Pts',(-9.21902589300006,11.6,6.41595430899999));
#248012=CARTESIAN_POINT('Ctrl Pts',(-9.21719041800005,15.2,6.41303461799998));
#248013=CARTESIAN_POINT('Ctrl Pts',(-9.21719041800005,11.6,6.41303461799998));
#248014=CARTESIAN_POINT('Ctrl Pts',(-9.21535521700006,15.2,6.41012044699998));
#248015=CARTESIAN_POINT('Ctrl Pts',(-9.21535521700006,11.6,6.41012044699998));
#248016=CARTESIAN_POINT('Ctrl Pts',(-9.21352029700006,15.2,6.40721179599999));
#248017=CARTESIAN_POINT('Ctrl Pts',(-9.21352029700006,11.6,6.40721179599999));
#248018=CARTESIAN_POINT('Ctrl Pts',(-9.21168567000005,15.2,6.40430867199999));
#248019=CARTESIAN_POINT('Ctrl Pts',(-9.21168567000005,11.6,6.40430867199999));
#248020=CARTESIAN_POINT('Ctrl Pts',(-9.20985134500006,15.2,6.40141107499999));
#248021=CARTESIAN_POINT('Ctrl Pts',(-9.20985134500006,11.6,6.40141107499999));
#248022=CARTESIAN_POINT('Ctrl Pts',(-9.20801733100006,15.2,6.39851900999999));
#248023=CARTESIAN_POINT('Ctrl Pts',(-9.20801733100006,11.6,6.39851900999999));
#248024=CARTESIAN_POINT('Ctrl Pts',(-9.20618363700006,15.2,6.39563248099999));
#248025=CARTESIAN_POINT('Ctrl Pts',(-9.20618363700006,11.6,6.39563248099999));
#248026=CARTESIAN_POINT('Ctrl Pts',(-9.20435027600006,15.2,6.39275148899999));
#248027=CARTESIAN_POINT('Ctrl Pts',(-9.20435027600006,11.6,6.39275148899999));
#248028=CARTESIAN_POINT('Ctrl Pts',(-9.20251725500006,15.2,6.38987603999999));
#248029=CARTESIAN_POINT('Ctrl Pts',(-9.20251725500006,11.6,6.38987603999999));
#248030=CARTESIAN_POINT('Ctrl Pts',(-9.20068458400005,15.2,6.38700613599998));
#248031=CARTESIAN_POINT('Ctrl Pts',(-9.20068458400005,11.6,6.38700613599998));
#248032=CARTESIAN_POINT('Ctrl Pts',(-9.19885227300006,15.2,6.38414178099998));
#248033=CARTESIAN_POINT('Ctrl Pts',(-9.19885227300006,11.6,6.38414178099998));
#248034=CARTESIAN_POINT('Ctrl Pts',(-9.19702033200006,15.2,6.38128297799998));
#248035=CARTESIAN_POINT('Ctrl Pts',(-9.19702033200006,11.6,6.38128297799998));
#248036=CARTESIAN_POINT('Ctrl Pts',(-9.19518877100005,15.2,6.37842972899998));
#248037=CARTESIAN_POINT('Ctrl Pts',(-9.19518877100005,11.6,6.37842972899998));
#248038=CARTESIAN_POINT('Ctrl Pts',(-9.19335760100006,15.2,6.37558203999999));
#248039=CARTESIAN_POINT('Ctrl Pts',(-9.19335760100006,11.6,6.37558203999999));
#248040=CARTESIAN_POINT('Ctrl Pts',(-9.19152683000006,15.2,6.37273991299999));
#248041=CARTESIAN_POINT('Ctrl Pts',(-9.19152683000006,11.6,6.37273991299999));
#248042=CARTESIAN_POINT('Ctrl Pts',(-9.18969646800005,15.2,6.36990335099998));
#248043=CARTESIAN_POINT('Ctrl Pts',(-9.18969646800005,11.6,6.36990335099998));
#248044=CARTESIAN_POINT('Ctrl Pts',(-9.18786652500006,15.2,6.36707235899999));
#248045=CARTESIAN_POINT('Ctrl Pts',(-9.18786652500006,11.6,6.36707235899999));
#248046=CARTESIAN_POINT('Ctrl Pts',(-9.18603701300006,15.2,6.36424693799999));
#248047=CARTESIAN_POINT('Ctrl Pts',(-9.18603701300006,11.6,6.36424693799999));
#248048=CARTESIAN_POINT('Ctrl Pts',(-9.18420793900006,15.2,6.36142709299998));
#248049=CARTESIAN_POINT('Ctrl Pts',(-9.18420793900006,11.6,6.36142709299998));
#248050=CARTESIAN_POINT('Ctrl Pts',(-9.18237931500006,15.2,6.35861282699998));
#248051=CARTESIAN_POINT('Ctrl Pts',(-9.18237931500006,11.6,6.35861282699998));
#248052=CARTESIAN_POINT('Ctrl Pts',(-9.18055115000006,15.2,6.35580414299999));
#248053=CARTESIAN_POINT('Ctrl Pts',(-9.18055115000006,11.6,6.35580414299999));
#248054=CARTESIAN_POINT('Ctrl Pts',(-9.17872345400006,15.2,6.35300104399998));
#248055=CARTESIAN_POINT('Ctrl Pts',(-9.17872345400006,11.6,6.35300104399998));
#248056=CARTESIAN_POINT('Ctrl Pts',(-9.17689623800005,15.2,6.35020353599998));
#248057=CARTESIAN_POINT('Ctrl Pts',(-9.17689623800005,11.6,6.35020353599998));
#248058=CARTESIAN_POINT('Ctrl Pts',(-9.17506951200006,15.2,6.34741161799998));
#248059=CARTESIAN_POINT('Ctrl Pts',(-9.17506951200006,11.6,6.34741161799998));
#248060=CARTESIAN_POINT('Ctrl Pts',(-9.17324328500005,15.2,6.34462529599999));
#248061=CARTESIAN_POINT('Ctrl Pts',(-9.17324328500005,11.6,6.34462529599999));
#248062=CARTESIAN_POINT('Ctrl Pts',(-9.17141756700006,15.2,6.34184457399999));
#248063=CARTESIAN_POINT('Ctrl Pts',(-9.17141756700006,11.6,6.34184457399999));
#248064=CARTESIAN_POINT('Ctrl Pts',(-9.16959236900006,15.2,6.33906945299999));
#248065=CARTESIAN_POINT('Ctrl Pts',(-9.16959236900006,11.6,6.33906945299999));
#248066=CARTESIAN_POINT('Ctrl Pts',(-9.16776770300006,15.2,6.33629993899999));
#248067=CARTESIAN_POINT('Ctrl Pts',(-9.16776770300006,11.6,6.33629993899999));
#248068=CARTESIAN_POINT('Ctrl Pts',(-9.16594357600006,15.2,6.33353603299999));
#248069=CARTESIAN_POINT('Ctrl Pts',(-9.16594357600006,11.6,6.33353603299999));
#248070=CARTESIAN_POINT('Ctrl Pts',(-9.16411999900006,15.2,6.33077774099998));
#248071=CARTESIAN_POINT('Ctrl Pts',(-9.16411999900006,11.6,6.33077774099998));
#248072=CARTESIAN_POINT('Ctrl Pts',(-9.16229698400005,15.2,6.32802506299999));
#248073=CARTESIAN_POINT('Ctrl Pts',(-9.16229698400005,11.6,6.32802506299999));
#248074=CARTESIAN_POINT('Ctrl Pts',(-9.16047453800006,15.2,6.32527800399998));
#248075=CARTESIAN_POINT('Ctrl Pts',(-9.16047453800006,11.6,6.32527800399998));
#248076=CARTESIAN_POINT('Ctrl Pts',(-9.15865267500006,15.2,6.32253656799998));
#248077=CARTESIAN_POINT('Ctrl Pts',(-9.15865267500006,11.6,6.32253656799998));
#248078=CARTESIAN_POINT('Ctrl Pts',(-9.15683140400006,15.2,6.31980075699998));
#248079=CARTESIAN_POINT('Ctrl Pts',(-9.15683140400006,11.6,6.31980075699998));
#248080=CARTESIAN_POINT('Ctrl Pts',(-9.15501073300005,15.2,6.31707057599999));
#248081=CARTESIAN_POINT('Ctrl Pts',(-9.15501073300005,11.6,6.31707057599999));
#248082=CARTESIAN_POINT('Ctrl Pts',(-9.15319067500005,15.2,6.31434602699999));
#248083=CARTESIAN_POINT('Ctrl Pts',(-9.15319067500005,11.6,6.31434602699999));
#248084=CARTESIAN_POINT('Ctrl Pts',(-9.15137124100006,15.2,6.31162711399998));
#248085=CARTESIAN_POINT('Ctrl Pts',(-9.15137124100006,11.6,6.31162711399998));
#248086=CARTESIAN_POINT('Ctrl Pts',(-9.14955243800006,15.2,6.30891383999998));
#248087=CARTESIAN_POINT('Ctrl Pts',(-9.14955243800006,11.6,6.30891383999998));
#248088=CARTESIAN_POINT('Ctrl Pts',(-9.14773428000006,15.2,6.30620620699998));
#248089=CARTESIAN_POINT('Ctrl Pts',(-9.14773428000006,11.6,6.30620620699998));
#248090=CARTESIAN_POINT('Ctrl Pts',(-9.14591677600006,15.2,6.30350422099998));
#248091=CARTESIAN_POINT('Ctrl Pts',(-9.14591677600006,11.6,6.30350422099998));
#248092=CARTESIAN_POINT('Ctrl Pts',(-9.14409993600006,15.2,6.30080788299999));
#248093=CARTESIAN_POINT('Ctrl Pts',(-9.14409993600006,11.6,6.30080788299999));
#248094=CARTESIAN_POINT('Ctrl Pts',(-9.14228377000006,15.2,6.29811719799999));
#248095=CARTESIAN_POINT('Ctrl Pts',(-9.14228377000006,11.6,6.29811719799999));
#248096=CARTESIAN_POINT('Ctrl Pts',(-9.14046829000006,15.2,6.29543216899999));
#248097=CARTESIAN_POINT('Ctrl Pts',(-9.14046829000006,11.6,6.29543216899999));
#248098=CARTESIAN_POINT('Ctrl Pts',(-9.13865350700006,15.2,6.29275279899999));
#248099=CARTESIAN_POINT('Ctrl Pts',(-9.13865350700006,11.6,6.29275279899999));
#248100=CARTESIAN_POINT('Ctrl Pts',(-9.13683942900006,15.2,6.29007908999998));
#248101=CARTESIAN_POINT('Ctrl Pts',(-9.13683942900006,11.6,6.29007908999998));
#248102=CARTESIAN_POINT('Ctrl Pts',(-9.13502606900006,15.2,6.28741104799998));
#248103=CARTESIAN_POINT('Ctrl Pts',(-9.13502606900006,11.6,6.28741104799998));
#248104=CARTESIAN_POINT('Ctrl Pts',(-9.13321343700006,15.2,6.28474867399999));
#248105=CARTESIAN_POINT('Ctrl Pts',(-9.13321343700006,11.6,6.28474867399999));
#248106=CARTESIAN_POINT('Ctrl Pts',(-9.13140154400006,15.2,6.28209197299999));
#248107=CARTESIAN_POINT('Ctrl Pts',(-9.13140154400006,11.6,6.28209197299999));
#248108=CARTESIAN_POINT('Ctrl Pts',(-9.12959039800005,15.2,6.27944094699998));
#248109=CARTESIAN_POINT('Ctrl Pts',(-9.12959039800005,11.6,6.27944094699998));
#248110=CARTESIAN_POINT('Ctrl Pts',(-9.12778001300006,15.2,6.27679559999999));
#248111=CARTESIAN_POINT('Ctrl Pts',(-9.12778001300006,11.6,6.27679559999999));
#248112=CARTESIAN_POINT('Ctrl Pts',(-9.12597039900006,15.2,6.27415593499999));
#248113=CARTESIAN_POINT('Ctrl Pts',(-9.12597039900006,11.6,6.27415593499999));
#248114=CARTESIAN_POINT('Ctrl Pts',(-9.12416156500005,15.2,6.27152195499999));
#248115=CARTESIAN_POINT('Ctrl Pts',(-9.12416156500005,11.6,6.27152195499999));
#248116=CARTESIAN_POINT('Ctrl Pts',(-9.12235352400005,15.2,6.26889366399999));
#248117=CARTESIAN_POINT('Ctrl Pts',(-9.12235352400005,11.6,6.26889366399999));
#248118=CARTESIAN_POINT('Ctrl Pts',(-9.12054628500006,15.2,6.26627106499999));
#248119=CARTESIAN_POINT('Ctrl Pts',(-9.12054628500006,11.6,6.26627106499999));
#248120=CARTESIAN_POINT('Ctrl Pts',(-9.11873986100005,15.2,6.26365416199998));
#248121=CARTESIAN_POINT('Ctrl Pts',(-9.11873986100005,11.6,6.26365416199998));
#248122=CARTESIAN_POINT('Ctrl Pts',(-9.11693426000006,15.2,6.26104295699999));
#248123=CARTESIAN_POINT('Ctrl Pts',(-9.11693426000006,11.6,6.26104295699999));
#248124=CARTESIAN_POINT('Ctrl Pts',(-9.11512949500005,15.2,6.25843745499999));
#248125=CARTESIAN_POINT('Ctrl Pts',(-9.11512949500005,11.6,6.25843745499999));
#248126=CARTESIAN_POINT('Ctrl Pts',(-9.11332557600005,15.2,6.25583765599998));
#248127=CARTESIAN_POINT('Ctrl Pts',(-9.11332557600005,11.6,6.25583765599998));
#248128=CARTESIAN_POINT('Ctrl Pts',(-9.11152251500006,15.2,6.25324356799998));
#248129=CARTESIAN_POINT('Ctrl Pts',(-9.11152251500006,11.6,6.25324356799998));
#248130=CARTESIAN_POINT('Ctrl Pts',(-9.10972032100006,15.2,6.25065518999998));
#248131=CARTESIAN_POINT('Ctrl Pts',(-9.10972032100006,11.6,6.25065518999998));
#248132=CARTESIAN_POINT('Ctrl Pts',(-9.10791900700006,15.2,6.24807252899998));
#248133=CARTESIAN_POINT('Ctrl Pts',(-9.10791900700006,11.6,6.24807252899998));
#248134=CARTESIAN_POINT('Ctrl Pts',(-9.10611858300006,15.2,6.24549558499999));
#248135=CARTESIAN_POINT('Ctrl Pts',(-9.10611858300006,11.6,6.24549558499999));
#248136=CARTESIAN_POINT('Ctrl Pts',(-9.10431906000005,15.2,6.24292436399998));
#248137=CARTESIAN_POINT('Ctrl Pts',(-9.10431906000005,11.6,6.24292436399998));
#248138=CARTESIAN_POINT('Ctrl Pts',(-9.10252044900006,15.2,6.24035886699998));
#248139=CARTESIAN_POINT('Ctrl Pts',(-9.10252044900006,11.6,6.24035886699998));
#248140=CARTESIAN_POINT('Ctrl Pts',(-9.10072276000006,15.2,6.23779909799998));
#248141=CARTESIAN_POINT('Ctrl Pts',(-9.10072276000006,11.6,6.23779909799998));
#248142=CARTESIAN_POINT('Ctrl Pts',(-9.09892600800006,15.2,6.23524506099999));
#248143=CARTESIAN_POINT('Ctrl Pts',(-9.09892600800006,11.6,6.23524506099999));
#248144=CARTESIAN_POINT('Ctrl Pts',(-9.09713019900006,15.2,6.23269675899999));
#248145=CARTESIAN_POINT('Ctrl Pts',(-9.09713019900006,11.6,6.23269675899999));
#248146=CARTESIAN_POINT('Ctrl Pts',(-9.09533534800006,15.2,6.23015419499998));
#248147=CARTESIAN_POINT('Ctrl Pts',(-9.09533534800006,11.6,6.23015419499998));
#248148=CARTESIAN_POINT('Ctrl Pts',(-9.09354146400006,15.2,6.22761737199998));
#248149=CARTESIAN_POINT('Ctrl Pts',(-9.09354146400006,11.6,6.22761737199998));
#248150=CARTESIAN_POINT('Ctrl Pts',(-9.09174856000006,15.2,6.22508629499999));
#248151=CARTESIAN_POINT('Ctrl Pts',(-9.09174856000006,11.6,6.22508629499999));
#248152=CARTESIAN_POINT('Ctrl Pts',(-9.08995664500006,15.2,6.22256096499999));
#248153=CARTESIAN_POINT('Ctrl Pts',(-9.08995664500006,11.6,6.22256096499999));
#248154=CARTESIAN_POINT('Ctrl Pts',(-9.08816573200006,15.2,6.22004138599999));
#248155=CARTESIAN_POINT('Ctrl Pts',(-9.08816573200006,11.6,6.22004138599999));
#248156=CARTESIAN_POINT('Ctrl Pts',(-9.08637583300006,15.2,6.21752756199999));
#248157=CARTESIAN_POINT('Ctrl Pts',(-9.08637583300006,11.6,6.21752756199999));
#248158=CARTESIAN_POINT('Ctrl Pts',(-9.08458695700006,15.2,6.21501949599998));
#248159=CARTESIAN_POINT('Ctrl Pts',(-9.08458695700006,11.6,6.21501949599998));
#248160=CARTESIAN_POINT('Ctrl Pts',(-9.08279911700006,15.2,6.21251719099998));
#248161=CARTESIAN_POINT('Ctrl Pts',(-9.08279911700006,11.6,6.21251719099998));
#248162=CARTESIAN_POINT('Ctrl Pts',(-9.08101232300006,15.2,6.21002064899999));
#248163=CARTESIAN_POINT('Ctrl Pts',(-9.08101232300006,11.6,6.21002064899999));
#248164=CARTESIAN_POINT('Ctrl Pts',(-9.07922658800006,15.2,6.20752987599998));
#248165=CARTESIAN_POINT('Ctrl Pts',(-9.07922658800006,11.6,6.20752987599998));
#248166=CARTESIAN_POINT('Ctrl Pts',(-9.07744192200006,15.2,6.20504487299999));
#248167=CARTESIAN_POINT('Ctrl Pts',(-9.07744192200006,11.6,6.20504487299999));
#248168=CARTESIAN_POINT('Ctrl Pts',(-9.07565833800006,15.2,6.20256564499999));
#248169=CARTESIAN_POINT('Ctrl Pts',(-9.07565833800006,11.6,6.20256564499999));
#248170=CARTESIAN_POINT('Ctrl Pts',(-9.07387584700006,15.2,6.20009219399999));
#248171=CARTESIAN_POINT('Ctrl Pts',(-9.07387584700006,11.6,6.20009219399999));
#248172=CARTESIAN_POINT('Ctrl Pts',(-9.07209445900006,15.2,6.19762452499998));
#248173=CARTESIAN_POINT('Ctrl Pts',(-9.07209445900006,11.6,6.19762452499998));
#248174=CARTESIAN_POINT('Ctrl Pts',(-9.07031418700005,15.2,6.19516263799999));
#248175=CARTESIAN_POINT('Ctrl Pts',(-9.07031418700005,11.6,6.19516263799999));
#248176=CARTESIAN_POINT('Ctrl Pts',(-9.06853504200006,15.2,6.19270653899999));
#248177=CARTESIAN_POINT('Ctrl Pts',(-9.06853504200006,11.6,6.19270653899999));
#248178=CARTESIAN_POINT('Ctrl Pts',(-9.06675703600006,15.2,6.19025622999998));
#248179=CARTESIAN_POINT('Ctrl Pts',(-9.06675703600006,11.6,6.19025622999998));
#248180=CARTESIAN_POINT('Ctrl Pts',(-9.06498018100006,15.2,6.18781171499998));
#248181=CARTESIAN_POINT('Ctrl Pts',(-9.06498018100006,11.6,6.18781171499998));
#248182=CARTESIAN_POINT('Ctrl Pts',(-9.06320448800006,15.2,6.18537299699998));
#248183=CARTESIAN_POINT('Ctrl Pts',(-9.06320448800006,11.6,6.18537299699998));
#248184=CARTESIAN_POINT('Ctrl Pts',(-9.06142996800006,15.2,6.18294007899999));
#248185=CARTESIAN_POINT('Ctrl Pts',(-9.06142996800006,11.6,6.18294007899999));
#248186=CARTESIAN_POINT('Ctrl Pts',(-9.05965663400006,15.2,6.18051296499999));
#248187=CARTESIAN_POINT('Ctrl Pts',(-9.05965663400006,11.6,6.18051296499999));
#248188=CARTESIAN_POINT('Ctrl Pts',(-9.05788449700006,15.2,6.17809165699998));
#248189=CARTESIAN_POINT('Ctrl Pts',(-9.05788449700006,11.6,6.17809165699998));
#248190=CARTESIAN_POINT('Ctrl Pts',(-9.05611357000006,15.2,6.17567615899999));
#248191=CARTESIAN_POINT('Ctrl Pts',(-9.05611357000006,11.6,6.17567615899999));
#248192=CARTESIAN_POINT('Ctrl Pts',(-9.05434386300006,15.2,6.17326647399998));
#248193=CARTESIAN_POINT('Ctrl Pts',(-9.05434386300006,11.6,6.17326647399998));
#248194=CARTESIAN_POINT('Ctrl Pts',(-9.05257538900005,15.2,6.17086260599999));
#248195=CARTESIAN_POINT('Ctrl Pts',(-9.05257538900005,11.6,6.17086260599999));
#248196=CARTESIAN_POINT('Ctrl Pts',(-9.05080816000006,15.2,6.16846455799998));
#248197=CARTESIAN_POINT('Ctrl Pts',(-9.05080816000006,11.6,6.16846455799998));
#248198=CARTESIAN_POINT('Ctrl Pts',(-9.04904218600005,15.2,6.16607233099998));
#248199=CARTESIAN_POINT('Ctrl Pts',(-9.04904218600005,11.6,6.16607233099998));
#248200=CARTESIAN_POINT('Ctrl Pts',(-9.04727748100006,15.2,6.16368593199999));
#248201=CARTESIAN_POINT('Ctrl Pts',(-9.04727748100006,11.6,6.16368593199999));
#248202=CARTESIAN_POINT('Ctrl Pts',(-9.04551405600006,15.2,6.16130536099998));
#248203=CARTESIAN_POINT('Ctrl Pts',(-9.04551405600006,11.6,6.16130536099998));
#248204=CARTESIAN_POINT('Ctrl Pts',(-9.04375192500006,15.2,6.15893062399999));
#248205=CARTESIAN_POINT('Ctrl Pts',(-9.04375192500006,11.6,6.15893062399999));
#248206=CARTESIAN_POINT('Ctrl Pts',(-9.04199109600006,15.2,6.15656172199999));
#248207=CARTESIAN_POINT('Ctrl Pts',(-9.04199109600006,11.6,6.15656172199999));
#248208=CARTESIAN_POINT('Ctrl Pts',(-9.04023158400006,15.2,6.15419865999999));
#248209=CARTESIAN_POINT('Ctrl Pts',(-9.04023158400006,11.6,6.15419865999999));
#248210=CARTESIAN_POINT('Ctrl Pts',(-9.03847340100006,15.2,6.15184143899998));
#248211=CARTESIAN_POINT('Ctrl Pts',(-9.03847340100006,11.6,6.15184143899998));
#248212=CARTESIAN_POINT('Ctrl Pts',(-9.03671655700006,15.2,6.14949006399998));
#248213=CARTESIAN_POINT('Ctrl Pts',(-9.03671655700006,11.6,6.14949006399998));
#248214=CARTESIAN_POINT('Ctrl Pts',(-9.03496106600005,15.2,6.14714453699998));
#248215=CARTESIAN_POINT('Ctrl Pts',(-9.03496106600005,11.6,6.14714453699998));
#248216=CARTESIAN_POINT('Ctrl Pts',(-9.03320694100006,15.2,6.14480486299998));
#248217=CARTESIAN_POINT('Ctrl Pts',(-9.03320694100006,11.6,6.14480486299998));
#248218=CARTESIAN_POINT('Ctrl Pts',(-9.03145419200006,15.2,6.14247104399999));
#248219=CARTESIAN_POINT('Ctrl Pts',(-9.03145419200006,11.6,6.14247104399999));
#248220=CARTESIAN_POINT('Ctrl Pts',(-9.02970283100006,15.2,6.14014308299998));
#248221=CARTESIAN_POINT('Ctrl Pts',(-9.02970283100006,11.6,6.14014308299998));
#248222=CARTESIAN_POINT('Ctrl Pts',(-9.02795287300006,15.2,6.13782098399999));
#248223=CARTESIAN_POINT('Ctrl Pts',(-9.02795287300006,11.6,6.13782098399999));
#248224=CARTESIAN_POINT('Ctrl Pts',(-9.02620432800006,15.2,6.13550474999998));
#248225=CARTESIAN_POINT('Ctrl Pts',(-9.02620432800006,11.6,6.13550474999998));
#248226=CARTESIAN_POINT('Ctrl Pts',(-9.02445720900005,15.2,6.13319438399999));
#248227=CARTESIAN_POINT('Ctrl Pts',(-9.02445720900005,11.6,6.13319438399999));
#248228=CARTESIAN_POINT('Ctrl Pts',(-9.02271153000006,15.2,6.13088988899998));
#248229=CARTESIAN_POINT('Ctrl Pts',(-9.02271153000006,11.6,6.13088988899998));
#248230=CARTESIAN_POINT('Ctrl Pts',(-9.02096729900006,15.2,6.12859126899998));
#248231=CARTESIAN_POINT('Ctrl Pts',(-9.02096729900006,11.6,6.12859126899998));
#248232=CARTESIAN_POINT('Ctrl Pts',(-9.01922453200006,15.2,6.12629852599999));
#248233=CARTESIAN_POINT('Ctrl Pts',(-9.01922453200006,11.6,6.12629852599999));
#248234=CARTESIAN_POINT('Ctrl Pts',(-9.01748324100006,15.2,6.12401166399999));
#248235=CARTESIAN_POINT('Ctrl Pts',(-9.01748324100006,11.6,6.12401166399999));
#248236=CARTESIAN_POINT('Ctrl Pts',(-9.01574343800006,15.2,6.12173068599999));
#248237=CARTESIAN_POINT('Ctrl Pts',(-9.01574343800006,11.6,6.12173068599999));
#248238=CARTESIAN_POINT('Ctrl Pts',(-9.01400513500005,15.2,6.11945559499999));
#248239=CARTESIAN_POINT('Ctrl Pts',(-9.01400513500005,11.6,6.11945559499999));
#248240=CARTESIAN_POINT('Ctrl Pts',(-9.01226834600006,15.2,6.11718639599999));
#248241=CARTESIAN_POINT('Ctrl Pts',(-9.01226834600006,11.6,6.11718639599999));
#248242=CARTESIAN_POINT('Ctrl Pts',(-9.01053308100006,15.2,6.11492308999999));
#248243=CARTESIAN_POINT('Ctrl Pts',(-9.01053308100006,11.6,6.11492308999999));
#248244=CARTESIAN_POINT('Ctrl Pts',(-9.00879935600006,15.2,6.11266568099998));
#248245=CARTESIAN_POINT('Ctrl Pts',(-9.00879935600006,11.6,6.11266568099998));
#248246=CARTESIAN_POINT('Ctrl Pts',(-9.00706718100006,15.2,6.11041417099998));
#248247=CARTESIAN_POINT('Ctrl Pts',(-9.00706718100006,11.6,6.11041417099998));
#248248=CARTESIAN_POINT('Ctrl Pts',(-9.00533657000006,15.2,6.10816856499999));
#248249=CARTESIAN_POINT('Ctrl Pts',(-9.00533657000006,11.6,6.10816856499999));
#248250=CARTESIAN_POINT('Ctrl Pts',(-9.00360753400006,15.2,6.10592886599999));
#248251=CARTESIAN_POINT('Ctrl Pts',(-9.00360753400006,11.6,6.10592886599999));
#248252=CARTESIAN_POINT('Ctrl Pts',(-9.00188008800006,15.2,6.10369507599999));
#248253=CARTESIAN_POINT('Ctrl Pts',(-9.00188008800006,11.6,6.10369507599999));
#248254=CARTESIAN_POINT('Ctrl Pts',(-9.00015424300006,15.2,6.10146719899999));
#248255=CARTESIAN_POINT('Ctrl Pts',(-9.00015424300006,11.6,6.10146719899999));
#248256=CARTESIAN_POINT('Ctrl Pts',(-8.99843001300006,15.2,6.09924523799998));
#248257=CARTESIAN_POINT('Ctrl Pts',(-8.99843001300006,11.6,6.09924523799998));
#248258=CARTESIAN_POINT('Ctrl Pts',(-8.99670741000006,15.2,6.09702919599999));
#248259=CARTESIAN_POINT('Ctrl Pts',(-8.99670741000006,11.6,6.09702919599999));
#248260=CARTESIAN_POINT('Ctrl Pts',(-8.99498644700006,15.2,6.09481907799999));
#248261=CARTESIAN_POINT('Ctrl Pts',(-8.99498644700006,11.6,6.09481907799999));
#248262=CARTESIAN_POINT('Ctrl Pts',(-8.99326713900006,15.2,6.09261488399999));
#248263=CARTESIAN_POINT('Ctrl Pts',(-8.99326713900006,11.6,6.09261488399999));
#248264=CARTESIAN_POINT('Ctrl Pts',(-8.99154949500005,15.2,6.09041661899998));
#248265=CARTESIAN_POINT('Ctrl Pts',(-8.99154949500005,11.6,6.09041661899998));
#248266=CARTESIAN_POINT('Ctrl Pts',(-8.98983353100006,15.2,6.08822428699998));
#248267=CARTESIAN_POINT('Ctrl Pts',(-8.98983353100006,11.6,6.08822428699998));
#248268=CARTESIAN_POINT('Ctrl Pts',(-8.98811925800005,15.2,6.08603788899998));
#248269=CARTESIAN_POINT('Ctrl Pts',(-8.98811925800005,11.6,6.08603788899998));
#248270=CARTESIAN_POINT('Ctrl Pts',(-8.98640669100006,15.2,6.08385742899999));
#248271=CARTESIAN_POINT('Ctrl Pts',(-8.98640669100006,11.6,6.08385742899999));
#248272=CARTESIAN_POINT('Ctrl Pts',(-8.98469584100006,15.2,6.08168291199998));
#248273=CARTESIAN_POINT('Ctrl Pts',(-8.98469584100006,11.6,6.08168291199998));
#248274=CARTESIAN_POINT('Ctrl Pts',(-8.98298672300006,15.2,6.07951433899999));
#248275=CARTESIAN_POINT('Ctrl Pts',(-8.98298672300006,11.6,6.07951433899999));
#248276=CARTESIAN_POINT('Ctrl Pts',(-8.98127935000005,15.2,6.07735171299999));
#248277=CARTESIAN_POINT('Ctrl Pts',(-8.98127935000005,11.6,6.07735171299999));
#248278=CARTESIAN_POINT('Ctrl Pts',(-8.97957373300006,15.2,6.07519503899999));
#248279=CARTESIAN_POINT('Ctrl Pts',(-8.97957373300006,11.6,6.07519503899999));
#248280=CARTESIAN_POINT('Ctrl Pts',(-8.97786988800006,15.2,6.07304431899998));
#248281=CARTESIAN_POINT('Ctrl Pts',(-8.97786988800006,11.6,6.07304431899998));
#248282=CARTESIAN_POINT('Ctrl Pts',(-8.97616782700006,15.2,6.07089955599999));
#248283=CARTESIAN_POINT('Ctrl Pts',(-8.97616782700006,11.6,6.07089955599999));
#248284=CARTESIAN_POINT('Ctrl Pts',(-8.97446756400005,15.2,6.06876075399998));
#248285=CARTESIAN_POINT('Ctrl Pts',(-8.97446756400005,11.6,6.06876075399998));
#248286=CARTESIAN_POINT('Ctrl Pts',(-8.97276911000005,15.2,6.06662791599998));
#248287=CARTESIAN_POINT('Ctrl Pts',(-8.97276911000005,11.6,6.06662791599998));
#248288=CARTESIAN_POINT('Ctrl Pts',(-8.97107248000006,15.2,6.06450104399999));
#248289=CARTESIAN_POINT('Ctrl Pts',(-8.97107248000006,11.6,6.06450104399999));
#248290=CARTESIAN_POINT('Ctrl Pts',(-8.96937768800005,15.2,6.06238014199998));
#248291=CARTESIAN_POINT('Ctrl Pts',(-8.96937768800005,11.6,6.06238014199998));
#248292=CARTESIAN_POINT('Ctrl Pts',(-8.96768474700006,15.2,6.06026521299999));
#248293=CARTESIAN_POINT('Ctrl Pts',(-8.96768474700006,11.6,6.06026521299999));
#248294=CARTESIAN_POINT('Ctrl Pts',(-8.96599367000006,15.2,6.05815626099999));
#248295=CARTESIAN_POINT('Ctrl Pts',(-8.96599367000006,11.6,6.05815626099999));
#248296=CARTESIAN_POINT('Ctrl Pts',(-8.96430447100006,15.2,6.05605328799999));
#248297=CARTESIAN_POINT('Ctrl Pts',(-8.96430447100006,11.6,6.05605328799999));
#248298=CARTESIAN_POINT('Ctrl Pts',(-8.96261716200006,15.2,6.05395629799999));
#248299=CARTESIAN_POINT('Ctrl Pts',(-8.96261716200006,11.6,6.05395629799999));
#248300=CARTESIAN_POINT('Ctrl Pts',(-8.96093175900005,15.2,6.05186529299999));
#248301=CARTESIAN_POINT('Ctrl Pts',(-8.96093175900005,11.6,6.05186529299999));
#248302=CARTESIAN_POINT('Ctrl Pts',(-8.95924827400006,15.2,6.04978027699998));
#248303=CARTESIAN_POINT('Ctrl Pts',(-8.95924827400006,11.6,6.04978027699998));
#248304=CARTESIAN_POINT('Ctrl Pts',(-8.95756672200006,15.2,6.04770125299999));
#248305=CARTESIAN_POINT('Ctrl Pts',(-8.95756672200006,11.6,6.04770125299999));
#248306=CARTESIAN_POINT('Ctrl Pts',(-8.95588711400006,15.2,6.04562822499998));
#248307=CARTESIAN_POINT('Ctrl Pts',(-8.95588711400006,11.6,6.04562822499998));
#248308=CARTESIAN_POINT('Ctrl Pts',(-8.95420946700006,15.2,6.04356119499998));
#248309=CARTESIAN_POINT('Ctrl Pts',(-8.95420946700006,11.6,6.04356119499998));
#248310=CARTESIAN_POINT('Ctrl Pts',(-8.95253379300006,15.2,6.04150016599998));
#248311=CARTESIAN_POINT('Ctrl Pts',(-8.95253379300006,11.6,6.04150016599998));
#248312=CARTESIAN_POINT('Ctrl Pts',(-8.95086010600006,15.2,6.03944514299998));
#248313=CARTESIAN_POINT('Ctrl Pts',(-8.95086010600006,11.6,6.03944514299998));
#248314=CARTESIAN_POINT('Ctrl Pts',(-8.94918841900006,15.2,6.03739612599998));
#248315=CARTESIAN_POINT('Ctrl Pts',(-8.94918841900006,11.6,6.03739612599998));
#248316=CARTESIAN_POINT('Ctrl Pts',(-8.94751874800006,15.2,6.03535311999998));
#248317=CARTESIAN_POINT('Ctrl Pts',(-8.94751874800006,11.6,6.03535311999998));
#248318=CARTESIAN_POINT('Ctrl Pts',(-8.94585110500006,15.2,6.03331612899999));
#248319=CARTESIAN_POINT('Ctrl Pts',(-8.94585110500006,11.6,6.03331612899999));
#248320=CARTESIAN_POINT('Ctrl Pts',(-8.94418550500006,15.2,6.03128515399998));
#248321=CARTESIAN_POINT('Ctrl Pts',(-8.94418550500006,11.6,6.03128515399998));
#248322=CARTESIAN_POINT('Ctrl Pts',(-8.94252196200006,15.2,6.02926019999998));
#248323=CARTESIAN_POINT('Ctrl Pts',(-8.94252196200006,11.6,6.02926019999998));
#248324=CARTESIAN_POINT('Ctrl Pts',(-8.94086048900006,15.2,6.02724126799998));
#248325=CARTESIAN_POINT('Ctrl Pts',(-8.94086048900006,11.6,6.02724126799998));
#248326=CARTESIAN_POINT('Ctrl Pts',(-8.93920110100006,15.2,6.02522836499999));
#248327=CARTESIAN_POINT('Ctrl Pts',(-8.93920110100006,11.6,6.02522836499999));
#248328=CARTESIAN_POINT('Ctrl Pts',(-8.93754381200005,15.2,6.02322148899999));
#248329=CARTESIAN_POINT('Ctrl Pts',(-8.93754381200005,11.6,6.02322148899999));
#248330=CARTESIAN_POINT('Ctrl Pts',(-8.93588863500005,15.2,6.02122064799998));
#248331=CARTESIAN_POINT('Ctrl Pts',(-8.93588863500005,11.6,6.02122064799998));
#248332=CARTESIAN_POINT('Ctrl Pts',(-8.93423558600006,15.2,6.01922584099999));
#248333=CARTESIAN_POINT('Ctrl Pts',(-8.93423558600006,11.6,6.01922584099999));
#248334=CARTESIAN_POINT('Ctrl Pts',(-8.93258467900005,15.2,6.01723707299998));
#248335=CARTESIAN_POINT('Ctrl Pts',(-8.93258467900005,11.6,6.01723707299998));
#248336=CARTESIAN_POINT('Ctrl Pts',(-8.93093592600006,15.2,6.01525434899998));
#248337=CARTESIAN_POINT('Ctrl Pts',(-8.93093592600006,11.6,6.01525434899998));
#248338=CARTESIAN_POINT('Ctrl Pts',(-8.92928934500006,15.2,6.01327766899999));
#248339=CARTESIAN_POINT('Ctrl Pts',(-8.92928934500006,11.6,6.01327766899999));
#248340=CARTESIAN_POINT('Ctrl Pts',(-8.92764494700005,15.2,6.01130703699998));
#248341=CARTESIAN_POINT('Ctrl Pts',(-8.92764494700005,11.6,6.01130703699998));
#248342=CARTESIAN_POINT('Ctrl Pts',(-8.92600274800006,15.2,6.00934245699998));
#248343=CARTESIAN_POINT('Ctrl Pts',(-8.92600274800006,11.6,6.00934245699998));
#248344=CARTESIAN_POINT('Ctrl Pts',(-8.92436276200005,15.2,6.00738392999999));
#248345=CARTESIAN_POINT('Ctrl Pts',(-8.92436276200005,11.6,6.00738392999999));
#248346=CARTESIAN_POINT('Ctrl Pts',(-8.92272500400006,15.2,6.00543146199998));
#248347=CARTESIAN_POINT('Ctrl Pts',(-8.92272500400006,11.6,6.00543146199998));
#248348=CARTESIAN_POINT('Ctrl Pts',(-8.92108948800006,15.2,6.00348505499999));
#248349=CARTESIAN_POINT('Ctrl Pts',(-8.92108948800006,11.6,6.00348505499999));
#248350=CARTESIAN_POINT('Ctrl Pts',(-8.91945622800005,15.2,6.00154471099999));
#248351=CARTESIAN_POINT('Ctrl Pts',(-8.91945622800005,11.6,6.00154471099999));
#248352=CARTESIAN_POINT('Ctrl Pts',(-8.91782524000006,15.2,5.99961043399999));
#248353=CARTESIAN_POINT('Ctrl Pts',(-8.91782524000006,11.6,5.99961043399999));
#248354=CARTESIAN_POINT('Ctrl Pts',(-8.91619653800005,15.2,5.99768222699999));
#248355=CARTESIAN_POINT('Ctrl Pts',(-8.91619653800005,11.6,5.99768222699999));
#248356=CARTESIAN_POINT('Ctrl Pts',(-8.91457013600006,15.2,5.99576009299999));
#248357=CARTESIAN_POINT('Ctrl Pts',(-8.91457013600006,11.6,5.99576009299999));
#248358=CARTESIAN_POINT('Ctrl Pts',(-8.91294605000006,15.2,5.99384403599998));
#248359=CARTESIAN_POINT('Ctrl Pts',(-8.91294605000006,11.6,5.99384403599998));
#248360=CARTESIAN_POINT('Ctrl Pts',(-8.91132429400006,15.2,5.99193405799999));
#248361=CARTESIAN_POINT('Ctrl Pts',(-8.91132429400006,11.6,5.99193405799999));
#248362=CARTESIAN_POINT('Ctrl Pts',(-8.90970488300006,15.2,5.99003016199998));
#248363=CARTESIAN_POINT('Ctrl Pts',(-8.90970488300006,11.6,5.99003016199998));
#248364=CARTESIAN_POINT('Ctrl Pts',(-8.90808783100006,15.2,5.98813235099998));
#248365=CARTESIAN_POINT('Ctrl Pts',(-8.90808783100006,11.6,5.98813235099998));
#248366=CARTESIAN_POINT('Ctrl Pts',(-8.90647315400006,15.2,5.98624062899999));
#248367=CARTESIAN_POINT('Ctrl Pts',(-8.90647315400006,11.6,5.98624062899999));
#248368=CARTESIAN_POINT('Ctrl Pts',(-8.90486086700006,15.2,5.98435499899999));
#248369=CARTESIAN_POINT('Ctrl Pts',(-8.90486086700006,11.6,5.98435499899999));
#248370=CARTESIAN_POINT('Ctrl Pts',(-8.90325098400006,15.2,5.98247546299999));
#248371=CARTESIAN_POINT('Ctrl Pts',(-8.90325098400006,11.6,5.98247546299999));
#248372=CARTESIAN_POINT('Ctrl Pts',(-8.90164352100006,15.2,5.98060202599999));
#248373=CARTESIAN_POINT('Ctrl Pts',(-8.90164352100006,11.6,5.98060202599999));
#248374=CARTESIAN_POINT('Ctrl Pts',(-8.90003849200006,15.2,5.97873468899999));
#248375=CARTESIAN_POINT('Ctrl Pts',(-8.90003849200006,11.6,5.97873468899999));
#248376=CARTESIAN_POINT('Ctrl Pts',(-8.89843591300006,15.2,5.97687345599999));
#248377=CARTESIAN_POINT('Ctrl Pts',(-8.89843591300006,11.6,5.97687345599999));
#248378=CARTESIAN_POINT('Ctrl Pts',(-8.89683579900005,15.2,5.97501832999999));
#248379=CARTESIAN_POINT('Ctrl Pts',(-8.89683579900005,11.6,5.97501832999999));
#248380=CARTESIAN_POINT('Ctrl Pts',(-8.89523816500006,15.2,5.97316931399998));
#248381=CARTESIAN_POINT('Ctrl Pts',(-8.89523816500006,11.6,5.97316931399998));
#248382=CARTESIAN_POINT('Ctrl Pts',(-8.89364302700006,15.2,5.97132641099999));
#248383=CARTESIAN_POINT('Ctrl Pts',(-8.89364302700006,11.6,5.97132641099999));
#248384=CARTESIAN_POINT('Ctrl Pts',(-8.89205039900006,15.2,5.96948962399999));
#248385=CARTESIAN_POINT('Ctrl Pts',(-8.89205039900006,11.6,5.96948962399999));
#248386=CARTESIAN_POINT('Ctrl Pts',(-8.89046029700006,15.2,5.96765895699999));
#248387=CARTESIAN_POINT('Ctrl Pts',(-8.89046029700006,11.6,5.96765895699999));
#248388=CARTESIAN_POINT('Ctrl Pts',(-8.88887273700006,15.2,5.96583441199999));
#248389=CARTESIAN_POINT('Ctrl Pts',(-8.88887273700006,11.6,5.96583441199999));
#248390=CARTESIAN_POINT('Ctrl Pts',(-8.88728773400006,15.2,5.96401599199999));
#248391=CARTESIAN_POINT('Ctrl Pts',(-8.88728773400006,11.6,5.96401599199999));
#248392=CARTESIAN_POINT('Ctrl Pts',(-8.88570530300006,15.2,5.96220370099999));
#248393=CARTESIAN_POINT('Ctrl Pts',(-8.88570530300006,11.6,5.96220370099999));
#248394=CARTESIAN_POINT('Ctrl Pts',(-8.88412545900006,15.2,5.96039754099999));
#248395=CARTESIAN_POINT('Ctrl Pts',(-8.88412545900006,11.6,5.96039754099999));
#248396=CARTESIAN_POINT('Ctrl Pts',(-8.88254821900006,15.2,5.95859751599999));
#248397=CARTESIAN_POINT('Ctrl Pts',(-8.88254821900006,11.6,5.95859751599999));
#248398=CARTESIAN_POINT('Ctrl Pts',(-8.88097359900006,15.2,5.95680362899999));
#248399=CARTESIAN_POINT('Ctrl Pts',(-8.88097359900006,11.6,5.95680362899999));
#248400=CARTESIAN_POINT('Ctrl Pts',(-8.87940161200006,15.2,5.95501588299998));
#248401=CARTESIAN_POINT('Ctrl Pts',(-8.87940161200006,11.6,5.95501588299998));
#248402=CARTESIAN_POINT('Ctrl Pts',(-8.87783227600006,15.2,5.95323427899999));
#248403=CARTESIAN_POINT('Ctrl Pts',(-8.87783227600006,11.6,5.95323427899999));
#248404=CARTESIAN_POINT('Ctrl Pts',(-8.87626560700006,15.2,5.95145882299998));
#248405=CARTESIAN_POINT('Ctrl Pts',(-8.87626560700006,11.6,5.95145882299998));
#248406=CARTESIAN_POINT('Ctrl Pts',(-8.87470161900006,15.2,5.94968951599999));
#248407=CARTESIAN_POINT('Ctrl Pts',(-8.87470161900006,11.6,5.94968951599999));
#248408=CARTESIAN_POINT('Ctrl Pts',(-8.87314032900006,15.2,5.94792636199998));
#248409=CARTESIAN_POINT('Ctrl Pts',(-8.87314032900006,11.6,5.94792636199998));
#248410=CARTESIAN_POINT('Ctrl Pts',(-8.87158175200006,15.2,5.94616936499998));
#248411=CARTESIAN_POINT('Ctrl Pts',(-8.87158175200006,11.6,5.94616936499998));
#248412=CARTESIAN_POINT('Ctrl Pts',(-8.87002590600006,15.2,5.94441852499998));
#248413=CARTESIAN_POINT('Ctrl Pts',(-8.87002590600006,11.6,5.94441852499998));
#248414=CARTESIAN_POINT('Ctrl Pts',(-8.86847280500006,15.2,5.94267384799998));
#248415=CARTESIAN_POINT('Ctrl Pts',(-8.86847280500006,11.6,5.94267384799998));
#248416=CARTESIAN_POINT('Ctrl Pts',(-8.86692246600006,15.2,5.94093533599998));
#248417=CARTESIAN_POINT('Ctrl Pts',(-8.86692246600006,11.6,5.94093533599998));
#248418=CARTESIAN_POINT('Ctrl Pts',(-8.86537490400006,15.2,5.93920299199999));
#248419=CARTESIAN_POINT('Ctrl Pts',(-8.86537490400006,11.6,5.93920299199999));
#248420=CARTESIAN_POINT('Ctrl Pts',(-8.86383013600006,15.2,5.93747681899998));
#248421=CARTESIAN_POINT('Ctrl Pts',(-8.86383013600006,11.6,5.93747681899998));
#248422=CARTESIAN_POINT('Ctrl Pts',(-8.86228818000006,15.2,5.93575682099999));
#248423=CARTESIAN_POINT('Ctrl Pts',(-8.86228818000006,11.6,5.93575682099999));
#248424=CARTESIAN_POINT('Ctrl Pts',(-8.86074904800006,15.2,5.93404299899999));
#248425=CARTESIAN_POINT('Ctrl Pts',(-8.86074904800006,11.6,5.93404299899999));
#248426=CARTESIAN_POINT('Ctrl Pts',(-8.85921276100006,15.2,5.93233535699999));
#248427=CARTESIAN_POINT('Ctrl Pts',(-8.85921276100006,11.6,5.93233535699999));
#248428=CARTESIAN_POINT('Ctrl Pts',(-8.85767933100006,15.2,5.93063389799998));
#248429=CARTESIAN_POINT('Ctrl Pts',(-8.85767933100006,11.6,5.93063389799998));
#248430=CARTESIAN_POINT('Ctrl Pts',(-8.85614877800006,15.2,5.92893862599999));
#248431=CARTESIAN_POINT('Ctrl Pts',(-8.85614877800006,11.6,5.92893862599999));
#248432=CARTESIAN_POINT('Ctrl Pts',(-8.85462111600006,15.2,5.92724954299998));
#248433=CARTESIAN_POINT('Ctrl Pts',(-8.85462111600006,11.6,5.92724954299998));
#248434=CARTESIAN_POINT('Ctrl Pts',(-8.85309636200006,15.2,5.92556665199999));
#248435=CARTESIAN_POINT('Ctrl Pts',(-8.85309636200006,11.6,5.92556665199999));
#248436=CARTESIAN_POINT('Ctrl Pts',(-8.85157453400006,15.2,5.92388995699999));
#248437=CARTESIAN_POINT('Ctrl Pts',(-8.85157453400006,11.6,5.92388995699999));
#248438=CARTESIAN_POINT('Ctrl Pts',(-8.85005564700006,15.2,5.92221945899999));
#248439=CARTESIAN_POINT('Ctrl Pts',(-8.85005564700006,11.6,5.92221945899999));
#248440=CARTESIAN_POINT('Ctrl Pts',(-8.84853971900006,15.2,5.92055516299999));
#248441=CARTESIAN_POINT('Ctrl Pts',(-8.84853971900006,11.6,5.92055516299999));
#248442=CARTESIAN_POINT('Ctrl Pts',(-8.84702676400006,15.2,5.91889707099998));
#248443=CARTESIAN_POINT('Ctrl Pts',(-8.84702676400006,11.6,5.91889707099998));
#248444=CARTESIAN_POINT('Ctrl Pts',(-8.84551680300006,15.2,5.91724518599998));
#248445=CARTESIAN_POINT('Ctrl Pts',(-8.84551680300006,11.6,5.91724518599998));
#248446=CARTESIAN_POINT('Ctrl Pts',(-8.84400984900006,15.2,5.91559951099998));
#248447=CARTESIAN_POINT('Ctrl Pts',(-8.84400984900006,11.6,5.91559951099998));
#248448=CARTESIAN_POINT('Ctrl Pts',(-8.84250592200006,15.2,5.91396004999999));
#248449=CARTESIAN_POINT('Ctrl Pts',(-8.84250592200006,11.6,5.91396004999999));
#248450=CARTESIAN_POINT('Ctrl Pts',(-8.84100503600006,15.2,5.91232680499999));
#248451=CARTESIAN_POINT('Ctrl Pts',(-8.84100503600006,11.6,5.91232680499999));
#248452=CARTESIAN_POINT('Ctrl Pts',(-8.83950720900006,15.2,5.91069977899998));
#248453=CARTESIAN_POINT('Ctrl Pts',(-8.83950720900006,11.6,5.91069977899998));
#248454=CARTESIAN_POINT('Ctrl Pts',(-8.83801245900005,15.2,5.90907897599998));
#248455=CARTESIAN_POINT('Ctrl Pts',(-8.83801245900005,11.6,5.90907897599998));
#248456=CARTESIAN_POINT('Ctrl Pts',(-8.83652080300006,15.2,5.90746439799998));
#248457=CARTESIAN_POINT('Ctrl Pts',(-8.83652080300006,11.6,5.90746439799998));
#248458=CARTESIAN_POINT('Ctrl Pts',(-8.83503225700006,15.2,5.90585604699999));
#248459=CARTESIAN_POINT('Ctrl Pts',(-8.83503225700006,11.6,5.90585604699999));
#248460=CARTESIAN_POINT('Ctrl Pts',(-8.83354683900006,15.2,5.90425392799999));
#248461=CARTESIAN_POINT('Ctrl Pts',(-8.83354683900006,11.6,5.90425392799999));
#248462=CARTESIAN_POINT('Ctrl Pts',(-8.83206456600006,15.2,5.90265804399999));
#248463=CARTESIAN_POINT('Ctrl Pts',(-8.83206456600006,11.6,5.90265804399999));
#248464=CARTESIAN_POINT('Ctrl Pts',(-8.83058545500005,15.2,5.90106839599999));
#248465=CARTESIAN_POINT('Ctrl Pts',(-8.83058545500005,11.6,5.90106839599999));
#248466=CARTESIAN_POINT('Ctrl Pts',(-8.82910952400006,15.2,5.89948498899999));
#248467=CARTESIAN_POINT('Ctrl Pts',(-8.82910952400006,11.6,5.89948498899999));
#248468=CARTESIAN_POINT('Ctrl Pts',(-8.82763679000006,15.2,5.89790782499998));
#248469=CARTESIAN_POINT('Ctrl Pts',(-8.82763679000006,11.6,5.89790782499998));
#248470=CARTESIAN_POINT('Ctrl Pts',(-8.82616727000006,15.2,5.89633690599998));
#248471=CARTESIAN_POINT('Ctrl Pts',(-8.82616727000006,11.6,5.89633690599998));
#248472=CARTESIAN_POINT('Ctrl Pts',(-8.82470098300006,15.2,5.89477223799998));
#248473=CARTESIAN_POINT('Ctrl Pts',(-8.82470098300006,11.6,5.89477223799998));
#248474=CARTESIAN_POINT('Ctrl Pts',(-8.82323794700006,15.2,5.89321382099998));
#248475=CARTESIAN_POINT('Ctrl Pts',(-8.82323794700006,11.6,5.89321382099998));
#248476=CARTESIAN_POINT('Ctrl Pts',(-8.82177817700006,15.2,5.89166165899999));
#248477=CARTESIAN_POINT('Ctrl Pts',(-8.82177817700006,11.6,5.89166165899999));
#248478=CARTESIAN_POINT('Ctrl Pts',(-8.82032169200006,15.2,5.89011575499998));
#248479=CARTESIAN_POINT('Ctrl Pts',(-8.82032169200006,11.6,5.89011575499998));
#248480=CARTESIAN_POINT('Ctrl Pts',(-8.81886850900005,15.2,5.88857611299999));
#248481=CARTESIAN_POINT('Ctrl Pts',(-8.81886850900005,11.6,5.88857611299999));
#248482=CARTESIAN_POINT('Ctrl Pts',(-8.81741864900006,15.2,5.88704273299999));
#248483=CARTESIAN_POINT('Ctrl Pts',(-8.81741864900006,11.6,5.88704273299999));
#248484=CARTESIAN_POINT('Ctrl Pts',(-8.81597212600006,15.2,5.88551562099998));
#248485=CARTESIAN_POINT('Ctrl Pts',(-8.81597212600006,11.6,5.88551562099998));
#248486=CARTESIAN_POINT('Ctrl Pts',(-8.81452896000006,15.2,5.88399477899999));
#248487=CARTESIAN_POINT('Ctrl Pts',(-8.81452896000006,11.6,5.88399477899999));
#248488=CARTESIAN_POINT('Ctrl Pts',(-8.81308916900006,15.2,5.88248020899999));
#248489=CARTESIAN_POINT('Ctrl Pts',(-8.81308916900006,11.6,5.88248020899999));
#248490=CARTESIAN_POINT('Ctrl Pts',(-8.81165277000006,15.2,5.88097191699998));
#248491=CARTESIAN_POINT('Ctrl Pts',(-8.81165277000006,11.6,5.88097191699998));
#248492=CARTESIAN_POINT('Ctrl Pts',(-8.81021978200006,15.2,5.87946990199999));
#248493=CARTESIAN_POINT('Ctrl Pts',(-8.81021978200006,11.6,5.87946990199999));
#248494=CARTESIAN_POINT('Ctrl Pts',(-8.80879022300006,15.2,5.87797416799998));
#248495=CARTESIAN_POINT('Ctrl Pts',(-8.80879022300006,11.6,5.87797416799998));
#248496=CARTESIAN_POINT('Ctrl Pts',(-8.80736411200006,15.2,5.87648471999999));
#248497=CARTESIAN_POINT('Ctrl Pts',(-8.80736411200006,11.6,5.87648471999999));
#248498=CARTESIAN_POINT('Ctrl Pts',(-8.80594146500006,15.2,5.87500155999999));
#248499=CARTESIAN_POINT('Ctrl Pts',(-8.80594146500006,11.6,5.87500155999999));
#248500=CARTESIAN_POINT('Ctrl Pts',(-8.80452230200006,15.2,5.87352468799998));
#248501=CARTESIAN_POINT('Ctrl Pts',(-8.80452230200006,11.6,5.87352468799998));
#248502=CARTESIAN_POINT('Ctrl Pts',(-8.80310664300006,15.2,5.87205411199999));
#248503=CARTESIAN_POINT('Ctrl Pts',(-8.80310664300006,11.6,5.87205411199999));
#248504=CARTESIAN_POINT('Ctrl Pts',(-8.80169450400006,15.2,5.87058983199999));
#248505=CARTESIAN_POINT('Ctrl Pts',(-8.80169450400006,11.6,5.87058983199999));
#248506=CARTESIAN_POINT('Ctrl Pts',(-8.80028590400006,15.2,5.86913184999998));
#248507=CARTESIAN_POINT('Ctrl Pts',(-8.80028590400006,11.6,5.86913184999998));
#248508=CARTESIAN_POINT('Ctrl Pts',(-8.79888086200006,15.2,5.86768017199999));
#248509=CARTESIAN_POINT('Ctrl Pts',(-8.79888086200006,11.6,5.86768017199999));
#248510=CARTESIAN_POINT('Ctrl Pts',(-8.79747939700006,15.2,5.86623479899998));
#248511=CARTESIAN_POINT('Ctrl Pts',(-8.79747939700006,11.6,5.86623479899998));
#248512=CARTESIAN_POINT('Ctrl Pts',(-8.79608152800006,15.2,5.86479573299999));
#248513=CARTESIAN_POINT('Ctrl Pts',(-8.79608152800006,11.6,5.86479573299999));
#248514=CARTESIAN_POINT('Ctrl Pts',(-8.79468727200006,15.2,5.86336297899998));
#248515=CARTESIAN_POINT('Ctrl Pts',(-8.79468727200006,11.6,5.86336297899998));
#248516=CARTESIAN_POINT('Ctrl Pts',(-8.79329665000006,15.2,5.86193653899999));
#248517=CARTESIAN_POINT('Ctrl Pts',(-8.79329665000006,11.6,5.86193653899999));
#248518=CARTESIAN_POINT('Ctrl Pts',(-8.79190968000006,15.2,5.86051641499999));
#248519=CARTESIAN_POINT('Ctrl Pts',(-8.79190968000006,11.6,5.86051641499999));
#248520=CARTESIAN_POINT('Ctrl Pts',(-8.79052638100006,15.2,5.85910261299999));
#248521=CARTESIAN_POINT('Ctrl Pts',(-8.79052638100006,11.6,5.85910261299999));
#248522=CARTESIAN_POINT('Ctrl Pts',(-8.78914677300006,15.2,5.85769513199998));
#248523=CARTESIAN_POINT('Ctrl Pts',(-8.78914677300006,11.6,5.85769513199998));
#248524=CARTESIAN_POINT('Ctrl Pts',(-8.78777087400006,15.2,5.85629397699999));
#248525=CARTESIAN_POINT('Ctrl Pts',(-8.78777087400006,11.6,5.85629397699999));
#248526=CARTESIAN_POINT('Ctrl Pts',(-8.78639870300006,15.2,5.85489915099998));
#248527=CARTESIAN_POINT('Ctrl Pts',(-8.78639870300006,11.6,5.85489915099998));
#248528=CARTESIAN_POINT('Ctrl Pts',(-8.78503028000006,15.2,5.85351065699999));
#248529=CARTESIAN_POINT('Ctrl Pts',(-8.78503028000006,11.6,5.85351065699999));
#248530=CARTESIAN_POINT('Ctrl Pts',(-8.78366562500006,15.2,5.85212849699998));
#248531=CARTESIAN_POINT('Ctrl Pts',(-8.78366562500006,11.6,5.85212849699998));
#248532=CARTESIAN_POINT('Ctrl Pts',(-8.78230475700006,15.2,5.85075267399999));
#248533=CARTESIAN_POINT('Ctrl Pts',(-8.78230475700006,11.6,5.85075267399999));
#248534=CARTESIAN_POINT('Ctrl Pts',(-8.78094769300005,15.2,5.84938319199999));
#248535=CARTESIAN_POINT('Ctrl Pts',(-8.78094769300005,11.6,5.84938319199999));
#248536=CARTESIAN_POINT('Ctrl Pts',(-8.77959445700006,15.2,5.84802005299998));
#248537=CARTESIAN_POINT('Ctrl Pts',(-8.77959445700006,11.6,5.84802005299998));
#248538=CARTESIAN_POINT('Ctrl Pts',(-8.77824506500006,15.2,5.84666325999999));
#248539=CARTESIAN_POINT('Ctrl Pts',(-8.77824506500006,11.6,5.84666325999999));
#248540=CARTESIAN_POINT('Ctrl Pts',(-8.77689953800006,15.2,5.84531281599999));
#248541=CARTESIAN_POINT('Ctrl Pts',(-8.77689953800006,11.6,5.84531281599999));
#248542=CARTESIAN_POINT('Ctrl Pts',(-8.77555789700006,15.2,5.84396872499998));
#248543=CARTESIAN_POINT('Ctrl Pts',(-8.77555789700006,11.6,5.84396872499998));
#248544=CARTESIAN_POINT('Ctrl Pts',(-8.77422015900006,15.2,5.84263098799998));
#248545=CARTESIAN_POINT('Ctrl Pts',(-8.77422015900006,11.6,5.84263098799998));
#248546=CARTESIAN_POINT('Ctrl Pts',(-8.77288634600006,15.2,5.84129960899999));
#248547=CARTESIAN_POINT('Ctrl Pts',(-8.77288634600006,11.6,5.84129960899999));
#248548=CARTESIAN_POINT('Ctrl Pts',(-8.77155647800006,15.2,5.83997458999999));
#248549=CARTESIAN_POINT('Ctrl Pts',(-8.77155647800006,11.6,5.83997458999999));
#248550=CARTESIAN_POINT('Ctrl Pts',(-8.77023057400006,15.2,5.83865593399998));
#248551=CARTESIAN_POINT('Ctrl Pts',(-8.77023057400006,11.6,5.83865593399998));
#248552=CARTESIAN_POINT('Ctrl Pts',(-8.76890865500006,15.2,5.83734364499998));
#248553=CARTESIAN_POINT('Ctrl Pts',(-8.76890865500006,11.6,5.83734364499998));
#248554=CARTESIAN_POINT('Ctrl Pts',(-8.76759074100006,15.2,5.83603772599999));
#248555=CARTESIAN_POINT('Ctrl Pts',(-8.76759074100006,11.6,5.83603772599999));
#248556=CARTESIAN_POINT('Ctrl Pts',(-8.76627685200006,15.2,5.83473817899999));
#248557=CARTESIAN_POINT('Ctrl Pts',(-8.76627685200006,11.6,5.83473817899999));
#248558=CARTESIAN_POINT('Ctrl Pts',(-8.76496700900006,15.2,5.83344500699998));
#248559=CARTESIAN_POINT('Ctrl Pts',(-8.76496700900006,11.6,5.83344500699998));
#248560=CARTESIAN_POINT('Ctrl Pts',(-8.76366123100006,15.2,5.83215821299999));
#248561=CARTESIAN_POINT('Ctrl Pts',(-8.76366123100006,11.6,5.83215821299999));
#248562=CARTESIAN_POINT('Ctrl Pts',(-8.76235953900006,15.2,5.83087779999998));
#248563=CARTESIAN_POINT('Ctrl Pts',(-8.76235953900006,11.6,5.83087779999998));
#248564=CARTESIAN_POINT('Ctrl Pts',(-8.76106195600006,15.2,5.82960376999999));
#248565=CARTESIAN_POINT('Ctrl Pts',(-8.76106195600006,11.6,5.82960376999999));
#248566=CARTESIAN_POINT('Ctrl Pts',(-8.75976849800006,15.2,5.82833612699999));
#248567=CARTESIAN_POINT('Ctrl Pts',(-8.75976849800006,11.6,5.82833612699999));
#248568=CARTESIAN_POINT('Ctrl Pts',(-8.75847919000006,15.2,5.82707487399999));
#248569=CARTESIAN_POINT('Ctrl Pts',(-8.75847919000006,11.6,5.82707487399999));
#248570=CARTESIAN_POINT('Ctrl Pts',(-8.75719405100006,15.2,5.82582001299999));
#248571=CARTESIAN_POINT('Ctrl Pts',(-8.75719405100006,11.6,5.82582001299999));
#248572=CARTESIAN_POINT('Ctrl Pts',(-8.75591310200006,15.2,5.82457154599999));
#248573=CARTESIAN_POINT('Ctrl Pts',(-8.75591310200006,11.6,5.82457154599999));
#248574=CARTESIAN_POINT('Ctrl Pts',(-8.75463636300006,15.2,5.82332947899998));
#248575=CARTESIAN_POINT('Ctrl Pts',(-8.75463636300006,11.6,5.82332947899998));
#248576=CARTESIAN_POINT('Ctrl Pts',(-8.75336385700006,15.2,5.82209381199998));
#248577=CARTESIAN_POINT('Ctrl Pts',(-8.75336385700006,11.6,5.82209381199998));
#248578=CARTESIAN_POINT('Ctrl Pts',(-8.75209560400006,15.2,5.82086454899999));
#248579=CARTESIAN_POINT('Ctrl Pts',(-8.75209560400006,11.6,5.82086454899999));
#248580=CARTESIAN_POINT('Ctrl Pts',(-8.75083162500006,15.2,5.81964169299999));
#248581=CARTESIAN_POINT('Ctrl Pts',(-8.75083162500006,11.6,5.81964169299999));
#248582=CARTESIAN_POINT('Ctrl Pts',(-8.74957194200006,15.2,5.81842524699999));
#248583=CARTESIAN_POINT('Ctrl Pts',(-8.74957194200006,11.6,5.81842524699999));
#248584=CARTESIAN_POINT('Ctrl Pts',(-8.74831657500006,15.2,5.81721521199999));
#248585=CARTESIAN_POINT('Ctrl Pts',(-8.74831657500006,11.6,5.81721521199999));
#248586=CARTESIAN_POINT('Ctrl Pts',(-8.74706554700006,15.2,5.81601159299999));
#248587=CARTESIAN_POINT('Ctrl Pts',(-8.74706554700006,11.6,5.81601159299999));
#248588=CARTESIAN_POINT('Ctrl Pts',(-8.74581887900005,15.2,5.81481439299999));
#248589=CARTESIAN_POINT('Ctrl Pts',(-8.74581887900005,11.6,5.81481439299999));
#248590=CARTESIAN_POINT('Ctrl Pts',(-8.74457659200005,15.2,5.81362361299998));
#248591=CARTESIAN_POINT('Ctrl Pts',(-8.74457659200005,11.6,5.81362361299998));
#248592=CARTESIAN_POINT('Ctrl Pts',(-8.74333870800006,15.2,5.81243925699999));
#248593=CARTESIAN_POINT('Ctrl Pts',(-8.74333870800006,11.6,5.81243925699999));
#248594=CARTESIAN_POINT('Ctrl Pts',(-8.74210524900005,15.2,5.81126132799999));
#248595=CARTESIAN_POINT('Ctrl Pts',(-8.74210524900005,11.6,5.81126132799999));
#248596=CARTESIAN_POINT('Ctrl Pts',(-8.74087623700006,15.2,5.81008982799998));
#248597=CARTESIAN_POINT('Ctrl Pts',(-8.74087623700006,11.6,5.81008982799998));
#248598=CARTESIAN_POINT('Ctrl Pts',(-8.73965169200006,15.2,5.80892475999998));
#248599=CARTESIAN_POINT('Ctrl Pts',(-8.73965169200006,11.6,5.80892475999998));
#248600=CARTESIAN_POINT('Ctrl Pts',(-8.73843163900006,15.2,5.80776612799998));
#248601=CARTESIAN_POINT('Ctrl Pts',(-8.73843163900006,11.6,5.80776612799998));
#248602=CARTESIAN_POINT('Ctrl Pts',(-8.73721609900005,15.2,5.80661393499999));
#248603=CARTESIAN_POINT('Ctrl Pts',(-8.73721609900005,11.6,5.80661393499999));
#248604=CARTESIAN_POINT('Ctrl Pts',(-8.73600509400006,15.2,5.80546818099998));
#248605=CARTESIAN_POINT('Ctrl Pts',(-8.73600509400006,11.6,5.80546818099998));
#248606=CARTESIAN_POINT('Ctrl Pts',(-8.73479864500006,15.2,5.80432887199999));
#248607=CARTESIAN_POINT('Ctrl Pts',(-8.73479864500006,11.6,5.80432887199999));
#248608=CARTESIAN_POINT('Ctrl Pts',(-8.73359677600006,15.2,5.80319600899998));
#248609=CARTESIAN_POINT('Ctrl Pts',(-8.73359677600006,11.6,5.80319600899998));
#248610=CARTESIAN_POINT('Ctrl Pts',(-8.73239951000006,15.2,5.80206959599998));
#248611=CARTESIAN_POINT('Ctrl Pts',(-8.73239951000006,11.6,5.80206959599998));
#248612=CARTESIAN_POINT('Ctrl Pts',(-8.73120686700006,15.2,5.80094963499998));
#248613=CARTESIAN_POINT('Ctrl Pts',(-8.73120686700006,11.6,5.80094963499998));
#248614=CARTESIAN_POINT('Ctrl Pts',(-8.73001887200006,15.2,5.79983612899999));
#248615=CARTESIAN_POINT('Ctrl Pts',(-8.73001887200006,11.6,5.79983612899999));
#248616=CARTESIAN_POINT('Ctrl Pts',(-8.72883554600006,15.2,5.79872908099999));
#248617=CARTESIAN_POINT('Ctrl Pts',(-8.72883554600006,11.6,5.79872908099999));
#248618=CARTESIAN_POINT('Ctrl Pts',(-8.72765691300006,15.2,5.79762849299998));
#248619=CARTESIAN_POINT('Ctrl Pts',(-8.72765691300006,11.6,5.79762849299998));
#248620=CARTESIAN_POINT('Ctrl Pts',(-8.72648299600005,15.2,5.79653436899999));
#248621=CARTESIAN_POINT('Ctrl Pts',(-8.72648299600005,11.6,5.79653436899999));
#248622=CARTESIAN_POINT('Ctrl Pts',(-8.72531381600006,15.2,5.79544671199999));
#248623=CARTESIAN_POINT('Ctrl Pts',(-8.72531381600006,11.6,5.79544671199999));
#248624=CARTESIAN_POINT('Ctrl Pts',(-8.72414939900005,15.2,5.79436552399999));
#248625=CARTESIAN_POINT('Ctrl Pts',(-8.72414939900005,11.6,5.79436552399999));
#248626=CARTESIAN_POINT('Ctrl Pts',(-8.72298976600005,15.2,5.79329080799998));
#248627=CARTESIAN_POINT('Ctrl Pts',(-8.72298976600005,11.6,5.79329080799998));
#248628=CARTESIAN_POINT('Ctrl Pts',(-8.72183494200006,15.2,5.79222256599999));
#248629=CARTESIAN_POINT('Ctrl Pts',(-8.72183494200006,11.6,5.79222256599999));
#248630=CARTESIAN_POINT('Ctrl Pts',(-8.72068494800006,15.2,5.79116080199999));
#248631=CARTESIAN_POINT('Ctrl Pts',(-8.72068494800006,11.6,5.79116080199999));
#248632=CARTESIAN_POINT('Ctrl Pts',(-8.71953981000006,15.2,5.79010551899999));
#248633=CARTESIAN_POINT('Ctrl Pts',(-8.71953981000006,11.6,5.79010551899999));
#248634=CARTESIAN_POINT('Ctrl Pts',(-8.71839954900006,15.2,5.78905671899999));
#248635=CARTESIAN_POINT('Ctrl Pts',(-8.71839954900006,11.6,5.78905671899999));
#248636=CARTESIAN_POINT('Ctrl Pts',(-8.71726419000005,15.2,5.78801440599998));
#248637=CARTESIAN_POINT('Ctrl Pts',(-8.71726419000005,11.6,5.78801440599998));
#248638=CARTESIAN_POINT('Ctrl Pts',(-8.71613375600005,15.2,5.78697858099999));
#248639=CARTESIAN_POINT('Ctrl Pts',(-8.71613375600005,11.6,5.78697858099999));
#248640=CARTESIAN_POINT('Ctrl Pts',(-8.71500827300006,15.2,5.78594924699999));
#248641=CARTESIAN_POINT('Ctrl Pts',(-8.71500827300006,11.6,5.78594924699999));
#248642=CARTESIAN_POINT('Ctrl Pts',(-8.71388776300006,15.2,5.78492640799999));
#248643=CARTESIAN_POINT('Ctrl Pts',(-8.71388776300006,11.6,5.78492640799999));
#248644=CARTESIAN_POINT('Ctrl Pts',(-8.71277225000006,15.2,5.78391006599999));
#248645=CARTESIAN_POINT('Ctrl Pts',(-8.71277225000006,11.6,5.78391006599999));
#248646=CARTESIAN_POINT('Ctrl Pts',(-8.71166175800006,15.2,5.78290022499999));
#248647=CARTESIAN_POINT('Ctrl Pts',(-8.71166175800006,11.6,5.78290022499999));
#248648=CARTESIAN_POINT('Ctrl Pts',(-8.71055631300005,15.2,5.78189688699998));
#248649=CARTESIAN_POINT('Ctrl Pts',(-8.71055631300005,11.6,5.78189688699998));
#248650=CARTESIAN_POINT('Ctrl Pts',(-8.70945593700006,15.2,5.78090005399999));
#248651=CARTESIAN_POINT('Ctrl Pts',(-8.70945593700006,11.6,5.78090005399999));
#248652=CARTESIAN_POINT('Ctrl Pts',(-8.70836065600006,15.2,5.77990972999999));
#248653=CARTESIAN_POINT('Ctrl Pts',(-8.70836065600006,11.6,5.77990972999999));
#248654=CARTESIAN_POINT('Ctrl Pts',(-8.70727049400006,15.2,5.77892591699998));
#248655=CARTESIAN_POINT('Ctrl Pts',(-8.70727049400006,11.6,5.77892591699998));
#248656=CARTESIAN_POINT('Ctrl Pts',(-8.70618547400005,15.2,5.77794861799998));
#248657=CARTESIAN_POINT('Ctrl Pts',(-8.70618547400005,11.6,5.77794861799998));
#248658=CARTESIAN_POINT('Ctrl Pts',(-8.70510562500005,15.2,5.77697783599999));
#248659=CARTESIAN_POINT('Ctrl Pts',(-8.70510562500005,11.6,5.77697783599999));
#248660=CARTESIAN_POINT('Ctrl Pts',(-8.70403096800005,15.2,5.77601357299999));
#248661=CARTESIAN_POINT('Ctrl Pts',(-8.70403096800005,11.6,5.77601357299999));
#248662=CARTESIAN_POINT('Ctrl Pts',(-8.70296152800006,15.2,5.77505583299998));
#248663=CARTESIAN_POINT('Ctrl Pts',(-8.70296152800006,11.6,5.77505583299998));
#248664=CARTESIAN_POINT('Ctrl Pts',(-8.70189733300006,15.2,5.77410461799998));
#248665=CARTESIAN_POINT('Ctrl Pts',(-8.70189733300006,11.6,5.77410461799998));
#248666=CARTESIAN_POINT('Ctrl Pts',(-8.70083840400006,15.2,5.77315993199999));
#248667=CARTESIAN_POINT('Ctrl Pts',(-8.70083840400006,11.6,5.77315993199999));
#248668=CARTESIAN_POINT('Ctrl Pts',(-8.69978477000006,15.2,5.77222177599998));
#248669=CARTESIAN_POINT('Ctrl Pts',(-8.69978477000006,11.6,5.77222177599998));
#248670=CARTESIAN_POINT('Ctrl Pts',(-8.69873645500006,15.2,5.77129015299998));
#248671=CARTESIAN_POINT('Ctrl Pts',(-8.69873645500006,11.6,5.77129015299998));
#248672=CARTESIAN_POINT('Ctrl Pts',(-8.69769348400006,15.2,5.77036506799999));
#248673=CARTESIAN_POINT('Ctrl Pts',(-8.69769348400006,11.6,5.77036506799999));
#248674=CARTESIAN_POINT('Ctrl Pts',(-8.69665588300006,15.2,5.76944652099999));
#248675=CARTESIAN_POINT('Ctrl Pts',(-8.69665588300006,11.6,5.76944652099999));
#248676=CARTESIAN_POINT('Ctrl Pts',(-8.69562367700006,15.2,5.76853451599998));
#248677=CARTESIAN_POINT('Ctrl Pts',(-8.69562367700006,11.6,5.76853451599998));
#248678=CARTESIAN_POINT('Ctrl Pts',(-8.69459689400006,15.2,5.76762905499999));
#248679=CARTESIAN_POINT('Ctrl Pts',(-8.69459689400006,11.6,5.76762905499999));
#248680=CARTESIAN_POINT('Ctrl Pts',(-8.69357555800006,15.2,5.76673014199999));
#248681=CARTESIAN_POINT('Ctrl Pts',(-8.69357555800006,11.6,5.76673014199999));
#248682=CARTESIAN_POINT('Ctrl Pts',(-8.69255969400006,15.2,5.76583777999998));
#248683=CARTESIAN_POINT('Ctrl Pts',(-8.69255969400006,11.6,5.76583777999998));
#248684=CARTESIAN_POINT('Ctrl Pts',(-8.69154933000006,15.2,5.76495196899998));
#248685=CARTESIAN_POINT('Ctrl Pts',(-8.69154933000006,11.6,5.76495196899998));
#248686=CARTESIAN_POINT('Ctrl Pts',(-8.69054449300006,15.2,5.76407271599999));
#248687=CARTESIAN_POINT('Ctrl Pts',(-8.69054449300006,11.6,5.76407271599999));
#248688=CARTESIAN_POINT('Ctrl Pts',(-8.68954520600006,15.2,5.76320001999999));
#248689=CARTESIAN_POINT('Ctrl Pts',(-8.68954520600006,11.6,5.76320001999999));
#248690=CARTESIAN_POINT('Ctrl Pts',(-8.68855149800006,15.2,5.76233388499999));
#248691=CARTESIAN_POINT('Ctrl Pts',(-8.68855149800006,11.6,5.76233388499999));
#248692=CARTESIAN_POINT('Ctrl Pts',(-8.68756339700005,15.2,5.76147431599999));
#248693=CARTESIAN_POINT('Ctrl Pts',(-8.68756339700005,11.6,5.76147431599999));
#248694=CARTESIAN_POINT('Ctrl Pts',(-8.68658092700005,15.2,5.76062131199999));
#248695=CARTESIAN_POINT('Ctrl Pts',(-8.68658092700005,11.6,5.76062131199999));
#248696=CARTESIAN_POINT('Ctrl Pts',(-8.68560411500006,15.2,5.75977487799998));
#248697=CARTESIAN_POINT('Ctrl Pts',(-8.68560411500006,11.6,5.75977487799998));
#248698=CARTESIAN_POINT('Ctrl Pts',(-8.68463299000006,15.2,5.75893501599998));
#248699=CARTESIAN_POINT('Ctrl Pts',(-8.68463299000006,11.6,5.75893501599998));
#248700=CARTESIAN_POINT('Ctrl Pts',(-8.68366757600005,15.2,5.75810172899998));
#248701=CARTESIAN_POINT('Ctrl Pts',(-8.68366757600005,11.6,5.75810172899998));
#248702=CARTESIAN_POINT('Ctrl Pts',(-8.68270790300006,15.2,5.75727502099999));
#248703=CARTESIAN_POINT('Ctrl Pts',(-8.68270790300006,11.6,5.75727502099999));
#248704=CARTESIAN_POINT('Ctrl Pts',(-8.68175399700006,15.2,5.75645489199999));
#248705=CARTESIAN_POINT('Ctrl Pts',(-8.68175399700006,11.6,5.75645489199999));
#248706=CARTESIAN_POINT('Ctrl Pts',(-8.68080588600005,15.2,5.75564134699999));
#248707=CARTESIAN_POINT('Ctrl Pts',(-8.68080588600005,11.6,5.75564134699999));
#248708=CARTESIAN_POINT('Ctrl Pts',(-8.67986359800006,15.2,5.75483438799999));
#248709=CARTESIAN_POINT('Ctrl Pts',(-8.67986359800006,11.6,5.75483438799999));
#248710=CARTESIAN_POINT('Ctrl Pts',(-8.67892715900006,15.2,5.75403401799999));
#248711=CARTESIAN_POINT('Ctrl Pts',(-8.67892715900006,11.6,5.75403401799999));
#248712=CARTESIAN_POINT('Ctrl Pts',(-8.67799659800006,15.2,5.75324023999999));
#248713=CARTESIAN_POINT('Ctrl Pts',(-8.67799659800006,11.6,5.75324023999999));
#248714=CARTESIAN_POINT('Ctrl Pts',(-8.67707194300005,15.2,5.75245305599999));
#248715=CARTESIAN_POINT('Ctrl Pts',(-8.67707194300005,11.6,5.75245305599999));
#248716=CARTESIAN_POINT('Ctrl Pts',(-8.67615322100006,15.2,5.75167246799998));
#248717=CARTESIAN_POINT('Ctrl Pts',(-8.67615322100006,11.6,5.75167246799998));
#248718=CARTESIAN_POINT('Ctrl Pts',(-8.67524046200005,15.2,5.75089848099999));
#248719=CARTESIAN_POINT('Ctrl Pts',(-8.67524046200005,11.6,5.75089848099999));
#248720=CARTESIAN_POINT('Ctrl Pts',(-8.67433369300005,15.2,5.75013109599999));
#248721=CARTESIAN_POINT('Ctrl Pts',(-8.67433369300005,11.6,5.75013109599999));
#248722=CARTESIAN_POINT('Ctrl Pts',(-8.67343294200005,15.2,5.74937031599998));
#248723=CARTESIAN_POINT('Ctrl Pts',(-8.67343294200005,11.6,5.74937031599998));
#248724=CARTESIAN_POINT('Ctrl Pts',(-8.67253824000005,15.2,5.74861614399998));
#248725=CARTESIAN_POINT('Ctrl Pts',(-8.67253824000005,11.6,5.74861614399998));
#248726=CARTESIAN_POINT('Ctrl Pts',(-8.67164961300006,15.2,5.74786858299999));
#248727=CARTESIAN_POINT('Ctrl Pts',(-8.67164961300006,11.6,5.74786858299999));
#248728=CARTESIAN_POINT('Ctrl Pts',(-8.67076709100006,15.2,5.74712763599998));
#248729=CARTESIAN_POINT('Ctrl Pts',(-8.67076709100006,11.6,5.74712763599998));
#248730=CARTESIAN_POINT('Ctrl Pts',(-8.66989070400006,15.2,5.74639330399998));
#248731=CARTESIAN_POINT('Ctrl Pts',(-8.66989070400006,11.6,5.74639330399998));
#248732=CARTESIAN_POINT('Ctrl Pts',(-8.66902047900006,15.2,5.74566559199998));
#248733=CARTESIAN_POINT('Ctrl Pts',(-8.66902047900006,11.6,5.74566559199998));
#248734=CARTESIAN_POINT('Ctrl Pts',(-8.66815644700005,15.2,5.74494450199998));
#248735=CARTESIAN_POINT('Ctrl Pts',(-8.66815644700005,11.6,5.74494450199998));
#248736=CARTESIAN_POINT('Ctrl Pts',(-8.66729863700006,15.2,5.74423003599998));
#248737=CARTESIAN_POINT('Ctrl Pts',(-8.66729863700006,11.6,5.74423003599998));
#248738=CARTESIAN_POINT('Ctrl Pts',(-8.66644707700006,15.2,5.74352219699998));
#248739=CARTESIAN_POINT('Ctrl Pts',(-8.66644707700006,11.6,5.74352219699998));
#248740=CARTESIAN_POINT('Ctrl Pts',(-8.66560179900006,15.2,5.74282098699998));
#248741=CARTESIAN_POINT('Ctrl Pts',(-8.66560179900006,11.6,5.74282098699998));
#248742=CARTESIAN_POINT('Ctrl Pts',(-8.66476283200006,15.2,5.74212641099999));
#248743=CARTESIAN_POINT('Ctrl Pts',(-8.66476283200006,11.6,5.74212641099999));
#248744=CARTESIAN_POINT('Ctrl Pts',(-8.66393020600006,15.2,5.74143846999998));
#248745=CARTESIAN_POINT('Ctrl Pts',(-8.66393020600006,11.6,5.74143846999998));
#248746=CARTESIAN_POINT('Ctrl Pts',(-8.66310395100006,15.2,5.74075716599998));
#248747=CARTESIAN_POINT('Ctrl Pts',(-8.66310395100006,11.6,5.74075716599998));
#248748=CARTESIAN_POINT('Ctrl Pts',(-8.66228409600006,15.2,5.74008250399999));
#248749=CARTESIAN_POINT('Ctrl Pts',(-8.66228409600006,11.6,5.74008250399999));
#248750=CARTESIAN_POINT('Ctrl Pts',(-8.66147067400006,15.2,5.73941448499999));
#248751=CARTESIAN_POINT('Ctrl Pts',(-8.66147067400006,11.6,5.73941448499999));
#248752=CARTESIAN_POINT('Ctrl Pts',(-8.66066371400006,15.2,5.73875311199998));
#248753=CARTESIAN_POINT('Ctrl Pts',(-8.66066371400006,11.6,5.73875311199998));
#248754=CARTESIAN_POINT('Ctrl Pts',(-8.65986324600006,15.2,5.73809838799999));
#248755=CARTESIAN_POINT('Ctrl Pts',(-8.65986324600006,11.6,5.73809838799999));
#248756=CARTESIAN_POINT('Ctrl Pts',(-8.65906930300006,15.2,5.73745031599999));
#248757=CARTESIAN_POINT('Ctrl Pts',(-8.65906930300006,11.6,5.73745031599999));
#248758=CARTESIAN_POINT('Ctrl Pts',(-8.65828191300006,15.2,5.73680889799999));
#248759=CARTESIAN_POINT('Ctrl Pts',(-8.65828191300006,11.6,5.73680889799999));
#248760=CARTESIAN_POINT('Ctrl Pts',(-8.65750111000006,15.2,5.73617413799998));
#248761=CARTESIAN_POINT('Ctrl Pts',(-8.65750111000006,11.6,5.73617413799998));
#248762=CARTESIAN_POINT('Ctrl Pts',(-8.65672692500006,15.2,5.73554603699999));
#248763=CARTESIAN_POINT('Ctrl Pts',(-8.65672692500006,11.6,5.73554603699999));
#248764=CARTESIAN_POINT('Ctrl Pts',(-8.65595938700006,15.2,5.73492459899998));
#248765=CARTESIAN_POINT('Ctrl Pts',(-8.65595938700006,11.6,5.73492459899998));
#248766=CARTESIAN_POINT('Ctrl Pts',(-8.65519853100006,15.2,5.73430982499998));
#248767=CARTESIAN_POINT('Ctrl Pts',(-8.65519853100006,11.6,5.73430982499998));
#248768=CARTESIAN_POINT('Ctrl Pts',(-8.65444438600005,15.2,5.73370172099998));
#248769=CARTESIAN_POINT('Ctrl Pts',(-8.65444438600005,11.6,5.73370172099998));
#248770=CARTESIAN_POINT('Ctrl Pts',(-8.65369698500006,15.2,5.73310028599998));
#248771=CARTESIAN_POINT('Ctrl Pts',(-8.65369698500006,11.6,5.73310028599998));
#248772=CARTESIAN_POINT('Ctrl Pts',(-8.65295636100005,15.2,5.73250552499999));
#248773=CARTESIAN_POINT('Ctrl Pts',(-8.65295636100005,11.6,5.73250552499999));
#248774=CARTESIAN_POINT('Ctrl Pts',(-8.65222254500006,15.2,5.73191744099999));
#248775=CARTESIAN_POINT('Ctrl Pts',(-8.65222254500006,11.6,5.73191744099999));
#248776=CARTESIAN_POINT('Ctrl Pts',(-8.65149557000005,15.2,5.73133603499999));
#248777=CARTESIAN_POINT('Ctrl Pts',(-8.65149557000005,11.6,5.73133603499999));
#248778=CARTESIAN_POINT('Ctrl Pts',(-8.65077961600005,15.2,5.73076462099999));
#248779=CARTESIAN_POINT('Ctrl Pts',(-8.65077961600005,11.6,5.73076462099999));
#248780=CARTESIAN_POINT('Ctrl Pts',(-8.65021312700006,15.2,5.73031342099998));
#248781=CARTESIAN_POINT('Ctrl Pts',(-8.65021312700006,11.6,5.73031342099998));
#248782=CARTESIAN_POINT('Ctrl Pts',(-8.64979235000006,15.2,5.72997879199999));
#248783=CARTESIAN_POINT('Ctrl Pts',(-8.64979235000006,11.6,5.72997879199999));
#248784=CARTESIAN_POINT('Ctrl Pts',(-8.64951454400006,15.2,5.72975808599999));
#248785=CARTESIAN_POINT('Ctrl Pts',(-8.64951454400006,11.6,5.72975808599999));
#248786=CARTESIAN_POINT('Ctrl Pts',(-8.64937799900006,15.2,5.72964966099998));
#248787=CARTESIAN_POINT('Ctrl Pts',(-8.64937799900006,11.6,5.72964966099998));
#248788=CARTESIAN_POINT('',(-8.64937799900006,12.2,5.72964966099998));
#248789=CARTESIAN_POINT('',(-8.64937799900006,15.2,5.72964966099998));
#248790=CARTESIAN_POINT('',(-8.64937799900006,12.2,5.72964966099998));
#248791=CARTESIAN_POINT('Ctrl Pts',(-9.36775917500006,12.2,6.67046385499999));
#248792=CARTESIAN_POINT('Ctrl Pts',(-9.36593194966811,12.2,6.66710588438994));
#248793=CARTESIAN_POINT('Ctrl Pts',(-9.36410408846955,12.2,6.66375578663033));
#248794=CARTESIAN_POINT('Ctrl Pts',(-9.36227560168602,12.2,6.66041356487326));
#248795=CARTESIAN_POINT('Ctrl Pts',(-9.3604471149025,12.2,6.6570713431162));
#248796=CARTESIAN_POINT('Ctrl Pts',(-9.35861799862892,12.2,6.65373699652317));
#248797=CARTESIAN_POINT('Ctrl Pts',(-9.35678826960406,12.2,6.65041053364359));
#248798=CARTESIAN_POINT('Ctrl Pts',(-9.3549585405792,12.2,6.64708407076401));
#248799=CARTESIAN_POINT('Ctrl Pts',(-9.35312819903259,12.2,6.64376549048578));
#248800=CARTESIAN_POINT('Ctrl Pts',(-9.35129728493254,12.2,6.64045481048));
#248801=CARTESIAN_POINT('Ctrl Pts',(-9.34946637049987,12.2,6.63714412987279));
#248802=CARTESIAN_POINT('Ctrl Pts',(-9.34763488481701,12.2,6.6338413503261));
#248803=CARTESIAN_POINT('Ctrl Pts',(-9.34580287284235,12.2,6.63054648926499));
#248804=CARTESIAN_POINT('Ctrl Pts',(-9.34336019076417,12.2,6.62615334218112));
#248805=CARTESIAN_POINT('Ctrl Pts',(-9.34091657485832,12.2,6.62177427441485));
#248806=CARTESIAN_POINT('Ctrl Pts',(-9.33847210989155,12.2,6.61740932104856));
#248807=CARTESIAN_POINT('Ctrl Pts',(-9.33663876108321,12.2,6.61413560587517));
#248808=CARTESIAN_POINT('Ctrl Pts',(-9.33480493317988,12.2,6.61086982962563));
#248809=CARTESIAN_POINT('Ctrl Pts',(-9.33297066182161,12.2,6.60761200637198));
#248810=CARTESIAN_POINT('Ctrl Pts',(-9.33113639046334,12.2,6.60435418311835));
#248811=CARTESIAN_POINT('Ctrl Pts',(-9.32930167588341,12.2,6.60110431429001));
#248812=CARTESIAN_POINT('Ctrl Pts',(-9.32746655815845,12.2,6.59786241474));
#248813=CARTESIAN_POINT('Ctrl Pts',(-9.32563144010011,12.2,6.59462051460104));
#248814=CARTESIAN_POINT('Ctrl Pts',(-9.32379591863337,12.2,6.59138658449776));
#248815=CARTESIAN_POINT('Ctrl Pts',(-9.32196003307483,12.2,6.58816064028001));
#248816=CARTESIAN_POINT('Ctrl Pts',(-9.32012414784982,12.2,6.5849346966483));
#248817=CARTESIAN_POINT('Ctrl Pts',(-9.31828789801651,12.2,6.58171673809954));
#248818=CARTESIAN_POINT('Ctrl Pts',(-9.31645132174987,12.2,6.57850678092518));
#248819=CARTESIAN_POINT('Ctrl Pts',(-9.31461474548322,12.2,6.57529682375082));
#248820=CARTESIAN_POINT('Ctrl Pts',(-9.31277784255665,12.2,6.57209486617878));
#248821=CARTESIAN_POINT('Ctrl Pts',(-9.31094065178172,12.2,6.56890092644703));
#248822=CARTESIAN_POINT('Ctrl Pts',(-9.3091034610068,12.2,6.56570698671527));
#248823=CARTESIAN_POINT('Ctrl Pts',(-9.30726598200996,12.2,6.56252106221848));
#248824=CARTESIAN_POINT('Ctrl Pts',(-9.30542825427673,12.2,6.55934317052782));
#248825=CARTESIAN_POINT('Ctrl Pts',(-9.30359052654349,12.2,6.55616527883715));
#248826=CARTESIAN_POINT('Ctrl Pts',(-9.30175254971693,12.2,6.55299541844716));
#248827=CARTESIAN_POINT('Ctrl Pts',(-9.29991436399208,12.2,6.54983360581136));
#248828=CARTESIAN_POINT('Ctrl Pts',(-9.29807617826723,12.2,6.54667179317556));
#248829=CARTESIAN_POINT('Ctrl Pts',(-9.29623778278405,12.2,6.54351802758918));
#248830=CARTESIAN_POINT('Ctrl Pts',(-9.29439921714253,12.2,6.54037232545236));
#248831=CARTESIAN_POINT('Ctrl Pts',(-9.292560651167,12.2,6.53722662274407));
#248832=CARTESIAN_POINT('Ctrl Pts',(-9.29072191578313,12.2,6.53408898272142));
#248833=CARTESIAN_POINT('Ctrl Pts',(-9.28888304884919,12.2,6.5309594210177));
#248834=CARTESIAN_POINT('Ctrl Pts',(-9.28704418224932,12.2,6.52782985988251));
#248835=CARTESIAN_POINT('Ctrl Pts',(-9.28520518586931,12.2,6.52470837647246));
#248836=CARTESIAN_POINT('Ctrl Pts',(-9.2833660986359,12.2,6.52159498718097));
#248837=CARTESIAN_POINT('Ctrl Pts',(-9.2815270114025,12.2,6.51848159788949));
#248838=CARTESIAN_POINT('Ctrl Pts',(-9.2796878344161,12.2,6.5153763027159));
#248839=CARTESIAN_POINT('Ctrl Pts',(-9.27784860631625,12.2,6.51227911616247));
#248840=CARTESIAN_POINT('Ctrl Pts',(-9.2760093782164,12.2,6.50918192960904));
#248841=CARTESIAN_POINT('Ctrl Pts',(-9.27417010034989,12.2,6.50609285228798));
#248842=CARTESIAN_POINT('Ctrl Pts',(-9.27233081270839,12.2,6.50301189923325));
#248843=CARTESIAN_POINT('Ctrl Pts',(-9.27049152506689,12.2,6.49993094617853));
#248844=CARTESIAN_POINT('Ctrl Pts',(-9.26865222811705,12.2,6.49685811820683));
#248845=CARTESIAN_POINT('Ctrl Pts',(-9.26681296143387,12.2,6.49379343006745));
#248846=CARTESIAN_POINT('Ctrl Pts',(-9.26497369475068,12.2,6.49072874192807));
#248847=CARTESIAN_POINT('Ctrl Pts',(-9.26313445886751,12.2,6.48767219308817));
#248848=CARTESIAN_POINT('Ctrl Pts',(-9.26129529518433,12.2,6.48462379990615));
#248849=CARTESIAN_POINT('Ctrl Pts',(-9.25884307671734,12.2,6.48055927529426));
#248850=CARTESIAN_POINT('Ctrl Pts',(-9.25639098632924,12.2,6.47650924741871));
#248851=CARTESIAN_POINT('Ctrl Pts',(-9.25393912124005,12.2,6.47247375551385));
#248852=CARTESIAN_POINT('Ctrl Pts',(-9.25210022259019,12.2,6.46944713686012));
#248853=CARTESIAN_POINT('Ctrl Pts',(-9.25026145087661,12.2,6.46642869339033));
#248854=CARTESIAN_POINT('Ctrl Pts',(-9.24842284722673,12.2,6.463418441236));
#248855=CARTESIAN_POINT('Ctrl Pts',(-9.24658424357685,12.2,6.46040818908167));
#248856=CARTESIAN_POINT('Ctrl Pts',(-9.24474580820033,12.2,6.45740612750167));
#248857=CARTESIAN_POINT('Ctrl Pts',(-9.24290758443376,12.2,6.45441227285973));
#248858=CARTESIAN_POINT('Ctrl Pts',(-9.24106936066718,12.2,6.45141841821777));
#248859=CARTESIAN_POINT('Ctrl Pts',(-9.23923134628396,12.2,6.44843276964197));
#248860=CARTESIAN_POINT('Ctrl Pts',(-9.23739358464235,12.2,6.44545534212401));
#248861=CARTESIAN_POINT('Ctrl Pts',(-9.23555582266689,12.2,6.44247791406516));
#248862=CARTESIAN_POINT('Ctrl Pts',(-9.23371831353318,12.2,6.43950870846698));
#248863=CARTESIAN_POINT('Ctrl Pts',(-9.23188109905788,12.2,6.43654773932945));
#248864=CARTESIAN_POINT('Ctrl Pts',(-9.23004388491633,12.2,6.43358677072982));
#248865=CARTESIAN_POINT('Ctrl Pts',(-9.22820696566972,12.2,6.4306340386695));
#248866=CARTESIAN_POINT('Ctrl Pts',(-9.22637038389473,12.2,6.42768955892199));
#248867=CARTESIAN_POINT('Ctrl Pts',(-9.22453380211974,12.2,6.42474507917449));
#248868=CARTESIAN_POINT('Ctrl Pts',(-9.22269755719989,12.2,6.42180885225716));
#248869=CARTESIAN_POINT('Ctrl Pts',(-9.22086169351662,12.2,6.41888089165592));
#248870=CARTESIAN_POINT('Ctrl Pts',(-9.21902582983335,12.2,6.41595293105468));
#248871=CARTESIAN_POINT('Ctrl Pts',(-9.21719034693338,12.2,6.41303323766081));
#248872=CARTESIAN_POINT('Ctrl Pts',(-9.21535528729172,12.2,6.41012182705826));
#248873=CARTESIAN_POINT('Ctrl Pts',(-9.21352022765006,12.2,6.4072104164557));
#248874=CARTESIAN_POINT('Ctrl Pts',(-9.21168559163339,12.2,6.40430728882782));
#248875=CARTESIAN_POINT('Ctrl Pts',(-9.20985142294998,12.2,6.40141245830727));
#248876=CARTESIAN_POINT('Ctrl Pts',(-9.20801725426658,12.2,6.39851762778672));
#248877=CARTESIAN_POINT('Ctrl Pts',(-9.20618355169643,12.2,6.39563109548038));
#248878=CARTESIAN_POINT('Ctrl Pts',(-9.20435036137973,12.2,6.39275287527354));
#248879=CARTESIAN_POINT('Ctrl Pts',(-9.20251717106304,12.2,6.3898746550667));
#248880=CARTESIAN_POINT('Ctrl Pts',(-9.20068449099963,12.2,6.38700474830425));
#248881=CARTESIAN_POINT('Ctrl Pts',(-9.19885236589946,12.2,6.38414316961542));
#248882=CARTESIAN_POINT('Ctrl Pts',(-9.19702024046645,12.2,6.38128159040674));
#248883=CARTESIAN_POINT('Ctrl Pts',(-9.19518867038359,12.2,6.37842833809208));
#248884=CARTESIAN_POINT('Ctrl Pts',(-9.19335770036757,12.2,6.37558342988809));
#248885=CARTESIAN_POINT('Ctrl Pts',(-9.19091640756726,12.2,6.37179021981081));
#248886=CARTESIAN_POINT('Ctrl Pts',(-9.18847617881958,12.2,6.36801184220659));
#248887=CARTESIAN_POINT('Ctrl Pts',(-9.18603712274112,12.2,6.36424833229107));
#248888=CARTESIAN_POINT('Ctrl Pts',(-9.18420783059919,12.2,6.36142569972623));
#248889=CARTESIAN_POINT('Ctrl Pts',(-9.18237919726203,12.2,6.35861143098206));
#248890=CARTESIAN_POINT('Ctrl Pts',(-9.18055126761205,12.2,6.35580553981788));
#248891=CARTESIAN_POINT('Ctrl Pts',(-9.17872333796207,12.2,6.35299964865369));
#248892=CARTESIAN_POINT('Ctrl Pts',(-9.17689611279862,12.2,6.35020213707442));
#248893=CARTESIAN_POINT('Ctrl Pts',(-9.17506963715655,12.2,6.34741301759129));
#248894=CARTESIAN_POINT('Ctrl Pts',(-9.17263433607925,12.2,6.34369419127598));
#248895=CARTESIAN_POINT('Ctrl Pts',(-9.17020036558262,12.2,6.33999028752041));
#248896=CARTESIAN_POINT('Ctrl Pts',(-9.16776783778339,12.2,6.3363013410416));
#248897=CARTESIAN_POINT('Ctrl Pts',(-9.16533530998416,12.2,6.33261239456279));
#248898=CARTESIAN_POINT('Ctrl Pts',(-9.16290422149898,12.2,6.32893840566626));
#248899=CARTESIAN_POINT('Ctrl Pts',(-9.16047468331115,12.2,6.32527940913502));
#248900=CARTESIAN_POINT('Ctrl Pts',(-9.15804514545435,12.2,6.32162041310232));
#248901=CARTESIAN_POINT('Ctrl Pts',(-9.15561715778105,12.2,6.31797640999172));
#248902=CARTESIAN_POINT('Ctrl Pts',(-9.15319083096837,12.2,6.31434743599407));
#248903=CARTESIAN_POINT('Ctrl Pts',(-9.1507645038251,12.2,6.31071846150197));
#248904=CARTESIAN_POINT('Ctrl Pts',(-9.14833983662467,12.2,6.30710451497278));
#248905=CARTESIAN_POINT('Ctrl Pts',(-9.14591694160391,12.2,6.30350563244485));
#248906=CARTESIAN_POINT('Ctrl Pts',(-9.14349404691327,12.2,6.29990675040727));
#248907=CARTESIAN_POINT('Ctrl Pts',(-9.14107292279186,12.2,6.29632293317329));
#248908=CARTESIAN_POINT('Ctrl Pts',(-9.13865368348951,12.2,6.29275421457515));
#248909=CARTESIAN_POINT('Ctrl Pts',(-9.13623444385753,12.2,6.28918549549077));
#248910=CARTESIAN_POINT('Ctrl Pts',(-9.13381708881282,12.2,6.28563187595487));
#248911=CARTESIAN_POINT('Ctrl Pts',(-9.13140173044958,12.2,6.28209339125322));
#248912=CARTESIAN_POINT('Ctrl Pts',(-9.12898637241543,12.2,6.2785549070337));
#248913=CARTESIAN_POINT('Ctrl Pts',(-9.12657301199467,12.2,6.27503155752053));
#248914=CARTESIAN_POINT('Ctrl Pts',(-9.12416176341385,12.2,6.27152337752852));
#248915=CARTESIAN_POINT('Ctrl Pts',(-9.12175051450449,12.2,6.26801519705854));
#248916=CARTESIAN_POINT('Ctrl Pts',(-9.11934137829824,12.2,6.26452218700155));
#248917=CARTESIAN_POINT('Ctrl Pts',(-9.1169344687783,12.2,6.26104438242409));
#248918=CARTESIAN_POINT('Ctrl Pts',(-9.11452755958629,12.2,6.25756657832047));
#248919=CARTESIAN_POINT('Ctrl Pts',(-9.11212287863636,12.2,6.25410397852805));
#248920=CARTESIAN_POINT('Ctrl Pts',(-9.10972054132365,12.2,6.25065661969191));
#248921=CARTESIAN_POINT('Ctrl Pts',(-9.10731820368362,12.2,6.24720926038604));
#248922=CARTESIAN_POINT('Ctrl Pts',(-9.10491821142067,12.2,6.24377714246149));
#248923=CARTESIAN_POINT('Ctrl Pts',(-9.10252067934574,12.2,6.24036029872075));
#248924=CARTESIAN_POINT('Ctrl Pts',(-9.10012314759748,12.2,6.23694345544554));
#248925=CARTESIAN_POINT('Ctrl Pts',(-9.09772807875701,12.2,6.23354188810056));
#248926=CARTESIAN_POINT('Ctrl Pts',(-9.09533559017455,12.2,6.23015563082025));
#248927=CARTESIAN_POINT('Ctrl Pts',(-9.09294310126612,12.2,6.22676937307857));
#248928=CARTESIAN_POINT('Ctrl Pts',(-9.0905531924477,12.2,6.22339842654849));
#248929=CARTESIAN_POINT('Ctrl Pts',(-9.08816598547342,12.2,6.22004282473931));
#248930=CARTESIAN_POINT('Ctrl Pts',(-9.0851819769182,12.2,6.21584832270643));
#248931=CARTESIAN_POINT('Ctrl Pts',(-9.0822021876497,12.2,6.21167779784431));
#248932=CARTESIAN_POINT('Ctrl Pts',(-9.07922685508048,12.2,6.20753131826222));
#248933=CARTESIAN_POINT('Ctrl Pts',(-9.07684658921969,12.2,6.20421413486774));
#248934=CARTESIAN_POINT('Ctrl Pts',(-9.07446917684448,12.2,6.20091234115352));
#248935=CARTESIAN_POINT('Ctrl Pts',(-9.0720947383716,12.2,6.19762597108725));
#248936=CARTESIAN_POINT('Ctrl Pts',(-9.0697202995752,12.2,6.1943396005732));
#248937=CARTESIAN_POINT('Ctrl Pts',(-9.06734883574021,12.2,6.19106865276066));
#248938=CARTESIAN_POINT('Ctrl Pts',(-9.06498047150005,12.2,6.18781316424993));
#248939=CARTESIAN_POINT('Ctrl Pts',(-9.06261210725988,12.2,6.1845576757392));
#248940=CARTESIAN_POINT('Ctrl Pts',(-9.06024684060615,12.2,6.181317646083));
#248941=CARTESIAN_POINT('Ctrl Pts',(-9.05788479908885,12.2,6.17809310896439));
#248942=CARTESIAN_POINT('Ctrl Pts',(-9.05493224767497,12.2,6.17406243822514));
#248943=CARTESIAN_POINT('Ctrl Pts',(-9.05198473405351,12.2,6.17005597587762));
#248944=CARTESIAN_POINT('Ctrl Pts',(-9.04904250360988,12.2,6.16607378846246));
#248945=CARTESIAN_POINT('Ctrl Pts',(-9.04668871887013,12.2,6.16288803800946));
#248946=CARTESIAN_POINT('Ctrl Pts',(-9.04433831785295,12.2,6.15971782447184));
#248947=CARTESIAN_POINT('Ctrl Pts',(-9.04199142522504,12.2,6.15656318196659));
#248948=CARTESIAN_POINT('Ctrl Pts',(-9.03964453259714,12.2,6.15340853946133));
#248949=CARTESIAN_POINT('Ctrl Pts',(-9.03730114994188,12.2,6.15026946682734));
#248950=CARTESIAN_POINT('Ctrl Pts',(-9.03496140709249,12.2,6.14714599971424));
#248951=CARTESIAN_POINT('Ctrl Pts',(-9.0326216645619,12.2,6.14402253302672));
#248952=CARTESIAN_POINT('Ctrl Pts',(-9.03028556015212,12.2,6.14091467168001));
#248953=CARTESIAN_POINT('Ctrl Pts',(-9.02795322627664,12.2,6.13782245025204));
#248954=CARTESIAN_POINT('Ctrl Pts',(-9.02562089208336,12.2,6.13473022840276));
#248955=CARTESIAN_POINT('Ctrl Pts',(-9.02329232849071,12.2,6.1316536462647));
#248956=CARTESIAN_POINT('Ctrl Pts',(-9.02096766458663,12.2,6.12859273776614));
#248957=CARTESIAN_POINT('Ctrl Pts',(-9.01864300099929,12.2,6.12553182968462));
#248958=CARTESIAN_POINT('Ctrl Pts',(-9.01632224013369,12.2,6.12248659430111));
#248959=CARTESIAN_POINT('Ctrl Pts',(-9.01400551365613,12.2,6.1194570682144));
#248960=CARTESIAN_POINT('Ctrl Pts',(-9.01168878686293,12.2,6.11642754171491));
#248961=CARTESIAN_POINT('Ctrl Pts',(-9.00937609449197,12.2,6.11341372374899));
#248962=CARTESIAN_POINT('Ctrl Pts',(-9.00706757164009,12.2,6.11041564654831));
#248963=CARTESIAN_POINT('Ctrl Pts',(-9.00475904910274,12.2,6.10741756975611));
#248964=CARTESIAN_POINT('Ctrl Pts',(-9.00245469528924,12.2,6.10443523633443));
#248965=CARTESIAN_POINT('Ctrl Pts',(-9.00015464692144,12.2,6.10146867824259));
#248966=CARTESIAN_POINT('Ctrl Pts',(-8.99785459824026,12.2,6.09850211974656));
#248967=CARTESIAN_POINT('Ctrl Pts',(-8.99555885494013,12.2,6.0955513383274));
#248968=CARTESIAN_POINT('Ctrl Pts',(-8.99326755487111,12.2,6.09261636600182));
#248969=CARTESIAN_POINT('Ctrl Pts',(-8.99097625511427,12.2,6.08968139407612));
#248970=CARTESIAN_POINT('Ctrl Pts',(-8.98868939709794,12.2,6.08676223271368));
#248971=CARTESIAN_POINT('Ctrl Pts',(-8.98640712061457,12.2,6.08385891513796));
#248972=CARTESIAN_POINT('Ctrl Pts',(-8.98412484382023,12.2,6.08095559716666));
#248973=CARTESIAN_POINT('Ctrl Pts',(-8.9818471490156,12.2,6.07806812315132));
#248974=CARTESIAN_POINT('Ctrl Pts',(-8.97957417578094,12.2,6.07519652727366));
#248975=CARTESIAN_POINT('Ctrl Pts',(-8.97730120285597,12.2,6.07232493178725));
#248976=CARTESIAN_POINT('Ctrl Pts',(-8.97503295389946,12.2,6.06946921408372));
#248977=CARTESIAN_POINT('Ctrl Pts',(-8.97276956636176,12.2,6.0666294079809));
#248978=CARTESIAN_POINT('Ctrl Pts',(-8.97050617851567,12.2,6.06378960149115));
#248979=CARTESIAN_POINT('Ctrl Pts',(-8.96824765550376,12.2,6.06096570559707));
#248980=CARTESIAN_POINT('Ctrl Pts',(-8.96599413948184,12.2,6.05815775576469));
#248981=CARTESIAN_POINT('Ctrl Pts',(-8.96374062376698,12.2,6.0553498063149));
#248982=CARTESIAN_POINT('Ctrl Pts',(-8.96149211395618,12.2,6.05255780151461));
#248983=CARTESIAN_POINT('Ctrl Pts',(-8.95924875758349,12.2,6.04978177546214));
#248984=CARTESIAN_POINT('Ctrl Pts',(-8.95700540090515,12.2,6.04700574903145));
#248985=CARTESIAN_POINT('Ctrl Pts',(-8.95476719569672,12.2,6.04424570199668));
#248986=CARTESIAN_POINT('Ctrl Pts',(-8.9525342897417,12.2,6.04150166745825));
#248987=CARTESIAN_POINT('Ctrl Pts',(-8.95030138378669,12.2,6.03875763291983));
#248988=CARTESIAN_POINT('Ctrl Pts',(-8.94807377588782,12.2,6.03602960973602));
#248989=CARTESIAN_POINT('Ctrl Pts',(-8.94585161537839,12.2,6.03331763258986));
#248990=CARTESIAN_POINT('Ctrl Pts',(-8.94307391519575,12.2,6.02992766171141));
#248991=CARTESIAN_POINT('Ctrl Pts',(-8.9403047264054,12.2,6.02656276143039));
#248992=CARTESIAN_POINT('Ctrl Pts',(-8.93754434038609,12.2,6.02322299811177));
#248993=CARTESIAN_POINT('Ctrl Pts',(-8.93533603120957,12.2,6.02055118702003));
#248994=CARTESIAN_POINT('Ctrl Pts',(-8.93313335678365,12.2,6.01789546262155));
#248995=CARTESIAN_POINT('Ctrl Pts',(-8.9309364689417,12.2,6.01525586003325));
#248996=CARTESIAN_POINT('Ctrl Pts',(-8.92873958109975,12.2,6.01261625744496));
#248997=CARTESIAN_POINT('Ctrl Pts',(-8.92654847980845,12.2,6.00999277398628));
#248998=CARTESIAN_POINT('Ctrl Pts',(-8.92436331863442,12.2,6.00738544429029));
#248999=CARTESIAN_POINT('Ctrl Pts',(-8.92217815775812,12.2,6.00477811494955));
#249000=CARTESIAN_POINT('Ctrl Pts',(-8.91999893644484,12.2,6.00218694030291));
#249001=CARTESIAN_POINT('Ctrl Pts',(-8.91782581150152,12.2,5.99961195150169));
#249002=CARTESIAN_POINT('Ctrl Pts',(-8.9156526862621,12.2,5.99703696234962));
#249003=CARTESIAN_POINT('Ctrl Pts',(-8.91348565639443,12.2,5.99447816055447));
#249004=CARTESIAN_POINT('Ctrl Pts',(-8.91132487988841,12.2,5.99193557808421));
#249005=CARTESIAN_POINT('Ctrl Pts',(-8.90862390940309,12.2,5.9887573501696));
#249006=CARTESIAN_POINT('Ctrl Pts',(-8.90593270821518,12.2,5.98560446438877));
#249007=CARTESIAN_POINT('Ctrl Pts',(-8.90325158863268,12.2,5.98247698730753));
#249008=CARTESIAN_POINT('Ctrl Pts',(-8.90057046934242,12.2,5.97934951056718));
#249009=CARTESIAN_POINT('Ctrl Pts',(-8.89789943029222,12.2,5.97624744106908));
#249010=CARTESIAN_POINT('Ctrl Pts',(-8.89523878933137,12.2,5.97317084265234));
#249011=CARTESIAN_POINT('Ctrl Pts',(-8.89257814808052,12.2,5.97009424390025));
#249012=CARTESIAN_POINT('Ctrl Pts',(-8.88992790359616,12.2,5.96704311671443));
#249013=CARTESIAN_POINT('Ctrl Pts',(-8.88728837734528,12.2,5.96401752462901));
#249014=CARTESIAN_POINT('Ctrl Pts',(-8.88464885109441,12.2,5.96099193254359));
#249015=CARTESIAN_POINT('Ctrl Pts',(-8.88202004188223,12.2,5.95799187677997));
#249016=CARTESIAN_POINT('Ctrl Pts',(-8.87940227507577,12.2,5.95501741893065));
#249017=CARTESIAN_POINT('Ctrl Pts',(-8.8752138482425,12.2,5.95025828643659));
#249018=CARTESIAN_POINT('Ctrl Pts',(-8.87105369166071,12.2,5.94556468565188));
#249019=CARTESIAN_POINT('Ctrl Pts',(-8.86692316060437,12.2,5.94093687837826));
#249020=CARTESIAN_POINT('Ctrl Pts',(-8.864341578659,12.2,5.93804449879283));
#249021=CARTESIAN_POINT('Ctrl Pts',(-8.86177157093003,12.2,5.93517782014584));
#249022=CARTESIAN_POINT('Ctrl Pts',(-8.85921347565129,12.2,5.93233690312985));
#249023=CARTESIAN_POINT('Ctrl Pts',(-8.85665538037255,12.2,5.92949598611385));
#249024=CARTESIAN_POINT('Ctrl Pts',(-8.85410919657167,12.2,5.92668083383164));
#249025=CARTESIAN_POINT('Ctrl Pts',(-8.85157526956922,12.2,5.92389150660714));
#249026=CARTESIAN_POINT('Ctrl Pts',(-8.84904134256677,12.2,5.92110217938266));
#249027=CARTESIAN_POINT('Ctrl Pts',(-8.84651967100374,12.2,5.91833867758046));
#249028=CARTESIAN_POINT('Ctrl Pts',(-8.84401060586419,12.2,5.91560106466244));
#249029=CARTESIAN_POINT('Ctrl Pts',(-8.84150154072464,12.2,5.91286345174443));
#249030=CARTESIAN_POINT('Ctrl Pts',(-8.83900507998542,12.2,5.91015172863265));
#249031=CARTESIAN_POINT('Ctrl Pts',(-8.83652158067919,12.2,5.90746595495072));
#249032=CARTESIAN_POINT('Ctrl Pts',(-8.83403808137295,12.2,5.90478018126881));
#249033=CARTESIAN_POINT('Ctrl Pts',(-8.83156754173479,12.2,5.90212035865229));
#249034=CARTESIAN_POINT('Ctrl Pts',(-8.82911032325137,12.2,5.89948654975137));
#249035=CARTESIAN_POINT('Ctrl Pts',(-8.82665310476795,12.2,5.89685274085044));
#249036=CARTESIAN_POINT('Ctrl Pts',(-8.82420920823334,12.2,5.8942449446888));
#249037=CARTESIAN_POINT('Ctrl Pts',(-8.82177899823336,12.2,5.89166322350825));
#249038=CARTESIAN_POINT('Ctrl Pts',(-8.81934878823337,12.2,5.88908150232771));
#249039=CARTESIAN_POINT('Ctrl Pts',(-8.81693226548736,12.2,5.88652585648773));
#249040=CARTESIAN_POINT('Ctrl Pts',(-8.81452980374038,12.2,5.88399634703187));
#249041=CARTESIAN_POINT('Ctrl Pts',(-8.81212734199339,12.2,5.88146683757603));
#249042=CARTESIAN_POINT('Ctrl Pts',(-8.80973894037744,12.2,5.87896346501449));
#249043=CARTESIAN_POINT('Ctrl Pts',(-8.80736497787818,12.2,5.8764862918214));
#249044=CARTESIAN_POINT('Ctrl Pts',(-8.80499101537891,12.2,5.87400911862832));
#249045=CARTESIAN_POINT('Ctrl Pts',(-8.80263149237376,12.2,5.87155814197902));
#249046=CARTESIAN_POINT('Ctrl Pts',(-8.80028679334676,12.2,5.86913342579982));
#249047=CARTESIAN_POINT('Ctrl Pts',(-8.79794209431974,12.2,5.86670870962063));
#249048=CARTESIAN_POINT('Ctrl Pts',(-8.79561222028486,12.2,5.86431025398577));
#249049=CARTESIAN_POINT('Ctrl Pts',(-8.79329756273971,12.2,5.86193811775798));
#249050=CARTESIAN_POINT('Ctrl Pts',(-8.79005704237834,12.2,5.85861712724592));
#249051=CARTESIAN_POINT('Ctrl Pts',(-8.78684634516754,12.2,5.85534772751428));
#249052=CARTESIAN_POINT('Ctrl Pts',(-8.78366657203044,12.2,5.85213008155888));
#249053=CARTESIAN_POINT('Ctrl Pts',(-8.78094105188033,12.2,5.84937209898929));
#249054=CARTESIAN_POINT('Ctrl Pts',(-8.77823824856104,12.2,5.84665214112681));
#249055=CARTESIAN_POINT('Ctrl Pts',(-8.77555887253255,12.2,5.84397031326558));
#249056=CARTESIAN_POINT('Ctrl Pts',(-8.77287949674744,12.2,5.84128848564795));
#249057=CARTESIAN_POINT('Ctrl Pts',(-8.77022354674606,12.2,5.83864478449692));
#249058=CARTESIAN_POINT('Ctrl Pts',(-8.76759174725834,12.2,5.83603931900825));
#249059=CARTESIAN_POINT('Ctrl Pts',(-8.76495994777063,12.2,5.83343385351958));
#249060=CARTESIAN_POINT('Ctrl Pts',(-8.7623522980699,12.2,5.83086662035635));
#249061=CARTESIAN_POINT('Ctrl Pts',(-8.75976953569992,12.2,5.82833772473631));
#249062=CARTESIAN_POINT('Ctrl Pts',(-8.75718677309533,12.2,5.82580882888658));
#249063=CARTESIAN_POINT('Ctrl Pts',(-8.75462890078526,12.2,5.82331826911366));
#249064=CARTESIAN_POINT('Ctrl Pts',(-8.75209667223233,12.2,5.82086615048264));
#249065=CARTESIAN_POINT('Ctrl Pts',(-8.74956444390942,12.2,5.81841403207436));
#249066=CARTESIAN_POINT('Ctrl Pts',(-8.74705786000329,12.2,5.81600035433157));
#249067=CARTESIAN_POINT('Ctrl Pts',(-8.74457769274889,12.2,5.81362521899051));
#249068=CARTESIAN_POINT('Ctrl Pts',(-8.74209752549448,12.2,5.81125008364944));
#249069=CARTESIAN_POINT('Ctrl Pts',(-8.7396437742037,12.2,5.8089134913435));
#249070=CARTESIAN_POINT('Ctrl Pts',(-8.73721723287403,12.2,5.80661554492531));
#249071=CARTESIAN_POINT('Ctrl Pts',(-8.73479069132394,12.2,5.80431759829841));
#249072=CARTESIAN_POINT('Ctrl Pts',(-8.73239135639386,12.2,5.80205829695126));
#249073=CARTESIAN_POINT('Ctrl Pts',(-8.73002003901654,12.2,5.79983774324955));
#249074=CARTESIAN_POINT('Ctrl Pts',(-8.72764872185461,12.2,5.79761718974955));
#249075=CARTESIAN_POINT('Ctrl Pts',(-8.72530542130863,12.2,5.79543538394739));
#249076=CARTESIAN_POINT('Ctrl Pts',(-8.72299096821562,12.2,5.79329242651561));
#249077=CARTESIAN_POINT('Ctrl Pts',(-8.72067651512262,12.2,5.79114946908385));
#249078=CARTESIAN_POINT('Ctrl Pts',(-8.71839090675908,12.2,5.7890453622143));
#249079=CARTESIAN_POINT('Ctrl Pts',(-8.71613499383974,12.2,5.78698020387097));
#249080=CARTESIAN_POINT('Ctrl Pts',(-8.71387908071548,12.2,5.78491504534004));
#249081=CARTESIAN_POINT('Ctrl Pts',(-8.71165286344493,12.2,5.7828888376223));
#249082=CARTESIAN_POINT('Ctrl Pts',(-8.70945721049402,12.2,5.78090168101666));
#249083=CARTESIAN_POINT('Ctrl Pts',(-8.70726155774254,12.2,5.77891452459151));
#249084=CARTESIAN_POINT('Ctrl Pts',(-8.7050964699133,12.2,5.77696641859167));
#249085=CARTESIAN_POINT('Ctrl Pts',(-8.70296283907551,12.2,5.7750574641627));
#249086=CARTESIAN_POINT('Ctrl Pts',(-8.70082920823772,12.2,5.77314850973373));
#249087=CARTESIAN_POINT('Ctrl Pts',(-8.69872703439749,12.2,5.77127870801839));
#249088=CARTESIAN_POINT('Ctrl Pts',(-8.69665723188794,12.2,5.76944815658318));
#249089=CARTESIAN_POINT('Ctrl Pts',(-8.6945874293784,12.2,5.76761760514797));
#249090=CARTESIAN_POINT('Ctrl Pts',(-8.69255000036457,12.2,5.76582630417156));
#249091=CARTESIAN_POINT('Ctrl Pts',(-8.69054588076846,12.2,5.76407435548256));
#249092=CARTESIAN_POINT('Ctrl Pts',(-8.6885417609903,12.2,5.76232240663441));
#249093=CARTESIAN_POINT('Ctrl Pts',(-8.68657095229864,12.2,5.76060980817335));
#249094=CARTESIAN_POINT('Ctrl Pts',(-8.6846344176946,12.2,5.75893665966723));
#249095=CARTESIAN_POINT('Ctrl Pts',(-8.68269788326646,12.2,5.75726351131309));
#249096=CARTESIAN_POINT('Ctrl Pts',(-8.68079562368323,12.2,5.75562981352503));
#249097=CARTESIAN_POINT('Ctrl Pts',(-8.67892862849251,12.2,5.75403566599231));
#249098=CARTESIAN_POINT('Ctrl Pts',(-8.6770616333018,12.2,5.75244151845958));
#249099=CARTESIAN_POINT('Ctrl Pts',(-8.67522990259125,12.2,5.75088691961269));
#249100=CARTESIAN_POINT('Ctrl Pts',(-8.67343445440404,12.2,5.74937196816505));
#249101=CARTESIAN_POINT('Ctrl Pts',(-8.67163900605374,12.2,5.74785701657981));
#249102=CARTESIAN_POINT('Ctrl Pts',(-8.66987983975288,12.2,5.74638171360046));
#249103=CARTESIAN_POINT('Ctrl Pts',(-8.66815800232518,12.2,5.74494615786947));
#249104=CARTESIAN_POINT('Ctrl Pts',(-8.66643616505387,12.2,5.74351060226887));
#249105=CARTESIAN_POINT('Ctrl Pts',(-8.66475165580683,12.2,5.74211479191732));
#249106=CARTESIAN_POINT('Ctrl Pts',(-8.66310555103332,12.2,5.74075882646657));
#249107=CARTESIAN_POINT('Ctrl Pts',(-8.66145944625979,12.2,5.73940286101584));
#249108=CARTESIAN_POINT('Ctrl Pts',(-8.65985174748376,12.2,5.73808674020149));
#249109=CARTESIAN_POINT('Ctrl Pts',(-8.65828355987679,12.2,5.73681056259847));
#249110=CARTESIAN_POINT('Ctrl Pts',(-8.65671537212737,12.2,5.73553438487952));
#249111=CARTESIAN_POINT('Ctrl Pts',(-8.65518669881612,12.2,5.73429814974866));
#249112=CARTESIAN_POINT('Ctrl Pts',(-8.65369867907114,12.2,5.73310195435287));
#249113=CARTESIAN_POINT('Ctrl Pts',(-8.6522178008694,12.2,5.73191149993006));
#249114=CARTESIAN_POINT('Ctrl Pts',(-8.65077718857068,12.2,5.73076070226254));
#249115=CARTESIAN_POINT('Ctrl Pts',(-8.64937799900006,12.2,5.72964966099998));
#249116=CARTESIAN_POINT('Ctrl Pts',(-8.64937799900006,15.2,5.72964966099998));
#249117=CARTESIAN_POINT('Ctrl Pts',(-8.65077718857068,15.2,5.73076070226254));
#249118=CARTESIAN_POINT('Ctrl Pts',(-8.65221780086937,15.2,5.73191149993004));
#249119=CARTESIAN_POINT('Ctrl Pts',(-8.65369867907113,15.2,5.73310195435287));
#249120=CARTESIAN_POINT('Ctrl Pts',(-8.65518669881613,15.2,5.73429814974867));
#249121=CARTESIAN_POINT('Ctrl Pts',(-8.65671537212734,15.2,5.7355343848795));
#249122=CARTESIAN_POINT('Ctrl Pts',(-8.65828355987679,15.2,5.73681056259847));
#249123=CARTESIAN_POINT('Ctrl Pts',(-8.65985174748379,15.2,5.73808674020152));
#249124=CARTESIAN_POINT('Ctrl Pts',(-8.6614594462598,15.2,5.73940286101585));
#249125=CARTESIAN_POINT('Ctrl Pts',(-8.66310555103331,15.2,5.74075882646657));
#249126=CARTESIAN_POINT('Ctrl Pts',(-8.66475165580682,15.2,5.74211479191731));
#249127=CARTESIAN_POINT('Ctrl Pts',(-8.66643616505388,15.2,5.74351060226888));
#249128=CARTESIAN_POINT('Ctrl Pts',(-8.66815800232518,15.2,5.74494615786947));
#249129=CARTESIAN_POINT('Ctrl Pts',(-8.66987983975287,15.2,5.74638171360045));
#249130=CARTESIAN_POINT('Ctrl Pts',(-8.6716390060537,15.2,5.74785701657977));
#249131=CARTESIAN_POINT('Ctrl Pts',(-8.67343445440403,15.2,5.74937196816505));
#249132=CARTESIAN_POINT('Ctrl Pts',(-8.67522990259129,15.2,5.75088691961273));
#249133=CARTESIAN_POINT('Ctrl Pts',(-8.67706163330177,15.2,5.75244151845955));
#249134=CARTESIAN_POINT('Ctrl Pts',(-8.67892862849251,15.2,5.75403566599231));
#249135=CARTESIAN_POINT('Ctrl Pts',(-8.68079562368326,15.2,5.75562981352506));
#249136=CARTESIAN_POINT('Ctrl Pts',(-8.68269788326646,15.2,5.75726351131309));
#249137=CARTESIAN_POINT('Ctrl Pts',(-8.6846344176946,15.2,5.75893665966723));
#249138=CARTESIAN_POINT('Ctrl Pts',(-8.68657095229864,15.2,5.76060980817335));
#249139=CARTESIAN_POINT('Ctrl Pts',(-8.68854176099027,15.2,5.76232240663438));
#249140=CARTESIAN_POINT('Ctrl Pts',(-8.69054588076846,15.2,5.76407435548256));
#249141=CARTESIAN_POINT('Ctrl Pts',(-8.69255000036461,15.2,5.7658263041716));
#249142=CARTESIAN_POINT('Ctrl Pts',(-8.69458742937841,15.2,5.76761760514798));
#249143=CARTESIAN_POINT('Ctrl Pts',(-8.69665723188794,15.2,5.76944815658318));
#249144=CARTESIAN_POINT('Ctrl Pts',(-8.69872703439747,15.2,5.77127870801838));
#249145=CARTESIAN_POINT('Ctrl Pts',(-8.70082920823772,15.2,5.77314850973373));
#249146=CARTESIAN_POINT('Ctrl Pts',(-8.70296283907552,15.2,5.77505746416271));
#249147=CARTESIAN_POINT('Ctrl Pts',(-8.70509646991331,15.2,5.77696641859168));
#249148=CARTESIAN_POINT('Ctrl Pts',(-8.70726155774256,15.2,5.77891452459153));
#249149=CARTESIAN_POINT('Ctrl Pts',(-8.70945721049402,15.2,5.78090168101666));
#249150=CARTESIAN_POINT('Ctrl Pts',(-8.71165286344492,15.2,5.78288883762229));
#249151=CARTESIAN_POINT('Ctrl Pts',(-8.71387908071551,15.2,5.78491504534007));
#249152=CARTESIAN_POINT('Ctrl Pts',(-8.71613499383974,15.2,5.78698020387097));
#249153=CARTESIAN_POINT('Ctrl Pts',(-8.7187668921773,15.2,5.78938955520896));
#249154=CARTESIAN_POINT('Ctrl Pts',(-8.72143920775675,15.2,5.79185192106912));
#249155=CARTESIAN_POINT('Ctrl Pts',(-8.72415059478003,15.2,5.79436714175661));
#249156=CARTESIAN_POINT('Ctrl Pts',(-8.72647464107139,15.2,5.79652304545479));
#249157=CARTESIAN_POINT('Ctrl Pts',(-8.72882739479893,15.2,5.79871778224841));
#249158=CARTESIAN_POINT('Ctrl Pts',(-8.73120802909653,15.2,5.8009512488718));
#249159=CARTESIAN_POINT('Ctrl Pts',(-8.7335886631779,15.2,5.80318471529232));
#249160=CARTESIAN_POINT('Ctrl Pts',(-8.73599717779872,15.2,5.80545691293479));
#249161=CARTESIAN_POINT('Ctrl Pts',(-8.73843276712572,15.2,5.80776773759914));
#249162=CARTESIAN_POINT('Ctrl Pts',(-8.74127428815468,15.2,5.81046369984749));
#249163=CARTESIAN_POINT('Ctrl Pts',(-8.74415266250621,15.2,5.81321224270758));
#249164=CARTESIAN_POINT('Ctrl Pts',(-8.74706663713624,15.2,5.81601319786425));
#249165=CARTESIAN_POINT('Ctrl Pts',(-8.74956432954663,15.2,5.81841401644537));
#249166=CARTESIAN_POINT('Ctrl Pts',(-8.75208817976324,15.2,5.82085334532339));
#249167=CARTESIAN_POINT('Ctrl Pts',(-8.75463742108618,15.2,5.82333107889837));
#249168=CARTESIAN_POINT('Ctrl Pts',(-8.75718666240915,15.2,5.82580881247335));
#249169=CARTESIAN_POINT('Ctrl Pts',(-8.75976129425447,15.2,5.82832495308358));
#249170=CARTESIAN_POINT('Ctrl Pts',(-8.76236056590836,15.2,5.83087939548815));
#249171=CARTESIAN_POINT('Ctrl Pts',(-8.76495983779834,15.2,5.83343383812474));
#249172=CARTESIAN_POINT('Ctrl Pts',(-8.7675837506574,15.2,5.8360265813234));
#249173=CARTESIAN_POINT('Ctrl Pts',(-8.77023157038609,15.2,5.83865752588513));
#249174=CARTESIAN_POINT('Ctrl Pts',(-8.77332069304212,15.2,5.84172696084867));
#249175=CARTESIAN_POINT('Ctrl Pts',(-8.77644235554255,15.2,5.84484838598747));
#249176=CARTESIAN_POINT('Ctrl Pts',(-8.77959541774711,15.2,5.84802163920346));
#249177=CARTESIAN_POINT('Ctrl Pts',(-8.78229804280949,15.2,5.8507415708491));
#249178=CARTESIAN_POINT('Ctrl Pts',(-8.78502373925748,15.2,5.85349957874843));
#249179=CARTESIAN_POINT('Ctrl Pts',(-8.78777180615821,15.2,5.85629555940246));
#249180=CARTESIAN_POINT('Ctrl Pts',(-8.79143589510955,15.2,5.86002353335384));
#249181=CARTESIAN_POINT('Ctrl Pts',(-8.79513975134169,15.2,5.86381901413341));
#249182=CARTESIAN_POINT('Ctrl Pts',(-8.79888175640306,15.2,5.8676817484163));
#249183=CARTESIAN_POINT('Ctrl Pts',(-8.8012205095983,15.2,5.87009595737601));
#249184=CARTESIAN_POINT('Ctrl Pts',(-8.80357416393203,15.2,5.87253643944894));
#249185=CARTESIAN_POINT('Ctrl Pts',(-8.80594233615498,15.2,5.87500313222806));
#249186=CARTESIAN_POINT('Ctrl Pts',(-8.80831050837794,15.2,5.87746982500719));
#249187=CARTESIAN_POINT('Ctrl Pts',(-8.81069319467424,15.2,5.87996272728698));
#249188=CARTESIAN_POINT('Ctrl Pts',(-8.81309001729498,15.2,5.88248177873411));
#249189=CARTESIAN_POINT('Ctrl Pts',(-8.81548683991571,15.2,5.88500083018124));
#249190=CARTESIAN_POINT('Ctrl Pts',(-8.81789779715491,15.2,5.88754603274521));
#249191=CARTESIAN_POINT('Ctrl Pts',(-8.82032251785052,15.2,5.89011732080292));
#249192=CARTESIAN_POINT('Ctrl Pts',(-8.82323218257952,15.2,5.89320286636009));
#249193=CARTESIAN_POINT('Ctrl Pts',(-8.82616166117839,15.2,5.89632597918507));
#249194=CARTESIAN_POINT('Ctrl Pts',(-8.82911032325136,15.2,5.89948654975136));
#249195=CARTESIAN_POINT('Ctrl Pts',(-8.83156754173478,15.2,5.90212035865228));
#249196=CARTESIAN_POINT('Ctrl Pts',(-8.83403808137296,15.2,5.90478018126882));
#249197=CARTESIAN_POINT('Ctrl Pts',(-8.83652158067919,15.2,5.90746595495072));
#249198=CARTESIAN_POINT('Ctrl Pts',(-8.83900507998541,15.2,5.91015172863263));
#249199=CARTESIAN_POINT('Ctrl Pts',(-8.84150154072465,15.2,5.91286345174443));
#249200=CARTESIAN_POINT('Ctrl Pts',(-8.8440106058642,15.2,5.91560106466246));
#249201=CARTESIAN_POINT('Ctrl Pts',(-8.84702148392227,15.2,5.91888620004472));
#249202=CARTESIAN_POINT('Ctrl Pts',(-8.85005051432056,15.2,5.92220861549699));
#249203=CARTESIAN_POINT('Ctrl Pts',(-8.85309709347364,15.2,5.9255682009734));
#249204=CARTESIAN_POINT('Ctrl Pts',(-8.85563590952679,15.2,5.92836785563879));
#249205=CARTESIAN_POINT('Ctrl Pts',(-8.85818691230002,15.2,5.93119332447771));
#249206=CARTESIAN_POINT('Ctrl Pts',(-8.86074975917502,15.2,5.93404454399158));
#249207=CARTESIAN_POINT('Ctrl Pts',(-8.86485031411913,15.2,5.93860649515163));
#249208=CARTESIAN_POINT('Ctrl Pts',(-8.86898118831148,15.2,5.94323436703555));
#249209=CARTESIAN_POINT('Ctrl Pts',(-8.87314100727362,15.2,5.947927901215));
#249210=CARTESIAN_POINT('Ctrl Pts',(-8.87574089416037,15.2,5.95086136011712));
#249211=CARTESIAN_POINT('Ctrl Pts',(-8.87835208694446,15.2,5.95382047034435));
#249212=CARTESIAN_POINT('Ctrl Pts',(-8.88097425729169,15.2,5.95680516423325));
#249213=CARTESIAN_POINT('Ctrl Pts',(-8.88412086159406,15.2,5.9603867967698));
#249214=CARTESIAN_POINT('Ctrl Pts',(-8.88728327284515,15.2,5.9640052756618));
#249215=CARTESIAN_POINT('Ctrl Pts',(-8.89046093214533,15.2,5.96766048710984));
#249216=CARTESIAN_POINT('Ctrl Pts',(-8.89310898165836,15.2,5.97070649676054));
#249217=CARTESIAN_POINT('Ctrl Pts',(-8.8957676200576,15.2,5.97377801682086));
#249218=CARTESIAN_POINT('Ctrl Pts',(-8.89843652894025,15.2,5.9768749823905));
#249219=CARTESIAN_POINT('Ctrl Pts',(-8.9011054378229,15.2,5.97997194796015));
#249220=CARTESIAN_POINT('Ctrl Pts',(-8.90378461666361,15.2,5.98309435880108));
#249221=CARTESIAN_POINT('Ctrl Pts',(-8.90647375131589,15.2,5.98624215178588));
#249222=CARTESIAN_POINT('Ctrl Pts',(-8.90916288596816,15.2,5.98938994477068));
#249223=CARTESIAN_POINT('Ctrl Pts',(-8.9118619768901,15.2,5.9925631199422));
#249224=CARTESIAN_POINT('Ctrl Pts',(-8.91457071480627,15.2,5.99576161202423));
#249225=CARTESIAN_POINT('Ctrl Pts',(-8.91782120018757,15.2,5.9995998023832));
#249226=CARTESIAN_POINT('Ctrl Pts',(-8.92108557717114,15.2,6.00347445010159));
#249227=CARTESIAN_POINT('Ctrl Pts',(-8.92436331863443,15.2,6.00738544429029));
#249228=CARTESIAN_POINT('Ctrl Pts',(-8.92709476995307,15.2,6.01064460623263));
#249229=CARTESIAN_POINT('Ctrl Pts',(-8.92983550260778,15.2,6.01392900720799));
#249230=CARTESIAN_POINT('Ctrl Pts',(-8.93258521719037,15.2,6.01723858352537));
#249231=CARTESIAN_POINT('Ctrl Pts',(-8.93533493177299,15.2,6.02054815984277));
#249232=CARTESIAN_POINT('Ctrl Pts',(-8.93809362763003,15.2,6.02388291246607));
#249233=CARTESIAN_POINT('Ctrl Pts',(-8.94086100992048,15.2,6.02724277478498));
#249234=CARTESIAN_POINT('Ctrl Pts',(-8.9430749158735,15.2,6.0299306647866));
#249235=CARTESIAN_POINT('Ctrl Pts',(-8.94529438058538,15.2,6.03263462607594));
#249236=CARTESIAN_POINT('Ctrl Pts',(-8.94751925520697,15.2,6.03535462394743));
#249237=CARTESIAN_POINT('Ctrl Pts',(-8.94974412952543,15.2,6.03807462144833));
#249238=CARTESIAN_POINT('Ctrl Pts',(-8.95197441419562,15.2,6.04081065615439));
#249239=CARTESIAN_POINT('Ctrl Pts',(-8.95420995990119,15.2,6.04356269481663));
#249240=CARTESIAN_POINT('Ctrl Pts',(-8.95644550591134,15.2,6.04631473385383));
#249241=CARTESIAN_POINT('Ctrl Pts',(-8.95868631456062,15.2,6.04908277646797));
#249242=CARTESIAN_POINT('Ctrl Pts',(-8.96093223852656,15.2,6.05186679024349));
#249243=CARTESIAN_POINT('Ctrl Pts',(-8.9631781621865,15.2,6.05465080363969));
#249244=CARTESIAN_POINT('Ctrl Pts',(-8.96542920232445,15.2,6.05745078667136));
#249245=CARTESIAN_POINT('Ctrl Pts',(-8.96768521263951,15.2,6.06026670677285));
#249246=CARTESIAN_POINT('Ctrl Pts',(-8.96994122326194,15.2,6.06308262725801));
#249247=CARTESIAN_POINT('Ctrl Pts',(-8.97220220627099,15.2,6.06591448511415));
#249248=CARTESIAN_POINT('Ctrl Pts',(-8.97446801628337,15.2,6.06876224499158));
#249249=CARTESIAN_POINT('Ctrl Pts',(-8.97730027864447,15.2,6.07232194464437));
#249250=CARTESIAN_POINT('Ctrl Pts',(-8.98014008505528,15.2,6.07590649380763));
#249251=CARTESIAN_POINT('Ctrl Pts',(-8.98298715923492,15.2,6.07951582576856));
#249252=CARTESIAN_POINT('Ctrl Pts',(-8.98526481839244,15.2,6.08240329110125));
#249253=CARTESIAN_POINT('Ctrl Pts',(-8.98754713037465,15.2,6.08530661723234));
#249254=CARTESIAN_POINT('Ctrl Pts',(-8.98983395340948,15.2,6.08822577004764));
#249255=CARTESIAN_POINT('Ctrl Pts',(-8.99269248243668,15.2,6.09187471136507));
#249256=CARTESIAN_POINT('Ctrl Pts',(-8.99555806028602,15.2,6.09554838200711));
#249257=CARTESIAN_POINT('Ctrl Pts',(-8.99843041938266,15.2,6.09924671728285));
#249258=CARTESIAN_POINT('Ctrl Pts',(-9.0013027784793,15.2,6.10294505255858));
#249259=CARTESIAN_POINT('Ctrl Pts',(-9.00418191823247,15.2,6.10666805025166));
#249260=CARTESIAN_POINT('Ctrl Pts',(-9.00706757164008,15.2,6.1104156465483));
#249261=CARTESIAN_POINT('Ctrl Pts',(-9.0099532250477,15.2,6.11416324284494));
#249262=CARTESIAN_POINT('Ctrl Pts',(-9.0128453929664,15.2,6.1179354339086));
#249263=CARTESIAN_POINT('Ctrl Pts',(-9.01574381282718,15.2,6.12173215751843));
#249264=CARTESIAN_POINT('Ctrl Pts',(-9.01806254884218,15.2,6.12476953657183));
#249265=CARTESIAN_POINT('Ctrl Pts',(-9.02038528679656,15.2,6.12782261481601));
#249266=CARTESIAN_POINT('Ctrl Pts',(-9.02271189225695,15.2,6.13089135798428));
#249267=CARTESIAN_POINT('Ctrl Pts',(-9.02503849740031,15.2,6.13396010073441));
#249268=CARTESIAN_POINT('Ctrl Pts',(-9.02736897016642,15.2,6.13704450853063));
#249269=CARTESIAN_POINT('Ctrl Pts',(-9.02970318136968,15.2,6.14014454804183));
#249270=CARTESIAN_POINT('Ctrl Pts',(-9.03262094561227,15.2,6.14401959774762));
#249271=CARTESIAN_POINT('Ctrl Pts',(-9.03554454809213,15.2,6.14791907070584));
#249272=CARTESIAN_POINT('Ctrl Pts',(-9.03847373559184,15.2,6.15184290021845));
#249273=CARTESIAN_POINT('Ctrl Pts',(-9.04140292309154,15.2,6.15576672973106));
#249274=CARTESIAN_POINT('Ctrl Pts',(-9.04433769423584,15.2,6.15971491420819));
#249275=CARTESIAN_POINT('Ctrl Pts',(-9.04727780083279,15.2,6.16368738879028));
#249276=CARTESIAN_POINT('Ctrl Pts',(-9.04962988623855,15.2,6.16686536862914));
#249277=CARTESIAN_POINT('Ctrl Pts',(-9.05198538539287,15.2,6.17005889342631));
#249278=CARTESIAN_POINT('Ctrl Pts',(-9.054344171584,15.2,6.17326792870733));
#249279=CARTESIAN_POINT('Ctrl Pts',(-9.05670295745375,15.2,6.17647696355111));
#249280=CARTESIAN_POINT('Ctrl Pts',(-9.05906502981693,15.2,6.1797015089844));
#249281=CARTESIAN_POINT('Ctrl Pts',(-9.06143026429005,15.2,6.18294152971853));
#249282=CARTESIAN_POINT('Ctrl Pts',(-9.06379549908542,15.2,6.1861815508941));
#249283=CARTESIAN_POINT('Ctrl Pts',(-9.06616389414783,15.2,6.18943704827154));
#249284=CARTESIAN_POINT('Ctrl Pts',(-9.06853532694394,15.2,6.19270798678414));
#249285=CARTESIAN_POINT('Ctrl Pts',(-9.07090675941694,15.2,6.19597892485107));
#249286=CARTESIAN_POINT('Ctrl Pts',(-9.07328122888098,15.2,6.19926530339546));
#249287=CARTESIAN_POINT('Ctrl Pts',(-9.07565861085301,15.2,6.20256708873509));
#249288=CARTESIAN_POINT('Ctrl Pts',(-9.07863033856098,15.2,6.20669432074703));
#249289=CARTESIAN_POINT('Ctrl Pts',(-9.08160662041098,15.2,6.21084562673059));
#249290=CARTESIAN_POINT('Ctrl Pts',(-9.08458721562906,15.2,6.21502093575699));
#249291=CARTESIAN_POINT('Ctrl Pts',(-9.08756781084713,15.2,6.21919624478339));
#249292=CARTESIAN_POINT('Ctrl Pts',(-9.09055272029924,15.2,6.22339555860844));
#249293=CARTESIAN_POINT('Ctrl Pts',(-9.09354170877125,15.2,6.22761880819053));
#249294=CARTESIAN_POINT('Ctrl Pts',(-9.09653069724327,15.2,6.23184205777262));
#249295=CARTESIAN_POINT('Ctrl Pts',(-9.09952376441539,15.2,6.23608924427754));
#249296=CARTESIAN_POINT('Ctrl Pts',(-9.10252067934573,15.2,6.24036029872074));
#249297=CARTESIAN_POINT('Ctrl Pts',(-9.10491821142068,15.2,6.24377714246151));
#249298=CARTESIAN_POINT('Ctrl Pts',(-9.10731820368361,15.2,6.24720926038603));
#249299=CARTESIAN_POINT('Ctrl Pts',(-9.10972054132366,15.2,6.25065661969191));
#249300=CARTESIAN_POINT('Ctrl Pts',(-9.11212287863637,15.2,6.25410397852807));
#249301=CARTESIAN_POINT('Ctrl Pts',(-9.11452755958632,15.2,6.2575665783205));
#249302=CARTESIAN_POINT('Ctrl Pts',(-9.1169344687783,15.2,6.26104438242409));
#249303=CARTESIAN_POINT('Ctrl Pts',(-9.11934137829823,15.2,6.26452218700154));
#249304=CARTESIAN_POINT('Ctrl Pts',(-9.12175051450451,15.2,6.26801519705856));
#249305=CARTESIAN_POINT('Ctrl Pts',(-9.12416176341386,15.2,6.27152337752853));
#249306=CARTESIAN_POINT('Ctrl Pts',(-9.12657301199466,15.2,6.27503155752052));
#249307=CARTESIAN_POINT('Ctrl Pts',(-9.12898637241543,15.2,6.2785549070337));
#249308=CARTESIAN_POINT('Ctrl Pts',(-9.13140173044957,15.2,6.28209339125321));
#249309=CARTESIAN_POINT('Ctrl Pts',(-9.1338170888128,15.2,6.28563187595485));
#249310=CARTESIAN_POINT('Ctrl Pts',(-9.13623444385753,15.2,6.28918549549077));
#249311=CARTESIAN_POINT('Ctrl Pts',(-9.13865368348951,15.2,6.29275421457515));
#249312=CARTESIAN_POINT('Ctrl Pts',(-9.14107292279187,15.2,6.2963229331733));
#249313=CARTESIAN_POINT('Ctrl Pts',(-9.14349404691327,15.2,6.29990675040727));
#249314=CARTESIAN_POINT('Ctrl Pts',(-9.1459169416039,15.2,6.30350563244484));
#249315=CARTESIAN_POINT('Ctrl Pts',(-9.14833983662467,15.2,6.30710451497278));
#249316=CARTESIAN_POINT('Ctrl Pts',(-9.15076450382512,15.2,6.310718461502));
#249317=CARTESIAN_POINT('Ctrl Pts',(-9.15319083096837,15.2,6.31434743599407));
#249318=CARTESIAN_POINT('Ctrl Pts',(-9.15561715778103,15.2,6.31797640999169));
#249319=CARTESIAN_POINT('Ctrl Pts',(-9.15804514545436,15.2,6.32162041310233));
#249320=CARTESIAN_POINT('Ctrl Pts',(-9.16047468331115,15.2,6.32527940913501));
#249321=CARTESIAN_POINT('Ctrl Pts',(-9.16290422149896,15.2,6.32893840566623));
#249322=CARTESIAN_POINT('Ctrl Pts',(-9.16533530998415,15.2,6.33261239456278));
#249323=CARTESIAN_POINT('Ctrl Pts',(-9.16776783778338,15.2,6.33630134104159));
#249324=CARTESIAN_POINT('Ctrl Pts',(-9.17020036558262,15.2,6.33999028752041));
#249325=CARTESIAN_POINT('Ctrl Pts',(-9.17263433607927,15.2,6.34369419127602));
#249326=CARTESIAN_POINT('Ctrl Pts',(-9.17506963715656,15.2,6.3474130175913));
#249327=CARTESIAN_POINT('Ctrl Pts',(-9.17689611279862,15.2,6.35020213707441));
#249328=CARTESIAN_POINT('Ctrl Pts',(-9.17872333796206,15.2,6.35299964865368));
#249329=CARTESIAN_POINT('Ctrl Pts',(-9.18055126761205,15.2,6.35580553981788));
#249330=CARTESIAN_POINT('Ctrl Pts',(-9.18237919726203,15.2,6.35861143098207));
#249331=CARTESIAN_POINT('Ctrl Pts',(-9.18420783059919,15.2,6.36142569972623));
#249332=CARTESIAN_POINT('Ctrl Pts',(-9.18603712274112,15.2,6.36424833229107));
#249333=CARTESIAN_POINT('Ctrl Pts',(-9.18786641488304,15.2,6.3670709648559));
#249334=CARTESIAN_POINT('Ctrl Pts',(-9.1896963666499,15.2,6.36990196020309));
#249335=CARTESIAN_POINT('Ctrl Pts',(-9.19152693225005,15.2,6.37274130426659));
#249336=CARTESIAN_POINT('Ctrl Pts',(-9.19396768660528,15.2,6.37652709669512));
#249337=CARTESIAN_POINT('Ctrl Pts',(-9.19640953221067,15.2,6.3803277310171));
#249338=CARTESIAN_POINT('Ctrl Pts',(-9.19885236589946,15.2,6.38414316961543));
#249339=CARTESIAN_POINT('Ctrl Pts',(-9.20068449099963,15.2,6.38700474830425));
#249340=CARTESIAN_POINT('Ctrl Pts',(-9.20251717106304,15.2,6.38987465506671));
#249341=CARTESIAN_POINT('Ctrl Pts',(-9.20435036137973,15.2,6.39275287527354));
#249342=CARTESIAN_POINT('Ctrl Pts',(-9.20618355169643,15.2,6.39563109548038));
#249343=CARTESIAN_POINT('Ctrl Pts',(-9.20801725426658,15.2,6.39851762778671));
#249344=CARTESIAN_POINT('Ctrl Pts',(-9.20985142294998,15.2,6.40141245830726));
#249345=CARTESIAN_POINT('Ctrl Pts',(-9.21168559163339,15.2,6.40430728882783));
#249346=CARTESIAN_POINT('Ctrl Pts',(-9.21352022765006,15.2,6.4072104164557));
#249347=CARTESIAN_POINT('Ctrl Pts',(-9.21535528729172,15.2,6.41012182705825));
#249348=CARTESIAN_POINT('Ctrl Pts',(-9.21719034693338,15.2,6.41303323766081));
#249349=CARTESIAN_POINT('Ctrl Pts',(-9.21902582983335,15.2,6.41595293105468));
#249350=CARTESIAN_POINT('Ctrl Pts',(-9.22086169351662,15.2,6.41888089165592));
#249351=CARTESIAN_POINT('Ctrl Pts',(-9.22269755719989,15.2,6.42180885225716));
#249352=CARTESIAN_POINT('Ctrl Pts',(-9.22453380211974,15.2,6.42474507917449));
#249353=CARTESIAN_POINT('Ctrl Pts',(-9.22637038389473,15.2,6.42768955892199));
#249354=CARTESIAN_POINT('Ctrl Pts',(-9.22820696566971,15.2,6.43063403866949));
#249355=CARTESIAN_POINT('Ctrl Pts',(-9.23004388491633,15.2,6.43358677072982));
#249356=CARTESIAN_POINT('Ctrl Pts',(-9.23188109905787,15.2,6.43654773932944));
#249357=CARTESIAN_POINT('Ctrl Pts',(-9.23371831353317,15.2,6.43950870846697));
#249358=CARTESIAN_POINT('Ctrl Pts',(-9.23555582266689,15.2,6.44247791406516));
#249359=CARTESIAN_POINT('Ctrl Pts',(-9.23739358464236,15.2,6.44545534212402));
#249360=CARTESIAN_POINT('Ctrl Pts',(-9.23923134628397,15.2,6.44843276964198));
#249361=CARTESIAN_POINT('Ctrl Pts',(-9.24106936066719,15.2,6.45141841821779));
#249362=CARTESIAN_POINT('Ctrl Pts',(-9.24290758443376,15.2,6.45441227285973));
#249363=CARTESIAN_POINT('Ctrl Pts',(-9.24474580820032,15.2,6.45740612750166));
#249364=CARTESIAN_POINT('Ctrl Pts',(-9.24658424357686,15.2,6.46040818908168));
#249365=CARTESIAN_POINT('Ctrl Pts',(-9.24842284722673,15.2,6.463418441236));
#249366=CARTESIAN_POINT('Ctrl Pts',(-9.2502614508766,15.2,6.46642869339033));
#249367=CARTESIAN_POINT('Ctrl Pts',(-9.25210022259017,15.2,6.4694471368601));
#249368=CARTESIAN_POINT('Ctrl Pts',(-9.25393912124005,15.2,6.47247375551385));
#249369=CARTESIAN_POINT('Ctrl Pts',(-9.25639098632926,15.2,6.47650924741873));
#249370=CARTESIAN_POINT('Ctrl Pts',(-9.25884307671734,15.2,6.48055927529425));
#249371=CARTESIAN_POINT('Ctrl Pts',(-9.26129529518433,15.2,6.48462379990616));
#249372=CARTESIAN_POINT('Ctrl Pts',(-9.26313445886752,15.2,6.48767219308819));
#249373=CARTESIAN_POINT('Ctrl Pts',(-9.26497369475068,15.2,6.49072874192808));
#249374=CARTESIAN_POINT('Ctrl Pts',(-9.26681296143387,15.2,6.49379343006745));
#249375=CARTESIAN_POINT('Ctrl Pts',(-9.26926531690006,15.2,6.49787968073436));
#249376=CARTESIAN_POINT('Ctrl Pts',(-9.27171772659957,15.2,6.50198040274556));
#249377=CARTESIAN_POINT('Ctrl Pts',(-9.27417009539909,15.2,6.5060955593521));
#249378=CARTESIAN_POINT('Ctrl Pts',(-9.2760093724164,15.2,6.50918192750788));
#249379=CARTESIAN_POINT('Ctrl Pts',(-9.27784862660039,15.2,6.51227641499096));
#249380=CARTESIAN_POINT('Ctrl Pts',(-9.27968781665933,15.2,6.51537900619297));
#249381=CARTESIAN_POINT('Ctrl Pts',(-9.2821400695144,15.2,6.5195157935229));
#249382=CARTESIAN_POINT('Ctrl Pts',(-9.28459220919047,15.2,6.52366698851598));
#249383=CARTESIAN_POINT('Ctrl Pts',(-9.28704414072339,15.2,6.52783255380543));
#249384=CARTESIAN_POINT('Ctrl Pts',(-9.2888830894566,15.2,6.53095672791441));
#249385=CARTESIAN_POINT('Ctrl Pts',(-9.29072192151643,15.2,6.53408898525591));
#249386=CARTESIAN_POINT('Ctrl Pts',(-9.29256059578298,15.2,6.5372293103911));
#249387=CARTESIAN_POINT('Ctrl Pts',(-9.29439927004952,15.2,6.5403696355263));
#249388=CARTESIAN_POINT('Ctrl Pts',(-9.29623778788273,15.2,6.54351802901093));
#249389=CARTESIAN_POINT('Ctrl Pts',(-9.29807610906597,15.2,6.54667447510349));
#249390=CARTESIAN_POINT('Ctrl Pts',(-9.29991443058316,15.2,6.54983092176947));
#249391=CARTESIAN_POINT('Ctrl Pts',(-9.30175255521699,15.2,6.55299542101272));
#249392=CARTESIAN_POINT('Ctrl Pts',(-9.30359044515072,15.2,6.55616795718322));
#249393=CARTESIAN_POINT('Ctrl Pts',(-9.30604096450588,15.2,6.56039800444996));
#249394=CARTESIAN_POINT('Ctrl Pts',(-9.30849106419308,15.2,6.56464234033144));
#249395=CARTESIAN_POINT('Ctrl Pts',(-9.31094065178172,15.2,6.56890092644704));
#249396=CARTESIAN_POINT('Ctrl Pts',(-9.31277784255665,15.2,6.57209486617879));
#249397=CARTESIAN_POINT('Ctrl Pts',(-9.31461474548323,15.2,6.57529682375083));
#249398=CARTESIAN_POINT('Ctrl Pts',(-9.31645132174987,15.2,6.57850678092517));
#249399=CARTESIAN_POINT('Ctrl Pts',(-9.3189000903278,15.2,6.58278672421304));
#249400=CARTESIAN_POINT('Ctrl Pts',(-9.32134827841678,15.2,6.58708089179985));
#249401=CARTESIAN_POINT('Ctrl Pts',(-9.3237957962168,15.2,6.59138924636893));
#249402=CARTESIAN_POINT('Ctrl Pts',(-9.32624331368334,15.2,6.59569760035099));
#249403=CARTESIAN_POINT('Ctrl Pts',(-9.32869016070891,15.2,6.60002014240703));
#249404=CARTESIAN_POINT('Ctrl Pts',(-9.33113624368678,15.2,6.60435683387906));
#249405=CARTESIAN_POINT('Ctrl Pts',(-9.3329708060035,15.2,6.6076093526308));
#249406=CARTESIAN_POINT('Ctrl Pts',(-9.33480493850019,15.2,6.61086983112389));
#249407=CARTESIAN_POINT('Ctrl Pts',(-9.33663860239199,15.2,6.61413825183742));
#249408=CARTESIAN_POINT('Ctrl Pts',(-9.33908348780312,15.2,6.61849614651796));
#249409=CARTESIAN_POINT('Ctrl Pts',(-9.34152754303359,15.2,6.62286816468036));
#249410=CARTESIAN_POINT('Ctrl Pts',(-9.34397068750006,15.2,6.62725426997492));
#249411=CARTESIAN_POINT('Ctrl Pts',(-9.34580304568348,15.2,6.63054384864704));
#249412=CARTESIAN_POINT('Ctrl Pts',(-9.34763489121691,15.2,6.6338413530272));
#249413=CARTESIAN_POINT('Ctrl Pts',(-9.34946618127544,15.2,6.63714676361477));
#249414=CARTESIAN_POINT('Ctrl Pts',(-9.35190790157527,15.2,6.64155397813186));
#249415=CARTESIAN_POINT('Ctrl Pts',(-9.35434863068266,15.2,6.64597524940131));
#249416=CARTESIAN_POINT('Ctrl Pts',(-9.35678826960406,15.2,6.6504105336436));
#249417=CARTESIAN_POINT('Ctrl Pts',(-9.35861799862891,15.2,6.65373699652316));
#249418=CARTESIAN_POINT('Ctrl Pts',(-9.3604471149025,15.2,6.65707134311622));
#249419=CARTESIAN_POINT('Ctrl Pts',(-9.36227560168603,15.2,6.66041356487327));
#249420=CARTESIAN_POINT('Ctrl Pts',(-9.36410408846955,15.2,6.66375578663033));
#249421=CARTESIAN_POINT('Ctrl Pts',(-9.36593194966811,15.2,6.66710588438994));
#249422=CARTESIAN_POINT('Ctrl Pts',(-9.36775917500006,15.2,6.67046385499999));
#249423=CARTESIAN_POINT('Origin',(-5.66257110645729E-14,15.2,-1.77635683940025E-14));
#249424=CARTESIAN_POINT('',(-8.88241603300006,15.2,5.36127880599999));
#249425=CARTESIAN_POINT('',(-8.88241603300006,12.2,5.36127880599999));
#249426=CARTESIAN_POINT('',(-8.88241603300006,15.2,5.36127880599999));
#249427=CARTESIAN_POINT('Origin',(-5.66257110645729E-14,12.2,-1.77635683940025E-14));
#249428=CARTESIAN_POINT('Origin',(-5.66257110645729E-14,15.2,-1.77635683940025E-14));
#249429=CARTESIAN_POINT('Origin',(-5.66257110645729E-14,15.2,-1.77635683940025E-14));
#249430=CARTESIAN_POINT('',(-10.0402696494501,15.2,5.60740451254565));
#249431=CARTESIAN_POINT('',(-10.2217148785197,15.2,5.26939701892417));
#249432=CARTESIAN_POINT('Origin',(-5.66257110645729E-14,15.2,-1.77635683940025E-14));
#249433=CARTESIAN_POINT('',(-10.2217148785197,12.2,5.26939701892417));
#249434=CARTESIAN_POINT('',(-10.2217148790001,15.2,5.26939701899998));
#249435=CARTESIAN_POINT('',(-10.0402696494501,12.2,5.60740451254564));
#249436=CARTESIAN_POINT('Origin',(-5.66257110645729E-14,12.2,-1.77635683940025E-14));
#249437=CARTESIAN_POINT('',(-10.0402696500001,15.2,5.60740451299999));
#249438=CARTESIAN_POINT('Ctrl Pts',(-10.2217148780001,15.2,5.26939701899998));
#249439=CARTESIAN_POINT('Ctrl Pts',(-10.2217148780001,11.6,5.26939701899998));
#249440=CARTESIAN_POINT('Ctrl Pts',(-10.2212575740001,15.2,5.26878426899999));
#249441=CARTESIAN_POINT('Ctrl Pts',(-10.2212575740001,11.6,5.26878426899999));
#249442=CARTESIAN_POINT('Ctrl Pts',(-10.2203430010001,15.2,5.26755929399998));
#249443=CARTESIAN_POINT('Ctrl Pts',(-10.2203430010001,11.6,5.26755929399998));
#249444=CARTESIAN_POINT('Ctrl Pts',(-10.2189712390001,15.2,5.26572340899998));
#249445=CARTESIAN_POINT('Ctrl Pts',(-10.2189712390001,11.6,5.26572340899998));
#249446=CARTESIAN_POINT('Ctrl Pts',(-10.2171424210001,15.2,5.26327871599998));
#249447=CARTESIAN_POINT('Ctrl Pts',(-10.2171424210001,11.6,5.26327871599998));
#249448=CARTESIAN_POINT('Ctrl Pts',(-10.2148567310001,15.2,5.26022810499998));
#249449=CARTESIAN_POINT('Ctrl Pts',(-10.2148567310001,11.6,5.26022810499998));
#249450=CARTESIAN_POINT('Ctrl Pts',(-10.2125713740001,15.2,5.25718275199999));
#249451=CARTESIAN_POINT('Ctrl Pts',(-10.2125713740001,11.6,5.25718275199999));
#249452=CARTESIAN_POINT('Ctrl Pts',(-10.2102863520001,15.2,5.25414265499998));
#249453=CARTESIAN_POINT('Ctrl Pts',(-10.2102863520001,11.6,5.25414265499998));
#249454=CARTESIAN_POINT('Ctrl Pts',(-10.2080016700001,15.2,5.25110781899999));
#249455=CARTESIAN_POINT('Ctrl Pts',(-10.2080016700001,11.6,5.25110781899999));
#249456=CARTESIAN_POINT('Ctrl Pts',(-10.2057173310001,15.2,5.24807824199998));
#249457=CARTESIAN_POINT('Ctrl Pts',(-10.2057173310001,11.6,5.24807824199998));
#249458=CARTESIAN_POINT('Ctrl Pts',(-10.2034333450001,15.2,5.24505392699999));
#249459=CARTESIAN_POINT('Ctrl Pts',(-10.2034333450001,11.6,5.24505392699999));
#249460=CARTESIAN_POINT('Ctrl Pts',(-10.2011497210001,15.2,5.24203487699998));
#249461=CARTESIAN_POINT('Ctrl Pts',(-10.2011497210001,11.6,5.24203487699998));
#249462=CARTESIAN_POINT('Ctrl Pts',(-10.1988664690001,15.2,5.23902109499998));
#249463=CARTESIAN_POINT('Ctrl Pts',(-10.1988664690001,11.6,5.23902109499998));
#249464=CARTESIAN_POINT('Ctrl Pts',(-10.1965836000001,15.2,5.23601258299998));
#249465=CARTESIAN_POINT('Ctrl Pts',(-10.1965836000001,11.6,5.23601258299998));
#249466=CARTESIAN_POINT('Ctrl Pts',(-10.1943011260001,15.2,5.23300934399998));
#249467=CARTESIAN_POINT('Ctrl Pts',(-10.1943011260001,11.6,5.23300934399998));
#249468=CARTESIAN_POINT('Ctrl Pts',(-10.1920190550001,15.2,5.23001137999999));
#249469=CARTESIAN_POINT('Ctrl Pts',(-10.1920190550001,11.6,5.23001137999999));
#249470=CARTESIAN_POINT('Ctrl Pts',(-10.1897373990001,15.2,5.22701869499999));
#249471=CARTESIAN_POINT('Ctrl Pts',(-10.1897373990001,11.6,5.22701869499999));
#249472=CARTESIAN_POINT('Ctrl Pts',(-10.1874561630001,15.2,5.22403128999999));
#249473=CARTESIAN_POINT('Ctrl Pts',(-10.1874561630001,11.6,5.22403128999999));
#249474=CARTESIAN_POINT('Ctrl Pts',(-10.1851753570001,15.2,5.22104916599999));
#249475=CARTESIAN_POINT('Ctrl Pts',(-10.1851753570001,11.6,5.22104916599999));
#249476=CARTESIAN_POINT('Ctrl Pts',(-10.1828949880001,15.2,5.21807232799999));
#249477=CARTESIAN_POINT('Ctrl Pts',(-10.1828949880001,11.6,5.21807232799999));
#249478=CARTESIAN_POINT('Ctrl Pts',(-10.1806150650001,15.2,5.21510077499999));
#249479=CARTESIAN_POINT('Ctrl Pts',(-10.1806150650001,11.6,5.21510077499999));
#249480=CARTESIAN_POINT('Ctrl Pts',(-10.1783355960001,15.2,5.21213451099998));
#249481=CARTESIAN_POINT('Ctrl Pts',(-10.1783355960001,11.6,5.21213451099998));
#249482=CARTESIAN_POINT('Ctrl Pts',(-10.1760565880001,15.2,5.20917353699998));
#249483=CARTESIAN_POINT('Ctrl Pts',(-10.1760565880001,11.6,5.20917353699998));
#249484=CARTESIAN_POINT('Ctrl Pts',(-10.1737780520001,15.2,5.20621785499999));
#249485=CARTESIAN_POINT('Ctrl Pts',(-10.1737780520001,11.6,5.20621785499999));
#249486=CARTESIAN_POINT('Ctrl Pts',(-10.1714999970001,15.2,5.20326746899999));
#249487=CARTESIAN_POINT('Ctrl Pts',(-10.1714999970001,11.6,5.20326746899999));
#249488=CARTESIAN_POINT('Ctrl Pts',(-10.1692224320001,15.2,5.20032237999998));
#249489=CARTESIAN_POINT('Ctrl Pts',(-10.1692224320001,11.6,5.20032237999998));
#249490=CARTESIAN_POINT('Ctrl Pts',(-10.1669453660001,15.2,5.19738259099999));
#249491=CARTESIAN_POINT('Ctrl Pts',(-10.1669453660001,11.6,5.19738259099999));
#249492=CARTESIAN_POINT('Ctrl Pts',(-10.1646688090001,15.2,5.19444810399998));
#249493=CARTESIAN_POINT('Ctrl Pts',(-10.1646688090001,11.6,5.19444810399998));
#249494=CARTESIAN_POINT('Ctrl Pts',(-10.1623927680001,15.2,5.19151892199999));
#249495=CARTESIAN_POINT('Ctrl Pts',(-10.1623927680001,11.6,5.19151892199999));
#249496=CARTESIAN_POINT('Ctrl Pts',(-10.1601172530001,15.2,5.18859504499999));
#249497=CARTESIAN_POINT('Ctrl Pts',(-10.1601172530001,11.6,5.18859504499999));
#249498=CARTESIAN_POINT('Ctrl Pts',(-10.1578422740001,15.2,5.18567647699999));
#249499=CARTESIAN_POINT('Ctrl Pts',(-10.1578422740001,11.6,5.18567647699999));
#249500=CARTESIAN_POINT('Ctrl Pts',(-10.1555678380001,15.2,5.18276321899998));
#249501=CARTESIAN_POINT('Ctrl Pts',(-10.1555678380001,11.6,5.18276321899998));
#249502=CARTESIAN_POINT('Ctrl Pts',(-10.1532939540001,15.2,5.17985527399999));
#249503=CARTESIAN_POINT('Ctrl Pts',(-10.1532939540001,11.6,5.17985527399999));
#249504=CARTESIAN_POINT('Ctrl Pts',(-10.1510206320001,15.2,5.17695264399999));
#249505=CARTESIAN_POINT('Ctrl Pts',(-10.1510206320001,11.6,5.17695264399999));
#249506=CARTESIAN_POINT('Ctrl Pts',(-10.1487478800001,15.2,5.17405533199998));
#249507=CARTESIAN_POINT('Ctrl Pts',(-10.1487478800001,11.6,5.17405533199998));
#249508=CARTESIAN_POINT('Ctrl Pts',(-10.1464757090001,15.2,5.17116333899998));
#249509=CARTESIAN_POINT('Ctrl Pts',(-10.1464757090001,11.6,5.17116333899998));
#249510=CARTESIAN_POINT('Ctrl Pts',(-10.1442041250001,15.2,5.16827666599998));
#249511=CARTESIAN_POINT('Ctrl Pts',(-10.1442041250001,11.6,5.16827666599998));
#249512=CARTESIAN_POINT('Ctrl Pts',(-10.1419331390001,15.2,5.16539531899999));
#249513=CARTESIAN_POINT('Ctrl Pts',(-10.1419331390001,11.6,5.16539531899999));
#249514=CARTESIAN_POINT('Ctrl Pts',(-10.1396627610001,15.2,5.16251929699998));
#249515=CARTESIAN_POINT('Ctrl Pts',(-10.1396627610001,11.6,5.16251929699998));
#249516=CARTESIAN_POINT('Ctrl Pts',(-10.1373930000001,15.2,5.15964860299999));
#249517=CARTESIAN_POINT('Ctrl Pts',(-10.1373930000001,11.6,5.15964860299999));
#249518=CARTESIAN_POINT('Ctrl Pts',(-10.1351238630001,15.2,5.15678323899999));
#249519=CARTESIAN_POINT('Ctrl Pts',(-10.1351238630001,11.6,5.15678323899999));
#249520=CARTESIAN_POINT('Ctrl Pts',(-10.1328553600001,15.2,5.15392320699998));
#249521=CARTESIAN_POINT('Ctrl Pts',(-10.1328553600001,11.6,5.15392320699998));
#249522=CARTESIAN_POINT('Ctrl Pts',(-10.1305875000001,15.2,5.15106850999998));
#249523=CARTESIAN_POINT('Ctrl Pts',(-10.1305875000001,11.6,5.15106850999998));
#249524=CARTESIAN_POINT('Ctrl Pts',(-10.1283202940001,15.2,5.14821914899999));
#249525=CARTESIAN_POINT('Ctrl Pts',(-10.1283202940001,11.6,5.14821914899999));
#249526=CARTESIAN_POINT('Ctrl Pts',(-10.1260537500001,15.2,5.14537512799999));
#249527=CARTESIAN_POINT('Ctrl Pts',(-10.1260537500001,11.6,5.14537512799999));
#249528=CARTESIAN_POINT('Ctrl Pts',(-10.1237878770001,15.2,5.14253644699998));
#249529=CARTESIAN_POINT('Ctrl Pts',(-10.1237878770001,11.6,5.14253644699998));
#249530=CARTESIAN_POINT('Ctrl Pts',(-10.1215226840001,15.2,5.13970310999999));
#249531=CARTESIAN_POINT('Ctrl Pts',(-10.1215226840001,11.6,5.13970310999999));
#249532=CARTESIAN_POINT('Ctrl Pts',(-10.1192581800001,15.2,5.13687511699998));
#249533=CARTESIAN_POINT('Ctrl Pts',(-10.1192581800001,11.6,5.13687511699998));
#249534=CARTESIAN_POINT('Ctrl Pts',(-10.1169943770001,15.2,5.13405247199999));
#249535=CARTESIAN_POINT('Ctrl Pts',(-10.1169943770001,11.6,5.13405247199999));
#249536=CARTESIAN_POINT('Ctrl Pts',(-10.1147312810001,15.2,5.13123517699999));
#249537=CARTESIAN_POINT('Ctrl Pts',(-10.1147312810001,11.6,5.13123517699999));
#249538=CARTESIAN_POINT('Ctrl Pts',(-10.1124689020001,15.2,5.12842323299999));
#249539=CARTESIAN_POINT('Ctrl Pts',(-10.1124689020001,11.6,5.12842323299999));
#249540=CARTESIAN_POINT('Ctrl Pts',(-10.1102072500001,15.2,5.12561664199998));
#249541=CARTESIAN_POINT('Ctrl Pts',(-10.1102072500001,11.6,5.12561664199998));
#249542=CARTESIAN_POINT('Ctrl Pts',(-10.1079463350001,15.2,5.12281540799999));
#249543=CARTESIAN_POINT('Ctrl Pts',(-10.1079463350001,11.6,5.12281540799999));
#249544=CARTESIAN_POINT('Ctrl Pts',(-10.1056861660001,15.2,5.12001953099999));
#249545=CARTESIAN_POINT('Ctrl Pts',(-10.1056861660001,11.6,5.12001953099999));
#249546=CARTESIAN_POINT('Ctrl Pts',(-10.1034267510001,15.2,5.11722901499999));
#249547=CARTESIAN_POINT('Ctrl Pts',(-10.1034267510001,11.6,5.11722901499999));
#249548=CARTESIAN_POINT('Ctrl Pts',(-10.1011681000001,15.2,5.11444385899999));
#249549=CARTESIAN_POINT('Ctrl Pts',(-10.1011681000001,11.6,5.11444385899999));
#249550=CARTESIAN_POINT('Ctrl Pts',(-10.0989102230001,15.2,5.11166406999998));
#249551=CARTESIAN_POINT('Ctrl Pts',(-10.0989102230001,11.6,5.11166406999998));
#249552=CARTESIAN_POINT('Ctrl Pts',(-10.0966531300001,15.2,5.10888964599998));
#249553=CARTESIAN_POINT('Ctrl Pts',(-10.0966531300001,11.6,5.10888964599998));
#249554=CARTESIAN_POINT('Ctrl Pts',(-10.0943968300001,15.2,5.10612058999998));
#249555=CARTESIAN_POINT('Ctrl Pts',(-10.0943968300001,11.6,5.10612058999998));
#249556=CARTESIAN_POINT('Ctrl Pts',(-10.0921413310001,15.2,5.10335690499998));
#249557=CARTESIAN_POINT('Ctrl Pts',(-10.0921413310001,11.6,5.10335690499998));
#249558=CARTESIAN_POINT('Ctrl Pts',(-10.0898866440001,15.2,5.10059859299999));
#249559=CARTESIAN_POINT('Ctrl Pts',(-10.0898866440001,11.6,5.10059859299999));
#249560=CARTESIAN_POINT('Ctrl Pts',(-10.0876327790001,15.2,5.09784565499999));
#249561=CARTESIAN_POINT('Ctrl Pts',(-10.0876327790001,11.6,5.09784565499999));
#249562=CARTESIAN_POINT('Ctrl Pts',(-10.0853797440001,15.2,5.09509809399999));
#249563=CARTESIAN_POINT('Ctrl Pts',(-10.0853797440001,11.6,5.09509809399999));
#249564=CARTESIAN_POINT('Ctrl Pts',(-10.0831275500001,15.2,5.09235591199998));
#249565=CARTESIAN_POINT('Ctrl Pts',(-10.0831275500001,11.6,5.09235591199998));
#249566=CARTESIAN_POINT('Ctrl Pts',(-10.0808762050001,15.2,5.08961910999999));
#249567=CARTESIAN_POINT('Ctrl Pts',(-10.0808762050001,11.6,5.08961910999999));
#249568=CARTESIAN_POINT('Ctrl Pts',(-10.0786257200001,15.2,5.08688769099999));
#249569=CARTESIAN_POINT('Ctrl Pts',(-10.0786257200001,11.6,5.08688769099999));
#249570=CARTESIAN_POINT('Ctrl Pts',(-10.0763761030001,15.2,5.08416165899998));
#249571=CARTESIAN_POINT('Ctrl Pts',(-10.0763761030001,11.6,5.08416165899998));
#249572=CARTESIAN_POINT('Ctrl Pts',(-10.0741273660001,15.2,5.08144101199999));
#249573=CARTESIAN_POINT('Ctrl Pts',(-10.0741273660001,11.6,5.08144101199999));
#249574=CARTESIAN_POINT('Ctrl Pts',(-10.0718795170001,15.2,5.07872575499999));
#249575=CARTESIAN_POINT('Ctrl Pts',(-10.0718795170001,11.6,5.07872575499999));
#249576=CARTESIAN_POINT('Ctrl Pts',(-10.0696325650001,15.2,5.07601588799999));
#249577=CARTESIAN_POINT('Ctrl Pts',(-10.0696325650001,11.6,5.07601588799999));
#249578=CARTESIAN_POINT('Ctrl Pts',(-10.0673865220001,15.2,5.07331141599998));
#249579=CARTESIAN_POINT('Ctrl Pts',(-10.0673865220001,11.6,5.07331141599998));
#249580=CARTESIAN_POINT('Ctrl Pts',(-10.0651413960001,15.2,5.07061233799998));
#249581=CARTESIAN_POINT('Ctrl Pts',(-10.0651413960001,11.6,5.07061233799998));
#249582=CARTESIAN_POINT('Ctrl Pts',(-10.0628971970001,15.2,5.06791865699999));
#249583=CARTESIAN_POINT('Ctrl Pts',(-10.0628971970001,11.6,5.06791865699999));
#249584=CARTESIAN_POINT('Ctrl Pts',(-10.0606539350001,15.2,5.06523037599998));
#249585=CARTESIAN_POINT('Ctrl Pts',(-10.0606539350001,11.6,5.06523037599998));
#249586=CARTESIAN_POINT('Ctrl Pts',(-10.0584116200001,15.2,5.06254749499998));
#249587=CARTESIAN_POINT('Ctrl Pts',(-10.0584116200001,11.6,5.06254749499998));
#249588=CARTESIAN_POINT('Ctrl Pts',(-10.0561702600001,15.2,5.05987001899998));
#249589=CARTESIAN_POINT('Ctrl Pts',(-10.0561702600001,11.6,5.05987001899998));
#249590=CARTESIAN_POINT('Ctrl Pts',(-10.0539298680001,15.2,5.05719794699999));
#249591=CARTESIAN_POINT('Ctrl Pts',(-10.0539298680001,11.6,5.05719794699999));
#249592=CARTESIAN_POINT('Ctrl Pts',(-10.0516904520001,15.2,5.05453128299998));
#249593=CARTESIAN_POINT('Ctrl Pts',(-10.0516904520001,11.6,5.05453128299998));
#249594=CARTESIAN_POINT('Ctrl Pts',(-10.0494520200001,15.2,5.05187002899999));
#249595=CARTESIAN_POINT('Ctrl Pts',(-10.0494520200001,11.6,5.05187002899999));
#249596=CARTESIAN_POINT('Ctrl Pts',(-10.0472145860001,15.2,5.04921418599999));
#249597=CARTESIAN_POINT('Ctrl Pts',(-10.0472145860001,11.6,5.04921418599999));
#249598=CARTESIAN_POINT('Ctrl Pts',(-10.0449781570001,15.2,5.04656375599998));
#249599=CARTESIAN_POINT('Ctrl Pts',(-10.0449781570001,11.6,5.04656375599998));
#249600=CARTESIAN_POINT('Ctrl Pts',(-10.0427427430001,15.2,5.04391874099999));
#249601=CARTESIAN_POINT('Ctrl Pts',(-10.0427427430001,11.6,5.04391874099999));
#249602=CARTESIAN_POINT('Ctrl Pts',(-10.0405083540001,15.2,5.04127914399999));
#249603=CARTESIAN_POINT('Ctrl Pts',(-10.0405083540001,11.6,5.04127914399999));
#249604=CARTESIAN_POINT('Ctrl Pts',(-10.0382750020001,15.2,5.03864496599999));
#249605=CARTESIAN_POINT('Ctrl Pts',(-10.0382750020001,11.6,5.03864496599999));
#249606=CARTESIAN_POINT('Ctrl Pts',(-10.0360426940001,15.2,5.03601620899998));
#249607=CARTESIAN_POINT('Ctrl Pts',(-10.0360426940001,11.6,5.03601620899998));
#249608=CARTESIAN_POINT('Ctrl Pts',(-10.0338114420001,15.2,5.03339287599999));
#249609=CARTESIAN_POINT('Ctrl Pts',(-10.0338114420001,11.6,5.03339287599999));
#249610=CARTESIAN_POINT('Ctrl Pts',(-10.0315812560001,15.2,5.03077496799998));
#249611=CARTESIAN_POINT('Ctrl Pts',(-10.0315812560001,11.6,5.03077496799998));
#249612=CARTESIAN_POINT('Ctrl Pts',(-10.0293521450001,15.2,5.02816248699999));
#249613=CARTESIAN_POINT('Ctrl Pts',(-10.0293521450001,11.6,5.02816248699999));
#249614=CARTESIAN_POINT('Ctrl Pts',(-10.0271241190001,15.2,5.02555543599998));
#249615=CARTESIAN_POINT('Ctrl Pts',(-10.0271241190001,11.6,5.02555543599998));
#249616=CARTESIAN_POINT('Ctrl Pts',(-10.0248971890001,15.2,5.02295381499999));
#249617=CARTESIAN_POINT('Ctrl Pts',(-10.0248971890001,11.6,5.02295381499999));
#249618=CARTESIAN_POINT('Ctrl Pts',(-10.0226713640001,15.2,5.02035762799999));
#249619=CARTESIAN_POINT('Ctrl Pts',(-10.0226713640001,11.6,5.02035762799999));
#249620=CARTESIAN_POINT('Ctrl Pts',(-10.0204466560001,15.2,5.01776687599998));
#249621=CARTESIAN_POINT('Ctrl Pts',(-10.0204466560001,11.6,5.01776687599998));
#249622=CARTESIAN_POINT('Ctrl Pts',(-10.0182230730001,15.2,5.01518155999998));
#249623=CARTESIAN_POINT('Ctrl Pts',(-10.0182230730001,11.6,5.01518155999998));
#249624=CARTESIAN_POINT('Ctrl Pts',(-10.0160006270001,15.2,5.01260168399998));
#249625=CARTESIAN_POINT('Ctrl Pts',(-10.0160006270001,11.6,5.01260168399998));
#249626=CARTESIAN_POINT('Ctrl Pts',(-10.0137793260001,15.2,5.01002724899998));
#249627=CARTESIAN_POINT('Ctrl Pts',(-10.0137793260001,11.6,5.01002724899998));
#249628=CARTESIAN_POINT('Ctrl Pts',(-10.0115591820001,15.2,5.00745825599999));
#249629=CARTESIAN_POINT('Ctrl Pts',(-10.0115591820001,11.6,5.00745825599999));
#249630=CARTESIAN_POINT('Ctrl Pts',(-10.0093402040001,15.2,5.00489470899999));
#249631=CARTESIAN_POINT('Ctrl Pts',(-10.0093402040001,11.6,5.00489470899999));
#249632=CARTESIAN_POINT('Ctrl Pts',(-10.0071224030001,15.2,5.00233660799999));
#249633=CARTESIAN_POINT('Ctrl Pts',(-10.0071224030001,11.6,5.00233660799999));
#249634=CARTESIAN_POINT('Ctrl Pts',(-10.0049057900001,15.2,4.99978395499999));
#249635=CARTESIAN_POINT('Ctrl Pts',(-10.0049057900001,11.6,4.99978395499998));
#249636=CARTESIAN_POINT('Ctrl Pts',(-10.0026903730001,15.2,4.99723675299999));
#249637=CARTESIAN_POINT('Ctrl Pts',(-10.0026903730001,11.6,4.99723675299998));
#249638=CARTESIAN_POINT('Ctrl Pts',(-10.0004761650001,15.2,4.99469500399999));
#249639=CARTESIAN_POINT('Ctrl Pts',(-10.0004761650001,11.6,4.99469500399999));
#249640=CARTESIAN_POINT('Ctrl Pts',(-9.99826317500006,15.2,4.99215870899998));
#249641=CARTESIAN_POINT('Ctrl Pts',(-9.99826317500006,11.6,4.99215870899998));
#249642=CARTESIAN_POINT('Ctrl Pts',(-9.99605141300006,15.2,4.98962787099998));
#249643=CARTESIAN_POINT('Ctrl Pts',(-9.99605141300006,11.6,4.98962787099998));
#249644=CARTESIAN_POINT('Ctrl Pts',(-9.99384088900005,15.2,4.98710248899998));
#249645=CARTESIAN_POINT('Ctrl Pts',(-9.99384088900005,11.6,4.98710248899998));
#249646=CARTESIAN_POINT('Ctrl Pts',(-9.99163161400006,15.2,4.98458256899998));
#249647=CARTESIAN_POINT('Ctrl Pts',(-9.99163161400006,11.6,4.98458256899998));
#249648=CARTESIAN_POINT('Ctrl Pts',(-9.98942360000006,15.2,4.98206810999999));
#249649=CARTESIAN_POINT('Ctrl Pts',(-9.98942360000006,11.6,4.98206810999999));
#249650=CARTESIAN_POINT('Ctrl Pts',(-9.98721685500006,15.2,4.97955911499999));
#249651=CARTESIAN_POINT('Ctrl Pts',(-9.98721685500006,11.6,4.97955911499999));
#249652=CARTESIAN_POINT('Ctrl Pts',(-9.98501139000006,15.2,4.97705558599999));
#249653=CARTESIAN_POINT('Ctrl Pts',(-9.98501139000006,11.6,4.97705558599998));
#249654=CARTESIAN_POINT('Ctrl Pts',(-9.98280721700005,15.2,4.97455752399999));
#249655=CARTESIAN_POINT('Ctrl Pts',(-9.98280721700005,11.6,4.97455752399999));
#249656=CARTESIAN_POINT('Ctrl Pts',(-9.98060434500006,15.2,4.97206493199998));
#249657=CARTESIAN_POINT('Ctrl Pts',(-9.98060434500006,11.6,4.97206493199998));
#249658=CARTESIAN_POINT('Ctrl Pts',(-9.97840278500006,15.2,4.96957781099999));
#249659=CARTESIAN_POINT('Ctrl Pts',(-9.97840278500006,11.6,4.96957781099999));
#249660=CARTESIAN_POINT('Ctrl Pts',(-9.97620254700006,15.2,4.96709616399999));
#249661=CARTESIAN_POINT('Ctrl Pts',(-9.97620254700006,11.6,4.96709616399999));
#249662=CARTESIAN_POINT('Ctrl Pts',(-9.97400364300006,15.2,4.96461999099999));
#249663=CARTESIAN_POINT('Ctrl Pts',(-9.97400364300006,11.6,4.96461999099999));
#249664=CARTESIAN_POINT('Ctrl Pts',(-9.97180608100006,15.2,4.96214929599999));
#249665=CARTESIAN_POINT('Ctrl Pts',(-9.97180608100006,11.6,4.96214929599999));
#249666=CARTESIAN_POINT('Ctrl Pts',(-9.96960987500006,15.2,4.95968407899999));
#249667=CARTESIAN_POINT('Ctrl Pts',(-9.96960987500006,11.6,4.95968407899999));
#249668=CARTESIAN_POINT('Ctrl Pts',(-9.96741503200005,15.2,4.95722434199998));
#249669=CARTESIAN_POINT('Ctrl Pts',(-9.96741503200005,11.6,4.95722434199998));
#249670=CARTESIAN_POINT('Ctrl Pts',(-9.96522156600006,15.2,4.95477008799998));
#249671=CARTESIAN_POINT('Ctrl Pts',(-9.96522156600006,11.6,4.95477008799998));
#249672=CARTESIAN_POINT('Ctrl Pts',(-9.96302948600006,15.2,4.95232131899999));
#249673=CARTESIAN_POINT('Ctrl Pts',(-9.96302948600006,11.6,4.95232131899999));
#249674=CARTESIAN_POINT('Ctrl Pts',(-9.96083880200005,15.2,4.94987803499999));
#249675=CARTESIAN_POINT('Ctrl Pts',(-9.96083880200005,11.6,4.94987803499999));
#249676=CARTESIAN_POINT('Ctrl Pts',(-9.95864952600006,15.2,4.94744023899998));
#249677=CARTESIAN_POINT('Ctrl Pts',(-9.95864952600006,11.6,4.94744023899998));
#249678=CARTESIAN_POINT('Ctrl Pts',(-9.95646166800006,15.2,4.94500793199999));
#249679=CARTESIAN_POINT('Ctrl Pts',(-9.95646166800006,11.6,4.94500793199998));
#249680=CARTESIAN_POINT('Ctrl Pts',(-9.95427524000006,15.2,4.94258111799999));
#249681=CARTESIAN_POINT('Ctrl Pts',(-9.95427524000006,11.6,4.94258111799999));
#249682=CARTESIAN_POINT('Ctrl Pts',(-9.95209025100005,15.2,4.94015979599999));
#249683=CARTESIAN_POINT('Ctrl Pts',(-9.95209025100005,11.6,4.94015979599998));
#249684=CARTESIAN_POINT('Ctrl Pts',(-9.94990671400006,15.2,4.93774396999999));
#249685=CARTESIAN_POINT('Ctrl Pts',(-9.94990671400006,11.6,4.93774396999999));
#249686=CARTESIAN_POINT('Ctrl Pts',(-9.94772463800006,15.2,4.93533364199998));
#249687=CARTESIAN_POINT('Ctrl Pts',(-9.94772463800006,11.6,4.93533364199998));
#249688=CARTESIAN_POINT('Ctrl Pts',(-9.94554403500005,15.2,4.93292881099999));
#249689=CARTESIAN_POINT('Ctrl Pts',(-9.94554403500005,11.6,4.93292881099998));
#249690=CARTESIAN_POINT('Ctrl Pts',(-9.94336491400006,15.2,4.93052947999999));
#249691=CARTESIAN_POINT('Ctrl Pts',(-9.94336491400006,11.6,4.93052947999998));
#249692=CARTESIAN_POINT('Ctrl Pts',(-9.94118728800006,15.2,4.92813565299999));
#249693=CARTESIAN_POINT('Ctrl Pts',(-9.94118728800006,11.6,4.92813565299999));
#249694=CARTESIAN_POINT('Ctrl Pts',(-9.93901116700006,15.2,4.92574732999999));
#249695=CARTESIAN_POINT('Ctrl Pts',(-9.93901116700006,11.6,4.92574732999999));
#249696=CARTESIAN_POINT('Ctrl Pts',(-9.93683656200006,15.2,4.92336451199999));
#249697=CARTESIAN_POINT('Ctrl Pts',(-9.93683656200006,11.6,4.92336451199998));
#249698=CARTESIAN_POINT('Ctrl Pts',(-9.93466348400006,15.2,4.92098720199999));
#249699=CARTESIAN_POINT('Ctrl Pts',(-9.93466348400006,11.6,4.92098720199999));
#249700=CARTESIAN_POINT('Ctrl Pts',(-9.93249194500006,15.2,4.91861540099999));
#249701=CARTESIAN_POINT('Ctrl Pts',(-9.93249194500006,11.6,4.91861540099999));
#249702=CARTESIAN_POINT('Ctrl Pts',(-9.93032195400006,15.2,4.91624911099999));
#249703=CARTESIAN_POINT('Ctrl Pts',(-9.93032195400006,11.6,4.91624911099999));
#249704=CARTESIAN_POINT('Ctrl Pts',(-9.92815352500006,15.2,4.91388833399999));
#249705=CARTESIAN_POINT('Ctrl Pts',(-9.92815352500006,11.6,4.91388833399998));
#249706=CARTESIAN_POINT('Ctrl Pts',(-9.92598666500006,15.2,4.91153307199999));
#249707=CARTESIAN_POINT('Ctrl Pts',(-9.92598666500006,11.6,4.91153307199998));
#249708=CARTESIAN_POINT('Ctrl Pts',(-9.92382138900006,15.2,4.90918332699999));
#249709=CARTESIAN_POINT('Ctrl Pts',(-9.92382138900006,11.6,4.90918332699999));
#249710=CARTESIAN_POINT('Ctrl Pts',(-9.92165770700005,15.2,4.90683909899998));
#249711=CARTESIAN_POINT('Ctrl Pts',(-9.92165770700005,11.6,4.90683909899998));
#249712=CARTESIAN_POINT('Ctrl Pts',(-9.91949562900006,15.2,4.90450039199998));
#249713=CARTESIAN_POINT('Ctrl Pts',(-9.91949562900006,11.6,4.90450039199998));
#249714=CARTESIAN_POINT('Ctrl Pts',(-9.91733516600006,15.2,4.90216720499999));
#249715=CARTESIAN_POINT('Ctrl Pts',(-9.91733516600006,11.6,4.90216720499998));
#249716=CARTESIAN_POINT('Ctrl Pts',(-9.91517633100005,15.2,4.89983954299999));
#249717=CARTESIAN_POINT('Ctrl Pts',(-9.91517633100005,11.6,4.89983954299999));
#249718=CARTESIAN_POINT('Ctrl Pts',(-9.91301913400006,15.2,4.89751740499998));
#249719=CARTESIAN_POINT('Ctrl Pts',(-9.91301913400006,11.6,4.89751740499998));
#249720=CARTESIAN_POINT('Ctrl Pts',(-9.91086358700005,15.2,4.89520079499999));
#249721=CARTESIAN_POINT('Ctrl Pts',(-9.91086358700005,11.6,4.89520079499999));
#249722=CARTESIAN_POINT('Ctrl Pts',(-9.90870970100006,15.2,4.89288971199999));
#249723=CARTESIAN_POINT('Ctrl Pts',(-9.90870970100006,11.6,4.89288971199999));
#249724=CARTESIAN_POINT('Ctrl Pts',(-9.90655748600006,15.2,4.89058415999998));
#249725=CARTESIAN_POINT('Ctrl Pts',(-9.90655748600006,11.6,4.89058415999998));
#249726=CARTESIAN_POINT('Ctrl Pts',(-9.90440695600006,15.2,4.88828413899999));
#249727=CARTESIAN_POINT('Ctrl Pts',(-9.90440695600006,11.6,4.88828413899998));
#249728=CARTESIAN_POINT('Ctrl Pts',(-9.90225812000006,15.2,4.88598965199999));
#249729=CARTESIAN_POINT('Ctrl Pts',(-9.90225812000006,11.6,4.88598965199999));
#249730=CARTESIAN_POINT('Ctrl Pts',(-9.90011099000006,15.2,4.88370070099998));
#249731=CARTESIAN_POINT('Ctrl Pts',(-9.90011099000006,11.6,4.88370070099998));
#249732=CARTESIAN_POINT('Ctrl Pts',(-9.89796557800006,15.2,4.88141728499999));
#249733=CARTESIAN_POINT('Ctrl Pts',(-9.89796557800006,11.6,4.88141728499999));
#249734=CARTESIAN_POINT('Ctrl Pts',(-9.89582189500006,15.2,4.87913940899999));
#249735=CARTESIAN_POINT('Ctrl Pts',(-9.89582189500006,11.6,4.87913940899999));
#249736=CARTESIAN_POINT('Ctrl Pts',(-9.89367995200006,15.2,4.87686707399998));
#249737=CARTESIAN_POINT('Ctrl Pts',(-9.89367995200006,11.6,4.87686707399998));
#249738=CARTESIAN_POINT('Ctrl Pts',(-9.89153976200006,15.2,4.87460027999998));
#249739=CARTESIAN_POINT('Ctrl Pts',(-9.89153976200006,11.6,4.87460027999998));
#249740=CARTESIAN_POINT('Ctrl Pts',(-9.88940133500006,15.2,4.87233902899998));
#249741=CARTESIAN_POINT('Ctrl Pts',(-9.88940133500006,11.6,4.87233902899998));
#249742=CARTESIAN_POINT('Ctrl Pts',(-9.88726468300005,15.2,4.87008332399999));
#249743=CARTESIAN_POINT('Ctrl Pts',(-9.88726468300005,11.6,4.87008332399998));
#249744=CARTESIAN_POINT('Ctrl Pts',(-9.88512981800006,15.2,4.86783316599999));
#249745=CARTESIAN_POINT('Ctrl Pts',(-9.88512981800006,11.6,4.86783316599999));
#249746=CARTESIAN_POINT('Ctrl Pts',(-9.88299675000006,15.2,4.86558855699998));
#249747=CARTESIAN_POINT('Ctrl Pts',(-9.88299675000006,11.6,4.86558855699998));
#249748=CARTESIAN_POINT('Ctrl Pts',(-9.88086549300006,15.2,4.86334949699998));
#249749=CARTESIAN_POINT('Ctrl Pts',(-9.88086549300006,11.6,4.86334949699998));
#249750=CARTESIAN_POINT('Ctrl Pts',(-9.87873605800005,15.2,4.86111598899999));
#249751=CARTESIAN_POINT('Ctrl Pts',(-9.87873605800005,11.6,4.86111598899999));
#249752=CARTESIAN_POINT('Ctrl Pts',(-9.87660845500006,15.2,4.85888803499999));
#249753=CARTESIAN_POINT('Ctrl Pts',(-9.87660845500006,11.6,4.85888803499999));
#249754=CARTESIAN_POINT('Ctrl Pts',(-9.87448269700005,15.2,4.85666563499999));
#249755=CARTESIAN_POINT('Ctrl Pts',(-9.87448269700005,11.6,4.85666563499999));
#249756=CARTESIAN_POINT('Ctrl Pts',(-9.87235879600006,15.2,4.85444879299998));
#249757=CARTESIAN_POINT('Ctrl Pts',(-9.87235879600006,11.6,4.85444879299998));
#249758=CARTESIAN_POINT('Ctrl Pts',(-9.87023676300005,15.2,4.85223750899999));
#249759=CARTESIAN_POINT('Ctrl Pts',(-9.87023676300005,11.6,4.85223750899998));
#249760=CARTESIAN_POINT('Ctrl Pts',(-9.86811661000005,15.2,4.85003178499999));
#249761=CARTESIAN_POINT('Ctrl Pts',(-9.86811661000005,11.6,4.85003178499999));
#249762=CARTESIAN_POINT('Ctrl Pts',(-9.86599834900005,15.2,4.84783162199999));
#249763=CARTESIAN_POINT('Ctrl Pts',(-9.86599834900005,11.6,4.84783162199999));
#249764=CARTESIAN_POINT('Ctrl Pts',(-9.86388199200006,15.2,4.84563702199999));
#249765=CARTESIAN_POINT('Ctrl Pts',(-9.86388199200006,11.6,4.84563702199999));
#249766=CARTESIAN_POINT('Ctrl Pts',(-9.86176755000006,15.2,4.84344798699999));
#249767=CARTESIAN_POINT('Ctrl Pts',(-9.86176755000006,11.6,4.84344798699999));
#249768=CARTESIAN_POINT('Ctrl Pts',(-9.85965503600006,15.2,4.84126451799998));
#249769=CARTESIAN_POINT('Ctrl Pts',(-9.85965503600006,11.6,4.84126451799998));
#249770=CARTESIAN_POINT('Ctrl Pts',(-9.85754446100006,15.2,4.83908661799998));
#249771=CARTESIAN_POINT('Ctrl Pts',(-9.85754446100006,11.6,4.83908661799998));
#249772=CARTESIAN_POINT('Ctrl Pts',(-9.85543583700006,15.2,4.83691428599998));
#249773=CARTESIAN_POINT('Ctrl Pts',(-9.85543583700006,11.6,4.83691428599998));
#249774=CARTESIAN_POINT('Ctrl Pts',(-9.85332917700006,15.2,4.83474752599999));
#249775=CARTESIAN_POINT('Ctrl Pts',(-9.85332917700006,11.6,4.83474752599999));
#249776=CARTESIAN_POINT('Ctrl Pts',(-9.85122449200006,15.2,4.83258633799998));
#249777=CARTESIAN_POINT('Ctrl Pts',(-9.85122449200006,11.6,4.83258633799998));
#249778=CARTESIAN_POINT('Ctrl Pts',(-9.84912179500006,15.2,4.83043072399998));
#249779=CARTESIAN_POINT('Ctrl Pts',(-9.84912179500006,11.6,4.83043072399998));
#249780=CARTESIAN_POINT('Ctrl Pts',(-9.84702109500006,15.2,4.82828068499998));
#249781=CARTESIAN_POINT('Ctrl Pts',(-9.84702109500006,11.6,4.82828068499998));
#249782=CARTESIAN_POINT('Ctrl Pts',(-9.84492240900006,15.2,4.82613622399998));
#249783=CARTESIAN_POINT('Ctrl Pts',(-9.84492240900006,11.6,4.82613622399998));
#249784=CARTESIAN_POINT('Ctrl Pts',(-9.84282574500006,15.2,4.82399734199999));
#249785=CARTESIAN_POINT('Ctrl Pts',(-9.84282574500006,11.6,4.82399734199999));
#249786=CARTESIAN_POINT('Ctrl Pts',(-9.84073111800006,15.2,4.82186403999999));
#249787=CARTESIAN_POINT('Ctrl Pts',(-9.84073111800006,11.6,4.82186403999999));
#249788=CARTESIAN_POINT('Ctrl Pts',(-9.83863853800005,15.2,4.81973631899999));
#249789=CARTESIAN_POINT('Ctrl Pts',(-9.83863853800005,11.6,4.81973631899999));
#249790=CARTESIAN_POINT('Ctrl Pts',(-9.83654801900006,15.2,4.81761418299998));
#249791=CARTESIAN_POINT('Ctrl Pts',(-9.83654801900006,11.6,4.81761418299998));
#249792=CARTESIAN_POINT('Ctrl Pts',(-9.83445957100006,15.2,4.81549763099999));
#249793=CARTESIAN_POINT('Ctrl Pts',(-9.83445957100006,11.6,4.81549763099998));
#249794=CARTESIAN_POINT('Ctrl Pts',(-9.83237320800006,15.2,4.81338666499998));
#249795=CARTESIAN_POINT('Ctrl Pts',(-9.83237320800006,11.6,4.81338666499998));
#249796=CARTESIAN_POINT('Ctrl Pts',(-9.83028894200006,15.2,4.81128128699999));
#249797=CARTESIAN_POINT('Ctrl Pts',(-9.83028894200006,11.6,4.81128128699999));
#249798=CARTESIAN_POINT('Ctrl Pts',(-9.82820678500006,15.2,4.80918149899999));
#249799=CARTESIAN_POINT('Ctrl Pts',(-9.82820678500006,11.6,4.80918149899999));
#249800=CARTESIAN_POINT('Ctrl Pts',(-9.82612674900006,15.2,4.80708729999999));
#249801=CARTESIAN_POINT('Ctrl Pts',(-9.82612674900006,11.6,4.80708729999998));
#249802=CARTESIAN_POINT('Ctrl Pts',(-9.82404884900006,15.2,4.80499869499998));
#249803=CARTESIAN_POINT('Ctrl Pts',(-9.82404884900006,11.6,4.80499869499998));
#249804=CARTESIAN_POINT('Ctrl Pts',(-9.82197309300006,15.2,4.80291568299998));
#249805=CARTESIAN_POINT('Ctrl Pts',(-9.82197309300006,11.6,4.80291568299998));
#249806=CARTESIAN_POINT('Ctrl Pts',(-9.81989949700005,15.2,4.80083826599999));
#249807=CARTESIAN_POINT('Ctrl Pts',(-9.81989949700005,11.6,4.80083826599999));
#249808=CARTESIAN_POINT('Ctrl Pts',(-9.81782807000006,15.2,4.79876644699999));
#249809=CARTESIAN_POINT('Ctrl Pts',(-9.81782807000006,11.6,4.79876644699999));
#249810=CARTESIAN_POINT('Ctrl Pts',(-9.81575883000006,15.2,4.79670022499998));
#249811=CARTESIAN_POINT('Ctrl Pts',(-9.81575883000006,11.6,4.79670022499998));
#249812=CARTESIAN_POINT('Ctrl Pts',(-9.81369178300006,15.2,4.79463960299999));
#249813=CARTESIAN_POINT('Ctrl Pts',(-9.81369178300006,11.6,4.79463960299999));
#249814=CARTESIAN_POINT('Ctrl Pts',(-9.81162694700006,15.2,4.79258458199999));
#249815=CARTESIAN_POINT('Ctrl Pts',(-9.81162694700006,11.6,4.79258458199998));
#249816=CARTESIAN_POINT('Ctrl Pts',(-9.80956433100006,15.2,4.79053516399999));
#249817=CARTESIAN_POINT('Ctrl Pts',(-9.80956433100006,11.6,4.79053516399999));
#249818=CARTESIAN_POINT('Ctrl Pts',(-9.80750395000006,15.2,4.78849134999999));
#249819=CARTESIAN_POINT('Ctrl Pts',(-9.80750395000006,11.6,4.78849134999999));
#249820=CARTESIAN_POINT('Ctrl Pts',(-9.80544581400006,15.2,4.78645313999999));
#249821=CARTESIAN_POINT('Ctrl Pts',(-9.80544581400006,11.6,4.78645313999999));
#249822=CARTESIAN_POINT('Ctrl Pts',(-9.80338993900006,15.2,4.78442053799998));
#249823=CARTESIAN_POINT('Ctrl Pts',(-9.80338993900006,11.6,4.78442053799998));
#249824=CARTESIAN_POINT('Ctrl Pts',(-9.80133633400006,15.2,4.78239354399999));
#249825=CARTESIAN_POINT('Ctrl Pts',(-9.80133633400006,11.6,4.78239354399999));
#249826=CARTESIAN_POINT('Ctrl Pts',(-9.79928501600006,15.2,4.78037215999999));
#249827=CARTESIAN_POINT('Ctrl Pts',(-9.79928501600006,11.6,4.78037215999999));
#249828=CARTESIAN_POINT('Ctrl Pts',(-9.79723599400005,15.2,4.77835638599998));
#249829=CARTESIAN_POINT('Ctrl Pts',(-9.79723599400005,11.6,4.77835638599998));
#249830=CARTESIAN_POINT('Ctrl Pts',(-9.79518928200006,15.2,4.77634622499998));
#249831=CARTESIAN_POINT('Ctrl Pts',(-9.79518928200006,11.6,4.77634622499998));
#249832=CARTESIAN_POINT('Ctrl Pts',(-9.79314489400006,15.2,4.77434167799998));
#249833=CARTESIAN_POINT('Ctrl Pts',(-9.79314489400006,11.6,4.77434167799998));
#249834=CARTESIAN_POINT('Ctrl Pts',(-9.79110284100006,15.2,4.77234274599999));
#249835=CARTESIAN_POINT('Ctrl Pts',(-9.79110284100006,11.6,4.77234274599999));
#249836=CARTESIAN_POINT('Ctrl Pts',(-9.78906313700006,15.2,4.77034943099999));
#249837=CARTESIAN_POINT('Ctrl Pts',(-9.78906313700006,11.6,4.77034943099999));
#249838=CARTESIAN_POINT('Ctrl Pts',(-9.78702579600006,15.2,4.76836173399998));
#249839=CARTESIAN_POINT('Ctrl Pts',(-9.78702579600006,11.6,4.76836173399998));
#249840=CARTESIAN_POINT('Ctrl Pts',(-9.78499082900005,15.2,4.76637965599998));
#249841=CARTESIAN_POINT('Ctrl Pts',(-9.78499082900005,11.6,4.76637965599998));
#249842=CARTESIAN_POINT('Ctrl Pts',(-9.78295824900006,15.2,4.76440319899999));
#249843=CARTESIAN_POINT('Ctrl Pts',(-9.78295824900006,11.6,4.76440319899999));
#249844=CARTESIAN_POINT('Ctrl Pts',(-9.78092807100006,15.2,4.76243236299998));
#249845=CARTESIAN_POINT('Ctrl Pts',(-9.78092807100006,11.6,4.76243236299998));
#249846=CARTESIAN_POINT('Ctrl Pts',(-9.77890030600006,15.2,4.76046715199999));
#249847=CARTESIAN_POINT('Ctrl Pts',(-9.77890030600006,11.6,4.76046715199998));
#249848=CARTESIAN_POINT('Ctrl Pts',(-9.77687496800005,15.2,4.75850756499998));
#249849=CARTESIAN_POINT('Ctrl Pts',(-9.77687496800005,11.6,4.75850756499998));
#249850=CARTESIAN_POINT('Ctrl Pts',(-9.77485207000005,15.2,4.75655360399998));
#249851=CARTESIAN_POINT('Ctrl Pts',(-9.77485207000005,11.6,4.75655360399998));
#249852=CARTESIAN_POINT('Ctrl Pts',(-9.77283162500006,15.2,4.75460526999999));
#249853=CARTESIAN_POINT('Ctrl Pts',(-9.77283162500006,11.6,4.75460526999999));
#249854=CARTESIAN_POINT('Ctrl Pts',(-9.77081364700006,15.2,4.75266256599999));
#249855=CARTESIAN_POINT('Ctrl Pts',(-9.77081364700006,11.6,4.75266256599998));
#249856=CARTESIAN_POINT('Ctrl Pts',(-9.76879814800006,15.2,4.75072549099998));
#249857=CARTESIAN_POINT('Ctrl Pts',(-9.76879814800006,11.6,4.75072549099998));
#249858=CARTESIAN_POINT('Ctrl Pts',(-9.76678514200006,15.2,4.74879404799999));
#249859=CARTESIAN_POINT('Ctrl Pts',(-9.76678514200006,11.6,4.74879404799999));
#249860=CARTESIAN_POINT('Ctrl Pts',(-9.76477464200006,15.2,4.74686823699999));
#249861=CARTESIAN_POINT('Ctrl Pts',(-9.76477464200006,11.6,4.74686823699999));
#249862=CARTESIAN_POINT('Ctrl Pts',(-9.76276666200006,15.2,4.74494805999999));
#249863=CARTESIAN_POINT('Ctrl Pts',(-9.76276666200006,11.6,4.74494805999999));
#249864=CARTESIAN_POINT('Ctrl Pts',(-9.76076121400006,15.2,4.74303351799998));
#249865=CARTESIAN_POINT('Ctrl Pts',(-9.76076121400006,11.6,4.74303351799998));
#249866=CARTESIAN_POINT('Ctrl Pts',(-9.75875831300005,15.2,4.74112461299999));
#249867=CARTESIAN_POINT('Ctrl Pts',(-9.75875831300005,11.6,4.74112461299998));
#249868=CARTESIAN_POINT('Ctrl Pts',(-9.75675797100006,15.2,4.73922134599999));
#249869=CARTESIAN_POINT('Ctrl Pts',(-9.75675797100006,11.6,4.73922134599999));
#249870=CARTESIAN_POINT('Ctrl Pts',(-9.75476020300006,15.2,4.73732371799999));
#249871=CARTESIAN_POINT('Ctrl Pts',(-9.75476020300006,11.6,4.73732371799999));
#249872=CARTESIAN_POINT('Ctrl Pts',(-9.75276502000006,15.2,4.73543172899999));
#249873=CARTESIAN_POINT('Ctrl Pts',(-9.75276502000006,11.6,4.73543172899998));
#249874=CARTESIAN_POINT('Ctrl Pts',(-9.75077243800006,15.2,4.73354538299999));
#249875=CARTESIAN_POINT('Ctrl Pts',(-9.75077243800006,11.6,4.73354538299999));
#249876=CARTESIAN_POINT('Ctrl Pts',(-9.74878247000006,15.2,4.73166467999998));
#249877=CARTESIAN_POINT('Ctrl Pts',(-9.74878247000006,11.6,4.73166467999998));
#249878=CARTESIAN_POINT('Ctrl Pts',(-9.74679512900006,15.2,4.72978961999999));
#249879=CARTESIAN_POINT('Ctrl Pts',(-9.74679512900006,11.6,4.72978961999999));
#249880=CARTESIAN_POINT('Ctrl Pts',(-9.74481042800006,15.2,4.72792020599999));
#249881=CARTESIAN_POINT('Ctrl Pts',(-9.74481042800006,11.6,4.72792020599999));
#249882=CARTESIAN_POINT('Ctrl Pts',(-9.74282838300006,15.2,4.72605643799999));
#249883=CARTESIAN_POINT('Ctrl Pts',(-9.74282838300006,11.6,4.72605643799999));
#249884=CARTESIAN_POINT('Ctrl Pts',(-9.74084900600005,15.2,4.72419831799999));
#249885=CARTESIAN_POINT('Ctrl Pts',(-9.74084900600005,11.6,4.72419831799998));
#249886=CARTESIAN_POINT('Ctrl Pts',(-9.73887231000005,15.2,4.72234584699999));
#249887=CARTESIAN_POINT('Ctrl Pts',(-9.73887231000005,11.6,4.72234584699999));
#249888=CARTESIAN_POINT('Ctrl Pts',(-9.73689831000006,15.2,4.72049902699998));
#249889=CARTESIAN_POINT('Ctrl Pts',(-9.73689831000006,11.6,4.72049902699998));
#249890=CARTESIAN_POINT('Ctrl Pts',(-9.73492702000006,15.2,4.71865785699999));
#249891=CARTESIAN_POINT('Ctrl Pts',(-9.73492702000006,11.6,4.71865785699999));
#249892=CARTESIAN_POINT('Ctrl Pts',(-9.73295845400006,15.2,4.71682233999999));
#249893=CARTESIAN_POINT('Ctrl Pts',(-9.73295845400006,11.6,4.71682233999999));
#249894=CARTESIAN_POINT('Ctrl Pts',(-9.73099262500006,15.2,4.71499247599999));
#249895=CARTESIAN_POINT('Ctrl Pts',(-9.73099262500006,11.6,4.71499247599999));
#249896=CARTESIAN_POINT('Ctrl Pts',(-9.72902954700006,15.2,4.71316826799999));
#249897=CARTESIAN_POINT('Ctrl Pts',(-9.72902954700006,11.6,4.71316826799998));
#249898=CARTESIAN_POINT('Ctrl Pts',(-9.72706923400006,15.2,4.71134971599999));
#249899=CARTESIAN_POINT('Ctrl Pts',(-9.72706923400006,11.6,4.71134971599999));
#249900=CARTESIAN_POINT('Ctrl Pts',(-9.72511170000006,15.2,4.70953682099999));
#249901=CARTESIAN_POINT('Ctrl Pts',(-9.72511170000006,11.6,4.70953682099999));
#249902=CARTESIAN_POINT('Ctrl Pts',(-9.72315695900006,15.2,4.70772958399999));
#249903=CARTESIAN_POINT('Ctrl Pts',(-9.72315695900006,11.6,4.70772958399999));
#249904=CARTESIAN_POINT('Ctrl Pts',(-9.72120502600006,15.2,4.70592800699999));
#249905=CARTESIAN_POINT('Ctrl Pts',(-9.72120502600006,11.6,4.70592800699999));
#249906=CARTESIAN_POINT('Ctrl Pts',(-9.71925591500005,15.2,4.70413208999998));
#249907=CARTESIAN_POINT('Ctrl Pts',(-9.71925591500005,11.6,4.70413208999998));
#249908=CARTESIAN_POINT('Ctrl Pts',(-9.71730963800006,15.2,4.70234183599998));
#249909=CARTESIAN_POINT('Ctrl Pts',(-9.71730963800006,11.6,4.70234183599998));
#249910=CARTESIAN_POINT('Ctrl Pts',(-9.71536621200006,15.2,4.70055724399998));
#249911=CARTESIAN_POINT('Ctrl Pts',(-9.71536621200006,11.6,4.70055724399998));
#249912=CARTESIAN_POINT('Ctrl Pts',(-9.71342564900005,15.2,4.69877831599998));
#249913=CARTESIAN_POINT('Ctrl Pts',(-9.71342564900005,11.6,4.69877831599998));
#249914=CARTESIAN_POINT('Ctrl Pts',(-9.71148796400006,15.2,4.69700505399998));
#249915=CARTESIAN_POINT('Ctrl Pts',(-9.71148796400006,11.6,4.69700505399998));
#249916=CARTESIAN_POINT('Ctrl Pts',(-9.70955317200006,15.2,4.69523745799999));
#249917=CARTESIAN_POINT('Ctrl Pts',(-9.70955317200006,11.6,4.69523745799999));
#249918=CARTESIAN_POINT('Ctrl Pts',(-9.70762128700006,15.2,4.69347552899999));
#249919=CARTESIAN_POINT('Ctrl Pts',(-9.70762128700006,11.6,4.69347552899999));
#249920=CARTESIAN_POINT('Ctrl Pts',(-9.70569232300006,15.2,4.69171926799999));
#249921=CARTESIAN_POINT('Ctrl Pts',(-9.70569232300006,11.6,4.69171926799999));
#249922=CARTESIAN_POINT('Ctrl Pts',(-9.70376629500005,15.2,4.68996867699998));
#249923=CARTESIAN_POINT('Ctrl Pts',(-9.70376629500005,11.6,4.68996867699998));
#249924=CARTESIAN_POINT('Ctrl Pts',(-9.70184321600006,15.2,4.68822375699999));
#249925=CARTESIAN_POINT('Ctrl Pts',(-9.70184321600006,11.6,4.68822375699998));
#249926=CARTESIAN_POINT('Ctrl Pts',(-9.69992310200006,15.2,4.68648450799999));
#249927=CARTESIAN_POINT('Ctrl Pts',(-9.69992310200006,11.6,4.68648450799999));
#249928=CARTESIAN_POINT('Ctrl Pts',(-9.69800596700006,15.2,4.68475093299999));
#249929=CARTESIAN_POINT('Ctrl Pts',(-9.69800596700006,11.6,4.68475093299999));
#249930=CARTESIAN_POINT('Ctrl Pts',(-9.69609182600006,15.2,4.68302302999999));
#249931=CARTESIAN_POINT('Ctrl Pts',(-9.69609182600006,11.6,4.68302302999999));
#249932=CARTESIAN_POINT('Ctrl Pts',(-9.69418069300006,15.2,4.68130080299999));
#249933=CARTESIAN_POINT('Ctrl Pts',(-9.69418069300006,11.6,4.68130080299998));
#249934=CARTESIAN_POINT('Ctrl Pts',(-9.69227258300006,15.2,4.67958425199999));
#249935=CARTESIAN_POINT('Ctrl Pts',(-9.69227258300006,11.6,4.67958425199999));
#249936=CARTESIAN_POINT('Ctrl Pts',(-9.69036751000005,15.2,4.67787337699999));
#249937=CARTESIAN_POINT('Ctrl Pts',(-9.69036751000005,11.6,4.67787337699998));
#249938=CARTESIAN_POINT('Ctrl Pts',(-9.68846549000006,15.2,4.67616818099999));
#249939=CARTESIAN_POINT('Ctrl Pts',(-9.68846549000006,11.6,4.67616818099999));
#249940=CARTESIAN_POINT('Ctrl Pts',(-9.68656653600006,15.2,4.67446866399998));
#249941=CARTESIAN_POINT('Ctrl Pts',(-9.68656653600006,11.6,4.67446866399998));
#249942=CARTESIAN_POINT('Ctrl Pts',(-9.68467066400006,15.2,4.67277482499998));
#249943=CARTESIAN_POINT('Ctrl Pts',(-9.68467066400006,11.6,4.67277482499998));
#249944=CARTESIAN_POINT('Ctrl Pts',(-9.68277788900006,15.2,4.67108666899998));
#249945=CARTESIAN_POINT('Ctrl Pts',(-9.68277788900006,11.6,4.67108666899998));
#249946=CARTESIAN_POINT('Ctrl Pts',(-9.68088822600006,15.2,4.66940419399998));
#249947=CARTESIAN_POINT('Ctrl Pts',(-9.68088822600006,11.6,4.66940419399998));
#249948=CARTESIAN_POINT('Ctrl Pts',(-9.67900168900006,15.2,4.66772740199998));
#249949=CARTESIAN_POINT('Ctrl Pts',(-9.67900168900006,11.6,4.66772740199998));
#249950=CARTESIAN_POINT('Ctrl Pts',(-9.67711829400006,15.2,4.66605629399999));
#249951=CARTESIAN_POINT('Ctrl Pts',(-9.67711829400006,11.6,4.66605629399999));
#249952=CARTESIAN_POINT('Ctrl Pts',(-9.67523805500005,15.2,4.66439086999999));
#249953=CARTESIAN_POINT('Ctrl Pts',(-9.67523805500005,11.6,4.66439086999998));
#249954=CARTESIAN_POINT('Ctrl Pts',(-9.67336098800006,15.2,4.66273113399998));
#249955=CARTESIAN_POINT('Ctrl Pts',(-9.67336098800006,11.6,4.66273113399998));
#249956=CARTESIAN_POINT('Ctrl Pts',(-9.67148710700006,15.2,4.66107708199999));
#249957=CARTESIAN_POINT('Ctrl Pts',(-9.67148710700006,11.6,4.66107708199999));
#249958=CARTESIAN_POINT('Ctrl Pts',(-9.66961642800005,15.2,4.65942871899999));
#249959=CARTESIAN_POINT('Ctrl Pts',(-9.66961642800005,11.6,4.65942871899998));
#249960=CARTESIAN_POINT('Ctrl Pts',(-9.66774896600005,15.2,4.65778604499998));
#249961=CARTESIAN_POINT('Ctrl Pts',(-9.66774896600005,11.6,4.65778604499998));
#249962=CARTESIAN_POINT('Ctrl Pts',(-9.66588473600006,15.2,4.65614906099999));
#249963=CARTESIAN_POINT('Ctrl Pts',(-9.66588473600006,11.6,4.65614906099999));
#249964=CARTESIAN_POINT('Ctrl Pts',(-9.66402375400006,15.2,4.65451776599998));
#249965=CARTESIAN_POINT('Ctrl Pts',(-9.66402375400006,11.6,4.65451776599998));
#249966=CARTESIAN_POINT('Ctrl Pts',(-9.66216603400006,15.2,4.65289216299999));
#249967=CARTESIAN_POINT('Ctrl Pts',(-9.66216603400006,11.6,4.65289216299999));
#249968=CARTESIAN_POINT('Ctrl Pts',(-9.66031159300006,15.2,4.65127225199998));
#249969=CARTESIAN_POINT('Ctrl Pts',(-9.66031159300006,11.6,4.65127225199998));
#249970=CARTESIAN_POINT('Ctrl Pts',(-9.65846044500006,15.2,4.64965803399998));
#249971=CARTESIAN_POINT('Ctrl Pts',(-9.65846044500006,11.6,4.64965803399998));
#249972=CARTESIAN_POINT('Ctrl Pts',(-9.65661260600006,15.2,4.64804950999999));
#249973=CARTESIAN_POINT('Ctrl Pts',(-9.65661260600006,11.6,4.64804950999999));
#249974=CARTESIAN_POINT('Ctrl Pts',(-9.65476809200006,15.2,4.64644668199998));
#249975=CARTESIAN_POINT('Ctrl Pts',(-9.65476809200006,11.6,4.64644668199998));
#249976=CARTESIAN_POINT('Ctrl Pts',(-9.65292691700006,15.2,4.64484954899999));
#249977=CARTESIAN_POINT('Ctrl Pts',(-9.65292691700006,11.6,4.64484954899999));
#249978=CARTESIAN_POINT('Ctrl Pts',(-9.65108909700006,15.2,4.64325811299998));
#249979=CARTESIAN_POINT('Ctrl Pts',(-9.65108909700006,11.6,4.64325811299998));
#249980=CARTESIAN_POINT('Ctrl Pts',(-9.64925465000006,15.2,4.64167237399998));
#249981=CARTESIAN_POINT('Ctrl Pts',(-9.64925465000006,11.6,4.64167237399998));
#249982=CARTESIAN_POINT('Ctrl Pts',(-9.64742358900006,15.2,4.64009233399998));
#249983=CARTESIAN_POINT('Ctrl Pts',(-9.64742358900006,11.6,4.64009233399998));
#249984=CARTESIAN_POINT('Ctrl Pts',(-9.64559593000006,15.2,4.63851799299999));
#249985=CARTESIAN_POINT('Ctrl Pts',(-9.64559593000006,11.6,4.63851799299999));
#249986=CARTESIAN_POINT('Ctrl Pts',(-9.64377169000005,15.2,4.63694935199998));
#249987=CARTESIAN_POINT('Ctrl Pts',(-9.64377169000005,11.6,4.63694935199998));
#249988=CARTESIAN_POINT('Ctrl Pts',(-9.64195088400006,15.2,4.63538641099999));
#249989=CARTESIAN_POINT('Ctrl Pts',(-9.64195088400006,11.6,4.63538641099999));
#249990=CARTESIAN_POINT('Ctrl Pts',(-9.64013352800006,15.2,4.63382917199999));
#249991=CARTESIAN_POINT('Ctrl Pts',(-9.64013352800006,11.6,4.63382917199999));
#249992=CARTESIAN_POINT('Ctrl Pts',(-9.63831963700006,15.2,4.63227763599999));
#249993=CARTESIAN_POINT('Ctrl Pts',(-9.63831963700006,11.6,4.63227763599999));
#249994=CARTESIAN_POINT('Ctrl Pts',(-9.63650922900005,15.2,4.63073180299999));
#249995=CARTESIAN_POINT('Ctrl Pts',(-9.63650922900005,11.6,4.63073180299998));
#249996=CARTESIAN_POINT('Ctrl Pts',(-9.63470231800006,15.2,4.62919167299999));
#249997=CARTESIAN_POINT('Ctrl Pts',(-9.63470231800006,11.6,4.62919167299999));
#249998=CARTESIAN_POINT('Ctrl Pts',(-9.63289892100006,15.2,4.62765724899998));
#249999=CARTESIAN_POINT('Ctrl Pts',(-9.63289892100006,11.6,4.62765724899998));
#250000=CARTESIAN_POINT('Ctrl Pts',(-9.63109905400006,15.2,4.62612852999998));
#250001=CARTESIAN_POINT('Ctrl Pts',(-9.63109905400006,11.6,4.62612852999998));
#250002=CARTESIAN_POINT('Ctrl Pts',(-9.62930273200006,15.2,4.62460551699999));
#250003=CARTESIAN_POINT('Ctrl Pts',(-9.62930273200006,11.6,4.62460551699999));
#250004=CARTESIAN_POINT('Ctrl Pts',(-9.62750997400006,15.2,4.62308821099998));
#250005=CARTESIAN_POINT('Ctrl Pts',(-9.62750997400006,11.6,4.62308821099998));
#250006=CARTESIAN_POINT('Ctrl Pts',(-9.62572079300006,15.2,4.62157661399999));
#250007=CARTESIAN_POINT('Ctrl Pts',(-9.62572079300006,11.6,4.62157661399999));
#250008=CARTESIAN_POINT('Ctrl Pts',(-9.62393520600006,15.2,4.62007072399999));
#250009=CARTESIAN_POINT('Ctrl Pts',(-9.62393520600006,11.6,4.62007072399999));
#250010=CARTESIAN_POINT('Ctrl Pts',(-9.62215323100006,15.2,4.61857054399999));
#250011=CARTESIAN_POINT('Ctrl Pts',(-9.62215323100006,11.6,4.61857054399999));
#250012=CARTESIAN_POINT('Ctrl Pts',(-9.62037488400006,15.2,4.61707607299999));
#250013=CARTESIAN_POINT('Ctrl Pts',(-9.62037488400006,11.6,4.61707607299999));
#250014=CARTESIAN_POINT('Ctrl Pts',(-9.61860017900005,15.2,4.61558731399998));
#250015=CARTESIAN_POINT('Ctrl Pts',(-9.61860017900005,11.6,4.61558731399998));
#250016=CARTESIAN_POINT('Ctrl Pts',(-9.61682913600006,15.2,4.61410426599999));
#250017=CARTESIAN_POINT('Ctrl Pts',(-9.61682913600006,11.6,4.61410426599999));
#250018=CARTESIAN_POINT('Ctrl Pts',(-9.61506176900006,15.2,4.61262692999998));
#250019=CARTESIAN_POINT('Ctrl Pts',(-9.61506176900006,11.6,4.61262692999998));
#250020=CARTESIAN_POINT('Ctrl Pts',(-9.61329809500005,15.2,4.61115530599999));
#250021=CARTESIAN_POINT('Ctrl Pts',(-9.61329809500005,11.6,4.61115530599999));
#250022=CARTESIAN_POINT('Ctrl Pts',(-9.61153813200006,15.2,4.60968939499999));
#250023=CARTESIAN_POINT('Ctrl Pts',(-9.61153813200006,11.6,4.60968939499998));
#250024=CARTESIAN_POINT('Ctrl Pts',(-9.60978189400005,15.2,4.60822919899999));
#250025=CARTESIAN_POINT('Ctrl Pts',(-9.60978189400005,11.6,4.60822919899999));
#250026=CARTESIAN_POINT('Ctrl Pts',(-9.60802940000006,15.2,4.60677471699999));
#250027=CARTESIAN_POINT('Ctrl Pts',(-9.60802940000006,11.6,4.60677471699999));
#250028=CARTESIAN_POINT('Ctrl Pts',(-9.60628066600006,15.2,4.60532595099998));
#250029=CARTESIAN_POINT('Ctrl Pts',(-9.60628066600006,11.6,4.60532595099998));
#250030=CARTESIAN_POINT('Ctrl Pts',(-9.60453570800006,15.2,4.60388289999998));
#250031=CARTESIAN_POINT('Ctrl Pts',(-9.60453570800006,11.6,4.60388289999998));
#250032=CARTESIAN_POINT('Ctrl Pts',(-9.60279454500006,15.2,4.60244556599999));
#250033=CARTESIAN_POINT('Ctrl Pts',(-9.60279454500006,11.6,4.60244556599999));
#250034=CARTESIAN_POINT('Ctrl Pts',(-9.60105719300006,15.2,4.60101394899999));
#250035=CARTESIAN_POINT('Ctrl Pts',(-9.60105719300006,11.6,4.60101394899999));
#250036=CARTESIAN_POINT('Ctrl Pts',(-9.59932366800006,15.2,4.59958804999999));
#250037=CARTESIAN_POINT('Ctrl Pts',(-9.59932366800006,11.6,4.59958804999999));
#250038=CARTESIAN_POINT('Ctrl Pts',(-9.59759398800006,15.2,4.59816786899999));
#250039=CARTESIAN_POINT('Ctrl Pts',(-9.59759398800006,11.6,4.59816786899999));
#250040=CARTESIAN_POINT('Ctrl Pts',(-9.59586816900006,15.2,4.59675340699999));
#250041=CARTESIAN_POINT('Ctrl Pts',(-9.59586816900006,11.6,4.59675340699999));
#250042=CARTESIAN_POINT('Ctrl Pts',(-9.59414622900006,15.2,4.59534466299999));
#250043=CARTESIAN_POINT('Ctrl Pts',(-9.59414622900006,11.6,4.59534466299999));
#250044=CARTESIAN_POINT('Ctrl Pts',(-9.59242818600006,15.2,4.59394164099999));
#250045=CARTESIAN_POINT('Ctrl Pts',(-9.59242818600006,11.6,4.59394164099999));
#250046=CARTESIAN_POINT('Ctrl Pts',(-9.59071405500006,15.2,4.59254433899999));
#250047=CARTESIAN_POINT('Ctrl Pts',(-9.59071405500006,11.6,4.59254433899999));
#250048=CARTESIAN_POINT('Ctrl Pts',(-9.58900385500005,15.2,4.59115275799999));
#250049=CARTESIAN_POINT('Ctrl Pts',(-9.58900385500005,11.6,4.59115275799998));
#250050=CARTESIAN_POINT('Ctrl Pts',(-9.58729760300006,15.2,4.58976689899998));
#250051=CARTESIAN_POINT('Ctrl Pts',(-9.58729760300006,11.6,4.58976689899998));
#250052=CARTESIAN_POINT('Ctrl Pts',(-9.58559531500006,15.2,4.58838676099998));
#250053=CARTESIAN_POINT('Ctrl Pts',(-9.58559531500006,11.6,4.58838676099998));
#250054=CARTESIAN_POINT('Ctrl Pts',(-9.58389701200005,15.2,4.58701234699999));
#250055=CARTESIAN_POINT('Ctrl Pts',(-9.58389701200005,11.6,4.58701234699998));
#250056=CARTESIAN_POINT('Ctrl Pts',(-9.58220270800006,15.2,4.58564365599998));
#250057=CARTESIAN_POINT('Ctrl Pts',(-9.58220270800006,11.6,4.58564365599998));
#250058=CARTESIAN_POINT('Ctrl Pts',(-9.58051242300006,15.2,4.58428068699998));
#250059=CARTESIAN_POINT('Ctrl Pts',(-9.58051242300006,11.6,4.58428068699998));
#250060=CARTESIAN_POINT('Ctrl Pts',(-9.57882617200006,15.2,4.58292344399998));
#250061=CARTESIAN_POINT('Ctrl Pts',(-9.57882617200006,11.6,4.58292344399998));
#250062=CARTESIAN_POINT('Ctrl Pts',(-9.57714397400006,15.2,4.58157192499999));
#250063=CARTESIAN_POINT('Ctrl Pts',(-9.57714397400006,11.6,4.58157192499998));
#250064=CARTESIAN_POINT('Ctrl Pts',(-9.57546584800006,15.2,4.58022613099998));
#250065=CARTESIAN_POINT('Ctrl Pts',(-9.57546584800006,11.6,4.58022613099998));
#250066=CARTESIAN_POINT('Ctrl Pts',(-9.57379181000006,15.2,4.57888606299999));
#250067=CARTESIAN_POINT('Ctrl Pts',(-9.57379181000006,11.6,4.57888606299999));
#250068=CARTESIAN_POINT('Ctrl Pts',(-9.57212187800006,15.2,4.57755171999998));
#250069=CARTESIAN_POINT('Ctrl Pts',(-9.57212187800006,11.6,4.57755171999998));
#250070=CARTESIAN_POINT('Ctrl Pts',(-9.57045607000006,15.2,4.57622310399999));
#250071=CARTESIAN_POINT('Ctrl Pts',(-9.57045607000006,11.6,4.57622310399999));
#250072=CARTESIAN_POINT('Ctrl Pts',(-9.56879440600006,15.2,4.57490021399998));
#250073=CARTESIAN_POINT('Ctrl Pts',(-9.56879440600006,11.6,4.57490021399998));
#250074=CARTESIAN_POINT('Ctrl Pts',(-9.56713690100005,15.2,4.57358305199998));
#250075=CARTESIAN_POINT('Ctrl Pts',(-9.56713690100005,11.6,4.57358305199998));
#250076=CARTESIAN_POINT('Ctrl Pts',(-9.56548357500006,15.2,4.57227161699999));
#250077=CARTESIAN_POINT('Ctrl Pts',(-9.56548357500006,11.6,4.57227161699999));
#250078=CARTESIAN_POINT('Ctrl Pts',(-9.56383444500006,15.2,4.57096591099998));
#250079=CARTESIAN_POINT('Ctrl Pts',(-9.56383444500006,11.6,4.57096591099998));
#250080=CARTESIAN_POINT('Ctrl Pts',(-9.56218953100005,15.2,4.56966593299998));
#250081=CARTESIAN_POINT('Ctrl Pts',(-9.56218953100005,11.6,4.56966593299998));
#250082=CARTESIAN_POINT('Ctrl Pts',(-9.56054884800006,15.2,4.56837168399999));
#250083=CARTESIAN_POINT('Ctrl Pts',(-9.56054884800006,11.6,4.56837168399998));
#250084=CARTESIAN_POINT('Ctrl Pts',(-9.55891241700006,15.2,4.56708316299999));
#250085=CARTESIAN_POINT('Ctrl Pts',(-9.55891241700006,11.6,4.56708316299998));
#250086=CARTESIAN_POINT('Ctrl Pts',(-9.55728025600006,15.2,4.56580037199998));
#250087=CARTESIAN_POINT('Ctrl Pts',(-9.55728025600006,11.6,4.56580037199998));
#250088=CARTESIAN_POINT('Ctrl Pts',(-9.55565238300006,15.2,4.56452331099998));
#250089=CARTESIAN_POINT('Ctrl Pts',(-9.55565238300006,11.6,4.56452331099998));
#250090=CARTESIAN_POINT('Ctrl Pts',(-9.55402881600006,15.2,4.56325197999998));
#250091=CARTESIAN_POINT('Ctrl Pts',(-9.55402881600006,11.6,4.56325197999998));
#250092=CARTESIAN_POINT('Ctrl Pts',(-9.55240957500006,15.2,4.56198637899998));
#250093=CARTESIAN_POINT('Ctrl Pts',(-9.55240957500006,11.6,4.56198637899998));
#250094=CARTESIAN_POINT('Ctrl Pts',(-9.55079467700006,15.2,4.56072650899999));
#250095=CARTESIAN_POINT('Ctrl Pts',(-9.55079467700006,11.6,4.56072650899999));
#250096=CARTESIAN_POINT('Ctrl Pts',(-9.54918414200005,15.2,4.55947236999998));
#250097=CARTESIAN_POINT('Ctrl Pts',(-9.54918414200005,11.6,4.55947236999998));
#250098=CARTESIAN_POINT('Ctrl Pts',(-9.54757798700006,15.2,4.55822396199999));
#250099=CARTESIAN_POINT('Ctrl Pts',(-9.54757798700006,11.6,4.55822396199998));
#250100=CARTESIAN_POINT('Ctrl Pts',(-9.54597623200005,15.2,4.55698128599998));
#250101=CARTESIAN_POINT('Ctrl Pts',(-9.54597623200005,11.6,4.55698128599998));
#250102=CARTESIAN_POINT('Ctrl Pts',(-9.54437889600005,15.2,4.55574434099999));
#250103=CARTESIAN_POINT('Ctrl Pts',(-9.54437889600005,11.6,4.55574434099999));
#250104=CARTESIAN_POINT('Ctrl Pts',(-9.54278599800006,15.2,4.55451312899999));
#250105=CARTESIAN_POINT('Ctrl Pts',(-9.54278599800006,11.6,4.55451312899999));
#250106=CARTESIAN_POINT('Ctrl Pts',(-9.54119755600006,15.2,4.55328764899999));
#250107=CARTESIAN_POINT('Ctrl Pts',(-9.54119755600006,11.6,4.55328764899999));
#250108=CARTESIAN_POINT('Ctrl Pts',(-9.53961359000006,15.2,4.55206790099999));
#250109=CARTESIAN_POINT('Ctrl Pts',(-9.53961359000006,11.6,4.55206790099999));
#250110=CARTESIAN_POINT('Ctrl Pts',(-9.53803411900006,15.2,4.55085388699998));
#250111=CARTESIAN_POINT('Ctrl Pts',(-9.53803411900006,11.6,4.55085388699998));
#250112=CARTESIAN_POINT('Ctrl Pts',(-9.53645916300006,15.2,4.54964560499998));
#250113=CARTESIAN_POINT('Ctrl Pts',(-9.53645916300006,11.6,4.54964560499998));
#250114=CARTESIAN_POINT('Ctrl Pts',(-9.53488873900006,15.2,4.54844305599998));
#250115=CARTESIAN_POINT('Ctrl Pts',(-9.53488873900006,11.6,4.54844305599998));
#250116=CARTESIAN_POINT('Ctrl Pts',(-9.53332286700006,15.2,4.54724623999999));
#250117=CARTESIAN_POINT('Ctrl Pts',(-9.53332286700006,11.6,4.54724623999999));
#250118=CARTESIAN_POINT('Ctrl Pts',(-9.53176156700006,15.2,4.54605515799998));
#250119=CARTESIAN_POINT('Ctrl Pts',(-9.53176156700006,11.6,4.54605515799998));
#250120=CARTESIAN_POINT('Ctrl Pts',(-9.53020485900005,15.2,4.54486980999998));
#250121=CARTESIAN_POINT('Ctrl Pts',(-9.53020485900005,11.6,4.54486980999998));
#250122=CARTESIAN_POINT('Ctrl Pts',(-9.52865276200006,15.2,4.54369019499998));
#250123=CARTESIAN_POINT('Ctrl Pts',(-9.52865276200006,11.6,4.54369019499998));
#250124=CARTESIAN_POINT('Ctrl Pts',(-9.52710529500006,15.2,4.54251631399998));
#250125=CARTESIAN_POINT('Ctrl Pts',(-9.52710529500006,11.6,4.54251631399998));
#250126=CARTESIAN_POINT('Ctrl Pts',(-9.52556247800005,15.2,4.54134816799999));
#250127=CARTESIAN_POINT('Ctrl Pts',(-9.52556247800005,11.6,4.54134816799998));
#250128=CARTESIAN_POINT('Ctrl Pts',(-9.52402433000006,15.2,4.54018575399999));
#250129=CARTESIAN_POINT('Ctrl Pts',(-9.52402433000006,11.6,4.54018575399999));
#250130=CARTESIAN_POINT('Ctrl Pts',(-9.52249087200006,15.2,4.53902907599999));
#250131=CARTESIAN_POINT('Ctrl Pts',(-9.52249087200006,11.6,4.53902907599998));
#250132=CARTESIAN_POINT('Ctrl Pts',(-9.52096212300006,15.2,4.53787813199998));
#250133=CARTESIAN_POINT('Ctrl Pts',(-9.52096212300006,11.6,4.53787813199998));
#250134=CARTESIAN_POINT('Ctrl Pts',(-9.51943810400006,15.2,4.53673292199999));
#250135=CARTESIAN_POINT('Ctrl Pts',(-9.51943810400006,11.6,4.53673292199999));
#250136=CARTESIAN_POINT('Ctrl Pts',(-9.51791883400006,15.2,4.53559344699999));
#250137=CARTESIAN_POINT('Ctrl Pts',(-9.51791883400006,11.6,4.53559344699999));
#250138=CARTESIAN_POINT('Ctrl Pts',(-9.51640433300006,15.2,4.53445970499998));
#250139=CARTESIAN_POINT('Ctrl Pts',(-9.51640433300006,11.6,4.53445970499998));
#250140=CARTESIAN_POINT('Ctrl Pts',(-9.51489462200006,15.2,4.53333169899999));
#250141=CARTESIAN_POINT('Ctrl Pts',(-9.51489462200006,11.6,4.53333169899999));
#250142=CARTESIAN_POINT('Ctrl Pts',(-9.51338972000006,15.2,4.53220942699998));
#250143=CARTESIAN_POINT('Ctrl Pts',(-9.51338972000006,11.6,4.53220942699998));
#250144=CARTESIAN_POINT('Ctrl Pts',(-9.51188964800006,15.2,4.53109288999999));
#250145=CARTESIAN_POINT('Ctrl Pts',(-9.51188964800006,11.6,4.53109288999998));
#250146=CARTESIAN_POINT('Ctrl Pts',(-9.51039442600005,15.2,4.52998208699999));
#250147=CARTESIAN_POINT('Ctrl Pts',(-9.51039442600005,11.6,4.52998208699999));
#250148=CARTESIAN_POINT('Ctrl Pts',(-9.50890407400006,15.2,4.52887701899999));
#250149=CARTESIAN_POINT('Ctrl Pts',(-9.50890407400006,11.6,4.52887701899999));
#250150=CARTESIAN_POINT('Ctrl Pts',(-9.50741861400006,15.2,4.52777768499999));
#250151=CARTESIAN_POINT('Ctrl Pts',(-9.50741861400006,11.6,4.52777768499998));
#250152=CARTESIAN_POINT('Ctrl Pts',(-9.50593806600006,15.2,4.52668408599998));
#250153=CARTESIAN_POINT('Ctrl Pts',(-9.50593806600006,11.6,4.52668408599998));
#250154=CARTESIAN_POINT('Ctrl Pts',(-9.50446244800006,15.2,4.52559622099999));
#250155=CARTESIAN_POINT('Ctrl Pts',(-9.50446244800006,11.6,4.52559622099999));
#250156=CARTESIAN_POINT('Ctrl Pts',(-9.50299178500006,15.2,4.52451408999998));
#250157=CARTESIAN_POINT('Ctrl Pts',(-9.50299178500006,11.6,4.52451408999998));
#250158=CARTESIAN_POINT('Ctrl Pts',(-9.50152609500006,15.2,4.52343769399998));
#250159=CARTESIAN_POINT('Ctrl Pts',(-9.50152609500006,11.6,4.52343769399998));
#250160=CARTESIAN_POINT('Ctrl Pts',(-9.50006539900006,15.2,4.52236703199999));
#250161=CARTESIAN_POINT('Ctrl Pts',(-9.50006539900006,11.6,4.52236703199999));
#250162=CARTESIAN_POINT('Ctrl Pts',(-9.49860971900006,15.2,4.52130210399999));
#250163=CARTESIAN_POINT('Ctrl Pts',(-9.49860971900006,11.6,4.52130210399999));
#250164=CARTESIAN_POINT('Ctrl Pts',(-9.49715907600006,15.2,4.52024290899999));
#250165=CARTESIAN_POINT('Ctrl Pts',(-9.49715907600006,11.6,4.52024290899998));
#250166=CARTESIAN_POINT('Ctrl Pts',(-9.49571348900006,15.2,4.51918944999999));
#250167=CARTESIAN_POINT('Ctrl Pts',(-9.49571348900006,11.6,4.51918944999999));
#250168=CARTESIAN_POINT('Ctrl Pts',(-9.49427298200006,15.2,4.51814172299999));
#250169=CARTESIAN_POINT('Ctrl Pts',(-9.49427298200006,11.6,4.51814172299999));
#250170=CARTESIAN_POINT('Ctrl Pts',(-9.49283757400006,15.2,4.51709972999998));
#250171=CARTESIAN_POINT('Ctrl Pts',(-9.49283757400006,11.6,4.51709972999998));
#250172=CARTESIAN_POINT('Ctrl Pts',(-9.49140728700005,15.2,4.51606347099998));
#250173=CARTESIAN_POINT('Ctrl Pts',(-9.49140728700005,11.6,4.51606347099998));
#250174=CARTESIAN_POINT('Ctrl Pts',(-9.48998214300006,15.2,4.51503294499998));
#250175=CARTESIAN_POINT('Ctrl Pts',(-9.48998214300006,11.6,4.51503294499998));
#250176=CARTESIAN_POINT('Ctrl Pts',(-9.48856216300005,15.2,4.51400815099999));
#250177=CARTESIAN_POINT('Ctrl Pts',(-9.48856216300005,11.6,4.51400815099999));
#250178=CARTESIAN_POINT('Ctrl Pts',(-9.48714736900006,15.2,4.51298908999998));
#250179=CARTESIAN_POINT('Ctrl Pts',(-9.48714736900006,11.6,4.51298908999998));
#250180=CARTESIAN_POINT('Ctrl Pts',(-9.48573778000006,15.2,4.51197576299998));
#250181=CARTESIAN_POINT('Ctrl Pts',(-9.48573778000006,11.6,4.51197576299998));
#250182=CARTESIAN_POINT('Ctrl Pts',(-9.48433342200006,15.2,4.51096816699998));
#250183=CARTESIAN_POINT('Ctrl Pts',(-9.48433342200006,11.6,4.51096816699998));
#250184=CARTESIAN_POINT('Ctrl Pts',(-9.48293431400005,15.2,4.50996630299999));
#250185=CARTESIAN_POINT('Ctrl Pts',(-9.48293431400005,11.6,4.50996630299999));
#250186=CARTESIAN_POINT('Ctrl Pts',(-9.48154047900006,15.2,4.50897017199999));
#250187=CARTESIAN_POINT('Ctrl Pts',(-9.48154047900006,11.6,4.50897017199999));
#250188=CARTESIAN_POINT('Ctrl Pts',(-9.48015193800006,15.2,4.50797977199999));
#250189=CARTESIAN_POINT('Ctrl Pts',(-9.48015193800006,11.6,4.50797977199999));
#250190=CARTESIAN_POINT('Ctrl Pts',(-9.47876871400006,15.2,4.50699510299999));
#250191=CARTESIAN_POINT('Ctrl Pts',(-9.47876871400006,11.6,4.50699510299999));
#250192=CARTESIAN_POINT('Ctrl Pts',(-9.47739082700006,15.2,4.50601616499998));
#250193=CARTESIAN_POINT('Ctrl Pts',(-9.47739082700006,11.6,4.50601616499998));
#250194=CARTESIAN_POINT('Ctrl Pts',(-9.47601830200006,15.2,4.50504295799998));
#250195=CARTESIAN_POINT('Ctrl Pts',(-9.47601830200006,11.6,4.50504295799998));
#250196=CARTESIAN_POINT('Ctrl Pts',(-9.47465116000006,15.2,4.50407548099999));
#250197=CARTESIAN_POINT('Ctrl Pts',(-9.47465116000006,11.6,4.50407548099999));
#250198=CARTESIAN_POINT('Ctrl Pts',(-9.47328942300006,15.2,4.50311373399998));
#250199=CARTESIAN_POINT('Ctrl Pts',(-9.47328942300006,11.6,4.50311373399998));
#250200=CARTESIAN_POINT('Ctrl Pts',(-9.47193311400006,15.2,4.50215771699998));
#250201=CARTESIAN_POINT('Ctrl Pts',(-9.47193311400006,11.6,4.50215771699998));
#250202=CARTESIAN_POINT('Ctrl Pts',(-9.47058225500006,15.2,4.50120742799999));
#250203=CARTESIAN_POINT('Ctrl Pts',(-9.47058225500006,11.6,4.50120742799999));
#250204=CARTESIAN_POINT('Ctrl Pts',(-9.46923686900006,15.2,4.50026286999999));
#250205=CARTESIAN_POINT('Ctrl Pts',(-9.46923686900006,11.6,4.50026286999999));
#250206=CARTESIAN_POINT('Ctrl Pts',(-9.46789697900006,15.2,4.49932403899999));
#250207=CARTESIAN_POINT('Ctrl Pts',(-9.46789697900006,11.6,4.49932403899999));
#250208=CARTESIAN_POINT('Ctrl Pts',(-9.46656260800006,15.2,4.49839093599999));
#250209=CARTESIAN_POINT('Ctrl Pts',(-9.46656260800006,11.6,4.49839093599999));
#250210=CARTESIAN_POINT('Ctrl Pts',(-9.46523377700006,15.2,4.49746356099999));
#250211=CARTESIAN_POINT('Ctrl Pts',(-9.46523377700006,11.6,4.49746356099998));
#250212=CARTESIAN_POINT('Ctrl Pts',(-9.46391051100005,15.2,4.49654191199999));
#250213=CARTESIAN_POINT('Ctrl Pts',(-9.46391051100005,11.6,4.49654191199999));
#250214=CARTESIAN_POINT('Ctrl Pts',(-9.46259283200006,15.2,4.49562599099998));
#250215=CARTESIAN_POINT('Ctrl Pts',(-9.46259283200006,11.6,4.49562599099998));
#250216=CARTESIAN_POINT('Ctrl Pts',(-9.46128076500005,15.2,4.49471579599999));
#250217=CARTESIAN_POINT('Ctrl Pts',(-9.46128076500005,11.6,4.49471579599999));
#250218=CARTESIAN_POINT('Ctrl Pts',(-9.45997433000005,15.2,4.49381132699998));
#250219=CARTESIAN_POINT('Ctrl Pts',(-9.45997433000005,11.6,4.49381132699998));
#250220=CARTESIAN_POINT('Ctrl Pts',(-9.45867355200006,15.2,4.49291258199998));
#250221=CARTESIAN_POINT('Ctrl Pts',(-9.45867355200006,11.6,4.49291258199998));
#250222=CARTESIAN_POINT('Ctrl Pts',(-9.45737845600006,15.2,4.49201956299999));
#250223=CARTESIAN_POINT('Ctrl Pts',(-9.45737845600006,11.6,4.49201956299999));
#250224=CARTESIAN_POINT('Ctrl Pts',(-9.45608906200006,15.2,4.49113226799999));
#250225=CARTESIAN_POINT('Ctrl Pts',(-9.45608906200006,11.6,4.49113226799999));
#250226=CARTESIAN_POINT('Ctrl Pts',(-9.45480539700006,15.2,4.49025069599998));
#250227=CARTESIAN_POINT('Ctrl Pts',(-9.45480539700006,11.6,4.49025069599998));
#250228=CARTESIAN_POINT('Ctrl Pts',(-9.45352748300006,15.2,4.48937484699999));
#250229=CARTESIAN_POINT('Ctrl Pts',(-9.45352748300006,11.6,4.48937484699999));
#250230=CARTESIAN_POINT('Ctrl Pts',(-9.45225534400005,15.2,4.48850472099998));
#250231=CARTESIAN_POINT('Ctrl Pts',(-9.45225534400005,11.6,4.48850472099998));
#250232=CARTESIAN_POINT('Ctrl Pts',(-9.45098900300006,15.2,4.48764031599998));
#250233=CARTESIAN_POINT('Ctrl Pts',(-9.45098900300006,11.6,4.48764031599998));
#250234=CARTESIAN_POINT('Ctrl Pts',(-9.44972848600005,15.2,4.48678163399999));
#250235=CARTESIAN_POINT('Ctrl Pts',(-9.44972848600005,11.6,4.48678163399998));
#250236=CARTESIAN_POINT('Ctrl Pts',(-9.44847381600006,15.2,4.48592867099999));
#250237=CARTESIAN_POINT('Ctrl Pts',(-9.44847381600006,11.6,4.48592867099998));
#250238=CARTESIAN_POINT('Ctrl Pts',(-9.44722501700006,15.2,4.48508142899998));
#250239=CARTESIAN_POINT('Ctrl Pts',(-9.44722501700006,11.6,4.48508142899998));
#250240=CARTESIAN_POINT('Ctrl Pts',(-9.44598211300006,15.2,4.48423990499998));
#250241=CARTESIAN_POINT('Ctrl Pts',(-9.44598211300006,11.6,4.48423990499998));
#250242=CARTESIAN_POINT('Ctrl Pts',(-9.44474512900005,15.2,4.48340410099998));
#250243=CARTESIAN_POINT('Ctrl Pts',(-9.44474512900005,11.6,4.48340410099998));
#250244=CARTESIAN_POINT('Ctrl Pts',(-9.44351409000006,15.2,4.48257401399999));
#250245=CARTESIAN_POINT('Ctrl Pts',(-9.44351409000006,11.6,4.48257401399999));
#250246=CARTESIAN_POINT('Ctrl Pts',(-9.44228901900006,15.2,4.48174964399998));
#250247=CARTESIAN_POINT('Ctrl Pts',(-9.44228901900006,11.6,4.48174964399998));
#250248=CARTESIAN_POINT('Ctrl Pts',(-9.44106994200006,15.2,4.48093099099999));
#250249=CARTESIAN_POINT('Ctrl Pts',(-9.44106994200006,11.6,4.48093099099999));
#250250=CARTESIAN_POINT('Ctrl Pts',(-9.43985688300006,15.2,4.48011805499998));
#250251=CARTESIAN_POINT('Ctrl Pts',(-9.43985688300006,11.6,4.48011805499998));
#250252=CARTESIAN_POINT('Ctrl Pts',(-9.43864986800006,15.2,4.47931083199999));
#250253=CARTESIAN_POINT('Ctrl Pts',(-9.43864986800006,11.6,4.47931083199998));
#250254=CARTESIAN_POINT('Ctrl Pts',(-9.43744892000005,15.2,4.47850932399999));
#250255=CARTESIAN_POINT('Ctrl Pts',(-9.43744892000005,11.6,4.47850932399999));
#250256=CARTESIAN_POINT('Ctrl Pts',(-9.43625406500006,15.2,4.47771352899998));
#250257=CARTESIAN_POINT('Ctrl Pts',(-9.43625406500006,11.6,4.47771352899998));
#250258=CARTESIAN_POINT('Ctrl Pts',(-9.43506532900006,15.2,4.47692344699998));
#250259=CARTESIAN_POINT('Ctrl Pts',(-9.43506532900006,11.6,4.47692344699998));
#250260=CARTESIAN_POINT('Ctrl Pts',(-9.43388273800006,15.2,4.47613907699999));
#250261=CARTESIAN_POINT('Ctrl Pts',(-9.43388273800006,11.6,4.47613907699999));
#250262=CARTESIAN_POINT('Ctrl Pts',(-9.43270631400006,15.2,4.47536041899999));
#250263=CARTESIAN_POINT('Ctrl Pts',(-9.43270631400006,11.6,4.47536041899998));
#250264=CARTESIAN_POINT('Ctrl Pts',(-9.43153608500005,15.2,4.47458746899999));
#250265=CARTESIAN_POINT('Ctrl Pts',(-9.43153608500005,11.6,4.47458746899999));
#250266=CARTESIAN_POINT('Ctrl Pts',(-9.43037207700005,15.2,4.47382022999999));
#250267=CARTESIAN_POINT('Ctrl Pts',(-9.43037207700005,11.6,4.47382022999999));
#250268=CARTESIAN_POINT('Ctrl Pts',(-9.42921431500006,15.2,4.47305869799998));
#250269=CARTESIAN_POINT('Ctrl Pts',(-9.42921431500006,11.6,4.47305869799998));
#250270=CARTESIAN_POINT('Ctrl Pts',(-9.42806282300005,15.2,4.47230287499998));
#250271=CARTESIAN_POINT('Ctrl Pts',(-9.42806282300005,11.6,4.47230287499998));
#250272=CARTESIAN_POINT('Ctrl Pts',(-9.42691763000006,15.2,4.47155275699998));
#250273=CARTESIAN_POINT('Ctrl Pts',(-9.42691763000006,11.6,4.47155275699998));
#250274=CARTESIAN_POINT('Ctrl Pts',(-9.42577876100006,15.2,4.47080834499998));
#250275=CARTESIAN_POINT('Ctrl Pts',(-9.42577876100006,11.6,4.47080834499998));
#250276=CARTESIAN_POINT('Ctrl Pts',(-9.42464624100005,15.2,4.47006963699998));
#250277=CARTESIAN_POINT('Ctrl Pts',(-9.42464624100005,11.6,4.47006963699998));
#250278=CARTESIAN_POINT('Ctrl Pts',(-9.42352009700006,15.2,4.46933663299999));
#250279=CARTESIAN_POINT('Ctrl Pts',(-9.42352009700006,11.6,4.46933663299998));
#250280=CARTESIAN_POINT('Ctrl Pts',(-9.42240035600006,15.2,4.46860933299998));
#250281=CARTESIAN_POINT('Ctrl Pts',(-9.42240035600006,11.6,4.46860933299998));
#250282=CARTESIAN_POINT('Ctrl Pts',(-9.42128704400006,15.2,4.46788773299998));
#250283=CARTESIAN_POINT('Ctrl Pts',(-9.42128704400006,11.6,4.46788773299998));
#250284=CARTESIAN_POINT('Ctrl Pts',(-9.42018018800006,15.2,4.46717183299998));
#250285=CARTESIAN_POINT('Ctrl Pts',(-9.42018018800006,11.6,4.46717183299998));
#250286=CARTESIAN_POINT('Ctrl Pts',(-9.41907981300006,15.2,4.46646163399999));
#250287=CARTESIAN_POINT('Ctrl Pts',(-9.41907981300006,11.6,4.46646163399999));
#250288=CARTESIAN_POINT('Ctrl Pts',(-9.41798594800006,15.2,4.46575713399999));
#250289=CARTESIAN_POINT('Ctrl Pts',(-9.41798594800006,11.6,4.46575713399999));
#250290=CARTESIAN_POINT('Ctrl Pts',(-9.41689861900005,15.2,4.46505832999998));
#250291=CARTESIAN_POINT('Ctrl Pts',(-9.41689861900005,11.6,4.46505832999998));
#250292=CARTESIAN_POINT('Ctrl Pts',(-9.41581785300006,15.2,4.46436522199999));
#250293=CARTESIAN_POINT('Ctrl Pts',(-9.41581785300006,11.6,4.46436522199999));
#250294=CARTESIAN_POINT('Ctrl Pts',(-9.41474367800006,15.2,4.46367780999999));
#250295=CARTESIAN_POINT('Ctrl Pts',(-9.41474367800006,11.6,4.46367780999999));
#250296=CARTESIAN_POINT('Ctrl Pts',(-9.41367611900005,15.2,4.46299609199999));
#250297=CARTESIAN_POINT('Ctrl Pts',(-9.41367611900005,11.6,4.46299609199999));
#250298=CARTESIAN_POINT('Ctrl Pts',(-9.41261520700006,15.2,4.46232006599999));
#250299=CARTESIAN_POINT('Ctrl Pts',(-9.41261520700006,11.6,4.46232006599998));
#250300=CARTESIAN_POINT('Ctrl Pts',(-9.41156096700006,15.2,4.46164973199998));
#250301=CARTESIAN_POINT('Ctrl Pts',(-9.41156096700006,11.6,4.46164973199998));
#250302=CARTESIAN_POINT('Ctrl Pts',(-9.41051342700005,15.2,4.46098508799999));
#250303=CARTESIAN_POINT('Ctrl Pts',(-9.41051342700005,11.6,4.46098508799999));
#250304=CARTESIAN_POINT('Ctrl Pts',(-9.40947261500006,15.2,4.46032613399999));
#250305=CARTESIAN_POINT('Ctrl Pts',(-9.40947261500006,11.6,4.46032613399998));
#250306=CARTESIAN_POINT('Ctrl Pts',(-9.40843855900006,15.2,4.45967286799998));
#250307=CARTESIAN_POINT('Ctrl Pts',(-9.40843855900006,11.6,4.45967286799998));
#250308=CARTESIAN_POINT('Ctrl Pts',(-9.40741128800006,15.2,4.45902528699998));
#250309=CARTESIAN_POINT('Ctrl Pts',(-9.40741128800006,11.6,4.45902528699998));
#250310=CARTESIAN_POINT('Ctrl Pts',(-9.40639082900006,15.2,4.45838339299998));
#250311=CARTESIAN_POINT('Ctrl Pts',(-9.40639082900006,11.6,4.45838339299998));
#250312=CARTESIAN_POINT('Ctrl Pts',(-9.40537721000006,15.2,4.45774718299998));
#250313=CARTESIAN_POINT('Ctrl Pts',(-9.40537721000006,11.6,4.45774718299998));
#250314=CARTESIAN_POINT('Ctrl Pts',(-9.40437046000006,15.2,4.45711665599998));
#250315=CARTESIAN_POINT('Ctrl Pts',(-9.40437046000006,11.6,4.45711665599998));
#250316=CARTESIAN_POINT('Ctrl Pts',(-9.40337060800006,15.2,4.45649180999999));
#250317=CARTESIAN_POINT('Ctrl Pts',(-9.40337060800006,11.6,4.45649180999998));
#250318=CARTESIAN_POINT('Ctrl Pts',(-9.40237768200006,15.2,4.45587264399999));
#250319=CARTESIAN_POINT('Ctrl Pts',(-9.40237768200006,11.6,4.45587264399998));
#250320=CARTESIAN_POINT('Ctrl Pts',(-9.40139171200006,15.2,4.45525915699999));
#250321=CARTESIAN_POINT('Ctrl Pts',(-9.40139171200006,11.6,4.45525915699999));
#250322=CARTESIAN_POINT('Ctrl Pts',(-9.40041272400006,15.2,4.45465134699998));
#250323=CARTESIAN_POINT('Ctrl Pts',(-9.40041272400006,11.6,4.45465134699998));
#250324=CARTESIAN_POINT('Ctrl Pts',(-9.39944075100006,15.2,4.45404921299998));
#250325=CARTESIAN_POINT('Ctrl Pts',(-9.39944075100006,11.6,4.45404921299998));
#250326=CARTESIAN_POINT('Ctrl Pts',(-9.39847582000005,15.2,4.45345275499999));
#250327=CARTESIAN_POINT('Ctrl Pts',(-9.39847582000005,11.6,4.45345275499999));
#250328=CARTESIAN_POINT('Ctrl Pts',(-9.39751796100006,15.2,4.45286196799999));
#250329=CARTESIAN_POINT('Ctrl Pts',(-9.39751796100006,11.6,4.45286196799999));
#250330=CARTESIAN_POINT('Ctrl Pts',(-9.39656720200006,15.2,4.45227685299999));
#250331=CARTESIAN_POINT('Ctrl Pts',(-9.39656720200006,11.6,4.45227685299999));
#250332=CARTESIAN_POINT('Ctrl Pts',(-9.39562357500006,15.2,4.45169740899999));
#250333=CARTESIAN_POINT('Ctrl Pts',(-9.39562357500006,11.6,4.45169740899999));
#250334=CARTESIAN_POINT('Ctrl Pts',(-9.39468710800006,15.2,4.45112363199998));
#250335=CARTESIAN_POINT('Ctrl Pts',(-9.39468710800006,11.6,4.45112363199998));
#250336=CARTESIAN_POINT('Ctrl Pts',(-9.39375783100006,15.2,4.45055552199998));
#250337=CARTESIAN_POINT('Ctrl Pts',(-9.39375783100006,11.6,4.45055552199998));
#250338=CARTESIAN_POINT('Ctrl Pts',(-9.39283577600006,15.2,4.44999307799999));
#250339=CARTESIAN_POINT('Ctrl Pts',(-9.39283577600006,11.6,4.44999307799998));
#250340=CARTESIAN_POINT('Ctrl Pts',(-9.39192097100005,15.2,4.44943629799998));
#250341=CARTESIAN_POINT('Ctrl Pts',(-9.39192097100005,11.6,4.44943629799998));
#250342=CARTESIAN_POINT('Ctrl Pts',(-9.39101344700006,15.2,4.44888517999999));
#250343=CARTESIAN_POINT('Ctrl Pts',(-9.39101344700006,11.6,4.44888517999999));
#250344=CARTESIAN_POINT('Ctrl Pts',(-9.39011323600005,15.2,4.44833972299998));
#250345=CARTESIAN_POINT('Ctrl Pts',(-9.39011323600005,11.6,4.44833972299998));
#250346=CARTESIAN_POINT('Ctrl Pts',(-9.38922036600006,15.2,4.44779992399998));
#250347=CARTESIAN_POINT('Ctrl Pts',(-9.38922036600006,11.6,4.44779992399998));
#250348=CARTESIAN_POINT('Ctrl Pts',(-9.38833486900006,15.2,4.44726578299999));
#250349=CARTESIAN_POINT('Ctrl Pts',(-9.38833486900006,11.6,4.44726578299999));
#250350=CARTESIAN_POINT('Ctrl Pts',(-9.38745677700006,15.2,4.44673729799998));
#250351=CARTESIAN_POINT('Ctrl Pts',(-9.38745677700006,11.6,4.44673729799998));
#250352=CARTESIAN_POINT('Ctrl Pts',(-9.38658611800006,15.2,4.44621446599999));
#250353=CARTESIAN_POINT('Ctrl Pts',(-9.38658611800006,11.6,4.44621446599999));
#250354=CARTESIAN_POINT('Ctrl Pts',(-9.38572292800006,15.2,4.44569728599999));
#250355=CARTESIAN_POINT('Ctrl Pts',(-9.38572292800006,11.6,4.44569728599998));
#250356=CARTESIAN_POINT('Ctrl Pts',(-9.38486723400005,15.2,4.44518575599999));
#250357=CARTESIAN_POINT('Ctrl Pts',(-9.38486723400005,11.6,4.44518575599999));
#250358=CARTESIAN_POINT('Ctrl Pts',(-9.38401906900006,15.2,4.44467987499999));
#250359=CARTESIAN_POINT('Ctrl Pts',(-9.38401906900006,11.6,4.44467987499999));
#250360=CARTESIAN_POINT('Ctrl Pts',(-9.38317846500006,15.2,4.44417964099999));
#250361=CARTESIAN_POINT('Ctrl Pts',(-9.38317846500006,11.6,4.44417964099998));
#250362=CARTESIAN_POINT('Ctrl Pts',(-9.38234545400006,15.2,4.44368505099998));
#250363=CARTESIAN_POINT('Ctrl Pts',(-9.38234545400006,11.6,4.44368505099998));
#250364=CARTESIAN_POINT('Ctrl Pts',(-9.38152006800006,15.2,4.44319610499999));
#250365=CARTESIAN_POINT('Ctrl Pts',(-9.38152006800006,11.6,4.44319610499999));
#250366=CARTESIAN_POINT('Ctrl Pts',(-9.38070233900006,15.2,4.44271279999998));
#250367=CARTESIAN_POINT('Ctrl Pts',(-9.38070233900006,11.6,4.44271279999998));
#250368=CARTESIAN_POINT('Ctrl Pts',(-9.37989229900005,15.2,4.44223513399999));
#250369=CARTESIAN_POINT('Ctrl Pts',(-9.37989229900005,11.6,4.44223513399999));
#250370=CARTESIAN_POINT('Ctrl Pts',(-9.37908998000006,15.2,4.44176310499999));
#250371=CARTESIAN_POINT('Ctrl Pts',(-9.37908998000006,11.6,4.44176310499999));
#250372=CARTESIAN_POINT('Ctrl Pts',(-9.37829999300006,15.2,4.44129939799998));
#250373=CARTESIAN_POINT('Ctrl Pts',(-9.37829999300006,11.6,4.44129939799998));
#250374=CARTESIAN_POINT('Ctrl Pts',(-9.37767505800006,15.2,4.44093341099999));
#250375=CARTESIAN_POINT('Ctrl Pts',(-9.37767505800006,11.6,4.44093341099998));
#250376=CARTESIAN_POINT('Ctrl Pts',(-9.37721094100005,15.2,4.44066207099999));
#250377=CARTESIAN_POINT('Ctrl Pts',(-9.37721094100005,11.6,4.44066207099999));
#250378=CARTESIAN_POINT('Ctrl Pts',(-9.37690455300006,15.2,4.44048314699998));
#250379=CARTESIAN_POINT('Ctrl Pts',(-9.37690455300006,11.6,4.44048314699998));
#250380=CARTESIAN_POINT('Ctrl Pts',(-9.37675396800006,15.2,4.44039525799998));
#250381=CARTESIAN_POINT('Ctrl Pts',(-9.37675396800006,11.6,4.44039525799998));
#250382=CARTESIAN_POINT('',(-9.37675396726197,12.2,4.44039525796617));
#250383=CARTESIAN_POINT('',(-9.37675396726197,15.2,4.44039525796617));
#250384=CARTESIAN_POINT('',(-9.37675396700006,12.2,4.44039525799998));
#250385=CARTESIAN_POINT('Ctrl Pts',(-10.2217148780001,12.2,5.26939701899998));
#250386=CARTESIAN_POINT('Ctrl Pts',(-10.2194283575847,12.2,5.26633326844343));
#250387=CARTESIAN_POINT('Ctrl Pts',(-10.2171423378183,12.2,5.26327740164306));
#250388=CARTESIAN_POINT('Ctrl Pts',(-10.2148568145106,12.2,5.26022941979131));
#250389=CARTESIAN_POINT('Ctrl Pts',(-10.212571291203,12.2,5.25718143793957));
#250390=CARTESIAN_POINT('Ctrl Pts',(-10.2102862662399,12.2,5.25414134087888));
#250391=CARTESIAN_POINT('Ctrl Pts',(-10.2080017562504,12.2,5.25110913437833));
#250392=CARTESIAN_POINT('Ctrl Pts',(-10.2057172462609,12.2,5.24807692787778));
#250393=CARTESIAN_POINT('Ctrl Pts',(-10.2034332515483,12.2,5.24505261033232));
#250394=CARTESIAN_POINT('Ctrl Pts',(-10.2011498145062,12.2,5.24203619464918));
#250395=CARTESIAN_POINT('Ctrl Pts',(-10.1988663770492,12.2,5.23901977841805));
#250396=CARTESIAN_POINT('Ctrl Pts',(-10.1965834982841,12.2,5.23601126379749));
#250397=CARTESIAN_POINT('Ctrl Pts',(-10.1943012262858,12.2,5.23301066211247));
#250398=CARTESIAN_POINT('Ctrl Pts',(-10.1920189547022,12.2,5.23001006097256));
#250399=CARTESIAN_POINT('Ctrl Pts',(-10.1897372904352,12.2,5.22701737409891));
#250400=CARTESIAN_POINT('Ctrl Pts',(-10.1874562702264,12.2,5.22403260995806));
#250401=CARTESIAN_POINT('Ctrl Pts',(-10.1851752500177,12.2,5.2210478458172));
#250402=CARTESIAN_POINT('Ctrl Pts',(-10.1828948737922,12.2,5.21807100541948));
#250403=CARTESIAN_POINT('Ctrl Pts',(-10.1806151784896,12.2,5.21510209722224));
#250404=CARTESIAN_POINT('Ctrl Pts',(-10.1783354831871,12.2,5.21213318902499));
#250405=CARTESIAN_POINT('Ctrl Pts',(-10.1760564669297,12.2,5.20917221267545));
#250406=CARTESIAN_POINT('Ctrl Pts',(-10.1737781722521,12.2,5.20621917897761));
#250407=CARTESIAN_POINT('Ctrl Pts',(-10.1714998775745,12.2,5.20326614527977));
#250408=CARTESIAN_POINT('Ctrl Pts',(-10.1692223041823,12.2,5.2003210545142));
#250409=CARTESIAN_POINT('Ctrl Pts',(-10.1669454934732,12.2,5.19738391682855));
#250410=CARTESIAN_POINT('Ctrl Pts',(-10.1646686827642,12.2,5.1944467791429));
#250411=CARTESIAN_POINT('Ctrl Pts',(-10.1623926336802,12.2,5.19151759504837));
#250412=CARTESIAN_POINT('Ctrl Pts',(-10.1601173874711,12.2,5.18859637286176));
#250413=CARTESIAN_POINT('Ctrl Pts',(-10.1578421408486,12.2,5.18567515014445));
#250414=CARTESIAN_POINT('Ctrl Pts',(-10.1555676965681,12.2,5.18276188983774));
#250415=CARTESIAN_POINT('Ctrl Pts',(-10.1532940939877,12.2,5.17985660212492));
#250416=CARTESIAN_POINT('Ctrl Pts',(-10.1510204918205,12.2,5.1769513149399));
#250417=CARTESIAN_POINT('Ctrl Pts',(-10.1487477321747,12.2,5.17405400122943));
#250418=CARTESIAN_POINT('Ctrl Pts',(-10.1464758553522,12.2,5.17116466848266));
#250419=CARTESIAN_POINT('Ctrl Pts',(-10.1434466863931,12.2,5.16731222499526));
#250420=CARTESIAN_POINT('Ctrl Pts',(-10.1404190870807,12.2,5.16347397394543));
#250421=CARTESIAN_POINT('Ctrl Pts',(-10.1373931562724,12.2,5.15964993581268));
#250422=CARTESIAN_POINT('Ctrl Pts',(-10.1351237080631,12.2,5.15678190708286));
#250423=CARTESIAN_POINT('Ctrl Pts',(-10.1328551960955,12.2,5.15392187333583));
#250424=CARTESIAN_POINT('Ctrl Pts',(-10.1305876639694,12.2,5.15106984464668));
#250425=CARTESIAN_POINT('Ctrl Pts',(-10.1283201314313,12.2,5.14821781543941));
#250426=CARTESIAN_POINT('Ctrl Pts',(-10.1260535790853,12.2,5.14537379159276));
#250427=CARTESIAN_POINT('Ctrl Pts',(-10.1237880465062,12.2,5.14253778234836));
#250428=CARTESIAN_POINT('Ctrl Pts',(-10.1215225143386,12.2,5.13970177361917));
#250429=CARTESIAN_POINT('Ctrl Pts',(-10.1192580022095,12.2,5.13687377885858));
#250430=CARTESIAN_POINT('Ctrl Pts',(-10.1169945533455,12.2,5.13405380894608));
#250431=CARTESIAN_POINT('Ctrl Pts',(-10.1147311044814,12.2,5.13123383903358));
#250432=CARTESIAN_POINT('Ctrl Pts',(-10.1124687166213,12.2,5.12842189314187));
#250433=CARTESIAN_POINT('Ctrl Pts',(-10.1102074339953,12.2,5.12561798091111));
#250434=CARTESIAN_POINT('Ctrl Pts',(-10.1079461513692,12.2,5.12281406868035));
#250435=CARTESIAN_POINT('Ctrl Pts',(-10.1056859740846,12.2,5.12001819071531));
#250436=CARTESIAN_POINT('Ctrl Pts',(-10.103426942,12.2,5.11723035506659));
#250437=CARTESIAN_POINT('Ctrl Pts',(-10.1011679099155,12.2,5.11444251941788));
#250438=CARTESIAN_POINT('Ctrl Pts',(-10.0989100241975,12.2,5.11166272795219));
#250439=CARTESIAN_POINT('Ctrl Pts',(-10.0966533284877,12.2,5.10889098830218));
#250440=CARTESIAN_POINT('Ctrl Pts',(-10.0943966327779,12.2,5.10611924865216));
#250441=CARTESIAN_POINT('Ctrl Pts',(-10.0921411251431,12.2,5.10335556185167));
#250442=CARTESIAN_POINT('Ctrl Pts',(-10.0898868499748,12.2,5.10059993711733));
#250443=CARTESIAN_POINT('Ctrl Pts',(-10.087632574397,12.2,5.09784431188239));
#250444=CARTESIAN_POINT('Ctrl Pts',(-10.0853795308196,12.2,5.09509674864976));
#250445=CARTESIAN_POINT('Ctrl Pts',(-10.0831277617842,12.2,5.0923572564194));
#250446=CARTESIAN_POINT('Ctrl Pts',(-10.0808759931578,12.2,5.08961776468671));
#250447=CARTESIAN_POINT('Ctrl Pts',(-10.0786254987287,12.2,5.08688634419262));
#250448=CARTESIAN_POINT('Ctrl Pts',(-10.0763763225316,12.2,5.08416300478145));
#250449=CARTESIAN_POINT('Ctrl Pts',(-10.0741271463344,12.2,5.08143966537029));
#250450=CARTESIAN_POINT('Ctrl Pts',(-10.0718792885568,12.2,5.07872440563927));
#250451=CARTESIAN_POINT('Ctrl Pts',(-10.0696327919719,12.2,5.07601723640499));
#250452=CARTESIAN_POINT('Ctrl Pts',(-10.0673862953869,12.2,5.07331006717071));
#250453=CARTESIAN_POINT('Ctrl Pts',(-10.0651411608352,12.2,5.07061098775214));
#250454=CARTESIAN_POINT('Ctrl Pts',(-10.06289743125,12.2,5.06792000697492));
#250455=CARTESIAN_POINT('Ctrl Pts',(-10.0606537016649,12.2,5.0652290261977));
#250456=CARTESIAN_POINT('Ctrl Pts',(-10.0584113772464,12.2,5.0625461441118));
#250457=CARTESIAN_POINT('Ctrl Pts',(-10.0561705022027,12.2,5.05987137033328));
#250458=CARTESIAN_POINT('Ctrl Pts',(-10.0539296271589,12.2,5.05719659655475));
#250459=CARTESIAN_POINT('Ctrl Pts',(-10.0516902020304,12.2,5.05452993068487));
#250460=CARTESIAN_POINT('Ctrl Pts',(-10.0494522698747,12.2,5.0518713822727));
#250461=CARTESIAN_POINT('Ctrl Pts',(-10.047214337719,12.2,5.04921283386054));
#250462=CARTESIAN_POINT('Ctrl Pts',(-10.0449779002563,12.2,5.04656240179774));
#250463=CARTESIAN_POINT('Ctrl Pts',(-10.0427429997539,12.2,5.04392009605929));
#250464=CARTESIAN_POINT('Ctrl Pts',(-10.0405080988456,12.2,5.04127778984082));
#250465=CARTESIAN_POINT('Ctrl Pts',(-10.0382747369043,12.2,5.03864360962468));
#250466=CARTESIAN_POINT('Ctrl Pts',(-10.0360429574969,12.2,5.0360175644108));
#250467=CARTESIAN_POINT('Ctrl Pts',(-10.0338111784948,12.2,5.03339151967399));
#250468=CARTESIAN_POINT('Ctrl Pts',(-10.0315809835594,12.2,5.03077360997007));
#250469=CARTESIAN_POINT('Ctrl Pts',(-10.0293524160155,12.2,5.02816384419061));
#250470=CARTESIAN_POINT('Ctrl Pts',(-10.0271238484716,12.2,5.02555407841114));
#250471=CARTESIAN_POINT('Ctrl Pts',(-10.0248969088106,12.2,5.02295245608174));
#250472=CARTESIAN_POINT('Ctrl Pts',(-10.0226716432147,12.2,5.02035898674758));
#250473=CARTESIAN_POINT('Ctrl Pts',(-10.0204463776188,12.2,5.01776551741343));
#250474=CARTESIAN_POINT('Ctrl Pts',(-10.0182227858814,12.2,5.01518019958702));
#250475=CARTESIAN_POINT('Ctrl Pts',(-10.0160009132854,12.2,5.01260304425227));
#250476=CARTESIAN_POINT('Ctrl Pts',(-10.0137790406894,12.2,5.01002588891752));
#250477=CARTESIAN_POINT('Ctrl Pts',(-10.0115588869948,12.2,5.0074568946202));
#250478=CARTESIAN_POINT('Ctrl Pts',(-10.0093404984919,12.2,5.00489607079587));
#250479=CARTESIAN_POINT('Ctrl Pts',(-10.007122109989,12.2,5.00233524697152));
#250480=CARTESIAN_POINT('Ctrl Pts',(-10.0049054872027,12.2,4.99978259207998));
#250481=CARTESIAN_POINT('Ctrl Pts',(-10.0026906756995,12.2,4.99723811679629));
#250482=CARTESIAN_POINT('Ctrl Pts',(-9.99973759342713,12.2,4.99384548277655));
#250483=CARTESIAN_POINT('Ctrl Pts',(-9.99678773281922,12.2,4.99046738902674));
#250484=CARTESIAN_POINT('Ctrl Pts',(-9.99384120125637,12.2,4.9871038544393));
#250485=CARTESIAN_POINT('Ctrl Pts',(-9.99163130278496,12.2,4.98458120372787));
#250486=CARTESIAN_POINT('Ctrl Pts',(-9.98942327898192,12.2,4.98206674328923));
#250487=CARTESIAN_POINT('Ctrl Pts',(-9.98721717501038,12.2,4.97956048149388));
#250488=CARTESIAN_POINT('Ctrl Pts',(-9.98427570278115,12.2,4.97621879879653));
#250489=CARTESIAN_POINT('Ctrl Pts',(-9.98133764597426,12.2,4.97289169094571));
#250490=CARTESIAN_POINT('Ctrl Pts',(-9.97840311503692,12.2,4.96957917893334));
#250491=CARTESIAN_POINT('Ctrl Pts',(-9.9754685844994,12.2,4.9662666673723));
#250492=CARTESIAN_POINT('Ctrl Pts',(-9.97253758064199,12.2,4.96296875139826));
#250493=CARTESIAN_POINT('Ctrl Pts',(-9.96961021604772,12.2,4.95968544927681));
#250494=CARTESIAN_POINT('Ctrl Pts',(-9.96668285105459,12.2,4.956402146708));
#250495=CARTESIAN_POINT('Ctrl Pts',(-9.96375912597549,12.2,4.95313345996091));
#250496=CARTESIAN_POINT('Ctrl Pts',(-9.96083915355969,12.2,4.94987940651116));
#250497=CARTESIAN_POINT('Ctrl Pts',(-9.95791918154174,12.2,4.94662535350478));
#250498=CARTESIAN_POINT('Ctrl Pts',(-9.95500296341143,12.2,4.94338593498435));
#250499=CARTESIAN_POINT('Ctrl Pts',(-9.95209061420482,12.2,4.94016117024702));
#250500=CARTESIAN_POINT('Ctrl Pts',(-9.9491782646014,12.2,4.93693640507031));
#250501=CARTESIAN_POINT('Ctrl Pts',(-9.94626978436788,12.2,4.93372629432313));
#250502=CARTESIAN_POINT('Ctrl Pts',(-9.94336528748764,12.2,4.93053085570551));
#250503=CARTESIAN_POINT('Ctrl Pts',(-9.94046079100314,12.2,4.92733541752327));
#250504=CARTESIAN_POINT('Ctrl Pts',(-9.93756027922028,12.2,4.9241546534517));
#250505=CARTESIAN_POINT('Ctrl Pts',(-9.93466386914536,12.2,4.92098857971777));
#250506=CARTESIAN_POINT('Ctrl Pts',(-9.93176745867579,12.2,4.91782250555245));
#250507=CARTESIAN_POINT('Ctrl Pts',(-9.92887515015721,12.2,4.91467112236918));
#250508=CARTESIAN_POINT('Ctrl Pts',(-9.92598706072231,12.2,4.91153445097698));
#250509=CARTESIAN_POINT('Ctrl Pts',(-9.92237694912543,12.2,4.90761361195041));
#250510=CARTESIAN_POINT('Ctrl Pts',(-9.91877343208672,12.2,4.90371575691212));
#250511=CARTESIAN_POINT('Ctrl Pts',(-9.91517674028152,12.2,4.89984092378831));
#250512=CARTESIAN_POINT('Ctrl Pts',(-9.91229938707256,12.2,4.89674105754268));
#250513=CARTESIAN_POINT('Ctrl Pts',(-9.90942640292271,12.2,4.89365592495753));
#250514=CARTESIAN_POINT('Ctrl Pts',(-9.90655790762463,12.2,4.89058554322054));
#250515=CARTESIAN_POINT('Ctrl Pts',(-9.90368941193574,12.2,4.88751516106521));
#250516=CARTESIAN_POINT('Ctrl Pts',(-9.90082540561631,12.2,4.88445953088292));
#250517=CARTESIAN_POINT('Ctrl Pts',(-9.89796601001632,12.2,4.88141866971814));
#250518=CARTESIAN_POINT('Ctrl Pts',(-9.89510661480593,12.2,4.87837780896768));
#250519=CARTESIAN_POINT('Ctrl Pts',(-9.89225183031684,12.2,4.87535171950872));
#250520=CARTESIAN_POINT('Ctrl Pts',(-9.88940177921602,12.2,4.87234041597561));
#250521=CARTESIAN_POINT('Ctrl Pts',(-9.88655172772689,12.2,4.86932911203222));
#250522=CARTESIAN_POINT('Ctrl Pts',(-9.88370640882412,12.2,4.86633259688777));
#250523=CARTESIAN_POINT('Ctrl Pts',(-9.88086594848977,12.2,4.86335088498956));
#250524=CARTESIAN_POINT('Ctrl Pts',(-9.87802548854243,12.2,4.86036917349761));
#250525=CARTESIAN_POINT('Ctrl Pts',(-9.8751898846292,12.2,4.85740226664836));
#250526=CARTESIAN_POINT('Ctrl Pts',(-9.87235926347118,12.2,4.85445018299927));
#250527=CARTESIAN_POINT('Ctrl Pts',(-9.86952864192748,12.2,4.85149809894794));
#250528=CARTESIAN_POINT('Ctrl Pts',(-9.86670300225377,12.2,4.84856083656754));
#250529=CARTESIAN_POINT('Ctrl Pts',(-9.8638824707667,12.2,4.84563841324159));
#250530=CARTESIAN_POINT('Ctrl Pts',(-9.86106193927965,12.2,4.84271598991564));
#250531=CARTESIAN_POINT('Ctrl Pts',(-9.85824651567651,12.2,4.83980840642754));
#250532=CARTESIAN_POINT('Ctrl Pts',(-9.85543632752391,12.2,4.83691567849364));
#250533=CARTESIAN_POINT('Ctrl Pts',(-9.85262613975418,12.2,4.83402295095388));
#250534=CARTESIAN_POINT('Ctrl Pts',(-9.84982118770322,12.2,4.83114507926216));
#250535=CARTESIAN_POINT('Ctrl Pts',(-9.84702159865395,12.2,4.82828207971745));
#250536=CARTESIAN_POINT('Ctrl Pts',(-9.84422200922323,12.2,4.82541907978265));
#250537=CARTESIAN_POINT('Ctrl Pts',(-9.84142778443624,12.2,4.82257095292523));
#250538=CARTESIAN_POINT('Ctrl Pts',(-9.83863905281207,12.2,4.81973771479723));
#250539=CARTESIAN_POINT('Ctrl Pts',(-9.83585032156787,12.2,4.81690447705526));
#250540=CARTESIAN_POINT('Ctrl Pts',(-9.83306708325046,12.2,4.81408612842048));
#250541=CARTESIAN_POINT('Ctrl Pts',(-9.83028946947715,12.2,4.81128268470424));
#250542=CARTESIAN_POINT('Ctrl Pts',(-9.8275118553254,12.2,4.80847924060603));
#250543=CARTESIAN_POINT('Ctrl Pts',(-9.82473986614378,12.2,4.8056907007374));
#250544=CARTESIAN_POINT('Ctrl Pts',(-9.82197363271562,12.2,4.80291708153166));
#250545=CARTESIAN_POINT('Ctrl Pts',(-9.81920739966435,12.2,4.80014346270382));
#250546=CARTESIAN_POINT('Ctrl Pts',(-9.81644692315438,12.2,4.79738476540388));
#250547=CARTESIAN_POINT('Ctrl Pts',(-9.81369233607478,12.2,4.79464100365648));
#250548=CARTESIAN_POINT('Ctrl Pts',(-9.81093774861986,12.2,4.79189724153524));
#250549=CARTESIAN_POINT('Ctrl Pts',(-9.80818905172774,12.2,4.78916841633625));
#250550=CARTESIAN_POINT('Ctrl Pts',(-9.80544637896755,12.2,4.78645454174488));
#250551=CARTESIAN_POINT('Ctrl Pts',(-9.80270370658105,12.2,4.78374066752328));
#250552=CARTESIAN_POINT('Ctrl Pts',(-9.79996705950166,12.2,4.78104174589867));
#250553=CARTESIAN_POINT('Ctrl Pts',(-9.79723657194646,12.2,4.77835778967209));
#250554=CARTESIAN_POINT('Ctrl Pts',(-9.79450608401922,12.2,4.77567383307982));
#250555=CARTESIAN_POINT('Ctrl Pts',(-9.79178175649476,12.2,4.77300484354367));
#250556=CARTESIAN_POINT('Ctrl Pts',(-9.78906372772319,12.2,4.77035083549813));
#250557=CARTESIAN_POINT('Ctrl Pts',(-9.78634569932194,12.2,4.7676968278142));
#250558=CARTESIAN_POINT('Ctrl Pts',(-9.78363396844132,12.2,4.76505780059101));
#250559=CARTESIAN_POINT('Ctrl Pts',(-9.78092867471736,12.2,4.7624337696373));
#250560=CARTESIAN_POINT('Ctrl Pts',(-9.77822338062479,12.2,4.75980973832607));
#250561=CARTESIAN_POINT('Ctrl Pts',(-9.77552452243563,12.2,4.75720070283017));
#250562=CARTESIAN_POINT('Ctrl Pts',(-9.77283224173336,12.2,4.75460667746659));
#250563=CARTESIAN_POINT('Ctrl Pts',(-9.7701399610311,12.2,4.75201265210301));
#250564=CARTESIAN_POINT('Ctrl Pts',(-9.76745425691289,12.2,4.74943363704393));
#250565=CARTESIAN_POINT('Ctrl Pts',(-9.76477527154536,12.2,4.7468696450724));
#250566=CARTESIAN_POINT('Ctrl Pts',(-9.76209628654284,12.2,4.7443056534502));
#250567=CARTESIAN_POINT('Ctrl Pts',(-9.75942401948496,12.2,4.74175668549217));
#250568=CARTESIAN_POINT('Ctrl Pts',(-9.75675861446852,12.2,4.73922275574333));
#250569=CARTESIAN_POINT('Ctrl Pts',(-9.75409320908892,12.2,4.73668882564924));
#250570=CARTESIAN_POINT('Ctrl Pts',(-9.75143466434919,12.2,4.73416993233382));
#250571=CARTESIAN_POINT('Ctrl Pts',(-9.74878312631651,12.2,4.73166609036556));
#250572=CARTESIAN_POINT('Ctrl Pts',(-9.7461315886451,12.2,4.72916224873845));
#250573=CARTESIAN_POINT('Ctrl Pts',(-9.74348705671168,12.2,4.72667345742606));
#250574=CARTESIAN_POINT('Ctrl Pts',(-9.74084967648237,12.2,4.72419973046063));
#250575=CARTESIAN_POINT('Ctrl Pts',(-9.73821229589372,12.2,4.72172600315816));
#250576=CARTESIAN_POINT('Ctrl Pts',(-9.73558206665115,12.2,4.71926734034104));
#250577=CARTESIAN_POINT('Ctrl Pts',(-9.73295913787779,12.2,4.71682375292042));
#250578=CARTESIAN_POINT('Ctrl Pts',(-9.7303362094618,12.2,4.71438016583275));
#250579=CARTESIAN_POINT('Ctrl Pts',(-9.72772057998116,12.2,4.71195165667608));
#250580=CARTESIAN_POINT('Ctrl Pts',(-9.72511239847165,12.2,4.7095382357057));
#250581=CARTESIAN_POINT('Ctrl Pts',(-9.72250421660677,12.2,4.70712481440649));
#250582=CARTESIAN_POINT('Ctrl Pts',(-9.71990348435951,12.2,4.70472648207026));
#250583=CARTESIAN_POINT('Ctrl Pts',(-9.71731035049645,12.2,4.70234325133024));
#250584=CARTESIAN_POINT('Ctrl Pts',(-9.71471721698669,12.2,4.69996002091493));
#250585=CARTESIAN_POINT('Ctrl Pts',(-9.71213168215395,12.2,4.6975918915735));
#250586=CARTESIAN_POINT('Ctrl Pts',(-9.70955389912412,12.2,4.69523887509144));
#250587=CARTESIAN_POINT('Ctrl Pts',(-9.7063316700734,12.2,4.69229760424842));
#250588=CARTESIAN_POINT('Ctrl Pts',(-9.7031215524543,12.2,4.68937994657944));
#250589=CARTESIAN_POINT('Ctrl Pts',(-9.69992384696756,12.2,4.68648592664767));
#250590=CARTESIAN_POINT('Ctrl Pts',(-9.69736568243876,12.2,4.68417071057608));
#250591=CARTESIAN_POINT('Ctrl Pts',(-9.69481546253031,12.2,4.68187062146182));
#250592=CARTESIAN_POINT('Ctrl Pts',(-9.69227334205895,12.2,4.67958567083828));
#250593=CARTESIAN_POINT('Ctrl Pts',(-9.68973122193397,12.2,4.67730072052607));
#250594=CARTESIAN_POINT('Ctrl Pts',(-9.68719720153699,12.2,4.67503090911514));
#250595=CARTESIAN_POINT('Ctrl Pts',(-9.68467143861657,12.2,4.67277624601884));
#250596=CARTESIAN_POINT('Ctrl Pts',(-9.68214567535202,12.2,4.67052158261535));
#250597=CARTESIAN_POINT('Ctrl Pts',(-9.6796281706145,12.2,4.66828206941623));
#250598=CARTESIAN_POINT('Ctrl Pts',(-9.67711908281165,12.2,4.66605771485156));
#250599=CARTESIAN_POINT('Ctrl Pts',(-9.67460999535067,12.2,4.66383336058997));
#250600=CARTESIAN_POINT('Ctrl Pts',(-9.67210932478798,12.2,4.66162416605031));
#250601=CARTESIAN_POINT('Ctrl Pts',(-9.66961723265747,12.2,4.65943014161698));
#250602=CARTESIAN_POINT('Ctrl Pts',(-9.66650211723967,12.2,4.65668761085112));
#250603=CARTESIAN_POINT('Ctrl Pts',(-9.66340040553041,12.2,4.65396878306026));
#250604=CARTESIAN_POINT('Ctrl Pts',(-9.6603124166252,12.2,4.65127367556287));
#250605=CARTESIAN_POINT('Ctrl Pts',(-9.65722442771999,12.2,4.64857856806547));
#250606=CARTESIAN_POINT('Ctrl Pts',(-9.65415016075654,12.2,4.64590718313558));
#250607=CARTESIAN_POINT('Ctrl Pts',(-9.65108994040858,12.2,4.64325953743989));
#250608=CARTESIAN_POINT('Ctrl Pts',(-9.64802972006061,12.2,4.6406118917442));
#250609=CARTESIAN_POINT('Ctrl Pts',(-9.64498354620468,12.2,4.63798798645468));
#250610=CARTESIAN_POINT('Ctrl Pts',(-9.64195174669005,12.2,4.63538783666178));
#250611=CARTESIAN_POINT('Ctrl Pts',(-9.63891994717543,12.2,4.63278768686889));
#250612=CARTESIAN_POINT('Ctrl Pts',(-9.63590252153616,12.2,4.6302112946016));
#250613=CARTESIAN_POINT('Ctrl Pts',(-9.63289980368815,12.2,4.62765867543367));
#250614=CARTESIAN_POINT('Ctrl Pts',(-9.62989708584016,12.2,4.62510605626576));
#250615=CARTESIAN_POINT('Ctrl Pts',(-9.62690907497074,12.2,4.62257720967385));
#250616=CARTESIAN_POINT('Ctrl Pts',(-9.62393610898497,12.2,4.62007215146796));
#250617=CARTESIAN_POINT('Ctrl Pts',(-9.62096314299921,12.2,4.61756709326207));
#250618=CARTESIAN_POINT('Ctrl Pts',(-9.61800522399446,12.2,4.61508582460547));
#250619=CARTESIAN_POINT('Ctrl Pts',(-9.61506269225835,12.2,4.61262835800825));
#250620=CARTESIAN_POINT('Ctrl Pts',(-9.61212016052223,12.2,4.61017089141103));
#250621=CARTESIAN_POINT('Ctrl Pts',(-9.60919301760605,12.2,4.60773722721505));
#250622=CARTESIAN_POINT('Ctrl Pts',(-9.60628161002344,12.2,4.60532737977362));
#250623=CARTESIAN_POINT('Ctrl Pts',(-9.60337020244082,12.2,4.60291753233219));
#250624=CARTESIAN_POINT('Ctrl Pts',(-9.60047453321649,12.2,4.60053150107767));
#250625=CARTESIAN_POINT('Ctrl Pts',(-9.59759495307845,12.2,4.59816929857892));
#250626=CARTESIAN_POINT('Ctrl Pts',(-9.59413945703836,12.2,4.59533465568341));
#250627=CARTESIAN_POINT('Ctrl Pts',(-9.5907071310214,12.2,4.59253432616847));
#250628=CARTESIAN_POINT('Ctrl Pts',(-9.58729859422755,12.2,4.58976832943415));
#250629=CARTESIAN_POINT('Ctrl Pts',(-9.58445814679615,12.2,4.5874633320718));
#250630=CARTESIAN_POINT('Ctrl Pts',(-9.58163422345882,12.2,4.58518217677261));
#250631=CARTESIAN_POINT('Ctrl Pts',(-9.57882718525156,12.2,4.58292487502617));
#250632=CARTESIAN_POINT('Ctrl Pts',(-9.5760201470443,12.2,4.58066757327973));
#250633=CARTESIAN_POINT('Ctrl Pts',(-9.57322999686115,12.2,4.57843412378882));
#250634=CARTESIAN_POINT('Ctrl Pts',(-9.57045710595835,12.2,4.57622453552492));
#250635=CARTESIAN_POINT('Ctrl Pts',(-9.56768421505556,12.2,4.57401494726103));
#250636=CARTESIAN_POINT('Ctrl Pts',(-9.56492858381089,12.2,4.57182922107515));
#250637=CARTESIAN_POINT('Ctrl Pts',(-9.56219058879852,12.2,4.56966736523208));
#250638=CARTESIAN_POINT('Ctrl Pts',(-9.55945259378616,12.2,4.56750550938902));
#250639=CARTESIAN_POINT('Ctrl Pts',(-9.55673223472799,12.2,4.56536752229944));
#250640=CARTESIAN_POINT('Ctrl Pts',(-9.5540298972984,12.2,4.56325341237014));
#250641=CARTESIAN_POINT('Ctrl Pts',(-9.55132755986879,12.2,4.56113930244085));
#250642=CARTESIAN_POINT('Ctrl Pts',(-9.54864324310258,12.2,4.55904906940256));
#250643=CARTESIAN_POINT('Ctrl Pts',(-9.54597733657577,12.2,4.55698271863993));
#250644=CARTESIAN_POINT('Ctrl Pts',(-9.54331143004894,12.2,4.55491636787729));
#250645=CARTESIAN_POINT('Ctrl Pts',(-9.54066393414717,12.2,4.55287389995932));
#250646=CARTESIAN_POINT('Ctrl Pts',(-9.53803524741992,12.2,4.55085531979068));
#250647=CARTESIAN_POINT('Ctrl Pts',(-9.53488082346185,12.2,4.54843302367633));
#250648=CARTESIAN_POINT('Ctrl Pts',(-9.53175348014572,12.2,4.54604512424774));
#250649=CARTESIAN_POINT('Ctrl Pts',(-9.52865391950833,12.2,4.54369162849992));
#250650=CARTESIAN_POINT('Ctrl Pts',(-9.52555435887095,12.2,4.54133813275209));
#250651=CARTESIAN_POINT('Ctrl Pts',(-9.52248257734592,12.2,4.53901904106248));
#250652=CARTESIAN_POINT('Ctrl Pts',(-9.51943929155281,12.2,4.53673435594602));
#250653=CARTESIAN_POINT('Ctrl Pts',(-9.51639600548326,12.2,4.53444967062206));
#250654=CARTESIAN_POINT('Ctrl Pts',(-9.51338121385195,12.2,4.53219939161014));
#250655=CARTESIAN_POINT('Ctrl Pts',(-9.51039564319125,12.2,4.52998352049174));
#250656=CARTESIAN_POINT('Ctrl Pts',(-9.50741007280173,12.2,4.5277676495746));
#250657=CARTESIAN_POINT('Ctrl Pts',(-9.50445372583058,12.2,4.52558618552228));
#250658=CARTESIAN_POINT('Ctrl Pts',(-9.50152734350701,12.2,4.52343912750728));
#250659=CARTESIAN_POINT('Ctrl Pts',(-9.49860096118344,12.2,4.52129206949229));
#250660=CARTESIAN_POINT('Ctrl Pts',(-9.49570454563684,12.2,4.51917941561431));
#250661=CARTESIAN_POINT('Ctrl Pts',(-9.49283885440628,12.2,4.51710116360498));
#250662=CARTESIAN_POINT('Ctrl Pts',(-9.48997316291541,12.2,4.51502291140687));
#250663=CARTESIAN_POINT('Ctrl Pts',(-9.48713819687841,12.2,4.5129790597214));
#250664=CARTESIAN_POINT('Ctrl Pts',(-9.48433473422776,12.2,4.5109695997809));
#250665=CARTESIAN_POINT('Ctrl Pts',(-9.48106402818397,12.2,4.50862523012409));
#250666=CARTESIAN_POINT('Ctrl Pts',(-9.47783619900219,12.2,4.5063276748001));
#250667=CARTESIAN_POINT('Ctrl Pts',(-9.47465251140719,12.2,4.50407691360521));
#250668=CARTESIAN_POINT('Ctrl Pts',(-9.47192363600705,12.2,4.50214768949858));
#250669=CARTESIAN_POINT('Ctrl Pts',(-9.46922719105261,12.2,4.50025284604621));
#250670=CARTESIAN_POINT('Ctrl Pts',(-9.46656399274305,12.2,4.49839236778048));
#250671=CARTESIAN_POINT('Ctrl Pts',(-9.4639007946754,12.2,4.49653188968374));
#250672=CARTESIAN_POINT('Ctrl Pts',(-9.46127084262453,12.2,4.49470577740873));
#250673=CARTESIAN_POINT('Ctrl Pts',(-9.45867497245716,12.2,4.49291401346578));
#250674=CARTESIAN_POINT('Ctrl Pts',(-9.45607910228978,12.2,4.49112224952284));
#250675=CARTESIAN_POINT('Ctrl Pts',(-9.45351731293923,12.2,4.48936483389953));
#250676=CARTESIAN_POINT('Ctrl Pts',(-9.45099045911286,12.2,4.48764174679398));
#250677=CARTESIAN_POINT('Ctrl Pts',(-9.44846360505695,12.2,4.4859186595319));
#250678=CARTESIAN_POINT('Ctrl Pts',(-9.44597168780536,12.2,4.48422990015743));
#250679=CARTESIAN_POINT('Ctrl Pts',(-9.44351558175729,12.2,4.4825754430696));
#250680=CARTESIAN_POINT('Ctrl Pts',(-9.44105947593231,12.2,4.48092098613205));
#250681=CARTESIAN_POINT('Ctrl Pts',(-9.43863918119872,12.2,4.47930083417953));
#250682=CARTESIAN_POINT('Ctrl Pts',(-9.43625559462024,12.2,4.4777149571553));
#250683=CARTESIAN_POINT('Ctrl Pts',(-9.43387200804177,12.2,4.47612908013107));
#250684=CARTESIAN_POINT('Ctrl Pts',(-9.43152513216872,12.2,4.47457748039578));
#250685=CARTESIAN_POINT('Ctrl Pts',(-9.42921588266767,12.2,4.47306012528276));
#250686=CARTESIAN_POINT('Ctrl Pts',(-9.42690663316663,12.2,4.47154277016975));
#250687=CARTESIAN_POINT('Ctrl Pts',(-9.42463501200656,12.2,4.47005965847421));
#250688=CARTESIAN_POINT('Ctrl Pts',(-9.42240196350173,12.2,4.46861075819119));
#250689=CARTESIAN_POINT('Ctrl Pts',(-9.42016891479406,12.2,4.46716185777656));
#250690=CARTESIAN_POINT('Ctrl Pts',(-9.41797443730677,12.2,4.46574716614859));
#250691=CARTESIAN_POINT('Ctrl Pts',(-9.41581950060771,12.2,4.46436664590817));
#250692=CARTESIAN_POINT('Ctrl Pts',(-9.41366456410439,12.2,4.46298612579314));
#250693=CARTESIAN_POINT('Ctrl Pts',(-9.4115491671934,12.2,4.46163977636722));
#250694=CARTESIAN_POINT('Ctrl Pts',(-9.40947430400926,12.2,4.46032755599219));
#250695=CARTESIAN_POINT('Ctrl Pts',(-9.40739944082513,12.2,4.45901533561715));
#250696=CARTESIAN_POINT('Ctrl Pts',(-9.40536511283097,12.2,4.45773724225932));
#250697=CARTESIAN_POINT('Ctrl Pts',(-9.40337233973387,12.2,4.45649323013553));
#250698=CARTESIAN_POINT('Ctrl Pts',(-9.40137956645577,12.2,4.45524921789875));
#250699=CARTESIAN_POINT('Ctrl Pts',(-9.39942834904569,12.2,4.45403928799046));
#250700=CARTESIAN_POINT('Ctrl Pts',(-9.39751973584878,12.2,4.45286338586959));
#250701=CARTESIAN_POINT('Ctrl Pts',(-9.39561112282524,12.2,4.45168748385553));
#250702=CARTESIAN_POINT('Ctrl Pts',(-9.3937451149421,12.2,4.450545611718));
#250703=CARTESIAN_POINT('Ctrl Pts',(-9.3919227912583,12.2,4.44943771350825));
#250704=CARTESIAN_POINT('Ctrl Pts',(-9.3901004675745,12.2,4.4483298152985));
#250705=CARTESIAN_POINT('Ctrl Pts',(-9.38832182911902,12.2,4.44725589135841));
#250706=CARTESIAN_POINT('Ctrl Pts',(-9.38658798534282,12.2,4.44621587909229));
#250707=CARTESIAN_POINT('Ctrl Pts',(-9.38485414140911,12.2,4.4451758667317));
#250708=CARTESIAN_POINT('Ctrl Pts',(-9.38316509182396,12.2,4.44416976661963));
#250709=CARTESIAN_POINT('Ctrl Pts',(-9.38152198207089,12.2,4.44319751515229));
#250710=CARTESIAN_POINT('Ctrl Pts',(-9.37988675819392,12.2,4.44222992987028));
#250711=CARTESIAN_POINT('Ctrl Pts',(-9.37829702764554,12.2,4.44129586542554));
#250712=CARTESIAN_POINT('Ctrl Pts',(-9.37675396800006,12.2,4.44039525799998));
#250713=CARTESIAN_POINT('Ctrl Pts',(-9.37675396800006,15.2,4.44039525799998));
#250714=CARTESIAN_POINT('Ctrl Pts',(-9.37829702764554,15.2,4.44129586542555));
#250715=CARTESIAN_POINT('Ctrl Pts',(-9.3798867581939,15.2,4.44222992987026));
#250716=CARTESIAN_POINT('Ctrl Pts',(-9.38152198207088,15.2,4.44319751515229));
#250717=CARTESIAN_POINT('Ctrl Pts',(-9.38316509182397,15.2,4.44416976661963));
#250718=CARTESIAN_POINT('Ctrl Pts',(-9.3848541414091,15.2,4.44517586673169));
#250719=CARTESIAN_POINT('Ctrl Pts',(-9.38658798534282,15.2,4.44621587909228));
#250720=CARTESIAN_POINT('Ctrl Pts',(-9.38832182911903,15.2,4.44725589135842));
#250721=CARTESIAN_POINT('Ctrl Pts',(-9.39010046757452,15.2,4.44832981529852));
#250722=CARTESIAN_POINT('Ctrl Pts',(-9.39192279125831,15.2,4.44943771350825));
#250723=CARTESIAN_POINT('Ctrl Pts',(-9.39374511494208,15.2,4.45054561171799));
#250724=CARTESIAN_POINT('Ctrl Pts',(-9.39561112282524,15.2,4.45168748385554));
#250725=CARTESIAN_POINT('Ctrl Pts',(-9.39751973584878,15.2,4.45286338586959));
#250726=CARTESIAN_POINT('Ctrl Pts',(-9.39942834904569,15.2,4.45403928799045));
#250727=CARTESIAN_POINT('Ctrl Pts',(-9.40137956645577,15.2,4.45524921789875));
#250728=CARTESIAN_POINT('Ctrl Pts',(-9.40337233973387,15.2,4.45649323013553));
#250729=CARTESIAN_POINT('Ctrl Pts',(-9.40569724162016,15.2,4.45794457757562));
#250730=CARTESIAN_POINT('Ctrl Pts',(-9.40807870360857,15.2,4.45944231251553));
#250731=CARTESIAN_POINT('Ctrl Pts',(-9.41051510879806,15.2,4.4609865103553));
#250732=CARTESIAN_POINT('Ctrl Pts',(-9.41260345634723,15.2,4.46231010865826));
#250733=CARTESIAN_POINT('Ctrl Pts',(-9.41473216945717,15.2,4.46366784207347));
#250734=CARTESIAN_POINT('Ctrl Pts',(-9.41690025999465,15.2,4.46505975415165));
#250735=CARTESIAN_POINT('Ctrl Pts',(-9.41906835033522,15.2,4.4664516661034));
#250736=CARTESIAN_POINT('Ctrl Pts',(-9.42127581723067,15.2,4.46787775468028));
#250737=CARTESIAN_POINT('Ctrl Pts',(-9.42352169774268,15.2,4.46933805896726));
#250738=CARTESIAN_POINT('Ctrl Pts',(-9.42576757825471,15.2,4.47079836325424));
#250739=CARTESIAN_POINT('Ctrl Pts',(-9.42805187253462,15.2,4.47229288560713));
#250740=CARTESIAN_POINT('Ctrl Pts',(-9.43037363836528,15.2,4.47382165671675));
#250741=CARTESIAN_POINT('Ctrl Pts',(-9.43269540440684,15.2,4.47535042796524));
#250742=CARTESIAN_POINT('Ctrl Pts',(-9.43505464471141,15.2,4.47691344918465));
#250743=CARTESIAN_POINT('Ctrl Pts',(-9.43745044351114,15.2,4.47851075244071));
#250744=CARTESIAN_POINT('Ctrl Pts',(-9.43984624209325,15.2,4.48010805555168));
#250745=CARTESIAN_POINT('Ctrl Pts',(-9.4422785964561,15.2,4.4817396391749));
#250746=CARTESIAN_POINT('Ctrl Pts',(-9.44474661536798,15.2,4.48340553036586));
#250747=CARTESIAN_POINT('Ctrl Pts',(-9.44721463427987,15.2,4.48507142155683));
#250748=CARTESIAN_POINT('Ctrl Pts',(-9.44971831756386,15.2,4.48677162025337));
#250749=CARTESIAN_POINT('Ctrl Pts',(-9.45225679338679,15.2,4.48850615118887));
#250750=CARTESIAN_POINT('Ctrl Pts',(-9.45479526920973,15.2,4.49024068212436));
#250751=CARTESIAN_POINT('Ctrl Pts',(-9.45736853522953,15.2,4.49200954390456));
#250752=CARTESIAN_POINT('Ctrl Pts',(-9.45997574396582,15.2,4.49381275783672));
#250753=CARTESIAN_POINT('Ctrl Pts',(-9.46258295293895,15.2,4.49561597193267));
#250754=CARTESIAN_POINT('Ctrl Pts',(-9.46522410139869,15.2,4.49745353707357));
#250755=CARTESIAN_POINT('Ctrl Pts',(-9.46789835887921,15.2,4.49932547109375));
#250756=CARTESIAN_POINT('Ctrl Pts',(-9.47057261611682,15.2,4.5011974049439));
#250757=CARTESIAN_POINT('Ctrl Pts',(-9.47327998429347,15.2,4.50310370639134));
#250758=CARTESIAN_POINT('Ctrl Pts',(-9.47601964760915,15.2,4.50504439040263));
#250759=CARTESIAN_POINT('Ctrl Pts',(-9.47875931092484,15.2,4.50698507441393));
#250760=CARTESIAN_POINT('Ctrl Pts',(-9.48153127183176,15.2,4.50896014002292));
#250761=CARTESIAN_POINT('Ctrl Pts',(-9.48433473422776,15.2,4.5109695997809));
#250762=CARTESIAN_POINT('Ctrl Pts',(-9.48713819687842,15.2,4.5129790597214));
#250763=CARTESIAN_POINT('Ctrl Pts',(-9.48997316291541,15.2,4.51502291140688));
#250764=CARTESIAN_POINT('Ctrl Pts',(-9.49283885440631,15.2,4.517101163605));
#250765=CARTESIAN_POINT('Ctrl Pts',(-9.4957045456369,15.2,4.51917941561435));
#250766=CARTESIAN_POINT('Ctrl Pts',(-9.49860096118346,15.2,4.52129206949231));
#250767=CARTESIAN_POINT('Ctrl Pts',(-9.50152734350701,15.2,4.52343912750729));
#250768=CARTESIAN_POINT('Ctrl Pts',(-9.50445372583056,15.2,4.52558618552227));
#250769=CARTESIAN_POINT('Ctrl Pts',(-9.5074100728017,15.2,4.52776764957458));
#250770=CARTESIAN_POINT('Ctrl Pts',(-9.51039564319125,15.2,4.52998352049174));
#250771=CARTESIAN_POINT('Ctrl Pts',(-9.51338121385199,15.2,4.53219939161017));
#250772=CARTESIAN_POINT('Ctrl Pts',(-9.51639600548326,15.2,4.53444967062205));
#250773=CARTESIAN_POINT('Ctrl Pts',(-9.51943929155281,15.2,4.53673435594603));
#250774=CARTESIAN_POINT('Ctrl Pts',(-9.52248257734592,15.2,4.53901904106248));
#250775=CARTESIAN_POINT('Ctrl Pts',(-9.52555435887099,15.2,4.54133813275212));
#250776=CARTESIAN_POINT('Ctrl Pts',(-9.52865391950834,15.2,4.54369162849992));
#250777=CARTESIAN_POINT('Ctrl Pts',(-9.53175348014569,15.2,4.54604512424771));
#250778=CARTESIAN_POINT('Ctrl Pts',(-9.53488082346189,15.2,4.54843302367636));
#250779=CARTESIAN_POINT('Ctrl Pts',(-9.53803524741992,15.2,4.55085531979068));
#250780=CARTESIAN_POINT('Ctrl Pts',(-9.54066393414713,15.2,4.5528738999593));
#250781=CARTESIAN_POINT('Ctrl Pts',(-9.54331143004896,15.2,4.55491636787731));
#250782=CARTESIAN_POINT('Ctrl Pts',(-9.54597733657577,15.2,4.55698271863993));
#250783=CARTESIAN_POINT('Ctrl Pts',(-9.54864324310257,15.2,4.55904906940256));
#250784=CARTESIAN_POINT('Ctrl Pts',(-9.55132755986875,15.2,4.56113930244082));
#250785=CARTESIAN_POINT('Ctrl Pts',(-9.55402989729839,15.2,4.56325341237013));
#250786=CARTESIAN_POINT('Ctrl Pts',(-9.556732234728,15.2,4.56536752229945));
#250787=CARTESIAN_POINT('Ctrl Pts',(-9.55945259378614,15.2,4.567505509389));
#250788=CARTESIAN_POINT('Ctrl Pts',(-9.56219058879852,15.2,4.56966736523208));
#250789=CARTESIAN_POINT('Ctrl Pts',(-9.5649285838109,15.2,4.57182922107516));
#250790=CARTESIAN_POINT('Ctrl Pts',(-9.56768421505557,15.2,4.57401494726103));
#250791=CARTESIAN_POINT('Ctrl Pts',(-9.57045710595835,15.2,4.57622453552492));
#250792=CARTESIAN_POINT('Ctrl Pts',(-9.57322999686113,15.2,4.57843412378881));
#250793=CARTESIAN_POINT('Ctrl Pts',(-9.57602014704429,15.2,4.58066757327972));
#250794=CARTESIAN_POINT('Ctrl Pts',(-9.57882718525154,15.2,4.58292487502616));
#250795=CARTESIAN_POINT('Ctrl Pts',(-9.58275703880289,15.2,4.58608509752038));
#250796=CARTESIAN_POINT('Ctrl Pts',(-9.58671998870917,15.2,4.58929207286161));
#250797=CARTESIAN_POINT('Ctrl Pts',(-9.5907150381066,15.2,4.59254576955392));
#250798=CARTESIAN_POINT('Ctrl Pts',(-9.59356864477462,15.2,4.59486983858366));
#250799=CARTESIAN_POINT('Ctrl Pts',(-9.59643862780398,15.2,4.59721774655266));
#250800=CARTESIAN_POINT('Ctrl Pts',(-9.59932462961084,15.2,4.59958947981849));
#250801=CARTESIAN_POINT('Ctrl Pts',(-9.60221063110313,15.2,4.6019612128258));
#250802=CARTESIAN_POINT('Ctrl Pts',(-9.60511265215992,15.2,4.60435677266025));
#250803=CARTESIAN_POINT('Ctrl Pts',(-9.6080303396184,15.2,4.60677614565849));
#250804=CARTESIAN_POINT('Ctrl Pts',(-9.6109480273949,15.2,4.60919551892044));
#250805=CARTESIAN_POINT('Ctrl Pts',(-9.61388138179336,15.2,4.61163870707363));
#250806=CARTESIAN_POINT('Ctrl Pts',(-9.61683005463933,15.2,4.61410569366892));
#250807=CARTESIAN_POINT('Ctrl Pts',(-9.6197787274853,15.2,4.61657268026419));
#250808=CARTESIAN_POINT('Ctrl Pts',(-9.62274272011203,15.2,4.61906346794525));
#250809=CARTESIAN_POINT('Ctrl Pts',(-9.62572169116259,15.2,4.62157804049978));
#250810=CARTESIAN_POINT('Ctrl Pts',(-9.62870066221316,15.2,4.62409261305431));
#250811=CARTESIAN_POINT('Ctrl Pts',(-9.63169460858744,15.2,4.62663097110597));
#250812=CARTESIAN_POINT('Ctrl Pts',(-9.63470319629502,15.2,4.62919309929918));
#250813=CARTESIAN_POINT('Ctrl Pts',(-9.63771178400259,15.2,4.63175522749239));
#250814=CARTESIAN_POINT('Ctrl Pts',(-9.64073501212998,15.2,4.63434112531953));
#250815=CARTESIAN_POINT('Ctrl Pts',(-9.64377254830979,15.2,4.63695077684606));
#250816=CARTESIAN_POINT('Ctrl Pts',(-9.64681008448958,15.2,4.63956042837259));
#250817=CARTESIAN_POINT('Ctrl Pts',(-9.64986192876144,15.2,4.64219383236642));
#250818=CARTESIAN_POINT('Ctrl Pts',(-9.65292775556627,15.2,4.64485097305962));
#250819=CARTESIAN_POINT('Ctrl Pts',(-9.6559935823711,15.2,4.64750811375284));
#250820=CARTESIAN_POINT('Ctrl Pts',(-9.65907338836212,15.2,4.65018899106402));
#250821=CARTESIAN_POINT('Ctrl Pts',(-9.66216685372334,15.2,4.65289358600679));
#250822=CARTESIAN_POINT('Ctrl Pts',(-9.66526031908456,15.2,4.65559818094955));
#250823=CARTESIAN_POINT('Ctrl Pts',(-9.6683674429778,15.2,4.65832649205549));
#250824=CARTESIAN_POINT('Ctrl Pts',(-9.67148790749169,15.2,4.66107850420826));
#250825=CARTESIAN_POINT('Ctrl Pts',(-9.67398427923885,15.2,4.66328011405047));
#250826=CARTESIAN_POINT('Ctrl Pts',(-9.67648918842313,15.2,4.66549688995556));
#250827=CARTESIAN_POINT('Ctrl Pts',(-9.67900247489428,15.2,4.66772882335652));
#250828=CARTESIAN_POINT('Ctrl Pts',(-9.681515761023,15.2,4.66996075645338));
#250829=CARTESIAN_POINT('Ctrl Pts',(-9.68403742440756,15.2,4.672207846612));
#250830=CARTESIAN_POINT('Ctrl Pts',(-9.68656730648997,15.2,4.67447008354838));
#250831=CARTESIAN_POINT('Ctrl Pts',(-9.68909718891707,15.2,4.676732320793));
#250832=CARTESIAN_POINT('Ctrl Pts',(-9.69163528862952,15.2,4.67900970358161));
#250833=CARTESIAN_POINT('Ctrl Pts',(-9.694181449158,15.2,4.68130222237477));
#250834=CARTESIAN_POINT('Ctrl Pts',(-9.69672760933955,15.2,4.68359474085557));
#250835=CARTESIAN_POINT('Ctrl Pts',(-9.69928183023395,15.2,4.68590239560939));
#250836=CARTESIAN_POINT('Ctrl Pts',(-9.70184395702398,15.2,4.68822517458518));
#250837=CARTESIAN_POINT('Ctrl Pts',(-9.70568714738355,15.2,4.69170934320709));
#250838=CARTESIAN_POINT('Ctrl Pts',(-9.70954812271937,15.2,4.6952275423941));
#250839=CARTESIAN_POINT('Ctrl Pts',(-9.7134263680773,15.2,4.69877973209607));
#250840=CARTESIAN_POINT('Ctrl Pts',(-9.71601186521744,15.2,4.70114785877916));
#250841=CARTESIAN_POINT('Ctrl Pts',(-9.71860503678607,15.2,4.70353109272755));
#250842=CARTESIAN_POINT('Ctrl Pts',(-9.72120573148336,15.2,4.70592942202492));
#250843=CARTESIAN_POINT('Ctrl Pts',(-9.72380642618065,15.2,4.7083277513223));
#250844=CARTESIAN_POINT('Ctrl Pts',(-9.72641464608994,15.2,4.71074117566034));
#250845=CARTESIAN_POINT('Ctrl Pts',(-9.72903023867769,15.2,4.71316968240533));
#250846=CARTESIAN_POINT('Ctrl Pts',(-9.73295362720292,15.2,4.71681244219195));
#250847=CARTESIAN_POINT('Ctrl Pts',(-9.73689360595874,15.2,4.72048913984397));
#250848=CARTESIAN_POINT('Ctrl Pts',(-9.74084967648236,15.2,4.72419973046063));
#250849=CARTESIAN_POINT('Ctrl Pts',(-9.74348705671167,15.2,4.72667345742605));
#250850=CARTESIAN_POINT('Ctrl Pts',(-9.74613158864511,15.2,4.72916224873846));
#250851=CARTESIAN_POINT('Ctrl Pts',(-9.7487831263165,15.2,4.73166609036555));
#250852=CARTESIAN_POINT('Ctrl Pts',(-9.7520975486767,15.2,4.73479589265528));
#250853=CARTESIAN_POINT('Ctrl Pts',(-9.75542291826356,15.2,4.73794921211305));
#250854=CARTESIAN_POINT('Ctrl Pts',(-9.7587589523878,15.2,4.74112602213122));
#250855=CARTESIAN_POINT('Ctrl Pts',(-9.76142777983264,15.2,4.74366747028427));
#250856=CARTESIAN_POINT('Ctrl Pts',(-9.76410343274775,15.2,4.74622395353028));
#250857=CARTESIAN_POINT('Ctrl Pts',(-9.76678576872771,15.2,4.74879545622696));
#250858=CARTESIAN_POINT('Ctrl Pts',(-9.76946810434219,15.2,4.75136695857326));
#250859=CARTESIAN_POINT('Ctrl Pts',(-9.77215712253867,15.2,4.75395348077768));
#250860=CARTESIAN_POINT('Ctrl Pts',(-9.77485268281764,15.2,4.75655501034124));
#250861=CARTESIAN_POINT('Ctrl Pts',(-9.77754824346387,15.2,4.75915654025926));
#250862=CARTESIAN_POINT('Ctrl Pts',(-9.78025034541972,15.2,4.76177307568519));
#250863=CARTESIAN_POINT('Ctrl Pts',(-9.78295884946855,15.2,4.76440460428506));
#250864=CARTESIAN_POINT('Ctrl Pts',(-9.78566735314835,15.2,4.76703613252638));
#250865=CARTESIAN_POINT('Ctrl Pts',(-9.78838225825046,15.2,4.76968265219224));
#250866=CARTESIAN_POINT('Ctrl Pts',(-9.79110342780512,15.2,4.77234414980644));
#250867=CARTESIAN_POINT('Ctrl Pts',(-9.79382459773054,15.2,4.77500564778328));
#250868=CARTESIAN_POINT('Ctrl Pts',(-9.7965520311705,15.2,4.77768212387824));
#250869=CARTESIAN_POINT('Ctrl Pts',(-9.7992855900417,15.2,4.78037356252493));
#250870=CARTESIAN_POINT('Ctrl Pts',(-9.80270253844448,15.2,4.78373786064993));
#250871=CARTESIAN_POINT('Ctrl Pts',(-9.80612906059742,15.2,4.78712553838071));
#250872=CARTESIAN_POINT('Ctrl Pts',(-9.80956488971024,15.2,4.79053656499345));
#250873=CARTESIAN_POINT('Ctrl Pts',(-9.81300071882306,15.2,4.7939475916062));
#250874=CARTESIAN_POINT('Ctrl Pts',(-9.81644585559219,15.2,4.79738196916389));
#250875=CARTESIAN_POINT('Ctrl Pts',(-9.81990003955099,15.2,4.80083966569287));
#250876=CARTESIAN_POINT('Ctrl Pts',(-9.82266338649212,15.2,4.80360582268993));
#250877=CARTESIAN_POINT('Ctrl Pts',(-9.82543252121545,15.2,4.80638690496179));
#250878=CARTESIAN_POINT('Ctrl Pts',(-9.82820731482136,15.2,4.80918289584279));
#250879=CARTESIAN_POINT('Ctrl Pts',(-9.83306320410427,15.2,4.81407588036073));
#250880=CARTESIAN_POINT('Ctrl Pts',(-9.83793641703867,15.2,4.81901452242558));
#250881=CARTESIAN_POINT('Ctrl Pts',(-9.84282625420647,15.2,4.82399873699799));
#250882=CARTESIAN_POINT('Ctrl Pts',(-9.84701754298989,15.2,4.82827092069546));
#250883=CARTESIAN_POINT('Ctrl Pts',(-9.85122104567787,15.2,4.83257658698693));
#250884=CARTESIAN_POINT('Ctrl Pts',(-9.8554363275239,15.2,4.83691567849363));
#250885=CARTESIAN_POINT('Ctrl Pts',(-9.8589490625232,15.2,4.84053158821392));
#250886=CARTESIAN_POINT('Ctrl Pts',(-9.86246997779467,15.2,4.84417071005058));
#250887=CARTESIAN_POINT('Ctrl Pts',(-9.86599882453013,15.2,4.84783301227091));
#250888=CARTESIAN_POINT('Ctrl Pts',(-9.86882190207234,15.2,4.85076285420684));
#250889=CARTESIAN_POINT('Ctrl Pts',(-9.87165005635413,15.2,4.85370752984939));
#250890=CARTESIAN_POINT('Ctrl Pts',(-9.87448316124364,15.2,4.85666702446861));
#250891=CARTESIAN_POINT('Ctrl Pts',(-9.87731626574712,15.2,4.8596265186846));
#250892=CARTESIAN_POINT('Ctrl Pts',(-9.88015432054869,15.2,4.86260083153209));
#250893=CARTESIAN_POINT('Ctrl Pts',(-9.88299720226023,15.2,4.86558994378622));
#250894=CARTESIAN_POINT('Ctrl Pts',(-9.88726152540856,15.2,4.8700736127783));
#250895=CARTESIAN_POINT('Ctrl Pts',(-9.8915367060163,15.2,4.87459058332362));
#250896=CARTESIAN_POINT('Ctrl Pts',(-9.89582233025032,15.2,4.87914079448973));
#250897=CARTESIAN_POINT('Ctrl Pts',(-9.89867941268372,15.2,4.88217426818715));
#250898=CARTESIAN_POINT('Ctrl Pts',(-9.90154113636733,15.2,4.8852225170903));
#250899=CARTESIAN_POINT('Ctrl Pts',(-9.90440737910916,15.2,4.88828552204722));
#250900=CARTESIAN_POINT('Ctrl Pts',(-9.90799018282933,15.2,4.89211427855635));
#250901=CARTESIAN_POINT('Ctrl Pts',(-9.91158004847632,15.2,4.89596609066453));
#250902=CARTESIAN_POINT('Ctrl Pts',(-9.91517674028152,15.2,4.89984092378832));
#250903=CARTESIAN_POINT('Ctrl Pts',(-9.91805409388249,15.2,4.90294079045629));
#250904=CARTESIAN_POINT('Ctrl Pts',(-9.92093581668955,15.2,4.90605539125659));
#250905=CARTESIAN_POINT('Ctrl Pts',(-9.92382178773601,15.2,4.90918470653923));
#250906=CARTESIAN_POINT('Ctrl Pts',(-9.92670775838926,15.2,4.91231402139548));
#250907=CARTESIAN_POINT('Ctrl Pts',(-9.92959797965857,15.2,4.91545805128225));
#250908=CARTESIAN_POINT('Ctrl Pts',(-9.93249233162174,15.2,4.91861677829165));
#250909=CARTESIAN_POINT('Ctrl Pts',(-9.93538668397927,15.2,4.92177550573144));
#250910=CARTESIAN_POINT('Ctrl Pts',(-9.93828516750391,15.2,4.92494892914987));
#250911=CARTESIAN_POINT('Ctrl Pts',(-9.94118766449569,15.2,4.92813702926903));
#250912=CARTESIAN_POINT('Ctrl Pts',(-9.944090161092,15.2,4.93132512895381));
#250913=CARTESIAN_POINT('Ctrl Pts',(-9.94699667153751,15.2,4.93452790826895));
#250914=CARTESIAN_POINT('Ctrl Pts',(-9.94990707879919,15.2,4.93774534394889));
#250915=CARTESIAN_POINT('Ctrl Pts',(-9.9535450881737,15.2,4.94176713887758));
#250916=CARTESIAN_POINT('Ctrl Pts',(-9.95718918823886,15.2,4.94581183992065));
#250917=CARTESIAN_POINT('Ctrl Pts',(-9.96083915355969,15.2,4.94987940651116));
#250918=CARTESIAN_POINT('Ctrl Pts',(-9.96375912597549,15.2,4.95313345996091));
#250919=CARTESIAN_POINT('Ctrl Pts',(-9.9666828510546,15.2,4.95640214670801));
#250920=CARTESIAN_POINT('Ctrl Pts',(-9.96961021604772,15.2,4.95968544927682));
#250921=CARTESIAN_POINT('Ctrl Pts',(-9.97253758064199,15.2,4.96296875139826));
#250922=CARTESIAN_POINT('Ctrl Pts',(-9.97546858449939,15.2,4.9662666673723));
#250923=CARTESIAN_POINT('Ctrl Pts',(-9.97840311503691,15.2,4.96957917893333));
#250924=CARTESIAN_POINT('Ctrl Pts',(-9.9828049114429,15.2,4.97454794695188));
#250925=CARTESIAN_POINT('Ctrl Pts',(-9.98721464184885,15.2,4.97954955540924));
#250926=CARTESIAN_POINT('Ctrl Pts',(-9.99163192964405,15.2,4.98458393477036));
#250927=CARTESIAN_POINT('Ctrl Pts',(-9.99384057334103,15.2,4.98710112422227));
#250928=CARTESIAN_POINT('Ctrl Pts',(-9.99605110715477,15.2,4.98962650716755));
#250929=CARTESIAN_POINT('Ctrl Pts',(-9.99826348224122,15.2,4.99216007349289));
#250930=CARTESIAN_POINT('Ctrl Pts',(-10.0004758573277,15.2,4.99469363981823));
#250931=CARTESIAN_POINT('Ctrl Pts',(-10.0026900749972,15.2,4.99723539054256));
#250932=CARTESIAN_POINT('Ctrl Pts',(-10.0049060890417,15.2,4.9997853177416));
#250933=CARTESIAN_POINT('Ctrl Pts',(-10.0071221030862,15.2,5.00233524494063));
#250934=CARTESIAN_POINT('Ctrl Pts',(-10.0093399131889,15.2,5.00489334744764));
#250935=CARTESIAN_POINT('Ctrl Pts',(-10.0115594732748,15.2,5.007459617187));
#250936=CARTESIAN_POINT('Ctrl Pts',(-10.0145188869914,15.2,5.01088131048363));
#250937=CARTESIAN_POINT('Ctrl Pts',(-10.0174814111815,15.2,5.0143175234418));
#250938=CARTESIAN_POINT('Ctrl Pts',(-10.0204469377137,15.2,5.01776823552572));
#250939=CARTESIAN_POINT('Ctrl Pts',(-10.0226710824109,15.2,5.02035626935358));
#250940=CARTESIAN_POINT('Ctrl Pts',(-10.0248969161403,15.2,5.02295245807785));
#250941=CARTESIAN_POINT('Ctrl Pts',(-10.0271243932262,15.2,5.02555679381727));
#250942=CARTESIAN_POINT('Ctrl Pts',(-10.0293518703121,15.2,5.0281611295567));
#250943=CARTESIAN_POINT('Ctrl Pts',(-10.0315809903644,15.2,5.03077361197848));
#250944=CARTESIAN_POINT('Ctrl Pts',(-10.0338117084917,15.2,5.03339423225826));
#250945=CARTESIAN_POINT('Ctrl Pts',(-10.036042426619,15.2,5.03601485253804));
#250946=CARTESIAN_POINT('Ctrl Pts',(-10.0382747433379,15.2,5.03864361119251));
#250947=CARTESIAN_POINT('Ctrl Pts',(-10.0405086129649,15.2,5.04128049847098));
#250948=CARTESIAN_POINT('Ctrl Pts',(-10.0427424825919,15.2,5.04391738574945));
#250949=CARTESIAN_POINT('Ctrl Pts',(-10.0449779060203,15.2,5.04656240236814));
#250950=CARTESIAN_POINT('Ctrl Pts',(-10.0472148368423,15.2,5.0492155387367));
#250951=CARTESIAN_POINT('Ctrl Pts',(-10.0494517676643,15.2,5.05186867510526));
#250952=CARTESIAN_POINT('Ctrl Pts',(-10.05169020826,15.2,5.05452993074946));
#250953=CARTESIAN_POINT('Ctrl Pts',(-10.0539301115118,15.2,5.05719929840135));
#250954=CARTESIAN_POINT('Ctrl Pts',(-10.0561700151704,15.2,5.05986866653817));
#250955=CARTESIAN_POINT('Ctrl Pts',(-10.0584113841462,15.2,5.06254614544398));
#250956=CARTESIAN_POINT('Ctrl Pts',(-10.0606541722223,15.2,5.06523172662706));
#250957=CARTESIAN_POINT('Ctrl Pts',(-10.062896959891,15.2,5.06791730732225));
#250958=CARTESIAN_POINT('Ctrl Pts',(-10.065141167843,15.2,5.07061099000869));
#250959=CARTESIAN_POINT('Ctrl Pts',(-10.0673867515115,15.2,5.07331276482789));
#250960=CARTESIAN_POINT('Ctrl Pts',(-10.06963233518,15.2,5.07601453964709));
#250961=CARTESIAN_POINT('Ctrl Pts',(-10.0718792957902,15.2,5.07872440775546));
#250962=CARTESIAN_POINT('Ctrl Pts',(-10.0741275880104,15.2,5.08144235946073));
#250963=CARTESIAN_POINT('Ctrl Pts',(-10.0771253108345,15.2,5.08506629490319));
#250964=CARTESIAN_POINT('Ctrl Pts',(-10.0801254037521,15.2,5.08870460094167));
#250965=CARTESIAN_POINT('Ctrl Pts',(-10.0831277617842,15.2,5.09235725641939));
#250966=CARTESIAN_POINT('Ctrl Pts',(-10.0853795308196,15.2,5.09509674864976));
#250967=CARTESIAN_POINT('Ctrl Pts',(-10.087632574397,15.2,5.09784431188241));
#250968=CARTESIAN_POINT('Ctrl Pts',(-10.0898868499748,15.2,5.10059993711734));
#250969=CARTESIAN_POINT('Ctrl Pts',(-10.0921411251431,15.2,5.10335556185167));
#250970=CARTESIAN_POINT('Ctrl Pts',(-10.0943966327779,15.2,5.10611924865218));
#250971=CARTESIAN_POINT('Ctrl Pts',(-10.0966533284877,15.2,5.10889098830218));
#250972=CARTESIAN_POINT('Ctrl Pts',(-10.0989100241975,15.2,5.1116627279522));
#250973=CARTESIAN_POINT('Ctrl Pts',(-10.1011679099155,15.2,5.11444251941791));
#250974=CARTESIAN_POINT('Ctrl Pts',(-10.103426942,15.2,5.1172303550666));
#250975=CARTESIAN_POINT('Ctrl Pts',(-10.1056859740846,15.2,5.12001819071529));
#250976=CARTESIAN_POINT('Ctrl Pts',(-10.1079461513692,15.2,5.12281406868034));
#250977=CARTESIAN_POINT('Ctrl Pts',(-10.1102074339952,15.2,5.12561798091109));
#250978=CARTESIAN_POINT('Ctrl Pts',(-10.1124687166213,15.2,5.12842189314185));
#250979=CARTESIAN_POINT('Ctrl Pts',(-10.1147311044814,15.2,5.13123383903359));
#250980=CARTESIAN_POINT('Ctrl Pts',(-10.1169945533455,15.2,5.13405380894608));
#250981=CARTESIAN_POINT('Ctrl Pts',(-10.1192580022095,15.2,5.13687377885856));
#250982=CARTESIAN_POINT('Ctrl Pts',(-10.1215225143386,15.2,5.13970177361916));
#250983=CARTESIAN_POINT('Ctrl Pts',(-10.1237880465062,15.2,5.14253778234835));
#250984=CARTESIAN_POINT('Ctrl Pts',(-10.1260535790853,15.2,5.14537379159274));
#250985=CARTESIAN_POINT('Ctrl Pts',(-10.1283201314313,15.2,5.14821781543941));
#250986=CARTESIAN_POINT('Ctrl Pts',(-10.1305876639694,15.2,5.15106984464669));
#250987=CARTESIAN_POINT('Ctrl Pts',(-10.1328551960955,15.2,5.15392187333584));
#250988=CARTESIAN_POINT('Ctrl Pts',(-10.1351237080632,15.2,5.15678190708287));
#250989=CARTESIAN_POINT('Ctrl Pts',(-10.1373931562724,15.2,5.15964993581269));
#250990=CARTESIAN_POINT('Ctrl Pts',(-10.1396626044817,15.2,5.16251796454251));
#250991=CARTESIAN_POINT('Ctrl Pts',(-10.141932990441,15.2,5.16539398774421));
#250992=CARTESIAN_POINT('Ctrl Pts',(-10.1442042744938,15.2,5.16827799744422));
#250993=CARTESIAN_POINT('Ctrl Pts',(-10.1464755585466,15.2,5.17116200714423));
#250994=CARTESIAN_POINT('Ctrl Pts',(-10.1487477383869,15.2,5.17405400273952));
#250995=CARTESIAN_POINT('Ctrl Pts',(-10.151020774523,15.2,5.17695397348064));
#250996=CARTESIAN_POINT('Ctrl Pts',(-10.1548091682208,15.2,5.18178725822477));
#250997=CARTESIAN_POINT('Ctrl Pts',(-10.1585999375556,15.2,5.1866426993944));
#250998=CARTESIAN_POINT('Ctrl Pts',(-10.1623928995001,15.2,5.19152024828326));
#250999=CARTESIAN_POINT('Ctrl Pts',(-10.164668676584,15.2,5.19444677751025));
#251000=CARTESIAN_POINT('Ctrl Pts',(-10.1669452418846,15.2,5.19738126598694));
#251001=CARTESIAN_POINT('Ctrl Pts',(-10.1692225565102,15.2,5.200323704671));
#251002=CARTESIAN_POINT('Ctrl Pts',(-10.1714998711357,15.2,5.20326614335507));
#251003=CARTESIAN_POINT('Ctrl Pts',(-10.1737779343449,15.2,5.20621653165492));
#251004=CARTESIAN_POINT('Ctrl Pts',(-10.1760567055425,15.2,5.20917485944431));
#251005=CARTESIAN_POINT('Ctrl Pts',(-10.1783354767401,15.2,5.21213318723369));
#251006=CARTESIAN_POINT('Ctrl Pts',(-10.1806149537859,15.2,5.21509945337738));
#251007=CARTESIAN_POINT('Ctrl Pts',(-10.1828950989946,15.2,5.21807364864323));
#251008=CARTESIAN_POINT('Ctrl Pts',(-10.1851752446176,15.2,5.2210478444494));
#251009=CARTESIAN_POINT('Ctrl Pts',(-10.1874560588324,15.2,5.22402997029947));
#251010=CARTESIAN_POINT('Ctrl Pts',(-10.1897375045391,15.2,5.22702001565178));
#251011=CARTESIAN_POINT('Ctrl Pts',(-10.1920189498313,15.2,5.23001006046089));
#251012=CARTESIAN_POINT('Ctrl Pts',(-10.1943010283817,15.2,5.23300802638621));
#251013=CARTESIAN_POINT('Ctrl Pts',(-10.1965836989655,15.2,5.23601390156937));
#251014=CARTESIAN_POINT('Ctrl Pts',(-10.1988663695493,15.2,5.23901977675254));
#251015=CARTESIAN_POINT('Ctrl Pts',(-10.2011496313747,15.2,5.24203356109871));
#251016=CARTESIAN_POINT('Ctrl Pts',(-10.2034334355105,15.2,5.24505524325268));
#251017=CARTESIAN_POINT('Ctrl Pts',(-10.2064785075531,15.2,5.24908415260831));
#251018=CARTESIAN_POINT('Ctrl Pts',(-10.2095245385816,15.2,5.25312709922805));
#251019=CARTESIAN_POINT('Ctrl Pts',(-10.2125714572769,15.2,5.25718406539495));
#251020=CARTESIAN_POINT('Ctrl Pts',(-10.2156183763873,15.2,5.2612410321146));
#251021=CARTESIAN_POINT('Ctrl Pts',(-10.2186661838359,15.2,5.26531201788687));
#251022=CARTESIAN_POINT('Ctrl Pts',(-10.2217148780001,15.2,5.26939701899998));
#251023=CARTESIAN_POINT('Ctrl Pts',(-8.88241603300006,15.2,5.36127880599999));
#251024=CARTESIAN_POINT('Ctrl Pts',(-8.88241603300006,11.6,5.36127880599999));
#251025=CARTESIAN_POINT('Ctrl Pts',(-8.88257249800006,15.2,5.36135574399999));
#251026=CARTESIAN_POINT('Ctrl Pts',(-8.88257249800006,11.6,5.36135574399999));
#251027=CARTESIAN_POINT('Ctrl Pts',(-8.88289093000006,15.2,5.36151222999998));
#251028=CARTESIAN_POINT('Ctrl Pts',(-8.88289093000006,11.6,5.36151222999998));
#251029=CARTESIAN_POINT('Ctrl Pts',(-8.88337354800005,15.2,5.36174910399998));
#251030=CARTESIAN_POINT('Ctrl Pts',(-8.88337354800005,11.6,5.36174910399998));
#251031=CARTESIAN_POINT('Ctrl Pts',(-8.88402391700006,15.2,5.36206771099998));
#251032=CARTESIAN_POINT('Ctrl Pts',(-8.88402391700006,11.6,5.36206771099998));
#251033=CARTESIAN_POINT('Ctrl Pts',(-8.88484693900006,15.2,5.36246988099998));
#251034=CARTESIAN_POINT('Ctrl Pts',(-8.88484693900006,11.6,5.36246988099998));
#251035=CARTESIAN_POINT('Ctrl Pts',(-8.88568370900006,15.2,5.36287772799999));
#251036=CARTESIAN_POINT('Ctrl Pts',(-8.88568370900006,11.6,5.36287772799999));
#251037=CARTESIAN_POINT('Ctrl Pts',(-8.88652944600006,15.2,5.36328889699998));
#251038=CARTESIAN_POINT('Ctrl Pts',(-8.88652944600006,11.6,5.36328889699998));
#251039=CARTESIAN_POINT('Ctrl Pts',(-8.88738413200005,15.2,5.36370335799998));
#251040=CARTESIAN_POINT('Ctrl Pts',(-8.88738413200005,11.6,5.36370335799998));
#251041=CARTESIAN_POINT('Ctrl Pts',(-8.88824775000005,15.2,5.36412108299999));
#251042=CARTESIAN_POINT('Ctrl Pts',(-8.88824775000005,11.6,5.36412108299999));
#251043=CARTESIAN_POINT('Ctrl Pts',(-8.88912028500006,15.2,5.36454204499999));
#251044=CARTESIAN_POINT('Ctrl Pts',(-8.88912028500006,11.6,5.36454204499999));
#251045=CARTESIAN_POINT('Ctrl Pts',(-8.89000172000006,15.2,5.36496621499998));
#251046=CARTESIAN_POINT('Ctrl Pts',(-8.89000172000006,11.6,5.36496621499998));
#251047=CARTESIAN_POINT('Ctrl Pts',(-8.89089204000006,15.2,5.36539356699999));
#251048=CARTESIAN_POINT('Ctrl Pts',(-8.89089204000006,11.6,5.36539356699999));
#251049=CARTESIAN_POINT('Ctrl Pts',(-8.89179122800006,15.2,5.36582407199998));
#251050=CARTESIAN_POINT('Ctrl Pts',(-8.89179122800006,11.6,5.36582407199998));
#251051=CARTESIAN_POINT('Ctrl Pts',(-8.89269926800005,15.2,5.36625770499998));
#251052=CARTESIAN_POINT('Ctrl Pts',(-8.89269926800005,11.6,5.36625770499998));
#251053=CARTESIAN_POINT('Ctrl Pts',(-8.89361614600006,15.2,5.36669443599998));
#251054=CARTESIAN_POINT('Ctrl Pts',(-8.89361614600006,11.6,5.36669443599998));
#251055=CARTESIAN_POINT('Ctrl Pts',(-8.89454184300006,15.2,5.36713423999998));
#251056=CARTESIAN_POINT('Ctrl Pts',(-8.89454184300006,11.6,5.36713423999998));
#251057=CARTESIAN_POINT('Ctrl Pts',(-8.89547634600006,15.2,5.36757709099999));
#251058=CARTESIAN_POINT('Ctrl Pts',(-8.89547634600006,11.6,5.36757709099999));
#251059=CARTESIAN_POINT('Ctrl Pts',(-8.89641963900005,15.2,5.36802295899999));
#251060=CARTESIAN_POINT('Ctrl Pts',(-8.89641963900005,11.6,5.36802295899999));
#251061=CARTESIAN_POINT('Ctrl Pts',(-8.89737170500006,15.2,5.36847181999998));
#251062=CARTESIAN_POINT('Ctrl Pts',(-8.89737170500006,11.6,5.36847181999998));
#251063=CARTESIAN_POINT('Ctrl Pts',(-8.89833252800006,15.2,5.36892364599999));
#251064=CARTESIAN_POINT('Ctrl Pts',(-8.89833252800006,11.6,5.36892364599999));
#251065=CARTESIAN_POINT('Ctrl Pts',(-8.89930209500006,15.2,5.36937841199999));
#251066=CARTESIAN_POINT('Ctrl Pts',(-8.89930209500006,11.6,5.36937841199999));
#251067=CARTESIAN_POINT('Ctrl Pts',(-8.90028038900006,15.2,5.36983609199999));
#251068=CARTESIAN_POINT('Ctrl Pts',(-8.90028038900006,11.6,5.36983609199999));
#251069=CARTESIAN_POINT('Ctrl Pts',(-8.90126739500005,15.2,5.37029665799999));
#251070=CARTESIAN_POINT('Ctrl Pts',(-8.90126739500005,11.6,5.37029665799999));
#251071=CARTESIAN_POINT('Ctrl Pts',(-8.90226309800006,15.2,5.37076008699999));
#251072=CARTESIAN_POINT('Ctrl Pts',(-8.90226309800006,11.6,5.37076008699999));
#251073=CARTESIAN_POINT('Ctrl Pts',(-8.90326748200006,15.2,5.37122635099998));
#251074=CARTESIAN_POINT('Ctrl Pts',(-8.90326748200006,11.6,5.37122635099998));
#251075=CARTESIAN_POINT('Ctrl Pts',(-8.90428053200005,15.2,5.37169542499999));
#251076=CARTESIAN_POINT('Ctrl Pts',(-8.90428053200005,11.6,5.37169542499999));
#251077=CARTESIAN_POINT('Ctrl Pts',(-8.90530223300006,15.2,5.37216728299998));
#251078=CARTESIAN_POINT('Ctrl Pts',(-8.90530223300006,11.6,5.37216728299998));
#251079=CARTESIAN_POINT('Ctrl Pts',(-8.90633257000006,15.2,5.37264189999998));
#251080=CARTESIAN_POINT('Ctrl Pts',(-8.90633257000006,11.6,5.37264189999998));
#251081=CARTESIAN_POINT('Ctrl Pts',(-8.90737152800006,15.2,5.37311925099999));
#251082=CARTESIAN_POINT('Ctrl Pts',(-8.90737152800006,11.6,5.37311925099999));
#251083=CARTESIAN_POINT('Ctrl Pts',(-8.90841909200006,15.2,5.37359930999998));
#251084=CARTESIAN_POINT('Ctrl Pts',(-8.90841909200006,11.6,5.37359930999998));
#251085=CARTESIAN_POINT('Ctrl Pts',(-8.90947524800006,15.2,5.37408205399998));
#251086=CARTESIAN_POINT('Ctrl Pts',(-8.90947524800006,11.6,5.37408205399998));
#251087=CARTESIAN_POINT('Ctrl Pts',(-8.91053997900006,15.2,5.37456745499998));
#251088=CARTESIAN_POINT('Ctrl Pts',(-8.91053997900006,11.6,5.37456745499998));
#251089=CARTESIAN_POINT('Ctrl Pts',(-8.91161327100006,15.2,5.37505549099999));
#251090=CARTESIAN_POINT('Ctrl Pts',(-8.91161327100006,11.6,5.37505549099999));
#251091=CARTESIAN_POINT('Ctrl Pts',(-8.91269511200005,15.2,5.37554613499999));
#251092=CARTESIAN_POINT('Ctrl Pts',(-8.91269511200005,11.6,5.37554613499999));
#251093=CARTESIAN_POINT('Ctrl Pts',(-8.91378548400005,15.2,5.37603936499998));
#251094=CARTESIAN_POINT('Ctrl Pts',(-8.91378548400005,11.6,5.37603936499998));
#251095=CARTESIAN_POINT('Ctrl Pts',(-8.91488437300006,15.2,5.37653515499999));
#251096=CARTESIAN_POINT('Ctrl Pts',(-8.91488437300006,11.6,5.37653515499999));
#251097=CARTESIAN_POINT('Ctrl Pts',(-8.91599176500005,15.2,5.37703347999998));
#251098=CARTESIAN_POINT('Ctrl Pts',(-8.91599176500005,11.6,5.37703347999998));
#251099=CARTESIAN_POINT('Ctrl Pts',(-8.91710764600005,15.2,5.37753431799998));
#251100=CARTESIAN_POINT('Ctrl Pts',(-8.91710764600005,11.6,5.37753431799998));
#251101=CARTESIAN_POINT('Ctrl Pts',(-8.91823200100006,15.2,5.37803764299999));
#251102=CARTESIAN_POINT('Ctrl Pts',(-8.91823200100006,11.6,5.37803764299999));
#251103=CARTESIAN_POINT('Ctrl Pts',(-8.91936481600006,15.2,5.37854343099998));
#251104=CARTESIAN_POINT('Ctrl Pts',(-8.91936481600006,11.6,5.37854343099998));
#251105=CARTESIAN_POINT('Ctrl Pts',(-8.92050607600006,15.2,5.37905165999998));
#251106=CARTESIAN_POINT('Ctrl Pts',(-8.92050607600006,11.6,5.37905165999998));
#251107=CARTESIAN_POINT('Ctrl Pts',(-8.92165576600006,15.2,5.37956230499999));
#251108=CARTESIAN_POINT('Ctrl Pts',(-8.92165576600006,11.6,5.37956230499999));
#251109=CARTESIAN_POINT('Ctrl Pts',(-8.92281387300006,15.2,5.38007534099999));
#251110=CARTESIAN_POINT('Ctrl Pts',(-8.92281387300006,11.6,5.38007534099999));
#251111=CARTESIAN_POINT('Ctrl Pts',(-8.92398038300006,15.2,5.38059074799998));
#251112=CARTESIAN_POINT('Ctrl Pts',(-8.92398038300006,11.6,5.38059074799998));
#251113=CARTESIAN_POINT('Ctrl Pts',(-8.92515528200006,15.2,5.38110849999998));
#251114=CARTESIAN_POINT('Ctrl Pts',(-8.92515528200006,11.6,5.38110849999998));
#251115=CARTESIAN_POINT('Ctrl Pts',(-8.92633855400006,15.2,5.38162857399998));
#251116=CARTESIAN_POINT('Ctrl Pts',(-8.92633855400006,11.6,5.38162857399998));
#251117=CARTESIAN_POINT('Ctrl Pts',(-8.92753018700006,15.2,5.38215094799998));
#251118=CARTESIAN_POINT('Ctrl Pts',(-8.92753018700006,11.6,5.38215094799998));
#251119=CARTESIAN_POINT('Ctrl Pts',(-8.92873016600005,15.2,5.38267559699998));
#251120=CARTESIAN_POINT('Ctrl Pts',(-8.92873016600005,11.6,5.38267559699998));
#251121=CARTESIAN_POINT('Ctrl Pts',(-8.92993847700006,15.2,5.38320249899999));
#251122=CARTESIAN_POINT('Ctrl Pts',(-8.92993847700006,11.6,5.38320249899999));
#251123=CARTESIAN_POINT('Ctrl Pts',(-8.93115510700006,15.2,5.38373163199999));
#251124=CARTESIAN_POINT('Ctrl Pts',(-8.93115510700006,11.6,5.38373163199999));
#251125=CARTESIAN_POINT('Ctrl Pts',(-8.93238004200006,15.2,5.38426297199998));
#251126=CARTESIAN_POINT('Ctrl Pts',(-8.93238004200006,11.6,5.38426297199998));
#251127=CARTESIAN_POINT('Ctrl Pts',(-8.93361326800006,15.2,5.38479649699998));
#251128=CARTESIAN_POINT('Ctrl Pts',(-8.93361326800006,11.6,5.38479649699998));
#251129=CARTESIAN_POINT('Ctrl Pts',(-8.93485477100005,15.2,5.38533218399999));
#251130=CARTESIAN_POINT('Ctrl Pts',(-8.93485477100005,11.6,5.38533218399999));
#251131=CARTESIAN_POINT('Ctrl Pts',(-8.93610453600006,15.2,5.38587001099998));
#251132=CARTESIAN_POINT('Ctrl Pts',(-8.93610453600006,11.6,5.38587001099998));
#251133=CARTESIAN_POINT('Ctrl Pts',(-8.93736255200006,15.2,5.38640995599999));
#251134=CARTESIAN_POINT('Ctrl Pts',(-8.93736255200006,11.6,5.38640995599999));
#251135=CARTESIAN_POINT('Ctrl Pts',(-8.93862880300006,15.2,5.38695199699998));
#251136=CARTESIAN_POINT('Ctrl Pts',(-8.93862880300006,11.6,5.38695199699998));
#251137=CARTESIAN_POINT('Ctrl Pts',(-8.93990327800006,15.2,5.38749611099998));
#251138=CARTESIAN_POINT('Ctrl Pts',(-8.93990327800006,11.6,5.38749611099998));
#251139=CARTESIAN_POINT('Ctrl Pts',(-8.94118596100006,15.2,5.38804227499998));
#251140=CARTESIAN_POINT('Ctrl Pts',(-8.94118596100006,11.6,5.38804227499998));
#251141=CARTESIAN_POINT('Ctrl Pts',(-8.94247684000005,15.2,5.38859046999999));
#251142=CARTESIAN_POINT('Ctrl Pts',(-8.94247684000005,11.6,5.38859046999999));
#251143=CARTESIAN_POINT('Ctrl Pts',(-8.94377590200006,15.2,5.38914067099999));
#251144=CARTESIAN_POINT('Ctrl Pts',(-8.94377590200006,11.6,5.38914067099999));
#251145=CARTESIAN_POINT('Ctrl Pts',(-8.94508313100006,15.2,5.38969285799999));
#251146=CARTESIAN_POINT('Ctrl Pts',(-8.94508313100006,11.6,5.38969285799999));
#251147=CARTESIAN_POINT('Ctrl Pts',(-8.94639851700006,15.2,5.39024700899999));
#251148=CARTESIAN_POINT('Ctrl Pts',(-8.94639851700006,11.6,5.39024700899999));
#251149=CARTESIAN_POINT('Ctrl Pts',(-8.94772204500006,15.2,5.39080310299998));
#251150=CARTESIAN_POINT('Ctrl Pts',(-8.94772204500006,11.6,5.39080310299998));
#251151=CARTESIAN_POINT('Ctrl Pts',(-8.94905370100006,15.2,5.39136111899998));
#251152=CARTESIAN_POINT('Ctrl Pts',(-8.94905370100006,11.6,5.39136111899998));
#251153=CARTESIAN_POINT('Ctrl Pts',(-8.95039347300006,15.2,5.39192103299998));
#251154=CARTESIAN_POINT('Ctrl Pts',(-8.95039347300006,11.6,5.39192103299998));
#251155=CARTESIAN_POINT('Ctrl Pts',(-8.95174134800006,15.2,5.39248282599999));
#251156=CARTESIAN_POINT('Ctrl Pts',(-8.95174134800006,11.6,5.39248282599999));
#251157=CARTESIAN_POINT('Ctrl Pts',(-8.95309731300006,15.2,5.39304647699999));
#251158=CARTESIAN_POINT('Ctrl Pts',(-8.95309731300006,11.6,5.39304647699999));
#251159=CARTESIAN_POINT('Ctrl Pts',(-8.95446135400006,15.2,5.39361196399998));
#251160=CARTESIAN_POINT('Ctrl Pts',(-8.95446135400006,11.6,5.39361196399998));
#251161=CARTESIAN_POINT('Ctrl Pts',(-8.95583345800006,15.2,5.39417926699999));
#251162=CARTESIAN_POINT('Ctrl Pts',(-8.95583345800006,11.6,5.39417926699999));
#251163=CARTESIAN_POINT('Ctrl Pts',(-8.95721361300006,15.2,5.39474836399998));
#251164=CARTESIAN_POINT('Ctrl Pts',(-8.95721361300006,11.6,5.39474836399998));
#251165=CARTESIAN_POINT('Ctrl Pts',(-8.95860180400006,15.2,5.39531923399998));
#251166=CARTESIAN_POINT('Ctrl Pts',(-8.95860180400006,11.6,5.39531923399998));
#251167=CARTESIAN_POINT('Ctrl Pts',(-8.95999802100006,15.2,5.39589185899998));
#251168=CARTESIAN_POINT('Ctrl Pts',(-8.95999802100006,11.6,5.39589185899998));
#251169=CARTESIAN_POINT('Ctrl Pts',(-8.96140225000006,15.2,5.39646621499998));
#251170=CARTESIAN_POINT('Ctrl Pts',(-8.96140225000006,11.6,5.39646621499998));
#251171=CARTESIAN_POINT('Ctrl Pts',(-8.96281447700006,15.2,5.39704228299998));
#251172=CARTESIAN_POINT('Ctrl Pts',(-8.96281447700006,11.6,5.39704228299998));
#251173=CARTESIAN_POINT('Ctrl Pts',(-8.96423469000006,15.2,5.39762004299998));
#251174=CARTESIAN_POINT('Ctrl Pts',(-8.96423469000006,11.6,5.39762004299998));
#251175=CARTESIAN_POINT('Ctrl Pts',(-8.96566287700006,15.2,5.39819947399998));
#251176=CARTESIAN_POINT('Ctrl Pts',(-8.96566287700006,11.6,5.39819947399998));
#251177=CARTESIAN_POINT('Ctrl Pts',(-8.96709902400006,15.2,5.39878055599999));
#251178=CARTESIAN_POINT('Ctrl Pts',(-8.96709902400006,11.6,5.39878055599999));
#251179=CARTESIAN_POINT('Ctrl Pts',(-8.96854312000006,15.2,5.39936326899999));
#251180=CARTESIAN_POINT('Ctrl Pts',(-8.96854312000006,11.6,5.39936326899999));
#251181=CARTESIAN_POINT('Ctrl Pts',(-8.96999515100006,15.2,5.39994759299999));
#251182=CARTESIAN_POINT('Ctrl Pts',(-8.96999515100006,11.6,5.39994759299999));
#251183=CARTESIAN_POINT('Ctrl Pts',(-8.97145510400006,15.2,5.40053350699999));
#251184=CARTESIAN_POINT('Ctrl Pts',(-8.97145510400006,11.6,5.40053350699999));
#251185=CARTESIAN_POINT('Ctrl Pts',(-8.97292296700006,15.2,5.40112099299999));
#251186=CARTESIAN_POINT('Ctrl Pts',(-8.97292296700006,11.6,5.40112099299999));
#251187=CARTESIAN_POINT('Ctrl Pts',(-8.97439872900006,15.2,5.40171002899999));
#251188=CARTESIAN_POINT('Ctrl Pts',(-8.97439872900006,11.6,5.40171002899999));
#251189=CARTESIAN_POINT('Ctrl Pts',(-8.97588237600005,15.2,5.40230059799998));
#251190=CARTESIAN_POINT('Ctrl Pts',(-8.97588237600005,11.6,5.40230059799998));
#251191=CARTESIAN_POINT('Ctrl Pts',(-8.97737389600006,15.2,5.40289267699999));
#251192=CARTESIAN_POINT('Ctrl Pts',(-8.97737389600006,11.6,5.40289267699999));
#251193=CARTESIAN_POINT('Ctrl Pts',(-8.97887327600005,15.2,5.40348624899998));
#251194=CARTESIAN_POINT('Ctrl Pts',(-8.97887327600005,11.6,5.40348624899998));
#251195=CARTESIAN_POINT('Ctrl Pts',(-8.98038050400006,15.2,5.40408129299998));
#251196=CARTESIAN_POINT('Ctrl Pts',(-8.98038050400006,11.6,5.40408129299998));
#251197=CARTESIAN_POINT('Ctrl Pts',(-8.98189556800006,15.2,5.40467779099998));
#251198=CARTESIAN_POINT('Ctrl Pts',(-8.98189556800006,11.6,5.40467779099998));
#251199=CARTESIAN_POINT('Ctrl Pts',(-8.98341845500006,15.2,5.40527572299998));
#251200=CARTESIAN_POINT('Ctrl Pts',(-8.98341845500006,11.6,5.40527572299998));
#251201=CARTESIAN_POINT('Ctrl Pts',(-8.98494915400006,15.2,5.40587506999999));
#251202=CARTESIAN_POINT('Ctrl Pts',(-8.98494915400006,11.6,5.40587506999999));
#251203=CARTESIAN_POINT('Ctrl Pts',(-8.98648765200005,15.2,5.40647581199998));
#251204=CARTESIAN_POINT('Ctrl Pts',(-8.98648765200005,11.6,5.40647581199998));
#251205=CARTESIAN_POINT('Ctrl Pts',(-8.98803393600006,15.2,5.40707793199999));
#251206=CARTESIAN_POINT('Ctrl Pts',(-8.98803393600006,11.6,5.40707793199999));
#251207=CARTESIAN_POINT('Ctrl Pts',(-8.98958799600006,15.2,5.40768140799998));
#251208=CARTESIAN_POINT('Ctrl Pts',(-8.98958799600006,11.6,5.40768140799998));
#251209=CARTESIAN_POINT('Ctrl Pts',(-8.99114981800006,15.2,5.40828622299999));
#251210=CARTESIAN_POINT('Ctrl Pts',(-8.99114981800006,11.6,5.40828622299999));
#251211=CARTESIAN_POINT('Ctrl Pts',(-8.99271939000006,15.2,5.40889235799998));
#251212=CARTESIAN_POINT('Ctrl Pts',(-8.99271939000006,11.6,5.40889235799998));
#251213=CARTESIAN_POINT('Ctrl Pts',(-8.99429670100006,15.2,5.40949979499998));
#251214=CARTESIAN_POINT('Ctrl Pts',(-8.99429670100006,11.6,5.40949979499998));
#251215=CARTESIAN_POINT('Ctrl Pts',(-8.99588173900005,15.2,5.41010851499999));
#251216=CARTESIAN_POINT('Ctrl Pts',(-8.99588173900005,11.6,5.41010851499999));
#251217=CARTESIAN_POINT('Ctrl Pts',(-8.99747449100006,15.2,5.41071849699998));
#251218=CARTESIAN_POINT('Ctrl Pts',(-8.99747449100006,11.6,5.41071849699998));
#251219=CARTESIAN_POINT('Ctrl Pts',(-8.99907494600006,15.2,5.41132972599998));
#251220=CARTESIAN_POINT('Ctrl Pts',(-8.99907494600006,11.6,5.41132972599998));
#251221=CARTESIAN_POINT('Ctrl Pts',(-9.00068309100006,15.2,5.41194217999998));
#251222=CARTESIAN_POINT('Ctrl Pts',(-9.00068309100006,11.6,5.41194217999998));
#251223=CARTESIAN_POINT('Ctrl Pts',(-9.00229891600006,15.2,5.41255584399998));
#251224=CARTESIAN_POINT('Ctrl Pts',(-9.00229891600006,11.6,5.41255584399998));
#251225=CARTESIAN_POINT('Ctrl Pts',(-9.00392240700005,15.2,5.41317069799998));
#251226=CARTESIAN_POINT('Ctrl Pts',(-9.00392240700005,11.6,5.41317069799998));
#251227=CARTESIAN_POINT('Ctrl Pts',(-9.00555355400006,15.2,5.41378672399999));
#251228=CARTESIAN_POINT('Ctrl Pts',(-9.00555355400006,11.6,5.41378672399999));
#251229=CARTESIAN_POINT('Ctrl Pts',(-9.00719234500006,15.2,5.41440390399998));
#251230=CARTESIAN_POINT('Ctrl Pts',(-9.00719234500006,11.6,5.41440390399998));
#251231=CARTESIAN_POINT('Ctrl Pts',(-9.00883876700006,15.2,5.41502221999998));
#251232=CARTESIAN_POINT('Ctrl Pts',(-9.00883876700006,11.6,5.41502221999998));
#251233=CARTESIAN_POINT('Ctrl Pts',(-9.01049280800006,15.2,5.41564165399999));
#251234=CARTESIAN_POINT('Ctrl Pts',(-9.01049280800006,11.6,5.41564165399999));
#251235=CARTESIAN_POINT('Ctrl Pts',(-9.01215445900006,15.2,5.41626218699999));
#251236=CARTESIAN_POINT('Ctrl Pts',(-9.01215445900006,11.6,5.41626218699999));
#251237=CARTESIAN_POINT('Ctrl Pts',(-9.01382370600006,15.2,5.41688380299998));
#251238=CARTESIAN_POINT('Ctrl Pts',(-9.01382370600006,11.6,5.41688380299998));
#251239=CARTESIAN_POINT('Ctrl Pts',(-9.01550053900005,15.2,5.41750648399999));
#251240=CARTESIAN_POINT('Ctrl Pts',(-9.01550053900005,11.6,5.41750648399999));
#251241=CARTESIAN_POINT('Ctrl Pts',(-9.01718494500006,15.2,5.41813020999999));
#251242=CARTESIAN_POINT('Ctrl Pts',(-9.01718494500006,11.6,5.41813020999999));
#251243=CARTESIAN_POINT('Ctrl Pts',(-9.01887691300006,15.2,5.41875496599998));
#251244=CARTESIAN_POINT('Ctrl Pts',(-9.01887691300006,11.6,5.41875496599998));
#251245=CARTESIAN_POINT('Ctrl Pts',(-9.02057643200006,15.2,5.41938073299999));
#251246=CARTESIAN_POINT('Ctrl Pts',(-9.02057643200006,11.6,5.41938073299999));
#251247=CARTESIAN_POINT('Ctrl Pts',(-9.02228349000006,15.2,5.42000749399998));
#251248=CARTESIAN_POINT('Ctrl Pts',(-9.02228349000006,11.6,5.42000749399998));
#251249=CARTESIAN_POINT('Ctrl Pts',(-9.02399807600006,15.2,5.42063523199998));
#251250=CARTESIAN_POINT('Ctrl Pts',(-9.02399807600006,11.6,5.42063523199998));
#251251=CARTESIAN_POINT('Ctrl Pts',(-9.02572017800006,15.2,5.42126392899998));
#251252=CARTESIAN_POINT('Ctrl Pts',(-9.02572017800006,11.6,5.42126392899998));
#251253=CARTESIAN_POINT('Ctrl Pts',(-9.02744978400005,15.2,5.42189356799998));
#251254=CARTESIAN_POINT('Ctrl Pts',(-9.02744978400005,11.6,5.42189356799998));
#251255=CARTESIAN_POINT('Ctrl Pts',(-9.02918688400005,15.2,5.42252413099998));
#251256=CARTESIAN_POINT('Ctrl Pts',(-9.02918688400005,11.6,5.42252413099998));
#251257=CARTESIAN_POINT('Ctrl Pts',(-9.03093146700006,15.2,5.42315560199999));
#251258=CARTESIAN_POINT('Ctrl Pts',(-9.03093146700006,11.6,5.42315560199999));
#251259=CARTESIAN_POINT('Ctrl Pts',(-9.03268352000006,15.2,5.42378796399999));
#251260=CARTESIAN_POINT('Ctrl Pts',(-9.03268352000006,11.6,5.42378796399999));
#251261=CARTESIAN_POINT('Ctrl Pts',(-9.03444303300006,15.2,5.42442119899999));
#251262=CARTESIAN_POINT('Ctrl Pts',(-9.03444303300006,11.6,5.42442119899999));
#251263=CARTESIAN_POINT('Ctrl Pts',(-9.03620999400006,15.2,5.42505528999998));
#251264=CARTESIAN_POINT('Ctrl Pts',(-9.03620999400006,11.6,5.42505528999998));
#251265=CARTESIAN_POINT('Ctrl Pts',(-9.03798439200006,15.2,5.42569022099999));
#251266=CARTESIAN_POINT('Ctrl Pts',(-9.03798439200006,11.6,5.42569022099999));
#251267=CARTESIAN_POINT('Ctrl Pts',(-9.03976621700006,15.2,5.42632597599999));
#251268=CARTESIAN_POINT('Ctrl Pts',(-9.03976621700006,11.6,5.42632597599999));
#251269=CARTESIAN_POINT('Ctrl Pts',(-9.04155545700006,15.2,5.42696253499999));
#251270=CARTESIAN_POINT('Ctrl Pts',(-9.04155545700006,11.6,5.42696253499999));
#251271=CARTESIAN_POINT('Ctrl Pts',(-9.04335210000006,15.2,5.42759988499999));
#251272=CARTESIAN_POINT('Ctrl Pts',(-9.04335210000006,11.6,5.42759988499999));
#251273=CARTESIAN_POINT('Ctrl Pts',(-9.04515613500006,15.2,5.42823800699999));
#251274=CARTESIAN_POINT('Ctrl Pts',(-9.04515613500006,11.6,5.42823800699999));
#251275=CARTESIAN_POINT('Ctrl Pts',(-9.04696755200005,15.2,5.42887688499999));
#251276=CARTESIAN_POINT('Ctrl Pts',(-9.04696755200005,11.6,5.42887688499999));
#251277=CARTESIAN_POINT('Ctrl Pts',(-9.04878634100006,15.2,5.42951650299998));
#251278=CARTESIAN_POINT('Ctrl Pts',(-9.04878634100006,11.6,5.42951650299998));
#251279=CARTESIAN_POINT('Ctrl Pts',(-9.05061248800006,15.2,5.43015684399998));
#251280=CARTESIAN_POINT('Ctrl Pts',(-9.05061248800006,11.6,5.43015684399998));
#251281=CARTESIAN_POINT('Ctrl Pts',(-9.05244598400006,15.2,5.43079789199999));
#251282=CARTESIAN_POINT('Ctrl Pts',(-9.05244598400006,11.6,5.43079789199999));
#251283=CARTESIAN_POINT('Ctrl Pts',(-9.05428681800006,15.2,5.43143963099999));
#251284=CARTESIAN_POINT('Ctrl Pts',(-9.05428681800006,11.6,5.43143963099999));
#251285=CARTESIAN_POINT('Ctrl Pts',(-9.05613497800006,15.2,5.43208204499999));
#251286=CARTESIAN_POINT('Ctrl Pts',(-9.05613497800006,11.6,5.43208204499999));
#251287=CARTESIAN_POINT('Ctrl Pts',(-9.05799045400006,15.2,5.43272511599999));
#251288=CARTESIAN_POINT('Ctrl Pts',(-9.05799045400006,11.6,5.43272511599999));
#251289=CARTESIAN_POINT('Ctrl Pts',(-9.05985323600006,15.2,5.43336882999998));
#251290=CARTESIAN_POINT('Ctrl Pts',(-9.05985323600006,11.6,5.43336882999998));
#251291=CARTESIAN_POINT('Ctrl Pts',(-9.06172331100005,15.2,5.43401316999999));
#251292=CARTESIAN_POINT('Ctrl Pts',(-9.06172331100005,11.6,5.43401316999999));
#251293=CARTESIAN_POINT('Ctrl Pts',(-9.06360067000006,15.2,5.43465811899999));
#251294=CARTESIAN_POINT('Ctrl Pts',(-9.06360067000006,11.6,5.43465811899999));
#251295=CARTESIAN_POINT('Ctrl Pts',(-9.06548530100006,15.2,5.43530366299999));
#251296=CARTESIAN_POINT('Ctrl Pts',(-9.06548530100006,11.6,5.43530366299999));
#251297=CARTESIAN_POINT('Ctrl Pts',(-9.06737719300006,15.2,5.43594978599998));
#251298=CARTESIAN_POINT('Ctrl Pts',(-9.06737719300006,11.6,5.43594978599998));
#251299=CARTESIAN_POINT('Ctrl Pts',(-9.06927633700005,15.2,5.43659646999998));
#251300=CARTESIAN_POINT('Ctrl Pts',(-9.06927633700005,11.6,5.43659646999998));
#251301=CARTESIAN_POINT('Ctrl Pts',(-9.07118272000006,15.2,5.43724370099999));
#251302=CARTESIAN_POINT('Ctrl Pts',(-9.07118272000006,11.6,5.43724370099999));
#251303=CARTESIAN_POINT('Ctrl Pts',(-9.07309633400006,15.2,5.43789146299999));
#251304=CARTESIAN_POINT('Ctrl Pts',(-9.07309633400006,11.6,5.43789146299999));
#251305=CARTESIAN_POINT('Ctrl Pts',(-9.07501716700006,15.2,5.43853974199998));
#251306=CARTESIAN_POINT('Ctrl Pts',(-9.07501716700006,11.6,5.43853974199998));
#251307=CARTESIAN_POINT('Ctrl Pts',(-9.07694520800005,15.2,5.43918851899999));
#251308=CARTESIAN_POINT('Ctrl Pts',(-9.07694520800005,11.6,5.43918851899999));
#251309=CARTESIAN_POINT('Ctrl Pts',(-9.07888044600006,15.2,5.43983778099999));
#251310=CARTESIAN_POINT('Ctrl Pts',(-9.07888044600006,11.6,5.43983778099999));
#251311=CARTESIAN_POINT('Ctrl Pts',(-9.08082287200006,15.2,5.44048751199998));
#251312=CARTESIAN_POINT('Ctrl Pts',(-9.08082287200006,11.6,5.44048751199998));
#251313=CARTESIAN_POINT('Ctrl Pts',(-9.08277247500006,15.2,5.44113769599999));
#251314=CARTESIAN_POINT('Ctrl Pts',(-9.08277247500006,11.6,5.44113769599999));
#251315=CARTESIAN_POINT('Ctrl Pts',(-9.08472924200005,15.2,5.44178831899998));
#251316=CARTESIAN_POINT('Ctrl Pts',(-9.08472924200005,11.6,5.44178831899998));
#251317=CARTESIAN_POINT('Ctrl Pts',(-9.08669316600006,15.2,5.44243936399998));
#251318=CARTESIAN_POINT('Ctrl Pts',(-9.08669316600006,11.6,5.44243936399998));
#251319=CARTESIAN_POINT('Ctrl Pts',(-9.08866423500006,15.2,5.44309081699998));
#251320=CARTESIAN_POINT('Ctrl Pts',(-9.08866423500006,11.6,5.44309081699998));
#251321=CARTESIAN_POINT('Ctrl Pts',(-9.09064243800006,15.2,5.44374266199998));
#251322=CARTESIAN_POINT('Ctrl Pts',(-9.09064243800006,11.6,5.44374266199998));
#251323=CARTESIAN_POINT('Ctrl Pts',(-9.09262776600006,15.2,5.44439488499999));
#251324=CARTESIAN_POINT('Ctrl Pts',(-9.09262776600006,11.6,5.44439488499999));
#251325=CARTESIAN_POINT('Ctrl Pts',(-9.09462020800006,15.2,5.44504746899998));
#251326=CARTESIAN_POINT('Ctrl Pts',(-9.09462020800006,11.6,5.44504746899998));
#251327=CARTESIAN_POINT('Ctrl Pts',(-9.09661975200006,15.2,5.44570040099998));
#251328=CARTESIAN_POINT('Ctrl Pts',(-9.09661975200006,11.6,5.44570040099998));
#251329=CARTESIAN_POINT('Ctrl Pts',(-9.09862638900006,15.2,5.44635366599999));
#251330=CARTESIAN_POINT('Ctrl Pts',(-9.09862638900006,11.6,5.44635366599999));
#251331=CARTESIAN_POINT('Ctrl Pts',(-9.10064011000006,15.2,5.44700724699998));
#251332=CARTESIAN_POINT('Ctrl Pts',(-9.10064011000006,11.6,5.44700724699998));
#251333=CARTESIAN_POINT('Ctrl Pts',(-9.10266090200006,15.2,5.44766113199999));
#251334=CARTESIAN_POINT('Ctrl Pts',(-9.10266090200006,11.6,5.44766113199999));
#251335=CARTESIAN_POINT('Ctrl Pts',(-9.10468875600005,15.2,5.44831530299999));
#251336=CARTESIAN_POINT('Ctrl Pts',(-9.10468875600005,11.6,5.44831530299999));
#251337=CARTESIAN_POINT('Ctrl Pts',(-9.10672366200006,15.2,5.44896974899999));
#251338=CARTESIAN_POINT('Ctrl Pts',(-9.10672366200006,11.6,5.44896974899999));
#251339=CARTESIAN_POINT('Ctrl Pts',(-9.10876561000006,15.2,5.44962445199998));
#251340=CARTESIAN_POINT('Ctrl Pts',(-9.10876561000006,11.6,5.44962445199998));
#251341=CARTESIAN_POINT('Ctrl Pts',(-9.11081458900006,15.2,5.45027939999999));
#251342=CARTESIAN_POINT('Ctrl Pts',(-9.11081458900006,11.6,5.45027939999999));
#251343=CARTESIAN_POINT('Ctrl Pts',(-9.11287058900006,15.2,5.45093457599998));
#251344=CARTESIAN_POINT('Ctrl Pts',(-9.11287058900006,11.6,5.45093457599998));
#251345=CARTESIAN_POINT('Ctrl Pts',(-9.11493360000006,15.2,5.45158996699998));
#251346=CARTESIAN_POINT('Ctrl Pts',(-9.11493360000006,11.6,5.45158996699998));
#251347=CARTESIAN_POINT('Ctrl Pts',(-9.11700361100005,15.2,5.45224555799999));
#251348=CARTESIAN_POINT('Ctrl Pts',(-9.11700361100005,11.6,5.45224555799999));
#251349=CARTESIAN_POINT('Ctrl Pts',(-9.11908061400006,15.2,5.45290133499999));
#251350=CARTESIAN_POINT('Ctrl Pts',(-9.11908061400006,11.6,5.45290133499999));
#251351=CARTESIAN_POINT('Ctrl Pts',(-9.12116459600006,15.2,5.45355728299998));
#251352=CARTESIAN_POINT('Ctrl Pts',(-9.12116459600006,11.6,5.45355728299998));
#251353=CARTESIAN_POINT('Ctrl Pts',(-9.12325554900006,15.2,5.45421338899998));
#251354=CARTESIAN_POINT('Ctrl Pts',(-9.12325554900006,11.6,5.45421338899998));
#251355=CARTESIAN_POINT('Ctrl Pts',(-9.12535346300006,15.2,5.45486963699998));
#251356=CARTESIAN_POINT('Ctrl Pts',(-9.12535346300006,11.6,5.45486963699998));
#251357=CARTESIAN_POINT('Ctrl Pts',(-9.12745832700006,15.2,5.45552601299998));
#251358=CARTESIAN_POINT('Ctrl Pts',(-9.12745832700006,11.6,5.45552601299998));
#251359=CARTESIAN_POINT('Ctrl Pts',(-9.12957013000005,15.2,5.45618250499999));
#251360=CARTESIAN_POINT('Ctrl Pts',(-9.12957013000005,11.6,5.45618250499999));
#251361=CARTESIAN_POINT('Ctrl Pts',(-9.13168886400006,15.2,5.45683909699999));
#251362=CARTESIAN_POINT('Ctrl Pts',(-9.13168886400006,11.6,5.45683909699999));
#251363=CARTESIAN_POINT('Ctrl Pts',(-9.13381451900005,15.2,5.45749577499999));
#251364=CARTESIAN_POINT('Ctrl Pts',(-9.13381451900005,11.6,5.45749577499999));
#251365=CARTESIAN_POINT('Ctrl Pts',(-9.13594708400005,15.2,5.45815252399999));
#251366=CARTESIAN_POINT('Ctrl Pts',(-9.13594708400005,11.6,5.45815252399999));
#251367=CARTESIAN_POINT('Ctrl Pts',(-9.13808654800006,15.2,5.45880933299999));
#251368=CARTESIAN_POINT('Ctrl Pts',(-9.13808654800006,11.6,5.45880933299999));
#251369=CARTESIAN_POINT('Ctrl Pts',(-9.14023290400005,15.2,5.45946618599999));
#251370=CARTESIAN_POINT('Ctrl Pts',(-9.14023290400005,11.6,5.45946618599999));
#251371=CARTESIAN_POINT('Ctrl Pts',(-9.14238614100006,15.2,5.46012306899998));
#251372=CARTESIAN_POINT('Ctrl Pts',(-9.14238614100006,11.6,5.46012306899998));
#251373=CARTESIAN_POINT('Ctrl Pts',(-9.14454624700006,15.2,5.46077996999998));
#251374=CARTESIAN_POINT('Ctrl Pts',(-9.14454624700006,11.6,5.46077996999998));
#251375=CARTESIAN_POINT('Ctrl Pts',(-9.14671321500006,15.2,5.46143687199999));
#251376=CARTESIAN_POINT('Ctrl Pts',(-9.14671321500006,11.6,5.46143687199999));
#251377=CARTESIAN_POINT('Ctrl Pts',(-9.14888703300005,15.2,5.46209376499998));
#251378=CARTESIAN_POINT('Ctrl Pts',(-9.14888703300005,11.6,5.46209376499998));
#251379=CARTESIAN_POINT('Ctrl Pts',(-9.15106769300005,15.2,5.46275063199998));
#251380=CARTESIAN_POINT('Ctrl Pts',(-9.15106769300005,11.6,5.46275063199998));
#251381=CARTESIAN_POINT('Ctrl Pts',(-9.15325518500006,15.2,5.46340746199999));
#251382=CARTESIAN_POINT('Ctrl Pts',(-9.15325518500006,11.6,5.46340746199999));
#251383=CARTESIAN_POINT('Ctrl Pts',(-9.15544949700006,15.2,5.46406423999999));
#251384=CARTESIAN_POINT('Ctrl Pts',(-9.15544949700006,11.6,5.46406423999999));
#251385=CARTESIAN_POINT('Ctrl Pts',(-9.15765062100006,15.2,5.46472095299999));
#251386=CARTESIAN_POINT('Ctrl Pts',(-9.15765062100006,11.6,5.46472095299999));
#251387=CARTESIAN_POINT('Ctrl Pts',(-9.15985854800006,15.2,5.46537758799998));
#251388=CARTESIAN_POINT('Ctrl Pts',(-9.15985854800006,11.6,5.46537758799998));
#251389=CARTESIAN_POINT('Ctrl Pts',(-9.16207326800006,15.2,5.46603412999998));
#251390=CARTESIAN_POINT('Ctrl Pts',(-9.16207326800006,11.6,5.46603412999998));
#251391=CARTESIAN_POINT('Ctrl Pts',(-9.16429476900005,15.2,5.46669056699999));
#251392=CARTESIAN_POINT('Ctrl Pts',(-9.16429476900005,11.6,5.46669056699999));
#251393=CARTESIAN_POINT('Ctrl Pts',(-9.16652304500005,15.2,5.46734688499999));
#251394=CARTESIAN_POINT('Ctrl Pts',(-9.16652304500005,11.6,5.46734688499999));
#251395=CARTESIAN_POINT('Ctrl Pts',(-9.16875808300006,15.2,5.46800307099998));
#251396=CARTESIAN_POINT('Ctrl Pts',(-9.16875808300006,11.6,5.46800307099998));
#251397=CARTESIAN_POINT('Ctrl Pts',(-9.17099987400006,15.2,5.46865911099999));
#251398=CARTESIAN_POINT('Ctrl Pts',(-9.17099987400006,11.6,5.46865911099999));
#251399=CARTESIAN_POINT('Ctrl Pts',(-9.17324841100006,15.2,5.46931499399999));
#251400=CARTESIAN_POINT('Ctrl Pts',(-9.17324841100006,11.6,5.46931499399999));
#251401=CARTESIAN_POINT('Ctrl Pts',(-9.17550368100006,15.2,5.46997070399998));
#251402=CARTESIAN_POINT('Ctrl Pts',(-9.17550368100006,11.6,5.46997070399998));
#251403=CARTESIAN_POINT('Ctrl Pts',(-9.17776567700006,15.2,5.47062622899999));
#251404=CARTESIAN_POINT('Ctrl Pts',(-9.17776567700006,11.6,5.47062622899999));
#251405=CARTESIAN_POINT('Ctrl Pts',(-9.18003438700006,15.2,5.47128155699999));
#251406=CARTESIAN_POINT('Ctrl Pts',(-9.18003438700006,11.6,5.47128155699999));
#251407=CARTESIAN_POINT('Ctrl Pts',(-9.18230980500006,15.2,5.47193667299998));
#251408=CARTESIAN_POINT('Ctrl Pts',(-9.18230980500006,11.6,5.47193667299998));
#251409=CARTESIAN_POINT('Ctrl Pts',(-9.18459191800006,15.2,5.47259156599999));
#251410=CARTESIAN_POINT('Ctrl Pts',(-9.18459191800006,11.6,5.47259156599999));
#251411=CARTESIAN_POINT('Ctrl Pts',(-9.18688071800006,15.2,5.47324622199999));
#251412=CARTESIAN_POINT('Ctrl Pts',(-9.18688071800006,11.6,5.47324622199999));
#251413=CARTESIAN_POINT('Ctrl Pts',(-9.18917619500006,15.2,5.47390062799998));
#251414=CARTESIAN_POINT('Ctrl Pts',(-9.18917619500006,11.6,5.47390062799998));
#251415=CARTESIAN_POINT('Ctrl Pts',(-9.19147834000006,15.2,5.47455477199998));
#251416=CARTESIAN_POINT('Ctrl Pts',(-9.19147834000006,11.6,5.47455477199998));
#251417=CARTESIAN_POINT('Ctrl Pts',(-9.19378714400005,15.2,5.47520864099998));
#251418=CARTESIAN_POINT('Ctrl Pts',(-9.19378714400005,11.6,5.47520864099998));
#251419=CARTESIAN_POINT('Ctrl Pts',(-9.19610259600006,15.2,5.47586222099999));
#251420=CARTESIAN_POINT('Ctrl Pts',(-9.19610259600006,11.6,5.47586222099999));
#251421=CARTESIAN_POINT('Ctrl Pts',(-9.19842468800006,15.2,5.47651549999999));
#251422=CARTESIAN_POINT('Ctrl Pts',(-9.19842468800006,11.6,5.47651549999999));
#251423=CARTESIAN_POINT('Ctrl Pts',(-9.20075341100006,15.2,5.47716846599998));
#251424=CARTESIAN_POINT('Ctrl Pts',(-9.20075341100006,11.6,5.47716846599998));
#251425=CARTESIAN_POINT('Ctrl Pts',(-9.20308875400006,15.2,5.47782110499998));
#251426=CARTESIAN_POINT('Ctrl Pts',(-9.20308875400006,11.6,5.47782110499998));
#251427=CARTESIAN_POINT('Ctrl Pts',(-9.20543070800005,15.2,5.47847340599999));
#251428=CARTESIAN_POINT('Ctrl Pts',(-9.20543070800005,11.6,5.47847340599999));
#251429=CARTESIAN_POINT('Ctrl Pts',(-9.20777926500006,15.2,5.47912535599998));
#251430=CARTESIAN_POINT('Ctrl Pts',(-9.20777926500006,11.6,5.47912535599998));
#251431=CARTESIAN_POINT('Ctrl Pts',(-9.21013441500006,15.2,5.47977694199999));
#251432=CARTESIAN_POINT('Ctrl Pts',(-9.21013441500006,11.6,5.47977694199999));
#251433=CARTESIAN_POINT('Ctrl Pts',(-9.21249614800006,15.2,5.48042815199998));
#251434=CARTESIAN_POINT('Ctrl Pts',(-9.21249614800006,11.6,5.48042815199998));
#251435=CARTESIAN_POINT('Ctrl Pts',(-9.21486445500006,15.2,5.48107897299998));
#251436=CARTESIAN_POINT('Ctrl Pts',(-9.21486445500006,11.6,5.48107897299998));
#251437=CARTESIAN_POINT('Ctrl Pts',(-9.21723932700005,15.2,5.48172939299998));
#251438=CARTESIAN_POINT('Ctrl Pts',(-9.21723932700005,11.6,5.48172939299998));
#251439=CARTESIAN_POINT('Ctrl Pts',(-9.21962075500005,15.2,5.48237939999999));
#251440=CARTESIAN_POINT('Ctrl Pts',(-9.21962075500005,11.6,5.48237939999999));
#251441=CARTESIAN_POINT('Ctrl Pts',(-9.22200872900006,15.2,5.48302897999999));
#251442=CARTESIAN_POINT('Ctrl Pts',(-9.22200872900006,11.6,5.48302897999999));
#251443=CARTESIAN_POINT('Ctrl Pts',(-9.22440324100006,15.2,5.48367812299999));
#251444=CARTESIAN_POINT('Ctrl Pts',(-9.22440324100006,11.6,5.48367812299999));
#251445=CARTESIAN_POINT('Ctrl Pts',(-9.22680428000006,15.2,5.48432681599999));
#251446=CARTESIAN_POINT('Ctrl Pts',(-9.22680428000006,11.6,5.48432681599999));
#251447=CARTESIAN_POINT('Ctrl Pts',(-9.22921184000005,15.2,5.48497504599998));
#251448=CARTESIAN_POINT('Ctrl Pts',(-9.22921184000005,11.6,5.48497504599998));
#251449=CARTESIAN_POINT('Ctrl Pts',(-9.23162590700005,15.2,5.48562280199998));
#251450=CARTESIAN_POINT('Ctrl Pts',(-9.23162590700005,11.6,5.48562280199998));
#251451=CARTESIAN_POINT('Ctrl Pts',(-9.23404647600006,15.2,5.48627007099999));
#251452=CARTESIAN_POINT('Ctrl Pts',(-9.23404647600006,11.6,5.48627007099999));
#251453=CARTESIAN_POINT('Ctrl Pts',(-9.23647353600006,15.2,5.48691684199999));
#251454=CARTESIAN_POINT('Ctrl Pts',(-9.23647353600006,11.6,5.48691684199999));
#251455=CARTESIAN_POINT('Ctrl Pts',(-9.23890707800006,15.2,5.48756310099999));
#251456=CARTESIAN_POINT('Ctrl Pts',(-9.23890707800006,11.6,5.48756310099999));
#251457=CARTESIAN_POINT('Ctrl Pts',(-9.24134709500006,15.2,5.48820883899998));
#251458=CARTESIAN_POINT('Ctrl Pts',(-9.24134709500006,11.6,5.48820883899998));
#251459=CARTESIAN_POINT('Ctrl Pts',(-9.24379357400005,15.2,5.48885404199999));
#251460=CARTESIAN_POINT('Ctrl Pts',(-9.24379357400005,11.6,5.48885404199999));
#251461=CARTESIAN_POINT('Ctrl Pts',(-9.24624650800006,15.2,5.48949869799999));
#251462=CARTESIAN_POINT('Ctrl Pts',(-9.24624650800006,11.6,5.48949869799999));
#251463=CARTESIAN_POINT('Ctrl Pts',(-9.24870588900006,15.2,5.49014279599999));
#251464=CARTESIAN_POINT('Ctrl Pts',(-9.24870588900006,11.6,5.49014279599999));
#251465=CARTESIAN_POINT('Ctrl Pts',(-9.25117170700006,15.2,5.49078632299998));
#251466=CARTESIAN_POINT('Ctrl Pts',(-9.25117170700006,11.6,5.49078632299998));
#251467=CARTESIAN_POINT('Ctrl Pts',(-9.25364395300006,15.2,5.49142926899999));
#251468=CARTESIAN_POINT('Ctrl Pts',(-9.25364395300006,11.6,5.49142926899999));
#251469=CARTESIAN_POINT('Ctrl Pts',(-9.25612261700006,15.2,5.49207162099999));
#251470=CARTESIAN_POINT('Ctrl Pts',(-9.25612261700006,11.6,5.49207162099999));
#251471=CARTESIAN_POINT('Ctrl Pts',(-9.25860769100005,15.2,5.49271336799999));
#251472=CARTESIAN_POINT('Ctrl Pts',(-9.25860769100005,11.6,5.49271336799999));
#251473=CARTESIAN_POINT('Ctrl Pts',(-9.26109916600005,15.2,5.49335449699999));
#251474=CARTESIAN_POINT('Ctrl Pts',(-9.26109916600005,11.6,5.49335449699999));
#251475=CARTESIAN_POINT('Ctrl Pts',(-9.26359703400006,15.2,5.49399499799998));
#251476=CARTESIAN_POINT('Ctrl Pts',(-9.26359703400006,11.6,5.49399499799998));
#251477=CARTESIAN_POINT('Ctrl Pts',(-9.26610128400006,15.2,5.49463485799999));
#251478=CARTESIAN_POINT('Ctrl Pts',(-9.26610128400006,11.6,5.49463485799999));
#251479=CARTESIAN_POINT('Ctrl Pts',(-9.26861190800006,15.2,5.49527406699998));
#251480=CARTESIAN_POINT('Ctrl Pts',(-9.26861190800006,11.6,5.49527406699998));
#251481=CARTESIAN_POINT('Ctrl Pts',(-9.27112889900006,15.2,5.49591261299998));
#251482=CARTESIAN_POINT('Ctrl Pts',(-9.27112889900006,11.6,5.49591261299998));
#251483=CARTESIAN_POINT('Ctrl Pts',(-9.27365224500006,15.2,5.49655048299999));
#251484=CARTESIAN_POINT('Ctrl Pts',(-9.27365224500006,11.6,5.49655048299999));
#251485=CARTESIAN_POINT('Ctrl Pts',(-9.27618193800006,15.2,5.49718766699999));
#251486=CARTESIAN_POINT('Ctrl Pts',(-9.27618193800006,11.6,5.49718766699999));
#251487=CARTESIAN_POINT('Ctrl Pts',(-9.27871797000006,15.2,5.49782415299998));
#251488=CARTESIAN_POINT('Ctrl Pts',(-9.27871797000006,11.6,5.49782415299998));
#251489=CARTESIAN_POINT('Ctrl Pts',(-9.28126033200006,15.2,5.49845993099999));
#251490=CARTESIAN_POINT('Ctrl Pts',(-9.28126033200006,11.6,5.49845993099999));
#251491=CARTESIAN_POINT('Ctrl Pts',(-9.28380901600006,15.2,5.49909498699999));
#251492=CARTESIAN_POINT('Ctrl Pts',(-9.28380901600006,11.6,5.49909498699999));
#251493=CARTESIAN_POINT('Ctrl Pts',(-9.28636401000006,15.2,5.49972931199999));
#251494=CARTESIAN_POINT('Ctrl Pts',(-9.28636401000006,11.6,5.49972931199999));
#251495=CARTESIAN_POINT('Ctrl Pts',(-9.28892530800006,15.2,5.50036289399999));
#251496=CARTESIAN_POINT('Ctrl Pts',(-9.28892530800006,11.6,5.50036289399999));
#251497=CARTESIAN_POINT('Ctrl Pts',(-9.29149290100005,15.2,5.50099572199999));
#251498=CARTESIAN_POINT('Ctrl Pts',(-9.29149290100005,11.6,5.50099572199999));
#251499=CARTESIAN_POINT('Ctrl Pts',(-9.29406677900005,15.2,5.50162778399999));
#251500=CARTESIAN_POINT('Ctrl Pts',(-9.29406677900005,11.6,5.50162778399999));
#251501=CARTESIAN_POINT('Ctrl Pts',(-9.29664693500006,15.2,5.50225906999999));
#251502=CARTESIAN_POINT('Ctrl Pts',(-9.29664693500006,11.6,5.50225906999999));
#251503=CARTESIAN_POINT('Ctrl Pts',(-9.29923335800006,15.2,5.50288956699998));
#251504=CARTESIAN_POINT('Ctrl Pts',(-9.29923335800006,11.6,5.50288956699998));
#251505=CARTESIAN_POINT('Ctrl Pts',(-9.30182604200006,15.2,5.50351926599999));
#251506=CARTESIAN_POINT('Ctrl Pts',(-9.30182604200006,11.6,5.50351926599999));
#251507=CARTESIAN_POINT('Ctrl Pts',(-9.30442497600006,15.2,5.50414815599999));
#251508=CARTESIAN_POINT('Ctrl Pts',(-9.30442497600006,11.6,5.50414815599999));
#251509=CARTESIAN_POINT('Ctrl Pts',(-9.30703015100006,15.2,5.50477622499999));
#251510=CARTESIAN_POINT('Ctrl Pts',(-9.30703015100006,11.6,5.50477622499999));
#251511=CARTESIAN_POINT('Ctrl Pts',(-9.30964156100006,15.2,5.50540346099999));
#251512=CARTESIAN_POINT('Ctrl Pts',(-9.30964156100006,11.6,5.50540346099999));
#251513=CARTESIAN_POINT('Ctrl Pts',(-9.31225919500006,15.2,5.50602985399999));
#251514=CARTESIAN_POINT('Ctrl Pts',(-9.31225919500006,11.6,5.50602985399999));
#251515=CARTESIAN_POINT('Ctrl Pts',(-9.31488304500006,15.2,5.50665539299998));
#251516=CARTESIAN_POINT('Ctrl Pts',(-9.31488304500006,11.6,5.50665539299998));
#251517=CARTESIAN_POINT('Ctrl Pts',(-9.31751310300006,15.2,5.50728006899998));
#251518=CARTESIAN_POINT('Ctrl Pts',(-9.31751310300006,11.6,5.50728006899998));
#251519=CARTESIAN_POINT('Ctrl Pts',(-9.32014935900006,15.2,5.50790386899998));
#251520=CARTESIAN_POINT('Ctrl Pts',(-9.32014935900006,11.6,5.50790386899998));
#251521=CARTESIAN_POINT('Ctrl Pts',(-9.32279180500006,15.2,5.50852678299999));
#251522=CARTESIAN_POINT('Ctrl Pts',(-9.32279180500006,11.6,5.50852678299999));
#251523=CARTESIAN_POINT('Ctrl Pts',(-9.32544043300006,15.2,5.50914879899998));
#251524=CARTESIAN_POINT('Ctrl Pts',(-9.32544043300006,11.6,5.50914879899998));
#251525=CARTESIAN_POINT('Ctrl Pts',(-9.32809523400006,15.2,5.50976990799998));
#251526=CARTESIAN_POINT('Ctrl Pts',(-9.32809523400006,11.6,5.50976990799998));
#251527=CARTESIAN_POINT('Ctrl Pts',(-9.33075619900006,15.2,5.51039009699998));
#251528=CARTESIAN_POINT('Ctrl Pts',(-9.33075619900006,11.6,5.51039009699998));
#251529=CARTESIAN_POINT('Ctrl Pts',(-9.33342332100005,15.2,5.51100935799998));
#251530=CARTESIAN_POINT('Ctrl Pts',(-9.33342332100005,11.6,5.51100935799998));
#251531=CARTESIAN_POINT('Ctrl Pts',(-9.33609659000006,15.2,5.51162767899999));
#251532=CARTESIAN_POINT('Ctrl Pts',(-9.33609659000006,11.6,5.51162767899999));
#251533=CARTESIAN_POINT('Ctrl Pts',(-9.33877599800006,15.2,5.51224504999999));
#251534=CARTESIAN_POINT('Ctrl Pts',(-9.33877599800006,11.6,5.51224504999999));
#251535=CARTESIAN_POINT('Ctrl Pts',(-9.34146153500006,15.2,5.51286145899999));
#251536=CARTESIAN_POINT('Ctrl Pts',(-9.34146153500006,11.6,5.51286145899999));
#251537=CARTESIAN_POINT('Ctrl Pts',(-9.34415319400006,15.2,5.51347689699998));
#251538=CARTESIAN_POINT('Ctrl Pts',(-9.34415319400006,11.6,5.51347689699998));
#251539=CARTESIAN_POINT('Ctrl Pts',(-9.34685096600005,15.2,5.51409135199999));
#251540=CARTESIAN_POINT('Ctrl Pts',(-9.34685096600005,11.6,5.51409135199999));
#251541=CARTESIAN_POINT('Ctrl Pts',(-9.34955484400006,15.2,5.51470481499998));
#251542=CARTESIAN_POINT('Ctrl Pts',(-9.34955484400006,11.6,5.51470481499998));
#251543=CARTESIAN_POINT('Ctrl Pts',(-9.35226481800006,15.2,5.51531727499999));
#251544=CARTESIAN_POINT('Ctrl Pts',(-9.35226481800006,11.6,5.51531727499999));
#251545=CARTESIAN_POINT('Ctrl Pts',(-9.35498087900006,15.2,5.51592872299998));
#251546=CARTESIAN_POINT('Ctrl Pts',(-9.35498087900006,11.6,5.51592872299998));
#251547=CARTESIAN_POINT('Ctrl Pts',(-9.35770302000006,15.2,5.51653914499998));
#251548=CARTESIAN_POINT('Ctrl Pts',(-9.35770302000006,11.6,5.51653914499998));
#251549=CARTESIAN_POINT('Ctrl Pts',(-9.36043123200006,15.2,5.51714853399999));
#251550=CARTESIAN_POINT('Ctrl Pts',(-9.36043123200006,11.6,5.51714853399999));
#251551=CARTESIAN_POINT('Ctrl Pts',(-9.36316550600005,15.2,5.51775687799999));
#251552=CARTESIAN_POINT('Ctrl Pts',(-9.36316550600005,11.6,5.51775687799999));
#251553=CARTESIAN_POINT('Ctrl Pts',(-9.36590583500006,15.2,5.51836416599999));
#251554=CARTESIAN_POINT('Ctrl Pts',(-9.36590583500006,11.6,5.51836416599999));
#251555=CARTESIAN_POINT('Ctrl Pts',(-9.36865220900006,15.2,5.51897039099998));
#251556=CARTESIAN_POINT('Ctrl Pts',(-9.36865220900006,11.6,5.51897039099998));
#251557=CARTESIAN_POINT('Ctrl Pts',(-9.37140462000006,15.2,5.51957553899998));
#251558=CARTESIAN_POINT('Ctrl Pts',(-9.37140462000006,11.6,5.51957553899998));
#251559=CARTESIAN_POINT('Ctrl Pts',(-9.37416306100006,15.2,5.52017960199999));
#251560=CARTESIAN_POINT('Ctrl Pts',(-9.37416306100006,11.6,5.52017960199999));
#251561=CARTESIAN_POINT('Ctrl Pts',(-9.37692752300006,15.2,5.52078256899998));
#251562=CARTESIAN_POINT('Ctrl Pts',(-9.37692752300006,11.6,5.52078256899998));
#251563=CARTESIAN_POINT('Ctrl Pts',(-9.37969799600006,15.2,5.52138443099999));
#251564=CARTESIAN_POINT('Ctrl Pts',(-9.37969799600006,11.6,5.52138443099999));
#251565=CARTESIAN_POINT('Ctrl Pts',(-9.38247447400006,15.2,5.52198517699999));
#251566=CARTESIAN_POINT('Ctrl Pts',(-9.38247447400006,11.6,5.52198517699999));
#251567=CARTESIAN_POINT('Ctrl Pts',(-9.38525694800006,15.2,5.52258479699999));
#251568=CARTESIAN_POINT('Ctrl Pts',(-9.38525694800006,11.6,5.52258479699999));
#251569=CARTESIAN_POINT('Ctrl Pts',(-9.38804540900006,15.2,5.52318327999998));
#251570=CARTESIAN_POINT('Ctrl Pts',(-9.38804540900006,11.6,5.52318327999998));
#251571=CARTESIAN_POINT('Ctrl Pts',(-9.39083984900006,15.2,5.52378061799998));
#251572=CARTESIAN_POINT('Ctrl Pts',(-9.39083984900006,11.6,5.52378061799998));
#251573=CARTESIAN_POINT('Ctrl Pts',(-9.39364025900005,15.2,5.52437679899998));
#251574=CARTESIAN_POINT('Ctrl Pts',(-9.39364025900005,11.6,5.52437679899998));
#251575=CARTESIAN_POINT('Ctrl Pts',(-9.39644663200006,15.2,5.52497181399998));
#251576=CARTESIAN_POINT('Ctrl Pts',(-9.39644663200006,11.6,5.52497181399998));
#251577=CARTESIAN_POINT('Ctrl Pts',(-9.39925896000006,15.2,5.52556565399998));
#251578=CARTESIAN_POINT('Ctrl Pts',(-9.39925896000006,11.6,5.52556565399998));
#251579=CARTESIAN_POINT('Ctrl Pts',(-9.40207723400006,15.2,5.52615830699998));
#251580=CARTESIAN_POINT('Ctrl Pts',(-9.40207723400006,11.6,5.52615830699998));
#251581=CARTESIAN_POINT('Ctrl Pts',(-9.40490144600006,15.2,5.52674976499999));
#251582=CARTESIAN_POINT('Ctrl Pts',(-9.40490144600006,11.6,5.52674976499999));
#251583=CARTESIAN_POINT('Ctrl Pts',(-9.40773158700006,15.2,5.52734001699999));
#251584=CARTESIAN_POINT('Ctrl Pts',(-9.40773158700006,11.6,5.52734001699999));
#251585=CARTESIAN_POINT('Ctrl Pts',(-9.41056765000006,15.2,5.52792905499999));
#251586=CARTESIAN_POINT('Ctrl Pts',(-9.41056765000006,11.6,5.52792905499999));
#251587=CARTESIAN_POINT('Ctrl Pts',(-9.41340962600006,15.2,5.52851686599999));
#251588=CARTESIAN_POINT('Ctrl Pts',(-9.41340962600006,11.6,5.52851686599999));
#251589=CARTESIAN_POINT('Ctrl Pts',(-9.41625750700006,15.2,5.52910344399999));
#251590=CARTESIAN_POINT('Ctrl Pts',(-9.41625750700006,11.6,5.52910344399999));
#251591=CARTESIAN_POINT('Ctrl Pts',(-9.41911128500006,15.2,5.52968877599999));
#251592=CARTESIAN_POINT('Ctrl Pts',(-9.41911128500006,11.6,5.52968877599999));
#251593=CARTESIAN_POINT('Ctrl Pts',(-9.42197095100006,15.2,5.53027285299999));
#251594=CARTESIAN_POINT('Ctrl Pts',(-9.42197095100006,11.6,5.53027285299999));
#251595=CARTESIAN_POINT('Ctrl Pts',(-9.42483649800005,15.2,5.53085566799999));
#251596=CARTESIAN_POINT('Ctrl Pts',(-9.42483649800005,11.6,5.53085566799999));
#251597=CARTESIAN_POINT('Ctrl Pts',(-9.42770791800006,15.2,5.53143720799999));
#251598=CARTESIAN_POINT('Ctrl Pts',(-9.42770791800006,11.6,5.53143720799999));
#251599=CARTESIAN_POINT('Ctrl Pts',(-9.43058520300006,15.2,5.53201746599999));
#251600=CARTESIAN_POINT('Ctrl Pts',(-9.43058520300006,11.6,5.53201746599999));
#251601=CARTESIAN_POINT('Ctrl Pts',(-9.43346834300005,15.2,5.53259642999999));
#251602=CARTESIAN_POINT('Ctrl Pts',(-9.43346834300005,11.6,5.53259642999999));
#251603=CARTESIAN_POINT('Ctrl Pts',(-9.43635733100006,15.2,5.53317409299999));
#251604=CARTESIAN_POINT('Ctrl Pts',(-9.43635733100006,11.6,5.53317409299999));
#251605=CARTESIAN_POINT('Ctrl Pts',(-9.43925215900006,15.2,5.53375044299998));
#251606=CARTESIAN_POINT('Ctrl Pts',(-9.43925215900006,11.6,5.53375044299998));
#251607=CARTESIAN_POINT('Ctrl Pts',(-9.44215282000006,15.2,5.53432547199999));
#251608=CARTESIAN_POINT('Ctrl Pts',(-9.44215282000006,11.6,5.53432547199999));
#251609=CARTESIAN_POINT('Ctrl Pts',(-9.44505930500006,15.2,5.53489916999998));
#251610=CARTESIAN_POINT('Ctrl Pts',(-9.44505930500006,11.6,5.53489916999998));
#251611=CARTESIAN_POINT('Ctrl Pts',(-9.44797160500006,15.2,5.53547152899998));
#251612=CARTESIAN_POINT('Ctrl Pts',(-9.44797160500006,11.6,5.53547152899998));
#251613=CARTESIAN_POINT('Ctrl Pts',(-9.45088971300006,15.2,5.53604253699999));
#251614=CARTESIAN_POINT('Ctrl Pts',(-9.45088971300006,11.6,5.53604253699999));
#251615=CARTESIAN_POINT('Ctrl Pts',(-9.45381362100006,15.2,5.53661218699999));
#251616=CARTESIAN_POINT('Ctrl Pts',(-9.45381362100006,11.6,5.53661218699999));
#251617=CARTESIAN_POINT('Ctrl Pts',(-9.45674332000005,15.2,5.53718046699998));
#251618=CARTESIAN_POINT('Ctrl Pts',(-9.45674332000005,11.6,5.53718046699998));
#251619=CARTESIAN_POINT('Ctrl Pts',(-9.45967880400006,15.2,5.53774737099998));
#251620=CARTESIAN_POINT('Ctrl Pts',(-9.45967880400006,11.6,5.53774737099998));
#251621=CARTESIAN_POINT('Ctrl Pts',(-9.46262006300006,15.2,5.53831288699998));
#251622=CARTESIAN_POINT('Ctrl Pts',(-9.46262006300006,11.6,5.53831288699998));
#251623=CARTESIAN_POINT('Ctrl Pts',(-9.46556709000006,15.2,5.53887700699998));
#251624=CARTESIAN_POINT('Ctrl Pts',(-9.46556709000006,11.6,5.53887700699998));
#251625=CARTESIAN_POINT('Ctrl Pts',(-9.46851987800006,15.2,5.53943972199999));
#251626=CARTESIAN_POINT('Ctrl Pts',(-9.46851987800006,11.6,5.53943972199999));
#251627=CARTESIAN_POINT('Ctrl Pts',(-9.47147841600006,15.2,5.54000102199999));
#251628=CARTESIAN_POINT('Ctrl Pts',(-9.47147841600006,11.6,5.54000102199999));
#251629=CARTESIAN_POINT('Ctrl Pts',(-9.47444269900006,15.2,5.54056089699999));
#251630=CARTESIAN_POINT('Ctrl Pts',(-9.47444269900006,11.6,5.54056089699999));
#251631=CARTESIAN_POINT('Ctrl Pts',(-9.47741271700006,15.2,5.54111933999998));
#251632=CARTESIAN_POINT('Ctrl Pts',(-9.47741271700006,11.6,5.54111933999998));
#251633=CARTESIAN_POINT('Ctrl Pts',(-9.48038846400006,15.2,5.54167634099999));
#251634=CARTESIAN_POINT('Ctrl Pts',(-9.48038846400006,11.6,5.54167634099999));
#251635=CARTESIAN_POINT('Ctrl Pts',(-9.48336993000006,15.2,5.54223188999998));
#251636=CARTESIAN_POINT('Ctrl Pts',(-9.48336993000006,11.6,5.54223188999998));
#251637=CARTESIAN_POINT('Ctrl Pts',(-9.48635711000006,15.2,5.54278597899999));
#251638=CARTESIAN_POINT('Ctrl Pts',(-9.48635711000006,11.6,5.54278597899999));
#251639=CARTESIAN_POINT('Ctrl Pts',(-9.48934999300005,15.2,5.54333859899998));
#251640=CARTESIAN_POINT('Ctrl Pts',(-9.48934999300005,11.6,5.54333859899998));
#251641=CARTESIAN_POINT('Ctrl Pts',(-9.49234857200006,15.2,5.54388973899999));
#251642=CARTESIAN_POINT('Ctrl Pts',(-9.49234857200006,11.6,5.54388973899999));
#251643=CARTESIAN_POINT('Ctrl Pts',(-9.49535284000006,15.2,5.54443939299999));
#251644=CARTESIAN_POINT('Ctrl Pts',(-9.49535284000006,11.6,5.54443939299999));
#251645=CARTESIAN_POINT('Ctrl Pts',(-9.49836278900005,15.2,5.54498754999998));
#251646=CARTESIAN_POINT('Ctrl Pts',(-9.49836278900005,11.6,5.54498754999998));
#251647=CARTESIAN_POINT('Ctrl Pts',(-9.50137841100006,15.2,5.54553420099998));
#251648=CARTESIAN_POINT('Ctrl Pts',(-9.50137841100006,11.6,5.54553420099998));
#251649=CARTESIAN_POINT('Ctrl Pts',(-9.50439969700006,15.2,5.54607933899998));
#251650=CARTESIAN_POINT('Ctrl Pts',(-9.50439969700006,11.6,5.54607933899998));
#251651=CARTESIAN_POINT('Ctrl Pts',(-9.50742664100006,15.2,5.54662295199999));
#251652=CARTESIAN_POINT('Ctrl Pts',(-9.50742664100006,11.6,5.54662295199999));
#251653=CARTESIAN_POINT('Ctrl Pts',(-9.51045923400006,15.2,5.54716503299999));
#251654=CARTESIAN_POINT('Ctrl Pts',(-9.51045923400006,11.6,5.54716503299999));
#251655=CARTESIAN_POINT('Ctrl Pts',(-9.51349746800006,15.2,5.54770557499998));
#251656=CARTESIAN_POINT('Ctrl Pts',(-9.51349746800006,11.6,5.54770557499998));
#251657=CARTESIAN_POINT('Ctrl Pts',(-9.51654133700006,15.2,5.54824456499999));
#251658=CARTESIAN_POINT('Ctrl Pts',(-9.51654133700006,11.6,5.54824456499999));
#251659=CARTESIAN_POINT('Ctrl Pts',(-9.51959083100006,15.2,5.54878199699999));
#251660=CARTESIAN_POINT('Ctrl Pts',(-9.51959083100006,11.6,5.54878199699999));
#251661=CARTESIAN_POINT('Ctrl Pts',(-9.52264594400006,15.2,5.54931786199998));
#251662=CARTESIAN_POINT('Ctrl Pts',(-9.52264594400006,11.6,5.54931786199998));
#251663=CARTESIAN_POINT('Ctrl Pts',(-9.52570666500005,15.2,5.54985215099999));
#251664=CARTESIAN_POINT('Ctrl Pts',(-9.52570666500005,11.6,5.54985215099999));
#251665=CARTESIAN_POINT('Ctrl Pts',(-9.52877299100006,15.2,5.55038485499999));
#251666=CARTESIAN_POINT('Ctrl Pts',(-9.52877299100006,11.6,5.55038485499999));
#251667=CARTESIAN_POINT('Ctrl Pts',(-9.53184491100006,15.2,5.55091596499998));
#251668=CARTESIAN_POINT('Ctrl Pts',(-9.53184491100006,11.6,5.55091596499998));
#251669=CARTESIAN_POINT('Ctrl Pts',(-9.53492241700006,15.2,5.55144547299999));
#251670=CARTESIAN_POINT('Ctrl Pts',(-9.53492241700006,11.6,5.55144547299999));
#251671=CARTESIAN_POINT('Ctrl Pts',(-9.53800550500005,15.2,5.55197336999999));
#251672=CARTESIAN_POINT('Ctrl Pts',(-9.53800550500005,11.6,5.55197336999999));
#251673=CARTESIAN_POINT('Ctrl Pts',(-9.54109416200006,15.2,5.55249964699998));
#251674=CARTESIAN_POINT('Ctrl Pts',(-9.54109416200006,11.6,5.55249964699998));
#251675=CARTESIAN_POINT('Ctrl Pts',(-9.54418838400005,15.2,5.55302429599998));
#251676=CARTESIAN_POINT('Ctrl Pts',(-9.54418838400005,11.6,5.55302429599998));
#251677=CARTESIAN_POINT('Ctrl Pts',(-9.54728816200006,15.2,5.55354730899998));
#251678=CARTESIAN_POINT('Ctrl Pts',(-9.54728816200006,11.6,5.55354730899998));
#251679=CARTESIAN_POINT('Ctrl Pts',(-9.55039348900005,15.2,5.55406867699999));
#251680=CARTESIAN_POINT('Ctrl Pts',(-9.55039348900005,11.6,5.55406867699999));
#251681=CARTESIAN_POINT('Ctrl Pts',(-9.55350435500005,15.2,5.55458838999999));
#251682=CARTESIAN_POINT('Ctrl Pts',(-9.55350435500005,11.6,5.55458838999999));
#251683=CARTESIAN_POINT('Ctrl Pts',(-9.55662075600006,15.2,5.55510644099999));
#251684=CARTESIAN_POINT('Ctrl Pts',(-9.55662075600006,11.6,5.55510644099999));
#251685=CARTESIAN_POINT('Ctrl Pts',(-9.55974268200006,15.2,5.55562282199999));
#251686=CARTESIAN_POINT('Ctrl Pts',(-9.55974268200006,11.6,5.55562282199999));
#251687=CARTESIAN_POINT('Ctrl Pts',(-9.56287012600006,15.2,5.55613752299998));
#251688=CARTESIAN_POINT('Ctrl Pts',(-9.56287012600006,11.6,5.55613752299998));
#251689=CARTESIAN_POINT('Ctrl Pts',(-9.56600308000005,15.2,5.55665053699999));
#251690=CARTESIAN_POINT('Ctrl Pts',(-9.56600308000005,11.6,5.55665053699999));
#251691=CARTESIAN_POINT('Ctrl Pts',(-9.56914153600006,15.2,5.55716185399999));
#251692=CARTESIAN_POINT('Ctrl Pts',(-9.56914153600006,11.6,5.55716185399999));
#251693=CARTESIAN_POINT('Ctrl Pts',(-9.57228548800006,15.2,5.55767146699999));
#251694=CARTESIAN_POINT('Ctrl Pts',(-9.57228548800006,11.6,5.55767146699999));
#251695=CARTESIAN_POINT('Ctrl Pts',(-9.57543492600006,15.2,5.55817936699999));
#251696=CARTESIAN_POINT('Ctrl Pts',(-9.57543492600006,11.6,5.55817936699999));
#251697=CARTESIAN_POINT('Ctrl Pts',(-9.57858984400006,15.2,5.55868554599999));
#251698=CARTESIAN_POINT('Ctrl Pts',(-9.57858984400006,11.6,5.55868554599999));
#251699=CARTESIAN_POINT('Ctrl Pts',(-9.58175023400005,15.2,5.55918999599999));
#251700=CARTESIAN_POINT('Ctrl Pts',(-9.58175023400005,11.6,5.55918999599999));
#251701=CARTESIAN_POINT('Ctrl Pts',(-9.58491608900006,15.2,5.55969270699999));
#251702=CARTESIAN_POINT('Ctrl Pts',(-9.58491608900006,11.6,5.55969270699999));
#251703=CARTESIAN_POINT('Ctrl Pts',(-9.58808740100006,15.2,5.56019367399998));
#251704=CARTESIAN_POINT('Ctrl Pts',(-9.58808740100006,11.6,5.56019367399998));
#251705=CARTESIAN_POINT('Ctrl Pts',(-9.59126416200006,15.2,5.56069288399998));
#251706=CARTESIAN_POINT('Ctrl Pts',(-9.59126416200006,11.6,5.56069288399998));
#251707=CARTESIAN_POINT('Ctrl Pts',(-9.59444636500006,15.2,5.56119033399998));
#251708=CARTESIAN_POINT('Ctrl Pts',(-9.59444636500006,11.6,5.56119033399998));
#251709=CARTESIAN_POINT('Ctrl Pts',(-9.59763400200006,15.2,5.56168601199998));
#251710=CARTESIAN_POINT('Ctrl Pts',(-9.59763400200006,11.6,5.56168601199998));
#251711=CARTESIAN_POINT('Ctrl Pts',(-9.60082706500006,15.2,5.56217991099999));
#251712=CARTESIAN_POINT('Ctrl Pts',(-9.60082706500006,11.6,5.56217991099999));
#251713=CARTESIAN_POINT('Ctrl Pts',(-9.60402554800006,15.2,5.56267202299999));
#251714=CARTESIAN_POINT('Ctrl Pts',(-9.60402554800006,11.6,5.56267202299999));
#251715=CARTESIAN_POINT('Ctrl Pts',(-9.60722944200005,15.2,5.56316234099998));
#251716=CARTESIAN_POINT('Ctrl Pts',(-9.60722944200005,11.6,5.56316234099998));
#251717=CARTESIAN_POINT('Ctrl Pts',(-9.61043874100006,15.2,5.56365085399998));
#251718=CARTESIAN_POINT('Ctrl Pts',(-9.61043874100006,11.6,5.56365085399998));
#251719=CARTESIAN_POINT('Ctrl Pts',(-9.61365343600006,15.2,5.56413755599999));
#251720=CARTESIAN_POINT('Ctrl Pts',(-9.61365343600006,11.6,5.56413755599999));
#251721=CARTESIAN_POINT('Ctrl Pts',(-9.61687352100006,15.2,5.56462243899999));
#251722=CARTESIAN_POINT('Ctrl Pts',(-9.61687352100006,11.6,5.56462243899999));
#251723=CARTESIAN_POINT('Ctrl Pts',(-9.62009898600006,15.2,5.56510549499999));
#251724=CARTESIAN_POINT('Ctrl Pts',(-9.62009898600006,11.6,5.56510549499999));
#251725=CARTESIAN_POINT('Ctrl Pts',(-9.62332982600006,15.2,5.56558671499998));
#251726=CARTESIAN_POINT('Ctrl Pts',(-9.62332982600006,11.6,5.56558671499998));
#251727=CARTESIAN_POINT('Ctrl Pts',(-9.62656603200006,15.2,5.56606609099998));
#251728=CARTESIAN_POINT('Ctrl Pts',(-9.62656603200006,11.6,5.56606609099998));
#251729=CARTESIAN_POINT('Ctrl Pts',(-9.62980759800006,15.2,5.56654361499999));
#251730=CARTESIAN_POINT('Ctrl Pts',(-9.62980759800006,11.6,5.56654361499999));
#251731=CARTESIAN_POINT('Ctrl Pts',(-9.63305451500006,15.2,5.56701928099999));
#251732=CARTESIAN_POINT('Ctrl Pts',(-9.63305451500006,11.6,5.56701928099999));
#251733=CARTESIAN_POINT('Ctrl Pts',(-9.63630677600005,15.2,5.56749307899998));
#251734=CARTESIAN_POINT('Ctrl Pts',(-9.63630677600005,11.6,5.56749307899998));
#251735=CARTESIAN_POINT('Ctrl Pts',(-9.63956437500006,15.2,5.56796500199999));
#251736=CARTESIAN_POINT('Ctrl Pts',(-9.63956437500006,11.6,5.56796500199999));
#251737=CARTESIAN_POINT('Ctrl Pts',(-9.64282730300006,15.2,5.56843504199998));
#251738=CARTESIAN_POINT('Ctrl Pts',(-9.64282730300006,11.6,5.56843504199998));
#251739=CARTESIAN_POINT('Ctrl Pts',(-9.64609555300006,15.2,5.56890318999999));
#251740=CARTESIAN_POINT('Ctrl Pts',(-9.64609555300006,11.6,5.56890318999999));
#251741=CARTESIAN_POINT('Ctrl Pts',(-9.64936911700006,15.2,5.56936944099998));
#251742=CARTESIAN_POINT('Ctrl Pts',(-9.64936911700006,11.6,5.56936944099998));
#251743=CARTESIAN_POINT('Ctrl Pts',(-9.65264798900006,15.2,5.56983378399998));
#251744=CARTESIAN_POINT('Ctrl Pts',(-9.65264798900006,11.6,5.56983378399998));
#251745=CARTESIAN_POINT('Ctrl Pts',(-9.65593215900006,15.2,5.57029621199998));
#251746=CARTESIAN_POINT('Ctrl Pts',(-9.65593215900006,11.6,5.57029621199998));
#251747=CARTESIAN_POINT('Ctrl Pts',(-9.65922162400006,15.2,5.57075671799999));
#251748=CARTESIAN_POINT('Ctrl Pts',(-9.65922162400006,11.6,5.57075671799999));
#251749=CARTESIAN_POINT('Ctrl Pts',(-9.66251637200006,15.2,5.57121529599998));
#251750=CARTESIAN_POINT('Ctrl Pts',(-9.66251637200006,11.6,5.57121529599998));
#251751=CARTESIAN_POINT('Ctrl Pts',(-9.66581639800006,15.2,5.57167193399999));
#251752=CARTESIAN_POINT('Ctrl Pts',(-9.66581639800006,11.6,5.57167193399999));
#251753=CARTESIAN_POINT('Ctrl Pts',(-9.66912169500005,15.2,5.57212662699998));
#251754=CARTESIAN_POINT('Ctrl Pts',(-9.66912169500005,11.6,5.57212662699998));
#251755=CARTESIAN_POINT('Ctrl Pts',(-9.67243225500006,15.2,5.57257936599999));
#251756=CARTESIAN_POINT('Ctrl Pts',(-9.67243225500006,11.6,5.57257936599999));
#251757=CARTESIAN_POINT('Ctrl Pts',(-9.67574806900006,15.2,5.57303014499999));
#251758=CARTESIAN_POINT('Ctrl Pts',(-9.67574806900006,11.6,5.57303014499999));
#251759=CARTESIAN_POINT('Ctrl Pts',(-9.67906913300006,15.2,5.57347895599998));
#251760=CARTESIAN_POINT('Ctrl Pts',(-9.67906913300006,11.6,5.57347895599998));
#251761=CARTESIAN_POINT('Ctrl Pts',(-9.68239543700006,15.2,5.57392579099999));
#251762=CARTESIAN_POINT('Ctrl Pts',(-9.68239543700006,11.6,5.57392579099999));
#251763=CARTESIAN_POINT('Ctrl Pts',(-9.68572697500005,15.2,5.57437064099998));
#251764=CARTESIAN_POINT('Ctrl Pts',(-9.68572697500005,11.6,5.57437064099998));
#251765=CARTESIAN_POINT('Ctrl Pts',(-9.68906374000005,15.2,5.57481349999998));
#251766=CARTESIAN_POINT('Ctrl Pts',(-9.68906374000005,11.6,5.57481349999998));
#251767=CARTESIAN_POINT('Ctrl Pts',(-9.69240572300006,15.2,5.57525436099999));
#251768=CARTESIAN_POINT('Ctrl Pts',(-9.69240572300006,11.6,5.57525436099999));
#251769=CARTESIAN_POINT('Ctrl Pts',(-9.69575291800006,15.2,5.57569321499999));
#251770=CARTESIAN_POINT('Ctrl Pts',(-9.69575291800006,11.6,5.57569321499999));
#251771=CARTESIAN_POINT('Ctrl Pts',(-9.69910531700006,15.2,5.57613005499999));
#251772=CARTESIAN_POINT('Ctrl Pts',(-9.69910531700006,11.6,5.57613005499999));
#251773=CARTESIAN_POINT('Ctrl Pts',(-9.70246291400005,15.2,5.57656487399999));
#251774=CARTESIAN_POINT('Ctrl Pts',(-9.70246291400005,11.6,5.57656487399999));
#251775=CARTESIAN_POINT('Ctrl Pts',(-9.70582569900006,15.2,5.57699766299999));
#251776=CARTESIAN_POINT('Ctrl Pts',(-9.70582569900006,11.6,5.57699766299999));
#251777=CARTESIAN_POINT('Ctrl Pts',(-9.70919366900005,15.2,5.57742841599998));
#251778=CARTESIAN_POINT('Ctrl Pts',(-9.70919366900005,11.6,5.57742841599998));
#251779=CARTESIAN_POINT('Ctrl Pts',(-9.71256681200006,15.2,5.57785712499999));
#251780=CARTESIAN_POINT('Ctrl Pts',(-9.71256681200006,11.6,5.57785712499999));
#251781=CARTESIAN_POINT('Ctrl Pts',(-9.71594512500005,15.2,5.57828378299998));
#251782=CARTESIAN_POINT('Ctrl Pts',(-9.71594512500005,11.6,5.57828378299998));
#251783=CARTESIAN_POINT('Ctrl Pts',(-9.71932859800006,15.2,5.57870838199998));
#251784=CARTESIAN_POINT('Ctrl Pts',(-9.71932859800006,11.6,5.57870838199998));
#251785=CARTESIAN_POINT('Ctrl Pts',(-9.72271722500006,15.2,5.57913091399998));
#251786=CARTESIAN_POINT('Ctrl Pts',(-9.72271722500006,11.6,5.57913091399998));
#251787=CARTESIAN_POINT('Ctrl Pts',(-9.72611099800006,15.2,5.57955137399999));
#251788=CARTESIAN_POINT('Ctrl Pts',(-9.72611099800006,11.6,5.57955137399999));
#251789=CARTESIAN_POINT('Ctrl Pts',(-9.72950991000006,15.2,5.57996975199998));
#251790=CARTESIAN_POINT('Ctrl Pts',(-9.72950991000006,11.6,5.57996975199998));
#251791=CARTESIAN_POINT('Ctrl Pts',(-9.73291395500006,15.2,5.58038604299998));
#251792=CARTESIAN_POINT('Ctrl Pts',(-9.73291395500006,11.6,5.58038604299998));
#251793=CARTESIAN_POINT('Ctrl Pts',(-9.73632312400006,15.2,5.58080023799998));
#251794=CARTESIAN_POINT('Ctrl Pts',(-9.73632312400006,11.6,5.58080023799998));
#251795=CARTESIAN_POINT('Ctrl Pts',(-9.73973741000006,15.2,5.58121232999999));
#251796=CARTESIAN_POINT('Ctrl Pts',(-9.73973741000006,11.6,5.58121232999999));
#251797=CARTESIAN_POINT('Ctrl Pts',(-9.74315680900006,15.2,5.58162231199999));
#251798=CARTESIAN_POINT('Ctrl Pts',(-9.74315680900006,11.6,5.58162231199999));
#251799=CARTESIAN_POINT('Ctrl Pts',(-9.74658130800006,15.2,5.58203017699999));
#251800=CARTESIAN_POINT('Ctrl Pts',(-9.74658130800006,11.6,5.58203017699999));
#251801=CARTESIAN_POINT('Ctrl Pts',(-9.75001090500006,15.2,5.58243591699998));
#251802=CARTESIAN_POINT('Ctrl Pts',(-9.75001090500006,11.6,5.58243591699998));
#251803=CARTESIAN_POINT('Ctrl Pts',(-9.75344559100006,15.2,5.58283952599999));
#251804=CARTESIAN_POINT('Ctrl Pts',(-9.75344559100006,11.6,5.58283952599999));
#251805=CARTESIAN_POINT('Ctrl Pts',(-9.75688535800005,15.2,5.58324099599999));
#251806=CARTESIAN_POINT('Ctrl Pts',(-9.75688535800005,11.6,5.58324099599999));
#251807=CARTESIAN_POINT('Ctrl Pts',(-9.76033020000006,15.2,5.58364031899998));
#251808=CARTESIAN_POINT('Ctrl Pts',(-9.76033020000006,11.6,5.58364031899998));
#251809=CARTESIAN_POINT('Ctrl Pts',(-9.76378010900006,15.2,5.58403748999999));
#251810=CARTESIAN_POINT('Ctrl Pts',(-9.76378010900006,11.6,5.58403748999999));
#251811=CARTESIAN_POINT('Ctrl Pts',(-9.76723507900006,15.2,5.58443249899998));
#251812=CARTESIAN_POINT('Ctrl Pts',(-9.76723507900006,11.6,5.58443249899998));
#251813=CARTESIAN_POINT('Ctrl Pts',(-9.77069510200005,15.2,5.58482534199998));
#251814=CARTESIAN_POINT('Ctrl Pts',(-9.77069510200005,11.6,5.58482534199998));
#251815=CARTESIAN_POINT('Ctrl Pts',(-9.77416017100006,15.2,5.58521600999998));
#251816=CARTESIAN_POINT('Ctrl Pts',(-9.77416017100006,11.6,5.58521600999998));
#251817=CARTESIAN_POINT('Ctrl Pts',(-9.77763027800006,15.2,5.58560449599998));
#251818=CARTESIAN_POINT('Ctrl Pts',(-9.77763027800006,11.6,5.58560449599998));
#251819=CARTESIAN_POINT('Ctrl Pts',(-9.78110541800006,15.2,5.58599079299999));
#251820=CARTESIAN_POINT('Ctrl Pts',(-9.78110541800006,11.6,5.58599079299999));
#251821=CARTESIAN_POINT('Ctrl Pts',(-9.78458558400006,15.2,5.58637489499999));
#251822=CARTESIAN_POINT('Ctrl Pts',(-9.78458558400006,11.6,5.58637489499999));
#251823=CARTESIAN_POINT('Ctrl Pts',(-9.78807076600006,15.2,5.58675679399999));
#251824=CARTESIAN_POINT('Ctrl Pts',(-9.78807076600006,11.6,5.58675679399999));
#251825=CARTESIAN_POINT('Ctrl Pts',(-9.79156095900005,15.2,5.58713648399999));
#251826=CARTESIAN_POINT('Ctrl Pts',(-9.79156095900005,11.6,5.58713648399999));
#251827=CARTESIAN_POINT('Ctrl Pts',(-9.79505615600005,15.2,5.58751395499999));
#251828=CARTESIAN_POINT('Ctrl Pts',(-9.79505615600005,11.6,5.58751395499999));
#251829=CARTESIAN_POINT('Ctrl Pts',(-9.79855634900006,15.2,5.58788920399999));
#251830=CARTESIAN_POINT('Ctrl Pts',(-9.79855634900006,11.6,5.58788920399999));
#251831=CARTESIAN_POINT('Ctrl Pts',(-9.80206153200006,15.2,5.58826222199999));
#251832=CARTESIAN_POINT('Ctrl Pts',(-9.80206153200006,11.6,5.58826222199999));
#251833=CARTESIAN_POINT('Ctrl Pts',(-9.80557169700005,15.2,5.58863300199998));
#251834=CARTESIAN_POINT('Ctrl Pts',(-9.80557169700005,11.6,5.58863300199998));
#251835=CARTESIAN_POINT('Ctrl Pts',(-9.80908683800006,15.2,5.58900153799998));
#251836=CARTESIAN_POINT('Ctrl Pts',(-9.80908683800006,11.6,5.58900153799998));
#251837=CARTESIAN_POINT('Ctrl Pts',(-9.81260694600006,15.2,5.58936782199999));
#251838=CARTESIAN_POINT('Ctrl Pts',(-9.81260694600006,11.6,5.58936782199999));
#251839=CARTESIAN_POINT('Ctrl Pts',(-9.81613201600006,15.2,5.58973184899998));
#251840=CARTESIAN_POINT('Ctrl Pts',(-9.81613201600006,11.6,5.58973184899998));
#251841=CARTESIAN_POINT('Ctrl Pts',(-9.81966204100006,15.2,5.59009360999998));
#251842=CARTESIAN_POINT('Ctrl Pts',(-9.81966204100006,11.6,5.59009360999998));
#251843=CARTESIAN_POINT('Ctrl Pts',(-9.82319701200005,15.2,5.59045309799998));
#251844=CARTESIAN_POINT('Ctrl Pts',(-9.82319701200005,11.6,5.59045309799998));
#251845=CARTESIAN_POINT('Ctrl Pts',(-9.82673692500006,15.2,5.59081030799998));
#251846=CARTESIAN_POINT('Ctrl Pts',(-9.82673692500006,11.6,5.59081030799998));
#251847=CARTESIAN_POINT('Ctrl Pts',(-9.83028177000006,15.2,5.59116523399998));
#251848=CARTESIAN_POINT('Ctrl Pts',(-9.83028177000006,11.6,5.59116523399998));
#251849=CARTESIAN_POINT('Ctrl Pts',(-9.83383154200006,15.2,5.59151786499999));
#251850=CARTESIAN_POINT('Ctrl Pts',(-9.83383154200006,11.6,5.59151786499999));
#251851=CARTESIAN_POINT('Ctrl Pts',(-9.83738623300006,15.2,5.59186819799999));
#251852=CARTESIAN_POINT('Ctrl Pts',(-9.83738623300006,11.6,5.59186819799999));
#251853=CARTESIAN_POINT('Ctrl Pts',(-9.84094583600006,15.2,5.59221622599999));
#251854=CARTESIAN_POINT('Ctrl Pts',(-9.84094583600006,11.6,5.59221622599999));
#251855=CARTESIAN_POINT('Ctrl Pts',(-9.84451034500006,15.2,5.59256193999998));
#251856=CARTESIAN_POINT('Ctrl Pts',(-9.84451034500006,11.6,5.59256193999998));
#251857=CARTESIAN_POINT('Ctrl Pts',(-9.84807975200006,15.2,5.59290533499999));
#251858=CARTESIAN_POINT('Ctrl Pts',(-9.84807975200006,11.6,5.59290533499999));
#251859=CARTESIAN_POINT('Ctrl Pts',(-9.85165405100006,15.2,5.59324640399999));
#251860=CARTESIAN_POINT('Ctrl Pts',(-9.85165405100006,11.6,5.59324640399999));
#251861=CARTESIAN_POINT('Ctrl Pts',(-9.85523323300006,15.2,5.59358514099999));
#251862=CARTESIAN_POINT('Ctrl Pts',(-9.85523323300006,11.6,5.59358514099999));
#251863=CARTESIAN_POINT('Ctrl Pts',(-9.85881729400005,15.2,5.59392153799998));
#251864=CARTESIAN_POINT('Ctrl Pts',(-9.85881729400005,11.6,5.59392153799998));
#251865=CARTESIAN_POINT('Ctrl Pts',(-9.86240622600006,15.2,5.59425558899999));
#251866=CARTESIAN_POINT('Ctrl Pts',(-9.86240622600006,11.6,5.59425558899999));
#251867=CARTESIAN_POINT('Ctrl Pts',(-9.86600002100005,15.2,5.59458728699998));
#251868=CARTESIAN_POINT('Ctrl Pts',(-9.86600002100005,11.6,5.59458728699998));
#251869=CARTESIAN_POINT('Ctrl Pts',(-9.86959867100006,15.2,5.59491662699998));
#251870=CARTESIAN_POINT('Ctrl Pts',(-9.86959867100006,11.6,5.59491662699998));
#251871=CARTESIAN_POINT('Ctrl Pts',(-9.87320217400006,15.2,5.59524360099999));
#251872=CARTESIAN_POINT('Ctrl Pts',(-9.87320217400006,11.6,5.59524360099999));
#251873=CARTESIAN_POINT('Ctrl Pts',(-9.87681051700006,15.2,5.59556820099999));
#251874=CARTESIAN_POINT('Ctrl Pts',(-9.87681051700006,11.6,5.59556820099999));
#251875=CARTESIAN_POINT('Ctrl Pts',(-9.88042369800005,15.2,5.59589042299999));
#251876=CARTESIAN_POINT('Ctrl Pts',(-9.88042369800005,11.6,5.59589042299999));
#251877=CARTESIAN_POINT('Ctrl Pts',(-9.88404170800005,15.2,5.59621025999999));
#251878=CARTESIAN_POINT('Ctrl Pts',(-9.88404170800005,11.6,5.59621025999999));
#251879=CARTESIAN_POINT('Ctrl Pts',(-9.88766454000006,15.2,5.59652770399998));
#251880=CARTESIAN_POINT('Ctrl Pts',(-9.88766454000006,11.6,5.59652770399998));
#251881=CARTESIAN_POINT('Ctrl Pts',(-9.89129218700005,15.2,5.59684274999999));
#251882=CARTESIAN_POINT('Ctrl Pts',(-9.89129218700005,11.6,5.59684274999999));
#251883=CARTESIAN_POINT('Ctrl Pts',(-9.89492464300006,15.2,5.59715539099999));
#251884=CARTESIAN_POINT('Ctrl Pts',(-9.89492464300006,11.6,5.59715539099999));
#251885=CARTESIAN_POINT('Ctrl Pts',(-9.89856190100006,15.2,5.59746561999999));
#251886=CARTESIAN_POINT('Ctrl Pts',(-9.89856190100006,11.6,5.59746561999999));
#251887=CARTESIAN_POINT('Ctrl Pts',(-9.90220395200006,15.2,5.59777343199999));
#251888=CARTESIAN_POINT('Ctrl Pts',(-9.90220395200006,11.6,5.59777343199999));
#251889=CARTESIAN_POINT('Ctrl Pts',(-9.90585079300006,15.2,5.59807881899999));
#251890=CARTESIAN_POINT('Ctrl Pts',(-9.90585079300006,11.6,5.59807881899999));
#251891=CARTESIAN_POINT('Ctrl Pts',(-9.90950241400006,15.2,5.59838177499999));
#251892=CARTESIAN_POINT('Ctrl Pts',(-9.90950241400006,11.6,5.59838177499999));
#251893=CARTESIAN_POINT('Ctrl Pts',(-9.91315881000006,15.2,5.59868229499998));
#251894=CARTESIAN_POINT('Ctrl Pts',(-9.91315881000006,11.6,5.59868229499998));
#251895=CARTESIAN_POINT('Ctrl Pts',(-9.91681997300006,15.2,5.59898036999999));
#251896=CARTESIAN_POINT('Ctrl Pts',(-9.91681997300006,11.6,5.59898036999999));
#251897=CARTESIAN_POINT('Ctrl Pts',(-9.92048589700006,15.2,5.59927599599998));
#251898=CARTESIAN_POINT('Ctrl Pts',(-9.92048589700006,11.6,5.59927599599998));
#251899=CARTESIAN_POINT('Ctrl Pts',(-9.92415657500005,15.2,5.59956916599998));
#251900=CARTESIAN_POINT('Ctrl Pts',(-9.92415657500005,11.6,5.59956916599998));
#251901=CARTESIAN_POINT('Ctrl Pts',(-9.92783199800006,15.2,5.59985987199998));
#251902=CARTESIAN_POINT('Ctrl Pts',(-9.92783199800006,11.6,5.59985987199998));
#251903=CARTESIAN_POINT('Ctrl Pts',(-9.93151216200006,15.2,5.60014810999999));
#251904=CARTESIAN_POINT('Ctrl Pts',(-9.93151216200006,11.6,5.60014810999999));
#251905=CARTESIAN_POINT('Ctrl Pts',(-9.93519706000006,15.2,5.60043387199999));
#251906=CARTESIAN_POINT('Ctrl Pts',(-9.93519706000006,11.6,5.60043387199999));
#251907=CARTESIAN_POINT('Ctrl Pts',(-9.93888668400006,15.2,5.60071715299999));
#251908=CARTESIAN_POINT('Ctrl Pts',(-9.93888668400006,11.6,5.60071715299999));
#251909=CARTESIAN_POINT('Ctrl Pts',(-9.94258102800006,15.2,5.60099794499998));
#251910=CARTESIAN_POINT('Ctrl Pts',(-9.94258102800006,11.6,5.60099794499998));
#251911=CARTESIAN_POINT('Ctrl Pts',(-9.94628008500005,15.2,5.60127624499999));
#251912=CARTESIAN_POINT('Ctrl Pts',(-9.94628008500005,11.6,5.60127624499999));
#251913=CARTESIAN_POINT('Ctrl Pts',(-9.94998384800006,15.2,5.60155204399998));
#251914=CARTESIAN_POINT('Ctrl Pts',(-9.94998384800006,11.6,5.60155204399998));
#251915=CARTESIAN_POINT('Ctrl Pts',(-9.95369231100005,15.2,5.60182533599999));
#251916=CARTESIAN_POINT('Ctrl Pts',(-9.95369231100005,11.6,5.60182533599999));
#251917=CARTESIAN_POINT('Ctrl Pts',(-9.95740546800005,15.2,5.60209611699998));
#251918=CARTESIAN_POINT('Ctrl Pts',(-9.95740546800005,11.6,5.60209611699998));
#251919=CARTESIAN_POINT('Ctrl Pts',(-9.96112331000005,15.2,5.60236437799999));
#251920=CARTESIAN_POINT('Ctrl Pts',(-9.96112331000005,11.6,5.60236437799999));
#251921=CARTESIAN_POINT('Ctrl Pts',(-9.96484583100005,15.2,5.60263011399999));
#251922=CARTESIAN_POINT('Ctrl Pts',(-9.96484583100005,11.6,5.60263011399999));
#251923=CARTESIAN_POINT('Ctrl Pts',(-9.96857302300005,15.2,5.60289331699998));
#251924=CARTESIAN_POINT('Ctrl Pts',(-9.96857302300005,11.6,5.60289331699998));
#251925=CARTESIAN_POINT('Ctrl Pts',(-9.97230488000006,15.2,5.60315398299998));
#251926=CARTESIAN_POINT('Ctrl Pts',(-9.97230488000006,11.6,5.60315398299998));
#251927=CARTESIAN_POINT('Ctrl Pts',(-9.97604139600006,15.2,5.60341210499999));
#251928=CARTESIAN_POINT('Ctrl Pts',(-9.97604139600006,11.6,5.60341210499999));
#251929=CARTESIAN_POINT('Ctrl Pts',(-9.97978256300006,15.2,5.60366767599999));
#251930=CARTESIAN_POINT('Ctrl Pts',(-9.97978256300006,11.6,5.60366767599999));
#251931=CARTESIAN_POINT('Ctrl Pts',(-9.98352837700006,15.2,5.60392069199998));
#251932=CARTESIAN_POINT('Ctrl Pts',(-9.98352837700006,11.6,5.60392069199998));
#251933=CARTESIAN_POINT('Ctrl Pts',(-9.98727883000005,15.2,5.60417114799999));
#251934=CARTESIAN_POINT('Ctrl Pts',(-9.98727883000005,11.6,5.60417114799999));
#251935=CARTESIAN_POINT('Ctrl Pts',(-9.99103391600006,15.2,5.60441903699999));
#251936=CARTESIAN_POINT('Ctrl Pts',(-9.99103391600006,11.6,5.60441903699999));
#251937=CARTESIAN_POINT('Ctrl Pts',(-9.99479363100006,15.2,5.60466435399999));
#251938=CARTESIAN_POINT('Ctrl Pts',(-9.99479363100006,11.6,5.60466435399999));
#251939=CARTESIAN_POINT('Ctrl Pts',(-9.99855796500006,15.2,5.60490709199998));
#251940=CARTESIAN_POINT('Ctrl Pts',(-9.99855796500006,11.6,5.60490709199998));
#251941=CARTESIAN_POINT('Ctrl Pts',(-10.0023269120001,15.2,5.60514724399999));
#251942=CARTESIAN_POINT('Ctrl Pts',(-10.0023269120001,11.6,5.60514724399999));
#251943=CARTESIAN_POINT('Ctrl Pts',(-10.0061004630001,15.2,5.60538480399998));
#251944=CARTESIAN_POINT('Ctrl Pts',(-10.0061004630001,11.6,5.60538480399998));
#251945=CARTESIAN_POINT('Ctrl Pts',(-10.0098786100001,15.2,5.60561976299999));
#251946=CARTESIAN_POINT('Ctrl Pts',(-10.0098786100001,11.6,5.60561976299999));
#251947=CARTESIAN_POINT('Ctrl Pts',(-10.0136613450001,15.2,5.60585211399999));
#251948=CARTESIAN_POINT('Ctrl Pts',(-10.0136613450001,11.6,5.60585211399999));
#251949=CARTESIAN_POINT('Ctrl Pts',(-10.0174486610001,15.2,5.60608185199998));
#251950=CARTESIAN_POINT('Ctrl Pts',(-10.0174486610001,11.6,5.60608185199998));
#251951=CARTESIAN_POINT('Ctrl Pts',(-10.0212405510001,15.2,5.60630896999999));
#251952=CARTESIAN_POINT('Ctrl Pts',(-10.0212405510001,11.6,5.60630896999999));
#251953=CARTESIAN_POINT('Ctrl Pts',(-10.0250370120001,15.2,5.60653346399998));
#251954=CARTESIAN_POINT('Ctrl Pts',(-10.0250370120001,11.6,5.60653346399998));
#251955=CARTESIAN_POINT('Ctrl Pts',(-10.0288380390001,15.2,5.60675533199999));
#251956=CARTESIAN_POINT('Ctrl Pts',(-10.0288380390001,11.6,5.60675533199999));
#251957=CARTESIAN_POINT('Ctrl Pts',(-10.0326436310001,15.2,5.60697457399999));
#251958=CARTESIAN_POINT('Ctrl Pts',(-10.0326436310001,11.6,5.60697457399999));
#251959=CARTESIAN_POINT('Ctrl Pts',(-10.0356917560001,15.2,5.60714786299998));
#251960=CARTESIAN_POINT('Ctrl Pts',(-10.0356917560001,11.6,5.60714786299998));
#251961=CARTESIAN_POINT('Ctrl Pts',(-10.0379799050001,15.2,5.60727664799998));
#251962=CARTESIAN_POINT('Ctrl Pts',(-10.0379799050001,11.6,5.60727664799998));
#251963=CARTESIAN_POINT('Ctrl Pts',(-10.0395062490001,15.2,5.60736197799999));
#251964=CARTESIAN_POINT('Ctrl Pts',(-10.0395062490001,11.6,5.60736197799999));
#251965=CARTESIAN_POINT('Ctrl Pts',(-10.0402696490001,15.2,5.60740451199998));
#251966=CARTESIAN_POINT('Ctrl Pts',(-10.0402696490001,11.6,5.60740451199998));
#251967=CARTESIAN_POINT('Ctrl Pts',(-8.88241603300006,15.2,5.36127880599999));
#251968=CARTESIAN_POINT('Ctrl Pts',(-8.8840193341511,15.2,5.36206719179848));
#251969=CARTESIAN_POINT('Ctrl Pts',(-8.88567631015408,15.2,5.36287598639576));
#251970=CARTESIAN_POINT('Ctrl Pts',(-8.88738636482935,15.2,5.36370417391758));
#251971=CARTESIAN_POINT('Ctrl Pts',(-8.88910466625265,15.2,5.36453635537826));
#251972=CARTESIAN_POINT('Ctrl Pts',(-8.89087656219126,15.2,5.3653881201172));
#251973=CARTESIAN_POINT('Ctrl Pts',(-8.89270147763497,15.2,5.36625847962586));
#251974=CARTESIAN_POINT('Ctrl Pts',(-8.89452639291292,15.2,5.36712883905549));
#251975=CARTESIAN_POINT('Ctrl Pts',(-8.89640432653677,15.2,5.36801779327457));
#251976=CARTESIAN_POINT('Ctrl Pts',(-8.89833471396663,15.2,5.36892438099162));
#251977=CARTESIAN_POINT('Ctrl Pts',(-8.90026510139648,15.2,5.36983096870868));
#251978=CARTESIAN_POINT('Ctrl Pts',(-8.90224794602853,15.2,5.37075519315545));
#251979=CARTESIAN_POINT('Ctrl Pts',(-8.90428269455326,15.2,5.37169612091731));
#251980=CARTESIAN_POINT('Ctrl Pts',(-8.9063174432628,15.2,5.37263704876463));
#251981=CARTESIAN_POINT('Ctrl Pts',(-8.90840409854633,15.2,5.3735946808436));
#251982=CARTESIAN_POINT('Ctrl Pts',(-8.91054211949969,15.2,5.3745681138144));
#251983=CARTESIAN_POINT('Ctrl Pts',(-8.91268014025887,15.2,5.37554154669679));
#251984=CARTESIAN_POINT('Ctrl Pts',(-8.9148695309971,15.2,5.37653078096564));
#251985=CARTESIAN_POINT('Ctrl Pts',(-8.91710976450932,15.2,5.37753493976708));
#251986=CARTESIAN_POINT('Ctrl Pts',(-8.91934999802154,15.2,5.37853909856852));
#251987=CARTESIAN_POINT('Ctrl Pts',(-8.9216410736932,15.2,5.37955817934021));
#251988=CARTESIAN_POINT('Ctrl Pts',(-8.92398248010591,15.2,5.38059133421871));
#251989=CARTESIAN_POINT('Ctrl Pts',(-8.9263238867313,15.2,5.38162448919106));
#251990=CARTESIAN_POINT('Ctrl Pts',(-8.92871562071298,15.2,5.38267171465686));
#251991=CARTESIAN_POINT('Ctrl Pts',(-8.93115718351611,15.2,5.38373218388222));
#251992=CARTESIAN_POINT('Ctrl Pts',(-8.93359874609746,15.2,5.38479265301127));
#251993=CARTESIAN_POINT('Ctrl Pts',(-8.93609013543712,15.2,5.38586636418146));
#251994=CARTESIAN_POINT('Ctrl Pts',(-8.93863085909698,15.2,5.38695251530921));
#251995=CARTESIAN_POINT('Ctrl Pts',(-8.94117158275683,15.2,5.38803866643696));
#251996=CARTESIAN_POINT('Ctrl Pts',(-8.94376164087935,15.2,5.38913725323035));
#251997=CARTESIAN_POINT('Ctrl Pts',(-8.94640055236469,15.2,5.39024749468951));
#251998=CARTESIAN_POINT('Ctrl Pts',(-8.94903946385004,15.2,5.39135773614867));
#251999=CARTESIAN_POINT('Ctrl Pts',(-8.95172722664611,15.2,5.39247963140172));
#252000=CARTESIAN_POINT('Ctrl Pts',(-8.95446336946008,15.2,5.39361241785983));
#252001=CARTESIAN_POINT('Ctrl Pts',(-8.95765553624206,15.2,5.39493400212955));
#252002=CARTESIAN_POINT('Ctrl Pts',(-8.96091355247342,15.2,5.39627040849422));
#252003=CARTESIAN_POINT('Ctrl Pts',(-8.96423668332827,15.2,5.39762046069527));
#252004=CARTESIAN_POINT('Ctrl Pts',(-8.967085081056,15.2,5.39877764823612));
#252005=CARTESIAN_POINT('Ctrl Pts',(-8.96998131859761,15.2,5.39994486170677));
#252006=CARTESIAN_POINT('Ctrl Pts',(-8.97292494140413,15.2,5.4011213804134));
#252007=CARTESIAN_POINT('Ctrl Pts',(-8.97586856447803,15.2,5.4022978992269));
#252008=CARTESIAN_POINT('Ctrl Pts',(-8.97885957476477,15.2,5.40348372275796));
#252009=CARTESIAN_POINT('Ctrl Pts',(-8.98189752393241,15.2,5.40467814957344));
#252010=CARTESIAN_POINT('Ctrl Pts',(-8.98493547282408,15.2,5.40587257628041));
#252011=CARTESIAN_POINT('Ctrl Pts',(-8.98802036337031,15.2,5.40707560607001));
#252012=CARTESIAN_POINT('Ctrl Pts',(-8.99115175533785,15.2,5.40828655294234));
#252013=CARTESIAN_POINT('Ctrl Pts',(-8.99428314730538,15.2,5.40949749981467));
#252014=CARTESIAN_POINT('Ctrl Pts',(-8.99746104273554,15.2,5.41071636728638));
#252015=CARTESIAN_POINT('Ctrl Pts',(-9.00068501061524,15.2,5.41194248232466));
#252016=CARTESIAN_POINT('Ctrl Pts',(-9.0039089787878,15.2,5.41316859747432));
#252017=CARTESIAN_POINT('Ctrl Pts',(-9.00717902037317,15.2,5.41440196469138));
#252018=CARTESIAN_POINT('Ctrl Pts',(-9.01049471063921,15.2,5.41564192884258));
#252019=CARTESIAN_POINT('Ctrl Pts',(-9.01381040060406,15.2,5.41688189288116));
#252020=CARTESIAN_POINT('Ctrl Pts',(-9.01717174178186,15.2,5.41812845637257));
#252021=CARTESIAN_POINT('Ctrl Pts',(-9.02057831675677,15.2,5.41938098149941));
#252022=CARTESIAN_POINT('Ctrl Pts',(-9.0239848917317,15.2,5.42063350662624));
#252023=CARTESIAN_POINT('Ctrl Pts',(-9.02743670019061,15.2,5.42189199456684));
#252024=CARTESIAN_POINT('Ctrl Pts',(-9.03093333414386,15.2,5.42315582460389));
#252025=CARTESIAN_POINT('Ctrl Pts',(-9.03501274063439,15.2,5.42463029305699));
#252026=CARTESIAN_POINT('Ctrl Pts',(-9.03915315896396,15.2,5.4261120307306));
#252027=CARTESIAN_POINT('Ctrl Pts',(-9.04335394800668,15.2,5.4276000780244));
#252028=CARTESIAN_POINT('Ctrl Pts',(-9.04695462414212,15.2,5.42887554706717));
#252029=CARTESIAN_POINT('Ctrl Pts',(-9.05059965708492,15.2,5.4301556494736));
#252030=CARTESIAN_POINT('Ctrl Pts',(-9.05428864911456,15.2,5.43143979959334));
#252031=CARTESIAN_POINT('Ctrl Pts',(-9.05797764147928,15.2,5.43272394982973));
#252032=CARTESIAN_POINT('Ctrl Pts',(-9.06171059490176,15.2,5.43401214355649));
#252033=CARTESIAN_POINT('Ctrl Pts',(-9.06548711663208,15.2,5.43530380785827));
#252034=CARTESIAN_POINT('Ctrl Pts',(-9.06863421790251,15.2,5.43638019471775));
#252035=CARTESIAN_POINT('Ctrl Pts',(-9.07181157594484,15.2,5.43745898891341));
#252036=CARTESIAN_POINT('Ctrl Pts',(-9.07501896941952,15.2,5.43853986669136));
#252037=CARTESIAN_POINT('Ctrl Pts',(-9.07822636289421,15.2,5.43962074446931));
#252038=CARTESIAN_POINT('Ctrl Pts',(-9.08146379045268,15.2,5.44070370348617));
#252039=CARTESIAN_POINT('Ctrl Pts',(-9.08473103163568,15.2,5.44178842466686));
#252040=CARTESIAN_POINT('Ctrl Pts',(-9.08799827246255,15.2,5.44287314572932));
#252041=CARTESIAN_POINT('Ctrl Pts',(-9.09129532991322,15.2,5.44395962790417));
#252042=CARTESIAN_POINT('Ctrl Pts',(-9.09462198308987,15.2,5.44504755584101));
#252043=CARTESIAN_POINT('Ctrl Pts',(-9.09794863662913,15.2,5.44613548389646));
#252044=CARTESIAN_POINT('Ctrl Pts',(-9.1013048866151,15.2,5.44722485939632));
#252045=CARTESIAN_POINT('Ctrl Pts',(-9.10469051855715,15.2,5.44831537154901));
#252046=CARTESIAN_POINT('Ctrl Pts',(-9.10807615049921,15.2,5.44940588370169));
#252047=CARTESIAN_POINT('Ctrl Pts',(-9.11149116577466,15.2,5.45049753384086));
#252048=CARTESIAN_POINT('Ctrl Pts',(-9.11493534962527,15.2,5.4515900168815));
#252049=CARTESIAN_POINT('Ctrl Pts',(-9.11837953347588,15.2,5.45268249992214));
#252050=CARTESIAN_POINT('Ctrl Pts',(-9.12185288680039,15.2,5.45377581741736));
#252051=CARTESIAN_POINT('Ctrl Pts',(-9.12535520027111,15.2,5.45486966894511));
#252052=CARTESIAN_POINT('Ctrl Pts',(-9.13025843920647,15.2,5.45640106110782));
#252053=CARTESIAN_POINT('Ctrl Pts',(-9.1352184345454,15.2,5.45793350401421));
#252054=CARTESIAN_POINT('Ctrl Pts',(-9.14023462424361,15.2,5.45946619351725));
#252055=CARTESIAN_POINT('Ctrl Pts',(-9.14381761682939,15.2,5.46056097171666));
#252056=CARTESIAN_POINT('Ctrl Pts',(-9.14742927608118,15.2,5.46165587709381));
#252057=CARTESIAN_POINT('Ctrl Pts',(-9.15106940122156,15.2,5.46275062278825));
#252058=CARTESIAN_POINT('Ctrl Pts',(-9.15470952636195,15.2,5.46384536848269));
#252059=CARTESIAN_POINT('Ctrl Pts',(-9.15837811395712,15.2,5.46493995644377));
#252060=CARTESIAN_POINT('Ctrl Pts',(-9.16207496354193,15.2,5.46603410380488));
#252061=CARTESIAN_POINT('Ctrl Pts',(-9.16577181312675,15.2,5.46712825116596));
#252062=CARTESIAN_POINT('Ctrl Pts',(-9.16949692343519,15.2,5.46822195863343));
#252063=CARTESIAN_POINT('Ctrl Pts',(-9.17325009473577,15.2,5.4693149509102));
#252064=CARTESIAN_POINT('Ctrl Pts',(-9.17700326603634,15.2,5.47040794318698));
#252065=CARTESIAN_POINT('Ctrl Pts',(-9.18078449731264,15.2,5.47150021794281));
#252066=CARTESIAN_POINT('Ctrl Pts',(-9.18459359023155,15.2,5.47259150690106));
#252067=CARTESIAN_POINT('Ctrl Pts',(-9.18840268315046,15.2,5.47368279585931));
#252068=CARTESIAN_POINT('Ctrl Pts',(-9.19223963767545,15.2,5.47477309839254));
#252069=CARTESIAN_POINT('Ctrl Pts',(-9.19610425649715,15.2,5.47586214589244));
#252070=CARTESIAN_POINT('Ctrl Pts',(-9.19996887531887,15.2,5.47695119339233));
#252071=CARTESIAN_POINT('Ctrl Pts',(-9.20386115931602,15.2,5.47803898688665));
#252072=CARTESIAN_POINT('Ctrl Pts',(-9.2077809137627,15.2,5.47912526515041));
#252073=CARTESIAN_POINT('Ctrl Pts',(-9.21170066778212,15.2,5.48021154329576));
#252074=CARTESIAN_POINT('Ctrl Pts',(-9.21564789101556,15.2,5.48129630575956));
#252075=CARTESIAN_POINT('Ctrl Pts',(-9.2196223909968,15.2,5.48237929314167));
#252076=CARTESIAN_POINT('Ctrl Pts',(-9.22359689141125,15.2,5.48346228064183));
#252077=CARTESIAN_POINT('Ctrl Pts',(-9.22759866970303,15.2,5.48454349429199));
#252078=CARTESIAN_POINT('Ctrl Pts',(-9.23162753192301,15.2,5.4856226801255));
#252079=CARTESIAN_POINT('Ctrl Pts',(-9.23485062187466,15.2,5.48648602883934));
#252080=CARTESIAN_POINT('Ctrl Pts',(-9.23809104747093,15.2,5.48734807932755));
#252081=CARTESIAN_POINT('Ctrl Pts',(-9.24134871055221,15.2,5.48820870526724));
#252082=CARTESIAN_POINT('Ctrl Pts',(-9.24460637318962,15.2,5.48906933108967));
#252083=CARTESIAN_POINT('Ctrl Pts',(-9.2478812721132,15.2,5.48992853026584));
#252084=CARTESIAN_POINT('Ctrl Pts',(-9.25117331345341,15.2,5.49078617758477));
#252085=CARTESIAN_POINT('Ctrl Pts',(-9.25528836546509,15.2,5.49185823682106));
#252086=CARTESIAN_POINT('Ctrl Pts',(-9.2594301986347,15.2,5.49292787173243));
#252087=CARTESIAN_POINT('Ctrl Pts',(-9.26359862897977,15.2,5.49399483763543));
#252088=CARTESIAN_POINT('Ctrl Pts',(-9.26693337343756,15.2,5.49484841040436));
#252089=CARTESIAN_POINT('Ctrl Pts',(-9.27028513977554,15.2,5.49570027665594));
#252090=CARTESIAN_POINT('Ctrl Pts',(-9.2736538317523,15.2,5.49655031148391));
#252091=CARTESIAN_POINT('Ctrl Pts',(-9.27786469649376,15.2,5.49761285496097));
#252092=CARTESIAN_POINT('Ctrl Pts',(-9.28210201062762,15.2,5.49867253875812));
#252093=CARTESIAN_POINT('Ctrl Pts',(-9.28636558625399,15.2,5.49972912632741));
#252094=CARTESIAN_POINT('Ctrl Pts',(-9.28977644647625,15.2,5.50057439631374));
#252095=CARTESIAN_POINT('Ctrl Pts',(-9.29320411645626,15.2,5.50141768526991));
#252096=CARTESIAN_POINT('Ctrl Pts',(-9.2966485012285,15.2,5.50225887264579));
#252097=CARTESIAN_POINT('Ctrl Pts',(-9.30009288647004,15.2,5.50310006013629));
#252098=CARTESIAN_POINT('Ctrl Pts',(-9.30355398711643,15.2,5.50393914794005));
#252099=CARTESIAN_POINT('Ctrl Pts',(-9.3070317097107,15.2,5.50477601676723));
#252100=CARTESIAN_POINT('Ctrl Pts',(-9.31137886271662,15.2,5.5058221027442));
#252101=CARTESIAN_POINT('Ctrl Pts',(-9.31575198956426,15.2,5.50686472074589));
#252102=CARTESIAN_POINT('Ctrl Pts',(-9.32015090678784,15.2,5.50790364755125));
#252103=CARTESIAN_POINT('Ctrl Pts',(-9.32367004027901,15.2,5.5087347889276));
#252104=CARTESIAN_POINT('Ctrl Pts',(-9.32720568088073,15.2,5.50956356600996));
#252105=CARTESIAN_POINT('Ctrl Pts',(-9.33075773764424,15.2,5.51038986483156));
#252106=CARTESIAN_POINT('Ctrl Pts',(-9.33608582351545,15.2,5.51162931323283));
#252107=CARTESIAN_POINT('Ctrl Pts',(-9.34145084384792,15.2,5.51286318764083));
#252108=CARTESIAN_POINT('Ctrl Pts',(-9.34685249299762,15.2,5.5140911041021));
#252109=CARTESIAN_POINT('Ctrl Pts',(-9.35045359194011,15.2,5.51490971496473));
#252110=CARTESIAN_POINT('Ctrl Pts',(-9.35407097008452,15.2,5.51572568043034));
#252111=CARTESIAN_POINT('Ctrl Pts',(-9.3577045374531,15.2,5.51653888664182));
#252112=CARTESIAN_POINT('Ctrl Pts',(-9.36224649703511,15.2,5.51755539448927));
#252113=CARTESIAN_POINT('Ctrl Pts',(-9.36681375162889,15.2,5.51856759314494));
#252114=CARTESIAN_POINT('Ctrl Pts',(-9.37140612718314,15.2,5.51957526765906));
#252115=CARTESIAN_POINT('Ctrl Pts',(-9.37599850273737,15.2,5.5205829421732));
#252116=CARTESIAN_POINT('Ctrl Pts',(-9.38061600008199,15.2,5.52158609492269));
#252117=CARTESIAN_POINT('Ctrl Pts',(-9.38525844475581,15.2,5.52258451277446));
#252118=CARTESIAN_POINT('Ctrl Pts',(-9.39082937816199,15.2,5.52378261415306));
#252119=CARTESIAN_POINT('Ctrl Pts',(-9.39643623350076,15.2,5.52497389872179));
#252120=CARTESIAN_POINT('Ctrl Pts',(-9.40207871787664,15.2,5.52615800809593));
#252121=CARTESIAN_POINT('Ctrl Pts',(-9.40584037446891,15.2,5.52694741441706));
#252122=CARTESIAN_POINT('Ctrl Pts',(-9.40961786491746,15.2,5.52773363270154));
#252123=CARTESIAN_POINT('Ctrl Pts',(-9.41341110225258,15.2,5.5285165576922));
#252124=CARTESIAN_POINT('Ctrl Pts',(-9.41720433907087,15.2,5.52929948257618));
#252125=CARTESIAN_POINT('Ctrl Pts',(-9.42101332216117,15.2,5.53007911368064));
#252126=CARTESIAN_POINT('Ctrl Pts',(-9.42483796562467,15.2,5.53085534917308));
#252127=CARTESIAN_POINT('Ctrl Pts',(-9.42866260960928,15.2,5.5316315847713));
#252128=CARTESIAN_POINT('Ctrl Pts',(-9.43250291429818,15.2,5.53240442385252));
#252129=CARTESIAN_POINT('Ctrl Pts',(-9.43635879100832,15.2,5.53317376478333));
#252130=CARTESIAN_POINT('Ctrl Pts',(-9.44021466771848,15.2,5.53394310571416));
#252131=CARTESIAN_POINT('Ctrl Pts',(-9.44408611958045,15.2,5.534708947764));
#252132=CARTESIAN_POINT('Ctrl Pts',(-9.44797305762719,15.2,5.53547119141629));
#252133=CARTESIAN_POINT('Ctrl Pts',(-9.45185999514433,15.2,5.53623343496472));
#252134=CARTESIAN_POINT('Ctrl Pts',(-9.45576242035266,15.2,5.53699207853553));
#252135=CARTESIAN_POINT('Ctrl Pts',(-9.45968024777233,15.2,5.53774702403282));
#252136=CARTESIAN_POINT('Ctrl Pts',(-9.46359807572581,15.2,5.53850196963296));
#252137=CARTESIAN_POINT('Ctrl Pts',(-9.46753130613716,15.2,5.53925321680131));
#252138=CARTESIAN_POINT('Ctrl Pts',(-9.47147985285392,15.2,5.54000066589721));
#252139=CARTESIAN_POINT('Ctrl Pts',(-9.4754283990327,15.2,5.54074811489126));
#252140=CARTESIAN_POINT('Ctrl Pts',(-9.47939226200669,15.2,5.54149176726915));
#252141=CARTESIAN_POINT('Ctrl Pts',(-9.48337135812485,15.2,5.54223152493116));
#252142=CARTESIAN_POINT('Ctrl Pts',(-9.48735045478516,15.2,5.54297128269394));
#252143=CARTESIAN_POINT('Ctrl Pts',(-9.49134478324729,15.2,5.54370714589795));
#252144=CARTESIAN_POINT('Ctrl Pts',(-9.49535426057792,15.2,5.54443901882646));
#252145=CARTESIAN_POINT('Ctrl Pts',(-9.49936373736225,15.2,5.54517089165525));
#252146=CARTESIAN_POINT('Ctrl Pts',(-9.5033883624131,15.2,5.54589877369539));
#252147=CARTESIAN_POINT('Ctrl Pts',(-9.50742805267223,15.2,5.54662256889495));
#252148=CARTESIAN_POINT('Ctrl Pts',(-9.51146774348178,15.2,5.54734636419314));
#252149=CARTESIAN_POINT('Ctrl Pts',(-9.51552249876285,15.2,5.54806607493641));
#252150=CARTESIAN_POINT('Ctrl Pts',(-9.51959223604117,15.2,5.54878160530846));
#252151=CARTESIAN_POINT('Ctrl Pts',(-9.52467940736183,15.2,5.54967601822477));
#252152=CARTESIAN_POINT('Ctrl Pts',(-9.52978998560691,15.2,5.55056390072461));
#252153=CARTESIAN_POINT('Ctrl Pts',(-9.53492381276089,15.2,5.55144507030759));
#252154=CARTESIAN_POINT('Ctrl Pts',(-9.53903087414833,15.2,5.55215000591636));
#252155=CARTESIAN_POINT('Ctrl Pts',(-9.54315281303538,15.2,5.55285064471792));
#252156=CARTESIAN_POINT('Ctrl Pts',(-9.54728954862481,15.2,5.55354689764061));
#252157=CARTESIAN_POINT('Ctrl Pts',(-9.55142628477788,15.2,5.55424315065817));
#252158=CARTESIAN_POINT('Ctrl Pts',(-9.55557781577106,15.2,5.55493501498843));
#252159=CARTESIAN_POINT('Ctrl Pts',(-9.5597440618324,15.2,5.55562240208115));
#252160=CARTESIAN_POINT('Ctrl Pts',(-9.5639103073261,15.2,5.55630978908022));
#252161=CARTESIAN_POINT('Ctrl Pts',(-9.56809126674741,15.2,5.55699269764686));
#252162=CARTESIAN_POINT('Ctrl Pts',(-9.57228685884736,15.2,5.55767103864743));
#252163=CARTESIAN_POINT('Ctrl Pts',(-9.57648245151896,15.2,5.55834937974042));
#252164=CARTESIAN_POINT('Ctrl Pts',(-9.5806926758923,15.2,5.55902315322764));
#252165=CARTESIAN_POINT('Ctrl Pts',(-9.58491745325288,15.2,5.55969227093379));
#252166=CARTESIAN_POINT('Ctrl Pts',(-9.58914223003784,15.2,5.56036138854878));
#252167=CARTESIAN_POINT('Ctrl Pts',(-9.59338155894819,15.2,5.56102585002058));
#252168=CARTESIAN_POINT('Ctrl Pts',(-9.59763535782118,15.2,5.5616855671338));
#252169=CARTESIAN_POINT('Ctrl Pts',(-9.60188915727375,15.2,5.56234528433691));
#252170=CARTESIAN_POINT('Ctrl Pts',(-9.60615742795827,15.2,5.56300025864234));
#252171=CARTESIAN_POINT('Ctrl Pts',(-9.610440090025,15.2,5.56365040123334));
#252172=CARTESIAN_POINT('Ctrl Pts',(-9.61579341731665,15.2,5.56446307942779));
#252173=CARTESIAN_POINT('Ctrl Pts',(-9.6211692296617,15.2,5.56526821231906));
#252174=CARTESIAN_POINT('Ctrl Pts',(-9.62656737197794,15.2,5.5660656280171));
#252175=CARTESIAN_POINT('Ctrl Pts',(-9.63088588547791,15.2,5.56670356052339));
#252176=CARTESIAN_POINT('Ctrl Pts',(-9.63521868980163,15.2,5.56733655680093));
#252177=CARTESIAN_POINT('Ctrl Pts',(-9.63956570655594,15.2,5.567964531139));
#252178=CARTESIAN_POINT('Ctrl Pts',(-9.64499947794302,15.2,5.56874949912575));
#252179=CARTESIAN_POINT('Ctrl Pts',(-9.65045545383529,15.2,5.56952662064318));
#252180=CARTESIAN_POINT('Ctrl Pts',(-9.65593348195848,15.2,5.57029573140773));
#252181=CARTESIAN_POINT('Ctrl Pts',(-9.66141151008166,15.2,5.57106484217227));
#252182=CARTESIAN_POINT('Ctrl Pts',(-9.66691159019583,15.2,5.57182594516328));
#252183=CARTESIAN_POINT('Ctrl Pts',(-9.67243356790073,15.2,5.57257887589591));
#252184=CARTESIAN_POINT('Ctrl Pts',(-9.67574675440329,15.2,5.57303063431907));
#252185=CARTESIAN_POINT('Ctrl Pts',(-9.67906782442966,15.2,5.5734794528186));
#252186=CARTESIAN_POINT('Ctrl Pts',(-9.68239674476597,15.2,5.57392529467781));
#252187=CARTESIAN_POINT('Ctrl Pts',(-9.68572566570703,15.2,5.57437113661801));
#252188=CARTESIAN_POINT('Ctrl Pts',(-9.68906243780864,15.2,5.57481400246571));
#252189=CARTESIAN_POINT('Ctrl Pts',(-9.69240702671247,15.2,5.57525385936256));
#252190=CARTESIAN_POINT('Ctrl Pts',(-9.69798134074204,15.2,5.5759869540841));
#252191=CARTESIAN_POINT('Ctrl Pts',(-9.70357736993304,15.2,5.57671168781106));
#252192=CARTESIAN_POINT('Ctrl Pts',(-9.70919496305979,15.2,5.57742790510202));
#252193=CARTESIAN_POINT('Ctrl Pts',(-9.71256551881337,15.2,5.57785763546099));
#252194=CARTESIAN_POINT('Ctrl Pts',(-9.71594383767483,15.2,5.57828430039318));
#252195=CARTESIAN_POINT('Ctrl Pts',(-9.71932988713853,15.2,5.57870786535692));
#252196=CARTESIAN_POINT('Ctrl Pts',(-9.72384461955176,15.2,5.57927261861627));
#252197=CARTESIAN_POINT('Ctrl Pts',(-9.72837309423991,15.2,5.57983186257181));
#252198=CARTESIAN_POINT('Ctrl Pts',(-9.73291523564548,15.2,5.58038551897136));
#252199=CARTESIAN_POINT('Ctrl Pts',(-9.73632184185437,15.2,5.58080076128988));
#252200=CARTESIAN_POINT('Ctrl Pts',(-9.73973613509606,15.2,5.58121285979195));
#252201=CARTESIAN_POINT('Ctrl Pts',(-9.74315808334569,15.2,5.58162178265253));
#252202=CARTESIAN_POINT('Ctrl Pts',(-9.74658003221697,15.2,5.58203070558739));
#252203=CARTESIAN_POINT('Ctrl Pts',(-9.75000963559875,15.2,5.58243645244636));
#252204=CARTESIAN_POINT('Ctrl Pts',(-9.75344686201599,15.2,5.58283899133776));
#252205=CARTESIAN_POINT('Ctrl Pts',(-9.7580298295316,15.2,5.58337570973774));
#252206=CARTESIAN_POINT('Ctrl Pts',(-9.76262634811119,15.2,5.58390672355407));
#252207=CARTESIAN_POINT('Ctrl Pts',(-9.7672363422552,15.2,5.58443195745798));
#252208=CARTESIAN_POINT('Ctrl Pts',(-9.7729988354063,15.2,5.58508849989153));
#252209=CARTESIAN_POINT('Ctrl Pts',(-9.77878238241668,15.2,5.58573601107224));
#252210=CARTESIAN_POINT('Ctrl Pts',(-9.78458683804167,15.2,5.58637434426668));
#252211=CARTESIAN_POINT('Ctrl Pts',(-9.78806951129013,15.2,5.58675734416943));
#252212=CARTESIAN_POINT('Ctrl Pts',(-9.79155971034661,15.2,5.58713703992232));
#252213=CARTESIAN_POINT('Ctrl Pts',(-9.79505740463555,15.2,5.58751339940893));
#252214=CARTESIAN_POINT('Ctrl Pts',(-9.79855509892447,15.2,5.58788975889555));
#252215=CARTESIAN_POINT('Ctrl Pts',(-9.80206028787347,15.2,5.5882627834897));
#252216=CARTESIAN_POINT('Ctrl Pts',(-9.80557294029547,15.2,5.58863244091179));
#252217=CARTESIAN_POINT('Ctrl Pts',(-9.81142736121148,15.2,5.58924853663765));
#252218=CARTESIAN_POINT('Ctrl Pts',(-9.81730251137116,15.2,5.58985528088261));
#252219=CARTESIAN_POINT('Ctrl Pts',(-9.82319824706455,15.2,5.59045252845256));
#252220=CARTESIAN_POINT('Ctrl Pts',(-9.82673568835205,15.2,5.5908108769815));
#252221=CARTESIAN_POINT('Ctrl Pts',(-9.83028054023903,15.2,5.59116580881902));
#252222=CARTESIAN_POINT('Ctrl Pts',(-9.83383277098396,15.2,5.59151729039005));
#252223=CARTESIAN_POINT('Ctrl Pts',(-9.83738500237421,15.2,5.59186877202494));
#252224=CARTESIAN_POINT('Ctrl Pts',(-9.84094461235821,15.2,5.59221680625885));
#252225=CARTESIAN_POINT('Ctrl Pts',(-9.84451157029427,15.2,5.59256136030845));
#252226=CARTESIAN_POINT('Ctrl Pts',(-9.84807852758235,15.2,5.59290591429546));
#252227=CARTESIAN_POINT('Ctrl Pts',(-9.8516528322367,15.2,5.59324698964932));
#252228=CARTESIAN_POINT('Ctrl Pts',(-9.85523445310719,15.2,5.59358455605341));
#252229=CARTESIAN_POINT('Ctrl Pts',(-9.85881607397769,15.2,5.59392212245751));
#252230=CARTESIAN_POINT('Ctrl Pts',(-9.86240501283424,15.2,5.5942561790275));
#252231=CARTESIAN_POINT('Ctrl Pts',(-9.86600123480328,15.2,5.59458669747531));
#252232=CARTESIAN_POINT('Ctrl Pts',(-9.8707961972109,15.2,5.59502738871904));
#252233=CARTESIAN_POINT('Ctrl Pts',(-9.87560411176278,15.2,5.59546178820603));
#252234=CARTESIAN_POINT('Ctrl Pts',(-9.88042490447848,15.2,5.59588982667169));
#252235=CARTESIAN_POINT('Ctrl Pts',(-9.88404049983629,15.2,5.59621085559384));
#252236=CARTESIAN_POINT('Ctrl Pts',(-9.88766333854615,15.2,5.59652830585663));
#252237=CARTESIAN_POINT('Ctrl Pts',(-9.89129339003303,15.2,5.59684214881843));
#252238=CARTESIAN_POINT('Ctrl Pts',(-9.89492344086046,15.2,5.5971559917232));
#252239=CARTESIAN_POINT('Ctrl Pts',(-9.8985607045125,15.2,5.59746622689483));
#252240=CARTESIAN_POINT('Ctrl Pts',(-9.90220514983904,15.2,5.59777282580004));
#252241=CARTESIAN_POINT('Ctrl Pts',(-9.90584959516559,15.2,5.59807942470525));
#252242=CARTESIAN_POINT('Ctrl Pts',(-9.90950122296962,15.2,5.59838238684315));
#252243=CARTESIAN_POINT('Ctrl Pts',(-9.91316000177,15.2,5.59868168379195));
#252244=CARTESIAN_POINT('Ctrl Pts',(-9.91681878057039,15.2,5.59898098074075));
#252245=CARTESIAN_POINT('Ctrl Pts',(-9.92048471144682,15.2,5.59927661254234));
#252246=CARTESIAN_POINT('Ctrl Pts',(-9.92415776128833,15.2,5.59956855003307));
#252247=CARTESIAN_POINT('Ctrl Pts',(-9.92905516152187,15.2,5.59995780005608));
#252248=CARTESIAN_POINT('Ctrl Pts',(-9.93396521991586,15.2,5.60034048277779));
#252249=CARTESIAN_POINT('Ctrl Pts',(-9.93888786479654,15.2,5.60071653085316));
#252250=CARTESIAN_POINT('Ctrl Pts',(-9.94257984812169,15.2,5.60099856688407));
#252251=CARTESIAN_POINT('Ctrl Pts',(-9.94627891103813,15.2,5.60127687222351));
#252252=CARTESIAN_POINT('Ctrl Pts',(-9.9499850234041,15.2,5.60155141729654));
#252253=CARTESIAN_POINT('Ctrl Pts',(-9.95369113577006,15.2,5.60182596236957));
#252254=CARTESIAN_POINT('Ctrl Pts',(-9.95740429893828,15.2,5.60209674877543));
#252255=CARTESIAN_POINT('Ctrl Pts',(-9.96112447973672,15.2,5.60236374672525));
#252256=CARTESIAN_POINT('Ctrl Pts',(-9.96484466053517,15.2,5.60263074467508));
#252257=CARTESIAN_POINT('Ctrl Pts',(-9.96857185893203,15.2,5.60289395359133));
#252258=CARTESIAN_POINT('Ctrl Pts',(-9.97230604472995,15.2,5.60315334699977));
#252259=CARTESIAN_POINT('Ctrl Pts',(-9.97728495957944,15.2,5.60349920490911));
#252260=CARTESIAN_POINT('Ctrl Pts',(-9.98227629669971,15.2,5.60383827697025));
#252261=CARTESIAN_POINT('Ctrl Pts',(-9.98727998908478,15.2,5.604170506321));
#252262=CARTESIAN_POINT('Ctrl Pts',(-9.99103275803271,15.2,5.60441967831142));
#252263=CARTESIAN_POINT('Ctrl Pts',(-9.99479247889694,15.2,5.60466500108538));
#252264=CARTESIAN_POINT('Ctrl Pts',(-9.99855911863569,15.2,5.6049064455346));
#252265=CARTESIAN_POINT('Ctrl Pts',(-10.0023257583744,15.2,5.60514788998382));
#252266=CARTESIAN_POINT('Ctrl Pts',(-10.0060993167569,15.2,5.60538545652434));
#252267=CARTESIAN_POINT('Ctrl Pts',(-10.0098797570118,15.2,5.60561911101689));
#252268=CARTESIAN_POINT('Ctrl Pts',(-10.0161804909988,15.2,5.6060085351853));
#252269=CARTESIAN_POINT('Ctrl Pts',(-10.0225003316333,15.2,5.60638708414889));
#252270=CARTESIAN_POINT('Ctrl Pts',(-10.028839180665,15.2,5.6067546754843));
#252271=CARTESIAN_POINT('Ctrl Pts',(-10.0326424899459,15.2,5.60697523027754));
#252272=CARTESIAN_POINT('Ctrl Pts',(-10.0364526481964,15.2,5.60719184195524));
#252273=CARTESIAN_POINT('Ctrl Pts',(-10.0402696490001,15.2,5.60740451199998));
#252274=CARTESIAN_POINT('Ctrl Pts',(-8.88241603300006,12.2,5.36127880599999));
#252275=CARTESIAN_POINT('Ctrl Pts',(-8.8840193341511,12.2,5.36206719179848));
#252276=CARTESIAN_POINT('Ctrl Pts',(-8.88567631015408,12.2,5.36287598639576));
#252277=CARTESIAN_POINT('Ctrl Pts',(-8.88738636482935,12.2,5.36370417391758));
#252278=CARTESIAN_POINT('Ctrl Pts',(-8.88910466625265,12.2,5.36453635537826));
#252279=CARTESIAN_POINT('Ctrl Pts',(-8.89087656219126,12.2,5.3653881201172));
#252280=CARTESIAN_POINT('Ctrl Pts',(-8.89270147763497,12.2,5.36625847962586));
#252281=CARTESIAN_POINT('Ctrl Pts',(-8.89452639291292,12.2,5.36712883905548));
#252282=CARTESIAN_POINT('Ctrl Pts',(-8.89640432653677,12.2,5.36801779327457));
#252283=CARTESIAN_POINT('Ctrl Pts',(-8.89833471396663,12.2,5.36892438099162));
#252284=CARTESIAN_POINT('Ctrl Pts',(-8.90026510139648,12.2,5.36983096870868));
#252285=CARTESIAN_POINT('Ctrl Pts',(-8.90224794602853,12.2,5.37075519315545));
#252286=CARTESIAN_POINT('Ctrl Pts',(-8.90428269455326,12.2,5.37169612091731));
#252287=CARTESIAN_POINT('Ctrl Pts',(-8.9063174432628,12.2,5.37263704876463));
#252288=CARTESIAN_POINT('Ctrl Pts',(-8.90840409854632,12.2,5.3735946808436));
#252289=CARTESIAN_POINT('Ctrl Pts',(-8.91054211949969,12.2,5.3745681138144));
#252290=CARTESIAN_POINT('Ctrl Pts',(-8.91268014025887,12.2,5.37554154669679));
#252291=CARTESIAN_POINT('Ctrl Pts',(-8.9148695309971,12.2,5.37653078096564));
#252292=CARTESIAN_POINT('Ctrl Pts',(-8.91710976450932,12.2,5.37753493976708));
#252293=CARTESIAN_POINT('Ctrl Pts',(-8.91934999802154,12.2,5.37853909856852));
#252294=CARTESIAN_POINT('Ctrl Pts',(-8.9216410736932,12.2,5.37955817934021));
#252295=CARTESIAN_POINT('Ctrl Pts',(-8.92398248010591,12.2,5.38059133421871));
#252296=CARTESIAN_POINT('Ctrl Pts',(-8.9263238867313,12.2,5.38162448919106));
#252297=CARTESIAN_POINT('Ctrl Pts',(-8.92871562071298,12.2,5.38267171465686));
#252298=CARTESIAN_POINT('Ctrl Pts',(-8.93115718351611,12.2,5.38373218388222));
#252299=CARTESIAN_POINT('Ctrl Pts',(-8.93359874609746,12.2,5.38479265301126));
#252300=CARTESIAN_POINT('Ctrl Pts',(-8.93609013543712,12.2,5.38586636418146));
#252301=CARTESIAN_POINT('Ctrl Pts',(-8.93863085909698,12.2,5.38695251530921));
#252302=CARTESIAN_POINT('Ctrl Pts',(-8.94117158275683,12.2,5.38803866643696));
#252303=CARTESIAN_POINT('Ctrl Pts',(-8.94376164087935,12.2,5.38913725323035));
#252304=CARTESIAN_POINT('Ctrl Pts',(-8.94640055236469,12.2,5.39024749468951));
#252305=CARTESIAN_POINT('Ctrl Pts',(-8.94903946385004,12.2,5.39135773614867));
#252306=CARTESIAN_POINT('Ctrl Pts',(-8.95172722664611,12.2,5.39247963140172));
#252307=CARTESIAN_POINT('Ctrl Pts',(-8.95446336946008,12.2,5.39361241785983));
#252308=CARTESIAN_POINT('Ctrl Pts',(-8.95765553624206,12.2,5.39493400212955));
#252309=CARTESIAN_POINT('Ctrl Pts',(-8.96091355247342,12.2,5.39627040849422));
#252310=CARTESIAN_POINT('Ctrl Pts',(-8.96423668332826,12.2,5.39762046069527));
#252311=CARTESIAN_POINT('Ctrl Pts',(-8.967085081056,12.2,5.39877764823612));
#252312=CARTESIAN_POINT('Ctrl Pts',(-8.96998131859761,12.2,5.39994486170677));
#252313=CARTESIAN_POINT('Ctrl Pts',(-8.97292494140413,12.2,5.4011213804134));
#252314=CARTESIAN_POINT('Ctrl Pts',(-8.97586856447803,12.2,5.4022978992269));
#252315=CARTESIAN_POINT('Ctrl Pts',(-8.97885957476478,12.2,5.40348372275796));
#252316=CARTESIAN_POINT('Ctrl Pts',(-8.98189752393241,12.2,5.40467814957344));
#252317=CARTESIAN_POINT('Ctrl Pts',(-8.98493547282408,12.2,5.40587257628041));
#252318=CARTESIAN_POINT('Ctrl Pts',(-8.9880203633703,12.2,5.40707560607));
#252319=CARTESIAN_POINT('Ctrl Pts',(-8.99115175533783,12.2,5.40828655294233));
#252320=CARTESIAN_POINT('Ctrl Pts',(-8.99428314730537,12.2,5.40949749981466));
#252321=CARTESIAN_POINT('Ctrl Pts',(-8.99746104273554,12.2,5.41071636728638));
#252322=CARTESIAN_POINT('Ctrl Pts',(-9.00068501061524,12.2,5.41194248232466));
#252323=CARTESIAN_POINT('Ctrl Pts',(-9.0039089787878,12.2,5.41316859747432));
#252324=CARTESIAN_POINT('Ctrl Pts',(-9.00717902037317,12.2,5.41440196469138));
#252325=CARTESIAN_POINT('Ctrl Pts',(-9.01049471063921,12.2,5.41564192884258));
#252326=CARTESIAN_POINT('Ctrl Pts',(-9.01381040060406,12.2,5.41688189288116));
#252327=CARTESIAN_POINT('Ctrl Pts',(-9.01717174178186,12.2,5.41812845637257));
#252328=CARTESIAN_POINT('Ctrl Pts',(-9.02057831675677,12.2,5.41938098149941));
#252329=CARTESIAN_POINT('Ctrl Pts',(-9.0239848917317,12.2,5.42063350662624));
#252330=CARTESIAN_POINT('Ctrl Pts',(-9.02743670019061,12.2,5.42189199456683));
#252331=CARTESIAN_POINT('Ctrl Pts',(-9.03093333414385,12.2,5.42315582460389));
#252332=CARTESIAN_POINT('Ctrl Pts',(-9.03442996841472,12.2,5.42441965475574));
#252333=CARTESIAN_POINT('Ctrl Pts',(-9.03797142664485,12.2,5.42568882635657));
#252334=CARTESIAN_POINT('Ctrl Pts',(-9.04155730810531,12.2,5.42696273282322));
#252335=CARTESIAN_POINT('Ctrl Pts',(-9.04514318924006,12.2,5.42823663917418));
#252336=CARTESIAN_POINT('Ctrl Pts',(-9.0487734905418,12.2,5.42951528046325));
#252337=CARTESIAN_POINT('Ctrl Pts',(-9.05244781849163,12.2,5.43079806474998));
#252338=CARTESIAN_POINT('Ctrl Pts',(-9.05612214644144,12.2,5.43208084903669));
#252339=CARTESIAN_POINT('Ctrl Pts',(-9.05984049951241,12.2,5.43336777709109));
#252340=CARTESIAN_POINT('Ctrl Pts',(-9.0636024876445,12.2,5.43465826760849));
#252341=CARTESIAN_POINT('Ctrl Pts',(-9.06673747786849,12.2,5.43573367641205));
#252342=CARTESIAN_POINT('Ctrl Pts',(-9.06990276764833,12.2,5.4368115602628));
#252343=CARTESIAN_POINT('Ctrl Pts',(-9.07309813854951,12.2,5.43789159213769));
#252344=CARTESIAN_POINT('Ctrl Pts',(-9.0762935094507,12.2,5.43897162401257));
#252345=CARTESIAN_POINT('Ctrl Pts',(-9.0795189588944,12.2,5.44005380197364));
#252346=CARTESIAN_POINT('Ctrl Pts',(-9.08277426583726,12.2,5.4411378056541));
#252347=CARTESIAN_POINT('Ctrl Pts',(-9.08602957278013,12.2,5.44222180933455));
#252348=CARTESIAN_POINT('Ctrl Pts',(-9.08931473773876,12.2,5.44330763819446));
#252349=CARTESIAN_POINT('Ctrl Pts',(-9.09262954448984,12.2,5.44439497528272));
#252350=CARTESIAN_POINT('Ctrl Pts',(-9.09594435124093,12.2,5.44548231237099));
#252351=CARTESIAN_POINT('Ctrl Pts',(-9.09928879714441,12.2,5.44657115890554));
#252352=CARTESIAN_POINT('Ctrl Pts',(-9.10266266749165,12.2,5.44766120355832));
#252353=CARTESIAN_POINT('Ctrl Pts',(-9.10603653783888,12.2,5.4487512482111));
#252354=CARTESIAN_POINT('Ctrl Pts',(-9.10943983401953,12.2,5.44984249250673));
#252355=CARTESIAN_POINT('Ctrl Pts',(-9.11287234174352,12.2,5.45093462973391));
#252356=CARTESIAN_POINT('Ctrl Pts',(-9.11630484946751,12.2,5.45202676696109));
#252357=CARTESIAN_POINT('Ctrl Pts',(-9.11976656842696,12.2,5.45311979833815));
#252358=CARTESIAN_POINT('Ctrl Pts',(-9.12325728947012,12.2,5.45421342458818));
#252359=CARTESIAN_POINT('Ctrl Pts',(-9.12674801051328,12.2,5.4553070508382));
#252360=CARTESIAN_POINT('Ctrl Pts',(-9.13026773159184,12.2,5.45640127216045));
#252361=CARTESIAN_POINT('Ctrl Pts',(-9.13381624673223,12.2,5.4574957928549));
#252362=CARTESIAN_POINT('Ctrl Pts',(-9.13736476187261,12.2,5.45859031354936));
#252363=CARTESIAN_POINT('Ctrl Pts',(-9.14094206901435,12.2,5.45968513642239));
#252364=CARTESIAN_POINT('Ctrl Pts',(-9.14454796287701,12.2,5.46077997043541));
#252365=CARTESIAN_POINT('Ctrl Pts',(-9.14815385673968,12.2,5.46187480444844));
#252366=CARTESIAN_POINT('Ctrl Pts',(-9.15178833831566,12.2,5.4629696498654));
#252367=CARTESIAN_POINT('Ctrl Pts',(-9.15545120047076,12.2,5.46406422389316));
#252368=CARTESIAN_POINT('Ctrl Pts',(-9.15911406262587,12.2,5.46515879792092));
#252369=CARTESIAN_POINT('Ctrl Pts',(-9.16280530921198,12.2,5.46625310067644));
#252370=CARTESIAN_POINT('Ctrl Pts',(-9.16652473601983,12.2,5.46734685213471));
#252371=CARTESIAN_POINT('Ctrl Pts',(-9.17098804802709,12.2,5.46865935383697));
#252372=CARTESIAN_POINT('Ctrl Pts',(-9.17549193793619,12.2,5.46997106231907));
#252373=CARTESIAN_POINT('Ctrl Pts',(-9.18003606418948,12.2,5.47128150410474));
#252374=CARTESIAN_POINT('Ctrl Pts',(-9.18382283620483,12.2,5.4723735389658));
#252375=CARTESIAN_POINT('Ctrl Pts',(-9.18763754887222,12.2,5.47346469435466));
#252376=CARTESIAN_POINT('Ctrl Pts',(-9.1914800049848,12.2,5.47455470331293));
#252377=CARTESIAN_POINT('Ctrl Pts',(-9.19609095215236,12.2,5.47586271401534));
#252378=CARTESIAN_POINT('Ctrl Pts',(-9.20074184915,12.2,5.47716906939287));
#252379=CARTESIAN_POINT('Ctrl Pts',(-9.20543235847785,12.2,5.4784733181789));
#252380=CARTESIAN_POINT('Ctrl Pts',(-9.20934111639308,12.2,5.47956019220676));
#252381=CARTESIAN_POINT('Ctrl Pts',(-9.21327738395769,12.2,5.48064560236669));
#252382=CARTESIAN_POINT('Ctrl Pts',(-9.21724096598949,12.2,5.48172928973273));
#252383=CARTESIAN_POINT('Ctrl Pts',(-9.22120454802129,12.2,5.48281297709876));
#252384=CARTESIAN_POINT('Ctrl Pts',(-9.22519544564443,12.2,5.48389494081666));
#252385=CARTESIAN_POINT('Ctrl Pts',(-9.22921346682499,12.2,5.48497492748332));
#252386=CARTESIAN_POINT('Ctrl Pts',(-9.23242788394462,12.2,5.48583891686375));
#252387=CARTESIAN_POINT('Ctrl Pts',(-9.23565965883015,12.2,5.4867016407468));
#252388=CARTESIAN_POINT('Ctrl Pts',(-9.23890869723122,12.2,5.48756297084915));
#252389=CARTESIAN_POINT('Ctrl Pts',(-9.24296999456853,12.2,5.48863963330106));
#252390=CARTESIAN_POINT('Ctrl Pts',(-9.24705826189028,12.2,5.48971411846532));
#252391=CARTESIAN_POINT('Ctrl Pts',(-9.25117331345342,12.2,5.49078617758477));
#252392=CARTESIAN_POINT('Ctrl Pts',(-9.25446535524217,12.2,5.49164382502054));
#252393=CARTESIAN_POINT('Ctrl Pts',(-9.25777453643259,12.2,5.4924999212062));
#252394=CARTESIAN_POINT('Ctrl Pts',(-9.26110076422498,12.2,5.49335433997499));
#252395=CARTESIAN_POINT('Ctrl Pts',(-9.26442699201738,12.2,5.49420875874378));
#252396=CARTESIAN_POINT('Ctrl Pts',(-9.2677702645923,12.2,5.4950615013957));
#252397=CARTESIAN_POINT('Ctrl Pts',(-9.27113048833273,12.2,5.49591244416412));
#252398=CARTESIAN_POINT('Ctrl Pts',(-9.27449071161533,12.2,5.49676338681659));
#252399=CARTESIAN_POINT('Ctrl Pts',(-9.27786788317086,12.2,5.49761252921759));
#252400=CARTESIAN_POINT('Ctrl Pts',(-9.28126191246435,12.2,5.49845975054108));
#252401=CARTESIAN_POINT('Ctrl Pts',(-9.28465594222028,12.2,5.49930697198001));
#252402=CARTESIAN_POINT('Ctrl Pts',(-9.28806682625804,12.2,5.50015227183102));
#252403=CARTESIAN_POINT('Ctrl Pts',(-9.29149447283542,12.2,5.50099553065453));
#252404=CARTESIAN_POINT('Ctrl Pts',(-9.2949221189458,12.2,5.50183878936316));
#252405=CARTESIAN_POINT('Ctrl Pts',(-9.29836652696233,12.2,5.50268000568594));
#252406=CARTESIAN_POINT('Ctrl Pts',(-9.30182760423387,12.2,5.50351906367305));
#252407=CARTESIAN_POINT('Ctrl Pts',(-9.30528868197698,12.2,5.50435812177448));
#252408=CARTESIAN_POINT('Ctrl Pts',(-9.30876642736289,12.2,5.50519502032855));
#252409=CARTESIAN_POINT('Ctrl Pts',(-9.31226074950713,12.2,5.50602964063776));
#252410=CARTESIAN_POINT('Ctrl Pts',(-9.31575507117526,12.2,5.50686426083325));
#252411=CARTESIAN_POINT('Ctrl Pts',(-9.31926596877066,12.2,5.50769660635815));
#252412=CARTESIAN_POINT('Ctrl Pts',(-9.32279335020345,12.2,5.50852655845712));
#252413=CARTESIAN_POINT('Ctrl Pts',(-9.32632073211684,12.2,5.50935651066919));
#252414=CARTESIAN_POINT('Ctrl Pts',(-9.32986459819609,12.2,5.51018406959484));
#252415=CARTESIAN_POINT('Ctrl Pts',(-9.33342485805786,12.2,5.51100912308408));
#252416=CARTESIAN_POINT('Ctrl Pts',(-9.33698511743456,12.2,5.51183417646092));
#252417=CARTESIAN_POINT('Ctrl Pts',(-9.34056176874994,12.2,5.51265672368185));
#252418=CARTESIAN_POINT('Ctrl Pts',(-9.34415472174539,12.2,5.513476651156));
#252419=CARTESIAN_POINT('Ctrl Pts',(-9.34774767523037,12.2,5.51429657874187));
#252420=CARTESIAN_POINT('Ctrl Pts',(-9.35135693197009,12.2,5.51511388774734));
#252421=CARTESIAN_POINT('Ctrl Pts',(-9.35498239927986,12.2,5.51592846662489));
#252422=CARTESIAN_POINT('Ctrl Pts',(-9.35860786609566,12.2,5.51674304539146));
#252423=CARTESIAN_POINT('Ctrl Pts',(-9.36224954496928,12.2,5.51755489262524));
#252424=CARTESIAN_POINT('Ctrl Pts',(-9.3659073456686,12.2,5.51836390005939));
#252425=CARTESIAN_POINT('Ctrl Pts',(-9.36956514686629,12.2,5.51917290760377));
#252426=CARTESIAN_POINT('Ctrl Pts',(-9.37323906979015,12.2,5.51997907446424));
#252427=CARTESIAN_POINT('Ctrl Pts',(-9.37692902578585,12.2,5.52078229273388));
#252428=CARTESIAN_POINT('Ctrl Pts',(-9.3806189812788,12.2,5.52158551089408));
#252429=CARTESIAN_POINT('Ctrl Pts',(-9.38432497038347,12.2,5.5223857807623));
#252430=CARTESIAN_POINT('Ctrl Pts',(-9.38804690313313,12.2,5.52318299358632));
#252431=CARTESIAN_POINT('Ctrl Pts',(-9.39176883638989,12.2,5.52398020651896));
#252432=CARTESIAN_POINT('Ctrl Pts',(-9.39550671258152,12.2,5.524774363018));
#252433=CARTESIAN_POINT('Ctrl Pts',(-9.39926044650833,12.2,5.52556535728333));
#252434=CARTESIAN_POINT('Ctrl Pts',(-9.40301418043514,12.2,5.52635635154866));
#252435=CARTESIAN_POINT('Ctrl Pts',(-9.40678377028045,12.2,5.52714418344975));
#252436=CARTESIAN_POINT('Ctrl Pts',(-9.41056912887724,12.2,5.52792874843661));
#252437=CARTESIAN_POINT('Ctrl Pts',(-9.4153008263496,12.2,5.52890945450984));
#252438=CARTESIAN_POINT('Ctrl Pts',(-9.42005716142557,12.2,5.52988505483397));
#252439=CARTESIAN_POINT('Ctrl Pts',(-9.42483796562467,12.2,5.53085534917308));
#252440=CARTESIAN_POINT('Ctrl Pts',(-9.42866260960928,12.2,5.5316315847713));
#252441=CARTESIAN_POINT('Ctrl Pts',(-9.43250291429818,12.2,5.53240442385252));
#252442=CARTESIAN_POINT('Ctrl Pts',(-9.43635879100832,12.2,5.53317376478333));
#252443=CARTESIAN_POINT('Ctrl Pts',(-9.44021466771848,12.2,5.53394310571416));
#252444=CARTESIAN_POINT('Ctrl Pts',(-9.44408611958044,12.2,5.534708947764));
#252445=CARTESIAN_POINT('Ctrl Pts',(-9.44797305762718,12.2,5.53547119141629));
#252446=CARTESIAN_POINT('Ctrl Pts',(-9.45185999514432,12.2,5.53623343496471));
#252447=CARTESIAN_POINT('Ctrl Pts',(-9.45576242035266,12.2,5.53699207853553));
#252448=CARTESIAN_POINT('Ctrl Pts',(-9.45968024777233,12.2,5.53774702403282));
#252449=CARTESIAN_POINT('Ctrl Pts',(-9.46359807572581,12.2,5.53850196963296));
#252450=CARTESIAN_POINT('Ctrl Pts',(-9.46753130613716,12.2,5.53925321680131));
#252451=CARTESIAN_POINT('Ctrl Pts',(-9.47147985285392,12.2,5.54000066589721));
#252452=CARTESIAN_POINT('Ctrl Pts',(-9.4754283990327,12.2,5.54074811489126));
#252453=CARTESIAN_POINT('Ctrl Pts',(-9.47939226200669,12.2,5.54149176726915));
#252454=CARTESIAN_POINT('Ctrl Pts',(-9.48337135812485,12.2,5.54223152493116));
#252455=CARTESIAN_POINT('Ctrl Pts',(-9.48735045478516,12.2,5.54297128269394));
#252456=CARTESIAN_POINT('Ctrl Pts',(-9.49134478324729,12.2,5.54370714589795));
#252457=CARTESIAN_POINT('Ctrl Pts',(-9.49535426057792,12.2,5.54443901882646));
#252458=CARTESIAN_POINT('Ctrl Pts',(-9.49936373736225,12.2,5.54517089165525));
#252459=CARTESIAN_POINT('Ctrl Pts',(-9.5033883624131,12.2,5.54589877369539));
#252460=CARTESIAN_POINT('Ctrl Pts',(-9.50742805267223,12.2,5.54662256889495));
#252461=CARTESIAN_POINT('Ctrl Pts',(-9.51146774348177,12.2,5.54734636419314));
#252462=CARTESIAN_POINT('Ctrl Pts',(-9.51552249876285,12.2,5.54806607493641));
#252463=CARTESIAN_POINT('Ctrl Pts',(-9.51959223604117,12.2,5.54878160530846));
#252464=CARTESIAN_POINT('Ctrl Pts',(-9.52467940736183,12.2,5.54967601822477));
#252465=CARTESIAN_POINT('Ctrl Pts',(-9.52978998560691,12.2,5.55056390072461));
#252466=CARTESIAN_POINT('Ctrl Pts',(-9.53492381276089,12.2,5.55144507030759));
#252467=CARTESIAN_POINT('Ctrl Pts',(-9.53903087414833,12.2,5.55215000591636));
#252468=CARTESIAN_POINT('Ctrl Pts',(-9.54315281303538,12.2,5.55285064471792));
#252469=CARTESIAN_POINT('Ctrl Pts',(-9.54728954862481,12.2,5.55354689764061));
#252470=CARTESIAN_POINT('Ctrl Pts',(-9.55142628477788,12.2,5.55424315065817));
#252471=CARTESIAN_POINT('Ctrl Pts',(-9.55557781577105,12.2,5.55493501498843));
#252472=CARTESIAN_POINT('Ctrl Pts',(-9.5597440618324,12.2,5.55562240208115));
#252473=CARTESIAN_POINT('Ctrl Pts',(-9.5639103073261,12.2,5.55630978908022));
#252474=CARTESIAN_POINT('Ctrl Pts',(-9.56809126674741,12.2,5.55699269764686));
#252475=CARTESIAN_POINT('Ctrl Pts',(-9.57228685884736,12.2,5.55767103864743));
#252476=CARTESIAN_POINT('Ctrl Pts',(-9.57648245151896,12.2,5.55834937974042));
#252477=CARTESIAN_POINT('Ctrl Pts',(-9.5806926758923,12.2,5.55902315322764));
#252478=CARTESIAN_POINT('Ctrl Pts',(-9.58491745325288,12.2,5.55969227093379));
#252479=CARTESIAN_POINT('Ctrl Pts',(-9.58914223003784,12.2,5.56036138854878));
#252480=CARTESIAN_POINT('Ctrl Pts',(-9.59338155894819,12.2,5.56102585002058));
#252481=CARTESIAN_POINT('Ctrl Pts',(-9.59763535782118,12.2,5.5616855671338));
#252482=CARTESIAN_POINT('Ctrl Pts',(-9.60188915727375,12.2,5.56234528433691));
#252483=CARTESIAN_POINT('Ctrl Pts',(-9.60615742795827,12.2,5.56300025864234));
#252484=CARTESIAN_POINT('Ctrl Pts',(-9.610440090025,12.2,5.56365040123334));
#252485=CARTESIAN_POINT('Ctrl Pts',(-9.61472275209172,12.2,5.56430054382433));
#252486=CARTESIAN_POINT('Ctrl Pts',(-9.61901980482682,12.2,5.56494585762586));
#252487=CARTESIAN_POINT('Ctrl Pts',(-9.62333116822992,12.2,5.5655862541047));
#252488=CARTESIAN_POINT('Ctrl Pts',(-9.62764253104559,12.2,5.56622665049629));
#252489=CARTESIAN_POINT('Ctrl Pts',(-9.63196820497383,12.2,5.56686213045657));
#252490=CARTESIAN_POINT('Ctrl Pts',(-9.63630811047205,12.2,5.56749261024124));
#252491=CARTESIAN_POINT('Ctrl Pts',(-9.64064801656159,12.2,5.56812309011182));
#252492=CARTESIAN_POINT('Ctrl Pts',(-9.64500215466359,12.2,5.56874856910148));
#252493=CARTESIAN_POINT('Ctrl Pts',(-9.64937044468089,12.2,5.56936896413477));
#252494=CARTESIAN_POINT('Ctrl Pts',(-9.65373873410301,12.2,5.56998935908353));
#252495=CARTESIAN_POINT('Ctrl Pts',(-9.65812117615106,12.2,5.57060466800239));
#252496=CARTESIAN_POINT('Ctrl Pts',(-9.66251769112405,12.2,5.57121481100841));
#252497=CARTESIAN_POINT('Ctrl Pts',(-9.66581507750354,12.2,5.57167241828371));
#252498=CARTESIAN_POINT('Ctrl Pts',(-9.66912038139817,12.2,5.57212711747274));
#252499=CARTESIAN_POINT('Ctrl Pts',(-9.67243356790073,12.2,5.57257887589591));
#252500=CARTESIAN_POINT('Ctrl Pts',(-9.67574675440329,12.2,5.57303063431907));
#252501=CARTESIAN_POINT('Ctrl Pts',(-9.67906782442966,12.2,5.5734794528186));
#252502=CARTESIAN_POINT('Ctrl Pts',(-9.68239674476597,12.2,5.57392529467781));
#252503=CARTESIAN_POINT('Ctrl Pts',(-9.68572566570703,12.2,5.57437113661801));
#252504=CARTESIAN_POINT('Ctrl Pts',(-9.68906243780863,12.2,5.57481400246571));
#252505=CARTESIAN_POINT('Ctrl Pts',(-9.69240702671246,12.2,5.57525385936256));
#252506=CARTESIAN_POINT('Ctrl Pts',(-9.69575161500868,12.2,5.57569371617951));
#252507=CARTESIAN_POINT('Ctrl Pts',(-9.6991040210878,12.2,5.57613056321327));
#252508=CARTESIAN_POINT('Ctrl Pts',(-9.70246421142472,12.2,5.57656436657224));
#252509=CARTESIAN_POINT('Ctrl Pts',(-9.70582440176164,12.2,5.57699816993121));
#252510=CARTESIAN_POINT('Ctrl Pts',(-9.70919237709369,12.2,5.57742892938067));
#252511=CARTESIAN_POINT('Ctrl Pts',(-9.71256810444474,12.2,5.57785661224206));
#252512=CARTESIAN_POINT('Ctrl Pts',(-9.7181943169009,12.2,5.57856941703695));
#252513=CARTESIAN_POINT('Ctrl Pts',(-9.72384206380311,12.2,5.57927367373479));
#252514=CARTESIAN_POINT('Ctrl Pts',(-9.72951119359589,12.2,5.57996923026211));
#252515=CARTESIAN_POINT('Ctrl Pts',(-9.73404649705935,12.2,5.58052567543848));
#252516=CARTESIAN_POINT('Ctrl Pts',(-9.73859548588673,12.2,5.58107655219652));
#252517=CARTESIAN_POINT('Ctrl Pts',(-9.74315808334569,12.2,5.58162178265253));
#252518=CARTESIAN_POINT('Ctrl Pts',(-9.74658003221697,12.2,5.58203070558739));
#252519=CARTESIAN_POINT('Ctrl Pts',(-9.75000963559875,12.2,5.58243645244636));
#252520=CARTESIAN_POINT('Ctrl Pts',(-9.753446862016,12.2,5.58283899133776));
#252521=CARTESIAN_POINT('Ctrl Pts',(-9.75688408780881,12.2,5.58324153015603));
#252522=CARTESIAN_POINT('Ctrl Pts',(-9.7603289359368,12.2,5.58364086020492));
#252523=CARTESIAN_POINT('Ctrl Pts',(-9.76378137490137,12.2,5.58403694962661));
#252524=CARTESIAN_POINT('Ctrl Pts',(-9.76723381386595,12.2,5.5844330390483));
#252525=CARTESIAN_POINT('Ctrl Pts',(-9.7706938435701,12.2,5.58482588814019));
#252526=CARTESIAN_POINT('Ctrl Pts',(-9.7741614309031,12.2,5.58521546454242));
#252527=CARTESIAN_POINT('Ctrl Pts',(-9.77762901823611,12.2,5.58560504094464));
#252528=CARTESIAN_POINT('Ctrl Pts',(-9.78110416479321,12.2,5.58599134436393));
#252529=CARTESIAN_POINT('Ctrl Pts',(-9.78458683804167,12.2,5.58637434426668));
#252530=CARTESIAN_POINT('Ctrl Pts',(-9.78806951129012,12.2,5.58675734416943));
#252531=CARTESIAN_POINT('Ctrl Pts',(-9.79155971034661,12.2,5.58713703992232));
#252532=CARTESIAN_POINT('Ctrl Pts',(-9.79505740463555,12.2,5.58751339940893));
#252533=CARTESIAN_POINT('Ctrl Pts',(-9.79855509892447,12.2,5.58788975889555));
#252534=CARTESIAN_POINT('Ctrl Pts',(-9.80206028787347,12.2,5.5882627834897));
#252535=CARTESIAN_POINT('Ctrl Pts',(-9.80557294029547,12.2,5.58863244091179));
#252536=CARTESIAN_POINT('Ctrl Pts',(-9.80908559271745,12.2,5.58900209833388));
#252537=CARTESIAN_POINT('Ctrl Pts',(-9.81260570726018,12.2,5.58936838911695));
#252538=CARTESIAN_POINT('Ctrl Pts',(-9.81613325396433,12.2,5.58973128243756));
#252539=CARTESIAN_POINT('Ctrl Pts',(-9.81966080130931,12.2,5.5900941758241));
#252540=CARTESIAN_POINT('Ctrl Pts',(-9.82319577992308,12.2,5.59045366969301));
#252541=CARTESIAN_POINT('Ctrl Pts',(-9.82673815881393,12.2,5.59080973703596));
#252542=CARTESIAN_POINT('Ctrl Pts',(-9.83146132959582,12.2,5.59128449338542));
#252543=CARTESIAN_POINT('Ctrl Pts',(-9.8361976552621,12.2,5.591753153644));
#252544=CARTESIAN_POINT('Ctrl Pts',(-9.84094706209519,12.2,5.59221564749548));
#252545=CARTESIAN_POINT('Ctrl Pts',(-9.84450911738179,12.2,5.59256251789984));
#252546=CARTESIAN_POINT('Ctrl Pts',(-9.84807853118457,12.2,5.59290591850444));
#252547=CARTESIAN_POINT('Ctrl Pts',(-9.85165527101195,12.2,5.59324582090924));
#252548=CARTESIAN_POINT('Ctrl Pts',(-9.85523201148911,12.2,5.59358572337579));
#252549=CARTESIAN_POINT('Ctrl Pts',(-9.85881607917667,12.2,5.59392212679134));
#252550=CARTESIAN_POINT('Ctrl Pts',(-9.86240744253293,12.2,5.59425500083924));
#252551=CARTESIAN_POINT('Ctrl Pts',(-9.86599880523677,12.2,5.59458787482666));
#252552=CARTESIAN_POINT('Ctrl Pts',(-9.86959746236442,12.2,5.59491722109231));
#252553=CARTESIAN_POINT('Ctrl Pts',(-9.8732033847894,12.2,5.59524300759634));
#252554=CARTESIAN_POINT('Ctrl Pts',(-9.87801128113769,12.2,5.59567738958199));
#252555=CARTESIAN_POINT('Ctrl Pts',(-9.88283209181486,12.2,5.59610544514953));
#252556=CARTESIAN_POINT('Ctrl Pts',(-9.88766574336331,12.2,5.59652710444881));
#252557=CARTESIAN_POINT('Ctrl Pts',(-9.89129098218929,12.2,5.59684334893764));
#252558=CARTESIAN_POINT('Ctrl Pts',(-9.89492344463978,12.2,5.59715599571005));
#252559=CARTESIAN_POINT('Ctrl Pts',(-9.89856309850657,12.2,5.59746501565764));
#252560=CARTESIAN_POINT('Ctrl Pts',(-9.90220275303456,12.2,5.59777403566139));
#252561=CARTESIAN_POINT('Ctrl Pts',(-9.90584960003122,12.2,5.59807942857243));
#252562=CARTESIAN_POINT('Ctrl Pts',(-9.90950360852158,12.2,5.59838116603245));
#252563=CARTESIAN_POINT('Ctrl Pts',(-9.91315761634814,12.2,5.59868290343766));
#252564=CARTESIAN_POINT('Ctrl Pts',(-9.916818785809,12.2,5.59898098467001));
#252565=CARTESIAN_POINT('Ctrl Pts',(-9.92048708619313,12.2,5.5992753820486));
#252566=CARTESIAN_POINT('Ctrl Pts',(-9.92415538657726,12.2,5.59956977942718));
#252567=CARTESIAN_POINT('Ctrl Pts',(-9.92783081565137,12.2,5.59986049160864));
#252568=CARTESIAN_POINT('Ctrl Pts',(-9.93151334589319,12.2,5.60014749105623));
#252569=CARTESIAN_POINT('Ctrl Pts',(-9.93642338599263,12.2,5.60053015696896));
#252570=CARTESIAN_POINT('Ctrl Pts',(-9.94134604849508,12.2,5.60090622124413));
#252571=CARTESIAN_POINT('Ctrl Pts',(-9.94628126070143,12.2,5.60127561971461));
#252572=CARTESIAN_POINT('Ctrl Pts',(-9.94998267069671,12.2,5.60155266863039));
#252573=CARTESIAN_POINT('Ctrl Pts',(-9.95369114066905,12.2,5.60182596663677));
#252574=CARTESIAN_POINT('Ctrl Pts',(-9.95740664008499,12.2,5.6020954870921));
#252575=CARTESIAN_POINT('Ctrl Pts',(-9.96112213882595,12.2,5.60236500749846));
#252576=CARTESIAN_POINT('Ctrl Pts',(-9.96484466592003,12.2,5.60263074873086));
#252577=CARTESIAN_POINT('Ctrl Pts',(-9.96857418997165,12.2,5.60289268277565));
#252578=CARTESIAN_POINT('Ctrl Pts',(-9.97354688848131,12.2,5.60324192815285));
#252579=CARTESIAN_POINT('Ctrl Pts',(-9.97853202621204,12.2,5.6035844046495));
#252580=CARTESIAN_POINT('Ctrl Pts',(-9.98352953635825,12.2,5.60392005195584));
#252581=CARTESIAN_POINT('Ctrl Pts',(-9.98727766913814,12.2,5.60417178744703));
#252582=CARTESIAN_POINT('Ctrl Pts',(-9.99103276126752,12.2,5.60441968228848));
#252583=CARTESIAN_POINT('Ctrl Pts',(-9.99479478496322,12.2,5.60466370919681));
#252584=CARTESIAN_POINT('Ctrl Pts',(-9.99855680934236,12.2,5.60490773614947));
#252585=CARTESIAN_POINT('Ctrl Pts',(-10.0023257639401,12.2,5.60514789495104));
#252586=CARTESIAN_POINT('Ctrl Pts',(-10.0061016128231,12.2,5.60538415381818));
#252587=CARTESIAN_POINT('Ctrl Pts',(-10.0098774610202,12.2,5.6056204126424));
#252588=CARTESIAN_POINT('Ctrl Pts',(-10.0136602026308,12.2,5.60585276952485));
#252589=CARTESIAN_POINT('Ctrl Pts',(-10.0174498052666,12.2,5.60608119706917));
#252590=CARTESIAN_POINT('Ctrl Pts',(-10.0212394079023,12.2,5.60630962461349));
#252591=CARTESIAN_POINT('Ctrl Pts',(-10.0250358713842,12.2,5.60653412069107));
#252592=CARTESIAN_POINT('Ctrl Pts',(-10.028839180665,12.2,5.6067546754843));
#252593=CARTESIAN_POINT('Ctrl Pts',(-10.0326424899459,12.2,5.60697523027754));
#252594=CARTESIAN_POINT('Ctrl Pts',(-10.0364526481964,12.2,5.60719184195524));
#252595=CARTESIAN_POINT('Ctrl Pts',(-10.0402696490001,12.2,5.60740451199998));
#252596=CARTESIAN_POINT('Origin',(-5.66257110645729E-14,15.2,-1.77635683940025E-14));
#252597=CARTESIAN_POINT('',(-9.55499537100006,15.2,4.04260911599999));
#252598=CARTESIAN_POINT('',(-9.55499537100006,12.2,4.04260911599999));
#252599=CARTESIAN_POINT('',(-9.55499537100006,15.2,4.04260911599999));
#252600=CARTESIAN_POINT('Origin',(-5.66257110645729E-14,12.2,-1.77635683940025E-14));
#252601=CARTESIAN_POINT('Origin',(-5.66257110645729E-14,15.2,-1.77635683940025E-14));
#252602=CARTESIAN_POINT('Origin',(-5.66257110645729E-14,15.2,-1.77635683940025E-14));
#252603=CARTESIAN_POINT('',(-10.7360910480001,15.2,4.12144986899998));
#252604=CARTESIAN_POINT('',(-10.8675859440001,15.2,3.76106045599998));
#252605=CARTESIAN_POINT('Origin',(-5.66257110645729E-14,15.2,-1.77635683940025E-14));
#252606=CARTESIAN_POINT('',(-10.8675859440001,12.2,3.76106045599998));
#252607=CARTESIAN_POINT('',(-10.8675859440001,15.2,3.76106045599998));
#252608=CARTESIAN_POINT('',(-10.7360910480001,12.2,4.12144986899998));
#252609=CARTESIAN_POINT('Origin',(-5.66257110645729E-14,12.2,-1.77635683940025E-14));
#252610=CARTESIAN_POINT('',(-10.7360910480001,15.2,4.12144986899998));
#252611=CARTESIAN_POINT('Ctrl Pts',(-9.55499537100006,15.2,4.04260911699998));
#252612=CARTESIAN_POINT('Ctrl Pts',(-9.55499537100006,11.6,4.04260911699998));
#252613=CARTESIAN_POINT('Ctrl Pts',(-9.55516119300006,15.2,4.04266300499999));
#252614=CARTESIAN_POINT('Ctrl Pts',(-9.55516119300006,11.6,4.04266300499999));
#252615=CARTESIAN_POINT('Ctrl Pts',(-9.55549865500006,15.2,4.04277257899999));
#252616=CARTESIAN_POINT('Ctrl Pts',(-9.55549865500006,11.6,4.04277257899999));
#252617=CARTESIAN_POINT('Ctrl Pts',(-9.55601007100006,15.2,4.04293835899999));
#252618=CARTESIAN_POINT('Ctrl Pts',(-9.55601007100006,11.6,4.04293835899998));
#252619=CARTESIAN_POINT('Ctrl Pts',(-9.55669916300005,15.2,4.04316116599999));
#252620=CARTESIAN_POINT('Ctrl Pts',(-9.55669916300005,11.6,4.04316116599999));
#252621=CARTESIAN_POINT('Ctrl Pts',(-9.55757104200006,15.2,4.04344211399999));
#252622=CARTESIAN_POINT('Ctrl Pts',(-9.55757104200006,11.6,4.04344211399999));
#252623=CARTESIAN_POINT('Ctrl Pts',(-9.55845733900006,15.2,4.04372672599998));
#252624=CARTESIAN_POINT('Ctrl Pts',(-9.55845733900006,11.6,4.04372672599998));
#252625=CARTESIAN_POINT('Ctrl Pts',(-9.55935298100006,15.2,4.04401334799999));
#252626=CARTESIAN_POINT('Ctrl Pts',(-9.55935298100006,11.6,4.04401334799999));
#252627=CARTESIAN_POINT('Ctrl Pts',(-9.56025795200006,15.2,4.04430195599998));
#252628=CARTESIAN_POINT('Ctrl Pts',(-9.56025795200006,11.6,4.04430195599998));
#252629=CARTESIAN_POINT('Ctrl Pts',(-9.56117222800006,15.2,4.04459252399998));
#252630=CARTESIAN_POINT('Ctrl Pts',(-9.56117222800006,11.6,4.04459252399998));
#252631=CARTESIAN_POINT('Ctrl Pts',(-9.56209579100006,15.2,4.04488502599998));
#252632=CARTESIAN_POINT('Ctrl Pts',(-9.56209579100006,11.6,4.04488502599998));
#252633=CARTESIAN_POINT('Ctrl Pts',(-9.56302862000006,15.2,4.04517943699998));
#252634=CARTESIAN_POINT('Ctrl Pts',(-9.56302862000006,11.6,4.04517943699998));
#252635=CARTESIAN_POINT('Ctrl Pts',(-9.56397069600006,15.2,4.04547573399999));
#252636=CARTESIAN_POINT('Ctrl Pts',(-9.56397069600006,11.6,4.04547573399998));
#252637=CARTESIAN_POINT('Ctrl Pts',(-9.56492199900006,15.2,4.04577388999999));
#252638=CARTESIAN_POINT('Ctrl Pts',(-9.56492199900006,11.6,4.04577388999999));
#252639=CARTESIAN_POINT('Ctrl Pts',(-9.56588251000005,15.2,4.04607387999998));
#252640=CARTESIAN_POINT('Ctrl Pts',(-9.56588251000005,11.6,4.04607387999998));
#252641=CARTESIAN_POINT('Ctrl Pts',(-9.56685220800006,15.2,4.04637568199998));
#252642=CARTESIAN_POINT('Ctrl Pts',(-9.56685220800006,11.6,4.04637568199998));
#252643=CARTESIAN_POINT('Ctrl Pts',(-9.56783107300006,15.2,4.04667926899998));
#252644=CARTESIAN_POINT('Ctrl Pts',(-9.56783107300006,11.6,4.04667926899998));
#252645=CARTESIAN_POINT('Ctrl Pts',(-9.56881908800005,15.2,4.04698461699999));
#252646=CARTESIAN_POINT('Ctrl Pts',(-9.56881908800005,11.6,4.04698461699999));
#252647=CARTESIAN_POINT('Ctrl Pts',(-9.56981623300006,15.2,4.04729170299999));
#252648=CARTESIAN_POINT('Ctrl Pts',(-9.56981623300006,11.6,4.04729170299999));
#252649=CARTESIAN_POINT('Ctrl Pts',(-9.57082248800005,15.2,4.04760050199998));
#252650=CARTESIAN_POINT('Ctrl Pts',(-9.57082248800005,11.6,4.04760050199998));
#252651=CARTESIAN_POINT('Ctrl Pts',(-9.57183783400006,15.2,4.04791098999999));
#252652=CARTESIAN_POINT('Ctrl Pts',(-9.57183783400006,11.6,4.04791098999999));
#252653=CARTESIAN_POINT('Ctrl Pts',(-9.57286225200006,15.2,4.04822314299999));
#252654=CARTESIAN_POINT('Ctrl Pts',(-9.57286225200006,11.6,4.04822314299999));
#252655=CARTESIAN_POINT('Ctrl Pts',(-9.57389572300006,15.2,4.04853693899998));
#252656=CARTESIAN_POINT('Ctrl Pts',(-9.57389572300006,11.6,4.04853693899998));
#252657=CARTESIAN_POINT('Ctrl Pts',(-9.57493822900006,15.2,4.04885235199998));
#252658=CARTESIAN_POINT('Ctrl Pts',(-9.57493822900006,11.6,4.04885235199998));
#252659=CARTESIAN_POINT('Ctrl Pts',(-9.57598974800005,15.2,4.04916935999999));
#252660=CARTESIAN_POINT('Ctrl Pts',(-9.57598974800005,11.6,4.04916935999999));
#252661=CARTESIAN_POINT('Ctrl Pts',(-9.57705026600006,15.2,4.04948793999999));
#252662=CARTESIAN_POINT('Ctrl Pts',(-9.57705026600006,11.6,4.04948793999999));
#252663=CARTESIAN_POINT('Ctrl Pts',(-9.57811976000006,15.2,4.04980806699999));
#252664=CARTESIAN_POINT('Ctrl Pts',(-9.57811976000006,11.6,4.04980806699999));
#252665=CARTESIAN_POINT('Ctrl Pts',(-9.57919821400005,15.2,4.05012971899998));
#252666=CARTESIAN_POINT('Ctrl Pts',(-9.57919821400005,11.6,4.05012971899998));
#252667=CARTESIAN_POINT('Ctrl Pts',(-9.58028560900006,15.2,4.05045287299998));
#252668=CARTESIAN_POINT('Ctrl Pts',(-9.58028560900006,11.6,4.05045287299998));
#252669=CARTESIAN_POINT('Ctrl Pts',(-9.58138192600006,15.2,4.05077750599999));
#252670=CARTESIAN_POINT('Ctrl Pts',(-9.58138192600006,11.6,4.05077750599998));
#252671=CARTESIAN_POINT('Ctrl Pts',(-9.58248714800006,15.2,4.05110359599998));
#252672=CARTESIAN_POINT('Ctrl Pts',(-9.58248714800006,11.6,4.05110359599998));
#252673=CARTESIAN_POINT('Ctrl Pts',(-9.58360125400005,15.2,4.05143111799998));
#252674=CARTESIAN_POINT('Ctrl Pts',(-9.58360125400005,11.6,4.05143111799998));
#252675=CARTESIAN_POINT('Ctrl Pts',(-9.58472422800006,15.2,4.05176005199999));
#252676=CARTESIAN_POINT('Ctrl Pts',(-9.58472422800006,11.6,4.05176005199999));
#252677=CARTESIAN_POINT('Ctrl Pts',(-9.58585605100006,15.2,4.05209037499999));
#252678=CARTESIAN_POINT('Ctrl Pts',(-9.58585605100006,11.6,4.05209037499999));
#252679=CARTESIAN_POINT('Ctrl Pts',(-9.58699670500006,15.2,4.05242206399999));
#252680=CARTESIAN_POINT('Ctrl Pts',(-9.58699670500006,11.6,4.05242206399999));
#252681=CARTESIAN_POINT('Ctrl Pts',(-9.58814617200006,15.2,4.05275509699998));
#252682=CARTESIAN_POINT('Ctrl Pts',(-9.58814617200006,11.6,4.05275509699998));
#252683=CARTESIAN_POINT('Ctrl Pts',(-9.58930443500006,15.2,4.05308945199998));
#252684=CARTESIAN_POINT('Ctrl Pts',(-9.58930443500006,11.6,4.05308945199998));
#252685=CARTESIAN_POINT('Ctrl Pts',(-9.59047147500005,15.2,4.05342510699998));
#252686=CARTESIAN_POINT('Ctrl Pts',(-9.59047147500005,11.6,4.05342510699998));
#252687=CARTESIAN_POINT('Ctrl Pts',(-9.59164727400006,15.2,4.05376203999998));
#252688=CARTESIAN_POINT('Ctrl Pts',(-9.59164727400006,11.6,4.05376203999998));
#252689=CARTESIAN_POINT('Ctrl Pts',(-9.59283181500006,15.2,4.05410022899999));
#252690=CARTESIAN_POINT('Ctrl Pts',(-9.59283181500006,11.6,4.05410022899999));
#252691=CARTESIAN_POINT('Ctrl Pts',(-9.59402508100006,15.2,4.05443965299998));
#252692=CARTESIAN_POINT('Ctrl Pts',(-9.59402508100006,11.6,4.05443965299998));
#252693=CARTESIAN_POINT('Ctrl Pts',(-9.59522705300006,15.2,4.05478028999998));
#252694=CARTESIAN_POINT('Ctrl Pts',(-9.59522705300006,11.6,4.05478028999998));
#252695=CARTESIAN_POINT('Ctrl Pts',(-9.59643771400006,15.2,4.05512211999999));
#252696=CARTESIAN_POINT('Ctrl Pts',(-9.59643771400006,11.6,4.05512211999999));
#252697=CARTESIAN_POINT('Ctrl Pts',(-9.59765704500006,15.2,4.05546511899999));
#252698=CARTESIAN_POINT('Ctrl Pts',(-9.59765704500006,11.6,4.05546511899998));
#252699=CARTESIAN_POINT('Ctrl Pts',(-9.59888503300006,15.2,4.05580926699999));
#252700=CARTESIAN_POINT('Ctrl Pts',(-9.59888503300006,11.6,4.05580926699999));
#252701=CARTESIAN_POINT('Ctrl Pts',(-9.60012165600006,15.2,4.05615454399998));
#252702=CARTESIAN_POINT('Ctrl Pts',(-9.60012165600006,11.6,4.05615454399998));
#252703=CARTESIAN_POINT('Ctrl Pts',(-9.60136689800006,15.2,4.05650092799998));
#252704=CARTESIAN_POINT('Ctrl Pts',(-9.60136689800006,11.6,4.05650092799998));
#252705=CARTESIAN_POINT('Ctrl Pts',(-9.60262074400006,15.2,4.05684839599999));
#252706=CARTESIAN_POINT('Ctrl Pts',(-9.60262074400006,11.6,4.05684839599999));
#252707=CARTESIAN_POINT('Ctrl Pts',(-9.60388317400006,15.2,4.05719693099999));
#252708=CARTESIAN_POINT('Ctrl Pts',(-9.60388317400006,11.6,4.05719693099999));
#252709=CARTESIAN_POINT('Ctrl Pts',(-9.60515417300006,15.2,4.05754650999998));
#252710=CARTESIAN_POINT('Ctrl Pts',(-9.60515417300006,11.6,4.05754650999998));
#252711=CARTESIAN_POINT('Ctrl Pts',(-9.60643372200006,15.2,4.05789711199999));
#252712=CARTESIAN_POINT('Ctrl Pts',(-9.60643372200006,11.6,4.05789711199999));
#252713=CARTESIAN_POINT('Ctrl Pts',(-9.60772180600006,15.2,4.05824871799998));
#252714=CARTESIAN_POINT('Ctrl Pts',(-9.60772180600006,11.6,4.05824871799998));
#252715=CARTESIAN_POINT('Ctrl Pts',(-9.60901840800006,15.2,4.05860130499998));
#252716=CARTESIAN_POINT('Ctrl Pts',(-9.60901840800006,11.6,4.05860130499998));
#252717=CARTESIAN_POINT('Ctrl Pts',(-9.61032351000006,15.2,4.05895485699999));
#252718=CARTESIAN_POINT('Ctrl Pts',(-9.61032351000006,11.6,4.05895485699998));
#252719=CARTESIAN_POINT('Ctrl Pts',(-9.61163709700006,15.2,4.05930934899998));
#252720=CARTESIAN_POINT('Ctrl Pts',(-9.61163709700006,11.6,4.05930934899998));
#252721=CARTESIAN_POINT('Ctrl Pts',(-9.61295914900005,15.2,4.05966476399998));
#252722=CARTESIAN_POINT('Ctrl Pts',(-9.61295914900005,11.6,4.05966476399998));
#252723=CARTESIAN_POINT('Ctrl Pts',(-9.61428965300006,15.2,4.06002107999999));
#252724=CARTESIAN_POINT('Ctrl Pts',(-9.61428965300006,11.6,4.06002107999999));
#252725=CARTESIAN_POINT('Ctrl Pts',(-9.61562859000006,15.2,4.06037827999998));
#252726=CARTESIAN_POINT('Ctrl Pts',(-9.61562859000006,11.6,4.06037827999998));
#252727=CARTESIAN_POINT('Ctrl Pts',(-9.61697594500006,15.2,4.06073633999998));
#252728=CARTESIAN_POINT('Ctrl Pts',(-9.61697594500006,11.6,4.06073633999998));
#252729=CARTESIAN_POINT('Ctrl Pts',(-9.61833170200006,15.2,4.06109524299998));
#252730=CARTESIAN_POINT('Ctrl Pts',(-9.61833170200006,11.6,4.06109524299998));
#252731=CARTESIAN_POINT('Ctrl Pts',(-9.61969584100006,15.2,4.06145496799999));
#252732=CARTESIAN_POINT('Ctrl Pts',(-9.61969584100006,11.6,4.06145496799999));
#252733=CARTESIAN_POINT('Ctrl Pts',(-9.62106835000006,15.2,4.06181549699999));
#252734=CARTESIAN_POINT('Ctrl Pts',(-9.62106835000006,11.6,4.06181549699998));
#252735=CARTESIAN_POINT('Ctrl Pts',(-9.62244921100006,15.2,4.06217680799998));
#252736=CARTESIAN_POINT('Ctrl Pts',(-9.62244921100006,11.6,4.06217680799998));
#252737=CARTESIAN_POINT('Ctrl Pts',(-9.62383840700006,15.2,4.06253888499998));
#252738=CARTESIAN_POINT('Ctrl Pts',(-9.62383840700006,11.6,4.06253888499998));
#252739=CARTESIAN_POINT('Ctrl Pts',(-9.62523592300006,15.2,4.06290170499998));
#252740=CARTESIAN_POINT('Ctrl Pts',(-9.62523592300006,11.6,4.06290170499998));
#252741=CARTESIAN_POINT('Ctrl Pts',(-9.62664174300006,15.2,4.06326525199999));
#252742=CARTESIAN_POINT('Ctrl Pts',(-9.62664174300006,11.6,4.06326525199999));
#252743=CARTESIAN_POINT('Ctrl Pts',(-9.62805585000006,15.2,4.06362950399998));
#252744=CARTESIAN_POINT('Ctrl Pts',(-9.62805585000006,11.6,4.06362950399998));
#252745=CARTESIAN_POINT('Ctrl Pts',(-9.62947822800006,15.2,4.06399444399998));
#252746=CARTESIAN_POINT('Ctrl Pts',(-9.62947822800006,11.6,4.06399444399998));
#252747=CARTESIAN_POINT('Ctrl Pts',(-9.63090886200006,15.2,4.06436005199998));
#252748=CARTESIAN_POINT('Ctrl Pts',(-9.63090886200006,11.6,4.06436005199998));
#252749=CARTESIAN_POINT('Ctrl Pts',(-9.63234773700006,15.2,4.06472630899999));
#252750=CARTESIAN_POINT('Ctrl Pts',(-9.63234773700006,11.6,4.06472630899999));
#252751=CARTESIAN_POINT('Ctrl Pts',(-9.63379483400006,15.2,4.06509319699998));
#252752=CARTESIAN_POINT('Ctrl Pts',(-9.63379483400006,11.6,4.06509319699998));
#252753=CARTESIAN_POINT('Ctrl Pts',(-9.63525014000006,15.2,4.06546069799998));
#252754=CARTESIAN_POINT('Ctrl Pts',(-9.63525014000006,11.6,4.06546069799998));
#252755=CARTESIAN_POINT('Ctrl Pts',(-9.63671363700006,15.2,4.06582879099999));
#252756=CARTESIAN_POINT('Ctrl Pts',(-9.63671363700006,11.6,4.06582879099999));
#252757=CARTESIAN_POINT('Ctrl Pts',(-9.63818531300005,15.2,4.06619745799999));
#252758=CARTESIAN_POINT('Ctrl Pts',(-9.63818531300005,11.6,4.06619745799999));
#252759=CARTESIAN_POINT('Ctrl Pts',(-9.63966514800006,15.2,4.06656668199999));
#252760=CARTESIAN_POINT('Ctrl Pts',(-9.63966514800006,11.6,4.06656668199999));
#252761=CARTESIAN_POINT('Ctrl Pts',(-9.64115313000006,15.2,4.06693644299998));
#252762=CARTESIAN_POINT('Ctrl Pts',(-9.64115313000006,11.6,4.06693644299998));
#252763=CARTESIAN_POINT('Ctrl Pts',(-9.64264924100006,15.2,4.06730672499998));
#252764=CARTESIAN_POINT('Ctrl Pts',(-9.64264924100006,11.6,4.06730672499998));
#252765=CARTESIAN_POINT('Ctrl Pts',(-9.64415346700006,15.2,4.06767750699998));
#252766=CARTESIAN_POINT('Ctrl Pts',(-9.64415346700006,11.6,4.06767750699998));
#252767=CARTESIAN_POINT('Ctrl Pts',(-9.64566579300006,15.2,4.06804877199999));
#252768=CARTESIAN_POINT('Ctrl Pts',(-9.64566579300006,11.6,4.06804877199998));
#252769=CARTESIAN_POINT('Ctrl Pts',(-9.64718620100006,15.2,4.06842050299999));
#252770=CARTESIAN_POINT('Ctrl Pts',(-9.64718620100006,11.6,4.06842050299998));
#252771=CARTESIAN_POINT('Ctrl Pts',(-9.64871467900006,15.2,4.06879268099999));
#252772=CARTESIAN_POINT('Ctrl Pts',(-9.64871467900006,11.6,4.06879268099999));
#252773=CARTESIAN_POINT('Ctrl Pts',(-9.65025121000006,15.2,4.06916528799999));
#252774=CARTESIAN_POINT('Ctrl Pts',(-9.65025121000006,11.6,4.06916528799999));
#252775=CARTESIAN_POINT('Ctrl Pts',(-9.65179577900006,15.2,4.06953830699998));
#252776=CARTESIAN_POINT('Ctrl Pts',(-9.65179577900006,11.6,4.06953830699998));
#252777=CARTESIAN_POINT('Ctrl Pts',(-9.65334837100006,15.2,4.06991171799999));
#252778=CARTESIAN_POINT('Ctrl Pts',(-9.65334837100006,11.6,4.06991171799999));
#252779=CARTESIAN_POINT('Ctrl Pts',(-9.65490897100005,15.2,4.07028550599998));
#252780=CARTESIAN_POINT('Ctrl Pts',(-9.65490897100005,11.6,4.07028550599998));
#252781=CARTESIAN_POINT('Ctrl Pts',(-9.65647756400006,15.2,4.07065965099999));
#252782=CARTESIAN_POINT('Ctrl Pts',(-9.65647756400006,11.6,4.07065965099999));
#252783=CARTESIAN_POINT('Ctrl Pts',(-9.65805413400006,15.2,4.07103413899998));
#252784=CARTESIAN_POINT('Ctrl Pts',(-9.65805413400006,11.6,4.07103413899998));
#252785=CARTESIAN_POINT('Ctrl Pts',(-9.65963866800006,15.2,4.07140894899998));
#252786=CARTESIAN_POINT('Ctrl Pts',(-9.65963866800006,11.6,4.07140894899998));
#252787=CARTESIAN_POINT('Ctrl Pts',(-9.66123114800006,15.2,4.07178406499998));
#252788=CARTESIAN_POINT('Ctrl Pts',(-9.66123114800006,11.6,4.07178406499998));
#252789=CARTESIAN_POINT('Ctrl Pts',(-9.66283156300005,15.2,4.07215947099999));
#252790=CARTESIAN_POINT('Ctrl Pts',(-9.66283156300005,11.6,4.07215947099999));
#252791=CARTESIAN_POINT('Ctrl Pts',(-9.66443989600006,15.2,4.07253514799999));
#252792=CARTESIAN_POINT('Ctrl Pts',(-9.66443989600006,11.6,4.07253514799999));
#252793=CARTESIAN_POINT('Ctrl Pts',(-9.66605613200005,15.2,4.07291107899999));
#252794=CARTESIAN_POINT('Ctrl Pts',(-9.66605613200005,11.6,4.07291107899999));
#252795=CARTESIAN_POINT('Ctrl Pts',(-9.66768025600006,15.2,4.07328724699998));
#252796=CARTESIAN_POINT('Ctrl Pts',(-9.66768025600006,11.6,4.07328724699998));
#252797=CARTESIAN_POINT('Ctrl Pts',(-9.66931225600005,15.2,4.07366363599999));
#252798=CARTESIAN_POINT('Ctrl Pts',(-9.66931225600005,11.6,4.07366363599999));
#252799=CARTESIAN_POINT('Ctrl Pts',(-9.67095211400006,15.2,4.07404022799999));
#252800=CARTESIAN_POINT('Ctrl Pts',(-9.67095211400006,11.6,4.07404022799999));
#252801=CARTESIAN_POINT('Ctrl Pts',(-9.67259981800006,15.2,4.07441700699999));
#252802=CARTESIAN_POINT('Ctrl Pts',(-9.67259981800006,11.6,4.07441700699999));
#252803=CARTESIAN_POINT('Ctrl Pts',(-9.67425535200006,15.2,4.07479395599999));
#252804=CARTESIAN_POINT('Ctrl Pts',(-9.67425535200006,11.6,4.07479395599999));
#252805=CARTESIAN_POINT('Ctrl Pts',(-9.67591870200006,15.2,4.07517105799998));
#252806=CARTESIAN_POINT('Ctrl Pts',(-9.67591870200006,11.6,4.07517105799998));
#252807=CARTESIAN_POINT('Ctrl Pts',(-9.67758985300006,15.2,4.07554829499999));
#252808=CARTESIAN_POINT('Ctrl Pts',(-9.67758985300006,11.6,4.07554829499999));
#252809=CARTESIAN_POINT('Ctrl Pts',(-9.67926879200006,15.2,4.07592565399998));
#252810=CARTESIAN_POINT('Ctrl Pts',(-9.67926879200006,11.6,4.07592565399998));
#252811=CARTESIAN_POINT('Ctrl Pts',(-9.68095550300006,15.2,4.07630311599998));
#252812=CARTESIAN_POINT('Ctrl Pts',(-9.68095550300006,11.6,4.07630311599998));
#252813=CARTESIAN_POINT('Ctrl Pts',(-9.68264997200006,15.2,4.07668066399999));
#252814=CARTESIAN_POINT('Ctrl Pts',(-9.68264997200006,11.6,4.07668066399999));
#252815=CARTESIAN_POINT('Ctrl Pts',(-9.68435218600005,15.2,4.07705828399998));
#252816=CARTESIAN_POINT('Ctrl Pts',(-9.68435218600005,11.6,4.07705828399998));
#252817=CARTESIAN_POINT('Ctrl Pts',(-9.68606212900006,15.2,4.07743595699999));
#252818=CARTESIAN_POINT('Ctrl Pts',(-9.68606212900006,11.6,4.07743595699999));
#252819=CARTESIAN_POINT('Ctrl Pts',(-9.68777978900006,15.2,4.07781366999998));
#252820=CARTESIAN_POINT('Ctrl Pts',(-9.68777978900006,11.6,4.07781366999998));
#252821=CARTESIAN_POINT('Ctrl Pts',(-9.68950515000006,15.2,4.07819140399998));
#252822=CARTESIAN_POINT('Ctrl Pts',(-9.68950515000006,11.6,4.07819140399998));
#252823=CARTESIAN_POINT('Ctrl Pts',(-9.69123819800006,15.2,4.07856914399999));
#252824=CARTESIAN_POINT('Ctrl Pts',(-9.69123819800006,11.6,4.07856914399999));
#252825=CARTESIAN_POINT('Ctrl Pts',(-9.69297892100006,15.2,4.07894687399998));
#252826=CARTESIAN_POINT('Ctrl Pts',(-9.69297892100006,11.6,4.07894687399998));
#252827=CARTESIAN_POINT('Ctrl Pts',(-9.69472730100006,15.2,4.07932457799999));
#252828=CARTESIAN_POINT('Ctrl Pts',(-9.69472730100006,11.6,4.07932457799998));
#252829=CARTESIAN_POINT('Ctrl Pts',(-9.69648332900006,15.2,4.07970223999998));
#252830=CARTESIAN_POINT('Ctrl Pts',(-9.69648332900006,11.6,4.07970223999998));
#252831=CARTESIAN_POINT('Ctrl Pts',(-9.69824698700006,15.2,4.08007984399998));
#252832=CARTESIAN_POINT('Ctrl Pts',(-9.69824698700006,11.6,4.08007984399998));
#252833=CARTESIAN_POINT('Ctrl Pts',(-9.70001826300006,15.2,4.08045737499998));
#252834=CARTESIAN_POINT('Ctrl Pts',(-9.70001826300006,11.6,4.08045737499998));
#252835=CARTESIAN_POINT('Ctrl Pts',(-9.70179714400006,15.2,4.08083481799999));
#252836=CARTESIAN_POINT('Ctrl Pts',(-9.70179714400006,11.6,4.08083481799998));
#252837=CARTESIAN_POINT('Ctrl Pts',(-9.70358361300006,15.2,4.08121215499998));
#252838=CARTESIAN_POINT('Ctrl Pts',(-9.70358361300006,11.6,4.08121215499998));
#252839=CARTESIAN_POINT('Ctrl Pts',(-9.70537765900006,15.2,4.08158937199998));
#252840=CARTESIAN_POINT('Ctrl Pts',(-9.70537765900006,11.6,4.08158937199998));
#252841=CARTESIAN_POINT('Ctrl Pts',(-9.70717926800006,15.2,4.08196645299999));
#252842=CARTESIAN_POINT('Ctrl Pts',(-9.70717926800006,11.6,4.08196645299998));
#252843=CARTESIAN_POINT('Ctrl Pts',(-9.70898842600005,15.2,4.08234338299999));
#252844=CARTESIAN_POINT('Ctrl Pts',(-9.70898842600005,11.6,4.08234338299999));
#252845=CARTESIAN_POINT('Ctrl Pts',(-9.71080511900006,15.2,4.08272014699998));
#252846=CARTESIAN_POINT('Ctrl Pts',(-9.71080511900006,11.6,4.08272014699998));
#252847=CARTESIAN_POINT('Ctrl Pts',(-9.71262933300006,15.2,4.08309672899998));
#252848=CARTESIAN_POINT('Ctrl Pts',(-9.71262933300006,11.6,4.08309672899998));
#252849=CARTESIAN_POINT('Ctrl Pts',(-9.71446105500006,15.2,4.08347311399999));
#252850=CARTESIAN_POINT('Ctrl Pts',(-9.71446105500006,11.6,4.08347311399999));
#252851=CARTESIAN_POINT('Ctrl Pts',(-9.71630027200005,15.2,4.08384928499999));
#252852=CARTESIAN_POINT('Ctrl Pts',(-9.71630027200005,11.6,4.08384928499998));
#252853=CARTESIAN_POINT('Ctrl Pts',(-9.71814696900006,15.2,4.08422523099999));
#252854=CARTESIAN_POINT('Ctrl Pts',(-9.71814696900006,11.6,4.08422523099999));
#252855=CARTESIAN_POINT('Ctrl Pts',(-9.72000113500006,15.2,4.08460093399999));
#252856=CARTESIAN_POINT('Ctrl Pts',(-9.72000113500006,11.6,4.08460093399999));
#252857=CARTESIAN_POINT('Ctrl Pts',(-9.72186275500006,15.2,4.08497637899998));
#252858=CARTESIAN_POINT('Ctrl Pts',(-9.72186275500006,11.6,4.08497637899998));
#252859=CARTESIAN_POINT('Ctrl Pts',(-9.72373181400006,15.2,4.08535155199999));
#252860=CARTESIAN_POINT('Ctrl Pts',(-9.72373181400006,11.6,4.08535155199999));
#252861=CARTESIAN_POINT('Ctrl Pts',(-9.72560830200005,15.2,4.08572643799998));
#252862=CARTESIAN_POINT('Ctrl Pts',(-9.72560830200005,11.6,4.08572643799998));
#252863=CARTESIAN_POINT('Ctrl Pts',(-9.72749220300006,15.2,4.08610102199999));
#252864=CARTESIAN_POINT('Ctrl Pts',(-9.72749220300006,11.6,4.08610102199999));
#252865=CARTESIAN_POINT('Ctrl Pts',(-9.72938350600005,15.2,4.08647528899999));
#252866=CARTESIAN_POINT('Ctrl Pts',(-9.72938350600005,11.6,4.08647528899999));
#252867=CARTESIAN_POINT('Ctrl Pts',(-9.73128219600006,15.2,4.08684922499998));
#252868=CARTESIAN_POINT('Ctrl Pts',(-9.73128219600006,11.6,4.08684922499998));
#252869=CARTESIAN_POINT('Ctrl Pts',(-9.73318826000006,15.2,4.08722281399999));
#252870=CARTESIAN_POINT('Ctrl Pts',(-9.73318826000006,11.6,4.08722281399999));
#252871=CARTESIAN_POINT('Ctrl Pts',(-9.73510168600006,15.2,4.08759604299998));
#252872=CARTESIAN_POINT('Ctrl Pts',(-9.73510168600006,11.6,4.08759604299998));
#252873=CARTESIAN_POINT('Ctrl Pts',(-9.73702246000006,15.2,4.08796889699998));
#252874=CARTESIAN_POINT('Ctrl Pts',(-9.73702246000006,11.6,4.08796889699998));
#252875=CARTESIAN_POINT('Ctrl Pts',(-9.73895056800006,15.2,4.08834136099999));
#252876=CARTESIAN_POINT('Ctrl Pts',(-9.73895056800006,11.6,4.08834136099998));
#252877=CARTESIAN_POINT('Ctrl Pts',(-9.74088599900006,15.2,4.08871342199999));
#252878=CARTESIAN_POINT('Ctrl Pts',(-9.74088599900006,11.6,4.08871342199998));
#252879=CARTESIAN_POINT('Ctrl Pts',(-9.74282873900006,15.2,4.08908506299999));
#252880=CARTESIAN_POINT('Ctrl Pts',(-9.74282873900006,11.6,4.08908506299999));
#252881=CARTESIAN_POINT('Ctrl Pts',(-9.74477877400006,15.2,4.08945627299998));
#252882=CARTESIAN_POINT('Ctrl Pts',(-9.74477877400006,11.6,4.08945627299998));
#252883=CARTESIAN_POINT('Ctrl Pts',(-9.74673609300006,15.2,4.08982703499999));
#252884=CARTESIAN_POINT('Ctrl Pts',(-9.74673609300006,11.6,4.08982703499999));
#252885=CARTESIAN_POINT('Ctrl Pts',(-9.74870068200006,15.2,4.09019733599998));
#252886=CARTESIAN_POINT('Ctrl Pts',(-9.74870068200006,11.6,4.09019733599998));
#252887=CARTESIAN_POINT('Ctrl Pts',(-9.75067252800006,15.2,4.09056716199999));
#252888=CARTESIAN_POINT('Ctrl Pts',(-9.75067252800006,11.6,4.09056716199998));
#252889=CARTESIAN_POINT('Ctrl Pts',(-9.75265161800005,15.2,4.09093649899999));
#252890=CARTESIAN_POINT('Ctrl Pts',(-9.75265161800005,11.6,4.09093649899999));
#252891=CARTESIAN_POINT('Ctrl Pts',(-9.75463794100006,15.2,4.09130533199999));
#252892=CARTESIAN_POINT('Ctrl Pts',(-9.75463794100006,11.6,4.09130533199999));
#252893=CARTESIAN_POINT('Ctrl Pts',(-9.75663148100006,15.2,4.09167364799998));
#252894=CARTESIAN_POINT('Ctrl Pts',(-9.75663148100006,11.6,4.09167364799998));
#252895=CARTESIAN_POINT('Ctrl Pts',(-9.75863222800006,15.2,4.09204143399998));
#252896=CARTESIAN_POINT('Ctrl Pts',(-9.75863222800006,11.6,4.09204143399998));
#252897=CARTESIAN_POINT('Ctrl Pts',(-9.76064016800006,15.2,4.09240867399999));
#252898=CARTESIAN_POINT('Ctrl Pts',(-9.76064016800006,11.6,4.09240867399998));
#252899=CARTESIAN_POINT('Ctrl Pts',(-9.76265528900005,15.2,4.09277535599998));
#252900=CARTESIAN_POINT('Ctrl Pts',(-9.76265528900005,11.6,4.09277535599998));
#252901=CARTESIAN_POINT('Ctrl Pts',(-9.76467757800006,15.2,4.09314146399999));
#252902=CARTESIAN_POINT('Ctrl Pts',(-9.76467757800006,11.6,4.09314146399998));
#252903=CARTESIAN_POINT('Ctrl Pts',(-9.76670702300006,15.2,4.09350698699999));
#252904=CARTESIAN_POINT('Ctrl Pts',(-9.76670702300006,11.6,4.09350698699999));
#252905=CARTESIAN_POINT('Ctrl Pts',(-9.76874361000006,15.2,4.09387190999999));
#252906=CARTESIAN_POINT('Ctrl Pts',(-9.76874361000006,11.6,4.09387190999999));
#252907=CARTESIAN_POINT('Ctrl Pts',(-9.77078732700006,15.2,4.09423621999998));
#252908=CARTESIAN_POINT('Ctrl Pts',(-9.77078732700006,11.6,4.09423621999998));
#252909=CARTESIAN_POINT('Ctrl Pts',(-9.77283816300006,15.2,4.09459990199998));
#252910=CARTESIAN_POINT('Ctrl Pts',(-9.77283816300006,11.6,4.09459990199998));
#252911=CARTESIAN_POINT('Ctrl Pts',(-9.77489610300006,15.2,4.09496294399998));
#252912=CARTESIAN_POINT('Ctrl Pts',(-9.77489610300006,11.6,4.09496294399998));
#252913=CARTESIAN_POINT('Ctrl Pts',(-9.77696113600006,15.2,4.09532533299998));
#252914=CARTESIAN_POINT('Ctrl Pts',(-9.77696113600006,11.6,4.09532533299998));
#252915=CARTESIAN_POINT('Ctrl Pts',(-9.77903325100005,15.2,4.09568705499999));
#252916=CARTESIAN_POINT('Ctrl Pts',(-9.77903325100005,11.6,4.09568705499998));
#252917=CARTESIAN_POINT('Ctrl Pts',(-9.78111243200006,15.2,4.09604809499999));
#252918=CARTESIAN_POINT('Ctrl Pts',(-9.78111243200006,11.6,4.09604809499999));
#252919=CARTESIAN_POINT('Ctrl Pts',(-9.78319867100006,15.2,4.09640844199998));
#252920=CARTESIAN_POINT('Ctrl Pts',(-9.78319867100006,11.6,4.09640844199998));
#252921=CARTESIAN_POINT('Ctrl Pts',(-9.78529195100006,15.2,4.09676808199999));
#252922=CARTESIAN_POINT('Ctrl Pts',(-9.78529195100006,11.6,4.09676808199999));
#252923=CARTESIAN_POINT('Ctrl Pts',(-9.78739226300006,15.2,4.09712700199999));
#252924=CARTESIAN_POINT('Ctrl Pts',(-9.78739226300006,11.6,4.09712700199999));
#252925=CARTESIAN_POINT('Ctrl Pts',(-9.78949959500006,15.2,4.09748518799999));
#252926=CARTESIAN_POINT('Ctrl Pts',(-9.78949959500006,11.6,4.09748518799999));
#252927=CARTESIAN_POINT('Ctrl Pts',(-9.79161393300006,15.2,4.09784262799998));
#252928=CARTESIAN_POINT('Ctrl Pts',(-9.79161393300006,11.6,4.09784262799998));
#252929=CARTESIAN_POINT('Ctrl Pts',(-9.79373526500006,15.2,4.09819930899998));
#252930=CARTESIAN_POINT('Ctrl Pts',(-9.79373526500006,11.6,4.09819930899998));
#252931=CARTESIAN_POINT('Ctrl Pts',(-9.79586357800006,15.2,4.09855521699999));
#252932=CARTESIAN_POINT('Ctrl Pts',(-9.79586357800006,11.6,4.09855521699999));
#252933=CARTESIAN_POINT('Ctrl Pts',(-9.79799886300006,15.2,4.09891033999998));
#252934=CARTESIAN_POINT('Ctrl Pts',(-9.79799886300006,11.6,4.09891033999998));
#252935=CARTESIAN_POINT('Ctrl Pts',(-9.80014110600005,15.2,4.09926466599998));
#252936=CARTESIAN_POINT('Ctrl Pts',(-9.80014110600005,11.6,4.09926466599998));
#252937=CARTESIAN_POINT('Ctrl Pts',(-9.80229029300006,15.2,4.09961817999999));
#252938=CARTESIAN_POINT('Ctrl Pts',(-9.80229029300006,11.6,4.09961817999999));
#252939=CARTESIAN_POINT('Ctrl Pts',(-9.80444641500006,15.2,4.09997086899998));
#252940=CARTESIAN_POINT('Ctrl Pts',(-9.80444641500006,11.6,4.09997086899998));
#252941=CARTESIAN_POINT('Ctrl Pts',(-9.80660945900006,15.2,4.10032272299999));
#252942=CARTESIAN_POINT('Ctrl Pts',(-9.80660945900006,11.6,4.10032272299999));
#252943=CARTESIAN_POINT('Ctrl Pts',(-9.80877941300006,15.2,4.10067372699999));
#252944=CARTESIAN_POINT('Ctrl Pts',(-9.80877941300006,11.6,4.10067372699999));
#252945=CARTESIAN_POINT('Ctrl Pts',(-9.81095626400006,15.2,4.10102386999998));
#252946=CARTESIAN_POINT('Ctrl Pts',(-9.81095626400006,11.6,4.10102386999998));
#252947=CARTESIAN_POINT('Ctrl Pts',(-9.81314000100006,15.2,4.10137313799999));
#252948=CARTESIAN_POINT('Ctrl Pts',(-9.81314000100006,11.6,4.10137313799999));
#252949=CARTESIAN_POINT('Ctrl Pts',(-9.81533061200006,15.2,4.10172151899998));
#252950=CARTESIAN_POINT('Ctrl Pts',(-9.81533061200006,11.6,4.10172151899998));
#252951=CARTESIAN_POINT('Ctrl Pts',(-9.81752808600006,15.2,4.10206899999999));
#252952=CARTESIAN_POINT('Ctrl Pts',(-9.81752808600006,11.6,4.10206899999999));
#252953=CARTESIAN_POINT('Ctrl Pts',(-9.81973240800006,15.2,4.10241556999999));
#252954=CARTESIAN_POINT('Ctrl Pts',(-9.81973240800006,11.6,4.10241556999999));
#252955=CARTESIAN_POINT('Ctrl Pts',(-9.82194357100006,15.2,4.10276121599999));
#252956=CARTESIAN_POINT('Ctrl Pts',(-9.82194357100006,11.6,4.10276121599999));
#252957=CARTESIAN_POINT('Ctrl Pts',(-9.82416156000006,15.2,4.10310592499999));
#252958=CARTESIAN_POINT('Ctrl Pts',(-9.82416156000006,11.6,4.10310592499999));
#252959=CARTESIAN_POINT('Ctrl Pts',(-9.82638636300005,15.2,4.10344968399999));
#252960=CARTESIAN_POINT('Ctrl Pts',(-9.82638636300005,11.6,4.10344968399999));
#252961=CARTESIAN_POINT('Ctrl Pts',(-9.82861797000006,15.2,4.10379248299999));
#252962=CARTESIAN_POINT('Ctrl Pts',(-9.82861797000006,11.6,4.10379248299999));
#252963=CARTESIAN_POINT('Ctrl Pts',(-9.83085636800006,15.2,4.10413430699998));
#252964=CARTESIAN_POINT('Ctrl Pts',(-9.83085636800006,11.6,4.10413430699998));
#252965=CARTESIAN_POINT('Ctrl Pts',(-9.83310154600006,15.2,4.10447514799999));
#252966=CARTESIAN_POINT('Ctrl Pts',(-9.83310154600006,11.6,4.10447514799999));
#252967=CARTESIAN_POINT('Ctrl Pts',(-9.83535349200006,15.2,4.10481498899999));
#252968=CARTESIAN_POINT('Ctrl Pts',(-9.83535349200006,11.6,4.10481498899998));
#252969=CARTESIAN_POINT('Ctrl Pts',(-9.83761219400006,15.2,4.10515382099998));
#252970=CARTESIAN_POINT('Ctrl Pts',(-9.83761219400006,11.6,4.10515382099998));
#252971=CARTESIAN_POINT('Ctrl Pts',(-9.83987764100006,15.2,4.10549162999998));
#252972=CARTESIAN_POINT('Ctrl Pts',(-9.83987764100006,11.6,4.10549162999998));
#252973=CARTESIAN_POINT('Ctrl Pts',(-9.84214982200006,15.2,4.10582840699998));
#252974=CARTESIAN_POINT('Ctrl Pts',(-9.84214982200006,11.6,4.10582840699998));
#252975=CARTESIAN_POINT('Ctrl Pts',(-9.84442872400006,15.2,4.10616413599998));
#252976=CARTESIAN_POINT('Ctrl Pts',(-9.84442872400006,11.6,4.10616413599998));
#252977=CARTESIAN_POINT('Ctrl Pts',(-9.84671433600005,15.2,4.10649880899999));
#252978=CARTESIAN_POINT('Ctrl Pts',(-9.84671433600005,11.6,4.10649880899999));
#252979=CARTESIAN_POINT('Ctrl Pts',(-9.84900664700006,15.2,4.10683241099999));
#252980=CARTESIAN_POINT('Ctrl Pts',(-9.84900664700006,11.6,4.10683241099999));
#252981=CARTESIAN_POINT('Ctrl Pts',(-9.85130564400006,15.2,4.10716493199998));
#252982=CARTESIAN_POINT('Ctrl Pts',(-9.85130564400006,11.6,4.10716493199998));
#252983=CARTESIAN_POINT('Ctrl Pts',(-9.85361131800006,15.2,4.10749635999998));
#252984=CARTESIAN_POINT('Ctrl Pts',(-9.85361131800006,11.6,4.10749635999998));
#252985=CARTESIAN_POINT('Ctrl Pts',(-9.85592365600005,15.2,4.10782668199998));
#252986=CARTESIAN_POINT('Ctrl Pts',(-9.85592365600005,11.6,4.10782668199998));
#252987=CARTESIAN_POINT('Ctrl Pts',(-9.85824264700006,15.2,4.10815588899998));
#252988=CARTESIAN_POINT('Ctrl Pts',(-9.85824264700006,11.6,4.10815588899998));
#252989=CARTESIAN_POINT('Ctrl Pts',(-9.86056828000006,15.2,4.10848396699999));
#252990=CARTESIAN_POINT('Ctrl Pts',(-9.86056828000006,11.6,4.10848396699999));
#252991=CARTESIAN_POINT('Ctrl Pts',(-9.86290054200006,15.2,4.10881090399998));
#252992=CARTESIAN_POINT('Ctrl Pts',(-9.86290054200006,11.6,4.10881090399998));
#252993=CARTESIAN_POINT('Ctrl Pts',(-9.86523942400006,15.2,4.10913668999999));
#252994=CARTESIAN_POINT('Ctrl Pts',(-9.86523942400006,11.6,4.10913668999999));
#252995=CARTESIAN_POINT('Ctrl Pts',(-9.86758491300006,15.2,4.10946131299998));
#252996=CARTESIAN_POINT('Ctrl Pts',(-9.86758491300006,11.6,4.10946131299998));
#252997=CARTESIAN_POINT('Ctrl Pts',(-9.86993699900006,15.2,4.10978476199999));
#252998=CARTESIAN_POINT('Ctrl Pts',(-9.86993699900006,11.6,4.10978476199999));
#252999=CARTESIAN_POINT('Ctrl Pts',(-9.87229566900006,15.2,4.11010702399999));
#253000=CARTESIAN_POINT('Ctrl Pts',(-9.87229566900006,11.6,4.11010702399999));
#253001=CARTESIAN_POINT('Ctrl Pts',(-9.87466091400006,15.2,4.11042808899998));
#253002=CARTESIAN_POINT('Ctrl Pts',(-9.87466091400006,11.6,4.11042808899998));
#253003=CARTESIAN_POINT('Ctrl Pts',(-9.87703272000006,15.2,4.11074794499999));
#253004=CARTESIAN_POINT('Ctrl Pts',(-9.87703272000006,11.6,4.11074794499999));
#253005=CARTESIAN_POINT('Ctrl Pts',(-9.87941107900006,15.2,4.11106658099998));
#253006=CARTESIAN_POINT('Ctrl Pts',(-9.87941107900006,11.6,4.11106658099998));
#253007=CARTESIAN_POINT('Ctrl Pts',(-9.88179597700006,15.2,4.11138398499999));
#253008=CARTESIAN_POINT('Ctrl Pts',(-9.88179597700006,11.6,4.11138398499998));
#253009=CARTESIAN_POINT('Ctrl Pts',(-9.88418740600006,15.2,4.11170014699999));
#253010=CARTESIAN_POINT('Ctrl Pts',(-9.88418740600006,11.6,4.11170014699999));
#253011=CARTESIAN_POINT('Ctrl Pts',(-9.88658535100006,15.2,4.11201505499999));
#253012=CARTESIAN_POINT('Ctrl Pts',(-9.88658535100006,11.6,4.11201505499999));
#253013=CARTESIAN_POINT('Ctrl Pts',(-9.88898980500006,15.2,4.11232869699998));
#253014=CARTESIAN_POINT('Ctrl Pts',(-9.88898980500006,11.6,4.11232869699998));
#253015=CARTESIAN_POINT('Ctrl Pts',(-9.89140075400006,15.2,4.11264106399998));
#253016=CARTESIAN_POINT('Ctrl Pts',(-9.89140075400006,11.6,4.11264106399998));
#253017=CARTESIAN_POINT('Ctrl Pts',(-9.89381818800006,15.2,4.11295214299999));
#253018=CARTESIAN_POINT('Ctrl Pts',(-9.89381818800006,11.6,4.11295214299999));
#253019=CARTESIAN_POINT('Ctrl Pts',(-9.89624209600005,15.2,4.11326192399999));
#253020=CARTESIAN_POINT('Ctrl Pts',(-9.89624209600005,11.6,4.11326192399999));
#253021=CARTESIAN_POINT('Ctrl Pts',(-9.89867246700006,15.2,4.11357039599999));
#253022=CARTESIAN_POINT('Ctrl Pts',(-9.89867246700006,11.6,4.11357039599998));
#253023=CARTESIAN_POINT('Ctrl Pts',(-9.90110928900006,15.2,4.11387754799998));
#253024=CARTESIAN_POINT('Ctrl Pts',(-9.90110928900006,11.6,4.11387754799998));
#253025=CARTESIAN_POINT('Ctrl Pts',(-9.90355255300006,15.2,4.11418336699998));
#253026=CARTESIAN_POINT('Ctrl Pts',(-9.90355255300006,11.6,4.11418336699998));
#253027=CARTESIAN_POINT('Ctrl Pts',(-9.90600224700006,15.2,4.11448784599998));
#253028=CARTESIAN_POINT('Ctrl Pts',(-9.90600224700006,11.6,4.11448784599998));
#253029=CARTESIAN_POINT('Ctrl Pts',(-9.90845836000006,15.2,4.11479096999999));
#253030=CARTESIAN_POINT('Ctrl Pts',(-9.90845836000006,11.6,4.11479096999999));
#253031=CARTESIAN_POINT('Ctrl Pts',(-9.91092088200006,15.2,4.11509273099998));
#253032=CARTESIAN_POINT('Ctrl Pts',(-9.91092088200006,11.6,4.11509273099998));
#253033=CARTESIAN_POINT('Ctrl Pts',(-9.91338980100006,15.2,4.11539311699999));
#253034=CARTESIAN_POINT('Ctrl Pts',(-9.91338980100006,11.6,4.11539311699998));
#253035=CARTESIAN_POINT('Ctrl Pts',(-9.91586510700006,15.2,4.11569211899998));
#253036=CARTESIAN_POINT('Ctrl Pts',(-9.91586510700006,11.6,4.11569211899998));
#253037=CARTESIAN_POINT('Ctrl Pts',(-9.91834678800006,15.2,4.11598972399998));
#253038=CARTESIAN_POINT('Ctrl Pts',(-9.91834678800006,11.6,4.11598972399998));
#253039=CARTESIAN_POINT('Ctrl Pts',(-9.92083483500006,15.2,4.11628592099999));
#253040=CARTESIAN_POINT('Ctrl Pts',(-9.92083483500006,11.6,4.11628592099999));
#253041=CARTESIAN_POINT('Ctrl Pts',(-9.92332923600006,15.2,4.11658070199999));
#253042=CARTESIAN_POINT('Ctrl Pts',(-9.92332923600006,11.6,4.11658070199999));
#253043=CARTESIAN_POINT('Ctrl Pts',(-9.92582998100006,15.2,4.11687405499999));
#253044=CARTESIAN_POINT('Ctrl Pts',(-9.92582998100006,11.6,4.11687405499999));
#253045=CARTESIAN_POINT('Ctrl Pts',(-9.92833705900006,15.2,4.11716596899999));
#253046=CARTESIAN_POINT('Ctrl Pts',(-9.92833705900006,11.6,4.11716596899998));
#253047=CARTESIAN_POINT('Ctrl Pts',(-9.93085045900006,15.2,4.11745643499999));
#253048=CARTESIAN_POINT('Ctrl Pts',(-9.93085045900006,11.6,4.11745643499999));
#253049=CARTESIAN_POINT('Ctrl Pts',(-9.93337017000006,15.2,4.11774543999999));
#253050=CARTESIAN_POINT('Ctrl Pts',(-9.93337017000006,11.6,4.11774543999999));
#253051=CARTESIAN_POINT('Ctrl Pts',(-9.93589618200006,15.2,4.11803297499999));
#253052=CARTESIAN_POINT('Ctrl Pts',(-9.93589618200006,11.6,4.11803297499999));
#253053=CARTESIAN_POINT('Ctrl Pts',(-9.93842848600006,15.2,4.11831903099999));
#253054=CARTESIAN_POINT('Ctrl Pts',(-9.93842848600006,11.6,4.11831903099999));
#253055=CARTESIAN_POINT('Ctrl Pts',(-9.94096706800006,15.2,4.11860359499999));
#253056=CARTESIAN_POINT('Ctrl Pts',(-9.94096706800006,11.6,4.11860359499998));
#253057=CARTESIAN_POINT('Ctrl Pts',(-9.94351191900006,15.2,4.11888665699998));
#253058=CARTESIAN_POINT('Ctrl Pts',(-9.94351191900006,11.6,4.11888665699998));
#253059=CARTESIAN_POINT('Ctrl Pts',(-9.94606302900005,15.2,4.11916820899999));
#253060=CARTESIAN_POINT('Ctrl Pts',(-9.94606302900005,11.6,4.11916820899999));
#253061=CARTESIAN_POINT('Ctrl Pts',(-9.94862038700006,15.2,4.11944823899999));
#253062=CARTESIAN_POINT('Ctrl Pts',(-9.94862038700006,11.6,4.11944823899999));
#253063=CARTESIAN_POINT('Ctrl Pts',(-9.95118398200006,15.2,4.11972673699999));
#253064=CARTESIAN_POINT('Ctrl Pts',(-9.95118398200006,11.6,4.11972673699999));
#253065=CARTESIAN_POINT('Ctrl Pts',(-9.95375380500005,15.2,4.12000369299999));
#253066=CARTESIAN_POINT('Ctrl Pts',(-9.95375380500005,11.6,4.12000369299999));
#253067=CARTESIAN_POINT('Ctrl Pts',(-9.95632984400006,15.2,4.12027909599999));
#253068=CARTESIAN_POINT('Ctrl Pts',(-9.95632984400006,11.6,4.12027909599998));
#253069=CARTESIAN_POINT('Ctrl Pts',(-9.95891208900006,15.2,4.12055293699999));
#253070=CARTESIAN_POINT('Ctrl Pts',(-9.95891208900006,11.6,4.12055293699999));
#253071=CARTESIAN_POINT('Ctrl Pts',(-9.96150052900006,15.2,4.12082520499998));
#253072=CARTESIAN_POINT('Ctrl Pts',(-9.96150052900006,11.6,4.12082520499998));
#253073=CARTESIAN_POINT('Ctrl Pts',(-9.96409515500006,15.2,4.12109588999999));
#253074=CARTESIAN_POINT('Ctrl Pts',(-9.96409515500006,11.6,4.12109588999999));
#253075=CARTESIAN_POINT('Ctrl Pts',(-9.96669595600006,15.2,4.12136498299999));
#253076=CARTESIAN_POINT('Ctrl Pts',(-9.96669595600006,11.6,4.12136498299999));
#253077=CARTESIAN_POINT('Ctrl Pts',(-9.96930292000006,15.2,4.12163247299999));
#253078=CARTESIAN_POINT('Ctrl Pts',(-9.96930292000006,11.6,4.12163247299999));
#253079=CARTESIAN_POINT('Ctrl Pts',(-9.97191603900006,15.2,4.12189835099999));
#253080=CARTESIAN_POINT('Ctrl Pts',(-9.97191603900006,11.6,4.12189835099999));
#253081=CARTESIAN_POINT('Ctrl Pts',(-9.97453530200006,15.2,4.12216260499999));
#253082=CARTESIAN_POINT('Ctrl Pts',(-9.97453530200006,11.6,4.12216260499999));
#253083=CARTESIAN_POINT('Ctrl Pts',(-9.97716069800006,15.2,4.12242522699999));
#253084=CARTESIAN_POINT('Ctrl Pts',(-9.97716069800006,11.6,4.12242522699999));
#253085=CARTESIAN_POINT('Ctrl Pts',(-9.97979221700006,15.2,4.12268620699999));
#253086=CARTESIAN_POINT('Ctrl Pts',(-9.97979221700006,11.6,4.12268620699999));
#253087=CARTESIAN_POINT('Ctrl Pts',(-9.98242984800006,15.2,4.12294553499999));
#253088=CARTESIAN_POINT('Ctrl Pts',(-9.98242984800006,11.6,4.12294553499999));
#253089=CARTESIAN_POINT('Ctrl Pts',(-9.98507358300006,15.2,4.12320320099998));
#253090=CARTESIAN_POINT('Ctrl Pts',(-9.98507358300006,11.6,4.12320320099998));
#253091=CARTESIAN_POINT('Ctrl Pts',(-9.98772341000006,15.2,4.12345919499998));
#253092=CARTESIAN_POINT('Ctrl Pts',(-9.98772341000006,11.6,4.12345919499998));
#253093=CARTESIAN_POINT('Ctrl Pts',(-9.99037931900006,15.2,4.12371350699999));
#253094=CARTESIAN_POINT('Ctrl Pts',(-9.99037931900006,11.6,4.12371350699999));
#253095=CARTESIAN_POINT('Ctrl Pts',(-9.99304129900005,15.2,4.12396612799999));
#253096=CARTESIAN_POINT('Ctrl Pts',(-9.99304129900005,11.6,4.12396612799998));
#253097=CARTESIAN_POINT('Ctrl Pts',(-9.99570934200005,15.2,4.12421704799999));
#253098=CARTESIAN_POINT('Ctrl Pts',(-9.99570934200005,11.6,4.12421704799998));
#253099=CARTESIAN_POINT('Ctrl Pts',(-9.99838343600005,15.2,4.12446625799999));
#253100=CARTESIAN_POINT('Ctrl Pts',(-9.99838343600005,11.6,4.12446625799998));
#253101=CARTESIAN_POINT('Ctrl Pts',(-10.0010635710001,15.2,4.12471374699999));
#253102=CARTESIAN_POINT('Ctrl Pts',(-10.0010635710001,11.6,4.12471374699999));
#253103=CARTESIAN_POINT('Ctrl Pts',(-10.0037497380001,15.2,4.12495950799999));
#253104=CARTESIAN_POINT('Ctrl Pts',(-10.0037497380001,11.6,4.12495950799998));
#253105=CARTESIAN_POINT('Ctrl Pts',(-10.0064419260001,15.2,4.12520352799999));
#253106=CARTESIAN_POINT('Ctrl Pts',(-10.0064419260001,11.6,4.12520352799999));
#253107=CARTESIAN_POINT('Ctrl Pts',(-10.0091401250001,15.2,4.12544580099999));
#253108=CARTESIAN_POINT('Ctrl Pts',(-10.0091401250001,11.6,4.12544580099999));
#253109=CARTESIAN_POINT('Ctrl Pts',(-10.0118443250001,15.2,4.12568631499998));
#253110=CARTESIAN_POINT('Ctrl Pts',(-10.0118443250001,11.6,4.12568631499998));
#253111=CARTESIAN_POINT('Ctrl Pts',(-10.0145545170001,15.2,4.12592506099998));
#253112=CARTESIAN_POINT('Ctrl Pts',(-10.0145545170001,11.6,4.12592506099998));
#253113=CARTESIAN_POINT('Ctrl Pts',(-10.0172706880001,15.2,4.12616202899999));
#253114=CARTESIAN_POINT('Ctrl Pts',(-10.0172706880001,11.6,4.12616202899999));
#253115=CARTESIAN_POINT('Ctrl Pts',(-10.0199928310001,15.2,4.12639721199999));
#253116=CARTESIAN_POINT('Ctrl Pts',(-10.0199928310001,11.6,4.12639721199999));
#253117=CARTESIAN_POINT('Ctrl Pts',(-10.0227209350001,15.2,4.12663059799999));
#253118=CARTESIAN_POINT('Ctrl Pts',(-10.0227209350001,11.6,4.12663059799998));
#253119=CARTESIAN_POINT('Ctrl Pts',(-10.0254549900001,15.2,4.12686217999998));
#253120=CARTESIAN_POINT('Ctrl Pts',(-10.0254549900001,11.6,4.12686217999998));
#253121=CARTESIAN_POINT('Ctrl Pts',(-10.0281949850001,15.2,4.12709194699998));
#253122=CARTESIAN_POINT('Ctrl Pts',(-10.0281949850001,11.6,4.12709194699998));
#253123=CARTESIAN_POINT('Ctrl Pts',(-10.0309409120001,15.2,4.12731989099999));
#253124=CARTESIAN_POINT('Ctrl Pts',(-10.0309409120001,11.6,4.12731989099999));
#253125=CARTESIAN_POINT('Ctrl Pts',(-10.0336927600001,15.2,4.12754600099999));
#253126=CARTESIAN_POINT('Ctrl Pts',(-10.0336927600001,11.6,4.12754600099999));
#253127=CARTESIAN_POINT('Ctrl Pts',(-10.0364505200001,15.2,4.12777026899998));
#253128=CARTESIAN_POINT('Ctrl Pts',(-10.0364505200001,11.6,4.12777026899998));
#253129=CARTESIAN_POINT('Ctrl Pts',(-10.0392141810001,15.2,4.12799268699998));
#253130=CARTESIAN_POINT('Ctrl Pts',(-10.0392141810001,11.6,4.12799268699998));
#253131=CARTESIAN_POINT('Ctrl Pts',(-10.0419837320001,15.2,4.12821324399999));
#253132=CARTESIAN_POINT('Ctrl Pts',(-10.0419837320001,11.6,4.12821324399999));
#253133=CARTESIAN_POINT('Ctrl Pts',(-10.0447591670001,15.2,4.12843193099998));
#253134=CARTESIAN_POINT('Ctrl Pts',(-10.0447591670001,11.6,4.12843193099998));
#253135=CARTESIAN_POINT('Ctrl Pts',(-10.0475404720001,15.2,4.12864873899998));
#253136=CARTESIAN_POINT('Ctrl Pts',(-10.0475404720001,11.6,4.12864873899998));
#253137=CARTESIAN_POINT('Ctrl Pts',(-10.0503276400001,15.2,4.12886365899999));
#253138=CARTESIAN_POINT('Ctrl Pts',(-10.0503276400001,11.6,4.12886365899999));
#253139=CARTESIAN_POINT('Ctrl Pts',(-10.0531206590001,15.2,4.12907668399999));
#253140=CARTESIAN_POINT('Ctrl Pts',(-10.0531206590001,11.6,4.12907668399999));
#253141=CARTESIAN_POINT('Ctrl Pts',(-10.0559195220001,15.2,4.12928780199999));
#253142=CARTESIAN_POINT('Ctrl Pts',(-10.0559195220001,11.6,4.12928780199999));
#253143=CARTESIAN_POINT('Ctrl Pts',(-10.0587242160001,15.2,4.12949700499999));
#253144=CARTESIAN_POINT('Ctrl Pts',(-10.0587242160001,11.6,4.12949700499999));
#253145=CARTESIAN_POINT('Ctrl Pts',(-10.0615347350001,15.2,4.12970428599999));
#253146=CARTESIAN_POINT('Ctrl Pts',(-10.0615347350001,11.6,4.12970428599999));
#253147=CARTESIAN_POINT('Ctrl Pts',(-10.0643510650001,15.2,4.12990963299999));
#253148=CARTESIAN_POINT('Ctrl Pts',(-10.0643510650001,11.6,4.12990963299999));
#253149=CARTESIAN_POINT('Ctrl Pts',(-10.0671731990001,15.2,4.13011303899999));
#253150=CARTESIAN_POINT('Ctrl Pts',(-10.0671731990001,11.6,4.13011303899999));
#253151=CARTESIAN_POINT('Ctrl Pts',(-10.0700011270001,15.2,4.13031449499999));
#253152=CARTESIAN_POINT('Ctrl Pts',(-10.0700011270001,11.6,4.13031449499999));
#253153=CARTESIAN_POINT('Ctrl Pts',(-10.0728348400001,15.2,4.13051399199999));
#253154=CARTESIAN_POINT('Ctrl Pts',(-10.0728348400001,11.6,4.13051399199999));
#253155=CARTESIAN_POINT('Ctrl Pts',(-10.0756743260001,15.2,4.13071152099998));
#253156=CARTESIAN_POINT('Ctrl Pts',(-10.0756743260001,11.6,4.13071152099998));
#253157=CARTESIAN_POINT('Ctrl Pts',(-10.0785195780001,15.2,4.13090707399999));
#253158=CARTESIAN_POINT('Ctrl Pts',(-10.0785195780001,11.6,4.13090707399998));
#253159=CARTESIAN_POINT('Ctrl Pts',(-10.0813705840001,15.2,4.13110064099998));
#253160=CARTESIAN_POINT('Ctrl Pts',(-10.0813705840001,11.6,4.13110064099998));
#253161=CARTESIAN_POINT('Ctrl Pts',(-10.0842273370001,15.2,4.13129221499998));
#253162=CARTESIAN_POINT('Ctrl Pts',(-10.0842273370001,11.6,4.13129221499998));
#253163=CARTESIAN_POINT('Ctrl Pts',(-10.0870898240001,15.2,4.13148178499998));
#253164=CARTESIAN_POINT('Ctrl Pts',(-10.0870898240001,11.6,4.13148178499998));
#253165=CARTESIAN_POINT('Ctrl Pts',(-10.0899580390001,15.2,4.13166934399998));
#253166=CARTESIAN_POINT('Ctrl Pts',(-10.0899580390001,11.6,4.13166934399998));
#253167=CARTESIAN_POINT('Ctrl Pts',(-10.0928319700001,15.2,4.13185488299998));
#253168=CARTESIAN_POINT('Ctrl Pts',(-10.0928319700001,11.6,4.13185488299998));
#253169=CARTESIAN_POINT('Ctrl Pts',(-10.0957116090001,15.2,4.13203839299998));
#253170=CARTESIAN_POINT('Ctrl Pts',(-10.0957116090001,11.6,4.13203839299998));
#253171=CARTESIAN_POINT('Ctrl Pts',(-10.0985969450001,15.2,4.13221986699998));
#253172=CARTESIAN_POINT('Ctrl Pts',(-10.0985969450001,11.6,4.13221986699998));
#253173=CARTESIAN_POINT('Ctrl Pts',(-10.1014879690001,15.2,4.13239929399998));
#253174=CARTESIAN_POINT('Ctrl Pts',(-10.1014879690001,11.6,4.13239929399998));
#253175=CARTESIAN_POINT('Ctrl Pts',(-10.1043846720001,15.2,4.13257666799999));
#253176=CARTESIAN_POINT('Ctrl Pts',(-10.1043846720001,11.6,4.13257666799998));
#253177=CARTESIAN_POINT('Ctrl Pts',(-10.1072870450001,15.2,4.13275197899999));
#253178=CARTESIAN_POINT('Ctrl Pts',(-10.1072870450001,11.6,4.13275197899999));
#253179=CARTESIAN_POINT('Ctrl Pts',(-10.1101950770001,15.2,4.13292521799999));
#253180=CARTESIAN_POINT('Ctrl Pts',(-10.1101950770001,11.6,4.13292521799998));
#253181=CARTESIAN_POINT('Ctrl Pts',(-10.1131087590001,15.2,4.13309637799999));
#253182=CARTESIAN_POINT('Ctrl Pts',(-10.1131087590001,11.6,4.13309637799998));
#253183=CARTESIAN_POINT('Ctrl Pts',(-10.1160280820001,15.2,4.13326544999999));
#253184=CARTESIAN_POINT('Ctrl Pts',(-10.1160280820001,11.6,4.13326544999998));
#253185=CARTESIAN_POINT('Ctrl Pts',(-10.1189530370001,15.2,4.13343242499998));
#253186=CARTESIAN_POINT('Ctrl Pts',(-10.1189530370001,11.6,4.13343242499998));
#253187=CARTESIAN_POINT('Ctrl Pts',(-10.1218836130001,15.2,4.13359729699999));
#253188=CARTESIAN_POINT('Ctrl Pts',(-10.1218836130001,11.6,4.13359729699999));
#253189=CARTESIAN_POINT('Ctrl Pts',(-10.1248198030001,15.2,4.13376005499998));
#253190=CARTESIAN_POINT('Ctrl Pts',(-10.1248198030001,11.6,4.13376005499998));
#253191=CARTESIAN_POINT('Ctrl Pts',(-10.1277615950001,15.2,4.13392069099999));
#253192=CARTESIAN_POINT('Ctrl Pts',(-10.1277615950001,11.6,4.13392069099999));
#253193=CARTESIAN_POINT('Ctrl Pts',(-10.1307089820001,15.2,4.13407919799998));
#253194=CARTESIAN_POINT('Ctrl Pts',(-10.1307089820001,11.6,4.13407919799998));
#253195=CARTESIAN_POINT('Ctrl Pts',(-10.1336619530001,15.2,4.13423556699998));
#253196=CARTESIAN_POINT('Ctrl Pts',(-10.1336619530001,11.6,4.13423556699998));
#253197=CARTESIAN_POINT('Ctrl Pts',(-10.1366205000001,15.2,4.13438978999999));
#253198=CARTESIAN_POINT('Ctrl Pts',(-10.1366205000001,11.6,4.13438978999999));
#253199=CARTESIAN_POINT('Ctrl Pts',(-10.1395846120001,15.2,4.13454185899998));
#253200=CARTESIAN_POINT('Ctrl Pts',(-10.1395846120001,11.6,4.13454185899998));
#253201=CARTESIAN_POINT('Ctrl Pts',(-10.1425542810001,15.2,4.13469176499999));
#253202=CARTESIAN_POINT('Ctrl Pts',(-10.1425542810001,11.6,4.13469176499999));
#253203=CARTESIAN_POINT('Ctrl Pts',(-10.1455294970001,15.2,4.13483949999998));
#253204=CARTESIAN_POINT('Ctrl Pts',(-10.1455294970001,11.6,4.13483949999998));
#253205=CARTESIAN_POINT('Ctrl Pts',(-10.1485102510001,15.2,4.13498505799998));
#253206=CARTESIAN_POINT('Ctrl Pts',(-10.1485102510001,11.6,4.13498505799998));
#253207=CARTESIAN_POINT('Ctrl Pts',(-10.1514965350001,15.2,4.13512842799998));
#253208=CARTESIAN_POINT('Ctrl Pts',(-10.1514965350001,11.6,4.13512842799998));
#253209=CARTESIAN_POINT('Ctrl Pts',(-10.1544883380001,15.2,4.13526960399999));
#253210=CARTESIAN_POINT('Ctrl Pts',(-10.1544883380001,11.6,4.13526960399999));
#253211=CARTESIAN_POINT('Ctrl Pts',(-10.1574856510001,15.2,4.13540857599998));
#253212=CARTESIAN_POINT('Ctrl Pts',(-10.1574856510001,11.6,4.13540857599998));
#253213=CARTESIAN_POINT('Ctrl Pts',(-10.1604884650001,15.2,4.13554533699998));
#253214=CARTESIAN_POINT('Ctrl Pts',(-10.1604884650001,11.6,4.13554533699998));
#253215=CARTESIAN_POINT('Ctrl Pts',(-10.1634967710001,15.2,4.13567987999999));
#253216=CARTESIAN_POINT('Ctrl Pts',(-10.1634967710001,11.6,4.13567987999999));
#253217=CARTESIAN_POINT('Ctrl Pts',(-10.1665105610001,15.2,4.13581219599998));
#253218=CARTESIAN_POINT('Ctrl Pts',(-10.1665105610001,11.6,4.13581219599998));
#253219=CARTESIAN_POINT('Ctrl Pts',(-10.1695298240001,15.2,4.13594227699999));
#253220=CARTESIAN_POINT('Ctrl Pts',(-10.1695298240001,11.6,4.13594227699999));
#253221=CARTESIAN_POINT('Ctrl Pts',(-10.1725545500001,15.2,4.13607011499998));
#253222=CARTESIAN_POINT('Ctrl Pts',(-10.1725545500001,11.6,4.13607011499998));
#253223=CARTESIAN_POINT('Ctrl Pts',(-10.1755847340001,15.2,4.13619570299999));
#253224=CARTESIAN_POINT('Ctrl Pts',(-10.1755847340001,11.6,4.13619570299998));
#253225=CARTESIAN_POINT('Ctrl Pts',(-10.1786203620001,15.2,4.13631903199998));
#253226=CARTESIAN_POINT('Ctrl Pts',(-10.1786203620001,11.6,4.13631903199998));
#253227=CARTESIAN_POINT('Ctrl Pts',(-10.1816614280001,15.2,4.13644009499999));
#253228=CARTESIAN_POINT('Ctrl Pts',(-10.1816614280001,11.6,4.13644009499999));
#253229=CARTESIAN_POINT('Ctrl Pts',(-10.1847079220001,15.2,4.13655888299999));
#253230=CARTESIAN_POINT('Ctrl Pts',(-10.1847079220001,11.6,4.13655888299999));
#253231=CARTESIAN_POINT('Ctrl Pts',(-10.1877598350001,15.2,4.13667538999999));
#253232=CARTESIAN_POINT('Ctrl Pts',(-10.1877598350001,11.6,4.13667538999999));
#253233=CARTESIAN_POINT('Ctrl Pts',(-10.1908171570001,15.2,4.13678960699999));
#253234=CARTESIAN_POINT('Ctrl Pts',(-10.1908171570001,11.6,4.13678960699999));
#253235=CARTESIAN_POINT('Ctrl Pts',(-10.1938798810001,15.2,4.13690152799998));
#253236=CARTESIAN_POINT('Ctrl Pts',(-10.1938798810001,11.6,4.13690152799998));
#253237=CARTESIAN_POINT('Ctrl Pts',(-10.1969479960001,15.2,4.13701114199998));
#253238=CARTESIAN_POINT('Ctrl Pts',(-10.1969479960001,11.6,4.13701114199998));
#253239=CARTESIAN_POINT('Ctrl Pts',(-10.2000214950001,15.2,4.13711844399998));
#253240=CARTESIAN_POINT('Ctrl Pts',(-10.2000214950001,11.6,4.13711844399998));
#253241=CARTESIAN_POINT('Ctrl Pts',(-10.2031003670001,15.2,4.13722342499998));
#253242=CARTESIAN_POINT('Ctrl Pts',(-10.2031003670001,11.6,4.13722342499998));
#253243=CARTESIAN_POINT('Ctrl Pts',(-10.2061846030001,15.2,4.13732607699998));
#253244=CARTESIAN_POINT('Ctrl Pts',(-10.2061846030001,11.6,4.13732607699998));
#253245=CARTESIAN_POINT('Ctrl Pts',(-10.2092741960001,15.2,4.13742639399998));
#253246=CARTESIAN_POINT('Ctrl Pts',(-10.2092741960001,11.6,4.13742639399998));
#253247=CARTESIAN_POINT('Ctrl Pts',(-10.2123691360001,15.2,4.13752436799999));
#253248=CARTESIAN_POINT('Ctrl Pts',(-10.2123691360001,11.6,4.13752436799999));
#253249=CARTESIAN_POINT('Ctrl Pts',(-10.2154694120001,15.2,4.13761999099999));
#253250=CARTESIAN_POINT('Ctrl Pts',(-10.2154694120001,11.6,4.13761999099999));
#253251=CARTESIAN_POINT('Ctrl Pts',(-10.2185750180001,15.2,4.13771325499999));
#253252=CARTESIAN_POINT('Ctrl Pts',(-10.2185750180001,11.6,4.13771325499999));
#253253=CARTESIAN_POINT('Ctrl Pts',(-10.2216859440001,15.2,4.13780415299998));
#253254=CARTESIAN_POINT('Ctrl Pts',(-10.2216859440001,11.6,4.13780415299998));
#253255=CARTESIAN_POINT('Ctrl Pts',(-10.2248021810001,15.2,4.13789267699999));
#253256=CARTESIAN_POINT('Ctrl Pts',(-10.2248021810001,11.6,4.13789267699998));
#253257=CARTESIAN_POINT('Ctrl Pts',(-10.2279237210001,15.2,4.13797881999999));
#253258=CARTESIAN_POINT('Ctrl Pts',(-10.2279237210001,11.6,4.13797881999999));
#253259=CARTESIAN_POINT('Ctrl Pts',(-10.2310505530001,15.2,4.13806257599998));
#253260=CARTESIAN_POINT('Ctrl Pts',(-10.2310505530001,11.6,4.13806257599998));
#253261=CARTESIAN_POINT('Ctrl Pts',(-10.2341826700001,15.2,4.13814393399999));
#253262=CARTESIAN_POINT('Ctrl Pts',(-10.2341826700001,11.6,4.13814393399999));
#253263=CARTESIAN_POINT('Ctrl Pts',(-10.2373200620001,15.2,4.13822288999998));
#253264=CARTESIAN_POINT('Ctrl Pts',(-10.2373200620001,11.6,4.13822288999998));
#253265=CARTESIAN_POINT('Ctrl Pts',(-10.2404627220001,15.2,4.13829943499999));
#253266=CARTESIAN_POINT('Ctrl Pts',(-10.2404627220001,11.6,4.13829943499999));
#253267=CARTESIAN_POINT('Ctrl Pts',(-10.2436106390001,15.2,4.13837356099998));
#253268=CARTESIAN_POINT('Ctrl Pts',(-10.2436106390001,11.6,4.13837356099998));
#253269=CARTESIAN_POINT('Ctrl Pts',(-10.2467638050001,15.2,4.13844526199998));
#253270=CARTESIAN_POINT('Ctrl Pts',(-10.2467638050001,11.6,4.13844526199998));
#253271=CARTESIAN_POINT('Ctrl Pts',(-10.2499222120001,15.2,4.13851453099999));
#253272=CARTESIAN_POINT('Ctrl Pts',(-10.2499222120001,11.6,4.13851453099999));
#253273=CARTESIAN_POINT('Ctrl Pts',(-10.2530858490001,15.2,4.13858135799998));
#253274=CARTESIAN_POINT('Ctrl Pts',(-10.2530858490001,11.6,4.13858135799998));
#253275=CARTESIAN_POINT('Ctrl Pts',(-10.2562547100001,15.2,4.13864573899998));
#253276=CARTESIAN_POINT('Ctrl Pts',(-10.2562547100001,11.6,4.13864573899998));
#253277=CARTESIAN_POINT('Ctrl Pts',(-10.2594287840001,15.2,4.13870766499999));
#253278=CARTESIAN_POINT('Ctrl Pts',(-10.2594287840001,11.6,4.13870766499999));
#253279=CARTESIAN_POINT('Ctrl Pts',(-10.2626080630001,15.2,4.13876712999999));
#253280=CARTESIAN_POINT('Ctrl Pts',(-10.2626080630001,11.6,4.13876712999999));
#253281=CARTESIAN_POINT('Ctrl Pts',(-10.2657925390001,15.2,4.13882412399998));
#253282=CARTESIAN_POINT('Ctrl Pts',(-10.2657925390001,11.6,4.13882412399998));
#253283=CARTESIAN_POINT('Ctrl Pts',(-10.2689822020001,15.2,4.13887864299999));
#253284=CARTESIAN_POINT('Ctrl Pts',(-10.2689822020001,11.6,4.13887864299998));
#253285=CARTESIAN_POINT('Ctrl Pts',(-10.2721770450001,15.2,4.13893067799999));
#253286=CARTESIAN_POINT('Ctrl Pts',(-10.2721770450001,11.6,4.13893067799999));
#253287=CARTESIAN_POINT('Ctrl Pts',(-10.2753770580001,15.2,4.13898022199999));
#253288=CARTESIAN_POINT('Ctrl Pts',(-10.2753770580001,11.6,4.13898022199999));
#253289=CARTESIAN_POINT('Ctrl Pts',(-10.2785822320001,15.2,4.13902726899998));
#253290=CARTESIAN_POINT('Ctrl Pts',(-10.2785822320001,11.6,4.13902726899998));
#253291=CARTESIAN_POINT('Ctrl Pts',(-10.2817925600001,15.2,4.13907181099999));
#253292=CARTESIAN_POINT('Ctrl Pts',(-10.2817925600001,11.6,4.13907181099999));
#253293=CARTESIAN_POINT('Ctrl Pts',(-10.2850080310001,15.2,4.13911384099999));
#253294=CARTESIAN_POINT('Ctrl Pts',(-10.2850080310001,11.6,4.13911384099999));
#253295=CARTESIAN_POINT('Ctrl Pts',(-10.2882286380001,15.2,4.13915335199999));
#253296=CARTESIAN_POINT('Ctrl Pts',(-10.2882286380001,11.6,4.13915335199999));
#253297=CARTESIAN_POINT('Ctrl Pts',(-10.2914543720001,15.2,4.13919033599999));
#253298=CARTESIAN_POINT('Ctrl Pts',(-10.2914543720001,11.6,4.13919033599999));
#253299=CARTESIAN_POINT('Ctrl Pts',(-10.2946852240001,15.2,4.13922478899998));
#253300=CARTESIAN_POINT('Ctrl Pts',(-10.2946852240001,11.6,4.13922478899998));
#253301=CARTESIAN_POINT('Ctrl Pts',(-10.2979211850001,15.2,4.13925669999998));
#253302=CARTESIAN_POINT('Ctrl Pts',(-10.2979211850001,11.6,4.13925669999998));
#253303=CARTESIAN_POINT('Ctrl Pts',(-10.3011622480001,15.2,4.13928606399999));
#253304=CARTESIAN_POINT('Ctrl Pts',(-10.3011622480001,11.6,4.13928606399998));
#253305=CARTESIAN_POINT('Ctrl Pts',(-10.3044084030001,15.2,4.13931287499998));
#253306=CARTESIAN_POINT('Ctrl Pts',(-10.3044084030001,11.6,4.13931287499998));
#253307=CARTESIAN_POINT('Ctrl Pts',(-10.3076596430001,15.2,4.13933712499999));
#253308=CARTESIAN_POINT('Ctrl Pts',(-10.3076596430001,11.6,4.13933712499999));
#253309=CARTESIAN_POINT('Ctrl Pts',(-10.3109159570001,15.2,4.13935880599999));
#253310=CARTESIAN_POINT('Ctrl Pts',(-10.3109159570001,11.6,4.13935880599999));
#253311=CARTESIAN_POINT('Ctrl Pts',(-10.3141773370001,15.2,4.13937791399999));
#253312=CARTESIAN_POINT('Ctrl Pts',(-10.3141773370001,11.6,4.13937791399999));
#253313=CARTESIAN_POINT('Ctrl Pts',(-10.3174437770001,15.2,4.13939443899999));
#253314=CARTESIAN_POINT('Ctrl Pts',(-10.3174437770001,11.6,4.13939443899999));
#253315=CARTESIAN_POINT('Ctrl Pts',(-10.3207152650001,15.2,4.13940837599998));
#253316=CARTESIAN_POINT('Ctrl Pts',(-10.3207152650001,11.6,4.13940837599998));
#253317=CARTESIAN_POINT('Ctrl Pts',(-10.3239917950001,15.2,4.13941971799999));
#253318=CARTESIAN_POINT('Ctrl Pts',(-10.3239917950001,11.6,4.13941971799998));
#253319=CARTESIAN_POINT('Ctrl Pts',(-10.3272733590001,15.2,4.13942845699999));
#253320=CARTESIAN_POINT('Ctrl Pts',(-10.3272733590001,11.6,4.13942845699999));
#253321=CARTESIAN_POINT('Ctrl Pts',(-10.3305599450001,15.2,4.13943458699999));
#253322=CARTESIAN_POINT('Ctrl Pts',(-10.3305599450001,11.6,4.13943458699999));
#253323=CARTESIAN_POINT('Ctrl Pts',(-10.3338515480001,15.2,4.13943810199999));
#253324=CARTESIAN_POINT('Ctrl Pts',(-10.3338515480001,11.6,4.13943810199999));
#253325=CARTESIAN_POINT('Ctrl Pts',(-10.3371481570001,15.2,4.13943899399998));
#253326=CARTESIAN_POINT('Ctrl Pts',(-10.3371481570001,11.6,4.13943899399998));
#253327=CARTESIAN_POINT('Ctrl Pts',(-10.3404497650001,15.2,4.13943725699998));
#253328=CARTESIAN_POINT('Ctrl Pts',(-10.3404497650001,11.6,4.13943725699998));
#253329=CARTESIAN_POINT('Ctrl Pts',(-10.3437563640001,15.2,4.13943288499999));
#253330=CARTESIAN_POINT('Ctrl Pts',(-10.3437563640001,11.6,4.13943288499999));
#253331=CARTESIAN_POINT('Ctrl Pts',(-10.3470679440001,15.2,4.13942586999998));
#253332=CARTESIAN_POINT('Ctrl Pts',(-10.3470679440001,11.6,4.13942586999998));
#253333=CARTESIAN_POINT('Ctrl Pts',(-10.3503844980001,15.2,4.13941620499998));
#253334=CARTESIAN_POINT('Ctrl Pts',(-10.3503844980001,11.6,4.13941620499998));
#253335=CARTESIAN_POINT('Ctrl Pts',(-10.3537060160001,15.2,4.13940388499999));
#253336=CARTESIAN_POINT('Ctrl Pts',(-10.3537060160001,11.6,4.13940388499999));
#253337=CARTESIAN_POINT('Ctrl Pts',(-10.3570324910001,15.2,4.13938890199999));
#253338=CARTESIAN_POINT('Ctrl Pts',(-10.3570324910001,11.6,4.13938890199999));
#253339=CARTESIAN_POINT('Ctrl Pts',(-10.3603639140001,15.2,4.13937124899999));
#253340=CARTESIAN_POINT('Ctrl Pts',(-10.3603639140001,11.6,4.13937124899998));
#253341=CARTESIAN_POINT('Ctrl Pts',(-10.3637002770001,15.2,4.13935092199999));
#253342=CARTESIAN_POINT('Ctrl Pts',(-10.3637002770001,11.6,4.13935092199999));
#253343=CARTESIAN_POINT('Ctrl Pts',(-10.3670415720001,15.2,4.13932791199999));
#253344=CARTESIAN_POINT('Ctrl Pts',(-10.3670415720001,11.6,4.13932791199999));
#253345=CARTESIAN_POINT('Ctrl Pts',(-10.3703877890001,15.2,4.13930221299999));
#253346=CARTESIAN_POINT('Ctrl Pts',(-10.3703877890001,11.6,4.13930221299999));
#253347=CARTESIAN_POINT('Ctrl Pts',(-10.3737389220001,15.2,4.13927381799999));
#253348=CARTESIAN_POINT('Ctrl Pts',(-10.3737389220001,11.6,4.13927381799999));
#253349=CARTESIAN_POINT('Ctrl Pts',(-10.3770949600001,15.2,4.13924272199999));
#253350=CARTESIAN_POINT('Ctrl Pts',(-10.3770949600001,11.6,4.13924272199999));
#253351=CARTESIAN_POINT('Ctrl Pts',(-10.3804558970001,15.2,4.13920891799999));
#253352=CARTESIAN_POINT('Ctrl Pts',(-10.3804558970001,11.6,4.13920891799999));
#253353=CARTESIAN_POINT('Ctrl Pts',(-10.3838217220001,15.2,4.13917239799999));
#253354=CARTESIAN_POINT('Ctrl Pts',(-10.3838217220001,11.6,4.13917239799999));
#253355=CARTESIAN_POINT('Ctrl Pts',(-10.3871924310001,15.2,4.13913315699999));
#253356=CARTESIAN_POINT('Ctrl Pts',(-10.3871924310001,11.6,4.13913315699998));
#253357=CARTESIAN_POINT('Ctrl Pts',(-10.3905680110001,15.2,4.13909118899999));
#253358=CARTESIAN_POINT('Ctrl Pts',(-10.3905680110001,11.6,4.13909118899999));
#253359=CARTESIAN_POINT('Ctrl Pts',(-10.3939484570001,15.2,4.13904648699998));
#253360=CARTESIAN_POINT('Ctrl Pts',(-10.3939484570001,11.6,4.13904648699998));
#253361=CARTESIAN_POINT('Ctrl Pts',(-10.3973337590001,15.2,4.13899904299999));
#253362=CARTESIAN_POINT('Ctrl Pts',(-10.3973337590001,11.6,4.13899904299999));
#253363=CARTESIAN_POINT('Ctrl Pts',(-10.4007239090001,15.2,4.13894885299998));
#253364=CARTESIAN_POINT('Ctrl Pts',(-10.4007239090001,11.6,4.13894885299998));
#253365=CARTESIAN_POINT('Ctrl Pts',(-10.4041188990001,15.2,4.13889590999998));
#253366=CARTESIAN_POINT('Ctrl Pts',(-10.4041188990001,11.6,4.13889590999998));
#253367=CARTESIAN_POINT('Ctrl Pts',(-10.4075187210001,15.2,4.13884020699999));
#253368=CARTESIAN_POINT('Ctrl Pts',(-10.4075187210001,11.6,4.13884020699999));
#253369=CARTESIAN_POINT('Ctrl Pts',(-10.4109233670001,15.2,4.13878173799999));
#253370=CARTESIAN_POINT('Ctrl Pts',(-10.4109233670001,11.6,4.13878173799999));
#253371=CARTESIAN_POINT('Ctrl Pts',(-10.4143328290001,15.2,4.13872049599998));
#253372=CARTESIAN_POINT('Ctrl Pts',(-10.4143328290001,11.6,4.13872049599998));
#253373=CARTESIAN_POINT('Ctrl Pts',(-10.4177470960001,15.2,4.13865647699998));
#253374=CARTESIAN_POINT('Ctrl Pts',(-10.4177470960001,11.6,4.13865647699998));
#253375=CARTESIAN_POINT('Ctrl Pts',(-10.4211661640001,15.2,4.13858967199998));
#253376=CARTESIAN_POINT('Ctrl Pts',(-10.4211661640001,11.6,4.13858967199998));
#253377=CARTESIAN_POINT('Ctrl Pts',(-10.4245900210001,15.2,4.13852007699998));
#253378=CARTESIAN_POINT('Ctrl Pts',(-10.4245900210001,11.6,4.13852007699998));
#253379=CARTESIAN_POINT('Ctrl Pts',(-10.4280186620001,15.2,4.13844768399999));
#253380=CARTESIAN_POINT('Ctrl Pts',(-10.4280186620001,11.6,4.13844768399999));
#253381=CARTESIAN_POINT('Ctrl Pts',(-10.4314520770001,15.2,4.13837248799998));
#253382=CARTESIAN_POINT('Ctrl Pts',(-10.4314520770001,11.6,4.13837248799998));
#253383=CARTESIAN_POINT('Ctrl Pts',(-10.4348902580001,15.2,4.13829448199999));
#253384=CARTESIAN_POINT('Ctrl Pts',(-10.4348902580001,11.6,4.13829448199999));
#253385=CARTESIAN_POINT('Ctrl Pts',(-10.4383331970001,15.2,4.13821365999999));
#253386=CARTESIAN_POINT('Ctrl Pts',(-10.4383331970001,11.6,4.13821365999999));
#253387=CARTESIAN_POINT('Ctrl Pts',(-10.4417808860001,15.2,4.13813001599999));
#253388=CARTESIAN_POINT('Ctrl Pts',(-10.4417808860001,11.6,4.13813001599998));
#253389=CARTESIAN_POINT('Ctrl Pts',(-10.4452333170001,15.2,4.13804354299998));
#253390=CARTESIAN_POINT('Ctrl Pts',(-10.4452333170001,11.6,4.13804354299998));
#253391=CARTESIAN_POINT('Ctrl Pts',(-10.4486904820001,15.2,4.13795423799999));
#253392=CARTESIAN_POINT('Ctrl Pts',(-10.4486904820001,11.6,4.13795423799998));
#253393=CARTESIAN_POINT('Ctrl Pts',(-10.4521523720001,15.2,4.13786209099998));
#253394=CARTESIAN_POINT('Ctrl Pts',(-10.4521523720001,11.6,4.13786209099998));
#253395=CARTESIAN_POINT('Ctrl Pts',(-10.4556189810001,15.2,4.13776709799999));
#253396=CARTESIAN_POINT('Ctrl Pts',(-10.4556189810001,11.6,4.13776709799999));
#253397=CARTESIAN_POINT('Ctrl Pts',(-10.4590902980001,15.2,4.13766925199998));
#253398=CARTESIAN_POINT('Ctrl Pts',(-10.4590902980001,11.6,4.13766925199998));
#253399=CARTESIAN_POINT('Ctrl Pts',(-10.4625663170001,15.2,4.13756854899999));
#253400=CARTESIAN_POINT('Ctrl Pts',(-10.4625663170001,11.6,4.13756854899999));
#253401=CARTESIAN_POINT('Ctrl Pts',(-10.4660470290001,15.2,4.13746497899999));
#253402=CARTESIAN_POINT('Ctrl Pts',(-10.4660470290001,11.6,4.13746497899999));
#253403=CARTESIAN_POINT('Ctrl Pts',(-10.4695324260001,15.2,4.13735853999999));
#253404=CARTESIAN_POINT('Ctrl Pts',(-10.4695324260001,11.6,4.13735853999999));
#253405=CARTESIAN_POINT('Ctrl Pts',(-10.4730225010001,15.2,4.13724922399999));
#253406=CARTESIAN_POINT('Ctrl Pts',(-10.4730225010001,11.6,4.13724922399999));
#253407=CARTESIAN_POINT('Ctrl Pts',(-10.4765172450001,15.2,4.13713702599999));
#253408=CARTESIAN_POINT('Ctrl Pts',(-10.4765172450001,11.6,4.13713702599999));
#253409=CARTESIAN_POINT('Ctrl Pts',(-10.4800166500001,15.2,4.13702193899999));
#253410=CARTESIAN_POINT('Ctrl Pts',(-10.4800166500001,11.6,4.13702193899999));
#253411=CARTESIAN_POINT('Ctrl Pts',(-10.4835207080001,15.2,4.13690395699999));
#253412=CARTESIAN_POINT('Ctrl Pts',(-10.4835207080001,11.6,4.13690395699999));
#253413=CARTESIAN_POINT('Ctrl Pts',(-10.4870294120001,15.2,4.13678307599999));
#253414=CARTESIAN_POINT('Ctrl Pts',(-10.4870294120001,11.6,4.13678307599999));
#253415=CARTESIAN_POINT('Ctrl Pts',(-10.4905427520001,15.2,4.13665928699999));
#253416=CARTESIAN_POINT('Ctrl Pts',(-10.4905427520001,11.6,4.13665928699999));
#253417=CARTESIAN_POINT('Ctrl Pts',(-10.4940607220001,15.2,4.13653258699998));
#253418=CARTESIAN_POINT('Ctrl Pts',(-10.4940607220001,11.6,4.13653258699998));
#253419=CARTESIAN_POINT('Ctrl Pts',(-10.4975833130001,15.2,4.13640296899998));
#253420=CARTESIAN_POINT('Ctrl Pts',(-10.4975833130001,11.6,4.13640296899998));
#253421=CARTESIAN_POINT('Ctrl Pts',(-10.5011105170001,15.2,4.13627042599998));
#253422=CARTESIAN_POINT('Ctrl Pts',(-10.5011105170001,11.6,4.13627042599998));
#253423=CARTESIAN_POINT('Ctrl Pts',(-10.5046423270001,15.2,4.13613495399999));
#253424=CARTESIAN_POINT('Ctrl Pts',(-10.5046423270001,11.6,4.13613495399998));
#253425=CARTESIAN_POINT('Ctrl Pts',(-10.5081787340001,15.2,4.13599654699999));
#253426=CARTESIAN_POINT('Ctrl Pts',(-10.5081787340001,11.6,4.13599654699999));
#253427=CARTESIAN_POINT('Ctrl Pts',(-10.5117197300001,15.2,4.13585519699998));
#253428=CARTESIAN_POINT('Ctrl Pts',(-10.5117197300001,11.6,4.13585519699998));
#253429=CARTESIAN_POINT('Ctrl Pts',(-10.5152653080001,15.2,4.13571090099998));
#253430=CARTESIAN_POINT('Ctrl Pts',(-10.5152653080001,11.6,4.13571090099998));
#253431=CARTESIAN_POINT('Ctrl Pts',(-10.5188154600001,15.2,4.13556365299999));
#253432=CARTESIAN_POINT('Ctrl Pts',(-10.5188154600001,11.6,4.13556365299998));
#253433=CARTESIAN_POINT('Ctrl Pts',(-10.5223701770001,15.2,4.13541344499999));
#253434=CARTESIAN_POINT('Ctrl Pts',(-10.5223701770001,11.6,4.13541344499999));
#253435=CARTESIAN_POINT('Ctrl Pts',(-10.5259294520001,15.2,4.13526027299999));
#253436=CARTESIAN_POINT('Ctrl Pts',(-10.5259294520001,11.6,4.13526027299999));
#253437=CARTESIAN_POINT('Ctrl Pts',(-10.5294932760001,15.2,4.13510413099999));
#253438=CARTESIAN_POINT('Ctrl Pts',(-10.5294932760001,11.6,4.13510413099999));
#253439=CARTESIAN_POINT('Ctrl Pts',(-10.5330616440001,15.2,4.13494501199998));
#253440=CARTESIAN_POINT('Ctrl Pts',(-10.5330616440001,11.6,4.13494501199998));
#253441=CARTESIAN_POINT('Ctrl Pts',(-10.5366345450001,15.2,4.13478291199999));
#253442=CARTESIAN_POINT('Ctrl Pts',(-10.5366345450001,11.6,4.13478291199999));
#253443=CARTESIAN_POINT('Ctrl Pts',(-10.5402119720001,15.2,4.13461782599998));
#253444=CARTESIAN_POINT('Ctrl Pts',(-10.5402119720001,11.6,4.13461782599998));
#253445=CARTESIAN_POINT('Ctrl Pts',(-10.5437939180001,15.2,4.13444974599999));
#253446=CARTESIAN_POINT('Ctrl Pts',(-10.5437939180001,11.6,4.13444974599999));
#253447=CARTESIAN_POINT('Ctrl Pts',(-10.5473803750001,15.2,4.13427866799999));
#253448=CARTESIAN_POINT('Ctrl Pts',(-10.5473803750001,11.6,4.13427866799999));
#253449=CARTESIAN_POINT('Ctrl Pts',(-10.5509713340001,15.2,4.13410458499998));
#253450=CARTESIAN_POINT('Ctrl Pts',(-10.5509713340001,11.6,4.13410458499998));
#253451=CARTESIAN_POINT('Ctrl Pts',(-10.5545667880001,15.2,4.13392749399998));
#253452=CARTESIAN_POINT('Ctrl Pts',(-10.5545667880001,11.6,4.13392749399998));
#253453=CARTESIAN_POINT('Ctrl Pts',(-10.5581667290001,15.2,4.13374738699999));
#253454=CARTESIAN_POINT('Ctrl Pts',(-10.5581667290001,11.6,4.13374738699999));
#253455=CARTESIAN_POINT('Ctrl Pts',(-10.5617711500001,15.2,4.13356425799999));
#253456=CARTESIAN_POINT('Ctrl Pts',(-10.5617711500001,11.6,4.13356425799999));
#253457=CARTESIAN_POINT('Ctrl Pts',(-10.5653800430001,15.2,4.13337810299998));
#253458=CARTESIAN_POINT('Ctrl Pts',(-10.5653800430001,11.6,4.13337810299998));
#253459=CARTESIAN_POINT('Ctrl Pts',(-10.5689933990001,15.2,4.13318891799998));
#253460=CARTESIAN_POINT('Ctrl Pts',(-10.5689933990001,11.6,4.13318891799998));
#253461=CARTESIAN_POINT('Ctrl Pts',(-10.5726112110001,15.2,4.13299669399999));
#253462=CARTESIAN_POINT('Ctrl Pts',(-10.5726112110001,11.6,4.13299669399999));
#253463=CARTESIAN_POINT('Ctrl Pts',(-10.5762334720001,15.2,4.13280142599999));
#253464=CARTESIAN_POINT('Ctrl Pts',(-10.5762334720001,11.6,4.13280142599999));
#253465=CARTESIAN_POINT('Ctrl Pts',(-10.5798601730001,15.2,4.13260311199998));
#253466=CARTESIAN_POINT('Ctrl Pts',(-10.5798601730001,11.6,4.13260311199998));
#253467=CARTESIAN_POINT('Ctrl Pts',(-10.5834913070001,15.2,4.13240174199998));
#253468=CARTESIAN_POINT('Ctrl Pts',(-10.5834913070001,11.6,4.13240174199998));
#253469=CARTESIAN_POINT('Ctrl Pts',(-10.5871268660001,15.2,4.13219731299999));
#253470=CARTESIAN_POINT('Ctrl Pts',(-10.5871268660001,11.6,4.13219731299998));
#253471=CARTESIAN_POINT('Ctrl Pts',(-10.5907668410001,15.2,4.13198981899999));
#253472=CARTESIAN_POINT('Ctrl Pts',(-10.5907668410001,11.6,4.13198981899999));
#253473=CARTESIAN_POINT('Ctrl Pts',(-10.5944112280001,15.2,4.13177925499999));
#253474=CARTESIAN_POINT('Ctrl Pts',(-10.5944112280001,11.6,4.13177925499998));
#253475=CARTESIAN_POINT('Ctrl Pts',(-10.5980600150001,15.2,4.13156561499999));
#253476=CARTESIAN_POINT('Ctrl Pts',(-10.5980600150001,11.6,4.13156561499999));
#253477=CARTESIAN_POINT('Ctrl Pts',(-10.6017131970001,15.2,4.13134889499998));
#253478=CARTESIAN_POINT('Ctrl Pts',(-10.6017131970001,11.6,4.13134889499998));
#253479=CARTESIAN_POINT('Ctrl Pts',(-10.6053707650001,15.2,4.13112908799998));
#253480=CARTESIAN_POINT('Ctrl Pts',(-10.6053707650001,11.6,4.13112908799998));
#253481=CARTESIAN_POINT('Ctrl Pts',(-10.6090327130001,15.2,4.13090618899999));
#253482=CARTESIAN_POINT('Ctrl Pts',(-10.6090327130001,11.6,4.13090618899999));
#253483=CARTESIAN_POINT('Ctrl Pts',(-10.6126990310001,15.2,4.13068019299998));
#253484=CARTESIAN_POINT('Ctrl Pts',(-10.6126990310001,11.6,4.13068019299998));
#253485=CARTESIAN_POINT('Ctrl Pts',(-10.6163697120001,15.2,4.13045109399999));
#253486=CARTESIAN_POINT('Ctrl Pts',(-10.6163697120001,11.6,4.13045109399999));
#253487=CARTESIAN_POINT('Ctrl Pts',(-10.6200447500001,15.2,4.13021888799998));
#253488=CARTESIAN_POINT('Ctrl Pts',(-10.6200447500001,11.6,4.13021888799998));
#253489=CARTESIAN_POINT('Ctrl Pts',(-10.6237241360001,15.2,4.12998356799999));
#253490=CARTESIAN_POINT('Ctrl Pts',(-10.6237241360001,11.6,4.12998356799999));
#253491=CARTESIAN_POINT('Ctrl Pts',(-10.6274078610001,15.2,4.12974512999998));
#253492=CARTESIAN_POINT('Ctrl Pts',(-10.6274078610001,11.6,4.12974512999998));
#253493=CARTESIAN_POINT('Ctrl Pts',(-10.6310959200001,15.2,4.12950356799998));
#253494=CARTESIAN_POINT('Ctrl Pts',(-10.6310959200001,11.6,4.12950356799998));
#253495=CARTESIAN_POINT('Ctrl Pts',(-10.6347883040001,15.2,4.12925887599998));
#253496=CARTESIAN_POINT('Ctrl Pts',(-10.6347883040001,11.6,4.12925887599998));
#253497=CARTESIAN_POINT('Ctrl Pts',(-10.6384850050001,15.2,4.12901105099999));
#253498=CARTESIAN_POINT('Ctrl Pts',(-10.6384850050001,11.6,4.12901105099999));
#253499=CARTESIAN_POINT('Ctrl Pts',(-10.6421860180001,15.2,4.12876008799999));
#253500=CARTESIAN_POINT('Ctrl Pts',(-10.6421860180001,11.6,4.12876008799999));
#253501=CARTESIAN_POINT('Ctrl Pts',(-10.6458913320001,15.2,4.12850597899999));
#253502=CARTESIAN_POINT('Ctrl Pts',(-10.6458913320001,11.6,4.12850597899998));
#253503=CARTESIAN_POINT('Ctrl Pts',(-10.6496009430001,15.2,4.12824872099999));
#253504=CARTESIAN_POINT('Ctrl Pts',(-10.6496009430001,11.6,4.12824872099998));
#253505=CARTESIAN_POINT('Ctrl Pts',(-10.6533148400001,15.2,4.12798830699998));
#253506=CARTESIAN_POINT('Ctrl Pts',(-10.6533148400001,11.6,4.12798830699998));
#253507=CARTESIAN_POINT('Ctrl Pts',(-10.6570330180001,15.2,4.12772473399999));
#253508=CARTESIAN_POINT('Ctrl Pts',(-10.6570330180001,11.6,4.12772473399999));
#253509=CARTESIAN_POINT('Ctrl Pts',(-10.6607554670001,15.2,4.12745799499999));
#253510=CARTESIAN_POINT('Ctrl Pts',(-10.6607554670001,11.6,4.12745799499999));
#253511=CARTESIAN_POINT('Ctrl Pts',(-10.6644821790001,15.2,4.12718808499999));
#253512=CARTESIAN_POINT('Ctrl Pts',(-10.6644821790001,11.6,4.12718808499999));
#253513=CARTESIAN_POINT('Ctrl Pts',(-10.6682131480001,15.2,4.12691499899999));
#253514=CARTESIAN_POINT('Ctrl Pts',(-10.6682131480001,11.6,4.12691499899999));
#253515=CARTESIAN_POINT('Ctrl Pts',(-10.6719483670001,15.2,4.12663873099999));
#253516=CARTESIAN_POINT('Ctrl Pts',(-10.6719483670001,11.6,4.12663873099999));
#253517=CARTESIAN_POINT('Ctrl Pts',(-10.6756878260001,15.2,4.12635927799998));
#253518=CARTESIAN_POINT('Ctrl Pts',(-10.6756878260001,11.6,4.12635927799998));
#253519=CARTESIAN_POINT('Ctrl Pts',(-10.6794315200001,15.2,4.12607663399999));
#253520=CARTESIAN_POINT('Ctrl Pts',(-10.6794315200001,11.6,4.12607663399999));
#253521=CARTESIAN_POINT('Ctrl Pts',(-10.6831794430001,15.2,4.12579079399999));
#253522=CARTESIAN_POINT('Ctrl Pts',(-10.6831794430001,11.6,4.12579079399999));
#253523=CARTESIAN_POINT('Ctrl Pts',(-10.6869315860001,15.2,4.12550175599999));
#253524=CARTESIAN_POINT('Ctrl Pts',(-10.6869315860001,11.6,4.12550175599998));
#253525=CARTESIAN_POINT('Ctrl Pts',(-10.6906879440001,15.2,4.12520951199999));
#253526=CARTESIAN_POINT('Ctrl Pts',(-10.6906879440001,11.6,4.12520951199998));
#253527=CARTESIAN_POINT('Ctrl Pts',(-10.6944485080001,15.2,4.12491405999998));
#253528=CARTESIAN_POINT('Ctrl Pts',(-10.6944485080001,11.6,4.12491405999998));
#253529=CARTESIAN_POINT('Ctrl Pts',(-10.6982132700001,15.2,4.12461538999998));
#253530=CARTESIAN_POINT('Ctrl Pts',(-10.6982132700001,11.6,4.12461538999998));
#253531=CARTESIAN_POINT('Ctrl Pts',(-10.7019822200001,15.2,4.12431349999999));
#253532=CARTESIAN_POINT('Ctrl Pts',(-10.7019822200001,11.6,4.12431349999998));
#253533=CARTESIAN_POINT('Ctrl Pts',(-10.7057553490001,15.2,4.12400838099998));
#253534=CARTESIAN_POINT('Ctrl Pts',(-10.7057553490001,11.6,4.12400838099998));
#253535=CARTESIAN_POINT('Ctrl Pts',(-10.7095326480001,15.2,4.12370002799998));
#253536=CARTESIAN_POINT('Ctrl Pts',(-10.7095326480001,11.6,4.12370002799998));
#253537=CARTESIAN_POINT('Ctrl Pts',(-10.7133141100001,15.2,4.12338843599999));
#253538=CARTESIAN_POINT('Ctrl Pts',(-10.7133141100001,11.6,4.12338843599999));
#253539=CARTESIAN_POINT('Ctrl Pts',(-10.7170997260001,15.2,4.12307359999998));
#253540=CARTESIAN_POINT('Ctrl Pts',(-10.7170997260001,11.6,4.12307359999998));
#253541=CARTESIAN_POINT('Ctrl Pts',(-10.7208894930001,15.2,4.12275551699998));
#253542=CARTESIAN_POINT('Ctrl Pts',(-10.7208894930001,11.6,4.12275551699998));
#253543=CARTESIAN_POINT('Ctrl Pts',(-10.7246834070001,15.2,4.12243418399999));
#253544=CARTESIAN_POINT('Ctrl Pts',(-10.7246834070001,11.6,4.12243418399999));
#253545=CARTESIAN_POINT('Ctrl Pts',(-10.7284814650001,15.2,4.12210960099999));
#253546=CARTESIAN_POINT('Ctrl Pts',(-10.7284814650001,11.6,4.12210960099998));
#253547=CARTESIAN_POINT('Ctrl Pts',(-10.7315232270001,15.2,4.12184733399998));
#253548=CARTESIAN_POINT('Ctrl Pts',(-10.7315232270001,11.6,4.12184733399998));
#253549=CARTESIAN_POINT('Ctrl Pts',(-10.7338064110001,15.2,4.12164916999998));
#253550=CARTESIAN_POINT('Ctrl Pts',(-10.7338064110001,11.6,4.12164916999998));
#253551=CARTESIAN_POINT('Ctrl Pts',(-10.7353293650001,15.2,4.12151641099998));
#253552=CARTESIAN_POINT('Ctrl Pts',(-10.7353293650001,11.6,4.12151641099998));
#253553=CARTESIAN_POINT('Ctrl Pts',(-10.7360910480001,15.2,4.12144986899998));
#253554=CARTESIAN_POINT('Ctrl Pts',(-10.7360910480001,11.6,4.12144986899998));
#253555=CARTESIAN_POINT('Ctrl Pts',(-9.55499537100006,15.2,4.04260911699998));
#253556=CARTESIAN_POINT('Ctrl Pts',(-9.55669455126496,15.2,4.04316130806102));
#253557=CARTESIAN_POINT('Ctrl Pts',(-9.55844976571224,15.2,4.0437260538932));
#253558=CARTESIAN_POINT('Ctrl Pts',(-9.56026027810168,15.2,4.04430244593684));
#253559=CARTESIAN_POINT('Ctrl Pts',(-9.56207952169703,15.2,4.04488161763427));
#253560=CARTESIAN_POINT('Ctrl Pts',(-9.563954601157,15.2,4.04547254503639));
#253561=CARTESIAN_POINT('Ctrl Pts',(-9.56588480694515,15.2,4.04607433301654));
#253562=CARTESIAN_POINT('Ctrl Pts',(-9.56781501255799,15.2,4.04667612094203));
#253563=CARTESIAN_POINT('Ctrl Pts',(-9.56980034124075,15.2,4.0472887691226));
#253564=CARTESIAN_POINT('Ctrl Pts',(-9.57184010199996,15.2,4.04791140626664));
#253565=CARTESIAN_POINT('Ctrl Pts',(-9.57387986275917,15.2,4.04853404341067));
#253566=CARTESIAN_POINT('Ctrl Pts',(-9.57597405465781,15.2,4.04916667292137));
#253567=CARTESIAN_POINT('Ctrl Pts',(-9.57812199976731,15.2,4.04980844817958));
#253568=CARTESIAN_POINT('Ctrl Pts',(-9.5802699450719,15.2,4.05045022349609));
#253569=CARTESIAN_POINT('Ctrl Pts',(-9.58247164646091,15.2,4.05110114611867));
#253570=CARTESIAN_POINT('Ctrl Pts',(-9.58472644050408,15.2,4.05176039932183));
#253571=CARTESIAN_POINT('Ctrl Pts',(-9.58698123434243,15.2,4.05241965246511));
#253572=CARTESIAN_POINT('Ctrl Pts',(-9.58928912240927,15.2,4.05308723561338));
#253573=CARTESIAN_POINT('Ctrl Pts',(-9.59164945950104,15.2,4.05376235400861));
#253574=CARTESIAN_POINT('Ctrl Pts',(-9.59400979659281,15.2,4.05443747240384));
#253575=CARTESIAN_POINT('Ctrl Pts',(-9.59642258392434,15.2,4.05512012772112));
#253576=CARTESIAN_POINT('Ctrl Pts',(-9.59888719166586,15.2,4.05580954919576));
#253577=CARTESIAN_POINT('Ctrl Pts',(-9.60135179963124,15.2,4.05649897073303));
#253578=CARTESIAN_POINT('Ctrl Pts',(-9.60386822553645,15.2,4.05719515850451));
#253579=CARTESIAN_POINT('Ctrl Pts',(-9.60643585601319,15.2,4.05789736304319));
#253580=CARTESIAN_POINT('Ctrl Pts',(-9.60900348625671,15.2,4.05859956751807));
#253581=CARTESIAN_POINT('Ctrl Pts',(-9.61162232335711,15.2,4.05930778842291));
#253582=CARTESIAN_POINT('Ctrl Pts',(-9.614291761429,15.2,4.06002130098055));
#253583=CARTESIAN_POINT('Ctrl Pts',(-9.61696119950089,15.2,4.06073481353819));
#253584=CARTESIAN_POINT('Ctrl Pts',(-9.61968124038537,15.2,4.06145361467872));
#253585=CARTESIAN_POINT('Ctrl Pts',(-9.62245129461588,15.2,4.06217699940224));
#253586=CARTESIAN_POINT('Ctrl Pts',(-9.62522134884639,15.2,4.06290038412575));
#253587=CARTESIAN_POINT('Ctrl Pts',(-9.62804141584483,15.2,4.06362835228872));
#253588=CARTESIAN_POINT('Ctrl Pts',(-9.63091092190387,15.2,4.06436021417854));
#253589=CARTESIAN_POINT('Ctrl Pts',(-9.63378042822357,15.2,4.06509207613484));
#253590=CARTESIAN_POINT('Ctrl Pts',(-9.63669937019805,15.2,4.06582783428319));
#253591=CARTESIAN_POINT('Ctrl Pts',(-9.63966718486192,15.2,4.0665668163236));
#253592=CARTESIAN_POINT('Ctrl Pts',(-9.64263499925622,15.2,4.06730579829689));
#253593=CARTESIAN_POINT('Ctrl Pts',(-9.64565168602948,15.2,4.06804800619833));
#253594=CARTESIAN_POINT('Ctrl Pts',(-9.64871669226525,15.2,4.06879278825798));
#253595=CARTESIAN_POINT('Ctrl Pts',(-9.65178169850103,15.2,4.06953757031763));
#253596=CARTESIAN_POINT('Ctrl Pts',(-9.65489502331519,15.2,4.07028492457067));
#253597=CARTESIAN_POINT('Ctrl Pts',(-9.65805612461376,15.2,4.07103421945998));
#253598=CARTESIAN_POINT('Ctrl Pts',(-9.66121722619947,15.2,4.07178351441735));
#253599=CARTESIAN_POINT('Ctrl Pts',(-9.6644261034481,15.2,4.0725347480666));
#253600=CARTESIAN_POINT('Ctrl Pts',(-9.66768222512764,15.2,4.07328730227434));
#253601=CARTESIAN_POINT('Ctrl Pts',(-9.6709383465114,15.2,4.07403985641372));
#253602=CARTESIAN_POINT('Ctrl Pts',(-9.67424171249674,15.2,4.0747937321403));
#253603=CARTESIAN_POINT('Ctrl Pts',(-9.67759179997346,15.2,4.07554832544964));
#253604=CARTESIAN_POINT('Ctrl Pts',(-9.68094188745019,15.2,4.07630291875899));
#253605=CARTESIAN_POINT('Ctrl Pts',(-9.6843386955196,15.2,4.07705823106177));
#253606=CARTESIAN_POINT('Ctrl Pts',(-9.68778171389136,15.2,4.07781367520097));
#253607=CARTESIAN_POINT('Ctrl Pts',(-9.69122473257588,15.2,4.0785691194088));
#253608=CARTESIAN_POINT('Ctrl Pts',(-9.69471395954516,15.2,4.07932469324418));
#253609=CARTESIAN_POINT('Ctrl Pts',(-9.69824889183372,15.2,4.08007982582303));
#253610=CARTESIAN_POINT('Ctrl Pts',(-9.70178382380118,15.2,4.08083495833329));
#253611=CARTESIAN_POINT('Ctrl Pts',(-9.70536446121434,15.2,4.08158965010223));
#253612=CARTESIAN_POINT('Ctrl Pts',(-9.70899030975022,15.2,4.08234334149171));
#253613=CARTESIAN_POINT('Ctrl Pts',(-9.7126161582861,15.2,4.08309703288118));
#253614=CARTESIAN_POINT('Ctrl Pts',(-9.71628721459259,15.2,4.083849723842));
#253615=CARTESIAN_POINT('Ctrl Pts',(-9.72000299814063,15.2,4.08460086943565));
#253616=CARTESIAN_POINT('Ctrl Pts',(-9.72433807917169,15.2,4.08547720600707));
#253617=CARTESIAN_POINT('Ctrl Pts',(-9.72873403127503,15.2,4.08635143902531));
#253618=CARTESIAN_POINT('Ctrl Pts',(-9.73319010048331,15.2,4.08722272398332));
#253619=CARTESIAN_POINT('Ctrl Pts',(-9.73764616969159,15.2,4.08809400894134));
#253620=CARTESIAN_POINT('Ctrl Pts',(-9.74216235387668,15.2,4.08896234888187));
#253621=CARTESIAN_POINT('Ctrl Pts',(-9.74673791088781,15.2,4.08982691981334));
#253622=CARTESIAN_POINT('Ctrl Pts',(-9.75000616584487,15.2,4.09044447046906));
#253623=CARTESIAN_POINT('Ctrl Pts',(-9.75330471231626,15.2,4.09106009923596));
#253624=CARTESIAN_POINT('Ctrl Pts',(-9.75663328315204,15.2,4.09167351555522));
#253625=CARTESIAN_POINT('Ctrl Pts',(-9.75996185398783,15.2,4.09228693187448));
#253626=CARTESIAN_POINT('Ctrl Pts',(-9.76332045076296,15.2,4.09289813404092));
#253627=CARTESIAN_POINT('Ctrl Pts',(-9.76670880895986,15.2,4.09350683709628));
#253628=CARTESIAN_POINT('Ctrl Pts',(-9.77009716678742,15.2,4.09411554008528));
#253629=CARTESIAN_POINT('Ctrl Pts',(-9.77351528492723,15.2,4.09472174240883));
#253630=CARTESIAN_POINT('Ctrl Pts',(-9.77696290600738,15.2,4.09532516616273));
#253631=CARTESIAN_POINT('Ctrl Pts',(-9.78041052746331,15.2,4.09592858998241));
#253632=CARTESIAN_POINT('Ctrl Pts',(-9.78388764933264,15.2,4.09652923191047));
#253633=CARTESIAN_POINT('Ctrl Pts',(-9.78739401752469,15.2,4.0971268184385));
#253634=CARTESIAN_POINT('Ctrl Pts',(-9.79090038571675,15.2,4.09772440496652));
#253635=CARTESIAN_POINT('Ctrl Pts',(-9.79443599718798,15.2,4.09831893500158));
#253636=CARTESIAN_POINT('Ctrl Pts',(-9.79800060208629,15.2,4.09891014065635));
#253637=CARTESIAN_POINT('Ctrl Pts',(-9.80156520698459,15.2,4.09950134631112));
#253638=CARTESIAN_POINT('Ctrl Pts',(-9.80515880119807,15.2,4.10008922425601));
#253639=CARTESIAN_POINT('Ctrl Pts',(-9.80878113702993,15.2,4.10067351168676));
#253640=CARTESIAN_POINT('Ctrl Pts',(-9.81240347286178,15.2,4.10125779911751));
#253641=CARTESIAN_POINT('Ctrl Pts',(-9.81605454863878,15.2,4.10183849410094));
#253642=CARTESIAN_POINT('Ctrl Pts',(-9.81973411794285,15.2,4.10241533896225));
#253643=CARTESIAN_POINT('Ctrl Pts',(-9.82341368724693,15.2,4.10299218382356));
#253644=CARTESIAN_POINT('Ctrl Pts',(-9.8271217512366,15.2,4.10356517540819));
#253645=CARTESIAN_POINT('Ctrl Pts',(-9.83085806298962,15.2,4.10413406117469));
#253646=CARTESIAN_POINT('Ctrl Pts',(-9.8360888995253,15.2,4.10493050126017));
#253647=CARTESIAN_POINT('Ctrl Pts',(-9.84137510306443,15.2,4.10571888958012));
#253648=CARTESIAN_POINT('Ctrl Pts',(-9.84671601098299,15.2,4.10649854132806));
#253649=CARTESIAN_POINT('Ctrl Pts',(-9.85053094515112,15.2,4.10705543542506));
#253650=CARTESIAN_POINT('Ctrl Pts',(-9.85437378940413,15.2,4.10760787110875));
#253651=CARTESIAN_POINT('Ctrl Pts',(-9.85824430793272,15.2,4.10815560683023));
#253652=CARTESIAN_POINT('Ctrl Pts',(-9.86288892999829,15.2,4.10881288967213));
#253653=CARTESIAN_POINT('Ctrl Pts',(-9.8675733997966,15.2,4.10946339959004));
#253654=CARTESIAN_POINT('Ctrl Pts',(-9.87229731270832,15.2,4.11010672473333));
#253655=CARTESIAN_POINT('Ctrl Pts',(-9.87702122562003,15.2,4.11075004987663));
#253656=CARTESIAN_POINT('Ctrl Pts',(-9.88178458059536,15.2,4.11138619022881));
#253657=CARTESIAN_POINT('Ctrl Pts',(-9.88658697766821,15.2,4.11201473845649));
#253658=CARTESIAN_POINT('Ctrl Pts',(-9.89058897537431,15.2,4.11253852866525));
#253659=CARTESIAN_POINT('Ctrl Pts',(-9.89461808639513,15.2,4.11305704756442));
#253660=CARTESIAN_POINT('Ctrl Pts',(-9.89867407930424,15.2,4.11357006592376));
#253661=CARTESIAN_POINT('Ctrl Pts',(-9.90273007221334,15.2,4.1140830842831));
#253662=CARTESIAN_POINT('Ctrl Pts',(-9.90681294836055,15.2,4.11459059953352));
#253663=CARTESIAN_POINT('Ctrl Pts',(-9.91092248099806,15.2,4.11509238724215));
#253664=CARTESIAN_POINT('Ctrl Pts',(-9.91503201363557,15.2,4.11559417495078));
#253665=CARTESIAN_POINT('Ctrl Pts',(-9.91916820151262,15.2,4.11609023490649));
#253666=CARTESIAN_POINT('Ctrl Pts',(-9.92333082171958,15.2,4.11658034497625));
#253667=CARTESIAN_POINT('Ctrl Pts',(-9.92666091806663,15.2,4.11697243305342));
#253668=CARTESIAN_POINT('Ctrl Pts',(-9.93000793111592,15.2,4.11736071351595));
#253669=CARTESIAN_POINT('Ctrl Pts',(-9.93337174574653,15.2,4.11774507255575));
#253670=CARTESIAN_POINT('Ctrl Pts',(-9.93673555991882,15.2,4.11812943154319));
#253671=CARTESIAN_POINT('Ctrl Pts',(-9.94011617757625,15.2,4.11850987124414));
#253672=CARTESIAN_POINT('Ctrl Pts',(-9.94351348346409,15.2,4.11888627943586));
#253673=CARTESIAN_POINT('Ctrl Pts',(-9.9469107898148,15.2,4.11926268767886));
#253674=CARTESIAN_POINT('Ctrl Pts',(-9.95032478566477,15.2,4.11963506655472));
#253675=CARTESIAN_POINT('Ctrl Pts',(-9.95375535929726,15.2,4.12000330479674));
#253676=CARTESIAN_POINT('Ctrl Pts',(-9.95718593246236,15.2,4.12037154298859));
#253677=CARTESIAN_POINT('Ctrl Pts',(-9.96063308162847,15.2,4.12073564105328));
#253678=CARTESIAN_POINT('Ctrl Pts',(-9.96409669823916,15.2,4.1210954919311));
#253679=CARTESIAN_POINT('Ctrl Pts',(-9.96756031532177,15.2,4.12145534285795));
#253680=CARTESIAN_POINT('Ctrl Pts',(-9.97104039718604,15.2,4.12181094732649));
#253681=CARTESIAN_POINT('Ctrl Pts',(-9.97453683554432,15.2,4.12216219701201));
#253682=CARTESIAN_POINT('Ctrl Pts',(-9.9780332734262,15.2,4.12251344664968));
#253683=CARTESIAN_POINT('Ctrl Pts',(-9.98154606561872,15.2,4.12286034408266));
#253684=CARTESIAN_POINT('Ctrl Pts',(-9.98507510543966,15.2,4.12320278294401));
#253685=CARTESIAN_POINT('Ctrl Pts',(-9.99125092572734,15.2,4.12380205100968));
#253686=CARTESIAN_POINT('Ctrl Pts',(-9.99747649767144,15.2,4.12438766347715));
#253687=CARTESIAN_POINT('Ctrl Pts',(-10.0037512432559,15.2,4.12495907280812));
#253688=CARTESIAN_POINT('Ctrl Pts',(-10.0073368123009,15.2,4.12528559243852));
#253689=CARTESIAN_POINT('Ctrl Pts',(-10.0109384379705,15.2,4.12560747483783));
#253690=CARTESIAN_POINT('Ctrl Pts',(-10.0145560123915,15.2,4.12592461657685));
#253691=CARTESIAN_POINT('Ctrl Pts',(-10.0181735863196,15.2,4.12624175827267));
#253692=CARTESIAN_POINT('Ctrl Pts',(-10.0218071094151,15.2,4.12655416133019));
#253693=CARTESIAN_POINT('Ctrl Pts',(-10.0254564747268,15.2,4.12686172624981));
#253694=CARTESIAN_POINT('Ctrl Pts',(-10.0318428646439,15.2,4.12739996491152));
#253695=CARTESIAN_POINT('Ctrl Pts',(-10.0382777734669,15.2,4.12792338551636));
#253696=CARTESIAN_POINT('Ctrl Pts',(-10.0447606348613,15.2,4.12843146127369));
#253697=CARTESIAN_POINT('Ctrl Pts',(-10.0484651267262,15.2,4.12872179024963));
#253698=CARTESIAN_POINT('Ctrl Pts',(-10.0521852758934,15.2,4.12900711006824));
#253699=CARTESIAN_POINT('Ctrl Pts',(-10.0559209791976,15.2,4.12928732321252));
#253700=CARTESIAN_POINT('Ctrl Pts',(-10.0605906087095,15.2,4.12963758967151));
#253701=CARTESIAN_POINT('Ctrl Pts',(-10.0652845397351,15.2,4.12997987894394));
#253702=CARTESIAN_POINT('Ctrl Pts',(-10.0700025726774,15.2,4.13031400521119));
#253703=CARTESIAN_POINT('Ctrl Pts',(-10.073776999237,15.2,4.13058130623956));
#253704=CARTESIAN_POINT('Ctrl Pts',(-10.0775668492473,15.2,4.1308433830573));
#253705=CARTESIAN_POINT('Ctrl Pts',(-10.0813720210112,15.2,4.13110014273761));
#253706=CARTESIAN_POINT('Ctrl Pts',(-10.0861284854569,15.2,4.13142109232051));
#253707=CARTESIAN_POINT('Ctrl Pts',(-10.0909088891353,15.2,4.13173373190362));
#253708=CARTESIAN_POINT('Ctrl Pts',(-10.095713033581,15.2,4.13203788398651));
#253709=CARTESIAN_POINT('Ctrl Pts',(-10.1024388353861,15.2,4.13246369687604));
#253710=CARTESIAN_POINT('Ctrl Pts',(-10.1092111673848,15.2,4.1328728723868));
#253711=CARTESIAN_POINT('Ctrl Pts',(-10.1160294893463,15.2,4.13326492573837));
#253712=CARTESIAN_POINT('Ctrl Pts',(-10.1218737659958,15.2,4.13360097150754));
#253713=CARTESIAN_POINT('Ctrl Pts',(-10.127751830557,15.2,4.13392443983384));
#253714=CARTESIAN_POINT('Ctrl Pts',(-10.1336633472973,15.2,4.13423503051688));
#253715=CARTESIAN_POINT('Ctrl Pts',(-10.1376043579206,15.2,4.13444209094403));
#253716=CARTESIAN_POINT('Ctrl Pts',(-10.1415602353375,15.2,4.13464342796343));
#253717=CARTESIAN_POINT('Ctrl Pts',(-10.1455308809322,15.2,4.13483895567994));
#253718=CARTESIAN_POINT('Ctrl Pts',(-10.1504941883314,15.2,4.13508336534555));
#253719=CARTESIAN_POINT('Ctrl Pts',(-10.1554805721959,15.2,4.13531869691245));
#253720=CARTESIAN_POINT('Ctrl Pts',(-10.1604898376809,15.2,4.1355447824685));
#253721=CARTESIAN_POINT('Ctrl Pts',(-10.1644972502872,15.2,4.13572565092319));
#253722=CARTESIAN_POINT('Ctrl Pts',(-10.1685193089231,15.2,4.1359006027105));
#253723=CARTESIAN_POINT('Ctrl Pts',(-10.1725559147551,15.2,4.13606955249709));
#253724=CARTESIAN_POINT('Ctrl Pts',(-10.1765925200372,15.2,4.13623850226067));
#253725=CARTESIAN_POINT('Ctrl Pts',(-10.1806436727997,15.2,4.13640145021156));
#253726=CARTESIAN_POINT('Ctrl Pts',(-10.1847092760769,15.2,4.13655831269936));
#253727=CARTESIAN_POINT('Ctrl Pts',(-10.1908076818238,15.2,4.13679360646312));
#253728=CARTESIAN_POINT('Ctrl Pts',(-10.1969386013006,15.2,4.13701521093252));
#253729=CARTESIAN_POINT('Ctrl Pts',(-10.203101708613,15.2,4.13722284278672));
#253730=CARTESIAN_POINT('Ctrl Pts',(-10.2072104462614,15.2,4.13736126400401));
#253731=CARTESIAN_POINT('Ctrl Pts',(-10.21133349069,15.2,4.13749347742454));
#253732=CARTESIAN_POINT('Ctrl Pts',(-10.2154707441286,15.2,4.13761940124799));
#253733=CARTESIAN_POINT('Ctrl Pts',(-10.2216766251321,15.2,4.1378082870089));
#253734=CARTESIAN_POINT('Ctrl Pts',(-10.2279144815312,15.2,4.1379830205514));
#253735=CARTESIAN_POINT('Ctrl Pts',(-10.2341839894584,15.2,4.13814333347581));
#253736=CARTESIAN_POINT('Ctrl Pts',(-10.2383636608404,15.2,4.1382502087442));
#253737=CARTESIAN_POINT('Ctrl Pts',(-10.2425574012693,15.2,4.13835067492662));
#253738=CARTESIAN_POINT('Ctrl Pts',(-10.2467651152221,15.2,4.13844465397495));
#253739=CARTESIAN_POINT('Ctrl Pts',(-10.2520247580932,15.2,4.13856212779495));
#253740=CARTESIAN_POINT('Ctrl Pts',(-10.2573062343166,15.2,4.13866946410557));
#253741=CARTESIAN_POINT('Ctrl Pts',(-10.2626093622333,15.2,4.13876651230001));
#253742=CARTESIAN_POINT('Ctrl Pts',(-10.2668518647979,15.2,4.1388441508598));
#253743=CARTESIAN_POINT('Ctrl Pts',(-10.2711082249529,15.2,4.13891520451883));
#253744=CARTESIAN_POINT('Ctrl Pts',(-10.2753783489648,15.2,4.13897959774387));
#253745=CARTESIAN_POINT('Ctrl Pts',(-10.280716003107,15.2,4.13906008926202));
#253746=CARTESIAN_POINT('Ctrl Pts',(-10.2860751643011,15.2,4.13913017339785));
#253747=CARTESIAN_POINT('Ctrl Pts',(-10.2914556507962,15.2,4.13918970318389));
#253748=CARTESIAN_POINT('Ctrl Pts',(-10.2989883328277,15.2,4.13927304489473));
#253749=CARTESIAN_POINT('Ctrl Pts',(-10.3065628132273,15.2,4.13933569791323));
#253750=CARTESIAN_POINT('Ctrl Pts',(-10.3141786015944,15.2,4.13937726828967));
#253751=CARTESIAN_POINT('Ctrl Pts',(-10.3185304808307,15.2,4.13940102279142));
#253752=CARTESIAN_POINT('Ctrl Pts',(-10.322895849013,15.2,4.13941789275098));
#253753=CARTESIAN_POINT('Ctrl Pts',(-10.3272746151938,15.2,4.13942780475142));
#253754=CARTESIAN_POINT('Ctrl Pts',(-10.331653380778,15.2,4.13943771675049));
#253755=CARTESIAN_POINT('Ctrl Pts',(-10.336045542401,15.2,4.13944067167726));
#253756=CARTESIAN_POINT('Ctrl Pts',(-10.3404510123733,15.2,4.13943659823361));
#253757=CARTESIAN_POINT('Ctrl Pts',(-10.3470592182321,15.2,4.13943048806731));
#253758=CARTESIAN_POINT('Ctrl Pts',(-10.3536973646947,15.2,4.1394085615407));
#253759=CARTESIAN_POINT('Ctrl Pts',(-10.3603651497268,15.2,4.13937058045421));
#253760=CARTESIAN_POINT('Ctrl Pts',(-10.36369904194,15.2,4.13935158991268));
#253761=CARTESIAN_POINT('Ctrl Pts',(-10.3670403442681,15.2,4.13932858651225));
#253762=CARTESIAN_POINT('Ctrl Pts',(-10.3703890186063,15.2,4.13930153901141));
#253763=CARTESIAN_POINT('Ctrl Pts',(-10.3737376929445,15.2,4.13927449151058));
#253764=CARTESIAN_POINT('Ctrl Pts',(-10.3770937391716,15.2,4.13924340156186));
#253765=CARTESIAN_POINT('Ctrl Pts',(-10.3804571194251,15.2,4.13920823902111));
#253766=CARTESIAN_POINT('Ctrl Pts',(-10.3838204996785,15.2,4.13917307648037));
#253767=CARTESIAN_POINT('Ctrl Pts',(-10.3871912152061,15.2,4.13913384111511));
#253768=CARTESIAN_POINT('Ctrl Pts',(-10.3905692274583,15.2,4.13909050549168));
#253769=CARTESIAN_POINT('Ctrl Pts',(-10.3939472397106,15.2,4.13904716986826));
#253770=CARTESIAN_POINT('Ctrl Pts',(-10.3973325494209,15.2,4.13899973183666));
#253771=CARTESIAN_POINT('Ctrl Pts',(-10.4007251186303,15.2,4.13894816475556));
#253772=CARTESIAN_POINT('Ctrl Pts',(-10.4063794008515,15.2,4.13886221961728));
#253773=CARTESIAN_POINT('Ctrl Pts',(-10.4120538514322,15.2,4.13876480144498));
#253774=CARTESIAN_POINT('Ctrl Pts',(-10.4177482961802,15.2,4.13865578054174));
#253775=CARTESIAN_POINT('Ctrl Pts',(-10.4223038522269,15.2,4.13856856381439));
#253776=CARTESIAN_POINT('Ctrl Pts',(-10.4268722058869,15.2,4.13847392088687));
#253777=CARTESIAN_POINT('Ctrl Pts',(-10.431453269249,15.2,4.13837178549165));
#253778=CARTESIAN_POINT('Ctrl Pts',(-10.4348890664585,15.2,4.13829518395218));
#253779=CARTESIAN_POINT('Ctrl Pts',(-10.4383320126671,15.2,4.13821436768797));
#253780=CARTESIAN_POINT('Ctrl Pts',(-10.4417820718757,15.2,4.13812930877402));
#253781=CARTESIAN_POINT('Ctrl Pts',(-10.4475321707656,15.2,4.13798754391229));
#253782=CARTESIAN_POINT('Ctrl Pts',(-10.4533020282315,15.2,4.13783399616208));
#253783=CARTESIAN_POINT('Ctrl Pts',(-10.4590914741471,15.2,4.13766853768077));
#253784=CARTESIAN_POINT('Ctrl Pts',(-10.463723030501,15.2,4.13753617090654));
#253785=CARTESIAN_POINT('Ctrl Pts',(-10.4683671232037,15.2,4.13739618014944));
#253786=CARTESIAN_POINT('Ctrl Pts',(-10.4730236678778,15.2,4.13724850349535));
#253787=CARTESIAN_POINT('Ctrl Pts',(-10.4788443491962,15.2,4.13706390766265));
#253788=CARTESIAN_POINT('Ctrl Pts',(-10.4846844851346,15.2,4.1368673007574));
#253789=CARTESIAN_POINT('Ctrl Pts',(-10.4905439090919,15.2,4.13665855923026));
#253790=CARTESIAN_POINT('Ctrl Pts',(-10.4940595633386,15.2,4.13653331431852));
#253791=CARTESIAN_POINT('Ctrl Pts',(-10.4975821614199,15.2,4.13640370167721));
#253792=CARTESIAN_POINT('Ctrl Pts',(-10.5011116678005,15.2,4.13626969375923));
#253793=CARTESIAN_POINT('Ctrl Pts',(-10.5058176767355,15.2,4.13609101651903));
#253794=CARTESIAN_POINT('Ctrl Pts',(-10.5105359658977,15.2,4.13590452642293));
#253795=CARTESIAN_POINT('Ctrl Pts',(-10.5152664518785,15.2,4.13571016296738));
#253796=CARTESIAN_POINT('Ctrl Pts',(-10.5188143160419,15.2,4.13556439038896));
#253797=CARTESIAN_POINT('Ctrl Pts',(-10.5223690404961,15.2,4.13541418802773));
#253798=CARTESIAN_POINT('Ctrl Pts',(-10.5259305892833,15.2,4.13525953049169));
#253799=CARTESIAN_POINT('Ctrl Pts',(-10.5294921380706,15.2,4.13510487295564));
#253800=CARTESIAN_POINT('Ctrl Pts',(-10.5330605128242,15.2,4.1349457590281));
#253801=CARTESIAN_POINT('Ctrl Pts',(-10.5366356761104,15.2,4.13478216549277));
#253802=CARTESIAN_POINT('Ctrl Pts',(-10.5425942818039,15.2,4.13450950959064));
#253803=CARTESIAN_POINT('Ctrl Pts',(-10.5485717479089,15.2,4.13422440600763));
#253804=CARTESIAN_POINT('Ctrl Pts',(-10.5545679093663,15.2,4.13392674003607));
#253805=CARTESIAN_POINT('Ctrl Pts',(-10.5605640708236,15.2,4.13362907406451));
#253806=CARTESIAN_POINT('Ctrl Pts',(-10.5665789301472,15.2,4.13331884351273));
#253807=CARTESIAN_POINT('Ctrl Pts',(-10.5726123232301,15.2,4.13299593302519));
#253808=CARTESIAN_POINT('Ctrl Pts',(-10.5774390379594,15.2,4.13273760462109));
#253809=CARTESIAN_POINT('Ctrl Pts',(-10.5822776152914,15.2,4.1324711626737));
#253810=CARTESIAN_POINT('Ctrl Pts',(-10.5871279708347,15.2,4.13219654671345));
#253811=CARTESIAN_POINT('Ctrl Pts',(-10.5919783257172,15.2,4.13192193079062));
#253812=CARTESIAN_POINT('Ctrl Pts',(-10.5968404610259,15.2,4.13163914193274));
#253813=CARTESIAN_POINT('Ctrl Pts',(-10.6017142931267,15.2,4.1313481232904));
#253814=CARTESIAN_POINT('Ctrl Pts',(-10.6053696673683,15.2,4.13112985929873));
#253815=CARTESIAN_POINT('Ctrl Pts',(-10.6090316220411,15.2,4.13090696522989));
#253816=CARTESIAN_POINT('Ctrl Pts',(-10.6127001210486,15.2,4.13067941731066));
#253817=CARTESIAN_POINT('Ctrl Pts',(-10.6163686200562,15.2,4.13045186939144));
#253818=CARTESIAN_POINT('Ctrl Pts',(-10.6200436651988,15.2,4.13021966794241));
#253819=CARTESIAN_POINT('Ctrl Pts',(-10.6237252199808,15.2,4.12998278853499));
#253820=CARTESIAN_POINT('Ctrl Pts',(-10.6274067754316,15.2,4.12974590908453));
#253821=CARTESIAN_POINT('Ctrl Pts',(-10.6310948415843,15.2,4.12950435154942));
#253822=CARTESIAN_POINT('Ctrl Pts',(-10.6347893840804,15.2,4.12925809267966));
#253823=CARTESIAN_POINT('Ctrl Pts',(-10.6384839259054,15.2,4.12901183385464));
#253824=CARTESIAN_POINT('Ctrl Pts',(-10.6421849448551,15.2,4.12876087559652));
#253825=CARTESIAN_POINT('Ctrl Pts',(-10.6458924065959,15.2,4.12850519168874));
#253826=CARTESIAN_POINT('Ctrl Pts',(-10.6508356886925,15.2,4.12816427982717));
#253827=CARTESIAN_POINT('Ctrl Pts',(-10.6557904256494,15.2,4.12781496884533));
#253828=CARTESIAN_POINT('Ctrl Pts',(-10.6607565320461,15.2,4.12745720230189));
#253829=CARTESIAN_POINT('Ctrl Pts',(-10.6644811120128,15.2,4.12718887738212));
#253830=CARTESIAN_POINT('Ctrl Pts',(-10.6682120879886,15.2,4.12691579564985));
#253831=CARTESIAN_POINT('Ctrl Pts',(-10.6719494262269,15.2,4.12663793478559));
#253832=CARTESIAN_POINT('Ctrl Pts',(-10.6756867651442,15.2,4.12636007387086));
#253833=CARTESIAN_POINT('Ctrl Pts',(-10.6794304658883,15.2,4.12607743384645));
#253834=CARTESIAN_POINT('Ctrl Pts',(-10.6831804988509,15.2,4.12578999438735));
#253835=CARTESIAN_POINT('Ctrl Pts',(-10.6881805416655,15.2,4.12540674186226));
#253836=CARTESIAN_POINT('Ctrl Pts',(-10.6931918433981,15.2,4.12501495888548));
#253837=CARTESIAN_POINT('Ctrl Pts',(-10.6982143165979,15.2,4.12461458497433));
#253838=CARTESIAN_POINT('Ctrl Pts',(-10.7019811716688,15.2,4.12431430452734));
#253839=CARTESIAN_POINT('Ctrl Pts',(-10.7057543081181,15.2,4.12400919123026));
#253840=CARTESIAN_POINT('Ctrl Pts',(-10.7095336880022,15.2,4.12369921830994));
#253841=CARTESIAN_POINT('Ctrl Pts',(-10.7145728616387,15.2,4.1232859210453));
#253842=CARTESIAN_POINT('Ctrl Pts',(-10.7196231286485,15.2,4.12286398219));
#253843=CARTESIAN_POINT('Ctrl Pts',(-10.7246844434413,15.2,4.12243337145863));
#253844=CARTESIAN_POINT('Ctrl Pts',(-10.7284804291911,15.2,4.12211041343944));
#253845=CARTESIAN_POINT('Ctrl Pts',(-10.7322826323082,15.2,4.12178257906042));
#253846=CARTESIAN_POINT('Ctrl Pts',(-10.7360910480001,15.2,4.12144986899998));
#253847=CARTESIAN_POINT('Ctrl Pts',(-9.55499537100006,12.2,4.04260911699998));
#253848=CARTESIAN_POINT('Ctrl Pts',(-9.55669455126496,12.2,4.04316130806102));
#253849=CARTESIAN_POINT('Ctrl Pts',(-9.55844976571224,12.2,4.0437260538932));
#253850=CARTESIAN_POINT('Ctrl Pts',(-9.56026027810168,12.2,4.04430244593684));
#253851=CARTESIAN_POINT('Ctrl Pts',(-9.56207952169703,12.2,4.04488161763427));
#253852=CARTESIAN_POINT('Ctrl Pts',(-9.563954601157,12.2,4.04547254503639));
#253853=CARTESIAN_POINT('Ctrl Pts',(-9.56588480694515,12.2,4.04607433301654));
#253854=CARTESIAN_POINT('Ctrl Pts',(-9.56781501255799,12.2,4.04667612094203));
#253855=CARTESIAN_POINT('Ctrl Pts',(-9.56980034124075,12.2,4.04728876912259));
#253856=CARTESIAN_POINT('Ctrl Pts',(-9.57184010199996,12.2,4.04791140626663));
#253857=CARTESIAN_POINT('Ctrl Pts',(-9.57387986275916,12.2,4.04853404341067));
#253858=CARTESIAN_POINT('Ctrl Pts',(-9.57597405465781,12.2,4.04916667292137));
#253859=CARTESIAN_POINT('Ctrl Pts',(-9.57812199976731,12.2,4.04980844817958));
#253860=CARTESIAN_POINT('Ctrl Pts',(-9.5802699450719,12.2,4.05045022349609));
#253861=CARTESIAN_POINT('Ctrl Pts',(-9.58247164646092,12.2,4.05110114611867));
#253862=CARTESIAN_POINT('Ctrl Pts',(-9.58472644050408,12.2,4.05176039932183));
#253863=CARTESIAN_POINT('Ctrl Pts',(-9.58698123434243,12.2,4.05241965246511));
#253864=CARTESIAN_POINT('Ctrl Pts',(-9.58928912240927,12.2,4.05308723561338));
#253865=CARTESIAN_POINT('Ctrl Pts',(-9.59164945950104,12.2,4.05376235400861));
#253866=CARTESIAN_POINT('Ctrl Pts',(-9.59400979659281,12.2,4.05443747240384));
#253867=CARTESIAN_POINT('Ctrl Pts',(-9.59642258392434,12.2,4.05512012772111));
#253868=CARTESIAN_POINT('Ctrl Pts',(-9.59888719166586,12.2,4.05580954919576));
#253869=CARTESIAN_POINT('Ctrl Pts',(-9.60135179963124,12.2,4.05649897073303));
#253870=CARTESIAN_POINT('Ctrl Pts',(-9.60386822553645,12.2,4.05719515850451));
#253871=CARTESIAN_POINT('Ctrl Pts',(-9.60643585601319,12.2,4.05789736304318));
#253872=CARTESIAN_POINT('Ctrl Pts',(-9.60900348625671,12.2,4.05859956751808));
#253873=CARTESIAN_POINT('Ctrl Pts',(-9.61162232335711,12.2,4.05930778842291));
#253874=CARTESIAN_POINT('Ctrl Pts',(-9.614291761429,12.2,4.06002130098055));
#253875=CARTESIAN_POINT('Ctrl Pts',(-9.61696119950089,12.2,4.06073481353819));
#253876=CARTESIAN_POINT('Ctrl Pts',(-9.61968124038537,12.2,4.06145361467873));
#253877=CARTESIAN_POINT('Ctrl Pts',(-9.62245129461588,12.2,4.06217699940224));
#253878=CARTESIAN_POINT('Ctrl Pts',(-9.62568302471922,12.2,4.06302094829014));
#253879=CARTESIAN_POINT('Ctrl Pts',(-9.6289828284303,12.2,4.06387113444311));
#253880=CARTESIAN_POINT('Ctrl Pts',(-9.63234979270746,12.2,4.06472646678995));
#253881=CARTESIAN_POINT('Ctrl Pts',(-9.63523576193808,12.2,4.06545960876348));
#253882=CARTESIAN_POINT('Ctrl Pts',(-9.63817107189807,12.2,4.06619653327835));
#253883=CARTESIAN_POINT('Ctrl Pts',(-9.64115516212088,12.2,4.06693657316799));
#253884=CARTESIAN_POINT('Ctrl Pts',(-9.64413925234367,12.2,4.06767661305763));
#253885=CARTESIAN_POINT('Ctrl Pts',(-9.64717212177936,12.2,4.0684197680043));
#253886=CARTESIAN_POINT('Ctrl Pts',(-9.65025321916415,12.2,4.06916539089371));
#253887=CARTESIAN_POINT('Ctrl Pts',(-9.65384783296631,12.2,4.07003528430984));
#253888=CARTESIAN_POINT('Ctrl Pts',(-9.65750809002614,12.2,4.07090853182331));
#253889=CARTESIAN_POINT('Ctrl Pts',(-9.66123313152617,12.2,4.07178413743409));
#253890=CARTESIAN_POINT('Ctrl Pts',(-9.66442602436478,12.2,4.07253465655826));
#253891=CARTESIAN_POINT('Ctrl Pts',(-9.66766651597591,12.2,4.07328690653263));
#253892=CARTESIAN_POINT('Ctrl Pts',(-9.67095407582499,12.2,4.07404027482377));
#253893=CARTESIAN_POINT('Ctrl Pts',(-9.67424163537545,12.2,4.07479364304648));
#253894=CARTESIAN_POINT('Ctrl Pts',(-9.67757626506359,12.2,4.07554813017687));
#253895=CARTESIAN_POINT('Ctrl Pts',(-9.68095744269278,12.2,4.07630313756613));
#253896=CARTESIAN_POINT('Ctrl Pts',(-9.68433862032196,12.2,4.07705814495539));
#253897=CARTESIAN_POINT('Ctrl Pts',(-9.68776634813906,12.2,4.07781367415292));
#253898=CARTESIAN_POINT('Ctrl Pts',(-9.69124011651085,12.2,4.07856914145881));
#253899=CARTESIAN_POINT('Ctrl Pts',(-9.69471388488263,12.2,4.0793246087647));
#253900=CARTESIAN_POINT('Ctrl Pts',(-9.69823369312732,12.2,4.08008001414509));
#253901=CARTESIAN_POINT('Ctrl Pts',(-9.70179904066136,12.2,4.08083479145105));
#253902=CARTESIAN_POINT('Ctrl Pts',(-9.70536438851924,12.2,4.08158956882556));
#253903=CARTESIAN_POINT('Ctrl Pts',(-9.70897527616608,12.2,4.08234371540028));
#253904=CARTESIAN_POINT('Ctrl Pts',(-9.71263121019966,12.2,4.0830966797744));
#253905=CARTESIAN_POINT('Ctrl Pts',(-9.71628714390117,12.2,4.08384964408013));
#253906=CARTESIAN_POINT('Ctrl Pts',(-9.7199881264841,12.2,4.08460142377348));
#253907=CARTESIAN_POINT('Ctrl Pts',(-9.72373367119828,12.2,4.08535148024965));
#253908=CARTESIAN_POINT('Ctrl Pts',(-9.72747921591246,12.2,4.08610153672581));
#253909=CARTESIAN_POINT('Ctrl Pts',(-9.7312693250577,12.2,4.08684986869563));
#253910=CARTESIAN_POINT('Ctrl Pts',(-9.73510352258207,12.2,4.08759594916867));
#253911=CARTESIAN_POINT('Ctrl Pts',(-9.73957675325933,12.2,4.08846637643239));
#253912=CARTESIAN_POINT('Ctrl Pts',(-9.74410999118372,12.2,4.0893337384545));
#253913=CARTESIAN_POINT('Ctrl Pts',(-9.7487024962482,12.2,4.09019721724965));
#253914=CARTESIAN_POINT('Ctrl Pts',(-9.75198285695747,12.2,4.09081398780802));
#253915=CARTESIAN_POINT('Ctrl Pts',(-9.7552934555722,12.2,4.0914287778111));
#253916=CARTESIAN_POINT('Ctrl Pts',(-9.75863402626664,12.2,4.09204129753332));
#253917=CARTESIAN_POINT('Ctrl Pts',(-9.76197459696108,12.2,4.09265381725555));
#253918=CARTESIAN_POINT('Ctrl Pts',(-9.76534514075853,12.2,4.09326406450868));
#253919=CARTESIAN_POINT('Ctrl Pts',(-9.76874539251017,12.2,4.09387175673366));
#253920=CARTESIAN_POINT('Ctrl Pts',(-9.77214564426181,12.2,4.09447944895863));
#253921=CARTESIAN_POINT('Ctrl Pts',(-9.77557560612487,12.2,4.09508458471173));
#253922=CARTESIAN_POINT('Ctrl Pts',(-9.77903501779307,12.2,4.0956868845727));
#253923=CARTESIAN_POINT('Ctrl Pts',(-9.78318631164409,12.2,4.0964096443796));
#253924=CARTESIAN_POINT('Ctrl Pts',(-9.78738001350006,12.2,4.09712831947848));
#253925=CARTESIAN_POINT('Ctrl Pts',(-9.791615681261,12.2,4.09784243820272));
#253926=CARTESIAN_POINT('Ctrl Pts',(-9.79514540452336,12.2,4.09843753716122));
#253927=CARTESIAN_POINT('Ctrl Pts',(-9.79870427072626,12.2,4.09902947286921));
#253928=CARTESIAN_POINT('Ctrl Pts',(-9.80229202671468,12.2,4.09961797377467));
#253929=CARTESIAN_POINT('Ctrl Pts',(-9.80587978270311,12.2,4.10020647468013));
#253930=CARTESIAN_POINT('Ctrl Pts',(-9.80949643110553,12.2,4.10079154381111));
#253931=CARTESIAN_POINT('Ctrl Pts',(-9.81314171950832,12.2,4.10137291624166));
#253932=CARTESIAN_POINT('Ctrl Pts',(-9.81678700791111,12.2,4.10195428867222));
#253933=CARTESIAN_POINT('Ctrl Pts',(-9.82046093836287,12.2,4.1025319657866));
#253934=CARTESIAN_POINT('Ctrl Pts',(-9.82416326351867,12.2,4.10310568752531));
#253935=CARTESIAN_POINT('Ctrl Pts',(-9.82786558867447,12.2,4.10367940926402));
#253936=CARTESIAN_POINT('Ctrl Pts',(-9.83159630951673,12.2,4.1042491775094));
#253937=CARTESIAN_POINT('Ctrl Pts',(-9.83535518125433,12.2,4.10481473674529));
#253938=CARTESIAN_POINT('Ctrl Pts',(-9.83911405299192,12.2,4.10538029598118));
#253939=CARTESIAN_POINT('Ctrl Pts',(-9.84290107681485,12.2,4.10594164723106));
#253940=CARTESIAN_POINT('Ctrl Pts',(-9.84671601098299,12.2,4.10649854132806));
#253941=CARTESIAN_POINT('Ctrl Pts',(-9.85053094515113,12.2,4.10705543542506));
#253942=CARTESIAN_POINT('Ctrl Pts',(-9.85437378940413,12.2,4.10760787110875));
#253943=CARTESIAN_POINT('Ctrl Pts',(-9.85824430793272,12.2,4.10815560683023));
#253944=CARTESIAN_POINT('Ctrl Pts',(-9.86211482646132,12.2,4.10870334255171));
#253945=CARTESIAN_POINT('Ctrl Pts',(-9.86601301707236,12.2,4.10924637444301));
#253946=CARTESIAN_POINT('Ctrl Pts',(-9.86993864554681,12.2,4.10978446534538));
#253947=CARTESIAN_POINT('Ctrl Pts',(-9.87386427402126,12.2,4.11032255624775));
#253948=CARTESIAN_POINT('Ctrl Pts',(-9.87781733930727,12.2,4.11085570441391));
#253949=CARTESIAN_POINT('Ctrl Pts',(-9.88179761021228,12.2,4.11138367455239));
#253950=CARTESIAN_POINT('Ctrl Pts',(-9.8857778811173,12.2,4.11191164469086));
#253951=CARTESIAN_POINT('Ctrl Pts',(-9.88978535688662,12.2,4.11243443668478));
#253952=CARTESIAN_POINT('Ctrl Pts',(-9.8938198070277,12.2,4.11295181855934));
#253953=CARTESIAN_POINT('Ctrl Pts',(-9.89785425672904,12.2,4.11346920037751));
#253954=CARTESIAN_POINT('Ctrl Pts',(-9.90191568062972,12.2,4.11398117306071));
#253955=CARTESIAN_POINT('Ctrl Pts',(-9.90600385122359,12.2,4.1144875072421));
#253956=CARTESIAN_POINT('Ctrl Pts',(-9.91009202226308,12.2,4.11499384147868));
#253957=CARTESIAN_POINT('Ctrl Pts',(-9.91420694039377,12.2,4.11549453827923));
#253958=CARTESIAN_POINT('Ctrl Pts',(-9.9183483789333,12.2,4.11598937196027));
#253959=CARTESIAN_POINT('Ctrl Pts',(-9.92166152994549,12.2,4.11638523892668));
#253960=CARTESIAN_POINT('Ctrl Pts',(-9.92499165519351,12.2,4.11677735483291));
#253961=CARTESIAN_POINT('Ctrl Pts',(-9.92833863950227,12.2,4.11716560696693));
#253962=CARTESIAN_POINT('Ctrl Pts',(-9.93168562335501,12.2,4.11755385904805));
#253963=CARTESIAN_POINT('Ctrl Pts',(-9.93504946587814,12.2,4.11793824593794));
#253964=CARTESIAN_POINT('Ctrl Pts',(-9.93843005498894,12.2,4.1183186579628));
#253965=CARTESIAN_POINT('Ctrl Pts',(-9.94181064456033,12.2,4.11869907003949));
#253966=CARTESIAN_POINT('Ctrl Pts',(-9.94520797852505,12.2,4.11907550509082));
#253967=CARTESIAN_POINT('Ctrl Pts',(-9.94862194626665,12.2,4.11944785600001));
#253968=CARTESIAN_POINT('Ctrl Pts',(-9.95203591400825,12.2,4.11982020690919));
#253969=CARTESIAN_POINT('Ctrl Pts',(-9.95546651591849,12.2,4.12018847229845));
#253970=CARTESIAN_POINT('Ctrl Pts',(-9.95891363833028,12.2,4.12055254381786));
#253971=CARTESIAN_POINT('Ctrl Pts',(-9.96236076027238,12.2,4.12091661528767));
#253972=CARTESIAN_POINT('Ctrl Pts',(-9.96582440471358,12.2,4.1212764925022));
#253973=CARTESIAN_POINT('Ctrl Pts',(-9.96930445872263,12.2,4.12163206997476));
#253974=CARTESIAN_POINT('Ctrl Pts',(-9.97278451320583,12.2,4.12198764749577));
#253975=CARTESIAN_POINT('Ctrl Pts',(-9.97628097979512,12.2,4.12233892314937));
#253976=CARTESIAN_POINT('Ctrl Pts',(-9.97979374559934,12.2,4.12268579405672));
#253977=CARTESIAN_POINT('Ctrl Pts',(-9.98330651092493,12.2,4.1230326649168));
#253978=CARTESIAN_POINT('Ctrl Pts',(-9.98683557849843,12.2,4.12337512996355));
#253979=CARTESIAN_POINT('Ctrl Pts',(-9.99038083648532,12.2,4.123713084214));
#253980=CARTESIAN_POINT('Ctrl Pts',(-9.99392609495527,12.2,4.12405103851049));
#253981=CARTESIAN_POINT('Ctrl Pts',(-9.99748754557189,12.2,4.12438448274153));
#253982=CARTESIAN_POINT('Ctrl Pts',(-10.0010650795025,12.2,4.1247133149977));
#253983=CARTESIAN_POINT('Ctrl Pts',(-10.0046426129457,12.2,4.12504214720907));
#253984=CARTESIAN_POINT('Ctrl Pts',(-10.0082362295234,12.2,4.12536636738021));
#253985=CARTESIAN_POINT('Ctrl Pts',(-10.0118458226717,12.2,4.1256858729655));
#253986=CARTESIAN_POINT('Ctrl Pts',(-10.0154554163118,12.2,4.12600537859433));
#253987=CARTESIAN_POINT('Ctrl Pts',(-10.0190809846733,12.2,4.12632016930872));
#253988=CARTESIAN_POINT('Ctrl Pts',(-10.0227224230395,12.2,4.12663014699197));
#253989=CARTESIAN_POINT('Ctrl Pts',(-10.0263638609095,12.2,4.12694012463298));
#253990=CARTESIAN_POINT('Ctrl Pts',(-10.0300211666797,12.2,4.12724528935442));
#253991=CARTESIAN_POINT('Ctrl Pts',(-10.0336942374504,12.2,4.12754554045641));
#253992=CARTESIAN_POINT('Ctrl Pts',(-10.0373673087216,12.2,4.12784579159931));
#253993=CARTESIAN_POINT('Ctrl Pts',(-10.0410561424917,12.2,4.1281411322582));
#253994=CARTESIAN_POINT('Ctrl Pts',(-10.0447606348613,12.2,4.12843146127369));
#253995=CARTESIAN_POINT('Ctrl Pts',(-10.0484651267262,12.2,4.12872179024963));
#253996=CARTESIAN_POINT('Ctrl Pts',(-10.0521852758934,12.2,4.12900711006824));
#253997=CARTESIAN_POINT('Ctrl Pts',(-10.0559209791976,12.2,4.12928732321252));
#253998=CARTESIAN_POINT('Ctrl Pts',(-10.0596566830107,12.2,4.12956753639498));
#253999=CARTESIAN_POINT('Ctrl Pts',(-10.063407940344,12.2,4.12984264448427));
#254000=CARTESIAN_POINT('Ctrl Pts',(-10.0671746475109,12.2,4.13011255150019));
#254001=CARTESIAN_POINT('Ctrl Pts',(-10.0709413541646,12.2,4.13038245847933));
#254002=CARTESIAN_POINT('Ctrl Pts',(-10.074723511955,12.2,4.13064716511437));
#254003=CARTESIAN_POINT('Ctrl Pts',(-10.0785210159208,12.2,4.13090657748259));
#254004=CARTESIAN_POINT('Ctrl Pts',(-10.082318520404,12.2,4.13116598988616));
#254005=CARTESIAN_POINT('Ctrl Pts',(-10.0861313716025,12.2,4.13142010798645));
#254006=CARTESIAN_POINT('Ctrl Pts',(-10.0899594680333,12.2,4.131668839));
#254007=CARTESIAN_POINT('Ctrl Pts',(-10.0937875644642,12.2,4.13191757001356));
#254008=CARTESIAN_POINT('Ctrl Pts',(-10.0976309055024,12.2,4.13216091429871));
#254009=CARTESIAN_POINT('Ctrl Pts',(-10.1014893893809,12.2,4.13239878075556));
#254010=CARTESIAN_POINT('Ctrl Pts',(-10.1053478727336,12.2,4.13263664718));
#254011=CARTESIAN_POINT('Ctrl Pts',(-10.1092215005477,12.2,4.13286903568402));
#254012=CARTESIAN_POINT('Ctrl Pts',(-10.1131101692473,12.2,4.13309585599985));
#254013=CARTESIAN_POINT('Ctrl Pts',(-10.1179710055193,12.2,4.13337938141782));
#254014=CARTESIAN_POINT('Ctrl Pts',(-10.1228553458,12.2,4.13365420734445));
#254015=CARTESIAN_POINT('Ctrl Pts',(-10.1277629937167,12.2,4.13392015873334));
#254016=CARTESIAN_POINT('Ctrl Pts',(-10.131689112264,12.2,4.13413291985605));
#254017=CARTESIAN_POINT('Ctrl Pts',(-10.135630148663,12.2,4.13434000255865));
#254018=CARTESIAN_POINT('Ctrl Pts',(-10.1395860018801,12.2,4.13454131829125));
#254019=CARTESIAN_POINT('Ctrl Pts',(-10.1435418545583,12.2,4.13474263399643));
#254020=CARTESIAN_POINT('Ctrl Pts',(-10.1475125248495,12.2,4.13493818303673));
#254021=CARTESIAN_POINT('Ctrl Pts',(-10.151497914764,12.2,4.13512787946654));
#254022=CARTESIAN_POINT('Ctrl Pts',(-10.1554833052214,12.2,4.13531757592221));
#254023=CARTESIAN_POINT('Ctrl Pts',(-10.1594834128,12.2,4.13550141822278));
#254024=CARTESIAN_POINT('Ctrl Pts',(-10.1634981426314,12.2,4.13567932328743));
#254025=CARTESIAN_POINT('Ctrl Pts',(-10.1675128719158,12.2,4.13585722832783));
#254026=CARTESIAN_POINT('Ctrl Pts',(-10.1715422215122,12.2,4.13602919448845));
#254027=CARTESIAN_POINT('Ctrl Pts',(-10.1755860947362,12.2,4.13619513825305));
#254028=CARTESIAN_POINT('Ctrl Pts',(-10.1796299685112,12.2,4.13636108204027));
#254029=CARTESIAN_POINT('Ctrl Pts',(-10.1836883649963,12.2,4.13652100236288));
#254030=CARTESIAN_POINT('Ctrl Pts',(-10.1877611876081,12.2,4.13667481753753));
#254031=CARTESIAN_POINT('Ctrl Pts',(-10.191834009665,12.2,4.13682863269122));
#254032=CARTESIAN_POINT('Ctrl Pts',(-10.1959212582477,12.2,4.13697634268618));
#254033=CARTESIAN_POINT('Ctrl Pts',(-10.2000228376716,12.2,4.13711786373777));
#254034=CARTESIAN_POINT('Ctrl Pts',(-10.2041244176543,12.2,4.13725938480864));
#254035=CARTESIAN_POINT('Ctrl Pts',(-10.2082403270979,12.2,4.1373947164761));
#254036=CARTESIAN_POINT('Ctrl Pts',(-10.2123704703794,12.2,4.1375237802605));
#254037=CARTESIAN_POINT('Ctrl Pts',(-10.2165006130983,12.2,4.13765284402732));
#254038=CARTESIAN_POINT('Ctrl Pts',(-10.2206449894421,12.2,4.13777563780373));
#254039=CARTESIAN_POINT('Ctrl Pts',(-10.2248035060451,12.2,4.1378920817393));
#254040=CARTESIAN_POINT('Ctrl Pts',(-10.2289620232147,12.2,4.13800852569074));
#254041=CARTESIAN_POINT('Ctrl Pts',(-10.2331346783889,12.2,4.13811862086342));
#254042=CARTESIAN_POINT('Ctrl Pts',(-10.2373213789695,12.2,4.13822228725841));
#254043=CARTESIAN_POINT('Ctrl Pts',(-10.2415080789797,12.2,4.13832595363928));
#254044=CARTESIAN_POINT('Ctrl Pts',(-10.245708824143,12.2,4.13842319065304));
#254045=CARTESIAN_POINT('Ctrl Pts',(-10.2499235188526,12.2,4.13851392053517));
#254046=CARTESIAN_POINT('Ctrl Pts',(-10.2541382141364,12.2,4.13860465042967));
#254047=CARTESIAN_POINT('Ctrl Pts',(-10.2583668596688,12.2,4.13868887374023));
#254048=CARTESIAN_POINT('Ctrl Pts',(-10.2626093622333,12.2,4.13876651230001));
#254049=CARTESIAN_POINT('Ctrl Pts',(-10.2668518647979,12.2,4.1388441508598));
#254050=CARTESIAN_POINT('Ctrl Pts',(-10.2711082249529,12.2,4.13891520451882));
#254051=CARTESIAN_POINT('Ctrl Pts',(-10.2753783489648,12.2,4.13897959774387));
#254052=CARTESIAN_POINT('Ctrl Pts',(-10.2796484723949,12.2,4.13904399096014));
#254053=CARTESIAN_POINT('Ctrl Pts',(-10.2839323604123,12.2,4.13910172428722));
#254054=CARTESIAN_POINT('Ctrl Pts',(-10.2882299197471,12.2,4.13915272028331));
#254055=CARTESIAN_POINT('Ctrl Pts',(-10.2925274796674,12.2,4.13920371628634));
#254056=CARTESIAN_POINT('Ctrl Pts',(-10.2968387104395,12.2,4.1392479765159));
#254057=CARTESIAN_POINT('Ctrl Pts',(-10.3011635217321,12.2,4.13928542573946));
#254058=CARTESIAN_POINT('Ctrl Pts',(-10.3054883324355,12.2,4.13932287495793));
#254059=CARTESIAN_POINT('Ctrl Pts',(-10.309826722951,12.2,4.13935351379117));
#254060=CARTESIAN_POINT('Ctrl Pts',(-10.3141786015944,12.2,4.13937726828967));
#254061=CARTESIAN_POINT('Ctrl Pts',(-10.3185304808307,12.2,4.13940102279141));
#254062=CARTESIAN_POINT('Ctrl Pts',(-10.322895849013,12.2,4.13941789275098));
#254063=CARTESIAN_POINT('Ctrl Pts',(-10.3272746151938,12.2,4.13942780475142));
#254064=CARTESIAN_POINT('Ctrl Pts',(-10.331653380778,12.2,4.13943771675049));
#254065=CARTESIAN_POINT('Ctrl Pts',(-10.336045542401,12.2,4.13944067167726));
#254066=CARTESIAN_POINT('Ctrl Pts',(-10.3404510123733,12.2,4.13943659823361));
#254067=CARTESIAN_POINT('Ctrl Pts',(-10.3459578502889,12.2,4.13943150642863));
#254068=CARTESIAN_POINT('Ctrl Pts',(-10.3514854804939,12.2,4.1394154319567));
#254069=CARTESIAN_POINT('Ctrl Pts',(-10.3570337276456,12.2,4.13938823452673));
#254070=CARTESIAN_POINT('Ctrl Pts',(-10.3603626758157,12.2,4.13937191606934));
#254071=CARTESIAN_POINT('Ctrl Pts',(-10.3636990465084,12.2,4.13935159478789));
#254072=CARTESIAN_POINT('Ctrl Pts',(-10.3670428018865,12.2,4.13932723974635));
#254073=CARTESIAN_POINT('Ctrl Pts',(-10.3703865572645,12.2,4.13930288470483));
#254074=CARTESIAN_POINT('Ctrl Pts',(-10.3737376973076,12.2,4.13927449562202));
#254075=CARTESIAN_POINT('Ctrl Pts',(-10.3770961839762,12.2,4.13924204499875));
#254076=CARTESIAN_POINT('Ctrl Pts',(-10.3804546712549,12.2,4.13920959436959));
#254077=CARTESIAN_POINT('Ctrl Pts',(-10.3838205053108,12.2,4.13917308028095));
#254078=CARTESIAN_POINT('Ctrl Pts',(-10.387193649552,12.2,4.13913247523283));
#254079=CARTESIAN_POINT('Ctrl Pts',(-10.3905667931805,12.2,4.13909187019208));
#254080=CARTESIAN_POINT('Ctrl Pts',(-10.3939472461585,12.2,4.13904717392654));
#254081=CARTESIAN_POINT('Ctrl Pts',(-10.3973349713694,12.2,4.13899835646962));
#254082=CARTESIAN_POINT('Ctrl Pts',(-10.4018519381121,12.2,4.13893326653002));
#254083=CARTESIAN_POINT('Ctrl Pts',(-10.4063818328503,12.2,4.13886085272782));
#254084=CARTESIAN_POINT('Ctrl Pts',(-10.4109245703159,12.2,4.13878104478656));
#254085=CARTESIAN_POINT('Ctrl Pts',(-10.4143316235698,12.2,4.13872118882789));
#254086=CARTESIAN_POINT('Ctrl Pts',(-10.4177458988961,12.2,4.13865717497849));
#254087=CARTESIAN_POINT('Ctrl Pts',(-10.4211673605625,12.2,4.13858897448154));
#254088=CARTESIAN_POINT('Ctrl Pts',(-10.4245888228504,12.2,4.1385207739722));
#254089=CARTESIAN_POINT('Ctrl Pts',(-10.4280174714154,12.2,4.13844838704502));
#254090=CARTESIAN_POINT('Ctrl Pts',(-10.431453269249,12.2,4.13837178549164));
#254091=CARTESIAN_POINT('Ctrl Pts',(-10.4360343319869,12.2,4.13826965011034));
#254092=CARTESIAN_POINT('Ctrl Pts',(-10.440628104103,12.2,4.13816002099669));
#254093=CARTESIAN_POINT('Ctrl Pts',(-10.445234500115,12.2,4.13804283495119));
#254094=CARTESIAN_POINT('Ctrl Pts',(-10.4486892972809,12.2,4.13795494541308));
#254095=CARTESIAN_POINT('Ctrl Pts',(-10.4521511950325,12.2,4.13786280475278));
#254096=CARTESIAN_POINT('Ctrl Pts',(-10.4556201573706,12.2,4.13776638479363));
#254097=CARTESIAN_POINT('Ctrl Pts',(-10.4590891197087,12.2,4.13766996483448));
#254098=CARTESIAN_POINT('Ctrl Pts',(-10.4625651457516,12.2,4.13756926663517));
#254099=CARTESIAN_POINT('Ctrl Pts',(-10.466048199499,12.2,4.1374642617229));
#254100=CARTESIAN_POINT('Ctrl Pts',(-10.4695312538793,12.2,4.13735925679156));
#254101=CARTESIAN_POINT('Ctrl Pts',(-10.4730213366699,12.2,4.13724994679234));
#254102=CARTESIAN_POINT('Ctrl Pts',(-10.4765184110124,12.2,4.13713630373357));
#254103=CARTESIAN_POINT('Ctrl Pts',(-10.4800154847196,12.2,4.13702266069544));
#254104=CARTESIAN_POINT('Ctrl Pts',(-10.4835195502098,12.2,4.13690468453255));
#254105=CARTESIAN_POINT('Ctrl Pts',(-10.4870305714162,12.2,4.13678234903661));
#254106=CARTESIAN_POINT('Ctrl Pts',(-10.491711932812,12.2,4.13661923504944));
#254107=CARTESIAN_POINT('Ctrl Pts',(-10.4964056595068,12.2,4.13644837097509));
#254108=CARTESIAN_POINT('Ctrl Pts',(-10.5011116678005,12.2,4.13626969375923));
#254109=CARTESIAN_POINT('Ctrl Pts',(-10.5046411741811,12.2,4.13613568584125));
#254110=CARTESIAN_POINT('Ctrl Pts',(-10.5081775884739,12.2,4.13599728387535));
#254111=CARTESIAN_POINT('Ctrl Pts',(-10.5117208747192,12.2,4.13585446050615));
#254112=CARTESIAN_POINT('Ctrl Pts',(-10.5152641616082,12.2,4.13571163711099));
#254113=CARTESIAN_POINT('Ctrl Pts',(-10.5188143214076,12.2,4.1355643943896));
#254114=CARTESIAN_POINT('Ctrl Pts',(-10.5223713172588,12.2,4.13541270395028));
#254115=CARTESIAN_POINT('Ctrl Pts',(-10.5271139773168,12.2,4.13521045007712));
#254116=CARTESIAN_POINT('Ctrl Pts',(-10.5318687919454,12.2,4.13500029019664));
#254117=CARTESIAN_POINT('Ctrl Pts',(-10.5366356761104,12.2,4.13478216549277));
#254118=CARTESIAN_POINT('Ctrl Pts',(-10.5402108393966,12.2,4.13461857195744));
#254119=CARTESIAN_POINT('Ctrl Pts',(-10.5437927925323,12.2,4.13445049773075));
#254120=CARTESIAN_POINT('Ctrl Pts',(-10.5473814997343,12.2,4.13427791682097));
#254121=CARTESIAN_POINT('Ctrl Pts',(-10.5509702075883,12.2,4.13410533587983));
#254122=CARTESIAN_POINT('Ctrl Pts',(-10.5545656688775,12.2,4.13392824992077));
#254123=CARTESIAN_POINT('Ctrl Pts',(-10.558167849777,12.2,4.13374663147709));
#254124=CARTESIAN_POINT('Ctrl Pts',(-10.561770030022,12.2,4.1335650130664));
#254125=CARTESIAN_POINT('Ctrl Pts',(-10.5653789302329,12.2,4.13337886333287));
#254126=CARTESIAN_POINT('Ctrl Pts',(-10.5689945136996,12.2,4.13318815824641));
#254127=CARTESIAN_POINT('Ctrl Pts',(-10.5738152914363,12.2,4.13293388480935));
#254128=CARTESIAN_POINT('Ctrl Pts',(-10.578647952187,12.2,4.13267151039107));
#254129=CARTESIAN_POINT('Ctrl Pts',(-10.5834924128458,12.2,4.13240097724706));
#254130=CARTESIAN_POINT('Ctrl Pts',(-10.5871257585048,12.2,4.13219807737983));
#254131=CARTESIAN_POINT('Ctrl Pts',(-10.5907657411051,12.2,4.13199058847125));
#254132=CARTESIAN_POINT('Ctrl Pts',(-10.5944123272634,12.2,4.13177848606292));
#254133=CARTESIAN_POINT('Ctrl Pts',(-10.5980589140841,12.2,4.13156638361606));
#254134=CARTESIAN_POINT('Ctrl Pts',(-10.6017121028984,12.2,4.13134966840122));
#254135=CARTESIAN_POINT('Ctrl Pts',(-10.6053718607645,12.2,4.13112831495176));
#254136=CARTESIAN_POINT('Ctrl Pts',(-10.6090316179658,12.2,4.1309069615425));
#254137=CARTESIAN_POINT('Ctrl Pts',(-10.6126979430099,12.2,4.13068097014236));
#254138=CARTESIAN_POINT('Ctrl Pts',(-10.6163708019357,12.2,4.13045031718034));
#254139=CARTESIAN_POINT('Ctrl Pts',(-10.6200436608615,12.2,4.13021966421833));
#254140=CARTESIAN_POINT('Ctrl Pts',(-10.6237230535852,12.2,4.12998434946547));
#254141=CARTESIAN_POINT('Ctrl Pts',(-10.6274089448685,12.2,4.12974434897378));
#254142=CARTESIAN_POINT('Ctrl Pts',(-10.6323234663564,12.2,4.12942434833273));
#254143=CARTESIAN_POINT('Ctrl Pts',(-10.6372495424059,12.2,4.12909601684613));
#254144=CARTESIAN_POINT('Ctrl Pts',(-10.6421870925011,12.2,4.12875930159673));
#254145=CARTESIAN_POINT('Ctrl Pts',(-10.6458902559134,12.2,4.12850676510234));
#254146=CARTESIAN_POINT('Ctrl Pts',(-10.6495998736025,12.2,4.12824951111496));
#254147=CARTESIAN_POINT('Ctrl Pts',(-10.6533159110185,12.2,4.12798751715956));
#254148=CARTESIAN_POINT('Ctrl Pts',(-10.6595093051365,12.2,4.1275508606783));
#254149=CARTESIAN_POINT('Ctrl Pts',(-10.6657205296157,12.2,4.12710103619236));
#254150=CARTESIAN_POINT('Ctrl Pts',(-10.6719494262269,12.2,4.12663793478559));
#254151=CARTESIAN_POINT('Ctrl Pts',(-10.6769325443307,12.2,4.1262674535996));
#254152=CARTESIAN_POINT('Ctrl Pts',(-10.6819269728883,12.2,4.12588847646003));
#254153=CARTESIAN_POINT('Ctrl Pts',(-10.6869326397167,12.2,4.12550095455002));
#254154=CARTESIAN_POINT('Ctrl Pts',(-10.690686889497,12.2,4.12521031314391));
#254155=CARTESIAN_POINT('Ctrl Pts',(-10.6944474615269,12.2,4.12491486542134));
#254156=CARTESIAN_POINT('Ctrl Pts',(-10.6982143165979,12.2,4.12461458497433));
#254157=CARTESIAN_POINT('Ctrl Pts',(-10.7019811716688,12.2,4.12431430452733));
#254158=CARTESIAN_POINT('Ctrl Pts',(-10.7057543081181,12.2,4.12400919123026));
#254159=CARTESIAN_POINT('Ctrl Pts',(-10.7095336880022,12.2,4.12369921830994));
#254160=CARTESIAN_POINT('Ctrl Pts',(-10.7133130678863,12.2,4.12338924538962));
#254161=CARTESIAN_POINT('Ctrl Pts',(-10.717098688862,12.2,4.12307441270743));
#254162=CARTESIAN_POINT('Ctrl Pts',(-10.7208905289317,12.2,4.12275470459471));
#254163=CARTESIAN_POINT('Ctrl Pts',(-10.7259463161506,12.2,4.12232842707236));
#254164=CARTESIAN_POINT('Ctrl Pts',(-10.7310131599497,12.2,4.12189348245419));
#254165=CARTESIAN_POINT('Ctrl Pts',(-10.7360910480001,12.2,4.12144986899998));
#254166=CARTESIAN_POINT('Ctrl Pts',(-10.8675859440001,15.2,3.76106045599998));
#254167=CARTESIAN_POINT('Ctrl Pts',(-10.8675859440001,11.6,3.76106045599998));
#254168=CARTESIAN_POINT('Ctrl Pts',(-10.8670460920001,15.2,3.76051902299999));
#254169=CARTESIAN_POINT('Ctrl Pts',(-10.8670460920001,11.6,3.76051902299999));
#254170=CARTESIAN_POINT('Ctrl Pts',(-10.8659664940001,15.2,3.75943667499998));
#254171=CARTESIAN_POINT('Ctrl Pts',(-10.8659664940001,11.6,3.75943667499998));
#254172=CARTESIAN_POINT('Ctrl Pts',(-10.8643474220001,15.2,3.75781469799998));
#254173=CARTESIAN_POINT('Ctrl Pts',(-10.8643474220001,11.6,3.75781469799998));
#254174=CARTESIAN_POINT('Ctrl Pts',(-10.8621893020001,15.2,3.75565515599998));
#254175=CARTESIAN_POINT('Ctrl Pts',(-10.8621893020001,11.6,3.75565515599998));
#254176=CARTESIAN_POINT('Ctrl Pts',(-10.8594927310001,15.2,3.75296088399999));
#254177=CARTESIAN_POINT('Ctrl Pts',(-10.8594927310001,11.6,3.75296088399998));
#254178=CARTESIAN_POINT('Ctrl Pts',(-10.8567972360001,15.2,3.75027176899999));
#254179=CARTESIAN_POINT('Ctrl Pts',(-10.8567972360001,11.6,3.75027176899999));
#254180=CARTESIAN_POINT('Ctrl Pts',(-10.8541028210001,15.2,3.74758780899998));
#254181=CARTESIAN_POINT('Ctrl Pts',(-10.8541028210001,11.6,3.74758780899998));
#254182=CARTESIAN_POINT('Ctrl Pts',(-10.8514094910001,15.2,3.74490900599999));
#254183=CARTESIAN_POINT('Ctrl Pts',(-10.8514094910001,11.6,3.74490900599999));
#254184=CARTESIAN_POINT('Ctrl Pts',(-10.8487172500001,15.2,3.74223536099999));
#254185=CARTESIAN_POINT('Ctrl Pts',(-10.8487172500001,11.6,3.74223536099999));
#254186=CARTESIAN_POINT('Ctrl Pts',(-10.8460261070001,15.2,3.73956687399998));
#254187=CARTESIAN_POINT('Ctrl Pts',(-10.8460261070001,11.6,3.73956687399998));
#254188=CARTESIAN_POINT('Ctrl Pts',(-10.8433360710001,15.2,3.73690354799999));
#254189=CARTESIAN_POINT('Ctrl Pts',(-10.8433360710001,11.6,3.73690354799999));
#254190=CARTESIAN_POINT('Ctrl Pts',(-10.8406471530001,15.2,3.73424538199998));
#254191=CARTESIAN_POINT('Ctrl Pts',(-10.8406471530001,11.6,3.73424538199998));
#254192=CARTESIAN_POINT('Ctrl Pts',(-10.8379593660001,15.2,3.73159237899999));
#254193=CARTESIAN_POINT('Ctrl Pts',(-10.8379593660001,11.6,3.73159237899999));
#254194=CARTESIAN_POINT('Ctrl Pts',(-10.8352727180001,15.2,3.72894453799999));
#254195=CARTESIAN_POINT('Ctrl Pts',(-10.8352727180001,11.6,3.72894453799999));
#254196=CARTESIAN_POINT('Ctrl Pts',(-10.8325872200001,15.2,3.72630186199999));
#254197=CARTESIAN_POINT('Ctrl Pts',(-10.8325872200001,11.6,3.72630186199999));
#254198=CARTESIAN_POINT('Ctrl Pts',(-10.8299028840001,15.2,3.72366435199999));
#254199=CARTESIAN_POINT('Ctrl Pts',(-10.8299028840001,11.6,3.72366435199999));
#254200=CARTESIAN_POINT('Ctrl Pts',(-10.8272197160001,15.2,3.72103200799998));
#254201=CARTESIAN_POINT('Ctrl Pts',(-10.8272197160001,11.6,3.72103200799998));
#254202=CARTESIAN_POINT('Ctrl Pts',(-10.8245377250001,15.2,3.71840482999998));
#254203=CARTESIAN_POINT('Ctrl Pts',(-10.8245377250001,11.6,3.71840482999998));
#254204=CARTESIAN_POINT('Ctrl Pts',(-10.8218569190001,15.2,3.71578282199999));
#254205=CARTESIAN_POINT('Ctrl Pts',(-10.8218569190001,11.6,3.71578282199999));
#254206=CARTESIAN_POINT('Ctrl Pts',(-10.8191773060001,15.2,3.71316598199999));
#254207=CARTESIAN_POINT('Ctrl Pts',(-10.8191773060001,11.6,3.71316598199999));
#254208=CARTESIAN_POINT('Ctrl Pts',(-10.8164988950001,15.2,3.71055431199999));
#254209=CARTESIAN_POINT('Ctrl Pts',(-10.8164988950001,11.6,3.71055431199998));
#254210=CARTESIAN_POINT('Ctrl Pts',(-10.8138216940001,15.2,3.70794781399999));
#254211=CARTESIAN_POINT('Ctrl Pts',(-10.8138216940001,11.6,3.70794781399999));
#254212=CARTESIAN_POINT('Ctrl Pts',(-10.8111457130001,15.2,3.70534648599998));
#254213=CARTESIAN_POINT('Ctrl Pts',(-10.8111457130001,11.6,3.70534648599998));
#254214=CARTESIAN_POINT('Ctrl Pts',(-10.8084709620001,15.2,3.70275033099999));
#254215=CARTESIAN_POINT('Ctrl Pts',(-10.8084709620001,11.6,3.70275033099999));
#254216=CARTESIAN_POINT('Ctrl Pts',(-10.8057974490001,15.2,3.70015935099998));
#254217=CARTESIAN_POINT('Ctrl Pts',(-10.8057974490001,11.6,3.70015935099998));
#254218=CARTESIAN_POINT('Ctrl Pts',(-10.8031251850001,15.2,3.69757354499999));
#254219=CARTESIAN_POINT('Ctrl Pts',(-10.8031251850001,11.6,3.69757354499999));
#254220=CARTESIAN_POINT('Ctrl Pts',(-10.8004541780001,15.2,3.69499291399999));
#254221=CARTESIAN_POINT('Ctrl Pts',(-10.8004541780001,11.6,3.69499291399999));
#254222=CARTESIAN_POINT('Ctrl Pts',(-10.7977844380001,15.2,3.69241746099998));
#254223=CARTESIAN_POINT('Ctrl Pts',(-10.7977844380001,11.6,3.69241746099998));
#254224=CARTESIAN_POINT('Ctrl Pts',(-10.7951159740001,15.2,3.68984718499998));
#254225=CARTESIAN_POINT('Ctrl Pts',(-10.7951159740001,11.6,3.68984718499998));
#254226=CARTESIAN_POINT('Ctrl Pts',(-10.7924487950001,15.2,3.68728208699999));
#254227=CARTESIAN_POINT('Ctrl Pts',(-10.7924487950001,11.6,3.68728208699999));
#254228=CARTESIAN_POINT('Ctrl Pts',(-10.7897829100001,15.2,3.68472216799999));
#254229=CARTESIAN_POINT('Ctrl Pts',(-10.7897829100001,11.6,3.68472216799999));
#254230=CARTESIAN_POINT('Ctrl Pts',(-10.7871183270001,15.2,3.68216742999999));
#254231=CARTESIAN_POINT('Ctrl Pts',(-10.7871183270001,11.6,3.68216742999999));
#254232=CARTESIAN_POINT('Ctrl Pts',(-10.7844550570001,15.2,3.67961787199999));
#254233=CARTESIAN_POINT('Ctrl Pts',(-10.7844550570001,11.6,3.67961787199999));
#254234=CARTESIAN_POINT('Ctrl Pts',(-10.7817931080001,15.2,3.67707349599999));
#254235=CARTESIAN_POINT('Ctrl Pts',(-10.7817931080001,11.6,3.67707349599998));
#254236=CARTESIAN_POINT('Ctrl Pts',(-10.7791324900001,15.2,3.67453430299998));
#254237=CARTESIAN_POINT('Ctrl Pts',(-10.7791324900001,11.6,3.67453430299998));
#254238=CARTESIAN_POINT('Ctrl Pts',(-10.7764732120001,15.2,3.67200029299998));
#254239=CARTESIAN_POINT('Ctrl Pts',(-10.7764732120001,11.6,3.67200029299998));
#254240=CARTESIAN_POINT('Ctrl Pts',(-10.7738152830001,15.2,3.66947146699999));
#254241=CARTESIAN_POINT('Ctrl Pts',(-10.7738152830001,11.6,3.66947146699999));
#254242=CARTESIAN_POINT('Ctrl Pts',(-10.7711587130001,15.2,3.66694782799998));
#254243=CARTESIAN_POINT('Ctrl Pts',(-10.7711587130001,11.6,3.66694782799998));
#254244=CARTESIAN_POINT('Ctrl Pts',(-10.7685035120001,15.2,3.66442937399999));
#254245=CARTESIAN_POINT('Ctrl Pts',(-10.7685035120001,11.6,3.66442937399999));
#254246=CARTESIAN_POINT('Ctrl Pts',(-10.7658496880001,15.2,3.66191610799999));
#254247=CARTESIAN_POINT('Ctrl Pts',(-10.7658496880001,11.6,3.66191610799999));
#254248=CARTESIAN_POINT('Ctrl Pts',(-10.7631972500001,15.2,3.65940802799999));
#254249=CARTESIAN_POINT('Ctrl Pts',(-10.7631972500001,11.6,3.65940802799999));
#254250=CARTESIAN_POINT('Ctrl Pts',(-10.7605462090001,15.2,3.65690513799999));
#254251=CARTESIAN_POINT('Ctrl Pts',(-10.7605462090001,11.6,3.65690513799999));
#254252=CARTESIAN_POINT('Ctrl Pts',(-10.7578965730001,15.2,3.65440743699998));
#254253=CARTESIAN_POINT('Ctrl Pts',(-10.7578965730001,11.6,3.65440743699998));
#254254=CARTESIAN_POINT('Ctrl Pts',(-10.7552483530001,15.2,3.65191492699999));
#254255=CARTESIAN_POINT('Ctrl Pts',(-10.7552483530001,11.6,3.65191492699999));
#254256=CARTESIAN_POINT('Ctrl Pts',(-10.7526015570001,15.2,3.64942760599998));
#254257=CARTESIAN_POINT('Ctrl Pts',(-10.7526015570001,11.6,3.64942760599998));
#254258=CARTESIAN_POINT('Ctrl Pts',(-10.7499561940001,15.2,3.64694547899998));
#254259=CARTESIAN_POINT('Ctrl Pts',(-10.7499561940001,11.6,3.64694547899998));
#254260=CARTESIAN_POINT('Ctrl Pts',(-10.7473122750001,15.2,3.64446854399999));
#254261=CARTESIAN_POINT('Ctrl Pts',(-10.7473122750001,11.6,3.64446854399999));
#254262=CARTESIAN_POINT('Ctrl Pts',(-10.7446698090001,15.2,3.64199680199999));
#254263=CARTESIAN_POINT('Ctrl Pts',(-10.7446698090001,11.6,3.64199680199999));
#254264=CARTESIAN_POINT('Ctrl Pts',(-10.7420288050001,15.2,3.63953025399999));
#254265=CARTESIAN_POINT('Ctrl Pts',(-10.7420288050001,11.6,3.63953025399999));
#254266=CARTESIAN_POINT('Ctrl Pts',(-10.7393892730001,15.2,3.63706890199998));
#254267=CARTESIAN_POINT('Ctrl Pts',(-10.7393892730001,11.6,3.63706890199998));
#254268=CARTESIAN_POINT('Ctrl Pts',(-10.7367512220001,15.2,3.63461274599998));
#254269=CARTESIAN_POINT('Ctrl Pts',(-10.7367512220001,11.6,3.63461274599998));
#254270=CARTESIAN_POINT('Ctrl Pts',(-10.7341146620001,15.2,3.63216178499999));
#254271=CARTESIAN_POINT('Ctrl Pts',(-10.7341146620001,11.6,3.63216178499999));
#254272=CARTESIAN_POINT('Ctrl Pts',(-10.7314796030001,15.2,3.62971602199998));
#254273=CARTESIAN_POINT('Ctrl Pts',(-10.7314796030001,11.6,3.62971602199998));
#254274=CARTESIAN_POINT('Ctrl Pts',(-10.7288460530001,15.2,3.62727545699999));
#254275=CARTESIAN_POINT('Ctrl Pts',(-10.7288460530001,11.6,3.62727545699998));
#254276=CARTESIAN_POINT('Ctrl Pts',(-10.7262140240001,15.2,3.62484009099998));
#254277=CARTESIAN_POINT('Ctrl Pts',(-10.7262140240001,11.6,3.62484009099998));
#254278=CARTESIAN_POINT('Ctrl Pts',(-10.7235835250001,15.2,3.62240992399999));
#254279=CARTESIAN_POINT('Ctrl Pts',(-10.7235835250001,11.6,3.62240992399998));
#254280=CARTESIAN_POINT('Ctrl Pts',(-10.7209545640001,15.2,3.61998495799998));
#254281=CARTESIAN_POINT('Ctrl Pts',(-10.7209545640001,11.6,3.61998495799998));
#254282=CARTESIAN_POINT('Ctrl Pts',(-10.7183271510001,15.2,3.61756519299998));
#254283=CARTESIAN_POINT('Ctrl Pts',(-10.7183271510001,11.6,3.61756519299998));
#254284=CARTESIAN_POINT('Ctrl Pts',(-10.7157012970001,15.2,3.61515062899999));
#254285=CARTESIAN_POINT('Ctrl Pts',(-10.7157012970001,11.6,3.61515062899999));
#254286=CARTESIAN_POINT('Ctrl Pts',(-10.7130770100001,15.2,3.61274126799999));
#254287=CARTESIAN_POINT('Ctrl Pts',(-10.7130770100001,11.6,3.61274126799999));
#254288=CARTESIAN_POINT('Ctrl Pts',(-10.7104543020001,15.2,3.61033710899999));
#254289=CARTESIAN_POINT('Ctrl Pts',(-10.7104543020001,11.6,3.61033710899999));
#254290=CARTESIAN_POINT('Ctrl Pts',(-10.7078331810001,15.2,3.60793815499999));
#254291=CARTESIAN_POINT('Ctrl Pts',(-10.7078331810001,11.6,3.60793815499999));
#254292=CARTESIAN_POINT('Ctrl Pts',(-10.7052136580001,15.2,3.60554440499998));
#254293=CARTESIAN_POINT('Ctrl Pts',(-10.7052136580001,11.6,3.60554440499998));
#254294=CARTESIAN_POINT('Ctrl Pts',(-10.7025957410001,15.2,3.60315585999999));
#254295=CARTESIAN_POINT('Ctrl Pts',(-10.7025957410001,11.6,3.60315585999999));
#254296=CARTESIAN_POINT('Ctrl Pts',(-10.6999794400001,15.2,3.60077252099998));
#254297=CARTESIAN_POINT('Ctrl Pts',(-10.6999794400001,11.6,3.60077252099998));
#254298=CARTESIAN_POINT('Ctrl Pts',(-10.6973647670001,15.2,3.59839438899999));
#254299=CARTESIAN_POINT('Ctrl Pts',(-10.6973647670001,11.6,3.59839438899999));
#254300=CARTESIAN_POINT('Ctrl Pts',(-10.6947517300001,15.2,3.59602146299999));
#254301=CARTESIAN_POINT('Ctrl Pts',(-10.6947517300001,11.6,3.59602146299998));
#254302=CARTESIAN_POINT('Ctrl Pts',(-10.6921403400001,15.2,3.59365374499999));
#254303=CARTESIAN_POINT('Ctrl Pts',(-10.6921403400001,11.6,3.59365374499998));
#254304=CARTESIAN_POINT('Ctrl Pts',(-10.6895306050001,15.2,3.59129123499999));
#254305=CARTESIAN_POINT('Ctrl Pts',(-10.6895306050001,11.6,3.59129123499999));
#254306=CARTESIAN_POINT('Ctrl Pts',(-10.6869225370001,15.2,3.58893393499999));
#254307=CARTESIAN_POINT('Ctrl Pts',(-10.6869225370001,11.6,3.58893393499999));
#254308=CARTESIAN_POINT('Ctrl Pts',(-10.6843161440001,15.2,3.58658184499999));
#254309=CARTESIAN_POINT('Ctrl Pts',(-10.6843161440001,11.6,3.58658184499998));
#254310=CARTESIAN_POINT('Ctrl Pts',(-10.6817114370001,15.2,3.58423496499999));
#254311=CARTESIAN_POINT('Ctrl Pts',(-10.6817114370001,11.6,3.58423496499999));
#254312=CARTESIAN_POINT('Ctrl Pts',(-10.6791084260001,15.2,3.58189329599998));
#254313=CARTESIAN_POINT('Ctrl Pts',(-10.6791084260001,11.6,3.58189329599998));
#254314=CARTESIAN_POINT('Ctrl Pts',(-10.6765071210001,15.2,3.57955683899998));
#254315=CARTESIAN_POINT('Ctrl Pts',(-10.6765071210001,11.6,3.57955683899998));
#254316=CARTESIAN_POINT('Ctrl Pts',(-10.6739075300001,15.2,3.57722559299999));
#254317=CARTESIAN_POINT('Ctrl Pts',(-10.6739075300001,11.6,3.57722559299999));
#254318=CARTESIAN_POINT('Ctrl Pts',(-10.6713096660001,15.2,3.57489956099998));
#254319=CARTESIAN_POINT('Ctrl Pts',(-10.6713096660001,11.6,3.57489956099998));
#254320=CARTESIAN_POINT('Ctrl Pts',(-10.6687135380001,15.2,3.57257874199998));
#254321=CARTESIAN_POINT('Ctrl Pts',(-10.6687135380001,11.6,3.57257874199998));
#254322=CARTESIAN_POINT('Ctrl Pts',(-10.6661191560001,15.2,3.57026313699999));
#254323=CARTESIAN_POINT('Ctrl Pts',(-10.6661191560001,11.6,3.57026313699999));
#254324=CARTESIAN_POINT('Ctrl Pts',(-10.6635265280001,15.2,3.56795274599998));
#254325=CARTESIAN_POINT('Ctrl Pts',(-10.6635265280001,11.6,3.56795274599998));
#254326=CARTESIAN_POINT('Ctrl Pts',(-10.6609356680001,15.2,3.56564757199998));
#254327=CARTESIAN_POINT('Ctrl Pts',(-10.6609356680001,11.6,3.56564757199998));
#254328=CARTESIAN_POINT('Ctrl Pts',(-10.6583465820001,15.2,3.56334761199999));
#254329=CARTESIAN_POINT('Ctrl Pts',(-10.6583465820001,11.6,3.56334761199999));
#254330=CARTESIAN_POINT('Ctrl Pts',(-10.6557592820001,15.2,3.56105286799998));
#254331=CARTESIAN_POINT('Ctrl Pts',(-10.6557592820001,11.6,3.56105286799998));
#254332=CARTESIAN_POINT('Ctrl Pts',(-10.6531737790001,15.2,3.55876334199999));
#254333=CARTESIAN_POINT('Ctrl Pts',(-10.6531737790001,11.6,3.55876334199999));
#254334=CARTESIAN_POINT('Ctrl Pts',(-10.6505900820001,15.2,3.55647903299998));
#254335=CARTESIAN_POINT('Ctrl Pts',(-10.6505900820001,11.6,3.55647903299998));
#254336=CARTESIAN_POINT('Ctrl Pts',(-10.6480082030001,15.2,3.55419994099999));
#254337=CARTESIAN_POINT('Ctrl Pts',(-10.6480082030001,11.6,3.55419994099999));
#254338=CARTESIAN_POINT('Ctrl Pts',(-10.6454281490001,15.2,3.55192606799999));
#254339=CARTESIAN_POINT('Ctrl Pts',(-10.6454281490001,11.6,3.55192606799999));
#254340=CARTESIAN_POINT('Ctrl Pts',(-10.6428499330001,15.2,3.54965741499999));
#254341=CARTESIAN_POINT('Ctrl Pts',(-10.6428499330001,11.6,3.54965741499999));
#254342=CARTESIAN_POINT('Ctrl Pts',(-10.6402735620001,15.2,3.54739398099999));
#254343=CARTESIAN_POINT('Ctrl Pts',(-10.6402735620001,11.6,3.54739398099999));
#254344=CARTESIAN_POINT('Ctrl Pts',(-10.6376990500001,15.2,3.54513576599999));
#254345=CARTESIAN_POINT('Ctrl Pts',(-10.6376990500001,11.6,3.54513576599999));
#254346=CARTESIAN_POINT('Ctrl Pts',(-10.6351264060001,15.2,3.54288277199998));
#254347=CARTESIAN_POINT('Ctrl Pts',(-10.6351264060001,11.6,3.54288277199998));
#254348=CARTESIAN_POINT('Ctrl Pts',(-10.6325556390001,15.2,3.54063499899999));
#254349=CARTESIAN_POINT('Ctrl Pts',(-10.6325556390001,11.6,3.54063499899999));
#254350=CARTESIAN_POINT('Ctrl Pts',(-10.6299867610001,15.2,3.53839244699999));
#254351=CARTESIAN_POINT('Ctrl Pts',(-10.6299867610001,11.6,3.53839244699999));
#254352=CARTESIAN_POINT('Ctrl Pts',(-10.6274197800001,15.2,3.53615511799998));
#254353=CARTESIAN_POINT('Ctrl Pts',(-10.6274197800001,11.6,3.53615511799998));
#254354=CARTESIAN_POINT('Ctrl Pts',(-10.6248547090001,15.2,3.53392300999998));
#254355=CARTESIAN_POINT('Ctrl Pts',(-10.6248547090001,11.6,3.53392300999998));
#254356=CARTESIAN_POINT('Ctrl Pts',(-10.6222915560001,15.2,3.53169612599999));
#254357=CARTESIAN_POINT('Ctrl Pts',(-10.6222915560001,11.6,3.53169612599999));
#254358=CARTESIAN_POINT('Ctrl Pts',(-10.6197303340001,15.2,3.52947446499999));
#254359=CARTESIAN_POINT('Ctrl Pts',(-10.6197303340001,11.6,3.52947446499999));
#254360=CARTESIAN_POINT('Ctrl Pts',(-10.6171710520001,15.2,3.52725802799998));
#254361=CARTESIAN_POINT('Ctrl Pts',(-10.6171710520001,11.6,3.52725802799998));
#254362=CARTESIAN_POINT('Ctrl Pts',(-10.6146137200001,15.2,3.52504681499998));
#254363=CARTESIAN_POINT('Ctrl Pts',(-10.6146137200001,11.6,3.52504681499998));
#254364=CARTESIAN_POINT('Ctrl Pts',(-10.6120583480001,15.2,3.52284082599999));
#254365=CARTESIAN_POINT('Ctrl Pts',(-10.6120583480001,11.6,3.52284082599999));
#254366=CARTESIAN_POINT('Ctrl Pts',(-10.6095049490001,15.2,3.52064006199999));
#254367=CARTESIAN_POINT('Ctrl Pts',(-10.6095049490001,11.6,3.52064006199999));
#254368=CARTESIAN_POINT('Ctrl Pts',(-10.6069535310001,15.2,3.51844452499999));
#254369=CARTESIAN_POINT('Ctrl Pts',(-10.6069535310001,11.6,3.51844452499999));
#254370=CARTESIAN_POINT('Ctrl Pts',(-10.6044041060001,15.2,3.51625421299998));
#254371=CARTESIAN_POINT('Ctrl Pts',(-10.6044041060001,11.6,3.51625421299998));
#254372=CARTESIAN_POINT('Ctrl Pts',(-10.6018566830001,15.2,3.51406912799998));
#254373=CARTESIAN_POINT('Ctrl Pts',(-10.6018566830001,11.6,3.51406912799998));
#254374=CARTESIAN_POINT('Ctrl Pts',(-10.5993112740001,15.2,3.51188926799999));
#254375=CARTESIAN_POINT('Ctrl Pts',(-10.5993112740001,11.6,3.51188926799999));
#254376=CARTESIAN_POINT('Ctrl Pts',(-10.5967678890001,15.2,3.50971463699998));
#254377=CARTESIAN_POINT('Ctrl Pts',(-10.5967678890001,11.6,3.50971463699998));
#254378=CARTESIAN_POINT('Ctrl Pts',(-10.5942265380001,15.2,3.50754523199999));
#254379=CARTESIAN_POINT('Ctrl Pts',(-10.5942265380001,11.6,3.50754523199999));
#254380=CARTESIAN_POINT('Ctrl Pts',(-10.5916872330001,15.2,3.50538105599998));
#254381=CARTESIAN_POINT('Ctrl Pts',(-10.5916872330001,11.6,3.50538105599998));
#254382=CARTESIAN_POINT('Ctrl Pts',(-10.5891499840001,15.2,3.50322210699999));
#254383=CARTESIAN_POINT('Ctrl Pts',(-10.5891499840001,11.6,3.50322210699999));
#254384=CARTESIAN_POINT('Ctrl Pts',(-10.5866148010001,15.2,3.50106838699999));
#254385=CARTESIAN_POINT('Ctrl Pts',(-10.5866148010001,11.6,3.50106838699999));
#254386=CARTESIAN_POINT('Ctrl Pts',(-10.5840816950001,15.2,3.49891989599998));
#254387=CARTESIAN_POINT('Ctrl Pts',(-10.5840816950001,11.6,3.49891989599998));
#254388=CARTESIAN_POINT('Ctrl Pts',(-10.5815506770001,15.2,3.49677663499998));
#254389=CARTESIAN_POINT('Ctrl Pts',(-10.5815506770001,11.6,3.49677663499998));
#254390=CARTESIAN_POINT('Ctrl Pts',(-10.5790217580001,15.2,3.49463860299998));
#254391=CARTESIAN_POINT('Ctrl Pts',(-10.5790217580001,11.6,3.49463860299998));
#254392=CARTESIAN_POINT('Ctrl Pts',(-10.5764949480001,15.2,3.49250580099999));
#254393=CARTESIAN_POINT('Ctrl Pts',(-10.5764949480001,11.6,3.49250580099999));
#254394=CARTESIAN_POINT('Ctrl Pts',(-10.5739702580001,15.2,3.49037822899999));
#254395=CARTESIAN_POINT('Ctrl Pts',(-10.5739702580001,11.6,3.49037822899999));
#254396=CARTESIAN_POINT('Ctrl Pts',(-10.5714477000001,15.2,3.48825588799999));
#254397=CARTESIAN_POINT('Ctrl Pts',(-10.5714477000001,11.6,3.48825588799999));
#254398=CARTESIAN_POINT('Ctrl Pts',(-10.5689272830001,15.2,3.48613877799998));
#254399=CARTESIAN_POINT('Ctrl Pts',(-10.5689272830001,11.6,3.48613877799998));
#254400=CARTESIAN_POINT('Ctrl Pts',(-10.5664090190001,15.2,3.48402689799999));
#254401=CARTESIAN_POINT('Ctrl Pts',(-10.5664090190001,11.6,3.48402689799999));
#254402=CARTESIAN_POINT('Ctrl Pts',(-10.5638929170001,15.2,3.48192024999998));
#254403=CARTESIAN_POINT('Ctrl Pts',(-10.5638929170001,11.6,3.48192024999998));
#254404=CARTESIAN_POINT('Ctrl Pts',(-10.5613789900001,15.2,3.47981883399999));
#254405=CARTESIAN_POINT('Ctrl Pts',(-10.5613789900001,11.6,3.47981883399999));
#254406=CARTESIAN_POINT('Ctrl Pts',(-10.5588672490001,15.2,3.47772264899999));
#254407=CARTESIAN_POINT('Ctrl Pts',(-10.5588672490001,11.6,3.47772264899999));
#254408=CARTESIAN_POINT('Ctrl Pts',(-10.5563577040001,15.2,3.47563169699999));
#254409=CARTESIAN_POINT('Ctrl Pts',(-10.5563577040001,11.6,3.47563169699999));
#254410=CARTESIAN_POINT('Ctrl Pts',(-10.5538503660001,15.2,3.47354597799999));
#254411=CARTESIAN_POINT('Ctrl Pts',(-10.5538503660001,11.6,3.47354597799999));
#254412=CARTESIAN_POINT('Ctrl Pts',(-10.5513452450001,15.2,3.47146549099998));
#254413=CARTESIAN_POINT('Ctrl Pts',(-10.5513452450001,11.6,3.47146549099998));
#254414=CARTESIAN_POINT('Ctrl Pts',(-10.5488423530001,15.2,3.46939023799998));
#254415=CARTESIAN_POINT('Ctrl Pts',(-10.5488423530001,11.6,3.46939023799998));
#254416=CARTESIAN_POINT('Ctrl Pts',(-10.5463417020001,15.2,3.46732021699999));
#254417=CARTESIAN_POINT('Ctrl Pts',(-10.5463417020001,11.6,3.46732021699999));
#254418=CARTESIAN_POINT('Ctrl Pts',(-10.5438433010001,15.2,3.46525543099999));
#254419=CARTESIAN_POINT('Ctrl Pts',(-10.5438433010001,11.6,3.46525543099998));
#254420=CARTESIAN_POINT('Ctrl Pts',(-10.5413471640001,15.2,3.46319587699998));
#254421=CARTESIAN_POINT('Ctrl Pts',(-10.5413471640001,11.6,3.46319587699998));
#254422=CARTESIAN_POINT('Ctrl Pts',(-10.5388532990001,15.2,3.46114155699999));
#254423=CARTESIAN_POINT('Ctrl Pts',(-10.5388532990001,11.6,3.46114155699999));
#254424=CARTESIAN_POINT('Ctrl Pts',(-10.5363617170001,15.2,3.45909247099998));
#254425=CARTESIAN_POINT('Ctrl Pts',(-10.5363617170001,11.6,3.45909247099998));
#254426=CARTESIAN_POINT('Ctrl Pts',(-10.5338724320001,15.2,3.45704862099999));
#254427=CARTESIAN_POINT('Ctrl Pts',(-10.5338724320001,11.6,3.45704862099998));
#254428=CARTESIAN_POINT('Ctrl Pts',(-10.5313854540001,15.2,3.45501000399998));
#254429=CARTESIAN_POINT('Ctrl Pts',(-10.5313854540001,11.6,3.45501000399998));
#254430=CARTESIAN_POINT('Ctrl Pts',(-10.5289007930001,15.2,3.45297662099998));
#254431=CARTESIAN_POINT('Ctrl Pts',(-10.5289007930001,11.6,3.45297662099998));
#254432=CARTESIAN_POINT('Ctrl Pts',(-10.5264184600001,15.2,3.45094847299999));
#254433=CARTESIAN_POINT('Ctrl Pts',(-10.5264184600001,11.6,3.45094847299999));
#254434=CARTESIAN_POINT('Ctrl Pts',(-10.5239384690001,15.2,3.44892556099998));
#254435=CARTESIAN_POINT('Ctrl Pts',(-10.5239384690001,11.6,3.44892556099998));
#254436=CARTESIAN_POINT('Ctrl Pts',(-10.5214608280001,15.2,3.44690788299998));
#254437=CARTESIAN_POINT('Ctrl Pts',(-10.5214608280001,11.6,3.44690788299998));
#254438=CARTESIAN_POINT('Ctrl Pts',(-10.5189855500001,15.2,3.44489544099999));
#254439=CARTESIAN_POINT('Ctrl Pts',(-10.5189855500001,11.6,3.44489544099999));
#254440=CARTESIAN_POINT('Ctrl Pts',(-10.5165126460001,15.2,3.44288823299999));
#254441=CARTESIAN_POINT('Ctrl Pts',(-10.5165126460001,11.6,3.44288823299999));
#254442=CARTESIAN_POINT('Ctrl Pts',(-10.5140421270001,15.2,3.44088626199999));
#254443=CARTESIAN_POINT('Ctrl Pts',(-10.5140421270001,11.6,3.44088626199999));
#254444=CARTESIAN_POINT('Ctrl Pts',(-10.5115740050001,15.2,3.43888952499999));
#254445=CARTESIAN_POINT('Ctrl Pts',(-10.5115740050001,11.6,3.43888952499999));
#254446=CARTESIAN_POINT('Ctrl Pts',(-10.5091082900001,15.2,3.43689802399999));
#254447=CARTESIAN_POINT('Ctrl Pts',(-10.5091082900001,11.6,3.43689802399999));
#254448=CARTESIAN_POINT('Ctrl Pts',(-10.5066449960001,15.2,3.43491175999999));
#254449=CARTESIAN_POINT('Ctrl Pts',(-10.5066449960001,11.6,3.43491175999999));
#254450=CARTESIAN_POINT('Ctrl Pts',(-10.5041841310001,15.2,3.43293073099999));
#254451=CARTESIAN_POINT('Ctrl Pts',(-10.5041841310001,11.6,3.43293073099999));
#254452=CARTESIAN_POINT('Ctrl Pts',(-10.5017257090001,15.2,3.43095493799999));
#254453=CARTESIAN_POINT('Ctrl Pts',(-10.5017257090001,11.6,3.43095493799999));
#254454=CARTESIAN_POINT('Ctrl Pts',(-10.4992697400001,15.2,3.42898438099999));
#254455=CARTESIAN_POINT('Ctrl Pts',(-10.4992697400001,11.6,3.42898438099999));
#254456=CARTESIAN_POINT('Ctrl Pts',(-10.4968162370001,15.2,3.42701905899998));
#254457=CARTESIAN_POINT('Ctrl Pts',(-10.4968162370001,11.6,3.42701905899998));
#254458=CARTESIAN_POINT('Ctrl Pts',(-10.4943652100001,15.2,3.42505897499999));
#254459=CARTESIAN_POINT('Ctrl Pts',(-10.4943652100001,11.6,3.42505897499999));
#254460=CARTESIAN_POINT('Ctrl Pts',(-10.4919166710001,15.2,3.42310412499998));
#254461=CARTESIAN_POINT('Ctrl Pts',(-10.4919166710001,11.6,3.42310412499998));
#254462=CARTESIAN_POINT('Ctrl Pts',(-10.4894706320001,15.2,3.42115451299998));
#254463=CARTESIAN_POINT('Ctrl Pts',(-10.4894706320001,11.6,3.42115451299998));
#254464=CARTESIAN_POINT('Ctrl Pts',(-10.4870271040001,15.2,3.41921013599999));
#254465=CARTESIAN_POINT('Ctrl Pts',(-10.4870271040001,11.6,3.41921013599999));
#254466=CARTESIAN_POINT('Ctrl Pts',(-10.4845861000001,15.2,3.41727099599999));
#254467=CARTESIAN_POINT('Ctrl Pts',(-10.4845861000001,11.6,3.41727099599999));
#254468=CARTESIAN_POINT('Ctrl Pts',(-10.4821476300001,15.2,3.41533709199999));
#254469=CARTESIAN_POINT('Ctrl Pts',(-10.4821476300001,11.6,3.41533709199999));
#254470=CARTESIAN_POINT('Ctrl Pts',(-10.4797117050001,15.2,3.41340842399998));
#254471=CARTESIAN_POINT('Ctrl Pts',(-10.4797117050001,11.6,3.41340842399998));
#254472=CARTESIAN_POINT('Ctrl Pts',(-10.4772783390001,15.2,3.41148499199999));
#254473=CARTESIAN_POINT('Ctrl Pts',(-10.4772783390001,11.6,3.41148499199999));
#254474=CARTESIAN_POINT('Ctrl Pts',(-10.4748475420001,15.2,3.40956679599999));
#254475=CARTESIAN_POINT('Ctrl Pts',(-10.4748475420001,11.6,3.40956679599999));
#254476=CARTESIAN_POINT('Ctrl Pts',(-10.4724193270001,15.2,3.40765383599998));
#254477=CARTESIAN_POINT('Ctrl Pts',(-10.4724193270001,11.6,3.40765383599998));
#254478=CARTESIAN_POINT('Ctrl Pts',(-10.4699937050001,15.2,3.40574611299999));
#254479=CARTESIAN_POINT('Ctrl Pts',(-10.4699937050001,11.6,3.40574611299999));
#254480=CARTESIAN_POINT('Ctrl Pts',(-10.4675706860001,15.2,3.40384362499999));
#254481=CARTESIAN_POINT('Ctrl Pts',(-10.4675706860001,11.6,3.40384362499999));
#254482=CARTESIAN_POINT('Ctrl Pts',(-10.4651502850001,15.2,3.40194637399998));
#254483=CARTESIAN_POINT('Ctrl Pts',(-10.4651502850001,11.6,3.40194637399998));
#254484=CARTESIAN_POINT('Ctrl Pts',(-10.4627325130001,15.2,3.40005435799998));
#254485=CARTESIAN_POINT('Ctrl Pts',(-10.4627325130001,11.6,3.40005435799998));
#254486=CARTESIAN_POINT('Ctrl Pts',(-10.4603173810001,15.2,3.39816757999999));
#254487=CARTESIAN_POINT('Ctrl Pts',(-10.4603173810001,11.6,3.39816757999999));
#254488=CARTESIAN_POINT('Ctrl Pts',(-10.4579049000001,15.2,3.39628603499998));
#254489=CARTESIAN_POINT('Ctrl Pts',(-10.4579049000001,11.6,3.39628603499998));
#254490=CARTESIAN_POINT('Ctrl Pts',(-10.4554950840001,15.2,3.39440972699999));
#254491=CARTESIAN_POINT('Ctrl Pts',(-10.4554950840001,11.6,3.39440972699998));
#254492=CARTESIAN_POINT('Ctrl Pts',(-10.4530879440001,15.2,3.39253865399999));
#254493=CARTESIAN_POINT('Ctrl Pts',(-10.4530879440001,11.6,3.39253865399999));
#254494=CARTESIAN_POINT('Ctrl Pts',(-10.4506834930001,15.2,3.39067281699998));
#254495=CARTESIAN_POINT('Ctrl Pts',(-10.4506834930001,11.6,3.39067281699998));
#254496=CARTESIAN_POINT('Ctrl Pts',(-10.4482817400001,15.2,3.38881221399999));
#254497=CARTESIAN_POINT('Ctrl Pts',(-10.4482817400001,11.6,3.38881221399999));
#254498=CARTESIAN_POINT('Ctrl Pts',(-10.4458827010001,15.2,3.38695684799998));
#254499=CARTESIAN_POINT('Ctrl Pts',(-10.4458827010001,11.6,3.38695684799998));
#254500=CARTESIAN_POINT('Ctrl Pts',(-10.4434863850001,15.2,3.38510671599998));
#254501=CARTESIAN_POINT('Ctrl Pts',(-10.4434863850001,11.6,3.38510671599998));
#254502=CARTESIAN_POINT('Ctrl Pts',(-10.4410928060001,15.2,3.38326181899999));
#254503=CARTESIAN_POINT('Ctrl Pts',(-10.4410928060001,11.6,3.38326181899998));
#254504=CARTESIAN_POINT('Ctrl Pts',(-10.4387019740001,15.2,3.38142215599999));
#254505=CARTESIAN_POINT('Ctrl Pts',(-10.4387019740001,11.6,3.38142215599999));
#254506=CARTESIAN_POINT('Ctrl Pts',(-10.4363139020001,15.2,3.37958772799999));
#254507=CARTESIAN_POINT('Ctrl Pts',(-10.4363139020001,11.6,3.37958772799999));
#254508=CARTESIAN_POINT('Ctrl Pts',(-10.4339286050001,15.2,3.37775853599998));
#254509=CARTESIAN_POINT('Ctrl Pts',(-10.4339286050001,11.6,3.37775853599998));
#254510=CARTESIAN_POINT('Ctrl Pts',(-10.4315460910001,15.2,3.37593457599999));
#254511=CARTESIAN_POINT('Ctrl Pts',(-10.4315460910001,11.6,3.37593457599999));
#254512=CARTESIAN_POINT('Ctrl Pts',(-10.4291663730001,15.2,3.37411585099999));
#254513=CARTESIAN_POINT('Ctrl Pts',(-10.4291663730001,11.6,3.37411585099999));
#254514=CARTESIAN_POINT('Ctrl Pts',(-10.4267894660001,15.2,3.37230235899998));
#254515=CARTESIAN_POINT('Ctrl Pts',(-10.4267894660001,11.6,3.37230235899998));
#254516=CARTESIAN_POINT('Ctrl Pts',(-10.4244153790001,15.2,3.37049410099999));
#254517=CARTESIAN_POINT('Ctrl Pts',(-10.4244153790001,11.6,3.37049410099999));
#254518=CARTESIAN_POINT('Ctrl Pts',(-10.4220441260001,15.2,3.36869107699999));
#254519=CARTESIAN_POINT('Ctrl Pts',(-10.4220441260001,11.6,3.36869107699999));
#254520=CARTESIAN_POINT('Ctrl Pts',(-10.4196757190001,15.2,3.36689328499999));
#254521=CARTESIAN_POINT('Ctrl Pts',(-10.4196757190001,11.6,3.36689328499999));
#254522=CARTESIAN_POINT('Ctrl Pts',(-10.4173101710001,15.2,3.36510072599999));
#254523=CARTESIAN_POINT('Ctrl Pts',(-10.4173101710001,11.6,3.36510072599999));
#254524=CARTESIAN_POINT('Ctrl Pts',(-10.4149474930001,15.2,3.36331339999998));
#254525=CARTESIAN_POINT('Ctrl Pts',(-10.4149474930001,11.6,3.36331339999998));
#254526=CARTESIAN_POINT('Ctrl Pts',(-10.4125876980001,15.2,3.36153130599998));
#254527=CARTESIAN_POINT('Ctrl Pts',(-10.4125876980001,11.6,3.36153130599998));
#254528=CARTESIAN_POINT('Ctrl Pts',(-10.4102307990001,15.2,3.35975444399998));
#254529=CARTESIAN_POINT('Ctrl Pts',(-10.4102307990001,11.6,3.35975444399998));
#254530=CARTESIAN_POINT('Ctrl Pts',(-10.4078768090001,15.2,3.35798281399998));
#254531=CARTESIAN_POINT('Ctrl Pts',(-10.4078768090001,11.6,3.35798281399998));
#254532=CARTESIAN_POINT('Ctrl Pts',(-10.4055257380001,15.2,3.35621641399998));
#254533=CARTESIAN_POINT('Ctrl Pts',(-10.4055257380001,11.6,3.35621641399998));
#254534=CARTESIAN_POINT('Ctrl Pts',(-10.4031776000001,15.2,3.35445524599999));
#254535=CARTESIAN_POINT('Ctrl Pts',(-10.4031776000001,11.6,3.35445524599999));
#254536=CARTESIAN_POINT('Ctrl Pts',(-10.4008324080001,15.2,3.35269930899998));
#254537=CARTESIAN_POINT('Ctrl Pts',(-10.4008324080001,11.6,3.35269930899998));
#254538=CARTESIAN_POINT('Ctrl Pts',(-10.3984901750001,15.2,3.35094860299999));
#254539=CARTESIAN_POINT('Ctrl Pts',(-10.3984901750001,11.6,3.35094860299999));
#254540=CARTESIAN_POINT('Ctrl Pts',(-10.3961509110001,15.2,3.34920312599999));
#254541=CARTESIAN_POINT('Ctrl Pts',(-10.3961509110001,11.6,3.34920312599999));
#254542=CARTESIAN_POINT('Ctrl Pts',(-10.3938146310001,15.2,3.34746287999998));
#254543=CARTESIAN_POINT('Ctrl Pts',(-10.3938146310001,11.6,3.34746287999998));
#254544=CARTESIAN_POINT('Ctrl Pts',(-10.3914813470001,15.2,3.34572786199999));
#254545=CARTESIAN_POINT('Ctrl Pts',(-10.3914813470001,11.6,3.34572786199998));
#254546=CARTESIAN_POINT('Ctrl Pts',(-10.3891510720001,15.2,3.34399807399999));
#254547=CARTESIAN_POINT('Ctrl Pts',(-10.3891510720001,11.6,3.34399807399999));
#254548=CARTESIAN_POINT('Ctrl Pts',(-10.3868238190001,15.2,3.34227351299998));
#254549=CARTESIAN_POINT('Ctrl Pts',(-10.3868238190001,11.6,3.34227351299998));
#254550=CARTESIAN_POINT('Ctrl Pts',(-10.3844995990001,15.2,3.34055418199998));
#254551=CARTESIAN_POINT('Ctrl Pts',(-10.3844995990001,11.6,3.34055418199998));
#254552=CARTESIAN_POINT('Ctrl Pts',(-10.3821784260001,15.2,3.33884007799998));
#254553=CARTESIAN_POINT('Ctrl Pts',(-10.3821784260001,11.6,3.33884007799998));
#254554=CARTESIAN_POINT('Ctrl Pts',(-10.3798603140001,15.2,3.33713120199998));
#254555=CARTESIAN_POINT('Ctrl Pts',(-10.3798603140001,11.6,3.33713120199998));
#254556=CARTESIAN_POINT('Ctrl Pts',(-10.3775452740001,15.2,3.33542755199999));
#254557=CARTESIAN_POINT('Ctrl Pts',(-10.3775452740001,11.6,3.33542755199998));
#254558=CARTESIAN_POINT('Ctrl Pts',(-10.3752333190001,15.2,3.33372912899998));
#254559=CARTESIAN_POINT('Ctrl Pts',(-10.3752333190001,11.6,3.33372912899998));
#254560=CARTESIAN_POINT('Ctrl Pts',(-10.3729244630001,15.2,3.33203593199999));
#254561=CARTESIAN_POINT('Ctrl Pts',(-10.3729244630001,11.6,3.33203593199999));
#254562=CARTESIAN_POINT('Ctrl Pts',(-10.3706187180001,15.2,3.33034796199998));
#254563=CARTESIAN_POINT('Ctrl Pts',(-10.3706187180001,11.6,3.33034796199998));
#254564=CARTESIAN_POINT('Ctrl Pts',(-10.3683160970001,15.2,3.32866521499999));
#254565=CARTESIAN_POINT('Ctrl Pts',(-10.3683160970001,11.6,3.32866521499999));
#254566=CARTESIAN_POINT('Ctrl Pts',(-10.3660166140001,15.2,3.32698769399999));
#254567=CARTESIAN_POINT('Ctrl Pts',(-10.3660166140001,11.6,3.32698769399998));
#254568=CARTESIAN_POINT('Ctrl Pts',(-10.3637202810001,15.2,3.32531539599999));
#254569=CARTESIAN_POINT('Ctrl Pts',(-10.3637202810001,11.6,3.32531539599999));
#254570=CARTESIAN_POINT('Ctrl Pts',(-10.3614271110001,15.2,3.32364832299999));
#254571=CARTESIAN_POINT('Ctrl Pts',(-10.3614271110001,11.6,3.32364832299999));
#254572=CARTESIAN_POINT('Ctrl Pts',(-10.3591371170001,15.2,3.32198647299998));
#254573=CARTESIAN_POINT('Ctrl Pts',(-10.3591371170001,11.6,3.32198647299998));
#254574=CARTESIAN_POINT('Ctrl Pts',(-10.3568503140001,15.2,3.32032984499998));
#254575=CARTESIAN_POINT('Ctrl Pts',(-10.3568503140001,11.6,3.32032984499998));
#254576=CARTESIAN_POINT('Ctrl Pts',(-10.3545667120001,15.2,3.31867843999999));
#254577=CARTESIAN_POINT('Ctrl Pts',(-10.3545667120001,11.6,3.31867843999999));
#254578=CARTESIAN_POINT('Ctrl Pts',(-10.3522863270001,15.2,3.31703225499999));
#254579=CARTESIAN_POINT('Ctrl Pts',(-10.3522863270001,11.6,3.31703225499999));
#254580=CARTESIAN_POINT('Ctrl Pts',(-10.3500091710001,15.2,3.31539129199999));
#254581=CARTESIAN_POINT('Ctrl Pts',(-10.3500091710001,11.6,3.31539129199999));
#254582=CARTESIAN_POINT('Ctrl Pts',(-10.3477352560001,15.2,3.31375554999998));
#254583=CARTESIAN_POINT('Ctrl Pts',(-10.3477352560001,11.6,3.31375554999998));
#254584=CARTESIAN_POINT('Ctrl Pts',(-10.3454645980001,15.2,3.31212502699999));
#254585=CARTESIAN_POINT('Ctrl Pts',(-10.3454645980001,11.6,3.31212502699999));
#254586=CARTESIAN_POINT('Ctrl Pts',(-10.3431972080001,15.2,3.31049972399998));
#254587=CARTESIAN_POINT('Ctrl Pts',(-10.3431972080001,11.6,3.31049972399998));
#254588=CARTESIAN_POINT('Ctrl Pts',(-10.3409331010001,15.2,3.30887963799999));
#254589=CARTESIAN_POINT('Ctrl Pts',(-10.3409331010001,11.6,3.30887963799999));
#254590=CARTESIAN_POINT('Ctrl Pts',(-10.3386722900001,15.2,3.30726477199998));
#254591=CARTESIAN_POINT('Ctrl Pts',(-10.3386722900001,11.6,3.30726477199998));
#254592=CARTESIAN_POINT('Ctrl Pts',(-10.3364147870001,15.2,3.30565512299999));
#254593=CARTESIAN_POINT('Ctrl Pts',(-10.3364147870001,11.6,3.30565512299999));
#254594=CARTESIAN_POINT('Ctrl Pts',(-10.3341606070001,15.2,3.30405068899999));
#254595=CARTESIAN_POINT('Ctrl Pts',(-10.3341606070001,11.6,3.30405068899999));
#254596=CARTESIAN_POINT('Ctrl Pts',(-10.3319097620001,15.2,3.30245147299999));
#254597=CARTESIAN_POINT('Ctrl Pts',(-10.3319097620001,11.6,3.30245147299998));
#254598=CARTESIAN_POINT('Ctrl Pts',(-10.3296622670001,15.2,3.30085747299999));
#254599=CARTESIAN_POINT('Ctrl Pts',(-10.3296622670001,11.6,3.30085747299999));
#254600=CARTESIAN_POINT('Ctrl Pts',(-10.3274181360001,15.2,3.29926868599999));
#254601=CARTESIAN_POINT('Ctrl Pts',(-10.3274181360001,11.6,3.29926868599998));
#254602=CARTESIAN_POINT('Ctrl Pts',(-10.3251773800001,15.2,3.29768511399998));
#254603=CARTESIAN_POINT('Ctrl Pts',(-10.3251773800001,11.6,3.29768511399998));
#254604=CARTESIAN_POINT('Ctrl Pts',(-10.3229400150001,15.2,3.29610675499998));
#254605=CARTESIAN_POINT('Ctrl Pts',(-10.3229400150001,11.6,3.29610675499998));
#254606=CARTESIAN_POINT('Ctrl Pts',(-10.3207060530001,15.2,3.29453360999998));
#254607=CARTESIAN_POINT('Ctrl Pts',(-10.3207060530001,11.6,3.29453360999998));
#254608=CARTESIAN_POINT('Ctrl Pts',(-10.3184755090001,15.2,3.29296567599999));
#254609=CARTESIAN_POINT('Ctrl Pts',(-10.3184755090001,11.6,3.29296567599999));
#254610=CARTESIAN_POINT('Ctrl Pts',(-10.3162483960001,15.2,3.29140295299998));
#254611=CARTESIAN_POINT('Ctrl Pts',(-10.3162483960001,11.6,3.29140295299998));
#254612=CARTESIAN_POINT('Ctrl Pts',(-10.3140247280001,15.2,3.28984543999999));
#254613=CARTESIAN_POINT('Ctrl Pts',(-10.3140247280001,11.6,3.28984543999999));
#254614=CARTESIAN_POINT('Ctrl Pts',(-10.3118045180001,15.2,3.28829313799999));
#254615=CARTESIAN_POINT('Ctrl Pts',(-10.3118045180001,11.6,3.28829313799999));
#254616=CARTESIAN_POINT('Ctrl Pts',(-10.3095877810001,15.2,3.28674604399998));
#254617=CARTESIAN_POINT('Ctrl Pts',(-10.3095877810001,11.6,3.28674604399998));
#254618=CARTESIAN_POINT('Ctrl Pts',(-10.3073745300001,15.2,3.28520415899998));
#254619=CARTESIAN_POINT('Ctrl Pts',(-10.3073745300001,11.6,3.28520415899998));
#254620=CARTESIAN_POINT('Ctrl Pts',(-10.3051647790001,15.2,3.28366748199999));
#254621=CARTESIAN_POINT('Ctrl Pts',(-10.3051647790001,11.6,3.28366748199999));
#254622=CARTESIAN_POINT('Ctrl Pts',(-10.3029585420001,15.2,3.28213600999998));
#254623=CARTESIAN_POINT('Ctrl Pts',(-10.3029585420001,11.6,3.28213600999998));
#254624=CARTESIAN_POINT('Ctrl Pts',(-10.3007558330001,15.2,3.28060974499999));
#254625=CARTESIAN_POINT('Ctrl Pts',(-10.3007558330001,11.6,3.28060974499999));
#254626=CARTESIAN_POINT('Ctrl Pts',(-10.2985566670001,15.2,3.27908868399999));
#254627=CARTESIAN_POINT('Ctrl Pts',(-10.2985566670001,11.6,3.27908868399999));
#254628=CARTESIAN_POINT('Ctrl Pts',(-10.2963610560001,15.2,3.27757282799999));
#254629=CARTESIAN_POINT('Ctrl Pts',(-10.2963610560001,11.6,3.27757282799999));
#254630=CARTESIAN_POINT('Ctrl Pts',(-10.2941690160001,15.2,3.27606217499999));
#254631=CARTESIAN_POINT('Ctrl Pts',(-10.2941690160001,11.6,3.27606217499999));
#254632=CARTESIAN_POINT('Ctrl Pts',(-10.2919805600001,15.2,3.27455672399999));
#254633=CARTESIAN_POINT('Ctrl Pts',(-10.2919805600001,11.6,3.27455672399999));
#254634=CARTESIAN_POINT('Ctrl Pts',(-10.2897957010001,15.2,3.27305647499998));
#254635=CARTESIAN_POINT('Ctrl Pts',(-10.2897957010001,11.6,3.27305647499998));
#254636=CARTESIAN_POINT('Ctrl Pts',(-10.2876144550001,15.2,3.27156142699998));
#254637=CARTESIAN_POINT('Ctrl Pts',(-10.2876144550001,11.6,3.27156142699998));
#254638=CARTESIAN_POINT('Ctrl Pts',(-10.2854368370001,15.2,3.27007157799999));
#254639=CARTESIAN_POINT('Ctrl Pts',(-10.2854368370001,11.6,3.27007157799999));
#254640=CARTESIAN_POINT('Ctrl Pts',(-10.2832628580001,15.2,3.26858692799998));
#254641=CARTESIAN_POINT('Ctrl Pts',(-10.2832628580001,11.6,3.26858692799998));
#254642=CARTESIAN_POINT('Ctrl Pts',(-10.2810925340001,15.2,3.26710747599999));
#254643=CARTESIAN_POINT('Ctrl Pts',(-10.2810925340001,11.6,3.26710747599999));
#254644=CARTESIAN_POINT('Ctrl Pts',(-10.2789258800001,15.2,3.26563322099998));
#254645=CARTESIAN_POINT('Ctrl Pts',(-10.2789258800001,11.6,3.26563322099998));
#254646=CARTESIAN_POINT('Ctrl Pts',(-10.2767629100001,15.2,3.26416416199999));
#254647=CARTESIAN_POINT('Ctrl Pts',(-10.2767629100001,11.6,3.26416416199999));
#254648=CARTESIAN_POINT('Ctrl Pts',(-10.2746036380001,15.2,3.26270029799999));
#254649=CARTESIAN_POINT('Ctrl Pts',(-10.2746036380001,11.6,3.26270029799998));
#254650=CARTESIAN_POINT('Ctrl Pts',(-10.2724480790001,15.2,3.26124162799999));
#254651=CARTESIAN_POINT('Ctrl Pts',(-10.2724480790001,11.6,3.26124162799999));
#254652=CARTESIAN_POINT('Ctrl Pts',(-10.2702962470001,15.2,3.25978815099998));
#254653=CARTESIAN_POINT('Ctrl Pts',(-10.2702962470001,11.6,3.25978815099998));
#254654=CARTESIAN_POINT('Ctrl Pts',(-10.2681481560001,15.2,3.25833986599999));
#254655=CARTESIAN_POINT('Ctrl Pts',(-10.2681481560001,11.6,3.25833986599999));
#254656=CARTESIAN_POINT('Ctrl Pts',(-10.2660038210001,15.2,3.25689677199998));
#254657=CARTESIAN_POINT('Ctrl Pts',(-10.2660038210001,11.6,3.25689677199998));
#254658=CARTESIAN_POINT('Ctrl Pts',(-10.2638632570001,15.2,3.25545886899998));
#254659=CARTESIAN_POINT('Ctrl Pts',(-10.2638632570001,11.6,3.25545886899998));
#254660=CARTESIAN_POINT('Ctrl Pts',(-10.2617264780001,15.2,3.25402615399998));
#254661=CARTESIAN_POINT('Ctrl Pts',(-10.2617264780001,11.6,3.25402615399998));
#254662=CARTESIAN_POINT('Ctrl Pts',(-10.2595934990001,15.2,3.25259862599999));
#254663=CARTESIAN_POINT('Ctrl Pts',(-10.2595934990001,11.6,3.25259862599999));
#254664=CARTESIAN_POINT('Ctrl Pts',(-10.2574643340001,15.2,3.25117628699999));
#254665=CARTESIAN_POINT('Ctrl Pts',(-10.2574643340001,11.6,3.25117628699999));
#254666=CARTESIAN_POINT('Ctrl Pts',(-10.2553389990001,15.2,3.24975913199999));
#254667=CARTESIAN_POINT('Ctrl Pts',(-10.2553389990001,11.6,3.24975913199999));
#254668=CARTESIAN_POINT('Ctrl Pts',(-10.2532175070001,15.2,3.24834716199998));
#254669=CARTESIAN_POINT('Ctrl Pts',(-10.2532175070001,11.6,3.24834716199998));
#254670=CARTESIAN_POINT('Ctrl Pts',(-10.2510998750001,15.2,3.24694037699999));
#254671=CARTESIAN_POINT('Ctrl Pts',(-10.2510998750001,11.6,3.24694037699999));
#254672=CARTESIAN_POINT('Ctrl Pts',(-10.2489861160001,15.2,3.24553877299999));
#254673=CARTESIAN_POINT('Ctrl Pts',(-10.2489861160001,11.6,3.24553877299999));
#254674=CARTESIAN_POINT('Ctrl Pts',(-10.2468762450001,15.2,3.24414234899999));
#254675=CARTESIAN_POINT('Ctrl Pts',(-10.2468762450001,11.6,3.24414234899999));
#254676=CARTESIAN_POINT('Ctrl Pts',(-10.2447702790001,15.2,3.24275110699999));
#254677=CARTESIAN_POINT('Ctrl Pts',(-10.2447702790001,11.6,3.24275110699999));
#254678=CARTESIAN_POINT('Ctrl Pts',(-10.2426682300001,15.2,3.24136504299998));
#254679=CARTESIAN_POINT('Ctrl Pts',(-10.2426682300001,11.6,3.24136504299998));
#254680=CARTESIAN_POINT('Ctrl Pts',(-10.2405701150001,15.2,3.23998415799998));
#254681=CARTESIAN_POINT('Ctrl Pts',(-10.2405701150001,11.6,3.23998415799998));
#254682=CARTESIAN_POINT('Ctrl Pts',(-10.2384759480001,15.2,3.23860844899999));
#254683=CARTESIAN_POINT('Ctrl Pts',(-10.2384759480001,11.6,3.23860844899999));
#254684=CARTESIAN_POINT('Ctrl Pts',(-10.2363857440001,15.2,3.23723791499999));
#254685=CARTESIAN_POINT('Ctrl Pts',(-10.2363857440001,11.6,3.23723791499999));
#254686=CARTESIAN_POINT('Ctrl Pts',(-10.2342995200001,15.2,3.23587255499999));
#254687=CARTESIAN_POINT('Ctrl Pts',(-10.2342995200001,11.6,3.23587255499999));
#254688=CARTESIAN_POINT('Ctrl Pts',(-10.2322172890001,15.2,3.23451236899999));
#254689=CARTESIAN_POINT('Ctrl Pts',(-10.2322172890001,11.6,3.23451236899999));
#254690=CARTESIAN_POINT('Ctrl Pts',(-10.2301390670001,15.2,3.23315735299998));
#254691=CARTESIAN_POINT('Ctrl Pts',(-10.2301390670001,11.6,3.23315735299998));
#254692=CARTESIAN_POINT('Ctrl Pts',(-10.2280648700001,15.2,3.23180750899999));
#254693=CARTESIAN_POINT('Ctrl Pts',(-10.2280648700001,11.6,3.23180750899999));
#254694=CARTESIAN_POINT('Ctrl Pts',(-10.2259947110001,15.2,3.23046283299998));
#254695=CARTESIAN_POINT('Ctrl Pts',(-10.2259947110001,11.6,3.23046283299998));
#254696=CARTESIAN_POINT('Ctrl Pts',(-10.2239286080001,15.2,3.22912332499998));
#254697=CARTESIAN_POINT('Ctrl Pts',(-10.2239286080001,11.6,3.22912332499998));
#254698=CARTESIAN_POINT('Ctrl Pts',(-10.2218665760001,15.2,3.22778898299998));
#254699=CARTESIAN_POINT('Ctrl Pts',(-10.2218665760001,11.6,3.22778898299998));
#254700=CARTESIAN_POINT('Ctrl Pts',(-10.2198086280001,15.2,3.22645980699999));
#254701=CARTESIAN_POINT('Ctrl Pts',(-10.2198086280001,11.6,3.22645980699999));
#254702=CARTESIAN_POINT('Ctrl Pts',(-10.2177547810001,15.2,3.22513579499999));
#254703=CARTESIAN_POINT('Ctrl Pts',(-10.2177547810001,11.6,3.22513579499999));
#254704=CARTESIAN_POINT('Ctrl Pts',(-10.2157050510001,15.2,3.22381694599999));
#254705=CARTESIAN_POINT('Ctrl Pts',(-10.2157050510001,11.6,3.22381694599999));
#254706=CARTESIAN_POINT('Ctrl Pts',(-10.2136594530001,15.2,3.22250325599998));
#254707=CARTESIAN_POINT('Ctrl Pts',(-10.2136594530001,11.6,3.22250325599998));
#254708=CARTESIAN_POINT('Ctrl Pts',(-10.2116180040001,15.2,3.22119472699999));
#254709=CARTESIAN_POINT('Ctrl Pts',(-10.2116180040001,11.6,3.22119472699998));
#254710=CARTESIAN_POINT('Ctrl Pts',(-10.2095807170001,15.2,3.21989135599999));
#254711=CARTESIAN_POINT('Ctrl Pts',(-10.2095807170001,11.6,3.21989135599999));
#254712=CARTESIAN_POINT('Ctrl Pts',(-10.2075476090001,15.2,3.21859314199998));
#254713=CARTESIAN_POINT('Ctrl Pts',(-10.2075476090001,11.6,3.21859314199998));
#254714=CARTESIAN_POINT('Ctrl Pts',(-10.2055186960001,15.2,3.21730008499999));
#254715=CARTESIAN_POINT('Ctrl Pts',(-10.2055186960001,11.6,3.21730008499999));
#254716=CARTESIAN_POINT('Ctrl Pts',(-10.2034939940001,15.2,3.21601217999999));
#254717=CARTESIAN_POINT('Ctrl Pts',(-10.2034939940001,11.6,3.21601217999999));
#254718=CARTESIAN_POINT('Ctrl Pts',(-10.2014735180001,15.2,3.21472942799998));
#254719=CARTESIAN_POINT('Ctrl Pts',(-10.2014735180001,11.6,3.21472942799998));
#254720=CARTESIAN_POINT('Ctrl Pts',(-10.1994572830001,15.2,3.21345182899999));
#254721=CARTESIAN_POINT('Ctrl Pts',(-10.1994572830001,11.6,3.21345182899999));
#254722=CARTESIAN_POINT('Ctrl Pts',(-10.1974453070001,15.2,3.21217937799998));
#254723=CARTESIAN_POINT('Ctrl Pts',(-10.1974453070001,11.6,3.21217937799998));
#254724=CARTESIAN_POINT('Ctrl Pts',(-10.1954376050001,15.2,3.21091207499999));
#254725=CARTESIAN_POINT('Ctrl Pts',(-10.1954376050001,11.6,3.21091207499998));
#254726=CARTESIAN_POINT('Ctrl Pts',(-10.1934341930001,15.2,3.20964991899999));
#254727=CARTESIAN_POINT('Ctrl Pts',(-10.1934341930001,11.6,3.20964991899999));
#254728=CARTESIAN_POINT('Ctrl Pts',(-10.1914350860001,15.2,3.20839290799999));
#254729=CARTESIAN_POINT('Ctrl Pts',(-10.1914350860001,11.6,3.20839290799999));
#254730=CARTESIAN_POINT('Ctrl Pts',(-10.1894403010001,15.2,3.20714103999999));
#254731=CARTESIAN_POINT('Ctrl Pts',(-10.1894403010001,11.6,3.20714103999999));
#254732=CARTESIAN_POINT('Ctrl Pts',(-10.1874498540001,15.2,3.20589431399998));
#254733=CARTESIAN_POINT('Ctrl Pts',(-10.1874498540001,11.6,3.20589431399998));
#254734=CARTESIAN_POINT('Ctrl Pts',(-10.1854637630001,15.2,3.20465272999999));
#254735=CARTESIAN_POINT('Ctrl Pts',(-10.1854637630001,11.6,3.20465272999999));
#254736=CARTESIAN_POINT('Ctrl Pts',(-10.1834820400001,15.2,3.20341628299998));
#254737=CARTESIAN_POINT('Ctrl Pts',(-10.1834820400001,11.6,3.20341628299998));
#254738=CARTESIAN_POINT('Ctrl Pts',(-10.1815047050001,15.2,3.20218497399999));
#254739=CARTESIAN_POINT('Ctrl Pts',(-10.1815047050001,11.6,3.20218497399999));
#254740=CARTESIAN_POINT('Ctrl Pts',(-10.1795317740001,15.2,3.20095879999998));
#254741=CARTESIAN_POINT('Ctrl Pts',(-10.1795317740001,11.6,3.20095879999998));
#254742=CARTESIAN_POINT('Ctrl Pts',(-10.1775632610001,15.2,3.19973776199999));
#254743=CARTESIAN_POINT('Ctrl Pts',(-10.1775632610001,11.6,3.19973776199999));
#254744=CARTESIAN_POINT('Ctrl Pts',(-10.1755991840001,15.2,3.19852185499998));
#254745=CARTESIAN_POINT('Ctrl Pts',(-10.1755991840001,11.6,3.19852185499998));
#254746=CARTESIAN_POINT('Ctrl Pts',(-10.1736395590001,15.2,3.19731107799999));
#254747=CARTESIAN_POINT('Ctrl Pts',(-10.1736395590001,11.6,3.19731107799999));
#254748=CARTESIAN_POINT('Ctrl Pts',(-10.1716844030001,15.2,3.19610542999998));
#254749=CARTESIAN_POINT('Ctrl Pts',(-10.1716844030001,11.6,3.19610542999998));
#254750=CARTESIAN_POINT('Ctrl Pts',(-10.1697337330001,15.2,3.19490490899998));
#254751=CARTESIAN_POINT('Ctrl Pts',(-10.1697337330001,11.6,3.19490490899998));
#254752=CARTESIAN_POINT('Ctrl Pts',(-10.1677875630001,15.2,3.19370951499998));
#254753=CARTESIAN_POINT('Ctrl Pts',(-10.1677875630001,11.6,3.19370951499998));
#254754=CARTESIAN_POINT('Ctrl Pts',(-10.1658459140001,15.2,3.19251924299999));
#254755=CARTESIAN_POINT('Ctrl Pts',(-10.1658459140001,11.6,3.19251924299999));
#254756=CARTESIAN_POINT('Ctrl Pts',(-10.1639087980001,15.2,3.19133409299998));
#254757=CARTESIAN_POINT('Ctrl Pts',(-10.1639087980001,11.6,3.19133409299998));
#254758=CARTESIAN_POINT('Ctrl Pts',(-10.1619762350001,15.2,3.19015406399998));
#254759=CARTESIAN_POINT('Ctrl Pts',(-10.1619762350001,11.6,3.19015406399998));
#254760=CARTESIAN_POINT('Ctrl Pts',(-10.1600482390001,15.2,3.18897915399998));
#254761=CARTESIAN_POINT('Ctrl Pts',(-10.1600482390001,11.6,3.18897915399998));
#254762=CARTESIAN_POINT('Ctrl Pts',(-10.1581248300001,15.2,3.18780935899999));
#254763=CARTESIAN_POINT('Ctrl Pts',(-10.1581248300001,11.6,3.18780935899999));
#254764=CARTESIAN_POINT('Ctrl Pts',(-10.1562060230001,15.2,3.18664467999999));
#254765=CARTESIAN_POINT('Ctrl Pts',(-10.1562060230001,11.6,3.18664467999999));
#254766=CARTESIAN_POINT('Ctrl Pts',(-10.1542918360001,15.2,3.18548511399998));
#254767=CARTESIAN_POINT('Ctrl Pts',(-10.1542918360001,11.6,3.18548511399998));
#254768=CARTESIAN_POINT('Ctrl Pts',(-10.1523822840001,15.2,3.18433065799999));
#254769=CARTESIAN_POINT('Ctrl Pts',(-10.1523822840001,11.6,3.18433065799999));
#254770=CARTESIAN_POINT('Ctrl Pts',(-10.1504773870001,15.2,3.18318131199998));
#254771=CARTESIAN_POINT('Ctrl Pts',(-10.1504773870001,11.6,3.18318131199998));
#254772=CARTESIAN_POINT('Ctrl Pts',(-10.1485771590001,15.2,3.18203707299999));
#254773=CARTESIAN_POINT('Ctrl Pts',(-10.1485771590001,11.6,3.18203707299999));
#254774=CARTESIAN_POINT('Ctrl Pts',(-10.1466816200001,15.2,3.18089793999999));
#254775=CARTESIAN_POINT('Ctrl Pts',(-10.1466816200001,11.6,3.18089793999999));
#254776=CARTESIAN_POINT('Ctrl Pts',(-10.1447907840001,15.2,3.17976390999998));
#254777=CARTESIAN_POINT('Ctrl Pts',(-10.1447907840001,11.6,3.17976390999998));
#254778=CARTESIAN_POINT('Ctrl Pts',(-10.1429046700001,15.2,3.17863498199999));
#254779=CARTESIAN_POINT('Ctrl Pts',(-10.1429046700001,11.6,3.17863498199999));
#254780=CARTESIAN_POINT('Ctrl Pts',(-10.1410232970001,15.2,3.17751115299998));
#254781=CARTESIAN_POINT('Ctrl Pts',(-10.1410232970001,11.6,3.17751115299998));
#254782=CARTESIAN_POINT('Ctrl Pts',(-10.1391466790001,15.2,3.17639242199999));
#254783=CARTESIAN_POINT('Ctrl Pts',(-10.1391466790001,11.6,3.17639242199998));
#254784=CARTESIAN_POINT('Ctrl Pts',(-10.1372748360001,15.2,3.17527878599999));
#254785=CARTESIAN_POINT('Ctrl Pts',(-10.1372748360001,11.6,3.17527878599999));
#254786=CARTESIAN_POINT('Ctrl Pts',(-10.1354077850001,15.2,3.17417024399998));
#254787=CARTESIAN_POINT('Ctrl Pts',(-10.1354077850001,11.6,3.17417024399998));
#254788=CARTESIAN_POINT('Ctrl Pts',(-10.1335455420001,15.2,3.17306679399999));
#254789=CARTESIAN_POINT('Ctrl Pts',(-10.1335455420001,11.6,3.17306679399999));
#254790=CARTESIAN_POINT('Ctrl Pts',(-10.1316881250001,15.2,3.17196843299998));
#254791=CARTESIAN_POINT('Ctrl Pts',(-10.1316881250001,11.6,3.17196843299998));
#254792=CARTESIAN_POINT('Ctrl Pts',(-10.1298355530001,15.2,3.17087515999999));
#254793=CARTESIAN_POINT('Ctrl Pts',(-10.1298355530001,11.6,3.17087515999999));
#254794=CARTESIAN_POINT('Ctrl Pts',(-10.1279878430001,15.2,3.16978697199998));
#254795=CARTESIAN_POINT('Ctrl Pts',(-10.1279878430001,11.6,3.16978697199998));
#254796=CARTESIAN_POINT('Ctrl Pts',(-10.1261450120001,15.2,3.16870386699998));
#254797=CARTESIAN_POINT('Ctrl Pts',(-10.1261450120001,11.6,3.16870386699998));
#254798=CARTESIAN_POINT('Ctrl Pts',(-10.1243070780001,15.2,3.16762584299998));
#254799=CARTESIAN_POINT('Ctrl Pts',(-10.1243070780001,11.6,3.16762584299998));
#254800=CARTESIAN_POINT('Ctrl Pts',(-10.1224740600001,15.2,3.16655289799999));
#254801=CARTESIAN_POINT('Ctrl Pts',(-10.1224740600001,11.6,3.16655289799999));
#254802=CARTESIAN_POINT('Ctrl Pts',(-10.1206459750001,15.2,3.16548503099998));
#254803=CARTESIAN_POINT('Ctrl Pts',(-10.1206459750001,11.6,3.16548503099998));
#254804=CARTESIAN_POINT('Ctrl Pts',(-10.1188228400001,15.2,3.16442223699998));
#254805=CARTESIAN_POINT('Ctrl Pts',(-10.1188228400001,11.6,3.16442223699998));
#254806=CARTESIAN_POINT('Ctrl Pts',(-10.1170046750001,15.2,3.16336451599999));
#254807=CARTESIAN_POINT('Ctrl Pts',(-10.1170046750001,11.6,3.16336451599999));
#254808=CARTESIAN_POINT('Ctrl Pts',(-10.1151914960001,15.2,3.16231186599998));
#254809=CARTESIAN_POINT('Ctrl Pts',(-10.1151914960001,11.6,3.16231186599998));
#254810=CARTESIAN_POINT('Ctrl Pts',(-10.1133833240001,15.2,3.16126428399999));
#254811=CARTESIAN_POINT('Ctrl Pts',(-10.1133833240001,11.6,3.16126428399999));
#254812=CARTESIAN_POINT('Ctrl Pts',(-10.1115801740001,15.2,3.16022176699998));
#254813=CARTESIAN_POINT('Ctrl Pts',(-10.1115801740001,11.6,3.16022176699998));
#254814=CARTESIAN_POINT('Ctrl Pts',(-10.1097820650001,15.2,3.15918431399999));
#254815=CARTESIAN_POINT('Ctrl Pts',(-10.1097820650001,11.6,3.15918431399999));
#254816=CARTESIAN_POINT('Ctrl Pts',(-10.1079890170001,15.2,3.15815192199998));
#254817=CARTESIAN_POINT('Ctrl Pts',(-10.1079890170001,11.6,3.15815192199998));
#254818=CARTESIAN_POINT('Ctrl Pts',(-10.1062010460001,15.2,3.15712458799998));
#254819=CARTESIAN_POINT('Ctrl Pts',(-10.1062010460001,11.6,3.15712458799998));
#254820=CARTESIAN_POINT('Ctrl Pts',(-10.1044181730001,15.2,3.15610231199998));
#254821=CARTESIAN_POINT('Ctrl Pts',(-10.1044181730001,11.6,3.15610231199998));
#254822=CARTESIAN_POINT('Ctrl Pts',(-10.1026404140001,15.2,3.15508508899998));
#254823=CARTESIAN_POINT('Ctrl Pts',(-10.1026404140001,11.6,3.15508508899998));
#254824=CARTESIAN_POINT('Ctrl Pts',(-10.1008677890001,15.2,3.15407291799998));
#254825=CARTESIAN_POINT('Ctrl Pts',(-10.1008677890001,11.6,3.15407291799998));
#254826=CARTESIAN_POINT('Ctrl Pts',(-10.0991003160001,15.2,3.15306579799999));
#254827=CARTESIAN_POINT('Ctrl Pts',(-10.0991003160001,11.6,3.15306579799999));
#254828=CARTESIAN_POINT('Ctrl Pts',(-10.0973380130001,15.2,3.15206372299999));
#254829=CARTESIAN_POINT('Ctrl Pts',(-10.0973380130001,11.6,3.15206372299999));
#254830=CARTESIAN_POINT('Ctrl Pts',(-10.0955809000001,15.2,3.15106669399999));
#254831=CARTESIAN_POINT('Ctrl Pts',(-10.0955809000001,11.6,3.15106669399999));
#254832=CARTESIAN_POINT('Ctrl Pts',(-10.0938289960001,15.2,3.15007470699998));
#254833=CARTESIAN_POINT('Ctrl Pts',(-10.0938289960001,11.6,3.15007470699998));
#254834=CARTESIAN_POINT('Ctrl Pts',(-10.0920823180001,15.2,3.14908775899998));
#254835=CARTESIAN_POINT('Ctrl Pts',(-10.0920823180001,11.6,3.14908775899998));
#254836=CARTESIAN_POINT('Ctrl Pts',(-10.0903408870001,15.2,3.14810584799999));
#254837=CARTESIAN_POINT('Ctrl Pts',(-10.0903408870001,11.6,3.14810584799999));
#254838=CARTESIAN_POINT('Ctrl Pts',(-10.0886047200001,15.2,3.14712897299999));
#254839=CARTESIAN_POINT('Ctrl Pts',(-10.0886047200001,11.6,3.14712897299999));
#254840=CARTESIAN_POINT('Ctrl Pts',(-10.0868738370001,15.2,3.14615712899998));
#254841=CARTESIAN_POINT('Ctrl Pts',(-10.0868738370001,11.6,3.14615712899998));
#254842=CARTESIAN_POINT('Ctrl Pts',(-10.0851482570001,15.2,3.14519031499999));
#254843=CARTESIAN_POINT('Ctrl Pts',(-10.0851482570001,11.6,3.14519031499999));
#254844=CARTESIAN_POINT('Ctrl Pts',(-10.0834279990001,15.2,3.14422852799999));
#254845=CARTESIAN_POINT('Ctrl Pts',(-10.0834279990001,11.6,3.14422852799999));
#254846=CARTESIAN_POINT('Ctrl Pts',(-10.0817130830001,15.2,3.14327176499998));
#254847=CARTESIAN_POINT('Ctrl Pts',(-10.0817130830001,11.6,3.14327176499998));
#254848=CARTESIAN_POINT('Ctrl Pts',(-10.0800035270001,15.2,3.14232002499998));
#254849=CARTESIAN_POINT('Ctrl Pts',(-10.0800035270001,11.6,3.14232002499998));
#254850=CARTESIAN_POINT('Ctrl Pts',(-10.0782993510001,15.2,3.14137330299998));
#254851=CARTESIAN_POINT('Ctrl Pts',(-10.0782993510001,11.6,3.14137330299998));
#254852=CARTESIAN_POINT('Ctrl Pts',(-10.0766005740001,15.2,3.14043159799999));
#254853=CARTESIAN_POINT('Ctrl Pts',(-10.0766005740001,11.6,3.14043159799999));
#254854=CARTESIAN_POINT('Ctrl Pts',(-10.0749072160001,15.2,3.13949490699999));
#254855=CARTESIAN_POINT('Ctrl Pts',(-10.0749072160001,11.6,3.13949490699999));
#254856=CARTESIAN_POINT('Ctrl Pts',(-10.0732192960001,15.2,3.13856322799998));
#254857=CARTESIAN_POINT('Ctrl Pts',(-10.0732192960001,11.6,3.13856322799998));
#254858=CARTESIAN_POINT('Ctrl Pts',(-10.0715368340001,15.2,3.13763655699999));
#254859=CARTESIAN_POINT('Ctrl Pts',(-10.0715368340001,11.6,3.13763655699999));
#254860=CARTESIAN_POINT('Ctrl Pts',(-10.0698598500001,15.2,3.13671489099999));
#254861=CARTESIAN_POINT('Ctrl Pts',(-10.0698598500001,11.6,3.13671489099998));
#254862=CARTESIAN_POINT('Ctrl Pts',(-10.0681883620001,15.2,3.13579822799999));
#254863=CARTESIAN_POINT('Ctrl Pts',(-10.0681883620001,11.6,3.13579822799999));
#254864=CARTESIAN_POINT('Ctrl Pts',(-10.0665223920001,15.2,3.13488656499998));
#254865=CARTESIAN_POINT('Ctrl Pts',(-10.0665223920001,11.6,3.13488656499998));
#254866=CARTESIAN_POINT('Ctrl Pts',(-10.0648619590001,15.2,3.13397989999999));
#254867=CARTESIAN_POINT('Ctrl Pts',(-10.0648619590001,11.6,3.13397989999999));
#254868=CARTESIAN_POINT('Ctrl Pts',(-10.0632070820001,15.2,3.13307822999998));
#254869=CARTESIAN_POINT('Ctrl Pts',(-10.0632070820001,11.6,3.13307822999998));
#254870=CARTESIAN_POINT('Ctrl Pts',(-10.0615577810001,15.2,3.13218154999999));
#254871=CARTESIAN_POINT('Ctrl Pts',(-10.0615577810001,11.6,3.13218154999999));
#254872=CARTESIAN_POINT('Ctrl Pts',(-10.0599140780001,15.2,3.13128986099999));
#254873=CARTESIAN_POINT('Ctrl Pts',(-10.0599140780001,11.6,3.13128986099999));
#254874=CARTESIAN_POINT('Ctrl Pts',(-10.0582759920001,15.2,3.13040315599999));
#254875=CARTESIAN_POINT('Ctrl Pts',(-10.0582759920001,11.6,3.13040315599999));
#254876=CARTESIAN_POINT('Ctrl Pts',(-10.0566435420001,15.2,3.12952143599999));
#254877=CARTESIAN_POINT('Ctrl Pts',(-10.0566435420001,11.6,3.12952143599999));
#254878=CARTESIAN_POINT('Ctrl Pts',(-10.0550167500001,15.2,3.12864469399998));
#254879=CARTESIAN_POINT('Ctrl Pts',(-10.0550167500001,11.6,3.12864469399998));
#254880=CARTESIAN_POINT('Ctrl Pts',(-10.0533956360001,15.2,3.12777292999999));
#254881=CARTESIAN_POINT('Ctrl Pts',(-10.0533956360001,11.6,3.12777292999999));
#254882=CARTESIAN_POINT('Ctrl Pts',(-10.0517802200001,15.2,3.12690613999998));
#254883=CARTESIAN_POINT('Ctrl Pts',(-10.0517802200001,11.6,3.12690613999998));
#254884=CARTESIAN_POINT('Ctrl Pts',(-10.0501705220001,15.2,3.12604432099998));
#254885=CARTESIAN_POINT('Ctrl Pts',(-10.0501705220001,11.6,3.12604432099998));
#254886=CARTESIAN_POINT('Ctrl Pts',(-10.0485665630001,15.2,3.12518747099999));
#254887=CARTESIAN_POINT('Ctrl Pts',(-10.0485665630001,11.6,3.12518747099999));
#254888=CARTESIAN_POINT('Ctrl Pts',(-10.0469683640001,15.2,3.12433558599999));
#254889=CARTESIAN_POINT('Ctrl Pts',(-10.0469683640001,11.6,3.12433558599999));
#254890=CARTESIAN_POINT('Ctrl Pts',(-10.0453759450001,15.2,3.12348866199999));
#254891=CARTESIAN_POINT('Ctrl Pts',(-10.0453759450001,11.6,3.12348866199999));
#254892=CARTESIAN_POINT('Ctrl Pts',(-10.0437893290001,15.2,3.12264669699999));
#254893=CARTESIAN_POINT('Ctrl Pts',(-10.0437893290001,11.6,3.12264669699999));
#254894=CARTESIAN_POINT('Ctrl Pts',(-10.0422085330001,15.2,3.12180968699998));
#254895=CARTESIAN_POINT('Ctrl Pts',(-10.0422085330001,11.6,3.12180968699998));
#254896=CARTESIAN_POINT('Ctrl Pts',(-10.0406335810001,15.2,3.12097763199999));
#254897=CARTESIAN_POINT('Ctrl Pts',(-10.0406335810001,11.6,3.12097763199999));
#254898=CARTESIAN_POINT('Ctrl Pts',(-10.0390644920001,15.2,3.12015052399998));
#254899=CARTESIAN_POINT('Ctrl Pts',(-10.0390644920001,11.6,3.12015052399998));
#254900=CARTESIAN_POINT('Ctrl Pts',(-10.0375012890001,15.2,3.11932836399999));
#254901=CARTESIAN_POINT('Ctrl Pts',(-10.0375012890001,11.6,3.11932836399999));
#254902=CARTESIAN_POINT('Ctrl Pts',(-10.0359439910001,15.2,3.11851114499999));
#254903=CARTESIAN_POINT('Ctrl Pts',(-10.0359439910001,11.6,3.11851114499999));
#254904=CARTESIAN_POINT('Ctrl Pts',(-10.0343926210001,15.2,3.11769886699999));
#254905=CARTESIAN_POINT('Ctrl Pts',(-10.0343926210001,11.6,3.11769886699999));
#254906=CARTESIAN_POINT('Ctrl Pts',(-10.0328472000001,15.2,3.11689152499999));
#254907=CARTESIAN_POINT('Ctrl Pts',(-10.0328472000001,11.6,3.11689152499999));
#254908=CARTESIAN_POINT('Ctrl Pts',(-10.0313077490001,15.2,3.11608911699999));
#254909=CARTESIAN_POINT('Ctrl Pts',(-10.0313077490001,11.6,3.11608911699999));
#254910=CARTESIAN_POINT('Ctrl Pts',(-10.0297742890001,15.2,3.11529163799998));
#254911=CARTESIAN_POINT('Ctrl Pts',(-10.0297742890001,11.6,3.11529163799998));
#254912=CARTESIAN_POINT('Ctrl Pts',(-10.0282468420001,15.2,3.11449908599998));
#254913=CARTESIAN_POINT('Ctrl Pts',(-10.0282468420001,11.6,3.11449908599998));
#254914=CARTESIAN_POINT('Ctrl Pts',(-10.0267254290001,15.2,3.11371145699999));
#254915=CARTESIAN_POINT('Ctrl Pts',(-10.0267254290001,11.6,3.11371145699999));
#254916=CARTESIAN_POINT('Ctrl Pts',(-10.0252100730001,15.2,3.11292874799998));
#254917=CARTESIAN_POINT('Ctrl Pts',(-10.0252100730001,11.6,3.11292874799998));
#254918=CARTESIAN_POINT('Ctrl Pts',(-10.0237007950001,15.2,3.11215095499998));
#254919=CARTESIAN_POINT('Ctrl Pts',(-10.0237007950001,11.6,3.11215095499998));
#254920=CARTESIAN_POINT('Ctrl Pts',(-10.0221976160001,15.2,3.11137807499998));
#254921=CARTESIAN_POINT('Ctrl Pts',(-10.0221976160001,11.6,3.11137807499998));
#254922=CARTESIAN_POINT('Ctrl Pts',(-10.0207005590001,15.2,3.11061010399998));
#254923=CARTESIAN_POINT('Ctrl Pts',(-10.0207005590001,11.6,3.11061010399998));
#254924=CARTESIAN_POINT('Ctrl Pts',(-10.0192096460001,15.2,3.10984703899998));
#254925=CARTESIAN_POINT('Ctrl Pts',(-10.0192096460001,11.6,3.10984703899998));
#254926=CARTESIAN_POINT('Ctrl Pts',(-10.0177248990001,15.2,3.10908887699998));
#254927=CARTESIAN_POINT('Ctrl Pts',(-10.0177248990001,11.6,3.10908887699998));
#254928=CARTESIAN_POINT('Ctrl Pts',(-10.0162463390001,15.2,3.10833561299999));
#254929=CARTESIAN_POINT('Ctrl Pts',(-10.0162463390001,11.6,3.10833561299999));
#254930=CARTESIAN_POINT('Ctrl Pts',(-10.0147739910001,15.2,3.10758724499999));
#254931=CARTESIAN_POINT('Ctrl Pts',(-10.0147739910001,11.6,3.10758724499998));
#254932=CARTESIAN_POINT('Ctrl Pts',(-10.0133078740001,15.2,3.10684376799998));
#254933=CARTESIAN_POINT('Ctrl Pts',(-10.0133078740001,11.6,3.10684376799998));
#254934=CARTESIAN_POINT('Ctrl Pts',(-10.0118480130001,15.2,3.10610517999999));
#254935=CARTESIAN_POINT('Ctrl Pts',(-10.0118480130001,11.6,3.10610517999999));
#254936=CARTESIAN_POINT('Ctrl Pts',(-10.0103944280001,15.2,3.10537147599998));
#254937=CARTESIAN_POINT('Ctrl Pts',(-10.0103944280001,11.6,3.10537147599998));
#254938=CARTESIAN_POINT('Ctrl Pts',(-10.0089471450001,15.2,3.10464265199998));
#254939=CARTESIAN_POINT('Ctrl Pts',(-10.0089471450001,11.6,3.10464265199998));
#254940=CARTESIAN_POINT('Ctrl Pts',(-10.0075061830001,15.2,3.10391870599998));
#254941=CARTESIAN_POINT('Ctrl Pts',(-10.0075061830001,11.6,3.10391870599998));
#254942=CARTESIAN_POINT('Ctrl Pts',(-10.0060715670001,15.2,3.10319963199999));
#254943=CARTESIAN_POINT('Ctrl Pts',(-10.0060715670001,11.6,3.10319963199999));
#254944=CARTESIAN_POINT('Ctrl Pts',(-10.0046433200001,15.2,3.10248542899998));
#254945=CARTESIAN_POINT('Ctrl Pts',(-10.0046433200001,11.6,3.10248542899998));
#254946=CARTESIAN_POINT('Ctrl Pts',(-10.0032214630001,15.2,3.10177608999999));
#254947=CARTESIAN_POINT('Ctrl Pts',(-10.0032214630001,11.6,3.10177608999999));
#254948=CARTESIAN_POINT('Ctrl Pts',(-10.0018060210001,15.2,3.10107161299998));
#254949=CARTESIAN_POINT('Ctrl Pts',(-10.0018060210001,11.6,3.10107161299998));
#254950=CARTESIAN_POINT('Ctrl Pts',(-10.0003970160001,15.2,3.10037199499998));
#254951=CARTESIAN_POINT('Ctrl Pts',(-10.0003970160001,11.6,3.10037199499998));
#254952=CARTESIAN_POINT('Ctrl Pts',(-9.99899447200006,15.2,3.09967723099999));
#254953=CARTESIAN_POINT('Ctrl Pts',(-9.99899447200006,11.6,3.09967723099999));
#254954=CARTESIAN_POINT('Ctrl Pts',(-9.99759841200006,15.2,3.09898731699998));
#254955=CARTESIAN_POINT('Ctrl Pts',(-9.99759841200006,11.6,3.09898731699998));
#254956=CARTESIAN_POINT('Ctrl Pts',(-9.99620885900006,15.2,3.09830224999998));
#254957=CARTESIAN_POINT('Ctrl Pts',(-9.99620885900006,11.6,3.09830224999998));
#254958=CARTESIAN_POINT('Ctrl Pts',(-9.99482583700006,15.2,3.09762202399998));
#254959=CARTESIAN_POINT('Ctrl Pts',(-9.99482583700006,11.6,3.09762202399998));
#254960=CARTESIAN_POINT('Ctrl Pts',(-9.99344936900006,15.2,3.09694663699998));
#254961=CARTESIAN_POINT('Ctrl Pts',(-9.99344936900006,11.6,3.09694663699998));
#254962=CARTESIAN_POINT('Ctrl Pts',(-9.99207947800006,15.2,3.09627608399998));
#254963=CARTESIAN_POINT('Ctrl Pts',(-9.99207947800006,11.6,3.09627608399998));
#254964=CARTESIAN_POINT('Ctrl Pts',(-9.99071619000006,15.2,3.09561036199998));
#254965=CARTESIAN_POINT('Ctrl Pts',(-9.99071619000006,11.6,3.09561036199998));
#254966=CARTESIAN_POINT('Ctrl Pts',(-9.98935952600006,15.2,3.09494946599998));
#254967=CARTESIAN_POINT('Ctrl Pts',(-9.98935952600006,11.6,3.09494946599998));
#254968=CARTESIAN_POINT('Ctrl Pts',(-9.98800951200005,15.2,3.09429339199998));
#254969=CARTESIAN_POINT('Ctrl Pts',(-9.98800951200005,11.6,3.09429339199998));
#254970=CARTESIAN_POINT('Ctrl Pts',(-9.98666617200006,15.2,3.09364213599999));
#254971=CARTESIAN_POINT('Ctrl Pts',(-9.98666617200006,11.6,3.09364213599999));
#254972=CARTESIAN_POINT('Ctrl Pts',(-9.98532952900005,15.2,3.09299569299998));
#254973=CARTESIAN_POINT('Ctrl Pts',(-9.98532952900005,11.6,3.09299569299998));
#254974=CARTESIAN_POINT('Ctrl Pts',(-9.98399960800005,15.2,3.09235406099998));
#254975=CARTESIAN_POINT('Ctrl Pts',(-9.98399960800005,11.6,3.09235406099998));
#254976=CARTESIAN_POINT('Ctrl Pts',(-9.98267643200006,15.2,3.09171723299999));
#254977=CARTESIAN_POINT('Ctrl Pts',(-9.98267643200006,11.6,3.09171723299999));
#254978=CARTESIAN_POINT('Ctrl Pts',(-9.98136002800005,15.2,3.09108520699999));
#254979=CARTESIAN_POINT('Ctrl Pts',(-9.98136002800005,11.6,3.09108520699999));
#254980=CARTESIAN_POINT('Ctrl Pts',(-9.98005041800005,15.2,3.09045797699999));
#254981=CARTESIAN_POINT('Ctrl Pts',(-9.98005041800005,11.6,3.09045797699999));
#254982=CARTESIAN_POINT('Ctrl Pts',(-9.97874762800006,15.2,3.08983553999998));
#254983=CARTESIAN_POINT('Ctrl Pts',(-9.97874762800006,11.6,3.08983553999998));
#254984=CARTESIAN_POINT('Ctrl Pts',(-9.97745168200005,15.2,3.08921789099998));
#254985=CARTESIAN_POINT('Ctrl Pts',(-9.97745168200005,11.6,3.08921789099998));
#254986=CARTESIAN_POINT('Ctrl Pts',(-9.97616260500006,15.2,3.08860502599998));
#254987=CARTESIAN_POINT('Ctrl Pts',(-9.97616260500006,11.6,3.08860502599998));
#254988=CARTESIAN_POINT('Ctrl Pts',(-9.97488042200006,15.2,3.08799693999998));
#254989=CARTESIAN_POINT('Ctrl Pts',(-9.97488042200006,11.6,3.08799693999998));
#254990=CARTESIAN_POINT('Ctrl Pts',(-9.97360515900005,15.2,3.08739362899999));
#254991=CARTESIAN_POINT('Ctrl Pts',(-9.97360515900005,11.6,3.08739362899999));
#254992=CARTESIAN_POINT('Ctrl Pts',(-9.97233683900006,15.2,3.08679508799998));
#254993=CARTESIAN_POINT('Ctrl Pts',(-9.97233683900006,11.6,3.08679508799998));
#254994=CARTESIAN_POINT('Ctrl Pts',(-9.97107548900006,15.2,3.08620131299998));
#254995=CARTESIAN_POINT('Ctrl Pts',(-9.97107548900006,11.6,3.08620131299998));
#254996=CARTESIAN_POINT('Ctrl Pts',(-9.96982113400006,15.2,3.08561229999999));
#254997=CARTESIAN_POINT('Ctrl Pts',(-9.96982113400006,11.6,3.08561229999999));
#254998=CARTESIAN_POINT('Ctrl Pts',(-9.96857379800005,15.2,3.08502804299999));
#254999=CARTESIAN_POINT('Ctrl Pts',(-9.96857379800005,11.6,3.08502804299999));
#255000=CARTESIAN_POINT('Ctrl Pts',(-9.96733350800006,15.2,3.08444853899999));
#255001=CARTESIAN_POINT('Ctrl Pts',(-9.96733350800006,11.6,3.08444853899999));
#255002=CARTESIAN_POINT('Ctrl Pts',(-9.96610029100006,15.2,3.08387378199999));
#255003=CARTESIAN_POINT('Ctrl Pts',(-9.96610029100006,11.6,3.08387378199999));
#255004=CARTESIAN_POINT('Ctrl Pts',(-9.96487416900005,15.2,3.08330376799999));
#255005=CARTESIAN_POINT('Ctrl Pts',(-9.96487416900005,11.6,3.08330376799999));
#255006=CARTESIAN_POINT('Ctrl Pts',(-9.96365517100006,15.2,3.08273849199999));
#255007=CARTESIAN_POINT('Ctrl Pts',(-9.96365517100006,11.6,3.08273849199999));
#255008=CARTESIAN_POINT('Ctrl Pts',(-9.96244332100006,15.2,3.08217794899999));
#255009=CARTESIAN_POINT('Ctrl Pts',(-9.96244332100006,11.6,3.08217794899999));
#255010=CARTESIAN_POINT('Ctrl Pts',(-9.96123864600006,15.2,3.08162213599999));
#255011=CARTESIAN_POINT('Ctrl Pts',(-9.96123864600006,11.6,3.08162213599999));
#255012=CARTESIAN_POINT('Ctrl Pts',(-9.96004117300006,15.2,3.08107104599999));
#255013=CARTESIAN_POINT('Ctrl Pts',(-9.96004117300006,11.6,3.08107104599999));
#255014=CARTESIAN_POINT('Ctrl Pts',(-9.95885092700006,15.2,3.08052467499999));
#255015=CARTESIAN_POINT('Ctrl Pts',(-9.95885092700006,11.6,3.08052467499999));
#255016=CARTESIAN_POINT('Ctrl Pts',(-9.95766793500006,15.2,3.07998301799999));
#255017=CARTESIAN_POINT('Ctrl Pts',(-9.95766793500006,11.6,3.07998301799999));
#255018=CARTESIAN_POINT('Ctrl Pts',(-9.95649222300005,15.2,3.07944606999998));
#255019=CARTESIAN_POINT('Ctrl Pts',(-9.95649222300005,11.6,3.07944606999998));
#255020=CARTESIAN_POINT('Ctrl Pts',(-9.95532381800006,15.2,3.07891382599998));
#255021=CARTESIAN_POINT('Ctrl Pts',(-9.95532381800006,11.6,3.07891382599998));
#255022=CARTESIAN_POINT('Ctrl Pts',(-9.95416274700006,15.2,3.07838628199999));
#255023=CARTESIAN_POINT('Ctrl Pts',(-9.95416274700006,11.6,3.07838628199998));
#255024=CARTESIAN_POINT('Ctrl Pts',(-9.95300903700005,15.2,3.07786343099998));
#255025=CARTESIAN_POINT('Ctrl Pts',(-9.95300903700005,11.6,3.07786343099998));
#255026=CARTESIAN_POINT('Ctrl Pts',(-9.95186271400006,15.2,3.07734527099999));
#255027=CARTESIAN_POINT('Ctrl Pts',(-9.95186271400006,11.6,3.07734527099999));
#255028=CARTESIAN_POINT('Ctrl Pts',(-9.95072380600006,15.2,3.07683179399999));
#255029=CARTESIAN_POINT('Ctrl Pts',(-9.95072380600006,11.6,3.07683179399999));
#255030=CARTESIAN_POINT('Ctrl Pts',(-9.94959234000006,15.2,3.07632299599998));
#255031=CARTESIAN_POINT('Ctrl Pts',(-9.94959234000006,11.6,3.07632299599998));
#255032=CARTESIAN_POINT('Ctrl Pts',(-9.94846834300006,15.2,3.07581887199999));
#255033=CARTESIAN_POINT('Ctrl Pts',(-9.94846834300006,11.6,3.07581887199999));
#255034=CARTESIAN_POINT('Ctrl Pts',(-9.94735184300006,15.2,3.07531941599999));
#255035=CARTESIAN_POINT('Ctrl Pts',(-9.94735184300006,11.6,3.07531941599999));
#255036=CARTESIAN_POINT('Ctrl Pts',(-9.94624286800006,15.2,3.07482462399999));
#255037=CARTESIAN_POINT('Ctrl Pts',(-9.94624286800006,11.6,3.07482462399999));
#255038=CARTESIAN_POINT('Ctrl Pts',(-9.94514144400006,15.2,3.07433448899998));
#255039=CARTESIAN_POINT('Ctrl Pts',(-9.94514144400006,11.6,3.07433448899998));
#255040=CARTESIAN_POINT('Ctrl Pts',(-9.94404760100006,15.2,3.07384900799998));
#255041=CARTESIAN_POINT('Ctrl Pts',(-9.94404760100006,11.6,3.07384900799998));
#255042=CARTESIAN_POINT('Ctrl Pts',(-9.94296136500006,15.2,3.07336817399998));
#255043=CARTESIAN_POINT('Ctrl Pts',(-9.94296136500006,11.6,3.07336817399998));
#255044=CARTESIAN_POINT('Ctrl Pts',(-9.94188276500006,15.2,3.07289198099999));
#255045=CARTESIAN_POINT('Ctrl Pts',(-9.94188276500006,11.6,3.07289198099999));
#255046=CARTESIAN_POINT('Ctrl Pts',(-9.94081182900005,15.2,3.07242042699999));
#255047=CARTESIAN_POINT('Ctrl Pts',(-9.94081182900005,11.6,3.07242042699999));
#255048=CARTESIAN_POINT('Ctrl Pts',(-9.93974858600006,15.2,3.07195350199999));
#255049=CARTESIAN_POINT('Ctrl Pts',(-9.93974858600006,11.6,3.07195350199999));
#255050=CARTESIAN_POINT('Ctrl Pts',(-9.93869306400006,15.2,3.07149120299999));
#255051=CARTESIAN_POINT('Ctrl Pts',(-9.93869306400006,11.6,3.07149120299999));
#255052=CARTESIAN_POINT('Ctrl Pts',(-9.93764529000006,15.2,3.07103352399999));
#255053=CARTESIAN_POINT('Ctrl Pts',(-9.93764529000006,11.6,3.07103352399999));
#255054=CARTESIAN_POINT('Ctrl Pts',(-9.93660529600006,15.2,3.07058045999998));
#255055=CARTESIAN_POINT('Ctrl Pts',(-9.93660529600006,11.6,3.07058045999998));
#255056=CARTESIAN_POINT('Ctrl Pts',(-9.93557310900006,15.2,3.07013200499998));
#255057=CARTESIAN_POINT('Ctrl Pts',(-9.93557310900006,11.6,3.07013200499998));
#255058=CARTESIAN_POINT('Ctrl Pts',(-9.93454875700006,15.2,3.06968815199999));
#255059=CARTESIAN_POINT('Ctrl Pts',(-9.93454875700006,11.6,3.06968815199998));
#255060=CARTESIAN_POINT('Ctrl Pts',(-9.93353227100006,15.2,3.06924889799999));
#255061=CARTESIAN_POINT('Ctrl Pts',(-9.93353227100006,11.6,3.06924889799999));
#255062=CARTESIAN_POINT('Ctrl Pts',(-9.93252368000006,15.2,3.06881423499998));
#255063=CARTESIAN_POINT('Ctrl Pts',(-9.93252368000006,11.6,3.06881423499998));
#255064=CARTESIAN_POINT('Ctrl Pts',(-9.93152301100006,15.2,3.06838415799999));
#255065=CARTESIAN_POINT('Ctrl Pts',(-9.93152301100006,11.6,3.06838415799999));
#255066=CARTESIAN_POINT('Ctrl Pts',(-9.93053029600006,15.2,3.06795866099999));
#255067=CARTESIAN_POINT('Ctrl Pts',(-9.93053029600006,11.6,3.06795866099998));
#255068=CARTESIAN_POINT('Ctrl Pts',(-9.92954556500005,15.2,3.06753773799999));
#255069=CARTESIAN_POINT('Ctrl Pts',(-9.92954556500005,11.6,3.06753773799999));
#255070=CARTESIAN_POINT('Ctrl Pts',(-9.92856884700006,15.2,3.06712138399998));
#255071=CARTESIAN_POINT('Ctrl Pts',(-9.92856884700006,11.6,3.06712138399998));
#255072=CARTESIAN_POINT('Ctrl Pts',(-9.92760017000006,15.2,3.06670959199998));
#255073=CARTESIAN_POINT('Ctrl Pts',(-9.92760017000006,11.6,3.06670959199998));
#255074=CARTESIAN_POINT('Ctrl Pts',(-9.92663956700006,15.2,3.06630235699998));
#255075=CARTESIAN_POINT('Ctrl Pts',(-9.92663956700006,11.6,3.06630235699998));
#255076=CARTESIAN_POINT('Ctrl Pts',(-9.92568706800006,15.2,3.06589967099999));
#255077=CARTESIAN_POINT('Ctrl Pts',(-9.92568706800006,11.6,3.06589967099998));
#255078=CARTESIAN_POINT('Ctrl Pts',(-9.92474270200006,15.2,3.06550152999999));
#255079=CARTESIAN_POINT('Ctrl Pts',(-9.92474270200006,11.6,3.06550152999999));
#255080=CARTESIAN_POINT('Ctrl Pts',(-9.92380649900005,15.2,3.06510792799998));
#255081=CARTESIAN_POINT('Ctrl Pts',(-9.92380649900005,11.6,3.06510792799998));
#255082=CARTESIAN_POINT('Ctrl Pts',(-9.92287849100006,15.2,3.06471885699998));
#255083=CARTESIAN_POINT('Ctrl Pts',(-9.92287849100006,11.6,3.06471885699998));
#255084=CARTESIAN_POINT('Ctrl Pts',(-9.92195870900006,15.2,3.06433431199999));
#255085=CARTESIAN_POINT('Ctrl Pts',(-9.92195870900006,11.6,3.06433431199999));
#255086=CARTESIAN_POINT('Ctrl Pts',(-9.92104718300006,15.2,3.06395428599998));
#255087=CARTESIAN_POINT('Ctrl Pts',(-9.92104718300006,11.6,3.06395428599998));
#255088=CARTESIAN_POINT('Ctrl Pts',(-9.92014394400006,15.2,3.06357877499998));
#255089=CARTESIAN_POINT('Ctrl Pts',(-9.92014394400006,11.6,3.06357877499998));
#255090=CARTESIAN_POINT('Ctrl Pts',(-9.91924902500006,15.2,3.06320776899998));
#255091=CARTESIAN_POINT('Ctrl Pts',(-9.91924902500006,11.6,3.06320776899998));
#255092=CARTESIAN_POINT('Ctrl Pts',(-9.91836245600006,15.2,3.06284126399999));
#255093=CARTESIAN_POINT('Ctrl Pts',(-9.91836245600006,11.6,3.06284126399999));
#255094=CARTESIAN_POINT('Ctrl Pts',(-9.91748426900006,15.2,3.06247925299999));
#255095=CARTESIAN_POINT('Ctrl Pts',(-9.91748426900006,11.6,3.06247925299999));
#255096=CARTESIAN_POINT('Ctrl Pts',(-9.91661449500005,15.2,3.06212172999999));
#255097=CARTESIAN_POINT('Ctrl Pts',(-9.91661449500005,11.6,3.06212172999999));
#255098=CARTESIAN_POINT('Ctrl Pts',(-9.91575316600006,15.2,3.06176868799999));
#255099=CARTESIAN_POINT('Ctrl Pts',(-9.91575316600006,11.6,3.06176868799999));
#255100=CARTESIAN_POINT('Ctrl Pts',(-9.91490522600006,15.2,3.06142212699999));
#255101=CARTESIAN_POINT('Ctrl Pts',(-9.91490522600006,11.6,3.06142212699999));
#255102=CARTESIAN_POINT('Ctrl Pts',(-9.91423456700005,15.2,3.06114880399999));
#255103=CARTESIAN_POINT('Ctrl Pts',(-9.91423456700005,11.6,3.06114880399999));
#255104=CARTESIAN_POINT('Ctrl Pts',(-9.91373655900006,15.2,3.06094627499998));
#255105=CARTESIAN_POINT('Ctrl Pts',(-9.91373655900006,11.6,3.06094627499998));
#255106=CARTESIAN_POINT('Ctrl Pts',(-9.91340782700006,15.2,3.06081277699998));
#255107=CARTESIAN_POINT('Ctrl Pts',(-9.91340782700006,11.6,3.06081277699998));
#255108=CARTESIAN_POINT('Ctrl Pts',(-9.91324626500005,15.2,3.06074721299999));
#255109=CARTESIAN_POINT('Ctrl Pts',(-9.91324626500005,11.6,3.06074721299999));
#255110=CARTESIAN_POINT('',(-9.91324626490332,12.2,3.06074721230345));
#255111=CARTESIAN_POINT('',(-9.91324626490332,15.2,3.06074721230345));
#255112=CARTESIAN_POINT('',(-9.91324626500005,12.2,3.06074721199998));
#255113=CARTESIAN_POINT('Ctrl Pts',(-10.8675859440001,12.2,3.76106045599998));
#255114=CARTESIAN_POINT('Ctrl Pts',(-10.8648866835097,12.2,3.75835329050819));
#255115=CARTESIAN_POINT('Ctrl Pts',(-10.8621890332054,12.2,3.75565386693063));
#255116=CARTESIAN_POINT('Ctrl Pts',(-10.859493000351,12.2,3.75296217351306));
#255117=CARTESIAN_POINT('Ctrl Pts',(-10.8567969674967,12.2,3.75027048009549));
#255118=CARTESIAN_POINT('Ctrl Pts',(-10.8541025488079,12.2,3.74758652000514));
#255119=CARTESIAN_POINT('Ctrl Pts',(-10.8514097638127,12.2,3.74491029600946));
#255120=CARTESIAN_POINT('Ctrl Pts',(-10.8487169788175,12.2,3.74223407201377));
#255121=CARTESIAN_POINT('Ctrl Pts',(-10.8460258270055,12.2,3.73956558443436));
#255122=CARTESIAN_POINT('Ctrl Pts',(-10.843336351103,12.2,3.73690483861331));
#255123=CARTESIAN_POINT('Ctrl Pts',(-10.8406468747119,12.2,3.7342440923089));
#255124=CARTESIAN_POINT('Ctrl Pts',(-10.8379590773546,12.2,3.73159108737333));
#255125=CARTESIAN_POINT('Ctrl Pts',(-10.8352730049228,12.2,3.72894582865661));
#255126=CARTESIAN_POINT('Ctrl Pts',(-10.832586932979,12.2,3.72630057042045));
#255127=CARTESIAN_POINT('Ctrl Pts',(-10.8299025886434,12.2,3.72366305998386));
#255128=CARTESIAN_POINT('Ctrl Pts',(-10.8272200099493,12.2,3.72103329924675));
#255129=CARTESIAN_POINT('Ctrl Pts',(-10.8245374312553,12.2,3.71840353850965));
#255130=CARTESIAN_POINT('Ctrl Pts',(-10.8218566176958,12.2,3.71578152924774));
#255131=CARTESIAN_POINT('Ctrl Pts',(-10.8191776064893,12.2,3.71316727449756));
#255132=CARTESIAN_POINT('Ctrl Pts',(-10.8156055917095,12.2,3.70968160165563));
#255133=CARTESIAN_POINT('Ctrl Pts',(-10.8120367800946,12.2,3.7062097149535));
#255134=CARTESIAN_POINT('Ctrl Pts',(-10.808471272108,12.2,3.70275162529033));
#255135=CARTESIAN_POINT('Ctrl Pts',(-10.8057971405108,12.2,3.700158057454));
#255136=CARTESIAN_POINT('Ctrl Pts',(-10.8031248672557,12.2,3.69757225019487));
#255137=CARTESIAN_POINT('Ctrl Pts',(-10.8004544941596,12.2,3.6949942079046));
#255138=CARTESIAN_POINT('Ctrl Pts',(-10.7977841215485,12.2,3.69241616608267));
#255139=CARTESIAN_POINT('Ctrl Pts',(-10.7951156493957,12.2,3.68984588976031));
#255140=CARTESIAN_POINT('Ctrl Pts',(-10.7924491182011,12.2,3.68728338147908));
#255141=CARTESIAN_POINT('Ctrl Pts',(-10.7897825870065,12.2,3.68472087319785));
#255142=CARTESIAN_POINT('Ctrl Pts',(-10.7871179959296,12.2,3.68216613428329));
#255143=CARTESIAN_POINT('Ctrl Pts',(-10.7844553872643,12.2,3.67961916748928));
#255144=CARTESIAN_POINT('Ctrl Pts',(-10.7817927785989,12.2,3.67707220069528));
#255145=CARTESIAN_POINT('Ctrl Pts',(-10.7791321518846,12.2,3.67453300677179));
#255146=CARTESIAN_POINT('Ctrl Pts',(-10.7764735492608,12.2,3.6720015890189));
#255147=CARTESIAN_POINT('Ctrl Pts',(-10.773814946637,12.2,3.66947017126601));
#255148=CARTESIAN_POINT('Ctrl Pts',(-10.7711583682432,12.2,3.66694653110023));
#255149=CARTESIAN_POINT('Ctrl Pts',(-10.7685038565478,12.2,3.66443067123262));
#255150=CARTESIAN_POINT('Ctrl Pts',(-10.7658493448523,12.2,3.66191481136502));
#255151=CARTESIAN_POINT('Ctrl Pts',(-10.7631968984651,12.2,3.65940673118856));
#255152=CARTESIAN_POINT('Ctrl Pts',(-10.7605465608528,12.2,3.65690643582));
#255153=CARTESIAN_POINT('Ctrl Pts',(-10.7570127770487,12.2,3.6535727083591));
#255154=CARTESIAN_POINT('Ctrl Pts',(-10.753482742078,12.2,3.6502528186067));
#255155=CARTESIAN_POINT('Ctrl Pts',(-10.749956554981,12.2,3.64694677702268));
#255156=CARTESIAN_POINT('Ctrl Pts',(-10.7473119148984,12.2,3.6444672460599));
#255157=CARTESIAN_POINT('Ctrl Pts',(-10.7446694401185,12.2,3.64199550282386));
#255158=CARTESIAN_POINT('Ctrl Pts',(-10.7420291729941,12.2,3.63953155298551));
#255159=CARTESIAN_POINT('Ctrl Pts',(-10.7393889058697,12.2,3.63706760314717));
#255160=CARTESIAN_POINT('Ctrl Pts',(-10.7367508461752,12.2,3.63461144652866));
#255161=CARTESIAN_POINT('Ctrl Pts',(-10.7341150375207,12.2,3.63216308474193));
#255162=CARTESIAN_POINT('Ctrl Pts',(-10.7314792288663,12.2,3.6297147229552));
#255163=CARTESIAN_POINT('Ctrl Pts',(-10.7288456702617,12.2,3.62727415762628));
#255164=CARTESIAN_POINT('Ctrl Pts',(-10.7262144070653,12.2,3.62484139129694));
#255165=CARTESIAN_POINT('Ctrl Pts',(-10.7235831433909,12.2,3.62240862452564));
#255166=CARTESIAN_POINT('Ctrl Pts',(-10.7209541732422,12.2,3.61998365750656));
#255167=CARTESIAN_POINT('Ctrl Pts',(-10.7183275401524,12.2,3.61756649273966));
#255168=CARTESIAN_POINT('Ctrl Pts',(-10.7157009075398,12.2,3.61514932841188));
#255169=CARTESIAN_POINT('Ctrl Pts',(-10.7130766121022,12.2,3.61273996628369));
#255170=CARTESIAN_POINT('Ctrl Pts',(-10.7104546984893,12.2,3.61033840995496));
#255171=CARTESIAN_POINT('Ctrl Pts',(-10.7078327848764,12.2,3.60793685362623));
#255172=CARTESIAN_POINT('Ctrl Pts',(-10.7052132530144,12.2,3.60554310333854));
#255173=CARTESIAN_POINT('Ctrl Pts',(-10.7025961450143,12.2,3.60315716149777));
#255174=CARTESIAN_POINT('Ctrl Pts',(-10.6999790370142,12.2,3.600771219657));
#255175=CARTESIAN_POINT('Ctrl Pts',(-10.6973643543527,12.2,3.59839308682676));
#255176=CARTESIAN_POINT('Ctrl Pts',(-10.6947521417274,12.2,3.59602276498542));
#255177=CARTESIAN_POINT('Ctrl Pts',(-10.6921399291021,12.2,3.59365244314408));
#255178=CARTESIAN_POINT('Ctrl Pts',(-10.6895301856731,12.2,3.59128993267185));
#255179=CARTESIAN_POINT('Ctrl Pts',(-10.6869229560593,12.2,3.58893523775673));
#255180=CARTESIAN_POINT('Ctrl Pts',(-10.6834466495917,12.2,3.58579564425137));
#255181=CARTESIAN_POINT('Ctrl Pts',(-10.6799748122803,12.2,3.58266994358657));
#255182=CARTESIAN_POINT('Ctrl Pts',(-10.6765075492583,12.2,3.579558141529));
#255183=CARTESIAN_POINT('Ctrl Pts',(-10.6730402867087,12.2,3.57644633989542));
#255184=CARTESIAN_POINT('Ctrl Pts',(-10.6695776003868,12.2,3.57334843804238));
#255185=CARTESIAN_POINT('Ctrl Pts',(-10.6661195950518,12.2,3.57026444097251));
#255186=CARTESIAN_POINT('Ctrl Pts',(-10.6635260909328,12.2,3.56795144306506));
#255187=CARTESIAN_POINT('Ctrl Pts',(-10.6609352210039,12.2,3.56564626825169));
#255188=CARTESIAN_POINT('Ctrl Pts',(-10.6583470290559,12.2,3.56334891650076));
#255189=CARTESIAN_POINT('Ctrl Pts',(-10.6557588366377,12.2,3.56105156433247));
#255190=CARTESIAN_POINT('Ctrl Pts',(-10.6531733234787,12.2,3.5587620375164));
#255191=CARTESIAN_POINT('Ctrl Pts',(-10.6505905358953,12.2,3.55648033676919));
#255192=CARTESIAN_POINT('Ctrl Pts',(-10.6480077487812,12.2,3.55419863643649));
#255193=CARTESIAN_POINT('Ctrl Pts',(-10.6454276865586,12.2,3.55192476297005));
#255194=CARTESIAN_POINT('Ctrl Pts',(-10.6428503940275,12.2,3.5496587195114));
#255195=CARTESIAN_POINT('Ctrl Pts',(-10.6402731014964,12.2,3.54739267605275));
#255196=CARTESIAN_POINT('Ctrl Pts',(-10.6376985798159,12.2,3.5451344606763));
#255197=CARTESIAN_POINT('Ctrl Pts',(-10.6351268752727,12.2,3.5428840772479));
#255198=CARTESIAN_POINT('Ctrl Pts',(-10.6325551707295,12.2,3.5406336938195));
#255199=CARTESIAN_POINT('Ctrl Pts',(-10.6299862825041,12.2,3.53839114168094));
#255200=CARTESIAN_POINT('Ctrl Pts',(-10.6274202574607,12.2,3.53615642329363));
#255201=CARTESIAN_POINT('Ctrl Pts',(-10.6248542324173,12.2,3.53392170490632));
#255202=CARTESIAN_POINT('Ctrl Pts',(-10.622291070403,12.2,3.531694820112));
#255203=CARTESIAN_POINT('Ctrl Pts',(-10.6197308192875,12.2,3.5294757712336));
#255204=CARTESIAN_POINT('Ctrl Pts',(-10.6171705681719,12.2,3.5272567223552));
#255205=CARTESIAN_POINT('Ctrl Pts',(-10.6146132262978,12.2,3.52504550903462));
#255206=CARTESIAN_POINT('Ctrl Pts',(-10.6120588417652,12.2,3.52284213273861));
#255207=CARTESIAN_POINT('Ctrl Pts',(-10.6086529954124,12.2,3.5199042974104));
#255208=CARTESIAN_POINT('Ctrl Pts',(-10.6052524067926,12.2,3.51698039769193));
#255209=CARTESIAN_POINT('Ctrl Pts',(-10.6018571864811,12.2,3.51407043429795));
#255210=CARTESIAN_POINT('Ctrl Pts',(-10.5993107714787,12.2,3.5118879619507));
#255211=CARTESIAN_POINT('Ctrl Pts',(-10.5967673764883,12.2,3.50971332959972));
#255212=CARTESIAN_POINT('Ctrl Pts',(-10.5942270494857,12.2,3.50754653921024));
#255213=CARTESIAN_POINT('Ctrl Pts',(-10.5908399465079,12.2,3.50465748509517));
#255214=CARTESIAN_POINT('Ctrl Pts',(-10.5874582980759,12.2,3.50178237116998));
#255215=CARTESIAN_POINT('Ctrl Pts',(-10.584082216448,12.2,3.49892120301547));
#255216=CARTESIAN_POINT('Ctrl Pts',(-10.5807061352801,12.2,3.49606003525078));
#255217=CARTESIAN_POINT('Ctrl Pts',(-10.5773356218088,12.2,3.49321281202043));
#255218=CARTESIAN_POINT('Ctrl Pts',(-10.5739707912502,12.2,3.49037953697335));
#255219=CARTESIAN_POINT('Ctrl Pts',(-10.5706059602331,12.2,3.48754626154024));
#255220=CARTESIAN_POINT('Ctrl Pts',(-10.5672468119299,12.2,3.48472693393198));
#255221=CARTESIAN_POINT('Ctrl Pts',(-10.5638934602468,12.2,3.4819215575846));
#255222=CARTESIAN_POINT('Ctrl Pts',(-10.5605401090206,12.2,3.47911618161945));
#255223=CARTESIAN_POINT('Ctrl Pts',(-10.5571925583782,12.2,3.47632475663708));
#255224=CARTESIAN_POINT('Ctrl Pts',(-10.5538509205399,12.2,3.47354728625212));
#255225=CARTESIAN_POINT('Ctrl Pts',(-10.5505092822463,12.2,3.47076981548872));
#255226=CARTESIAN_POINT('Ctrl Pts',(-10.5471735576367,12.2,3.46800629902145));
#255227=CARTESIAN_POINT('Ctrl Pts',(-10.5438438666779,12.2,3.46525673881695));
#255228=CARTESIAN_POINT('Ctrl Pts',(-10.5405141761727,12.2,3.46250717898708));
#255229=CARTESIAN_POINT('Ctrl Pts',(-10.5371905166821,12.2,3.45977157437072));
#255230=CARTESIAN_POINT('Ctrl Pts',(-10.5338730092315,12.2,3.45704992967827));
#255231=CARTESIAN_POINT('Ctrl Pts',(-10.5305555013288,12.2,3.45432828461499));
#255232=CARTESIAN_POINT('Ctrl Pts',(-10.5272441432846,12.2,3.45162059612574));
#255233=CARTESIAN_POINT('Ctrl Pts',(-10.5239390562716,12.2,3.44892686931318));
#255234=CARTESIAN_POINT('Ctrl Pts',(-10.5206339697088,12.2,3.44623314286764));
#255235=CARTESIAN_POINT('Ctrl Pts',(-10.5173351526143,12.2,3.44355337614984));
#255236=CARTESIAN_POINT('Ctrl Pts',(-10.5140427267717,12.2,3.44088757097746));
#255237=CARTESIAN_POINT('Ctrl Pts',(-10.5107503004805,12.2,3.43822176544185));
#255238=CARTESIAN_POINT('Ctrl Pts',(-10.5074642652414,12.2,3.43556992142328));
#255239=CARTESIAN_POINT('Ctrl Pts',(-10.5041847417145,12.2,3.4329320399898));
#255240=CARTESIAN_POINT('Ctrl Pts',(-10.5009052186344,12.2,3.43029415891573));
#255241=CARTESIAN_POINT('Ctrl Pts',(-10.4976322082677,12.2,3.42767023978141));
#255242=CARTESIAN_POINT('Ctrl Pts',(-10.4943658325341,12.2,3.42506028399333));
#255243=CARTESIAN_POINT('Ctrl Pts',(-10.4910994563553,12.2,3.42245032784964));
#255244=CARTESIAN_POINT('Ctrl Pts',(-10.4878397151856,12.2,3.41985433453786));
#255245=CARTESIAN_POINT('Ctrl Pts',(-10.4845867335084,12.2,3.41727230500826));
#255246=CARTESIAN_POINT('Ctrl Pts',(-10.4813337518311,12.2,3.41469027547866));
#255247=CARTESIAN_POINT('Ctrl Pts',(-10.4780875271296,12.2,3.4121222086729));
#255248=CARTESIAN_POINT('Ctrl Pts',(-10.4748481869537,12.2,3.40956810459068));
#255249=CARTESIAN_POINT('Ctrl Pts',(-10.470799012396,12.2,3.4063754750099));
#255250=CARTESIAN_POINT('Ctrl Pts',(-10.466760591561,12.2,3.40320466264262));
#255251=CARTESIAN_POINT('Ctrl Pts',(-10.4627331735268,12.2,3.40005566784516));
#255252=CARTESIAN_POINT('Ctrl Pts',(-10.4595112385727,12.2,3.3975364715953));
#255253=CARTESIAN_POINT('Ctrl Pts',(-10.4562963425026,12.2,3.39503123649959));
#255254=CARTESIAN_POINT('Ctrl Pts',(-10.4530886162167,12.2,3.39253996297493));
#255255=CARTESIAN_POINT('Ctrl Pts',(-10.4498808899308,12.2,3.39004868945026));
#255256=CARTESIAN_POINT('Ctrl Pts',(-10.4466803308679,12.2,3.38757137713001));
#255257=CARTESIAN_POINT('Ctrl Pts',(-10.4434870686946,12.2,3.38510802433052));
#255258=CARTESIAN_POINT('Ctrl Pts',(-10.4402938069564,12.2,3.38264467186666));
#255259=CARTESIAN_POINT('Ctrl Pts',(-10.4371078402922,12.2,3.38019527878154));
#255260=CARTESIAN_POINT('Ctrl Pts',(-10.4339293010516,12.2,3.37775984425749));
#255261=CARTESIAN_POINT('Ctrl Pts',(-10.4307507613779,12.2,3.37532440940161));
#255262=CARTESIAN_POINT('Ctrl Pts',(-10.4275796459097,12.2,3.37290293082871));
#255263=CARTESIAN_POINT('Ctrl Pts',(-10.4244160870244,12.2,3.370495409134));
#255264=CARTESIAN_POINT('Ctrl Pts',(-10.42125252857,12.2,3.36808788776732));
#255265=CARTESIAN_POINT('Ctrl Pts',(-10.4180965276395,12.2,3.36569432139819));
#255266=CARTESIAN_POINT('Ctrl Pts',(-10.4149482140075,12.2,3.36331470820292));
#255267=CARTESIAN_POINT('Ctrl Pts',(-10.4117998999465,12.2,3.36093509468343));
#255268=CARTESIAN_POINT('Ctrl Pts',(-10.4086592756559,12.2,3.35856943385453));
#255269=CARTESIAN_POINT('Ctrl Pts',(-10.4055264709857,12.2,3.35621772178281));
#255270=CARTESIAN_POINT('Ctrl Pts',(-10.4023936667422,12.2,3.35386601003151));
#255271=CARTESIAN_POINT('Ctrl Pts',(-10.3992686851623,12.2,3.35152824936178));
#255272=CARTESIAN_POINT('Ctrl Pts',(-10.3961516574274,12.2,3.34920443404554));
#255273=CARTESIAN_POINT('Ctrl Pts',(-10.3930346292677,12.2,3.34688061841268));
#255274=CARTESIAN_POINT('Ctrl Pts',(-10.3899255578012,12.2,3.34457074838659));
#255275=CARTESIAN_POINT('Ctrl Pts',(-10.3868245770216,12.2,3.34227482026237));
#255276=CARTESIAN_POINT('Ctrl Pts',(-10.3829483512584,12.2,3.3394049102635));
#255277=CARTESIAN_POINT('Ctrl Pts',(-10.3790847675087,12.2,3.33655678533073));
#255278=CARTESIAN_POINT('Ctrl Pts',(-10.3752340934816,12.2,3.33373043533189));
#255279=CARTESIAN_POINT('Ctrl Pts',(-10.3721535545118,12.2,3.33146935551765));
#255280=CARTESIAN_POINT('Ctrl Pts',(-10.3690812778008,12.2,3.32922221276817));
#255281=CARTESIAN_POINT('Ctrl Pts',(-10.366017401953,12.2,3.32698900011572));
#255282=CARTESIAN_POINT('Ctrl Pts',(-10.3629535256877,12.2,3.32475578715899));
#255283=CARTESIAN_POINT('Ctrl Pts',(-10.3598980494387,12.2,3.32253650610016));
#255284=CARTESIAN_POINT('Ctrl Pts',(-10.356851114051,12.2,3.32033115053644));
#255285=CARTESIAN_POINT('Ctrl Pts',(-10.3538041790785,12.2,3.3181257952732));
#255286=CARTESIAN_POINT('Ctrl Pts',(-10.3507657842903,12.2,3.31593436500993));
#255287=CARTESIAN_POINT('Ctrl Pts',(-10.3477360707037,12.2,3.31375685513096));
#255288=CARTESIAN_POINT('Ctrl Pts',(-10.3447063567044,12.2,3.3115793449553));
#255289=CARTESIAN_POINT('Ctrl Pts',(-10.3416853250341,12.2,3.30941575332812));
#255290=CARTESIAN_POINT('Ctrl Pts',(-10.338673117023,12.2,3.3072660762568));
#255291=CARTESIAN_POINT('Ctrl Pts',(-10.3356609094222,12.2,3.30511639947838));
#255292=CARTESIAN_POINT('Ctrl Pts',(-10.3326575241652,12.2,3.30298063452204));
#255293=CARTESIAN_POINT('Ctrl Pts',(-10.3296631084646,12.2,3.30085877663853));
#255294=CARTESIAN_POINT('Ctrl Pts',(-10.3266686923561,12.2,3.29873691846591));
#255295=CARTESIAN_POINT('Ctrl Pts',(-10.3236832434233,12.2,3.29662896572238));
#255296=CARTESIAN_POINT('Ctrl Pts',(-10.3207069074834,12.2,3.29453491277493));
#255297=CARTESIAN_POINT('Ctrl Pts',(-10.3177305715434,12.2,3.29244085982747));
#255298=CARTESIAN_POINT('Ctrl Pts',(-10.3147633490211,12.2,3.29036070391775));
#255299=CARTESIAN_POINT('Ctrl Pts',(-10.3118053857497,12.2,3.28829443969544));
#255300=CARTESIAN_POINT('Ctrl Pts',(-10.3088474228814,12.2,3.28622817575465));
#255301=CARTESIAN_POINT('Ctrl Pts',(-10.3058987195057,12.2,3.2841758029412));
#255302=CARTESIAN_POINT('Ctrl Pts',(-10.3029594240104,12.2,3.28213731170965));
#255303=CARTESIAN_POINT('Ctrl Pts',(-10.3000201281146,12.2,3.28009882020036));
#255304=CARTESIAN_POINT('Ctrl Pts',(-10.2970902409029,12.2,3.27807421134324));
#255305=CARTESIAN_POINT('Ctrl Pts',(-10.2941699115226,12.2,3.27606347517953));
#255306=CARTESIAN_POINT('Ctrl Pts',(-10.2912495825401,12.2,3.27405273928978));
#255307=CARTESIAN_POINT('Ctrl Pts',(-10.2883388099591,12.2,3.27205587713153));
#255308=CARTESIAN_POINT('Ctrl Pts',(-10.2854377470289,12.2,3.27007287790384));
#255309=CARTESIAN_POINT('Ctrl Pts',(-10.2825366837035,12.2,3.26808987840595));
#255310=CARTESIAN_POINT('Ctrl Pts',(-10.279645327446,12.2,3.26612074278043));
#255311=CARTESIAN_POINT('Ctrl Pts',(-10.2767638340903,12.2,3.26416546046629));
#255312=CARTESIAN_POINT('Ctrl Pts',(-10.2738823411272,12.2,3.26221017841855));
#255313=CARTESIAN_POINT('Ctrl Pts',(-10.2710107106674,12.2,3.26026874981486));
#255314=CARTESIAN_POINT('Ctrl Pts',(-10.268149095234,12.2,3.25834116391597));
#255315=CARTESIAN_POINT('Ctrl Pts',(-10.2652874794108,12.2,3.25641357775446));
#255316=CARTESIAN_POINT('Ctrl Pts',(-10.2624358801054,12.2,3.25449983463905));
#255317=CARTESIAN_POINT('Ctrl Pts',(-10.2595944522845,12.2,3.25259992303641));
#255318=CARTESIAN_POINT('Ctrl Pts',(-10.2567530248508,12.2,3.25070001169263));
#255319=CARTESIAN_POINT('Ctrl Pts',(-10.2539217693651,12.2,3.24881393209946));
#255320=CARTESIAN_POINT('Ctrl Pts',(-10.2511008436761,12.2,3.24694167254669));
#255321=CARTESIAN_POINT('Ctrl Pts',(-10.2482799176027,12.2,3.24506941273881));
#255322=CARTESIAN_POINT('Ctrl Pts',(-10.2454693210092,12.2,3.24321097044334));
#255323=CARTESIAN_POINT('Ctrl Pts',(-10.2426692132462,12.2,3.24136633756593));
#255324=CARTESIAN_POINT('Ctrl Pts',(-10.2391690787332,12.2,3.23906054659484));
#255325=CARTESIAN_POINT('Ctrl Pts',(-10.2356853329669,12.2,3.23677632987318));
#255326=CARTESIAN_POINT('Ctrl Pts',(-10.2322182910234,12.2,3.23451366140209));
#255327=CARTESIAN_POINT('Ctrl Pts',(-10.2280578408423,12.2,3.23179845933543));
#255328=CARTESIAN_POINT('Ctrl Pts',(-10.2239214453629,12.2,3.22911428617519));
#255329=CARTESIAN_POINT('Ctrl Pts',(-10.2198096532435,12.2,3.22646109800947));
#255330=CARTESIAN_POINT('Ctrl Pts',(-10.2163831596863,12.2,3.22425010779104));
#255331=CARTESIAN_POINT('Ctrl Pts',(-10.2129737552833,12.2,3.22206063282769));
#255332=CARTESIAN_POINT('Ctrl Pts',(-10.2095817617417,12.2,3.21989264525826));
#255333=CARTESIAN_POINT('Ctrl Pts',(-10.2061897682,12.2,3.21772465768884));
#255334=CARTESIAN_POINT('Ctrl Pts',(-10.2028151879334,12.2,3.21557815805548));
#255335=CARTESIAN_POINT('Ctrl Pts',(-10.199458347725,12.2,3.2134531160416));
#255336=CARTESIAN_POINT('Ctrl Pts',(-10.1961015075167,12.2,3.2113280740277));
#255337=CARTESIAN_POINT('Ctrl Pts',(-10.1927624098355,12.2,3.20922448725264));
#255338=CARTESIAN_POINT('Ctrl Pts',(-10.1894413855149,12.2,3.20714232550713));
#255339=CARTESIAN_POINT('Ctrl Pts',(-10.1861203611943,12.2,3.20506016376162));
#255340=CARTESIAN_POINT('Ctrl Pts',(-10.1828174127621,12.2,3.20299942742668));
#255341=CARTESIAN_POINT('Ctrl Pts',(-10.1795328783186,12.2,3.20096008381668));
#255342=CARTESIAN_POINT('Ctrl Pts',(-10.1762483438752,12.2,3.19892074020669));
#255343=CARTESIAN_POINT('Ctrl Pts',(-10.1729822220812,12.2,3.19690278675725));
#255344=CARTESIAN_POINT('Ctrl Pts',(-10.1697348578461,12.2,3.19490619057781));
#255345=CARTESIAN_POINT('Ctrl Pts',(-10.1664874936109,12.2,3.19290959439837));
#255346=CARTESIAN_POINT('Ctrl Pts',(-10.1632588872309,12.2,3.19093435370264));
#255347=CARTESIAN_POINT('Ctrl Pts',(-10.1600493853358,12.2,3.18898043256485));
#255348=CARTESIAN_POINT('Ctrl Pts',(-10.1568398834407,12.2,3.18702651142707));
#255349=CARTESIAN_POINT('Ctrl Pts',(-10.1536494890226,12.2,3.18509390962597));
#255350=CARTESIAN_POINT('Ctrl Pts',(-10.1504785538853,12.2,3.1831825885166));
#255351=CARTESIAN_POINT('Ctrl Pts',(-10.147307618748,12.2,3.18127126740723));
#255352=CARTESIAN_POINT('Ctrl Pts',(-10.1441561421943,12.2,3.17938122751488));
#255353=CARTESIAN_POINT('Ctrl Pts',(-10.1410244853904,12.2,3.17751242723883));
#255354=CARTESIAN_POINT('Ctrl Pts',(-10.1378928289278,12.2,3.17564362716648));
#255355=CARTESIAN_POINT('Ctrl Pts',(-10.1347809913024,12.2,3.17379606696927));
#255356=CARTESIAN_POINT('Ctrl Pts',(-10.1316893366377,12.2,3.17196970522216));
#255357=CARTESIAN_POINT('Ctrl Pts',(-10.1285976816361,12.2,3.17014334327599));
#255358=CARTESIAN_POINT('Ctrl Pts',(-10.1255262104563,12.2,3.16833817811835));
#255359=CARTESIAN_POINT('Ctrl Pts',(-10.1224752936491,12.2,3.16655416769995));
#255360=CARTESIAN_POINT('Ctrl Pts',(-10.1194243768418,12.2,3.16477015728156));
#255361=CARTESIAN_POINT('Ctrl Pts',(-10.1163940126735,12.2,3.1630073000018));
#255362=CARTESIAN_POINT('Ctrl Pts',(-10.1133845798828,12.2,3.16126555046886));
#255363=CARTESIAN_POINT('Ctrl Pts',(-10.1103751470921,12.2,3.15952380093593));
#255364=CARTESIAN_POINT('Ctrl Pts',(-10.1073866425619,12.2,3.1578031583123));
#255365=CARTESIAN_POINT('Ctrl Pts',(-10.1044194517275,12.2,3.15610357539454));
#255366=CARTESIAN_POINT('Ctrl Pts',(-10.1008588225322,12.2,3.15406407578209));
#255367=CARTESIAN_POINT('Ctrl Pts',(-10.0973288811739,12.2,3.15205490206503));
#255368=CARTESIAN_POINT('Ctrl Pts',(-10.093830302152,12.2,3.15007596654256));
#255369=CARTESIAN_POINT('Ctrl Pts',(-10.0903317234479,12.2,3.14809703119985));
#255370=CARTESIAN_POINT('Ctrl Pts',(-10.0868645050034,12.2,3.14614833417447));
#255371=CARTESIAN_POINT('Ctrl Pts',(-10.0834293342962,12.2,3.14422978391216));
#255372=CARTESIAN_POINT('Ctrl Pts',(-10.0799941635892,12.2,3.14231123364986));
#255373=CARTESIAN_POINT('Ctrl Pts',(-10.0765910392295,12.2,3.1404228306268));
#255374=CARTESIAN_POINT('Ctrl Pts',(-10.0732206606838,12.2,3.13856448010967));
#255375=CARTESIAN_POINT('Ctrl Pts',(-10.0698502821382,12.2,3.13670612959254));
#255376=CARTESIAN_POINT('Ctrl Pts',(-10.0665126507591,12.2,3.134877828016));
#255377=CARTESIAN_POINT('Ctrl Pts',(-10.0632084763768,12.2,3.13307947774596));
#255378=CARTESIAN_POINT('Ctrl Pts',(-10.0599043016944,12.2,3.13128112731257));
#255379=CARTESIAN_POINT('Ctrl Pts',(-10.0566335871653,12.2,3.12951272809042));
#255380=CARTESIAN_POINT('Ctrl Pts',(-10.0533970603237,12.2,3.12777417341364));
#255381=CARTESIAN_POINT('Ctrl Pts',(-10.0501605337762,12.2,3.12603561889478));
#255382=CARTESIAN_POINT('Ctrl Pts',(-10.0469581925425,12.2,3.12432691106407));
#255383=CARTESIAN_POINT('Ctrl Pts',(-10.0437907840598,12.2,3.12264793578403));
#255384=CARTESIAN_POINT('Ctrl Pts',(-10.040623375577,12.2,3.12096896050399));
#255385=CARTESIAN_POINT('Ctrl Pts',(-10.0374908959775,12.2,3.11931972172799));
#255386=CARTESIAN_POINT('Ctrl Pts',(-10.0343941085876,12.2,3.11770010120148));
#255387=CARTESIAN_POINT('Ctrl Pts',(-10.0312973209163,12.2,3.11608048052785));
#255388=CARTESIAN_POINT('Ctrl Pts',(-10.0282362230213,12.2,3.11449047960202));
#255389=CARTESIAN_POINT('Ctrl Pts',(-10.0252115922075,12.2,3.11292997685738));
#255390=CARTESIAN_POINT('Ctrl Pts',(-10.0221869616684,12.2,3.11136947425449));
#255391=CARTESIAN_POINT('Ctrl Pts',(-10.0191987961761,12.2,3.1098384695037));
#255392=CARTESIAN_POINT('Ctrl Pts',(-10.01624789195,12.2,3.10833683697493));
#255393=CARTESIAN_POINT('Ctrl Pts',(-10.0128051701741,12.2,3.1065849322671));
#255394=CARTESIAN_POINT('Ctrl Pts',(-10.0094131616831,12.2,3.10487300692428));
#255395=CARTESIAN_POINT('Ctrl Pts',(-10.0060731590775,12.2,3.10320084962194));
#255396=CARTESIAN_POINT('Ctrl Pts',(-10.0027331567319,12.2,3.10152869244979));
#255397=CARTESIAN_POINT('Ctrl Pts',(-9.99944515810944,12.2,3.09989630294632));
#255398=CARTESIAN_POINT('Ctrl Pts',(-9.99621049204389,12.2,3.0983034604321));
#255399=CARTESIAN_POINT('Ctrl Pts',(-9.99343792080676,12.2,3.09693816668903));
#255400=CARTESIAN_POINT('Ctrl Pts',(-9.99070453057342,12.2,3.09560192724046));
#255401=CARTESIAN_POINT('Ctrl Pts',(-9.98801118034504,12.2,3.09429459642047));
#255402=CARTESIAN_POINT('Ctrl Pts',(-9.98531783036131,12.2,3.09298726571924));
#255403=CARTESIAN_POINT('Ctrl Pts',(-9.98266451873488,12.2,3.09170884286084));
#255404=CARTESIAN_POINT('Ctrl Pts',(-9.9800521229845,12.2,3.09045917523384));
#255405=CARTESIAN_POINT('Ctrl Pts',(-9.97743972723414,12.2,3.08920950760683));
#255406=CARTESIAN_POINT('Ctrl Pts',(-9.97486824733664,12.2,3.08798859625519));
#255407=CARTESIAN_POINT('Ctrl Pts',(-9.97233858175906,12.2,3.0867962796299));
#255408=CARTESIAN_POINT('Ctrl Pts',(-9.9698089159517,12.2,3.08560396289631));
#255409=CARTESIAN_POINT('Ctrl Pts',(-9.96732106555814,12.2,3.08444024334045));
#255410=CARTESIAN_POINT('Ctrl Pts',(-9.96487594972188,12.2,3.08330495239018));
#255411=CARTESIAN_POINT('Ctrl Pts',(-9.96243083410772,12.2,3.08216966154304));
#255412=CARTESIAN_POINT('Ctrl Pts',(-9.96002845450592,12.2,3.08106280104407));
#255413=CARTESIAN_POINT('Ctrl Pts',(-9.95766975500831,12.2,3.07998419524993));
#255414=CARTESIAN_POINT('Ctrl Pts',(-9.9553110555107,12.2,3.0789055894558));
#255415=CARTESIAN_POINT('Ctrl Pts',(-9.95299603625324,12.2,3.07785523960613));
#255416=CARTESIAN_POINT('Ctrl Pts',(-9.95072566671972,12.2,3.07683296384056));
#255417=CARTESIAN_POINT('Ctrl Pts',(-9.94845529697996,12.2,3.07581068798214));
#255418=CARTESIAN_POINT('Ctrl Pts',(-9.94622957706972,12.2,3.07481648578705));
#255419=CARTESIAN_POINT('Ctrl Pts',(-9.94404950253736,12.2,3.07385016965295));
#255420=CARTESIAN_POINT('Ctrl Pts',(-9.94186942820301,12.2,3.07288385360662));
#255421=CARTESIAN_POINT('Ctrl Pts',(-9.93973499797421,12.2,3.07194542162885));
#255422=CARTESIAN_POINT('Ctrl Pts',(-9.93764723495736,12.2,3.07103467774119));
#255423=CARTESIAN_POINT('Ctrl Pts',(-9.9355594719405,12.2,3.07012393385354));
#255424=CARTESIAN_POINT('Ctrl Pts',(-9.93351837835514,12.2,3.0692408780168));
#255425=CARTESIAN_POINT('Ctrl Pts',(-9.93152499959215,12.2,3.06838530304668));
#255426=CARTESIAN_POINT('Ctrl Pts',(-9.92953162064808,12.2,3.06752972799885));
#255427=CARTESIAN_POINT('Ctrl Pts',(-9.92758596123495,12.2,3.0667016350211));
#255428=CARTESIAN_POINT('Ctrl Pts',(-9.92568910105156,12.2,3.06590080714599));
#255429=CARTESIAN_POINT('Ctrl Pts',(-9.92379224104047,12.2,3.06509997934361));
#255430=CARTESIAN_POINT('Ctrl Pts',(-9.92194417655968,12.2,3.06432641939773));
#255431=CARTESIAN_POINT('Ctrl Pts',(-9.92014602387718,12.2,3.06357990125936));
#255432=CARTESIAN_POINT('Ctrl Pts',(-9.91775711673322,12.2,3.06258812646115));
#255433=CARTESIAN_POINT('Ctrl Pts',(-9.91545630147826,12.2,3.06164407508172));
#255434=CARTESIAN_POINT('Ctrl Pts',(-9.91324626500005,12.2,3.06074721299999));
#255435=CARTESIAN_POINT('Ctrl Pts',(-9.91324626500005,15.2,3.06074721299999));
#255436=CARTESIAN_POINT('Ctrl Pts',(-9.91490179640639,15.2,3.0614190495774));
#255437=CARTESIAN_POINT('Ctrl Pts',(-9.91660827013208,15.2,3.06211736672399));
#255438=CARTESIAN_POINT('Ctrl Pts',(-9.91836455129929,15.2,3.06284238742887));
#255439=CARTESIAN_POINT('Ctrl Pts',(-9.92012930214203,15.2,3.06357090455005));
#255440=CARTESIAN_POINT('Ctrl Pts',(-9.92194434197449,15.2,3.06432638668404));
#255441=CARTESIAN_POINT('Ctrl Pts',(-9.92380854792209,15.2,3.06510906085072));
#255442=CARTESIAN_POINT('Ctrl Pts',(-9.92567275370037,15.2,3.0658917349463));
#255443=CARTESIAN_POINT('Ctrl Pts',(-9.92758612406289,15.2,3.06670160226368));
#255444=CARTESIAN_POINT('Ctrl Pts',(-9.92954756824164,15.2,3.06753888023327));
#255445=CARTESIAN_POINT('Ctrl Pts',(-9.93150901242039,15.2,3.06837615820286));
#255446=CARTESIAN_POINT('Ctrl Pts',(-9.93351853346753,15.2,3.06924084660314));
#255447=CARTESIAN_POINT('Ctrl Pts',(-9.93557506757615,15.2,3.07013315544702));
#255448=CARTESIAN_POINT('Ctrl Pts',(-9.93763160187157,15.2,3.07102546437195));
#255449=CARTESIAN_POINT('Ctrl Pts',(-9.93973514987236,15.2,3.07194539273305));
#255450=CARTESIAN_POINT('Ctrl Pts',(-9.94188468124262,15.2,3.07289314078658));
#255451=CARTESIAN_POINT('Ctrl Pts',(-9.94439246754838,15.2,3.07399884671991));
#255452=CARTESIAN_POINT('Ctrl Pts',(-9.94696283892296,15.2,3.07514242100738));
#255453=CARTESIAN_POINT('Ctrl Pts',(-9.94959420704024,15.2,3.07632416439369));
#255454=CARTESIAN_POINT('Ctrl Pts',(-9.9518496656899,15.2,3.07733708741453));
#255455=CARTESIAN_POINT('Ctrl Pts',(-9.95414993737473,15.2,3.07837805331461));
#255456=CARTESIAN_POINT('Ctrl Pts',(-9.9564940500055,15.2,3.07944724612482));
#255457=CARTESIAN_POINT('Ctrl Pts',(-9.95883816242334,15.2,3.0805164388379));
#255458=CARTESIAN_POINT('Ctrl Pts',(-9.96122611435326,15.2,3.08161385563617));
#255459=CARTESIAN_POINT('Ctrl Pts',(-9.96365695802609,15.2,3.08273967526712));
#255460=CARTESIAN_POINT('Ctrl Pts',(-9.96608780169892,15.2,3.08386549489807));
#255461=CARTESIAN_POINT('Ctrl Pts',(-9.9685615367813,15.2,3.08501971462982));
#255462=CARTESIAN_POINT('Ctrl Pts',(-9.97107723760472,15.2,3.08620250341892));
#255463=CARTESIAN_POINT('Ctrl Pts',(-9.97359293865666,15.2,3.08738529231547));
#255464=CARTESIAN_POINT('Ctrl Pts',(-9.97615060723048,15.2,3.0885966503239));
#255465=CARTESIAN_POINT('Ctrl Pts',(-9.97874933929158,15.2,3.08983673714344));
#255466=CARTESIAN_POINT('Ctrl Pts',(-9.98134807111662,15.2,3.09107682385034));
#255467=CARTESIAN_POINT('Ctrl Pts',(-9.98398786750849,15.2,3.09234563980833));
#255468=CARTESIAN_POINT('Ctrl Pts',(-9.98666784641287,15.2,3.09364333934578));
#255469=CARTESIAN_POINT('Ctrl Pts',(-9.98934782531727,15.2,3.09494103888323));
#255470=CARTESIAN_POINT('Ctrl Pts',(-9.99206798928508,15.2,3.09626762011837));
#255471=CARTESIAN_POINT('Ctrl Pts',(-9.99482747534976,15.2,3.09762323365117));
#255472=CARTESIAN_POINT('Ctrl Pts',(-9.99758696141443,15.2,3.09897884718398));
#255473=CARTESIAN_POINT('Ctrl Pts',(-10.0003857714381,15.2,3.10036348897419));
#255474=CARTESIAN_POINT('Ctrl Pts',(-10.0032230664157,15.2,3.1017773053375));
#255475=CARTESIAN_POINT('Ctrl Pts',(-10.0060603616511,15.2,3.10319112182923));
#255476=CARTESIAN_POINT('Ctrl Pts',(-10.0089361398819,15.2,3.10463410825712));
#255477=CARTESIAN_POINT('Ctrl Pts',(-10.0118495822089,15.2,3.10610640108863));
#255478=CARTESIAN_POINT('Ctrl Pts',(-10.0147630242714,15.2,3.10757869378641));
#255479=CARTESIAN_POINT('Ctrl Pts',(-10.0177141286141,15.2,3.10908029397352));
#255480=CARTESIAN_POINT('Ctrl Pts',(-10.0207020948373,15.2,3.11061133041661));
#255481=CARTESIAN_POINT('Ctrl Pts',(-10.0236900610605,15.2,3.1121423668597));
#255482=CARTESIAN_POINT('Ctrl Pts',(-10.026714888605,15.2,3.11370283811974));
#255483=CARTESIAN_POINT('Ctrl Pts',(-10.029775791908,15.2,3.11529286955996));
#255484=CARTESIAN_POINT('Ctrl Pts',(-10.0328366954891,15.2,3.11688290114462));
#255485=CARTESIAN_POINT('Ctrl Pts',(-10.0359336749653,15.2,3.11850249243209));
#255486=CARTESIAN_POINT('Ctrl Pts',(-10.0390659636375,15.2,3.12015176102328));
#255487=CARTESIAN_POINT('Ctrl Pts',(-10.0421982520253,15.2,3.12180102946465));
#255488=CARTESIAN_POINT('Ctrl Pts',(-10.0453658485088,15.2,3.12347997663689));
#255489=CARTESIAN_POINT('Ctrl Pts',(-10.0485680029902,15.2,3.12518871224916));
#255490=CARTESIAN_POINT('Ctrl Pts',(-10.0517701574717,15.2,3.12689744786143));
#255491=CARTESIAN_POINT('Ctrl Pts',(-10.0550068682063,15.2,3.12863597655681));
#255492=CARTESIAN_POINT('Ctrl Pts',(-10.0582774006685,15.2,3.13040440199052));
#255493=CARTESIAN_POINT('Ctrl Pts',(-10.0615479334278,15.2,3.13217282758486));
#255494=CARTESIAN_POINT('Ctrl Pts',(-10.0648522868641,15.2,3.13397115157582));
#255495=CARTESIAN_POINT('Ctrl Pts',(-10.0681897417979,15.2,3.13579947818521));
#255496=CARTESIAN_POINT('Ctrl Pts',(-10.0715271964287,15.2,3.13762780462852));
#255497=CARTESIAN_POINT('Ctrl Pts',(-10.074897751132,15.2,3.13948612996855));
#255498=CARTESIAN_POINT('Ctrl Pts',(-10.0783007007583,15.2,3.14137455723326));
#255499=CARTESIAN_POINT('Ctrl Pts',(-10.0817036503847,15.2,3.14326298449798));
#255500=CARTESIAN_POINT('Ctrl Pts',(-10.0851389938609,15.2,3.14518151107001));
#255501=CARTESIAN_POINT('Ctrl Pts',(-10.0886060406564,15.2,3.14713023059483));
#255502=CARTESIAN_POINT('Ctrl Pts',(-10.0914952464242,15.2,3.14875416359118));
#255503=CARTESIAN_POINT('Ctrl Pts',(-10.0944064663428,15.2,3.15039906414221));
#255504=CARTESIAN_POINT('Ctrl Pts',(-10.0973393103,15.2,3.15206498434944));
#255505=CARTESIAN_POINT('Ctrl Pts',(-10.1002721542572,15.2,3.15373090455667));
#255506=CARTESIAN_POINT('Ctrl Pts',(-10.1032266195011,15.2,3.15541784366724));
#255507=CARTESIAN_POINT('Ctrl Pts',(-10.1062023202639,15.2,3.15712585234669));
#255508=CARTESIAN_POINT('Ctrl Pts',(-10.1091780210266,15.2,3.15883386102613));
#255509=CARTESIAN_POINT('Ctrl Pts',(-10.1121749576847,15.2,3.16056293924108));
#255510=CARTESIAN_POINT('Ctrl Pts',(-10.1151927476984,15.2,3.16231313299898));
#255511=CARTESIAN_POINT('Ctrl Pts',(-10.118210537712,15.2,3.16406332675688));
#255512=CARTESIAN_POINT('Ctrl Pts',(-10.1212491828166,15.2,3.16583463838325));
#255513=CARTESIAN_POINT('Ctrl Pts',(-10.1243083069833,15.2,3.16762711275826));
#255514=CARTESIAN_POINT('Ctrl Pts',(-10.12736743115,15.2,3.16941958713328));
#255515=CARTESIAN_POINT('Ctrl Pts',(-10.1304470343987,15.2,3.17123322348144));
#255516=CARTESIAN_POINT('Ctrl Pts',(-10.13354674851,15.2,3.1730680662676));
#255517=CARTESIAN_POINT('Ctrl Pts',(-10.1366464626214,15.2,3.17490290905376));
#255518=CARTESIAN_POINT('Ctrl Pts',(-10.1397662852044,15.2,3.1767589591106));
#255519=CARTESIAN_POINT('Ctrl Pts',(-10.1429058554138,15.2,3.1786362568895));
#255520=CARTESIAN_POINT('Ctrl Pts',(-10.1460454256232,15.2,3.1805135546684));
#255521=CARTESIAN_POINT('Ctrl Pts',(-10.1492047427681,15.2,3.18241210039117));
#255522=CARTESIAN_POINT('Ctrl Pts',(-10.152383447908,15.2,3.18433193560062));
#255523=CARTESIAN_POINT('Ctrl Pts',(-10.1555621530479,15.2,3.18625177081007));
#255524=CARTESIAN_POINT('Ctrl Pts',(-10.1587602468726,15.2,3.18819289427828));
#255525=CARTESIAN_POINT('Ctrl Pts',(-10.1619773771735,15.2,3.19015534396115));
#255526=CARTESIAN_POINT('Ctrl Pts',(-10.1651945074745,15.2,3.19211779364402));
#255527=CARTESIAN_POINT('Ctrl Pts',(-10.168430672052,15.2,3.19410157105491));
#255528=CARTESIAN_POINT('Ctrl Pts',(-10.1716855249007,15.2,3.19610671202887));
#255529=CARTESIAN_POINT('Ctrl Pts',(-10.1749403777495,15.2,3.19811185300284));
#255530=CARTESIAN_POINT('Ctrl Pts',(-10.1782139201625,15.2,3.20013835541051));
#255531=CARTESIAN_POINT('Ctrl Pts',(-10.1815058064139,15.2,3.20218625805114));
#255532=CARTESIAN_POINT('Ctrl Pts',(-10.1847976923066,15.2,3.20423416046855));
#255533=CARTESIAN_POINT('Ctrl Pts',(-10.1881079253789,15.2,3.2063034610061));
#255534=CARTESIAN_POINT('Ctrl Pts',(-10.1914361660564,15.2,3.20839419348481));
#255535=CARTESIAN_POINT('Ctrl Pts',(-10.1947644070966,15.2,3.21048492619141));
#255536=CARTESIAN_POINT('Ctrl Pts',(-10.1981106542948,15.2,3.21259708975038));
#255537=CARTESIAN_POINT('Ctrl Pts',(-10.201474577835,15.2,3.21473071592919));
#255538=CARTESIAN_POINT('Ctrl Pts',(-10.2048385013752,15.2,3.216864342108));
#255539=CARTESIAN_POINT('Ctrl Pts',(-10.2082200995068,15.2,3.21901943262257));
#255540=CARTESIAN_POINT('Ctrl Pts',(-10.2116190440888,15.2,3.2211960162319));
#255541=CARTESIAN_POINT('Ctrl Pts',(-10.2163775665775,15.2,3.22424323333242));
#255542=CARTESIAN_POINT('Ctrl Pts',(-10.2211700890845,15.2,3.2273325767247));
#255543=CARTESIAN_POINT('Ctrl Pts',(-10.2259957249731,15.2,3.23046412498205));
#255544=CARTESIAN_POINT('Ctrl Pts',(-10.2294426076971,15.2,3.23270094513103));
#255545=CARTESIAN_POINT('Ctrl Pts',(-10.2329063843833,15.2,3.23495929677216));
#255546=CARTESIAN_POINT('Ctrl Pts',(-10.2363867389667,15.2,3.23723920850826));
#255547=CARTESIAN_POINT('Ctrl Pts',(-10.23986709355,15.2,3.23951912024437));
#255548=CARTESIAN_POINT('Ctrl Pts',(-10.2433640257081,15.2,3.2418205893017));
#255549=CARTESIAN_POINT('Ctrl Pts',(-10.2468772212103,15.2,3.2441436444512));
#255550=CARTESIAN_POINT('Ctrl Pts',(-10.2496877773822,15.2,3.24600208841888));
#255551=CARTESIAN_POINT('Ctrl Pts',(-10.2525087432196,15.2,3.24787434481106));
#255552=CARTESIAN_POINT('Ctrl Pts',(-10.2553399593204,15.2,3.24976042793323));
#255553=CARTESIAN_POINT('Ctrl Pts',(-10.2588789797358,15.2,3.25211803202867));
#255554=CARTESIAN_POINT('Ctrl Pts',(-10.2624340161231,15.2,3.25449723837101));
#255555=CARTESIAN_POINT('Ctrl Pts',(-10.2660047632746,15.2,3.2568980694109));
#255556=CARTESIAN_POINT('Ctrl Pts',(-10.2688613611515,15.2,3.25881873434749));
#255557=CARTESIAN_POINT('Ctrl Pts',(-10.2717280136849,15.2,3.26075324027506));
#255558=CARTESIAN_POINT('Ctrl Pts',(-10.2746045662436,15.2,3.26270159650126));
#255559=CARTESIAN_POINT('Ctrl Pts',(-10.2774811184105,15.2,3.26464995246201));
#255560=CARTESIAN_POINT('Ctrl Pts',(-10.2803675712281,15.2,3.2666121592287));
#255561=CARTESIAN_POINT('Ctrl Pts',(-10.2832637712682,15.2,3.26858822717685));
#255562=CARTESIAN_POINT('Ctrl Pts',(-10.2861599717028,15.2,3.27056429539425));
#255563=CARTESIAN_POINT('Ctrl Pts',(-10.2890659173939,15.2,3.27255422432683));
#255564=CARTESIAN_POINT('Ctrl Pts',(-10.291981459275,15.2,3.27455802449159));
#255565=CARTESIAN_POINT('Ctrl Pts',(-10.2948970011561,15.2,3.27656182465636));
#255566=CARTESIAN_POINT('Ctrl Pts',(-10.2978221372106,15.2,3.27857949547553));
#255567=CARTESIAN_POINT('Ctrl Pts',(-10.3007567192048,15.2,3.28061104636543));
#255568=CARTESIAN_POINT('Ctrl Pts',(-10.3036913007992,15.2,3.28264259697854));
#255569=CARTESIAN_POINT('Ctrl Pts',(-10.3066353289011,15.2,3.28468802705759));
#255570=CARTESIAN_POINT('Ctrl Pts',(-10.3095886525063,15.2,3.28674734623186));
#255571=CARTESIAN_POINT('Ctrl Pts',(-10.312541976514,15.2,3.28880666568672));
#255572=CARTESIAN_POINT('Ctrl Pts',(-10.315504597248,15.2,3.29087987424546));
#255573=CARTESIAN_POINT('Ctrl Pts',(-10.3184763672442,15.2,3.29296697908285));
#255574=CARTESIAN_POINT('Ctrl Pts',(-10.3214481368356,15.2,3.29505408363586));
#255575=CARTESIAN_POINT('Ctrl Pts',(-10.3244290566257,15.2,3.29715508371764));
#255576=CARTESIAN_POINT('Ctrl Pts',(-10.3274189795473,15.2,3.29926998954384));
#255577=CARTESIAN_POINT('Ctrl Pts',(-10.3304089028764,15.2,3.30138489565818));
#255578=CARTESIAN_POINT('Ctrl Pts',(-10.3334078306799,15.2,3.30351370493313));
#255579=CARTESIAN_POINT('Ctrl Pts',(-10.3364156181615,15.2,3.3056564271026));
#255580=CARTESIAN_POINT('Ctrl Pts',(-10.3394234052333,15.2,3.30779914898013));
#255581=CARTESIAN_POINT('Ctrl Pts',(-10.3424400511451,15.2,3.30995578118986));
#255582=CARTESIAN_POINT('Ctrl Pts',(-10.3454654147861,15.2,3.31212633178928));
#255583=CARTESIAN_POINT('Ctrl Pts',(-10.3484907788393,15.2,3.31429688268444));
#255584=CARTESIAN_POINT('Ctrl Pts',(-10.3515248598547,15.2,3.31648135171185));
#255585=CARTESIAN_POINT('Ctrl Pts',(-10.3545675164655,15.2,3.31867974522145));
#255586=CARTESIAN_POINT('Ctrl Pts',(-10.3591315009672,15.2,3.32197733518632));
#255587=CARTESIAN_POINT('Ctrl Pts',(-10.3637147797943,15.2,3.32530625355529));
#255588=CARTESIAN_POINT('Ctrl Pts',(-10.3683168814813,15.2,3.32866652144842));
#255589=CARTESIAN_POINT('Ctrl Pts',(-10.3721519663598,15.2,3.33146674479442));
#255590=CARTESIAN_POINT('Ctrl Pts',(-10.3760001236834,15.2,3.33428873678882));
#255591=CARTESIAN_POINT('Ctrl Pts',(-10.3798610820167,15.2,3.33713250852493));
#255592=CARTESIAN_POINT('Ctrl Pts',(-10.3829498488517,15.2,3.3394075260378));
#255593=CARTESIAN_POINT('Ctrl Pts',(-10.3860468104877,15.2,3.3416964817162));
#255594=CARTESIAN_POINT('Ctrl Pts',(-10.389151827991,15.2,3.34399938117647));
#255595=CARTESIAN_POINT('Ctrl Pts',(-10.3938093538231,15.2,3.34745373005311));
#255596=CARTESIAN_POINT('Ctrl Pts',(-10.3984850090923,15.2,3.35093944899316));
#255597=CARTESIAN_POINT('Ctrl Pts',(-10.4031783367559,15.2,3.35445655395008));
#255598=CARTESIAN_POINT('Ctrl Pts',(-10.4063072217228,15.2,3.35680129048154));
#255599=CARTESIAN_POINT('Ctrl Pts',(-10.4094439605215,15.2,3.35915997647408));
#255600=CARTESIAN_POINT('Ctrl Pts',(-10.4125884214859,15.2,3.36153261361201));
#255601=CARTESIAN_POINT('Ctrl Pts',(-10.4157328828787,15.2,3.36390525107321));
#255602=CARTESIAN_POINT('Ctrl Pts',(-10.4188850653795,15.2,3.36629184082924));
#255603=CARTESIAN_POINT('Ctrl Pts',(-10.4220448375105,15.2,3.36869238502657));
#255604=CARTESIAN_POINT('Ctrl Pts',(-10.425204609211,15.2,3.37109292889682));
#255605=CARTESIAN_POINT('Ctrl Pts',(-10.4283719699801,15.2,3.37350742790006));
#255606=CARTESIAN_POINT('Ctrl Pts',(-10.4315467894976,15.2,3.37593588431122));
#255607=CARTESIAN_POINT('Ctrl Pts',(-10.4347216094477,15.2,3.37836434105326));
#255608=CARTESIAN_POINT('Ctrl Pts',(-10.4379038865457,15.2,3.3808067540494));
#255609=CARTESIAN_POINT('Ctrl Pts',(-10.441093492775,15.2,3.38326312751659));
#255610=CARTESIAN_POINT('Ctrl Pts',(-10.4442830990044,15.2,3.38571950098379));
#255611=CARTESIAN_POINT('Ctrl Pts',(-10.4474800332957,15.2,3.38818983253317));
#255612=CARTESIAN_POINT('Ctrl Pts',(-10.4506841680822,15.2,3.39067412594779));
#255613=CARTESIAN_POINT('Ctrl Pts',(-10.4538883024322,15.2,3.39315841902392));
#255614=CARTESIAN_POINT('Ctrl Pts',(-10.4570996364978,15.2,3.39565667293709));
#255615=CARTESIAN_POINT('Ctrl Pts',(-10.460318043512,15.2,3.39816888811968));
#255616=CARTESIAN_POINT('Ctrl Pts',(-10.4643410526086,15.2,3.40130915735464));
#255617=CARTESIAN_POINT('Ctrl Pts',(-10.4683751125128,15.2,3.40447124263936));
#255618=CARTESIAN_POINT('Ctrl Pts',(-10.4724199752395,15.2,3.4076551452232));
#255619=CARTESIAN_POINT('Ctrl Pts',(-10.4756558655972,15.2,3.41020226742909));
#255620=CARTESIAN_POINT('Ctrl Pts',(-10.4788986713508,15.2,3.41276335327921));
#255621=CARTESIAN_POINT('Ctrl Pts',(-10.4821482668063,15.2,3.41533840142096));
#255622=CARTESIAN_POINT('Ctrl Pts',(-10.4853978618192,15.2,3.41791344921187));
#255623=CARTESIAN_POINT('Ctrl Pts',(-10.48865424527,15.2,3.42050245983154));
#255624=CARTESIAN_POINT('Ctrl Pts',(-10.491917295725,15.2,3.42310543422893));
#255625=CARTESIAN_POINT('Ctrl Pts',(-10.4951803466246,15.2,3.42570840898098));
#255626=CARTESIAN_POINT('Ctrl Pts',(-10.4984500630188,15.2,3.42832534704185));
#255627=CARTESIAN_POINT('Ctrl Pts',(-10.5017263227505,15.2,3.43095624737344));
#255628=CARTESIAN_POINT('Ctrl Pts',(-10.5050025820358,15.2,3.43358714734657));
#255629=CARTESIAN_POINT('Ctrl Pts',(-10.5082853834505,15.2,3.43623200882598));
#255630=CARTESIAN_POINT('Ctrl Pts',(-10.5115746065145,15.2,3.43889083377437));
#255631=CARTESIAN_POINT('Ctrl Pts',(-10.5148638300267,15.2,3.44154965908503));
#255632=CARTESIAN_POINT('Ctrl Pts',(-10.5181594741563,15.2,3.44422244537237));
#255633=CARTESIAN_POINT('Ctrl Pts',(-10.5214614190034,15.2,3.44690919218637));
#255634=CARTESIAN_POINT('Ctrl Pts',(-10.5247633634005,15.2,3.4495959386343));
#255635=CARTESIAN_POINT('Ctrl Pts',(-10.52807160805,15.2,3.45229664563806));
#255636=CARTESIAN_POINT('Ctrl Pts',(-10.5313860327774,15.2,3.45501131210608));
#255637=CARTESIAN_POINT('Ctrl Pts',(-10.5347004579565,15.2,3.45772597894398));
#255638=CARTESIAN_POINT('Ctrl Pts',(-10.5380210651709,15.2,3.46045460300166));
#255639=CARTESIAN_POINT('Ctrl Pts',(-10.541347732297,15.2,3.4631971857076));
#255640=CARTESIAN_POINT('Ctrl Pts',(-10.54467439897,15.2,3.46593976803986));
#255641=CARTESIAN_POINT('Ctrl Pts',(-10.5480071279777,15.2,3.46869630590821));
#255642=CARTESIAN_POINT('Ctrl Pts',(-10.5513458017042,15.2,3.47146679901363));
#255643=CARTESIAN_POINT('Ctrl Pts',(-10.5555191442034,15.2,3.4749299156785));
#255644=CARTESIAN_POINT('Ctrl Pts',(-10.5597017708714,15.2,3.47841483734146));
#255645=CARTESIAN_POINT('Ctrl Pts',(-10.5638934602468,15.2,3.48192155758459));
#255646=CARTESIAN_POINT('Ctrl Pts',(-10.5672468119299,15.2,3.48472693393199));
#255647=CARTESIAN_POINT('Ctrl Pts',(-10.5706059602331,15.2,3.48754626154025));
#255648=CARTESIAN_POINT('Ctrl Pts',(-10.5739707912502,15.2,3.49037953697335));
#255649=CARTESIAN_POINT('Ctrl Pts',(-10.5773356218088,15.2,3.49321281202042));
#255650=CARTESIAN_POINT('Ctrl Pts',(-10.5807061352802,15.2,3.4960600352508));
#255651=CARTESIAN_POINT('Ctrl Pts',(-10.584082216448,15.2,3.49892120301546));
#255652=CARTESIAN_POINT('Ctrl Pts',(-10.5874582980759,15.2,3.50178237116996));
#255653=CARTESIAN_POINT('Ctrl Pts',(-10.5908399465079,15.2,3.50465748509516));
#255654=CARTESIAN_POINT('Ctrl Pts',(-10.5942270494857,15.2,3.50754653921024));
#255655=CARTESIAN_POINT('Ctrl Pts',(-10.5984609279772,15.2,3.51115785665726));
#255656=CARTESIAN_POINT('Ctrl Pts',(-10.602703328461,15.2,3.51479095735461));
#255657=CARTESIAN_POINT('Ctrl Pts',(-10.6069540295031,15.2,3.51844583152242));
#255658=CARTESIAN_POINT('Ctrl Pts',(-10.6095044500357,15.2,3.52063875594344));
#255659=CARTESIAN_POINT('Ctrl Pts',(-10.6120578590762,15.2,3.52283952013017));
#255660=CARTESIAN_POINT('Ctrl Pts',(-10.614614210025,15.2,3.52504812100826));
#255661=CARTESIAN_POINT('Ctrl Pts',(-10.6171705609738,15.2,3.52725672188634));
#255662=CARTESIAN_POINT('Ctrl Pts',(-10.6197298519475,15.2,3.52947315910579));
#255663=CARTESIAN_POINT('Ctrl Pts',(-10.6222920384375,15.2,3.53169743152428));
#255664=CARTESIAN_POINT('Ctrl Pts',(-10.6248542249275,15.2,3.53392170394277));
#255665=CARTESIAN_POINT('Ctrl Pts',(-10.6274193061352,15.2,3.53615381175369));
#255666=CARTESIAN_POINT('Ctrl Pts',(-10.6299872347949,15.2,3.5383937522833));
#255667=CARTESIAN_POINT('Ctrl Pts',(-10.6325551634546,15.2,3.54063369281291));
#255668=CARTESIAN_POINT('Ctrl Pts',(-10.6351259392829,15.2,3.54288146640791));
#255669=CARTESIAN_POINT('Ctrl Pts',(-10.637699516439,15.2,3.54513707074155));
#255670=CARTESIAN_POINT('Ctrl Pts',(-10.6411309529588,15.2,3.54814454345958));
#255671=CARTESIAN_POINT('Ctrl Pts',(-10.6445673715569,15.2,3.55116593574284));
#255672=CARTESIAN_POINT('Ctrl Pts',(-10.6480086593,15.2,3.55420124574159));
#255673=CARTESIAN_POINT('Ctrl Pts',(-10.6505896248729,15.2,3.55647772803387));
#255674=CARTESIAN_POINT('Ctrl Pts',(-10.653173330379,15.2,3.55876203735084));
#255675=CARTESIAN_POINT('Ctrl Pts',(-10.6557597309515,15.2,3.56105417222522));
#255676=CARTESIAN_POINT('Ctrl Pts',(-10.658346131524,15.2,3.5633463070996));
#255677=CARTESIAN_POINT('Ctrl Pts',(-10.6609352262303,15.2,3.56564626722296));
#255678=CARTESIAN_POINT('Ctrl Pts',(-10.663526969432,15.2,3.56795404975351));
#255679=CARTESIAN_POINT('Ctrl Pts',(-10.6661187126336,15.2,3.57026183228405));
#255680=CARTESIAN_POINT('Ctrl Pts',(-10.6687131043286,15.2,3.57257743834558));
#255681=CARTESIAN_POINT('Ctrl Pts',(-10.6713100994422,15.2,3.57490086376009));
#255682=CARTESIAN_POINT('Ctrl Pts',(-10.6756384247888,15.2,3.57877323959165));
#255683=CARTESIAN_POINT('Ctrl Pts',(-10.6799739830493,15.2,3.58266733873398));
#255684=CARTESIAN_POINT('Ctrl Pts',(-10.6843165649237,15.2,3.58658314699608));
#255685=CARTESIAN_POINT('Ctrl Pts',(-10.686922114427,15.2,3.5889326322948));
#255686=CARTESIAN_POINT('Ctrl Pts',(-10.6895301923061,15.2,3.59128993327075));
#255687=CARTESIAN_POINT('Ctrl Pts',(-10.6921407543525,15.2,3.59365504753221));
#255688=CARTESIAN_POINT('Ctrl Pts',(-10.6964916899899,15.2,3.59759690363209));
#255689=CARTESIAN_POINT('Ctrl Pts',(-10.7008495273388,15.2,3.60156046047041));
#255690=CARTESIAN_POINT('Ctrl Pts',(-10.7052140589458,15.2,3.60554570572867));
#255691=CARTESIAN_POINT('Ctrl Pts',(-10.7078327785761,15.2,3.60793685349177));
#255692=CARTESIAN_POINT('Ctrl Pts',(-10.7104539082404,15.2,3.61033580879043));
#255693=CARTESIAN_POINT('Ctrl Pts',(-10.7130774052886,15.2,3.61274256905795));
#255694=CARTESIAN_POINT('Ctrl Pts',(-10.7157009018603,15.2,3.61514932888825));
#255695=CARTESIAN_POINT('Ctrl Pts',(-10.7183267652652,15.2,3.61756389310142));
#255696=CARTESIAN_POINT('Ctrl Pts',(-10.7209549512949,15.2,3.6199862585141));
#255697=CARTESIAN_POINT('Ctrl Pts',(-10.7244591991754,15.2,3.62321607891765));
#255698=CARTESIAN_POINT('Ctrl Pts',(-10.7279675751078,15.2,3.62645976929894));
#255699=CARTESIAN_POINT('Ctrl Pts',(-10.7314799797091,15.2,3.62971732097566));
#255700=CARTESIAN_POINT('Ctrl Pts',(-10.7341142837583,15.2,3.63216048528799));
#255701=CARTESIAN_POINT('Ctrl Pts',(-10.7367508527415,15.2,3.63461144712754));
#255702=CARTESIAN_POINT('Ctrl Pts',(-10.7393896438336,15.2,3.63707020152762));
#255703=CARTESIAN_POINT('Ctrl Pts',(-10.7420284344464,15.2,3.63952895548101));
#255704=CARTESIAN_POINT('Ctrl Pts',(-10.7446694469752,15.2,3.64199550427745));
#255705=CARTESIAN_POINT('Ctrl Pts',(-10.7473126387614,15.2,3.64446984272873));
#255706=CARTESIAN_POINT('Ctrl Pts',(-10.7499558305477,15.2,3.64694418118));
#255707=CARTESIAN_POINT('Ctrl Pts',(-10.7526012021013,15.2,3.64942630929459));
#255708=CARTESIAN_POINT('Ctrl Pts',(-10.755248709297,15.2,3.6519162245798));
#255709=CARTESIAN_POINT('Ctrl Pts',(-10.7578962164926,15.2,3.654406139865));
#255710=CARTESIAN_POINT('Ctrl Pts',(-10.7605458606131,15.2,3.6569038406743));
#255711=CARTESIAN_POINT('Ctrl Pts',(-10.763197599225,15.2,3.65940932545826));
#255712=CARTESIAN_POINT('Ctrl Pts',(-10.7676171637389,15.2,3.66358513358326));
#255713=CARTESIAN_POINT('Ctrl Pts',(-10.7720425447268,15.2,3.66778255927747));
#255714=CARTESIAN_POINT('Ctrl Pts',(-10.7764735492608,15.2,3.6720015890189));
#255715=CARTESIAN_POINT('Ctrl Pts',(-10.7791321518846,15.2,3.67453300677179));
#255716=CARTESIAN_POINT('Ctrl Pts',(-10.781792778599,15.2,3.6770722006953));
#255717=CARTESIAN_POINT('Ctrl Pts',(-10.7844553872643,15.2,3.67961916748929));
#255718=CARTESIAN_POINT('Ctrl Pts',(-10.7871179959296,15.2,3.68216613428328));
#255719=CARTESIAN_POINT('Ctrl Pts',(-10.7897825870065,15.2,3.68472087319786));
#255720=CARTESIAN_POINT('Ctrl Pts',(-10.7924491182011,15.2,3.68728338147908));
#255721=CARTESIAN_POINT('Ctrl Pts',(-10.7951156493957,15.2,3.68984588976029));
#255722=CARTESIAN_POINT('Ctrl Pts',(-10.7977841215485,15.2,3.69241616608266));
#255723=CARTESIAN_POINT('Ctrl Pts',(-10.8004544941596,15.2,3.69499420790458));
#255724=CARTESIAN_POINT('Ctrl Pts',(-10.8031248672557,15.2,3.69757225019485));
#255725=CARTESIAN_POINT('Ctrl Pts',(-10.8057971405108,15.2,3.70015805745401));
#255726=CARTESIAN_POINT('Ctrl Pts',(-10.808471272108,15.2,3.70275162529034));
#255727=CARTESIAN_POINT('Ctrl Pts',(-10.8120367800946,15.2,3.70620971495349));
#255728=CARTESIAN_POINT('Ctrl Pts',(-10.8156055917095,15.2,3.70968160165562));
#255729=CARTESIAN_POINT('Ctrl Pts',(-10.8191776064893,15.2,3.71316727449756));
#255730=CARTESIAN_POINT('Ctrl Pts',(-10.8218566176958,15.2,3.71578152924775));
#255731=CARTESIAN_POINT('Ctrl Pts',(-10.8245374312553,15.2,3.71840353850963));
#255732=CARTESIAN_POINT('Ctrl Pts',(-10.8272200099493,15.2,3.72103329924674));
#255733=CARTESIAN_POINT('Ctrl Pts',(-10.8299025886434,15.2,3.72366305998386));
#255734=CARTESIAN_POINT('Ctrl Pts',(-10.832586932979,15.2,3.72630057042044));
#255735=CARTESIAN_POINT('Ctrl Pts',(-10.8352730049228,15.2,3.7289458286566));
#255736=CARTESIAN_POINT('Ctrl Pts',(-10.8379590773546,15.2,3.73159108737332));
#255737=CARTESIAN_POINT('Ctrl Pts',(-10.8406468747119,15.2,3.7342440923089));
#255738=CARTESIAN_POINT('Ctrl Pts',(-10.843336351103,15.2,3.73690483861332));
#255739=CARTESIAN_POINT('Ctrl Pts',(-10.8460258270055,15.2,3.73956558443437));
#255740=CARTESIAN_POINT('Ctrl Pts',(-10.8487169788175,15.2,3.74223407201378));
#255741=CARTESIAN_POINT('Ctrl Pts',(-10.8514097638127,15.2,3.74491029600946));
#255742=CARTESIAN_POINT('Ctrl Pts',(-10.8541025488079,15.2,3.74758652000514));
#255743=CARTESIAN_POINT('Ctrl Pts',(-10.8567969674967,15.2,3.75027048009548));
#255744=CARTESIAN_POINT('Ctrl Pts',(-10.859493000351,15.2,3.75296217351306));
#255745=CARTESIAN_POINT('Ctrl Pts',(-10.8621890332054,15.2,3.75565386693064));
#255746=CARTESIAN_POINT('Ctrl Pts',(-10.8648866835097,15.2,3.75835329050819));
#255747=CARTESIAN_POINT('Ctrl Pts',(-10.8675859440001,15.2,3.76106045599998));
#255748=CARTESIAN_POINT('Origin',(-5.66257110645729E-14,15.2,-1.77635683940025E-14));
#255749=CARTESIAN_POINT('',(-10.0330625580001,15.2,2.64164356399998));
#255750=CARTESIAN_POINT('',(-10.0330625580001,12.2,2.64164356399998));
#255751=CARTESIAN_POINT('',(-10.0330625580001,15.2,2.64164356399998));
#255752=CARTESIAN_POINT('Origin',(-5.66257110645729E-14,12.2,-1.77635683940025E-14));
#255753=CARTESIAN_POINT('Origin',(-5.66257110645729E-14,15.2,-1.77635683940025E-14));
#255754=CARTESIAN_POINT('Origin',(-5.66257110645729E-14,15.2,-1.77635683940025E-14));
#255755=CARTESIAN_POINT('',(-11.213356592485,15.2,2.55159438995864));
#255756=CARTESIAN_POINT('',(-11.292224299446,15.2,2.17615954695745));
#255757=CARTESIAN_POINT('Origin',(-5.66257110645729E-14,15.2,-1.77635683940025E-14));
#255758=CARTESIAN_POINT('',(-11.292224299446,12.2,2.17615954695745));
#255759=CARTESIAN_POINT('',(-11.2922243000001,15.2,2.17615954699999));
#255760=CARTESIAN_POINT('',(-11.213356592485,12.2,2.55159438995864));
#255761=CARTESIAN_POINT('Origin',(-5.66257110645729E-14,12.2,-1.77635683940025E-14));
#255762=CARTESIAN_POINT('',(-11.2133565930001,15.2,2.55159438999998));
#255763=CARTESIAN_POINT('Ctrl Pts',(-11.2922242990001,15.2,2.17615954699999));
#255764=CARTESIAN_POINT('Ctrl Pts',(-11.2922242990001,11.6,2.17615954699998));
#255765=CARTESIAN_POINT('Ctrl Pts',(-11.2916128880001,15.2,2.17570045599999));
#255766=CARTESIAN_POINT('Ctrl Pts',(-11.2916128880001,11.6,2.17570045599999));
#255767=CARTESIAN_POINT('Ctrl Pts',(-11.2903902450001,15.2,2.17478276599998));
#255768=CARTESIAN_POINT('Ctrl Pts',(-11.2903902450001,11.6,2.17478276599998));
#255769=CARTESIAN_POINT('Ctrl Pts',(-11.2885568210001,15.2,2.17340771699998));
#255770=CARTESIAN_POINT('Ctrl Pts',(-11.2885568210001,11.6,2.17340771699998));
#255771=CARTESIAN_POINT('Ctrl Pts',(-11.2861133340001,15.2,2.17157728699998));
#255772=CARTESIAN_POINT('Ctrl Pts',(-11.2861133340001,11.6,2.17157728699998));
#255773=CARTESIAN_POINT('Ctrl Pts',(-11.2830607740001,15.2,2.16929420299998));
#255774=CARTESIAN_POINT('Ctrl Pts',(-11.2830607740001,11.6,2.16929420299998));
#255775=CARTESIAN_POINT('Ctrl Pts',(-11.2800100150001,15.2,2.16701606599999));
#255776=CARTESIAN_POINT('Ctrl Pts',(-11.2800100150001,11.6,2.16701606599999));
#255777=CARTESIAN_POINT('Ctrl Pts',(-11.2769610580001,15.2,2.16474288099999));
#255778=CARTESIAN_POINT('Ctrl Pts',(-11.2769610580001,11.6,2.16474288099999));
#255779=CARTESIAN_POINT('Ctrl Pts',(-11.2739139080001,15.2,2.16247464499999));
#255780=CARTESIAN_POINT('Ctrl Pts',(-11.2739139080001,11.6,2.16247464499998));
#255781=CARTESIAN_POINT('Ctrl Pts',(-11.2708685710001,15.2,2.16021135999998));
#255782=CARTESIAN_POINT('Ctrl Pts',(-11.2708685710001,11.6,2.16021135999998));
#255783=CARTESIAN_POINT('Ctrl Pts',(-11.2678250540001,15.2,2.15795302499998));
#255784=CARTESIAN_POINT('Ctrl Pts',(-11.2678250540001,11.6,2.15795302499998));
#255785=CARTESIAN_POINT('Ctrl Pts',(-11.2647833690001,15.2,2.15569963899998));
#255786=CARTESIAN_POINT('Ctrl Pts',(-11.2647833690001,11.6,2.15569963899998));
#255787=CARTESIAN_POINT('Ctrl Pts',(-11.2617435240001,15.2,2.15345120199999));
#255788=CARTESIAN_POINT('Ctrl Pts',(-11.2617435240001,11.6,2.15345120199998));
#255789=CARTESIAN_POINT('Ctrl Pts',(-11.2587055320001,15.2,2.15120771399999));
#255790=CARTESIAN_POINT('Ctrl Pts',(-11.2587055320001,11.6,2.15120771399999));
#255791=CARTESIAN_POINT('Ctrl Pts',(-11.2556694030001,15.2,2.14896917499999));
#255792=CARTESIAN_POINT('Ctrl Pts',(-11.2556694030001,11.6,2.14896917499999));
#255793=CARTESIAN_POINT('Ctrl Pts',(-11.2526351490001,15.2,2.14673558399999));
#255794=CARTESIAN_POINT('Ctrl Pts',(-11.2526351490001,11.6,2.14673558399999));
#255795=CARTESIAN_POINT('Ctrl Pts',(-11.2496027780001,15.2,2.14450693999999));
#255796=CARTESIAN_POINT('Ctrl Pts',(-11.2496027780001,11.6,2.14450693999999));
#255797=CARTESIAN_POINT('Ctrl Pts',(-11.2465723000001,15.2,2.14228324399999));
#255798=CARTESIAN_POINT('Ctrl Pts',(-11.2465723000001,11.6,2.14228324399999));
#255799=CARTESIAN_POINT('Ctrl Pts',(-11.2435437210001,15.2,2.14006449399998));
#255800=CARTESIAN_POINT('Ctrl Pts',(-11.2435437210001,11.6,2.14006449399998));
#255801=CARTESIAN_POINT('Ctrl Pts',(-11.2405170510001,15.2,2.13785069299998));
#255802=CARTESIAN_POINT('Ctrl Pts',(-11.2405170510001,11.6,2.13785069299998));
#255803=CARTESIAN_POINT('Ctrl Pts',(-11.2374922970001,15.2,2.13564183799999));
#255804=CARTESIAN_POINT('Ctrl Pts',(-11.2374922970001,11.6,2.13564183799999));
#255805=CARTESIAN_POINT('Ctrl Pts',(-11.2344694690001,15.2,2.13343792899999));
#255806=CARTESIAN_POINT('Ctrl Pts',(-11.2344694690001,11.6,2.13343792899999));
#255807=CARTESIAN_POINT('Ctrl Pts',(-11.2314485750001,15.2,2.13123896599999));
#255808=CARTESIAN_POINT('Ctrl Pts',(-11.2314485750001,11.6,2.13123896599999));
#255809=CARTESIAN_POINT('Ctrl Pts',(-11.2284296250001,15.2,2.12904494799998));
#255810=CARTESIAN_POINT('Ctrl Pts',(-11.2284296250001,11.6,2.12904494799998));
#255811=CARTESIAN_POINT('Ctrl Pts',(-11.2254126260001,15.2,2.12685587499998));
#255812=CARTESIAN_POINT('Ctrl Pts',(-11.2254126260001,11.6,2.12685587499998));
#255813=CARTESIAN_POINT('Ctrl Pts',(-11.2223975920001,15.2,2.12467174699999));
#255814=CARTESIAN_POINT('Ctrl Pts',(-11.2223975920001,11.6,2.12467174699999));
#255815=CARTESIAN_POINT('Ctrl Pts',(-11.2193845280001,15.2,2.12249256399998));
#255816=CARTESIAN_POINT('Ctrl Pts',(-11.2193845280001,11.6,2.12249256399998));
#255817=CARTESIAN_POINT('Ctrl Pts',(-11.2163734460001,15.2,2.12031832499999));
#255818=CARTESIAN_POINT('Ctrl Pts',(-11.2163734460001,11.6,2.12031832499999));
#255819=CARTESIAN_POINT('Ctrl Pts',(-11.2133643550001,15.2,2.11814902899999));
#255820=CARTESIAN_POINT('Ctrl Pts',(-11.2133643550001,11.6,2.11814902899999));
#255821=CARTESIAN_POINT('Ctrl Pts',(-11.2103572640001,15.2,2.11598467699998));
#255822=CARTESIAN_POINT('Ctrl Pts',(-11.2103572640001,11.6,2.11598467699998));
#255823=CARTESIAN_POINT('Ctrl Pts',(-11.2073521820001,15.2,2.11382526699999));
#255824=CARTESIAN_POINT('Ctrl Pts',(-11.2073521820001,11.6,2.11382526699999));
#255825=CARTESIAN_POINT('Ctrl Pts',(-11.2043491170001,15.2,2.11167079899999));
#255826=CARTESIAN_POINT('Ctrl Pts',(-11.2043491170001,11.6,2.11167079899999));
#255827=CARTESIAN_POINT('Ctrl Pts',(-11.2013480790001,15.2,2.10952127399999));
#255828=CARTESIAN_POINT('Ctrl Pts',(-11.2013480790001,11.6,2.10952127399999));
#255829=CARTESIAN_POINT('Ctrl Pts',(-11.1983490770001,15.2,2.10737668999998));
#255830=CARTESIAN_POINT('Ctrl Pts',(-11.1983490770001,11.6,2.10737668999998));
#255831=CARTESIAN_POINT('Ctrl Pts',(-11.1953521200001,15.2,2.10523704699999));
#255832=CARTESIAN_POINT('Ctrl Pts',(-11.1953521200001,11.6,2.10523704699999));
#255833=CARTESIAN_POINT('Ctrl Pts',(-11.1923572190001,15.2,2.10310234499998));
#255834=CARTESIAN_POINT('Ctrl Pts',(-11.1923572190001,11.6,2.10310234499998));
#255835=CARTESIAN_POINT('Ctrl Pts',(-11.1893643810001,15.2,2.10097258199998));
#255836=CARTESIAN_POINT('Ctrl Pts',(-11.1893643810001,11.6,2.10097258199998));
#255837=CARTESIAN_POINT('Ctrl Pts',(-11.1863736160001,15.2,2.09884775999999));
#255838=CARTESIAN_POINT('Ctrl Pts',(-11.1863736160001,11.6,2.09884775999999));
#255839=CARTESIAN_POINT('Ctrl Pts',(-11.1833849350001,15.2,2.09672787599999));
#255840=CARTESIAN_POINT('Ctrl Pts',(-11.1833849350001,11.6,2.09672787599999));
#255841=CARTESIAN_POINT('Ctrl Pts',(-11.1803983470001,15.2,2.09461293099999));
#255842=CARTESIAN_POINT('Ctrl Pts',(-11.1803983470001,11.6,2.09461293099999));
#255843=CARTESIAN_POINT('Ctrl Pts',(-11.1774138590001,15.2,2.09250292499998));
#255844=CARTESIAN_POINT('Ctrl Pts',(-11.1774138590001,11.6,2.09250292499998));
#255845=CARTESIAN_POINT('Ctrl Pts',(-11.1744314830001,15.2,2.09039785499999));
#255846=CARTESIAN_POINT('Ctrl Pts',(-11.1744314830001,11.6,2.09039785499999));
#255847=CARTESIAN_POINT('Ctrl Pts',(-11.1714512270001,15.2,2.08829772299998));
#255848=CARTESIAN_POINT('Ctrl Pts',(-11.1714512270001,11.6,2.08829772299998));
#255849=CARTESIAN_POINT('Ctrl Pts',(-11.1684731010001,15.2,2.08620252799999));
#255850=CARTESIAN_POINT('Ctrl Pts',(-11.1684731010001,11.6,2.08620252799998));
#255851=CARTESIAN_POINT('Ctrl Pts',(-11.1654971140001,15.2,2.08411226799999));
#255852=CARTESIAN_POINT('Ctrl Pts',(-11.1654971140001,11.6,2.08411226799999));
#255853=CARTESIAN_POINT('Ctrl Pts',(-11.1625232760001,15.2,2.08202694399999));
#255854=CARTESIAN_POINT('Ctrl Pts',(-11.1625232760001,11.6,2.08202694399999));
#255855=CARTESIAN_POINT('Ctrl Pts',(-11.1595515960001,15.2,2.07994655599999));
#255856=CARTESIAN_POINT('Ctrl Pts',(-11.1595515960001,11.6,2.07994655599998));
#255857=CARTESIAN_POINT('Ctrl Pts',(-11.1565820830001,15.2,2.07787110099999));
#255858=CARTESIAN_POINT('Ctrl Pts',(-11.1565820830001,11.6,2.07787110099999));
#255859=CARTESIAN_POINT('Ctrl Pts',(-11.1536147480001,15.2,2.07580057999999));
#255860=CARTESIAN_POINT('Ctrl Pts',(-11.1536147480001,11.6,2.07580057999999));
#255861=CARTESIAN_POINT('Ctrl Pts',(-11.1506495990001,15.2,2.07373499299999));
#255862=CARTESIAN_POINT('Ctrl Pts',(-11.1506495990001,11.6,2.07373499299999));
#255863=CARTESIAN_POINT('Ctrl Pts',(-11.1476866470001,15.2,2.07167433799999));
#255864=CARTESIAN_POINT('Ctrl Pts',(-11.1476866470001,11.6,2.07167433799999));
#255865=CARTESIAN_POINT('Ctrl Pts',(-11.1447259000001,15.2,2.06961861399999));
#255866=CARTESIAN_POINT('Ctrl Pts',(-11.1447259000001,11.6,2.06961861399999));
#255867=CARTESIAN_POINT('Ctrl Pts',(-11.1417673690001,15.2,2.06756782399999));
#255868=CARTESIAN_POINT('Ctrl Pts',(-11.1417673690001,11.6,2.06756782399998));
#255869=CARTESIAN_POINT('Ctrl Pts',(-11.1388110630001,15.2,2.06552196299999));
#255870=CARTESIAN_POINT('Ctrl Pts',(-11.1388110630001,11.6,2.06552196299999));
#255871=CARTESIAN_POINT('Ctrl Pts',(-11.1358569910001,15.2,2.06348103199999));
#255872=CARTESIAN_POINT('Ctrl Pts',(-11.1358569910001,11.6,2.06348103199998));
#255873=CARTESIAN_POINT('Ctrl Pts',(-11.1329051630001,15.2,2.06144503099999));
#255874=CARTESIAN_POINT('Ctrl Pts',(-11.1329051630001,11.6,2.06144503099999));
#255875=CARTESIAN_POINT('Ctrl Pts',(-11.1299555890001,15.2,2.05941395899998));
#255876=CARTESIAN_POINT('Ctrl Pts',(-11.1299555890001,11.6,2.05941395899998));
#255877=CARTESIAN_POINT('Ctrl Pts',(-11.1270082780001,15.2,2.05738781699999));
#255878=CARTESIAN_POINT('Ctrl Pts',(-11.1270082780001,11.6,2.05738781699999));
#255879=CARTESIAN_POINT('Ctrl Pts',(-11.1240632410001,15.2,2.05536660099999));
#255880=CARTESIAN_POINT('Ctrl Pts',(-11.1240632410001,11.6,2.05536660099999));
#255881=CARTESIAN_POINT('Ctrl Pts',(-11.1211204850001,15.2,2.05335031099999));
#255882=CARTESIAN_POINT('Ctrl Pts',(-11.1211204850001,11.6,2.05335031099999));
#255883=CARTESIAN_POINT('Ctrl Pts',(-11.1181800230001,15.2,2.05133894799999));
#255884=CARTESIAN_POINT('Ctrl Pts',(-11.1181800230001,11.6,2.05133894799999));
#255885=CARTESIAN_POINT('Ctrl Pts',(-11.1152418620001,15.2,2.04933251099999));
#255886=CARTESIAN_POINT('Ctrl Pts',(-11.1152418620001,11.6,2.04933251099999));
#255887=CARTESIAN_POINT('Ctrl Pts',(-11.1123060130001,15.2,2.04733099899999));
#255888=CARTESIAN_POINT('Ctrl Pts',(-11.1123060130001,11.6,2.04733099899999));
#255889=CARTESIAN_POINT('Ctrl Pts',(-11.1093724870001,15.2,2.04533441099999));
#255890=CARTESIAN_POINT('Ctrl Pts',(-11.1093724870001,11.6,2.04533441099999));
#255891=CARTESIAN_POINT('Ctrl Pts',(-11.1064412920001,15.2,2.04334274599999));
#255892=CARTESIAN_POINT('Ctrl Pts',(-11.1064412920001,11.6,2.04334274599998));
#255893=CARTESIAN_POINT('Ctrl Pts',(-11.1035124380001,15.2,2.04135600499999));
#255894=CARTESIAN_POINT('Ctrl Pts',(-11.1035124380001,11.6,2.04135600499999));
#255895=CARTESIAN_POINT('Ctrl Pts',(-11.1005859330001,15.2,2.03937418499998));
#255896=CARTESIAN_POINT('Ctrl Pts',(-11.1005859330001,11.6,2.03937418499998));
#255897=CARTESIAN_POINT('Ctrl Pts',(-11.0976617910001,15.2,2.03739728599999));
#255898=CARTESIAN_POINT('Ctrl Pts',(-11.0976617910001,11.6,2.03739728599999));
#255899=CARTESIAN_POINT('Ctrl Pts',(-11.0947400190001,15.2,2.03542530799998));
#255900=CARTESIAN_POINT('Ctrl Pts',(-11.0947400190001,11.6,2.03542530799998));
#255901=CARTESIAN_POINT('Ctrl Pts',(-11.0918206280001,15.2,2.03345824899999));
#255902=CARTESIAN_POINT('Ctrl Pts',(-11.0918206280001,11.6,2.03345824899999));
#255903=CARTESIAN_POINT('Ctrl Pts',(-11.0889036270001,15.2,2.03149611099999));
#255904=CARTESIAN_POINT('Ctrl Pts',(-11.0889036270001,11.6,2.03149611099999));
#255905=CARTESIAN_POINT('Ctrl Pts',(-11.0859890260001,15.2,2.02953888899998));
#255906=CARTESIAN_POINT('Ctrl Pts',(-11.0859890260001,11.6,2.02953888899998));
#255907=CARTESIAN_POINT('Ctrl Pts',(-11.0830768350001,15.2,2.02758658599999));
#255908=CARTESIAN_POINT('Ctrl Pts',(-11.0830768350001,11.6,2.02758658599999));
#255909=CARTESIAN_POINT('Ctrl Pts',(-11.0801670650001,15.2,2.02563919799998));
#255910=CARTESIAN_POINT('Ctrl Pts',(-11.0801670650001,11.6,2.02563919799998));
#255911=CARTESIAN_POINT('Ctrl Pts',(-11.0772597250001,15.2,2.02369672799998));
#255912=CARTESIAN_POINT('Ctrl Pts',(-11.0772597250001,11.6,2.02369672799998));
#255913=CARTESIAN_POINT('Ctrl Pts',(-11.0743548250001,15.2,2.02175917099999));
#255914=CARTESIAN_POINT('Ctrl Pts',(-11.0743548250001,11.6,2.02175917099999));
#255915=CARTESIAN_POINT('Ctrl Pts',(-11.0714523740001,15.2,2.01982652899999));
#255916=CARTESIAN_POINT('Ctrl Pts',(-11.0714523740001,11.6,2.01982652899999));
#255917=CARTESIAN_POINT('Ctrl Pts',(-11.0685523830001,15.2,2.01789879999998));
#255918=CARTESIAN_POINT('Ctrl Pts',(-11.0685523830001,11.6,2.01789879999998));
#255919=CARTESIAN_POINT('Ctrl Pts',(-11.0656548630001,15.2,2.01597598299998));
#255920=CARTESIAN_POINT('Ctrl Pts',(-11.0656548630001,11.6,2.01597598299998));
#255921=CARTESIAN_POINT('Ctrl Pts',(-11.0627598220001,15.2,2.01405807899999));
#255922=CARTESIAN_POINT('Ctrl Pts',(-11.0627598220001,11.6,2.01405807899999));
#255923=CARTESIAN_POINT('Ctrl Pts',(-11.0598672710001,15.2,2.01214508499998));
#255924=CARTESIAN_POINT('Ctrl Pts',(-11.0598672710001,11.6,2.01214508499998));
#255925=CARTESIAN_POINT('Ctrl Pts',(-11.0569772200001,15.2,2.01023700099999));
#255926=CARTESIAN_POINT('Ctrl Pts',(-11.0569772200001,11.6,2.01023700099999));
#255927=CARTESIAN_POINT('Ctrl Pts',(-11.0540896800001,15.2,2.00833382599999));
#255928=CARTESIAN_POINT('Ctrl Pts',(-11.0540896800001,11.6,2.00833382599999));
#255929=CARTESIAN_POINT('Ctrl Pts',(-11.0512046610001,15.2,2.00643555899998));
#255930=CARTESIAN_POINT('Ctrl Pts',(-11.0512046610001,11.6,2.00643555899998));
#255931=CARTESIAN_POINT('Ctrl Pts',(-11.0483221710001,15.2,2.00454219899999));
#255932=CARTESIAN_POINT('Ctrl Pts',(-11.0483221710001,11.6,2.00454219899999));
#255933=CARTESIAN_POINT('Ctrl Pts',(-11.0454422220001,15.2,2.00265374599998));
#255934=CARTESIAN_POINT('Ctrl Pts',(-11.0454422220001,11.6,2.00265374599998));
#255935=CARTESIAN_POINT('Ctrl Pts',(-11.0425648240001,15.2,2.00077019799998));
#255936=CARTESIAN_POINT('Ctrl Pts',(-11.0425648240001,11.6,2.00077019799998));
#255937=CARTESIAN_POINT('Ctrl Pts',(-11.0396899870001,15.2,1.99889155399998));
#255938=CARTESIAN_POINT('Ctrl Pts',(-11.0396899870001,11.6,1.99889155399998));
#255939=CARTESIAN_POINT('Ctrl Pts',(-11.0368177200001,15.2,1.99701781299999));
#255940=CARTESIAN_POINT('Ctrl Pts',(-11.0368177200001,11.6,1.99701781299999));
#255941=CARTESIAN_POINT('Ctrl Pts',(-11.0339480350001,15.2,1.99514897599999));
#255942=CARTESIAN_POINT('Ctrl Pts',(-11.0339480350001,11.6,1.99514897599998));
#255943=CARTESIAN_POINT('Ctrl Pts',(-11.0310809420001,15.2,1.99328503899999));
#255944=CARTESIAN_POINT('Ctrl Pts',(-11.0310809420001,11.6,1.99328503899999));
#255945=CARTESIAN_POINT('Ctrl Pts',(-11.0282164510001,15.2,1.99142600399998));
#255946=CARTESIAN_POINT('Ctrl Pts',(-11.0282164510001,11.6,1.99142600399998));
#255947=CARTESIAN_POINT('Ctrl Pts',(-11.0253545710001,15.2,1.98957186699999));
#255948=CARTESIAN_POINT('Ctrl Pts',(-11.0253545710001,11.6,1.98957186699999));
#255949=CARTESIAN_POINT('Ctrl Pts',(-11.0224953140001,15.2,1.98772262999999));
#255950=CARTESIAN_POINT('Ctrl Pts',(-11.0224953140001,11.6,1.98772262999999));
#255951=CARTESIAN_POINT('Ctrl Pts',(-11.0196386900001,15.2,1.98587828999999));
#255952=CARTESIAN_POINT('Ctrl Pts',(-11.0196386900001,11.6,1.98587828999999));
#255953=CARTESIAN_POINT('Ctrl Pts',(-11.0167847080001,15.2,1.98403884699998));
#255954=CARTESIAN_POINT('Ctrl Pts',(-11.0167847080001,11.6,1.98403884699998));
#255955=CARTESIAN_POINT('Ctrl Pts',(-11.0139333790001,15.2,1.98220429899999));
#255956=CARTESIAN_POINT('Ctrl Pts',(-11.0139333790001,11.6,1.98220429899999));
#255957=CARTESIAN_POINT('Ctrl Pts',(-11.0110847150001,15.2,1.98037464599999));
#255958=CARTESIAN_POINT('Ctrl Pts',(-11.0110847150001,11.6,1.98037464599999));
#255959=CARTESIAN_POINT('Ctrl Pts',(-11.0082387250001,15.2,1.97854988499999));
#255960=CARTESIAN_POINT('Ctrl Pts',(-11.0082387250001,11.6,1.97854988499999));
#255961=CARTESIAN_POINT('Ctrl Pts',(-11.0053954180001,15.2,1.97673001799998));
#255962=CARTESIAN_POINT('Ctrl Pts',(-11.0053954180001,11.6,1.97673001799998));
#255963=CARTESIAN_POINT('Ctrl Pts',(-11.0025548070001,15.2,1.97491504299999));
#255964=CARTESIAN_POINT('Ctrl Pts',(-11.0025548070001,11.6,1.97491504299998));
#255965=CARTESIAN_POINT('Ctrl Pts',(-10.9997169010001,15.2,1.97310495599998));
#255966=CARTESIAN_POINT('Ctrl Pts',(-10.9997169010001,11.6,1.97310495599998));
#255967=CARTESIAN_POINT('Ctrl Pts',(-10.9968817120001,15.2,1.97129975899998));
#255968=CARTESIAN_POINT('Ctrl Pts',(-10.9968817120001,11.6,1.97129975899998));
#255969=CARTESIAN_POINT('Ctrl Pts',(-10.9940492480001,15.2,1.96949945099998));
#255970=CARTESIAN_POINT('Ctrl Pts',(-10.9940492480001,11.6,1.96949945099998));
#255971=CARTESIAN_POINT('Ctrl Pts',(-10.9912195210001,15.2,1.96770402999999));
#255972=CARTESIAN_POINT('Ctrl Pts',(-10.9912195210001,11.6,1.96770402999999));
#255973=CARTESIAN_POINT('Ctrl Pts',(-10.9883925420001,15.2,1.96591349399998));
#255974=CARTESIAN_POINT('Ctrl Pts',(-10.9883925420001,11.6,1.96591349399998));
#255975=CARTESIAN_POINT('Ctrl Pts',(-10.9855683200001,15.2,1.96412784299998));
#255976=CARTESIAN_POINT('Ctrl Pts',(-10.9855683200001,11.6,1.96412784299998));
#255977=CARTESIAN_POINT('Ctrl Pts',(-10.9827468670001,15.2,1.96234707499999));
#255978=CARTESIAN_POINT('Ctrl Pts',(-10.9827468670001,11.6,1.96234707499999));
#255979=CARTESIAN_POINT('Ctrl Pts',(-10.9799281930001,15.2,1.96057118999999));
#255980=CARTESIAN_POINT('Ctrl Pts',(-10.9799281930001,11.6,1.96057118999999));
#255981=CARTESIAN_POINT('Ctrl Pts',(-10.9771123080001,15.2,1.95880018599999));
#255982=CARTESIAN_POINT('Ctrl Pts',(-10.9771123080001,11.6,1.95880018599999));
#255983=CARTESIAN_POINT('Ctrl Pts',(-10.9742992230001,15.2,1.95703406199998));
#255984=CARTESIAN_POINT('Ctrl Pts',(-10.9742992230001,11.6,1.95703406199998));
#255985=CARTESIAN_POINT('Ctrl Pts',(-10.9714889500001,15.2,1.95527281799999));
#255986=CARTESIAN_POINT('Ctrl Pts',(-10.9714889500001,11.6,1.95527281799999));
#255987=CARTESIAN_POINT('Ctrl Pts',(-10.9686814980001,15.2,1.95351644999999));
#255988=CARTESIAN_POINT('Ctrl Pts',(-10.9686814980001,11.6,1.95351644999999));
#255989=CARTESIAN_POINT('Ctrl Pts',(-10.9658768780001,15.2,1.95176495999998));
#255990=CARTESIAN_POINT('Ctrl Pts',(-10.9658768780001,11.6,1.95176495999998));
#255991=CARTESIAN_POINT('Ctrl Pts',(-10.9630751010001,15.2,1.95001834399998));
#255992=CARTESIAN_POINT('Ctrl Pts',(-10.9630751010001,11.6,1.95001834399998));
#255993=CARTESIAN_POINT('Ctrl Pts',(-10.9602761780001,15.2,1.94827660199998));
#255994=CARTESIAN_POINT('Ctrl Pts',(-10.9602761780001,11.6,1.94827660199998));
#255995=CARTESIAN_POINT('Ctrl Pts',(-10.9574801190001,15.2,1.94653973399999));
#255996=CARTESIAN_POINT('Ctrl Pts',(-10.9574801190001,11.6,1.94653973399999));
#255997=CARTESIAN_POINT('Ctrl Pts',(-10.9546869340001,15.2,1.94480773699999));
#255998=CARTESIAN_POINT('Ctrl Pts',(-10.9546869340001,11.6,1.94480773699999));
#255999=CARTESIAN_POINT('Ctrl Pts',(-10.9518966360001,15.2,1.94308060999999));
#256000=CARTESIAN_POINT('Ctrl Pts',(-10.9518966360001,11.6,1.94308060999999));
#256001=CARTESIAN_POINT('Ctrl Pts',(-10.9491092350001,15.2,1.94135835299999));
#256002=CARTESIAN_POINT('Ctrl Pts',(-10.9491092350001,11.6,1.94135835299999));
#256003=CARTESIAN_POINT('Ctrl Pts',(-10.9463247410001,15.2,1.93964096299998));
#256004=CARTESIAN_POINT('Ctrl Pts',(-10.9463247410001,11.6,1.93964096299998));
#256005=CARTESIAN_POINT('Ctrl Pts',(-10.9435431660001,15.2,1.93792843899999));
#256006=CARTESIAN_POINT('Ctrl Pts',(-10.9435431660001,11.6,1.93792843899998));
#256007=CARTESIAN_POINT('Ctrl Pts',(-10.9407645200001,15.2,1.93622078099999));
#256008=CARTESIAN_POINT('Ctrl Pts',(-10.9407645200001,11.6,1.93622078099999));
#256009=CARTESIAN_POINT('Ctrl Pts',(-10.9379888140001,15.2,1.93451798599999));
#256010=CARTESIAN_POINT('Ctrl Pts',(-10.9379888140001,11.6,1.93451798599999));
#256011=CARTESIAN_POINT('Ctrl Pts',(-10.9352160590001,15.2,1.93282005499999));
#256012=CARTESIAN_POINT('Ctrl Pts',(-10.9352160590001,11.6,1.93282005499999));
#256013=CARTESIAN_POINT('Ctrl Pts',(-10.9324462660001,15.2,1.93112698299998));
#256014=CARTESIAN_POINT('Ctrl Pts',(-10.9324462660001,11.6,1.93112698299998));
#256015=CARTESIAN_POINT('Ctrl Pts',(-10.9296794470001,15.2,1.92943877199999));
#256016=CARTESIAN_POINT('Ctrl Pts',(-10.9296794470001,11.6,1.92943877199998));
#256017=CARTESIAN_POINT('Ctrl Pts',(-10.9269156100001,15.2,1.92775541899998));
#256018=CARTESIAN_POINT('Ctrl Pts',(-10.9269156100001,11.6,1.92775541899998));
#256019=CARTESIAN_POINT('Ctrl Pts',(-10.9241547690001,15.2,1.92607692399998));
#256020=CARTESIAN_POINT('Ctrl Pts',(-10.9241547690001,11.6,1.92607692399998));
#256021=CARTESIAN_POINT('Ctrl Pts',(-10.9213969330001,15.2,1.92440328399998));
#256022=CARTESIAN_POINT('Ctrl Pts',(-10.9213969330001,11.6,1.92440328399998));
#256023=CARTESIAN_POINT('Ctrl Pts',(-10.9186421150001,15.2,1.92273449799998));
#256024=CARTESIAN_POINT('Ctrl Pts',(-10.9186421150001,11.6,1.92273449799998));
#256025=CARTESIAN_POINT('Ctrl Pts',(-10.9158903240001,15.2,1.92107056499998));
#256026=CARTESIAN_POINT('Ctrl Pts',(-10.9158903240001,11.6,1.92107056499998));
#256027=CARTESIAN_POINT('Ctrl Pts',(-10.9131415730001,15.2,1.91941148499998));
#256028=CARTESIAN_POINT('Ctrl Pts',(-10.9131415730001,11.6,1.91941148499998));
#256029=CARTESIAN_POINT('Ctrl Pts',(-10.9103958720001,15.2,1.91775725399999));
#256030=CARTESIAN_POINT('Ctrl Pts',(-10.9103958720001,11.6,1.91775725399998));
#256031=CARTESIAN_POINT('Ctrl Pts',(-10.9076532320001,15.2,1.91610787099998));
#256032=CARTESIAN_POINT('Ctrl Pts',(-10.9076532320001,11.6,1.91610787099998));
#256033=CARTESIAN_POINT('Ctrl Pts',(-10.9049136650001,15.2,1.91446333499998));
#256034=CARTESIAN_POINT('Ctrl Pts',(-10.9049136650001,11.6,1.91446333499998));
#256035=CARTESIAN_POINT('Ctrl Pts',(-10.9021771820001,15.2,1.91282364399999));
#256036=CARTESIAN_POINT('Ctrl Pts',(-10.9021771820001,11.6,1.91282364399999));
#256037=CARTESIAN_POINT('Ctrl Pts',(-10.8994437930001,15.2,1.91118879899999));
#256038=CARTESIAN_POINT('Ctrl Pts',(-10.8994437930001,11.6,1.91118879899998));
#256039=CARTESIAN_POINT('Ctrl Pts',(-10.8967135100001,15.2,1.90955879499999));
#256040=CARTESIAN_POINT('Ctrl Pts',(-10.8967135100001,11.6,1.90955879499999));
#256041=CARTESIAN_POINT('Ctrl Pts',(-10.8939863450001,15.2,1.90793363399999));
#256042=CARTESIAN_POINT('Ctrl Pts',(-10.8939863450001,11.6,1.90793363399999));
#256043=CARTESIAN_POINT('Ctrl Pts',(-10.8912623070001,15.2,1.90631331199999));
#256044=CARTESIAN_POINT('Ctrl Pts',(-10.8912623070001,11.6,1.90631331199999));
#256045=CARTESIAN_POINT('Ctrl Pts',(-10.8885414100001,15.2,1.90469782799998));
#256046=CARTESIAN_POINT('Ctrl Pts',(-10.8885414100001,11.6,1.90469782799998));
#256047=CARTESIAN_POINT('Ctrl Pts',(-10.8858236640001,15.2,1.90308717999998));
#256048=CARTESIAN_POINT('Ctrl Pts',(-10.8858236640001,11.6,1.90308717999998));
#256049=CARTESIAN_POINT('Ctrl Pts',(-10.8831090800001,15.2,1.90148136799999));
#256050=CARTESIAN_POINT('Ctrl Pts',(-10.8831090800001,11.6,1.90148136799999));
#256051=CARTESIAN_POINT('Ctrl Pts',(-10.8803976700001,15.2,1.89988038899998));
#256052=CARTESIAN_POINT('Ctrl Pts',(-10.8803976700001,11.6,1.89988038899998));
#256053=CARTESIAN_POINT('Ctrl Pts',(-10.8776894460001,15.2,1.89828424199999));
#256054=CARTESIAN_POINT('Ctrl Pts',(-10.8776894460001,11.6,1.89828424199999));
#256055=CARTESIAN_POINT('Ctrl Pts',(-10.8749844180001,15.2,1.89669292499998));
#256056=CARTESIAN_POINT('Ctrl Pts',(-10.8749844180001,11.6,1.89669292499998));
#256057=CARTESIAN_POINT('Ctrl Pts',(-10.8722825980001,15.2,1.89510643799998));
#256058=CARTESIAN_POINT('Ctrl Pts',(-10.8722825980001,11.6,1.89510643799998));
#256059=CARTESIAN_POINT('Ctrl Pts',(-10.8695839980001,15.2,1.89352477599999));
#256060=CARTESIAN_POINT('Ctrl Pts',(-10.8695839980001,11.6,1.89352477599999));
#256061=CARTESIAN_POINT('Ctrl Pts',(-10.8668886270001,15.2,1.89194794099999));
#256062=CARTESIAN_POINT('Ctrl Pts',(-10.8668886270001,11.6,1.89194794099999));
#256063=CARTESIAN_POINT('Ctrl Pts',(-10.8641965010001,15.2,1.89037592899998));
#256064=CARTESIAN_POINT('Ctrl Pts',(-10.8641965010001,11.6,1.89037592899998));
#256065=CARTESIAN_POINT('Ctrl Pts',(-10.8615076260001,15.2,1.88880873999999));
#256066=CARTESIAN_POINT('Ctrl Pts',(-10.8615076260001,11.6,1.88880873999999));
#256067=CARTESIAN_POINT('Ctrl Pts',(-10.8588220190001,15.2,1.88724637099998));
#256068=CARTESIAN_POINT('Ctrl Pts',(-10.8588220190001,11.6,1.88724637099998));
#256069=CARTESIAN_POINT('Ctrl Pts',(-10.8561396880001,15.2,1.88568882099998));
#256070=CARTESIAN_POINT('Ctrl Pts',(-10.8561396880001,11.6,1.88568882099998));
#256071=CARTESIAN_POINT('Ctrl Pts',(-10.8534606450001,15.2,1.88413608899999));
#256072=CARTESIAN_POINT('Ctrl Pts',(-10.8534606450001,11.6,1.88413608899999));
#256073=CARTESIAN_POINT('Ctrl Pts',(-10.8507849030001,15.2,1.88258817099999));
#256074=CARTESIAN_POINT('Ctrl Pts',(-10.8507849030001,11.6,1.88258817099999));
#256075=CARTESIAN_POINT('Ctrl Pts',(-10.8481124720001,15.2,1.88104506799998));
#256076=CARTESIAN_POINT('Ctrl Pts',(-10.8481124720001,11.6,1.88104506799998));
#256077=CARTESIAN_POINT('Ctrl Pts',(-10.8454433650001,15.2,1.87950677599999));
#256078=CARTESIAN_POINT('Ctrl Pts',(-10.8454433650001,11.6,1.87950677599999));
#256079=CARTESIAN_POINT('Ctrl Pts',(-10.8427775930001,15.2,1.87797329499999));
#256080=CARTESIAN_POINT('Ctrl Pts',(-10.8427775930001,11.6,1.87797329499999));
#256081=CARTESIAN_POINT('Ctrl Pts',(-10.8401151680001,15.2,1.87644462199998));
#256082=CARTESIAN_POINT('Ctrl Pts',(-10.8401151680001,11.6,1.87644462199998));
#256083=CARTESIAN_POINT('Ctrl Pts',(-10.8374561020001,15.2,1.87492075599998));
#256084=CARTESIAN_POINT('Ctrl Pts',(-10.8374561020001,11.6,1.87492075599998));
#256085=CARTESIAN_POINT('Ctrl Pts',(-10.8348004050001,15.2,1.87340169499999));
#256086=CARTESIAN_POINT('Ctrl Pts',(-10.8348004050001,11.6,1.87340169499999));
#256087=CARTESIAN_POINT('Ctrl Pts',(-10.8321480920001,15.2,1.87188743799998));
#256088=CARTESIAN_POINT('Ctrl Pts',(-10.8321480920001,11.6,1.87188743799998));
#256089=CARTESIAN_POINT('Ctrl Pts',(-10.8294991720001,15.2,1.87037798199999));
#256090=CARTESIAN_POINT('Ctrl Pts',(-10.8294991720001,11.6,1.87037798199999));
#256091=CARTESIAN_POINT('Ctrl Pts',(-10.8268536570001,15.2,1.86887332499999));
#256092=CARTESIAN_POINT('Ctrl Pts',(-10.8268536570001,11.6,1.86887332499999));
#256093=CARTESIAN_POINT('Ctrl Pts',(-10.8242115600001,15.2,1.86737346599998));
#256094=CARTESIAN_POINT('Ctrl Pts',(-10.8242115600001,11.6,1.86737346599998));
#256095=CARTESIAN_POINT('Ctrl Pts',(-10.8215728930001,15.2,1.86587840299998));
#256096=CARTESIAN_POINT('Ctrl Pts',(-10.8215728930001,11.6,1.86587840299998));
#256097=CARTESIAN_POINT('Ctrl Pts',(-10.8189376670001,15.2,1.86438813399999));
#256098=CARTESIAN_POINT('Ctrl Pts',(-10.8189376670001,11.6,1.86438813399999));
#256099=CARTESIAN_POINT('Ctrl Pts',(-10.8163058940001,15.2,1.86290265699999));
#256100=CARTESIAN_POINT('Ctrl Pts',(-10.8163058940001,11.6,1.86290265699998));
#256101=CARTESIAN_POINT('Ctrl Pts',(-10.8136775860001,15.2,1.86142197099999));
#256102=CARTESIAN_POINT('Ctrl Pts',(-10.8136775860001,11.6,1.86142197099999));
#256103=CARTESIAN_POINT('Ctrl Pts',(-10.8110527560001,15.2,1.85994607399998));
#256104=CARTESIAN_POINT('Ctrl Pts',(-10.8110527560001,11.6,1.85994607399998));
#256105=CARTESIAN_POINT('Ctrl Pts',(-10.8084314150001,15.2,1.85847496199999));
#256106=CARTESIAN_POINT('Ctrl Pts',(-10.8084314150001,11.6,1.85847496199999));
#256107=CARTESIAN_POINT('Ctrl Pts',(-10.8058135750001,15.2,1.85700863499999));
#256108=CARTESIAN_POINT('Ctrl Pts',(-10.8058135750001,11.6,1.85700863499999));
#256109=CARTESIAN_POINT('Ctrl Pts',(-10.8031992490001,15.2,1.85554709099998));
#256110=CARTESIAN_POINT('Ctrl Pts',(-10.8031992490001,11.6,1.85554709099998));
#256111=CARTESIAN_POINT('Ctrl Pts',(-10.8005884480001,15.2,1.85409032699999));
#256112=CARTESIAN_POINT('Ctrl Pts',(-10.8005884480001,11.6,1.85409032699999));
#256113=CARTESIAN_POINT('Ctrl Pts',(-10.7979811840001,15.2,1.85263834199999));
#256114=CARTESIAN_POINT('Ctrl Pts',(-10.7979811840001,11.6,1.85263834199999));
#256115=CARTESIAN_POINT('Ctrl Pts',(-10.7953774700001,15.2,1.85119113499999));
#256116=CARTESIAN_POINT('Ctrl Pts',(-10.7953774700001,11.6,1.85119113499998));
#256117=CARTESIAN_POINT('Ctrl Pts',(-10.7927773170001,15.2,1.84974870099999));
#256118=CARTESIAN_POINT('Ctrl Pts',(-10.7927773170001,11.6,1.84974870099999));
#256119=CARTESIAN_POINT('Ctrl Pts',(-10.7901807400001,15.2,1.84831103999999));
#256120=CARTESIAN_POINT('Ctrl Pts',(-10.7901807400001,11.6,1.84831103999999));
#256121=CARTESIAN_POINT('Ctrl Pts',(-10.7875877470001,15.2,1.84687815099998));
#256122=CARTESIAN_POINT('Ctrl Pts',(-10.7875877470001,11.6,1.84687815099998));
#256123=CARTESIAN_POINT('Ctrl Pts',(-10.7849983530001,15.2,1.84545002999998));
#256124=CARTESIAN_POINT('Ctrl Pts',(-10.7849983530001,11.6,1.84545002999998));
#256125=CARTESIAN_POINT('Ctrl Pts',(-10.7824125710001,15.2,1.84402667599999));
#256126=CARTESIAN_POINT('Ctrl Pts',(-10.7824125710001,11.6,1.84402667599999));
#256127=CARTESIAN_POINT('Ctrl Pts',(-10.7798304100001,15.2,1.84260808499999));
#256128=CARTESIAN_POINT('Ctrl Pts',(-10.7798304100001,11.6,1.84260808499999));
#256129=CARTESIAN_POINT('Ctrl Pts',(-10.7772518860001,15.2,1.84119425799999));
#256130=CARTESIAN_POINT('Ctrl Pts',(-10.7772518860001,11.6,1.84119425799999));
#256131=CARTESIAN_POINT('Ctrl Pts',(-10.7746770080001,15.2,1.83978519099998));
#256132=CARTESIAN_POINT('Ctrl Pts',(-10.7746770080001,11.6,1.83978519099998));
#256133=CARTESIAN_POINT('Ctrl Pts',(-10.7721057910001,15.2,1.83838088299999));
#256134=CARTESIAN_POINT('Ctrl Pts',(-10.7721057910001,11.6,1.83838088299999));
#256135=CARTESIAN_POINT('Ctrl Pts',(-10.7695382460001,15.2,1.83698133099998));
#256136=CARTESIAN_POINT('Ctrl Pts',(-10.7695382460001,11.6,1.83698133099998));
#256137=CARTESIAN_POINT('Ctrl Pts',(-10.7669743860001,15.2,1.83558653199999));
#256138=CARTESIAN_POINT('Ctrl Pts',(-10.7669743860001,11.6,1.83558653199999));
#256139=CARTESIAN_POINT('Ctrl Pts',(-10.7644142240001,15.2,1.83419648599998));
#256140=CARTESIAN_POINT('Ctrl Pts',(-10.7644142240001,11.6,1.83419648599998));
#256141=CARTESIAN_POINT('Ctrl Pts',(-10.7618577700001,15.2,1.83281118899998));
#256142=CARTESIAN_POINT('Ctrl Pts',(-10.7618577700001,11.6,1.83281118899998));
#256143=CARTESIAN_POINT('Ctrl Pts',(-10.7593050390001,15.2,1.83143063999998));
#256144=CARTESIAN_POINT('Ctrl Pts',(-10.7593050390001,11.6,1.83143063999998));
#256145=CARTESIAN_POINT('Ctrl Pts',(-10.7567560430001,15.2,1.83005483699999));
#256146=CARTESIAN_POINT('Ctrl Pts',(-10.7567560430001,11.6,1.83005483699999));
#256147=CARTESIAN_POINT('Ctrl Pts',(-10.7542107950001,15.2,1.82868377599998));
#256148=CARTESIAN_POINT('Ctrl Pts',(-10.7542107950001,11.6,1.82868377599998));
#256149=CARTESIAN_POINT('Ctrl Pts',(-10.7516693050001,15.2,1.82731745599999));
#256150=CARTESIAN_POINT('Ctrl Pts',(-10.7516693050001,11.6,1.82731745599999));
#256151=CARTESIAN_POINT('Ctrl Pts',(-10.7491315890001,15.2,1.82595587599998));
#256152=CARTESIAN_POINT('Ctrl Pts',(-10.7491315890001,11.6,1.82595587599998));
#256153=CARTESIAN_POINT('Ctrl Pts',(-10.7465976590001,15.2,1.82459903199998));
#256154=CARTESIAN_POINT('Ctrl Pts',(-10.7465976590001,11.6,1.82459903199998));
#256155=CARTESIAN_POINT('Ctrl Pts',(-10.7440675260001,15.2,1.82324692199999));
#256156=CARTESIAN_POINT('Ctrl Pts',(-10.7440675260001,11.6,1.82324692199999));
#256157=CARTESIAN_POINT('Ctrl Pts',(-10.7415412030001,15.2,1.82189954399998));
#256158=CARTESIAN_POINT('Ctrl Pts',(-10.7415412030001,11.6,1.82189954399998));
#256159=CARTESIAN_POINT('Ctrl Pts',(-10.7390187040001,15.2,1.82055689499999));
#256160=CARTESIAN_POINT('Ctrl Pts',(-10.7390187040001,11.6,1.82055689499998));
#256161=CARTESIAN_POINT('Ctrl Pts',(-10.7365000410001,15.2,1.81921897399999));
#256162=CARTESIAN_POINT('Ctrl Pts',(-10.7365000410001,11.6,1.81921897399999));
#256163=CARTESIAN_POINT('Ctrl Pts',(-10.7339852270001,15.2,1.81788577899999));
#256164=CARTESIAN_POINT('Ctrl Pts',(-10.7339852270001,11.6,1.81788577899999));
#256165=CARTESIAN_POINT('Ctrl Pts',(-10.7314742750001,15.2,1.81655730499998));
#256166=CARTESIAN_POINT('Ctrl Pts',(-10.7314742750001,11.6,1.81655730499998));
#256167=CARTESIAN_POINT('Ctrl Pts',(-10.7289671960001,15.2,1.81523355299999));
#256168=CARTESIAN_POINT('Ctrl Pts',(-10.7289671960001,11.6,1.81523355299999));
#256169=CARTESIAN_POINT('Ctrl Pts',(-10.7264640050001,15.2,1.81391451699998));
#256170=CARTESIAN_POINT('Ctrl Pts',(-10.7264640050001,11.6,1.81391451699998));
#256171=CARTESIAN_POINT('Ctrl Pts',(-10.7239647150001,15.2,1.81260019699998));
#256172=CARTESIAN_POINT('Ctrl Pts',(-10.7239647150001,11.6,1.81260019699998));
#256173=CARTESIAN_POINT('Ctrl Pts',(-10.7214693390001,15.2,1.81129059099999));
#256174=CARTESIAN_POINT('Ctrl Pts',(-10.7214693390001,11.6,1.81129059099999));
#256175=CARTESIAN_POINT('Ctrl Pts',(-10.7189778870001,15.2,1.80998569599998));
#256176=CARTESIAN_POINT('Ctrl Pts',(-10.7189778870001,11.6,1.80998569599998));
#256177=CARTESIAN_POINT('Ctrl Pts',(-10.7164903760001,15.2,1.80868550799998));
#256178=CARTESIAN_POINT('Ctrl Pts',(-10.7164903760001,11.6,1.80868550799998));
#256179=CARTESIAN_POINT('Ctrl Pts',(-10.7140068170001,15.2,1.80739002699998));
#256180=CARTESIAN_POINT('Ctrl Pts',(-10.7140068170001,11.6,1.80739002699998));
#256181=CARTESIAN_POINT('Ctrl Pts',(-10.7115272230001,15.2,1.80609924899999));
#256182=CARTESIAN_POINT('Ctrl Pts',(-10.7115272230001,11.6,1.80609924899999));
#256183=CARTESIAN_POINT('Ctrl Pts',(-10.7090516070001,15.2,1.80481317199999));
#256184=CARTESIAN_POINT('Ctrl Pts',(-10.7090516070001,11.6,1.80481317199999));
#256185=CARTESIAN_POINT('Ctrl Pts',(-10.7065799830001,15.2,1.80353179299999));
#256186=CARTESIAN_POINT('Ctrl Pts',(-10.7065799830001,11.6,1.80353179299999));
#256187=CARTESIAN_POINT('Ctrl Pts',(-10.7041123640001,15.2,1.80225510999998));
#256188=CARTESIAN_POINT('Ctrl Pts',(-10.7041123640001,11.6,1.80225510999998));
#256189=CARTESIAN_POINT('Ctrl Pts',(-10.7016487620001,15.2,1.80098312099998));
#256190=CARTESIAN_POINT('Ctrl Pts',(-10.7016487620001,11.6,1.80098312099998));
#256191=CARTESIAN_POINT('Ctrl Pts',(-10.6991891910001,15.2,1.79971582199999));
#256192=CARTESIAN_POINT('Ctrl Pts',(-10.6991891910001,11.6,1.79971582199998));
#256193=CARTESIAN_POINT('Ctrl Pts',(-10.6967336660001,15.2,1.79845321199998));
#256194=CARTESIAN_POINT('Ctrl Pts',(-10.6967336660001,11.6,1.79845321199998));
#256195=CARTESIAN_POINT('Ctrl Pts',(-10.6942821970001,15.2,1.79719528699998));
#256196=CARTESIAN_POINT('Ctrl Pts',(-10.6942821970001,11.6,1.79719528699998));
#256197=CARTESIAN_POINT('Ctrl Pts',(-10.6918347990001,15.2,1.79594204599999));
#256198=CARTESIAN_POINT('Ctrl Pts',(-10.6918347990001,11.6,1.79594204599998));
#256199=CARTESIAN_POINT('Ctrl Pts',(-10.6893914850001,15.2,1.79469348499998));
#256200=CARTESIAN_POINT('Ctrl Pts',(-10.6893914850001,11.6,1.79469348499998));
#256201=CARTESIAN_POINT('Ctrl Pts',(-10.6869522690001,15.2,1.79344960299999));
#256202=CARTESIAN_POINT('Ctrl Pts',(-10.6869522690001,11.6,1.79344960299999));
#256203=CARTESIAN_POINT('Ctrl Pts',(-10.6845171640001,15.2,1.79221039399998));
#256204=CARTESIAN_POINT('Ctrl Pts',(-10.6845171640001,11.6,1.79221039399998));
#256205=CARTESIAN_POINT('Ctrl Pts',(-10.6820861830001,15.2,1.79097585899999));
#256206=CARTESIAN_POINT('Ctrl Pts',(-10.6820861830001,11.6,1.79097585899999));
#256207=CARTESIAN_POINT('Ctrl Pts',(-10.6796593400001,15.2,1.78974599499998));
#256208=CARTESIAN_POINT('Ctrl Pts',(-10.6796593400001,11.6,1.78974599499998));
#256209=CARTESIAN_POINT('Ctrl Pts',(-10.6772366490001,15.2,1.78852079599999));
#256210=CARTESIAN_POINT('Ctrl Pts',(-10.6772366490001,11.6,1.78852079599999));
#256211=CARTESIAN_POINT('Ctrl Pts',(-10.6748181230001,15.2,1.78730026299998));
#256212=CARTESIAN_POINT('Ctrl Pts',(-10.6748181230001,11.6,1.78730026299998));
#256213=CARTESIAN_POINT('Ctrl Pts',(-10.6724037740001,15.2,1.78608439099999));
#256214=CARTESIAN_POINT('Ctrl Pts',(-10.6724037740001,11.6,1.78608439099999));
#256215=CARTESIAN_POINT('Ctrl Pts',(-10.6699936180001,15.2,1.78487317899998));
#256216=CARTESIAN_POINT('Ctrl Pts',(-10.6699936180001,11.6,1.78487317899998));
#256217=CARTESIAN_POINT('Ctrl Pts',(-10.6675876670001,15.2,1.78366662199998));
#256218=CARTESIAN_POINT('Ctrl Pts',(-10.6675876670001,11.6,1.78366662199998));
#256219=CARTESIAN_POINT('Ctrl Pts',(-10.6651859350001,15.2,1.78246471899998));
#256220=CARTESIAN_POINT('Ctrl Pts',(-10.6651859350001,11.6,1.78246471899998));
#256221=CARTESIAN_POINT('Ctrl Pts',(-10.6627884370001,15.2,1.78126746699999));
#256222=CARTESIAN_POINT('Ctrl Pts',(-10.6627884370001,11.6,1.78126746699998));
#256223=CARTESIAN_POINT('Ctrl Pts',(-10.6603951850001,15.2,1.78007486299999));
#256224=CARTESIAN_POINT('Ctrl Pts',(-10.6603951850001,11.6,1.78007486299998));
#256225=CARTESIAN_POINT('Ctrl Pts',(-10.6580061940001,15.2,1.77888690299998));
#256226=CARTESIAN_POINT('Ctrl Pts',(-10.6580061940001,11.6,1.77888690299998));
#256227=CARTESIAN_POINT('Ctrl Pts',(-10.6556214770001,15.2,1.77770358699998));
#256228=CARTESIAN_POINT('Ctrl Pts',(-10.6556214770001,11.6,1.77770358699998));
#256229=CARTESIAN_POINT('Ctrl Pts',(-10.6532410480001,15.2,1.77652490999999));
#256230=CARTESIAN_POINT('Ctrl Pts',(-10.6532410480001,11.6,1.77652490999999));
#256231=CARTESIAN_POINT('Ctrl Pts',(-10.6508649200001,15.2,1.77535086899999));
#256232=CARTESIAN_POINT('Ctrl Pts',(-10.6508649200001,11.6,1.77535086899998));
#256233=CARTESIAN_POINT('Ctrl Pts',(-10.6484931090001,15.2,1.77418146099999));
#256234=CARTESIAN_POINT('Ctrl Pts',(-10.6484931090001,11.6,1.77418146099999));
#256235=CARTESIAN_POINT('Ctrl Pts',(-10.6461256270001,15.2,1.77301668399998));
#256236=CARTESIAN_POINT('Ctrl Pts',(-10.6461256270001,11.6,1.77301668399998));
#256237=CARTESIAN_POINT('Ctrl Pts',(-10.6437624890001,15.2,1.77185653499999));
#256238=CARTESIAN_POINT('Ctrl Pts',(-10.6437624890001,11.6,1.77185653499999));
#256239=CARTESIAN_POINT('Ctrl Pts',(-10.6414037090001,15.2,1.77070101099998));
#256240=CARTESIAN_POINT('Ctrl Pts',(-10.6414037090001,11.6,1.77070101099998));
#256241=CARTESIAN_POINT('Ctrl Pts',(-10.6390493000001,15.2,1.76955010999999));
#256242=CARTESIAN_POINT('Ctrl Pts',(-10.6390493000001,11.6,1.76955010999999));
#256243=CARTESIAN_POINT('Ctrl Pts',(-10.6366992770001,15.2,1.76840382499998));
#256244=CARTESIAN_POINT('Ctrl Pts',(-10.6366992770001,11.6,1.76840382499998));
#256245=CARTESIAN_POINT('Ctrl Pts',(-10.6343536530001,15.2,1.76726215799999));
#256246=CARTESIAN_POINT('Ctrl Pts',(-10.6343536530001,11.6,1.76726215799999));
#256247=CARTESIAN_POINT('Ctrl Pts',(-10.6320124440001,15.2,1.76612510399998));
#256248=CARTESIAN_POINT('Ctrl Pts',(-10.6320124440001,11.6,1.76612510399998));
#256249=CARTESIAN_POINT('Ctrl Pts',(-10.6296756630001,15.2,1.76499265799999));
#256250=CARTESIAN_POINT('Ctrl Pts',(-10.6296756630001,11.6,1.76499265799999));
#256251=CARTESIAN_POINT('Ctrl Pts',(-10.6273433250001,15.2,1.76386481999999));
#256252=CARTESIAN_POINT('Ctrl Pts',(-10.6273433250001,11.6,1.76386481999998));
#256253=CARTESIAN_POINT('Ctrl Pts',(-10.6250154420001,15.2,1.76274158499998));
#256254=CARTESIAN_POINT('Ctrl Pts',(-10.6250154420001,11.6,1.76274158499998));
#256255=CARTESIAN_POINT('Ctrl Pts',(-10.6226920310001,15.2,1.76162295199998));
#256256=CARTESIAN_POINT('Ctrl Pts',(-10.6226920310001,11.6,1.76162295199998));
#256257=CARTESIAN_POINT('Ctrl Pts',(-10.6203731050001,15.2,1.76050891499999));
#256258=CARTESIAN_POINT('Ctrl Pts',(-10.6203731050001,11.6,1.76050891499999));
#256259=CARTESIAN_POINT('Ctrl Pts',(-10.6180586770001,15.2,1.75939947299999));
#256260=CARTESIAN_POINT('Ctrl Pts',(-10.6180586770001,11.6,1.75939947299998));
#256261=CARTESIAN_POINT('Ctrl Pts',(-10.6157487650001,15.2,1.75829462199999));
#256262=CARTESIAN_POINT('Ctrl Pts',(-10.6157487650001,11.6,1.75829462199998));
#256263=CARTESIAN_POINT('Ctrl Pts',(-10.6134433800001,15.2,1.75719435899999));
#256264=CARTESIAN_POINT('Ctrl Pts',(-10.6134433800001,11.6,1.75719435899999));
#256265=CARTESIAN_POINT('Ctrl Pts',(-10.6111425380001,15.2,1.75609868099999));
#256266=CARTESIAN_POINT('Ctrl Pts',(-10.6111425380001,11.6,1.75609868099999));
#256267=CARTESIAN_POINT('Ctrl Pts',(-10.6088462540001,15.2,1.75500758399998));
#256268=CARTESIAN_POINT('Ctrl Pts',(-10.6088462540001,11.6,1.75500758399998));
#256269=CARTESIAN_POINT('Ctrl Pts',(-10.6065545400001,15.2,1.75392106599999));
#256270=CARTESIAN_POINT('Ctrl Pts',(-10.6065545400001,11.6,1.75392106599999));
#256271=CARTESIAN_POINT('Ctrl Pts',(-10.6042674140001,15.2,1.75283912199999));
#256272=CARTESIAN_POINT('Ctrl Pts',(-10.6042674140001,11.6,1.75283912199998));
#256273=CARTESIAN_POINT('Ctrl Pts',(-10.6019848890001,15.2,1.75176175199999));
#256274=CARTESIAN_POINT('Ctrl Pts',(-10.6019848890001,11.6,1.75176175199998));
#256275=CARTESIAN_POINT('Ctrl Pts',(-10.5997069780001,15.2,1.75068894899999));
#256276=CARTESIAN_POINT('Ctrl Pts',(-10.5997069780001,11.6,1.75068894899999));
#256277=CARTESIAN_POINT('Ctrl Pts',(-10.5974336980001,15.2,1.74962071099999));
#256278=CARTESIAN_POINT('Ctrl Pts',(-10.5974336980001,11.6,1.74962071099999));
#256279=CARTESIAN_POINT('Ctrl Pts',(-10.5951650630001,15.2,1.74855703599999));
#256280=CARTESIAN_POINT('Ctrl Pts',(-10.5951650630001,11.6,1.74855703599999));
#256281=CARTESIAN_POINT('Ctrl Pts',(-10.5929010880001,15.2,1.74749791899998));
#256282=CARTESIAN_POINT('Ctrl Pts',(-10.5929010880001,11.6,1.74749791899998));
#256283=CARTESIAN_POINT('Ctrl Pts',(-10.5906417870001,15.2,1.74644335699998));
#256284=CARTESIAN_POINT('Ctrl Pts',(-10.5906417870001,11.6,1.74644335699998));
#256285=CARTESIAN_POINT('Ctrl Pts',(-10.5883871760001,15.2,1.74539334799999));
#256286=CARTESIAN_POINT('Ctrl Pts',(-10.5883871760001,11.6,1.74539334799999));
#256287=CARTESIAN_POINT('Ctrl Pts',(-10.5861372680001,15.2,1.74434788599998));
#256288=CARTESIAN_POINT('Ctrl Pts',(-10.5861372680001,11.6,1.74434788599998));
#256289=CARTESIAN_POINT('Ctrl Pts',(-10.5838920800001,15.2,1.74330696999998));
#256290=CARTESIAN_POINT('Ctrl Pts',(-10.5838920800001,11.6,1.74330696999998));
#256291=CARTESIAN_POINT('Ctrl Pts',(-10.5816516250001,15.2,1.74227059599998));
#256292=CARTESIAN_POINT('Ctrl Pts',(-10.5816516250001,11.6,1.74227059599998));
#256293=CARTESIAN_POINT('Ctrl Pts',(-10.5794159210001,15.2,1.74123875899999));
#256294=CARTESIAN_POINT('Ctrl Pts',(-10.5794159210001,11.6,1.74123875899999));
#256295=CARTESIAN_POINT('Ctrl Pts',(-10.5771849800001,15.2,1.74021145699998));
#256296=CARTESIAN_POINT('Ctrl Pts',(-10.5771849800001,11.6,1.74021145699998));
#256297=CARTESIAN_POINT('Ctrl Pts',(-10.5749588180001,15.2,1.73918868699999));
#256298=CARTESIAN_POINT('Ctrl Pts',(-10.5749588180001,11.6,1.73918868699999));
#256299=CARTESIAN_POINT('Ctrl Pts',(-10.5727374500001,15.2,1.73817044399998));
#256300=CARTESIAN_POINT('Ctrl Pts',(-10.5727374500001,11.6,1.73817044399998));
#256301=CARTESIAN_POINT('Ctrl Pts',(-10.5705208910001,15.2,1.73715672499998));
#256302=CARTESIAN_POINT('Ctrl Pts',(-10.5705208910001,11.6,1.73715672499998));
#256303=CARTESIAN_POINT('Ctrl Pts',(-10.5683091580001,15.2,1.73614752599998));
#256304=CARTESIAN_POINT('Ctrl Pts',(-10.5683091580001,11.6,1.73614752599998));
#256305=CARTESIAN_POINT('Ctrl Pts',(-10.5661022630001,15.2,1.73514284399999));
#256306=CARTESIAN_POINT('Ctrl Pts',(-10.5661022630001,11.6,1.73514284399999));
#256307=CARTESIAN_POINT('Ctrl Pts',(-10.5639002250001,15.2,1.73414267699998));
#256308=CARTESIAN_POINT('Ctrl Pts',(-10.5639002250001,11.6,1.73414267699998));
#256309=CARTESIAN_POINT('Ctrl Pts',(-10.5617030560001,15.2,1.73314701799999));
#256310=CARTESIAN_POINT('Ctrl Pts',(-10.5617030560001,11.6,1.73314701799998));
#256311=CARTESIAN_POINT('Ctrl Pts',(-10.5595107720001,15.2,1.73215586599999));
#256312=CARTESIAN_POINT('Ctrl Pts',(-10.5595107720001,11.6,1.73215586599999));
#256313=CARTESIAN_POINT('Ctrl Pts',(-10.5573233910001,15.2,1.73116921599998));
#256314=CARTESIAN_POINT('Ctrl Pts',(-10.5573233910001,11.6,1.73116921599998));
#256315=CARTESIAN_POINT('Ctrl Pts',(-10.5551409250001,15.2,1.73018706499999));
#256316=CARTESIAN_POINT('Ctrl Pts',(-10.5551409250001,11.6,1.73018706499999));
#256317=CARTESIAN_POINT('Ctrl Pts',(-10.5529633920001,15.2,1.72920940799999));
#256318=CARTESIAN_POINT('Ctrl Pts',(-10.5529633920001,11.6,1.72920940799999));
#256319=CARTESIAN_POINT('Ctrl Pts',(-10.5507908060001,15.2,1.72823624299999));
#256320=CARTESIAN_POINT('Ctrl Pts',(-10.5507908060001,11.6,1.72823624299998));
#256321=CARTESIAN_POINT('Ctrl Pts',(-10.5486231830001,15.2,1.72726756599999));
#256322=CARTESIAN_POINT('Ctrl Pts',(-10.5486231830001,11.6,1.72726756599999));
#256323=CARTESIAN_POINT('Ctrl Pts',(-10.5464605390001,15.2,1.72630337199998));
#256324=CARTESIAN_POINT('Ctrl Pts',(-10.5464605390001,11.6,1.72630337199998));
#256325=CARTESIAN_POINT('Ctrl Pts',(-10.5443028890001,15.2,1.72534365799998));
#256326=CARTESIAN_POINT('Ctrl Pts',(-10.5443028890001,11.6,1.72534365799998));
#256327=CARTESIAN_POINT('Ctrl Pts',(-10.5421502500001,15.2,1.72438842099998));
#256328=CARTESIAN_POINT('Ctrl Pts',(-10.5421502500001,11.6,1.72438842099998));
#256329=CARTESIAN_POINT('Ctrl Pts',(-10.5400026350001,15.2,1.72343765499999));
#256330=CARTESIAN_POINT('Ctrl Pts',(-10.5400026350001,11.6,1.72343765499999));
#256331=CARTESIAN_POINT('Ctrl Pts',(-10.5378600620001,15.2,1.72249135799999));
#256332=CARTESIAN_POINT('Ctrl Pts',(-10.5378600620001,11.6,1.72249135799999));
#256333=CARTESIAN_POINT('Ctrl Pts',(-10.5357225470001,15.2,1.72154952499998));
#256334=CARTESIAN_POINT('Ctrl Pts',(-10.5357225470001,11.6,1.72154952499998));
#256335=CARTESIAN_POINT('Ctrl Pts',(-10.5335901050001,15.2,1.72061215299999));
#256336=CARTESIAN_POINT('Ctrl Pts',(-10.5335901050001,11.6,1.72061215299998));
#256337=CARTESIAN_POINT('Ctrl Pts',(-10.5314627510001,15.2,1.71967923799999));
#256338=CARTESIAN_POINT('Ctrl Pts',(-10.5314627510001,11.6,1.71967923799999));
#256339=CARTESIAN_POINT('Ctrl Pts',(-10.5293405040001,15.2,1.71875077499998));
#256340=CARTESIAN_POINT('Ctrl Pts',(-10.5293405040001,11.6,1.71875077499998));
#256341=CARTESIAN_POINT('Ctrl Pts',(-10.5272233760001,15.2,1.71782676099999));
#256342=CARTESIAN_POINT('Ctrl Pts',(-10.5272233760001,11.6,1.71782676099998));
#256343=CARTESIAN_POINT('Ctrl Pts',(-10.5251113870001,15.2,1.71690719299999));
#256344=CARTESIAN_POINT('Ctrl Pts',(-10.5251113870001,11.6,1.71690719299999));
#256345=CARTESIAN_POINT('Ctrl Pts',(-10.5230045500001,15.2,1.71599206399998));
#256346=CARTESIAN_POINT('Ctrl Pts',(-10.5230045500001,11.6,1.71599206399998));
#256347=CARTESIAN_POINT('Ctrl Pts',(-10.5209028820001,15.2,1.71508137299998));
#256348=CARTESIAN_POINT('Ctrl Pts',(-10.5209028820001,11.6,1.71508137299998));
#256349=CARTESIAN_POINT('Ctrl Pts',(-10.5188064000001,15.2,1.71417511399999));
#256350=CARTESIAN_POINT('Ctrl Pts',(-10.5188064000001,11.6,1.71417511399999));
#256351=CARTESIAN_POINT('Ctrl Pts',(-10.5167151200001,15.2,1.71327328299999));
#256352=CARTESIAN_POINT('Ctrl Pts',(-10.5167151200001,11.6,1.71327328299998));
#256353=CARTESIAN_POINT('Ctrl Pts',(-10.5146290570001,15.2,1.71237587699999));
#256354=CARTESIAN_POINT('Ctrl Pts',(-10.5146290570001,11.6,1.71237587699998));
#256355=CARTESIAN_POINT('Ctrl Pts',(-10.5125482280001,15.2,1.71148289099999));
#256356=CARTESIAN_POINT('Ctrl Pts',(-10.5125482280001,11.6,1.71148289099999));
#256357=CARTESIAN_POINT('Ctrl Pts',(-10.5104726510001,15.2,1.71059432099999));
#256358=CARTESIAN_POINT('Ctrl Pts',(-10.5104726510001,11.6,1.71059432099998));
#256359=CARTESIAN_POINT('Ctrl Pts',(-10.5084023400001,15.2,1.70971016399998));
#256360=CARTESIAN_POINT('Ctrl Pts',(-10.5084023400001,11.6,1.70971016399998));
#256361=CARTESIAN_POINT('Ctrl Pts',(-10.5063373130001,15.2,1.70883041399998));
#256362=CARTESIAN_POINT('Ctrl Pts',(-10.5063373130001,11.6,1.70883041399998));
#256363=CARTESIAN_POINT('Ctrl Pts',(-10.5042775850001,15.2,1.70795506799998));
#256364=CARTESIAN_POINT('Ctrl Pts',(-10.5042775850001,11.6,1.70795506799998));
#256365=CARTESIAN_POINT('Ctrl Pts',(-10.5022231740001,15.2,1.70708412099998));
#256366=CARTESIAN_POINT('Ctrl Pts',(-10.5022231740001,11.6,1.70708412099998));
#256367=CARTESIAN_POINT('Ctrl Pts',(-10.5001740970001,15.2,1.70621756899999));
#256368=CARTESIAN_POINT('Ctrl Pts',(-10.5001740970001,11.6,1.70621756899999));
#256369=CARTESIAN_POINT('Ctrl Pts',(-10.4981303680001,15.2,1.70535540799999));
#256370=CARTESIAN_POINT('Ctrl Pts',(-10.4981303680001,11.6,1.70535540799999));
#256371=CARTESIAN_POINT('Ctrl Pts',(-10.4960920060001,15.2,1.70449763199999));
#256372=CARTESIAN_POINT('Ctrl Pts',(-10.4960920060001,11.6,1.70449763199999));
#256373=CARTESIAN_POINT('Ctrl Pts',(-10.4940590280001,15.2,1.70364423899999));
#256374=CARTESIAN_POINT('Ctrl Pts',(-10.4940590280001,11.6,1.70364423899999));
#256375=CARTESIAN_POINT('Ctrl Pts',(-10.4920314490001,15.2,1.70279522299999));
#256376=CARTESIAN_POINT('Ctrl Pts',(-10.4920314490001,11.6,1.70279522299999));
#256377=CARTESIAN_POINT('Ctrl Pts',(-10.4900092880001,15.2,1.70195057999999));
#256378=CARTESIAN_POINT('Ctrl Pts',(-10.4900092880001,11.6,1.70195057999999));
#256379=CARTESIAN_POINT('Ctrl Pts',(-10.4879925600001,15.2,1.70111030699998));
#256380=CARTESIAN_POINT('Ctrl Pts',(-10.4879925600001,11.6,1.70111030699998));
#256381=CARTESIAN_POINT('Ctrl Pts',(-10.4859812820001,15.2,1.70027439699998));
#256382=CARTESIAN_POINT('Ctrl Pts',(-10.4859812820001,11.6,1.70027439699998));
#256383=CARTESIAN_POINT('Ctrl Pts',(-10.4839754720001,15.2,1.69944284799998));
#256384=CARTESIAN_POINT('Ctrl Pts',(-10.4839754720001,11.6,1.69944284799998));
#256385=CARTESIAN_POINT('Ctrl Pts',(-10.4819751470001,15.2,1.69861565499998));
#256386=CARTESIAN_POINT('Ctrl Pts',(-10.4819751470001,11.6,1.69861565499998));
#256387=CARTESIAN_POINT('Ctrl Pts',(-10.4799803230001,15.2,1.69779281099999));
#256388=CARTESIAN_POINT('Ctrl Pts',(-10.4799803230001,11.6,1.69779281099998));
#256389=CARTESIAN_POINT('Ctrl Pts',(-10.4779910190001,15.2,1.69697431399999));
#256390=CARTESIAN_POINT('Ctrl Pts',(-10.4779910190001,11.6,1.69697431399999));
#256391=CARTESIAN_POINT('Ctrl Pts',(-10.4760072500001,15.2,1.69616015899999));
#256392=CARTESIAN_POINT('Ctrl Pts',(-10.4760072500001,11.6,1.69616015899999));
#256393=CARTESIAN_POINT('Ctrl Pts',(-10.4740290340001,15.2,1.69535034099999));
#256394=CARTESIAN_POINT('Ctrl Pts',(-10.4740290340001,11.6,1.69535034099999));
#256395=CARTESIAN_POINT('Ctrl Pts',(-10.4720563900001,15.2,1.69454485499998));
#256396=CARTESIAN_POINT('Ctrl Pts',(-10.4720563900001,11.6,1.69454485499998));
#256397=CARTESIAN_POINT('Ctrl Pts',(-10.4700893330001,15.2,1.69374369699999));
#256398=CARTESIAN_POINT('Ctrl Pts',(-10.4700893330001,11.6,1.69374369699998));
#256399=CARTESIAN_POINT('Ctrl Pts',(-10.4681278810001,15.2,1.69294686299999));
#256400=CARTESIAN_POINT('Ctrl Pts',(-10.4681278810001,11.6,1.69294686299999));
#256401=CARTESIAN_POINT('Ctrl Pts',(-10.4661720530001,15.2,1.69215434599999));
#256402=CARTESIAN_POINT('Ctrl Pts',(-10.4661720530001,11.6,1.69215434599999));
#256403=CARTESIAN_POINT('Ctrl Pts',(-10.4642218640001,15.2,1.69136614299998));
#256404=CARTESIAN_POINT('Ctrl Pts',(-10.4642218640001,11.6,1.69136614299998));
#256405=CARTESIAN_POINT('Ctrl Pts',(-10.4622773340001,15.2,1.69058224899999));
#256406=CARTESIAN_POINT('Ctrl Pts',(-10.4622773340001,11.6,1.69058224899999));
#256407=CARTESIAN_POINT('Ctrl Pts',(-10.4603384780001,15.2,1.68980265999998));
#256408=CARTESIAN_POINT('Ctrl Pts',(-10.4603384780001,11.6,1.68980265999998));
#256409=CARTESIAN_POINT('Ctrl Pts',(-10.4584053160001,15.2,1.68902736899998));
#256410=CARTESIAN_POINT('Ctrl Pts',(-10.4584053160001,11.6,1.68902736899998));
#256411=CARTESIAN_POINT('Ctrl Pts',(-10.4564778650001,15.2,1.68825637299999));
#256412=CARTESIAN_POINT('Ctrl Pts',(-10.4564778650001,11.6,1.68825637299999));
#256413=CARTESIAN_POINT('Ctrl Pts',(-10.4545561420001,15.2,1.68748966599999));
#256414=CARTESIAN_POINT('Ctrl Pts',(-10.4545561420001,11.6,1.68748966599999));
#256415=CARTESIAN_POINT('Ctrl Pts',(-10.4526401670001,15.2,1.68672724499999));
#256416=CARTESIAN_POINT('Ctrl Pts',(-10.4526401670001,11.6,1.68672724499999));
#256417=CARTESIAN_POINT('Ctrl Pts',(-10.4507299550001,15.2,1.68596910299998));
#256418=CARTESIAN_POINT('Ctrl Pts',(-10.4507299550001,11.6,1.68596910299998));
#256419=CARTESIAN_POINT('Ctrl Pts',(-10.4488255250001,15.2,1.68521523599999));
#256420=CARTESIAN_POINT('Ctrl Pts',(-10.4488255250001,11.6,1.68521523599999));
#256421=CARTESIAN_POINT('Ctrl Pts',(-10.4469268960001,15.2,1.68446563799999));
#256422=CARTESIAN_POINT('Ctrl Pts',(-10.4469268960001,11.6,1.68446563799999));
#256423=CARTESIAN_POINT('Ctrl Pts',(-10.4450340850001,15.2,1.68372030599999));
#256424=CARTESIAN_POINT('Ctrl Pts',(-10.4450340850001,11.6,1.68372030599999));
#256425=CARTESIAN_POINT('Ctrl Pts',(-10.4431471100001,15.2,1.68297923299999));
#256426=CARTESIAN_POINT('Ctrl Pts',(-10.4431471100001,11.6,1.68297923299999));
#256427=CARTESIAN_POINT('Ctrl Pts',(-10.4412659910001,15.2,1.68224241499999));
#256428=CARTESIAN_POINT('Ctrl Pts',(-10.4412659910001,11.6,1.68224241499999));
#256429=CARTESIAN_POINT('Ctrl Pts',(-10.4393907430001,15.2,1.68150984699999));
#256430=CARTESIAN_POINT('Ctrl Pts',(-10.4393907430001,11.6,1.68150984699999));
#256431=CARTESIAN_POINT('Ctrl Pts',(-10.4375213870001,15.2,1.68078152299998));
#256432=CARTESIAN_POINT('Ctrl Pts',(-10.4375213870001,11.6,1.68078152299998));
#256433=CARTESIAN_POINT('Ctrl Pts',(-10.4356579400001,15.2,1.68005743899998));
#256434=CARTESIAN_POINT('Ctrl Pts',(-10.4356579400001,11.6,1.68005743899998));
#256435=CARTESIAN_POINT('Ctrl Pts',(-10.4338004210001,15.2,1.67933758899999));
#256436=CARTESIAN_POINT('Ctrl Pts',(-10.4338004210001,11.6,1.67933758899998));
#256437=CARTESIAN_POINT('Ctrl Pts',(-10.4319488490001,15.2,1.67862196699998));
#256438=CARTESIAN_POINT('Ctrl Pts',(-10.4319488490001,11.6,1.67862196699998));
#256439=CARTESIAN_POINT('Ctrl Pts',(-10.4301032410001,15.2,1.67791056899999));
#256440=CARTESIAN_POINT('Ctrl Pts',(-10.4301032410001,11.6,1.67791056899999));
#256441=CARTESIAN_POINT('Ctrl Pts',(-10.4282636170001,15.2,1.67720339099999));
#256442=CARTESIAN_POINT('Ctrl Pts',(-10.4282636170001,11.6,1.67720339099999));
#256443=CARTESIAN_POINT('Ctrl Pts',(-10.4264299930001,15.2,1.67650042499998));
#256444=CARTESIAN_POINT('Ctrl Pts',(-10.4264299930001,11.6,1.67650042499998));
#256445=CARTESIAN_POINT('Ctrl Pts',(-10.4246023920001,15.2,1.67580166599999));
#256446=CARTESIAN_POINT('Ctrl Pts',(-10.4246023920001,11.6,1.67580166599999));
#256447=CARTESIAN_POINT('Ctrl Pts',(-10.4227808290001,15.2,1.67510710999998));
#256448=CARTESIAN_POINT('Ctrl Pts',(-10.4227808290001,11.6,1.67510710999998));
#256449=CARTESIAN_POINT('Ctrl Pts',(-10.4209653250001,15.2,1.67441675099999));
#256450=CARTESIAN_POINT('Ctrl Pts',(-10.4209653250001,11.6,1.67441675099999));
#256451=CARTESIAN_POINT('Ctrl Pts',(-10.4191558970001,15.2,1.67373058499999));
#256452=CARTESIAN_POINT('Ctrl Pts',(-10.4191558970001,11.6,1.67373058499999));
#256453=CARTESIAN_POINT('Ctrl Pts',(-10.4173525660001,15.2,1.67304860399998));
#256454=CARTESIAN_POINT('Ctrl Pts',(-10.4173525660001,11.6,1.67304860399998));
#256455=CARTESIAN_POINT('Ctrl Pts',(-10.4155553510001,15.2,1.67237080499998));
#256456=CARTESIAN_POINT('Ctrl Pts',(-10.4155553510001,11.6,1.67237080499998));
#256457=CARTESIAN_POINT('Ctrl Pts',(-10.4137642690001,15.2,1.67169717899998));
#256458=CARTESIAN_POINT('Ctrl Pts',(-10.4137642690001,11.6,1.67169717899998));
#256459=CARTESIAN_POINT('Ctrl Pts',(-10.4119793400001,15.2,1.67102772499998));
#256460=CARTESIAN_POINT('Ctrl Pts',(-10.4119793400001,11.6,1.67102772499998));
#256461=CARTESIAN_POINT('Ctrl Pts',(-10.4102005840001,15.2,1.67036243499998));
#256462=CARTESIAN_POINT('Ctrl Pts',(-10.4102005840001,11.6,1.67036243499998));
#256463=CARTESIAN_POINT('Ctrl Pts',(-10.4084280180001,15.2,1.66970130199998));
#256464=CARTESIAN_POINT('Ctrl Pts',(-10.4084280180001,11.6,1.66970130199998));
#256465=CARTESIAN_POINT('Ctrl Pts',(-10.4066616650001,15.2,1.66904432199999));
#256466=CARTESIAN_POINT('Ctrl Pts',(-10.4066616650001,11.6,1.66904432199999));
#256467=CARTESIAN_POINT('Ctrl Pts',(-10.4049015420001,15.2,1.66839148999999));
#256468=CARTESIAN_POINT('Ctrl Pts',(-10.4049015420001,11.6,1.66839148999998));
#256469=CARTESIAN_POINT('Ctrl Pts',(-10.4031476680001,15.2,1.66774279999998));
#256470=CARTESIAN_POINT('Ctrl Pts',(-10.4031476680001,11.6,1.66774279999998));
#256471=CARTESIAN_POINT('Ctrl Pts',(-10.4014000640001,15.2,1.66709824499998));
#256472=CARTESIAN_POINT('Ctrl Pts',(-10.4014000640001,11.6,1.66709824499998));
#256473=CARTESIAN_POINT('Ctrl Pts',(-10.3996587490001,15.2,1.66645781999998));
#256474=CARTESIAN_POINT('Ctrl Pts',(-10.3996587490001,11.6,1.66645781999998));
#256475=CARTESIAN_POINT('Ctrl Pts',(-10.3979237410001,15.2,1.66582151999998));
#256476=CARTESIAN_POINT('Ctrl Pts',(-10.3979237410001,11.6,1.66582151999998));
#256477=CARTESIAN_POINT('Ctrl Pts',(-10.3961950630001,15.2,1.66518933799999));
#256478=CARTESIAN_POINT('Ctrl Pts',(-10.3961950630001,11.6,1.66518933799999));
#256479=CARTESIAN_POINT('Ctrl Pts',(-10.3944727320001,15.2,1.66456126899998));
#256480=CARTESIAN_POINT('Ctrl Pts',(-10.3944727320001,11.6,1.66456126899998));
#256481=CARTESIAN_POINT('Ctrl Pts',(-10.3927567690001,15.2,1.66393730599999));
#256482=CARTESIAN_POINT('Ctrl Pts',(-10.3927567690001,11.6,1.66393730599998));
#256483=CARTESIAN_POINT('Ctrl Pts',(-10.3910471940001,15.2,1.66331744399999));
#256484=CARTESIAN_POINT('Ctrl Pts',(-10.3910471940001,11.6,1.66331744399998));
#256485=CARTESIAN_POINT('Ctrl Pts',(-10.3893440270001,15.2,1.66270167599999));
#256486=CARTESIAN_POINT('Ctrl Pts',(-10.3893440270001,11.6,1.66270167599999));
#256487=CARTESIAN_POINT('Ctrl Pts',(-10.3876472860001,15.2,1.66208999799998));
#256488=CARTESIAN_POINT('Ctrl Pts',(-10.3876472860001,11.6,1.66208999799998));
#256489=CARTESIAN_POINT('Ctrl Pts',(-10.3859569940001,15.2,1.66148240199998));
#256490=CARTESIAN_POINT('Ctrl Pts',(-10.3859569940001,11.6,1.66148240199998));
#256491=CARTESIAN_POINT('Ctrl Pts',(-10.3842731710001,15.2,1.66087888299999));
#256492=CARTESIAN_POINT('Ctrl Pts',(-10.3842731710001,11.6,1.66087888299998));
#256493=CARTESIAN_POINT('Ctrl Pts',(-10.3825958360001,15.2,1.66027943499999));
#256494=CARTESIAN_POINT('Ctrl Pts',(-10.3825958360001,11.6,1.66027943499999));
#256495=CARTESIAN_POINT('Ctrl Pts',(-10.3809250080001,15.2,1.65968405099999));
#256496=CARTESIAN_POINT('Ctrl Pts',(-10.3809250080001,11.6,1.65968405099999));
#256497=CARTESIAN_POINT('Ctrl Pts',(-10.3792607110001,15.2,1.65909272599999));
#256498=CARTESIAN_POINT('Ctrl Pts',(-10.3792607110001,11.6,1.65909272599999));
#256499=CARTESIAN_POINT('Ctrl Pts',(-10.3776029620001,15.2,1.65850545199998));
#256500=CARTESIAN_POINT('Ctrl Pts',(-10.3776029620001,11.6,1.65850545199998));
#256501=CARTESIAN_POINT('Ctrl Pts',(-10.3759517830001,15.2,1.65792222499999));
#256502=CARTESIAN_POINT('Ctrl Pts',(-10.3759517830001,11.6,1.65792222499999));
#256503=CARTESIAN_POINT('Ctrl Pts',(-10.3743071950001,15.2,1.65734303799999));
#256504=CARTESIAN_POINT('Ctrl Pts',(-10.3743071950001,11.6,1.65734303799998));
#256505=CARTESIAN_POINT('Ctrl Pts',(-10.3726692190001,15.2,1.65676788299999));
#256506=CARTESIAN_POINT('Ctrl Pts',(-10.3726692190001,11.6,1.65676788299999));
#256507=CARTESIAN_POINT('Ctrl Pts',(-10.3710378740001,15.2,1.65619675499999));
#256508=CARTESIAN_POINT('Ctrl Pts',(-10.3710378740001,11.6,1.65619675499999));
#256509=CARTESIAN_POINT('Ctrl Pts',(-10.3694131820001,15.2,1.65562964899999));
#256510=CARTESIAN_POINT('Ctrl Pts',(-10.3694131820001,11.6,1.65562964899999));
#256511=CARTESIAN_POINT('Ctrl Pts',(-10.3677951640001,15.2,1.65506655599998));
#256512=CARTESIAN_POINT('Ctrl Pts',(-10.3677951640001,11.6,1.65506655599998));
#256513=CARTESIAN_POINT('Ctrl Pts',(-10.3661838400001,15.2,1.65450747099999));
#256514=CARTESIAN_POINT('Ctrl Pts',(-10.3661838400001,11.6,1.65450747099999));
#256515=CARTESIAN_POINT('Ctrl Pts',(-10.3645792330001,15.2,1.65395238799999));
#256516=CARTESIAN_POINT('Ctrl Pts',(-10.3645792330001,11.6,1.65395238799999));
#256517=CARTESIAN_POINT('Ctrl Pts',(-10.3629813620001,15.2,1.65340129999999));
#256518=CARTESIAN_POINT('Ctrl Pts',(-10.3629813620001,11.6,1.65340129999999));
#256519=CARTESIAN_POINT('Ctrl Pts',(-10.3613902500001,15.2,1.65285419899998));
#256520=CARTESIAN_POINT('Ctrl Pts',(-10.3613902500001,11.6,1.65285419899998));
#256521=CARTESIAN_POINT('Ctrl Pts',(-10.3598059160001,15.2,1.65231107999999));
#256522=CARTESIAN_POINT('Ctrl Pts',(-10.3598059160001,11.6,1.65231107999999));
#256523=CARTESIAN_POINT('Ctrl Pts',(-10.3582283850001,15.2,1.65177193599999));
#256524=CARTESIAN_POINT('Ctrl Pts',(-10.3582283850001,11.6,1.65177193599999));
#256525=CARTESIAN_POINT('Ctrl Pts',(-10.3566576740001,15.2,1.65123676099999));
#256526=CARTESIAN_POINT('Ctrl Pts',(-10.3566576740001,11.6,1.65123676099999));
#256527=CARTESIAN_POINT('Ctrl Pts',(-10.3550938080001,15.2,1.65070554699998));
#256528=CARTESIAN_POINT('Ctrl Pts',(-10.3550938080001,11.6,1.65070554699998));
#256529=CARTESIAN_POINT('Ctrl Pts',(-10.3535368060001,15.2,1.65017828799999));
#256530=CARTESIAN_POINT('Ctrl Pts',(-10.3535368060001,11.6,1.65017828799999));
#256531=CARTESIAN_POINT('Ctrl Pts',(-10.3519866920001,15.2,1.64965497699999));
#256532=CARTESIAN_POINT('Ctrl Pts',(-10.3519866920001,11.6,1.64965497699999));
#256533=CARTESIAN_POINT('Ctrl Pts',(-10.3504434860001,15.2,1.64913560699999));
#256534=CARTESIAN_POINT('Ctrl Pts',(-10.3504434860001,11.6,1.64913560699999));
#256535=CARTESIAN_POINT('Ctrl Pts',(-10.3489072110001,15.2,1.64862017299999));
#256536=CARTESIAN_POINT('Ctrl Pts',(-10.3489072110001,11.6,1.64862017299999));
#256537=CARTESIAN_POINT('Ctrl Pts',(-10.3473778890001,15.2,1.64810866399999));
#256538=CARTESIAN_POINT('Ctrl Pts',(-10.3473778890001,11.6,1.64810866399998));
#256539=CARTESIAN_POINT('Ctrl Pts',(-10.3458555400001,15.2,1.64760107799999));
#256540=CARTESIAN_POINT('Ctrl Pts',(-10.3458555400001,11.6,1.64760107799998));
#256541=CARTESIAN_POINT('Ctrl Pts',(-10.3443401890001,15.2,1.64709740399998));
#256542=CARTESIAN_POINT('Ctrl Pts',(-10.3443401890001,11.6,1.64709740399998));
#256543=CARTESIAN_POINT('Ctrl Pts',(-10.3428318550001,15.2,1.64659763699999));
#256544=CARTESIAN_POINT('Ctrl Pts',(-10.3428318550001,11.6,1.64659763699999));
#256545=CARTESIAN_POINT('Ctrl Pts',(-10.3413305630001,15.2,1.64610176999998));
#256546=CARTESIAN_POINT('Ctrl Pts',(-10.3413305630001,11.6,1.64610176999998));
#256547=CARTESIAN_POINT('Ctrl Pts',(-10.3398363340001,15.2,1.64560979499999));
#256548=CARTESIAN_POINT('Ctrl Pts',(-10.3398363340001,11.6,1.64560979499999));
#256549=CARTESIAN_POINT('Ctrl Pts',(-10.3383491910001,15.2,1.64512170499998));
#256550=CARTESIAN_POINT('Ctrl Pts',(-10.3383491910001,11.6,1.64512170499998));
#256551=CARTESIAN_POINT('Ctrl Pts',(-10.3368691540001,15.2,1.64463749399999));
#256552=CARTESIAN_POINT('Ctrl Pts',(-10.3368691540001,11.6,1.64463749399998));
#256553=CARTESIAN_POINT('Ctrl Pts',(-10.3353962500001,15.2,1.64415715299999));
#256554=CARTESIAN_POINT('Ctrl Pts',(-10.3353962500001,11.6,1.64415715299999));
#256555=CARTESIAN_POINT('Ctrl Pts',(-10.3339304990001,15.2,1.64368067599999));
#256556=CARTESIAN_POINT('Ctrl Pts',(-10.3339304990001,11.6,1.64368067599999));
#256557=CARTESIAN_POINT('Ctrl Pts',(-10.3324719230001,15.2,1.64320805599999));
#256558=CARTESIAN_POINT('Ctrl Pts',(-10.3324719230001,11.6,1.64320805599999));
#256559=CARTESIAN_POINT('Ctrl Pts',(-10.3310205470001,15.2,1.64273928299998));
#256560=CARTESIAN_POINT('Ctrl Pts',(-10.3310205470001,11.6,1.64273928299998));
#256561=CARTESIAN_POINT('Ctrl Pts',(-10.3295763920001,15.2,1.64227435299999));
#256562=CARTESIAN_POINT('Ctrl Pts',(-10.3295763920001,11.6,1.64227435299999));
#256563=CARTESIAN_POINT('Ctrl Pts',(-10.3281394820001,15.2,1.64181325699999));
#256564=CARTESIAN_POINT('Ctrl Pts',(-10.3281394820001,11.6,1.64181325699999));
#256565=CARTESIAN_POINT('Ctrl Pts',(-10.3267098410001,15.2,1.64135598899998));
#256566=CARTESIAN_POINT('Ctrl Pts',(-10.3267098410001,11.6,1.64135598899998));
#256567=CARTESIAN_POINT('Ctrl Pts',(-10.3252874890001,15.2,1.64090253799999));
#256568=CARTESIAN_POINT('Ctrl Pts',(-10.3252874890001,11.6,1.64090253799999));
#256569=CARTESIAN_POINT('Ctrl Pts',(-10.3238724540001,15.2,1.64045289999999));
#256570=CARTESIAN_POINT('Ctrl Pts',(-10.3238724540001,11.6,1.64045289999999));
#256571=CARTESIAN_POINT('Ctrl Pts',(-10.3224647550001,15.2,1.64000706499999));
#256572=CARTESIAN_POINT('Ctrl Pts',(-10.3224647550001,11.6,1.64000706499999));
#256573=CARTESIAN_POINT('Ctrl Pts',(-10.3210644180001,15.2,1.63956502799998));
#256574=CARTESIAN_POINT('Ctrl Pts',(-10.3210644180001,11.6,1.63956502799998));
#256575=CARTESIAN_POINT('Ctrl Pts',(-10.3196714660001,15.2,1.63912677799999));
#256576=CARTESIAN_POINT('Ctrl Pts',(-10.3196714660001,11.6,1.63912677799999));
#256577=CARTESIAN_POINT('Ctrl Pts',(-10.3182859220001,15.2,1.63869230999998));
#256578=CARTESIAN_POINT('Ctrl Pts',(-10.3182859220001,11.6,1.63869230999998));
#256579=CARTESIAN_POINT('Ctrl Pts',(-10.3169078100001,15.2,1.63826161499999));
#256580=CARTESIAN_POINT('Ctrl Pts',(-10.3169078100001,11.6,1.63826161499998));
#256581=CARTESIAN_POINT('Ctrl Pts',(-10.3155371550001,15.2,1.63783468499998));
#256582=CARTESIAN_POINT('Ctrl Pts',(-10.3155371550001,11.6,1.63783468499998));
#256583=CARTESIAN_POINT('Ctrl Pts',(-10.3141739780001,15.2,1.63741151199998));
#256584=CARTESIAN_POINT('Ctrl Pts',(-10.3141739780001,11.6,1.63741151199998));
#256585=CARTESIAN_POINT('Ctrl Pts',(-10.3128183080001,15.2,1.63699208999999));
#256586=CARTESIAN_POINT('Ctrl Pts',(-10.3128183080001,11.6,1.63699208999999));
#256587=CARTESIAN_POINT('Ctrl Pts',(-10.3114701640001,15.2,1.63657640799999));
#256588=CARTESIAN_POINT('Ctrl Pts',(-10.3114701640001,11.6,1.63657640799999));
#256589=CARTESIAN_POINT('Ctrl Pts',(-10.3101295730001,15.2,1.63616446099998));
#256590=CARTESIAN_POINT('Ctrl Pts',(-10.3101295730001,11.6,1.63616446099998));
#256591=CARTESIAN_POINT('Ctrl Pts',(-10.3087965590001,15.2,1.63575623899999));
#256592=CARTESIAN_POINT('Ctrl Pts',(-10.3087965590001,11.6,1.63575623899999));
#256593=CARTESIAN_POINT('Ctrl Pts',(-10.3074711460001,15.2,1.63535173399998));
#256594=CARTESIAN_POINT('Ctrl Pts',(-10.3074711460001,11.6,1.63535173399998));
#256595=CARTESIAN_POINT('Ctrl Pts',(-10.3061533570001,15.2,1.63495093799999));
#256596=CARTESIAN_POINT('Ctrl Pts',(-10.3061533570001,11.6,1.63495093799999));
#256597=CARTESIAN_POINT('Ctrl Pts',(-10.3048432200001,15.2,1.63455384399999));
#256598=CARTESIAN_POINT('Ctrl Pts',(-10.3048432200001,11.6,1.63455384399999));
#256599=CARTESIAN_POINT('Ctrl Pts',(-10.3035407580001,15.2,1.63416044299999));
#256600=CARTESIAN_POINT('Ctrl Pts',(-10.3035407580001,11.6,1.63416044299999));
#256601=CARTESIAN_POINT('Ctrl Pts',(-10.3022459950001,15.2,1.63377072599999));
#256602=CARTESIAN_POINT('Ctrl Pts',(-10.3022459950001,11.6,1.63377072599999));
#256603=CARTESIAN_POINT('Ctrl Pts',(-10.3009589570001,15.2,1.63338468499999));
#256604=CARTESIAN_POINT('Ctrl Pts',(-10.3009589570001,11.6,1.63338468499999));
#256605=CARTESIAN_POINT('Ctrl Pts',(-10.2996796700001,15.2,1.63300231199999));
#256606=CARTESIAN_POINT('Ctrl Pts',(-10.2996796700001,11.6,1.63300231199999));
#256607=CARTESIAN_POINT('Ctrl Pts',(-10.2984081560001,15.2,1.63262359999999));
#256608=CARTESIAN_POINT('Ctrl Pts',(-10.2984081560001,11.6,1.63262359999999));
#256609=CARTESIAN_POINT('Ctrl Pts',(-10.2971444420001,15.2,1.63224853699999));
#256610=CARTESIAN_POINT('Ctrl Pts',(-10.2971444420001,11.6,1.63224853699999));
#256611=CARTESIAN_POINT('Ctrl Pts',(-10.2958885550001,15.2,1.63187711599999));
#256612=CARTESIAN_POINT('Ctrl Pts',(-10.2958885550001,11.6,1.63187711599999));
#256613=CARTESIAN_POINT('Ctrl Pts',(-10.2946405180001,15.2,1.63150932999998));
#256614=CARTESIAN_POINT('Ctrl Pts',(-10.2946405180001,11.6,1.63150932999998));
#256615=CARTESIAN_POINT('Ctrl Pts',(-10.2934003580001,15.2,1.63114516899999));
#256616=CARTESIAN_POINT('Ctrl Pts',(-10.2934003580001,11.6,1.63114516899999));
#256617=CARTESIAN_POINT('Ctrl Pts',(-10.2921680990001,15.2,1.63078462399998));
#256618=CARTESIAN_POINT('Ctrl Pts',(-10.2921680990001,11.6,1.63078462399998));
#256619=CARTESIAN_POINT('Ctrl Pts',(-10.2909437690001,15.2,1.63042768599999));
#256620=CARTESIAN_POINT('Ctrl Pts',(-10.2909437690001,11.6,1.63042768599999));
#256621=CARTESIAN_POINT('Ctrl Pts',(-10.2897273920001,15.2,1.63007434899999));
#256622=CARTESIAN_POINT('Ctrl Pts',(-10.2897273920001,11.6,1.63007434899999));
#256623=CARTESIAN_POINT('Ctrl Pts',(-10.2885189960001,15.2,1.62972459999999));
#256624=CARTESIAN_POINT('Ctrl Pts',(-10.2885189960001,11.6,1.62972459999999));
#256625=CARTESIAN_POINT('Ctrl Pts',(-10.2873186040001,15.2,1.62937843299999));
#256626=CARTESIAN_POINT('Ctrl Pts',(-10.2873186040001,11.6,1.62937843299999));
#256627=CARTESIAN_POINT('Ctrl Pts',(-10.2861262460001,15.2,1.62903583899999));
#256628=CARTESIAN_POINT('Ctrl Pts',(-10.2861262460001,11.6,1.62903583899999));
#256629=CARTESIAN_POINT('Ctrl Pts',(-10.2849419460001,15.2,1.62869680699998));
#256630=CARTESIAN_POINT('Ctrl Pts',(-10.2849419460001,11.6,1.62869680699998));
#256631=CARTESIAN_POINT('Ctrl Pts',(-10.2837657300001,15.2,1.62836132999999));
#256632=CARTESIAN_POINT('Ctrl Pts',(-10.2837657300001,11.6,1.62836132999999));
#256633=CARTESIAN_POINT('Ctrl Pts',(-10.2825976260001,15.2,1.62802939699999));
#256634=CARTESIAN_POINT('Ctrl Pts',(-10.2825976260001,11.6,1.62802939699999));
#256635=CARTESIAN_POINT('Ctrl Pts',(-10.2814376600001,15.2,1.62770100099999));
#256636=CARTESIAN_POINT('Ctrl Pts',(-10.2814376600001,11.6,1.62770100099999));
#256637=CARTESIAN_POINT('Ctrl Pts',(-10.2802858580001,15.2,1.62737613099999));
#256638=CARTESIAN_POINT('Ctrl Pts',(-10.2802858580001,11.6,1.62737613099999));
#256639=CARTESIAN_POINT('Ctrl Pts',(-10.2791422490001,15.2,1.62705477899999));
#256640=CARTESIAN_POINT('Ctrl Pts',(-10.2791422490001,11.6,1.62705477899999));
#256641=CARTESIAN_POINT('Ctrl Pts',(-10.2780068590001,15.2,1.62673693499999));
#256642=CARTESIAN_POINT('Ctrl Pts',(-10.2780068590001,11.6,1.62673693499999));
#256643=CARTESIAN_POINT('Ctrl Pts',(-10.2768797140001,15.2,1.62642258899998));
#256644=CARTESIAN_POINT('Ctrl Pts',(-10.2768797140001,11.6,1.62642258899998));
#256645=CARTESIAN_POINT('Ctrl Pts',(-10.2757608430001,15.2,1.62611173199998));
#256646=CARTESIAN_POINT('Ctrl Pts',(-10.2757608430001,11.6,1.62611173199998));
#256647=CARTESIAN_POINT('Ctrl Pts',(-10.2746502720001,15.2,1.62580435599998));
#256648=CARTESIAN_POINT('Ctrl Pts',(-10.2746502720001,11.6,1.62580435599998));
#256649=CARTESIAN_POINT('Ctrl Pts',(-10.2735480290001,15.2,1.62550044899998));
#256650=CARTESIAN_POINT('Ctrl Pts',(-10.2735480290001,11.6,1.62550044899998));
#256651=CARTESIAN_POINT('Ctrl Pts',(-10.2724541430001,15.2,1.62520000299998));
#256652=CARTESIAN_POINT('Ctrl Pts',(-10.2724541430001,11.6,1.62520000299998));
#256653=CARTESIAN_POINT('Ctrl Pts',(-10.2713686400001,15.2,1.62490300799998));
#256654=CARTESIAN_POINT('Ctrl Pts',(-10.2713686400001,11.6,1.62490300799998));
#256655=CARTESIAN_POINT('Ctrl Pts',(-10.2702915480001,15.2,1.62460945399999));
#256656=CARTESIAN_POINT('Ctrl Pts',(-10.2702915480001,11.6,1.62460945399999));
#256657=CARTESIAN_POINT('Ctrl Pts',(-10.2692228960001,15.2,1.62431933099999));
#256658=CARTESIAN_POINT('Ctrl Pts',(-10.2692228960001,11.6,1.62431933099999));
#256659=CARTESIAN_POINT('Ctrl Pts',(-10.2681627110001,15.2,1.62403262999999));
#256660=CARTESIAN_POINT('Ctrl Pts',(-10.2681627110001,11.6,1.62403262999998));
#256661=CARTESIAN_POINT('Ctrl Pts',(-10.2671110220001,15.2,1.62374933999998));
#256662=CARTESIAN_POINT('Ctrl Pts',(-10.2671110220001,11.6,1.62374933999998));
#256663=CARTESIAN_POINT('Ctrl Pts',(-10.2660678570001,15.2,1.62346945199999));
#256664=CARTESIAN_POINT('Ctrl Pts',(-10.2660678570001,11.6,1.62346945199999));
#256665=CARTESIAN_POINT('Ctrl Pts',(-10.2650332450001,15.2,1.62319295599998));
#256666=CARTESIAN_POINT('Ctrl Pts',(-10.2650332450001,11.6,1.62319295599998));
#256667=CARTESIAN_POINT('Ctrl Pts',(-10.2640072150001,15.2,1.62291984099999));
#256668=CARTESIAN_POINT('Ctrl Pts',(-10.2640072150001,11.6,1.62291984099999));
#256669=CARTESIAN_POINT('Ctrl Pts',(-10.2629897940001,15.2,1.62265009799999));
#256670=CARTESIAN_POINT('Ctrl Pts',(-10.2629897940001,11.6,1.62265009799999));
#256671=CARTESIAN_POINT('Ctrl Pts',(-10.2619810130001,15.2,1.62238371499999));
#256672=CARTESIAN_POINT('Ctrl Pts',(-10.2619810130001,11.6,1.62238371499999));
#256673=CARTESIAN_POINT('Ctrl Pts',(-10.2609809010001,15.2,1.62212068299999));
#256674=CARTESIAN_POINT('Ctrl Pts',(-10.2609809010001,11.6,1.62212068299999));
#256675=CARTESIAN_POINT('Ctrl Pts',(-10.2599894860001,15.2,1.62186099199999));
#256676=CARTESIAN_POINT('Ctrl Pts',(-10.2599894860001,11.6,1.62186099199999));
#256677=CARTESIAN_POINT('Ctrl Pts',(-10.2590067970001,15.2,1.62160463199998));
#256678=CARTESIAN_POINT('Ctrl Pts',(-10.2590067970001,11.6,1.62160463199998));
#256679=CARTESIAN_POINT('Ctrl Pts',(-10.2580328640001,15.2,1.62135158999998));
#256680=CARTESIAN_POINT('Ctrl Pts',(-10.2580328640001,11.6,1.62135158999998));
#256681=CARTESIAN_POINT('Ctrl Pts',(-10.2570677170001,15.2,1.62110185799999));
#256682=CARTESIAN_POINT('Ctrl Pts',(-10.2570677170001,11.6,1.62110185799999));
#256683=CARTESIAN_POINT('Ctrl Pts',(-10.2561113860001,15.2,1.62085542499999));
#256684=CARTESIAN_POINT('Ctrl Pts',(-10.2561113860001,11.6,1.62085542499998));
#256685=CARTESIAN_POINT('Ctrl Pts',(-10.2551639010001,15.2,1.62061227799999));
#256686=CARTESIAN_POINT('Ctrl Pts',(-10.2551639010001,11.6,1.62061227799999));
#256687=CARTESIAN_POINT('Ctrl Pts',(-10.2542252910001,15.2,1.62037240999998));
#256688=CARTESIAN_POINT('Ctrl Pts',(-10.2542252910001,11.6,1.62037240999998));
#256689=CARTESIAN_POINT('Ctrl Pts',(-10.2532955860001,15.2,1.62013580699998));
#256690=CARTESIAN_POINT('Ctrl Pts',(-10.2532955860001,11.6,1.62013580699998));
#256691=CARTESIAN_POINT('Ctrl Pts',(-10.2523748180001,15.2,1.61990246099998));
#256692=CARTESIAN_POINT('Ctrl Pts',(-10.2523748180001,11.6,1.61990246099998));
#256693=CARTESIAN_POINT('Ctrl Pts',(-10.2514630160001,15.2,1.61967235699999));
#256694=CARTESIAN_POINT('Ctrl Pts',(-10.2514630160001,11.6,1.61967235699999));
#256695=CARTESIAN_POINT('Ctrl Pts',(-10.2505602120001,15.2,1.61944548899998));
#256696=CARTESIAN_POINT('Ctrl Pts',(-10.2505602120001,11.6,1.61944548899998));
#256697=CARTESIAN_POINT('Ctrl Pts',(-10.2496715820001,15.2,1.61922312999998));
#256698=CARTESIAN_POINT('Ctrl Pts',(-10.2496715820001,11.6,1.61922312999998));
#256699=CARTESIAN_POINT('Ctrl Pts',(-10.2489688520001,15.2,1.61904803399999));
#256700=CARTESIAN_POINT('Ctrl Pts',(-10.2489688520001,11.6,1.61904803399999));
#256701=CARTESIAN_POINT('Ctrl Pts',(-10.2484470900001,15.2,1.61891843999999));
#256702=CARTESIAN_POINT('Ctrl Pts',(-10.2484470900001,11.6,1.61891843999999));
#256703=CARTESIAN_POINT('Ctrl Pts',(-10.2481027040001,15.2,1.61883308499998));
#256704=CARTESIAN_POINT('Ctrl Pts',(-10.2481027040001,11.6,1.61883308499998));
#256705=CARTESIAN_POINT('Ctrl Pts',(-10.2479334570001,15.2,1.61879117999999));
#256706=CARTESIAN_POINT('Ctrl Pts',(-10.2479334570001,11.6,1.61879117999999));
#256707=CARTESIAN_POINT('',(-10.2479334563364,12.2,1.61879117933379));
#256708=CARTESIAN_POINT('',(-10.2479334563364,15.2,1.61879117933379));
#256709=CARTESIAN_POINT('',(-10.2479334560001,12.2,1.61879117899999));
#256710=CARTESIAN_POINT('Ctrl Pts',(-11.2922242990001,12.2,2.17615954699998));
#256711=CARTESIAN_POINT('Ctrl Pts',(-11.288148224556,12.2,2.17309893949932));
#256712=CARTESIAN_POINT('Ctrl Pts',(-11.2840769420896,12.2,2.17005151815676));
#256713=CARTESIAN_POINT('Ctrl Pts',(-11.2800104648685,12.2,2.16701730343719));
#256714=CARTESIAN_POINT('Ctrl Pts',(-11.2769606072297,12.2,2.16474164260421));
#256715=CARTESIAN_POINT('Ctrl Pts',(-11.2739134517022,12.2,2.16247340717588));
#256716=CARTESIAN_POINT('Ctrl Pts',(-11.2708690254527,12.2,2.16021259706259));
#256717=CARTESIAN_POINT('Ctrl Pts',(-11.2678245992032,12.2,2.1579517869493));
#256718=CARTESIAN_POINT('Ctrl Pts',(-11.2647829043248,12.2,2.15569840142299));
#256719=CARTESIAN_POINT('Ctrl Pts',(-11.2617439868938,12.2,2.15345243900525));
#256720=CARTESIAN_POINT('Ctrl Pts',(-11.2587050694628,12.2,2.15120647658751));
#256721=CARTESIAN_POINT('Ctrl Pts',(-11.2556689314065,12.2,2.14896793818554));
#256722=CARTESIAN_POINT('Ctrl Pts',(-11.2526356197667,12.2,2.14673682076659));
#256723=CARTESIAN_POINT('Ctrl Pts',(-11.2496023081269,12.2,2.14450570334765));
#256724=CARTESIAN_POINT('Ctrl Pts',(-11.246571822237,12.2,2.14228200686175));
#256725=CARTESIAN_POINT('Ctrl Pts',(-11.2435441985551,12.2,2.14006573144163));
#256726=CARTESIAN_POINT('Ctrl Pts',(-11.2405165748732,12.2,2.1378494560215));
#256727=CARTESIAN_POINT('Ctrl Pts',(-11.2374918133929,12.2,2.13564060199011));
#256728=CARTESIAN_POINT('Ctrl Pts',(-11.2344699531014,12.2,2.1334391659176));
#256729=CARTESIAN_POINT('Ctrl Pts',(-11.2314480928099,12.2,2.13123772984508));
#256730=CARTESIAN_POINT('Ctrl Pts',(-11.2284291334317,12.2,2.12904371214819));
#256731=CARTESIAN_POINT('Ctrl Pts',(-11.2254131178325,12.2,2.12685711172662));
#256732=CARTESIAN_POINT('Ctrl Pts',(-11.2223971016855,12.2,2.12467051090782));
#256733=CARTESIAN_POINT('Ctrl Pts',(-11.2193840292809,12.2,2.12249132810778));
#256734=CARTESIAN_POINT('Ctrl Pts',(-11.2163739430938,12.2,2.12031956029316));
#256735=CARTESIAN_POINT('Ctrl Pts',(-11.2133638574536,12.2,2.11814779287309));
#256736=CARTESIAN_POINT('Ctrl Pts',(-11.2103567585799,12.2,2.1159834411526));
#256737=CARTESIAN_POINT('Ctrl Pts',(-11.2073526859393,12.2,2.11382650227328));
#256738=CARTESIAN_POINT('Ctrl Pts',(-11.2033472559338,12.2,2.11095058389815));
#256739=CARTESIAN_POINT('Ctrl Pts',(-11.1993472054199,12.2,2.10808784600184));
#256740=CARTESIAN_POINT('Ctrl Pts',(-11.1953526345464,12.2,2.10523828264682));
#256741=CARTESIAN_POINT('Ctrl Pts',(-11.1923567062552,12.2,2.1031011100335));
#256742=CARTESIAN_POINT('Ctrl Pts',(-11.1893638596936,12.2,2.10097134800317));
#256743=CARTESIAN_POINT('Ctrl Pts',(-11.1863741376351,12.2,2.09884899499594));
#256744=CARTESIAN_POINT('Ctrl Pts',(-11.1833844150335,12.2,2.09672664160315));
#256745=CARTESIAN_POINT('Ctrl Pts',(-11.1803978179162,12.2,2.09461169692912));
#256746=CARTESIAN_POINT('Ctrl Pts',(-11.1774143863163,12.2,2.09250415858217));
#256747=CARTESIAN_POINT('Ctrl Pts',(-11.1744309552585,12.2,2.09039662061809));
#256748=CARTESIAN_POINT('Ctrl Pts',(-11.1714506910338,12.2,2.08829648901194));
#256749=CARTESIAN_POINT('Ctrl Pts',(-11.1684736354339,12.2,2.08620376154695));
#256750=CARTESIAN_POINT('Ctrl Pts',(-11.165496579834,12.2,2.08411103408196));
#256751=CARTESIAN_POINT('Ctrl Pts',(-11.1625227333362,12.2,2.08202571079862));
#256752=CARTESIAN_POINT('Ctrl Pts',(-11.159552137764,12.2,2.07994778928138));
#256753=CARTESIAN_POINT('Ctrl Pts',(-11.1565815421918,12.2,2.07786986776415));
#256754=CARTESIAN_POINT('Ctrl Pts',(-11.1536141978418,12.2,2.07579934706958));
#256755=CARTESIAN_POINT('Ctrl Pts',(-11.1506501482277,12.2,2.07373622601015));
#256756=CARTESIAN_POINT('Ctrl Pts',(-11.1476860986136,12.2,2.07167310495071));
#256757=CARTESIAN_POINT('Ctrl Pts',(-11.1447253432153,12.2,2.06961738211622));
#256758=CARTESIAN_POINT('Ctrl Pts',(-11.1417679255724,12.2,2.06756905652332));
#256759=CARTESIAN_POINT('Ctrl Pts',(-11.1388105079296,12.2,2.06552073093042));
#256760=CARTESIAN_POINT('Ctrl Pts',(-11.1358564272366,12.2,2.06347980013705));
#256761=CARTESIAN_POINT('Ctrl Pts',(-11.132905727135,12.2,2.06144626370992));
#256762=CARTESIAN_POINT('Ctrl Pts',(-11.1299550264973,12.2,2.05941272691336));
#256763=CARTESIAN_POINT('Ctrl Pts',(-11.1270077067523,12.2,2.05738658531891));
#256764=CARTESIAN_POINT('Ctrl Pts',(-11.1240638106583,12.2,2.05536783206819));
#256765=CARTESIAN_POINT('Ctrl Pts',(-11.1201386167575,12.2,2.05267616167846));
#256766=CARTESIAN_POINT('Ctrl Pts',(-11.1162195093366,12.2,2.04999763011203));
#256767=CARTESIAN_POINT('Ctrl Pts',(-11.112306594045,12.2,2.04733223021796));
#256768=CARTESIAN_POINT('Ctrl Pts',(-11.109371907443,12.2,2.04533318020661));
#256769=CARTESIAN_POINT('Ctrl Pts',(-11.1064407044901,12.2,2.0433415163118));
#256770=CARTESIAN_POINT('Ctrl Pts',(-11.1035130258665,12.2,2.04135723565891));
#256771=CARTESIAN_POINT('Ctrl Pts',(-11.1005853472429,12.2,2.03937295500603));
#256772=CARTESIAN_POINT('Ctrl Pts',(-11.0976611954311,12.2,2.03739605664207));
#256773=CARTESIAN_POINT('Ctrl Pts',(-11.0947406148701,12.2,2.03542653821263));
#256774=CARTESIAN_POINT('Ctrl Pts',(-11.0918200337784,12.2,2.03345701942538));
#256775=CARTESIAN_POINT('Ctrl Pts',(-11.0889030234212,12.2,2.03149488109023));
#256776=CARTESIAN_POINT('Ctrl Pts',(-11.0859896278733,12.2,2.02954011826547));
#256777=CARTESIAN_POINT('Ctrl Pts',(-11.0830762328546,12.2,2.02758535579584));
#256778=CARTESIAN_POINT('Ctrl Pts',(-11.0801664537774,12.2,2.02563796965079));
#256779=CARTESIAN_POINT('Ctrl Pts',(-11.077260334675,12.2,2.02369795609693));
#256780=CARTESIAN_POINT('Ctrl Pts',(-11.0743542155726,12.2,2.02175794254307));
#256781=CARTESIAN_POINT('Ctrl Pts',(-11.0714517553386,12.2,2.01982530095362));
#256782=CARTESIAN_POINT('Ctrl Pts',(-11.0685530007224,12.2,2.01790002801485));
#256783=CARTESIAN_POINT('Ctrl Pts',(-11.064687994743,12.2,2.01533299754641));
#256784=CARTESIAN_POINT('Ctrl Pts',(-11.0608295742239,12.2,2.01277906790344));
#256785=CARTESIAN_POINT('Ctrl Pts',(-11.0569778483715,12.2,2.01023822866536));
#256786=CARTESIAN_POINT('Ctrl Pts',(-11.0540890533261,12.2,2.00833259880407));
#256787=CARTESIAN_POINT('Ctrl Pts',(-11.0512040246068,12.2,2.00643433217819));
#256788=CARTESIAN_POINT('Ctrl Pts',(-11.0483228056053,12.2,2.00454342532106));
#256789=CARTESIAN_POINT('Ctrl Pts',(-11.0454415871271,12.2,2.00265251880743));
#256790=CARTESIAN_POINT('Ctrl Pts',(-11.0425641802321,12.2,2.0007689719934));
#256791=CARTESIAN_POINT('Ctrl Pts',(-11.0396906292119,12.2,1.99889277956221));
#256792=CARTESIAN_POINT('Ctrl Pts',(-11.0368170781916,12.2,1.99701658713102));
#256793=CARTESIAN_POINT('Ctrl Pts',(-11.0339473836063,12.2,1.99514775047236));
#256794=CARTESIAN_POINT('Ctrl Pts',(-11.0310815924891,12.2,1.99328626444825));
#256795=CARTESIAN_POINT('Ctrl Pts',(-11.0282158013719,12.2,1.99142477842413));
#256796=CARTESIAN_POINT('Ctrl Pts',(-11.0253539118618,12.2,1.98957064284293));
#256797=CARTESIAN_POINT('Ctrl Pts',(-11.0224959722443,12.2,1.98772385427662));
#256798=CARTESIAN_POINT('Ctrl Pts',(-11.0196380326268,12.2,1.98587706571031));
#256799=CARTESIAN_POINT('Ctrl Pts',(-11.0167840410575,12.2,1.98403762348383));
#256800=CARTESIAN_POINT('Ctrl Pts',(-11.0139340455357,12.2,1.98220552292476));
#256801=CARTESIAN_POINT('Ctrl Pts',(-11.0110840500139,12.2,1.98037342236568));
#256802=CARTESIAN_POINT('Ctrl Pts',(-11.0082380505669,12.2,1.97854866256446));
#256803=CARTESIAN_POINT('Ctrl Pts',(-11.0053960925862,12.2,1.97673124137947));
#256804=CARTESIAN_POINT('Ctrl Pts',(-11.0016068149345,12.2,1.97430801291271));
#256805=CARTESIAN_POINT('Ctrl Pts',(-10.9978247251842,12.2,1.97189782577868));
#256806=CARTESIAN_POINT('Ctrl Pts',(-10.9940499322391,12.2,1.96950067274831));
#256807=CARTESIAN_POINT('Ctrl Pts',(-10.9912188377875,12.2,1.96770280813883));
#256808=CARTESIAN_POINT('Ctrl Pts',(-10.9883918487295,12.2,1.9659122732949));
#256809=CARTESIAN_POINT('Ctrl Pts',(-10.9855690122359,12.2,1.96412906376822));
#256810=CARTESIAN_POINT('Ctrl Pts',(-10.9808642845756,12.2,1.96115704778245));
#256811=CARTESIAN_POINT('Ctrl Pts',(-10.9761710913778,12.2,1.95820538052215));
#256812=CARTESIAN_POINT('Ctrl Pts',(-10.9714896552667,12.2,1.95527403704994));
#256813=CARTESIAN_POINT('Ctrl Pts',(-10.9677445061737,12.2,1.95292896214436));
#256814=CARTESIAN_POINT('Ctrl Pts',(-10.9640068804816,12.2,1.95059689372084));
#256815=CARTESIAN_POINT('Ctrl Pts',(-10.9602768933902,12.2,1.94827782009577));
#256816=CARTESIAN_POINT('Ctrl Pts',(-10.956546906807,12.2,1.94595874678669));
#256817=CARTESIAN_POINT('Ctrl Pts',(-10.9528245569269,12.2,1.9436526678134));
#256818=CARTESIAN_POINT('Ctrl Pts',(-10.9491099617692,12.2,1.94135956976817));
#256819=CARTESIAN_POINT('Ctrl Pts',(-10.9453953661054,12.2,1.9390664714105));
#256820=CARTESIAN_POINT('Ctrl Pts',(-10.9416885241238,12.2,1.9367863525904));
#256821=CARTESIAN_POINT('Ctrl Pts',(-10.9379895511452,12.2,1.93451920157926));
#256822=CARTESIAN_POINT('Ctrl Pts',(-10.9342905786707,12.2,1.93225205087702));
#256823=CARTESIAN_POINT('Ctrl Pts',(-10.9305994763479,12.2,1.92999786564257));
#256824=CARTESIAN_POINT('Ctrl Pts',(-10.9269163592595,12.2,1.92775663365828));
#256825=CARTESIAN_POINT('Ctrl Pts',(-10.9232332416694,12.2,1.92551540136861));
#256826=CARTESIAN_POINT('Ctrl Pts',(-10.9195581105475,12.2,1.92328712034772));
#256827=CARTESIAN_POINT('Ctrl Pts',(-10.915891083443,12.2,1.92107177789522));
#256828=CARTESIAN_POINT('Ctrl Pts',(-10.912224056838,12.2,1.91885643574456));
#256829=CARTESIAN_POINT('Ctrl Pts',(-10.9085651348257,12.2,1.91665403099813));
#256830=CARTESIAN_POINT('Ctrl Pts',(-10.9049144362902,12.2,1.91446454645404));
#256831=CARTESIAN_POINT('Ctrl Pts',(-10.9012637372574,12.2,1.91227506161164));
#256832=CARTESIAN_POINT('Ctrl Pts',(-10.8976212607477,12.2,1.91009849932637));
#256833=CARTESIAN_POINT('Ctrl Pts',(-10.8939871264947,12.2,1.90793484359818));
#256834=CARTESIAN_POINT('Ctrl Pts',(-10.8903529927368,12.2,1.90577118816479));
#256835=CARTESIAN_POINT('Ctrl Pts',(-10.8867272019107,12.2,1.90362043739894));
#256836=CARTESIAN_POINT('Ctrl Pts',(-10.883109874025,12.2,1.90148257657689));
#256837=CARTESIAN_POINT('Ctrl Pts',(-10.8794925456464,12.2,1.89934471546356));
#256838=CARTESIAN_POINT('Ctrl Pts',(-10.8758836817098,12.2,1.89721974375));
#256839=CARTESIAN_POINT('Ctrl Pts',(-10.8722834026808,12.2,1.89510764413572));
#256840=CARTESIAN_POINT('Ctrl Pts',(-10.8686831241423,12.2,1.89299554480923));
#256841=CARTESIAN_POINT('Ctrl Pts',(-10.86509142983,12.2,1.89089631741071));
#256842=CARTESIAN_POINT('Ctrl Pts',(-10.8615084435108,12.2,1.88880994535773));
#256843=CARTESIAN_POINT('Ctrl Pts',(-10.8579254567035,12.2,1.88672357302047));
#256844=CARTESIAN_POINT('Ctrl Pts',(-10.854351178372,12.2,1.88465005566183));
#256845=CARTESIAN_POINT('Ctrl Pts',(-10.8507857307726,12.2,1.88258937470686));
#256846=CARTESIAN_POINT('Ctrl Pts',(-10.8463289215163,12.2,1.88001352365354));
#256847=CARTESIAN_POINT('Ctrl Pts',(-10.8418859114319,12.2,1.87745772979982));
#256848=CARTESIAN_POINT('Ctrl Pts',(-10.8374569440021,12.2,1.87492195709255));
#256849=CARTESIAN_POINT('Ctrl Pts',(-10.8339137703479,12.2,1.87289333909257));
#256850=CARTESIAN_POINT('Ctrl Pts',(-10.8303795850586,12.2,1.87087753549001));
#256851=CARTESIAN_POINT('Ctrl Pts',(-10.826854512068,12.2,1.8688745248191));
#256852=CARTESIAN_POINT('Ctrl Pts',(-10.8233294385972,12.2,1.86687151387529));
#256853=CARTESIAN_POINT('Ctrl Pts',(-10.8198134797272,12.2,1.86488129701604));
#256854=CARTESIAN_POINT('Ctrl Pts',(-10.8163067602584,12.2,1.8629038547416));
#256855=CARTESIAN_POINT('Ctrl Pts',(-10.8128000407895,12.2,1.86092641246716));
#256856=CARTESIAN_POINT('Ctrl Pts',(-10.8093025624355,12.2,1.85896174480533));
#256857=CARTESIAN_POINT('Ctrl Pts',(-10.8058144529131,12.2,1.85700983042247));
#256858=CARTESIAN_POINT('Ctrl Pts',(-10.8023263438658,12.2,1.85505791630556));
#256859=CARTESIAN_POINT('Ctrl Pts',(-10.7988476032401,12.2,1.85311875575534));
#256860=CARTESIAN_POINT('Ctrl Pts',(-10.7953783602857,12.2,1.85119232829292));
#256861=CARTESIAN_POINT('Ctrl Pts',(-10.7910418062382,12.2,1.84878429376803));
#256862=CARTESIAN_POINT('Ctrl Pts',(-10.7867200937389,12.2,1.84639615449994));
#256863=CARTESIAN_POINT('Ctrl Pts',(-10.7824134763083,12.2,1.8440278667916));
#256864=CARTESIAN_POINT('Ctrl Pts',(-10.7789681821761,12.2,1.84213323652166));
#256865=CARTESIAN_POINT('Ctrl Pts',(-10.7755325486423,12.2,1.84025131212824));
#256866=CARTESIAN_POINT('Ctrl Pts',(-10.7721067084566,12.2,1.83838207169433));
#256867=CARTESIAN_POINT('Ctrl Pts',(-10.7686808687376,12.2,1.8365128315151));
#256868=CARTESIAN_POINT('Ctrl Pts',(-10.7652648222977,12.2,1.83465627335054));
#256869=CARTESIAN_POINT('Ctrl Pts',(-10.7618587007273,12.2,1.83281237599286));
#256870=CARTESIAN_POINT('Ctrl Pts',(-10.7584525786929,12.2,1.83096847838395));
#256871=CARTESIAN_POINT('Ctrl Pts',(-10.7550563838744,12.2,1.8291372410532));
#256872=CARTESIAN_POINT('Ctrl Pts',(-10.7516702479131,12.2,1.8273186406776));
#256873=CARTESIAN_POINT('Ctrl Pts',(-10.7482841124131,12.2,1.82550004054978));
#256874=CARTESIAN_POINT('Ctrl Pts',(-10.744908038873,12.2,1.82369407782311));
#256875=CARTESIAN_POINT('Ctrl Pts',(-10.7415421592586,12.2,1.82190072641333));
#256876=CARTESIAN_POINT('Ctrl Pts',(-10.7381762791856,12.2,1.82010737475919));
#256877=CARTESIAN_POINT('Ctrl Pts',(-10.7348205957021,12.2,1.81832663631315));
#256878=CARTESIAN_POINT('Ctrl Pts',(-10.731475242798,12.2,1.8165584851851));
#256879=CARTESIAN_POINT('Ctrl Pts',(-10.7281298903497,12.2,1.81479033429797));
#256880=CARTESIAN_POINT('Ctrl Pts',(-10.7247948705591,12.2,1.8130347697981));
#256881=CARTESIAN_POINT('Ctrl Pts',(-10.7214703203302,12.2,1.81129176888421));
#256882=CARTESIAN_POINT('Ctrl Pts',(-10.7181457696483,12.2,1.80954876773283));
#256883=CARTESIAN_POINT('Ctrl Pts',(-10.7148316892511,12.2,1.8078183278052));
#256884=CARTESIAN_POINT('Ctrl Pts',(-10.7115282172384,12.2,1.80610042410129));
#256885=CARTESIAN_POINT('Ctrl Pts',(-10.7082247456758,12.2,1.80438252063144));
#256886=CARTESIAN_POINT('Ctrl Pts',(-10.7049318838535,12.2,1.80267715266237));
#256887=CARTESIAN_POINT('Ctrl Pts',(-10.7016497702347,12.2,1.80098429377065));
#256888=CARTESIAN_POINT('Ctrl Pts',(-10.6983676561686,12.2,1.79929143464827));
#256889=CARTESIAN_POINT('Ctrl Pts',(-10.6950962930856,12.2,1.79761108425657));
#256890=CARTESIAN_POINT('Ctrl Pts',(-10.6918358197419,12.2,1.79594321588871));
#256891=CARTESIAN_POINT('Ctrl Pts',(-10.6885753468425,12.2,1.79427534774809));
#256892=CARTESIAN_POINT('Ctrl Pts',(-10.6853257655437,12.2,1.79261996002721));
#256893=CARTESIAN_POINT('Ctrl Pts',(-10.6820872180295,12.2,1.79097702699356));
#256894=CARTESIAN_POINT('Ctrl Pts',(-10.6788486700741,12.2,1.78933409373607));
#256895=CARTESIAN_POINT('Ctrl Pts',(-10.6756211575154,12.2,1.78770361239432));
#256896=CARTESIAN_POINT('Ctrl Pts',(-10.6724048222145,12.2,1.78608555596551));
#256897=CARTESIAN_POINT('Ctrl Pts',(-10.6691884873518,12.2,1.78446749975716));
#256898=CARTESIAN_POINT('Ctrl Pts',(-10.6659833306206,12.2,1.78286186684534));
#256899=CARTESIAN_POINT('Ctrl Pts',(-10.6627894990472,12.2,1.7812686292521));
#256900=CARTESIAN_POINT('Ctrl Pts',(-10.6595956670386,12.2,1.77967539144178));
#256901=CARTESIAN_POINT('Ctrl Pts',(-10.6564131598367,12.2,1.77809454808542));
#256902=CARTESIAN_POINT('Ctrl Pts',(-10.653242123275,12.2,1.77652606899993));
#256903=CARTESIAN_POINT('Ctrl Pts',(-10.6500710867133,12.2,1.77495758991445));
#256904=CARTESIAN_POINT('Ctrl Pts',(-10.6469115219807,12.2,1.77340147336653));
#256905=CARTESIAN_POINT('Ctrl Pts',(-10.643763577977,12.2,1.77185769100587));
#256906=CARTESIAN_POINT('Ctrl Pts',(-10.6406156344022,12.2,1.77031390885555));
#256907=CARTESIAN_POINT('Ctrl Pts',(-10.6374793102082,12.2,1.76878245902262));
#256908=CARTESIAN_POINT('Ctrl Pts',(-10.6343547567271,12.2,1.76726331125097));
#256909=CARTESIAN_POINT('Ctrl Pts',(-10.6312302028204,12.2,1.76574416327235));
#256910=CARTESIAN_POINT('Ctrl Pts',(-10.6281174206275,12.2,1.76423731434967));
#256911=CARTESIAN_POINT('Ctrl Pts',(-10.6250165594597,12.2,1.76274273521391));
#256912=CARTESIAN_POINT('Ctrl Pts',(-10.6219156987144,12.2,1.76124815628179));
#256913=CARTESIAN_POINT('Ctrl Pts',(-10.6188267599592,12.2,1.75976584533418));
#256914=CARTESIAN_POINT('Ctrl Pts',(-10.6157498970433,12.2,1.75829576912023));
#256915=CARTESIAN_POINT('Ctrl Pts',(-10.6126730337082,12.2,1.75682569270598));
#256916=CARTESIAN_POINT('Ctrl Pts',(-10.609608245111,12.2,1.75536785109296));
#256917=CARTESIAN_POINT('Ctrl Pts',(-10.6065556865155,12.2,1.7539222093319));
#256918=CARTESIAN_POINT('Ctrl Pts',(-10.6035031283358,12.2,1.75247656776782));
#256919=CARTESIAN_POINT('Ctrl Pts',(-10.6004628009815,12.2,1.75104312744808));
#256920=CARTESIAN_POINT('Ctrl Pts',(-10.597434859506,12.2,1.74962185184124));
#256921=CARTESIAN_POINT('Ctrl Pts',(-10.5928929466739,12.2,1.74748993814051));
#256922=CARTESIAN_POINT('Ctrl Pts',(-10.588378903462,12.2,1.74538539612655));
#256923=CARTESIAN_POINT('Ctrl Pts',(-10.5838932628027,12.2,1.74330810526518));
#256924=CARTESIAN_POINT('Ctrl Pts',(-10.5801552295312,12.2,1.74157702983041));
#256925=CARTESIAN_POINT('Ctrl Pts',(-10.5764369226267,12.2,1.73986487718285));
#256926=CARTESIAN_POINT('Ctrl Pts',(-10.5727386527504,12.2,1.73817157521309));
#256927=CARTESIAN_POINT('Ctrl Pts',(-10.569040382471,12.2,1.73647827305876));
#256928=CARTESIAN_POINT('Ctrl Pts',(-10.5653621528857,12.2,1.7348038211847));
#256929=CARTESIAN_POINT('Ctrl Pts',(-10.5617042777451,12.2,1.73314814493317));
#256930=CARTESIAN_POINT('Ctrl Pts',(-10.5580464026046,12.2,1.73149246868164));
#256931=CARTESIAN_POINT('Ctrl Pts',(-10.5544088858359,12.2,1.72985556749646));
#256932=CARTESIAN_POINT('Ctrl Pts',(-10.5507920472231,12.2,1.72823736520327));
#256933=CARTESIAN_POINT('Ctrl Pts',(-10.5471752086103,12.2,1.72661916291008));
#256934=CARTESIAN_POINT('Ctrl Pts',(-10.543579050384,12.2,1.72501965880824));
#256935=CARTESIAN_POINT('Ctrl Pts',(-10.5400038958984,12.2,1.72343877240852));
#256936=CARTESIAN_POINT('Ctrl Pts',(-10.5364287414128,12.2,1.72185788600881));
#256937=CARTESIAN_POINT('Ctrl Pts',(-10.5328745943267,12.2,1.72029561860198));
#256938=CARTESIAN_POINT('Ctrl Pts',(-10.5293417840478,12.2,1.71875188735101));
#256939=CARTESIAN_POINT('Ctrl Pts',(-10.525808973769,12.2,1.71720815610005));
#256940=CARTESIAN_POINT('Ctrl Pts',(-10.5222975002351,12.2,1.71568296326067));
#256941=CARTESIAN_POINT('Ctrl Pts',(-10.51880770072,12.2,1.71417622110692));
#256942=CARTESIAN_POINT('Ctrl Pts',(-10.515317901205,12.2,1.71266947895318));
#256943=CARTESIAN_POINT('Ctrl Pts',(-10.5118497737009,12.2,1.71118118890747));
#256944=CARTESIAN_POINT('Ctrl Pts',(-10.5084036609769,12.2,1.70971126577574));
#256945=CARTESIAN_POINT('Ctrl Pts',(-10.5049575482528,12.2,1.70824134264402));
#256946=CARTESIAN_POINT('Ctrl Pts',(-10.5015334497333,12.2,1.70678978567216));
#256947=CARTESIAN_POINT('Ctrl Pts',(-10.4981317097333,12.2,1.70535650428327));
#256948=CARTESIAN_POINT('Ctrl Pts',(-10.4947299697333,12.2,1.70392322289439));
#256949=CARTESIAN_POINT('Ctrl Pts',(-10.4913505917578,12.2,1.70250821758881));
#256950=CARTESIAN_POINT('Ctrl Pts',(-10.4879939225065,12.2,1.70111139779085));
#256951=CARTESIAN_POINT('Ctrl Pts',(-10.4846372532552,12.2,1.69971457799288));
#256952=CARTESIAN_POINT('Ctrl Pts',(-10.4813032944324,12.2,1.6983359434379));
#256953=CARTESIAN_POINT('Ctrl Pts',(-10.4779924025586,12.2,1.69697539941107));
#256954=CARTESIAN_POINT('Ctrl Pts',(-10.4746815106848,12.2,1.69561485538424));
#256955=CARTESIAN_POINT('Ctrl Pts',(-10.471393684391,12.2,1.69427240205694));
#256956=CARTESIAN_POINT('Ctrl Pts',(-10.4681292867533,12.2,1.69294794219676));
#256957=CARTESIAN_POINT('Ctrl Pts',(-10.4648648891156,12.2,1.69162348233659));
#256958=CARTESIAN_POINT('Ctrl Pts',(-10.4616239186746,12.2,1.69031701576354));
#256959=CARTESIAN_POINT('Ctrl Pts',(-10.4584067433766,12.2,1.68902844257542));
#256960=CARTESIAN_POINT('Ctrl Pts',(-10.4551895680787,12.2,1.68773986938729));
#256961=CARTESIAN_POINT('Ctrl Pts',(-10.4519961881502,12.2,1.68646919123461));
#256962=CARTESIAN_POINT('Ctrl Pts',(-10.4488269748188,12.2,1.68521630311107));
#256963=CARTESIAN_POINT('Ctrl Pts',(-10.4456577614874,12.2,1.68396341498752));
#256964=CARTESIAN_POINT('Ctrl Pts',(-10.4425127162509,12.2,1.68272831855038));
#256965=CARTESIAN_POINT('Ctrl Pts',(-10.4393922155585,12.2,1.68151090785737));
#256966=CARTESIAN_POINT('Ctrl Pts',(-10.4356476148636,12.2,1.68005001507885));
#256967=CARTESIAN_POINT('Ctrl Pts',(-10.4319383614733,12.2,1.6786145889792));
#256968=CARTESIAN_POINT('Ctrl Pts',(-10.4282651168583,12.2,1.6772044439482));
#256969=CARTESIAN_POINT('Ctrl Pts',(-10.4245918722433,12.2,1.67579429891719));
#256970=CARTESIAN_POINT('Ctrl Pts',(-10.4209546380505,12.2,1.67440943047585));
#256971=CARTESIAN_POINT('Ctrl Pts',(-10.4173540951797,12.2,1.67304964952415));
#256972=CARTESIAN_POINT('Ctrl Pts',(-10.4137535523089,12.2,1.67168986857245));
#256973=CARTESIAN_POINT('Ctrl Pts',(-10.4101896957755,12.2,1.67035517200516));
#256974=CARTESIAN_POINT('Ctrl Pts',(-10.4066632229011,12.2,1.66904535913438));
#256975=CARTESIAN_POINT('Ctrl Pts',(-10.4031367497063,12.2,1.66773554614464));
#256976=CARTESIAN_POINT('Ctrl Pts',(-10.3996476556151,12.2,1.6664506182323));
#256977=CARTESIAN_POINT('Ctrl Pts',(-10.3961966495954,12.2,1.66519036616469));
#256978=CARTESIAN_POINT('Ctrl Pts',(-10.3927456438891,12.2,1.66393011421156));
#256979=CARTESIAN_POINT('Ctrl Pts',(-10.389332722886,12.2,1.66269453712038));
#256980=CARTESIAN_POINT('Ctrl Pts',(-10.3859586112432,12.2,1.66148342124216));
#256981=CARTESIAN_POINT('Ctrl Pts',(-10.3825844996004,12.2,1.66027230536394));
#256982=CARTESIAN_POINT('Ctrl Pts',(-10.3792491944922,12.2,1.65908565032773));
#256983=CARTESIAN_POINT('Ctrl Pts',(-10.3759534311092,12.2,1.65792323511832));
#256984=CARTESIAN_POINT('Ctrl Pts',(-10.3726576674269,12.2,1.65676081980332));
#256985=CARTESIAN_POINT('Ctrl Pts',(-10.3694014467392,12.2,1.65562264058221));
#256986=CARTESIAN_POINT('Ctrl Pts',(-10.3661855189056,12.2,1.65450847138389));
#256987=CARTESIAN_POINT('Ctrl Pts',(-10.3629695913642,12.2,1.65339430228676));
#256988=CARTESIAN_POINT('Ctrl Pts',(-10.3597939584194,12.2,1.65230414139452));
#256989=CARTESIAN_POINT('Ctrl Pts',(-10.3566593852,12.2,1.6512377512666));
#256990=CARTESIAN_POINT('Ctrl Pts',(-10.3535248119805,12.2,1.65017136113868));
#256991=CARTESIAN_POINT('Ctrl Pts',(-10.3504312997662,12.2,1.64912874083394));
#256992=CARTESIAN_POINT('Ctrl Pts',(-10.3473796326243,12.2,1.64810964478603));
#256993=CARTESIAN_POINT('Ctrl Pts',(-10.3443279652051,12.2,1.64709054864556));
#256994=CARTESIAN_POINT('Ctrl Pts',(-10.3413181436622,12.2,1.64609497698116));
#256995=CARTESIAN_POINT('Ctrl Pts',(-10.3383509672714,12.2,1.64512267463094));
#256996=CARTESIAN_POINT('Ctrl Pts',(-10.3353837911501,12.2,1.64415037236905));
#256997=CARTESIAN_POINT('Ctrl Pts',(-10.3324592641453,12.2,1.6432013387413));
#256998=CARTESIAN_POINT('Ctrl Pts',(-10.32957820325,12.2,1.64227531152494));
#256999=CARTESIAN_POINT('Ctrl Pts',(-10.3266971423546,12.2,1.64134928430858));
#257000=CARTESIAN_POINT('Ctrl Pts',(-10.3238595497276,12.2,1.6404462632318));
#257001=CARTESIAN_POINT('Ctrl Pts',(-10.3210662645203,12.2,1.63956597488516));
#257002=CARTESIAN_POINT('Ctrl Pts',(-10.3182729790593,12.2,1.63868568645855));
#257003=CARTESIAN_POINT('Ctrl Pts',(-10.3155239995829,12.2,1.63782813033625));
#257004=CARTESIAN_POINT('Ctrl Pts',(-10.3128201892719,12.2,1.63699302495893));
#257005=CARTESIAN_POINT('Ctrl Pts',(-10.3101163792066,12.2,1.63615791965746));
#257006=CARTESIAN_POINT('Ctrl Pts',(-10.3074577337573,12.2,1.63534526372441));
#257007=CARTESIAN_POINT('Ctrl Pts',(-10.3048451387571,12.2,1.63455476724959));
#257008=CARTESIAN_POINT('Ctrl Pts',(-10.302232543757,12.2,1.63376427077477));
#257009=CARTESIAN_POINT('Ctrl Pts',(-10.299665995598,12.2,1.63299593268122));
#257010=CARTESIAN_POINT('Ctrl Pts',(-10.2971463988542,12.2,1.63224944754072));
#257011=CARTESIAN_POINT('Ctrl Pts',(-10.2946268018815,12.2,1.63150296233242));
#257012=CARTESIAN_POINT('Ctrl Pts',(-10.2921541558229,12.2,1.63077833360183));
#257013=CARTESIAN_POINT('Ctrl Pts',(-10.289729386944,12.2,1.63007524598165));
#257014=CARTESIAN_POINT('Ctrl Pts',(-10.2873046182854,12.2,1.62937215842533));
#257015=CARTESIAN_POINT('Ctrl Pts',(-10.2849277259532,12.2,1.6286906116558));
#257016=CARTESIAN_POINT('Ctrl Pts',(-10.2825996603733,12.2,1.62803028118072));
#257017=CARTESIAN_POINT('Ctrl Pts',(-10.2802715947934,12.2,1.62736995070563));
#257018=CARTESIAN_POINT('Ctrl Pts',(-10.2779923555595,12.2,1.62673083689551));
#257019=CARTESIAN_POINT('Ctrl Pts',(-10.2757629181383,12.2,1.62611260225039));
#257020=CARTESIAN_POINT('Ctrl Pts',(-10.2735334807172,12.2,1.62549436760528));
#257021=CARTESIAN_POINT('Ctrl Pts',(-10.2713538452582,12.2,1.62489701219327));
#257022=CARTESIAN_POINT('Ctrl Pts',(-10.2692250129987,12.2,1.62432018654616));
#257023=CARTESIAN_POINT('Ctrl Pts',(-10.2670961805458,12.2,1.62374336084665));
#257024=CARTESIAN_POINT('Ctrl Pts',(-10.2650181509812,12.2,1.62318706577415));
#257025=CARTESIAN_POINT('Ctrl Pts',(-10.2629919538731,12.2,1.62265093799582));
#257026=CARTESIAN_POINT('Ctrl Pts',(-10.260965756949,12.2,1.62211481026618));
#257027=CARTESIAN_POINT('Ctrl Pts',(-10.2589913939399,12.2,1.62159884971778));
#257028=CARTESIAN_POINT('Ctrl Pts',(-10.2570699210009,12.2,1.62110268273351));
#257029=CARTESIAN_POINT('Ctrl Pts',(-10.2538766876538,12.2,1.62027811896908));
#257030=CARTESIAN_POINT('Ctrl Pts',(-10.2508295201298,12.2,1.61950823569637));
#257031=CARTESIAN_POINT('Ctrl Pts',(-10.2479334570001,12.2,1.61879117999999));
#257032=CARTESIAN_POINT('Ctrl Pts',(-10.2479334570001,15.2,1.61879117999999));
#257033=CARTESIAN_POINT('Ctrl Pts',(-10.249667749424,15.2,1.61922058509445));
#257034=CARTESIAN_POINT('Ctrl Pts',(-10.2514562330726,15.2,1.61966892566345));
#257035=CARTESIAN_POINT('Ctrl Pts',(-10.2532978200233,15.2,1.6201366211404));
#257036=CARTESIAN_POINT('Ctrl Pts',(-10.2551482880371,15.2,1.62060657208134));
#257037=CARTESIAN_POINT('Ctrl Pts',(-10.257052368982,15.2,1.62109605778657));
#257038=CARTESIAN_POINT('Ctrl Pts',(-10.2590089861894,15.2,1.62160546159094));
#257039=CARTESIAN_POINT('Ctrl Pts',(-10.2609656032191,15.2,1.62211486534904));
#257040=CARTESIAN_POINT('Ctrl Pts',(-10.2629747532248,15.2,1.62264418861991));
#257041=CARTESIAN_POINT('Ctrl Pts',(-10.2650353904833,15.2,1.62319380126661));
#257042=CARTESIAN_POINT('Ctrl Pts',(-10.2670960277418,15.2,1.62374341391331));
#257043=CARTESIAN_POINT('Ctrl Pts',(-10.2692081522727,15.2,1.62431331751935));
#257044=CARTESIAN_POINT('Ctrl Pts',(-10.2713707425492,15.2,1.62490386819287));
#257045=CARTESIAN_POINT('Ctrl Pts',(-10.2735333330222,15.2,1.62549441892003));
#257046=CARTESIAN_POINT('Ctrl Pts',(-10.2757463899782,15.2,1.62610561795797));
#257047=CARTESIAN_POINT('Ctrl Pts',(-10.2780089205216,15.2,1.62673780957719));
#257048=CARTESIAN_POINT('Ctrl Pts',(-10.2806485391806,15.2,1.62747536638016));
#257049=CARTESIAN_POINT('Ctrl Pts',(-10.2833554975187,15.2,1.6282414973953));
#257050=CARTESIAN_POINT('Ctrl Pts',(-10.2861282602868,15.2,1.6290367294674));
#257051=CARTESIAN_POINT('Ctrl Pts',(-10.2885049143657,15.2,1.62971835703736));
#257052=CARTESIAN_POINT('Ctrl Pts',(-10.2909299187482,15.2,1.63042136553797));
#257053=CARTESIAN_POINT('Ctrl Pts',(-10.2934023335528,15.2,1.63114607307894));
#257054=CARTESIAN_POINT('Ctrl Pts',(-10.2958747481328,15.2,1.63187078055409));
#257055=CARTESIAN_POINT('Ctrl Pts',(-10.2983945737993,15.2,1.63261718678302));
#257056=CARTESIAN_POINT('Ctrl Pts',(-10.3009608947178,15.2,1.63338560200863));
#257057=CARTESIAN_POINT('Ctrl Pts',(-10.3035272156363,15.2,1.63415401723425));
#257058=CARTESIAN_POINT('Ctrl Pts',(-10.3061400361122,15.2,1.63494443990291));
#257059=CARTESIAN_POINT('Ctrl Pts',(-10.308798459097,15.2,1.63575716820575));
#257060=CARTESIAN_POINT('Ctrl Pts',(-10.3114568823232,15.2,1.6365698965824));
#257061=CARTESIAN_POINT('Ctrl Pts',(-10.3141609111968,15.2,1.63740492996182));
#257062=CARTESIAN_POINT('Ctrl Pts',(-10.3169096745163,15.2,1.63826255634343));
#257063=CARTESIAN_POINT('Ctrl Pts',(-10.3196584375861,15.2,1.63912018264714));
#257064=CARTESIAN_POINT('Ctrl Pts',(-10.3224519353476,15.2,1.64000040111441));
#257065=CARTESIAN_POINT('Ctrl Pts',(-10.3252893183298,15.2,1.64090349124926));
#257066=CARTESIAN_POINT('Ctrl Pts',(-10.3281267013119,15.2,1.64180658138411));
#257067=CARTESIAN_POINT('Ctrl Pts',(-10.3310079696406,15.2,1.64273254179215));
#257068=CARTESIAN_POINT('Ctrl Pts',(-10.3339322926158,15.2,1.64368164017332));
#257069=CARTESIAN_POINT('Ctrl Pts',(-10.3368566155909,15.2,1.64463073855448));
#257070=CARTESIAN_POINT('Ctrl Pts',(-10.3398239930841,15.2,1.64560297667086));
#257071=CARTESIAN_POINT('Ctrl Pts',(-10.3428336151386,15.2,1.64659861188309));
#257072=CARTESIAN_POINT('Ctrl Pts',(-10.3458432374665,15.2,1.64759424718577));
#257073=CARTESIAN_POINT('Ctrl Pts',(-10.3488951026067,15.2,1.64861328026567));
#257074=CARTESIAN_POINT('Ctrl Pts',(-10.3519884191937,15.2,1.64965596232354));
#257075=CARTESIAN_POINT('Ctrl Pts',(-10.3550817354998,15.2,1.65069864428669));
#257076=CARTESIAN_POINT('Ctrl Pts',(-10.3582165021609,15.2,1.6517649734646));
#257077=CARTESIAN_POINT('Ctrl Pts',(-10.3613919443771,15.2,1.65285519442396));
#257078=CARTESIAN_POINT('Ctrl Pts',(-10.3645673865933,15.2,1.65394541538332));
#257079=CARTESIAN_POINT('Ctrl Pts',(-10.3677835035911,15.2,1.65505952521889));
#257080=CARTESIAN_POINT('Ctrl Pts',(-10.3710395368868,15.2,1.65619776034255));
#257081=CARTESIAN_POINT('Ctrl Pts',(-10.3742955704781,15.2,1.6573359955696));
#257082=CARTESIAN_POINT('Ctrl Pts',(-10.3775915191068,15.2,1.65849835564065));
#257083=CARTESIAN_POINT('Ctrl Pts',(-10.3809266408736,15.2,1.65968506578972));
#257084=CARTESIAN_POINT('Ctrl Pts',(-10.3848176158138,15.2,1.66106956080195));
#257085=CARTESIAN_POINT('Ctrl Pts',(-10.3887619087675,15.2,1.66248720085672));
#257086=CARTESIAN_POINT('Ctrl Pts',(-10.3927583656266,15.2,1.6639383310977));
#257087=CARTESIAN_POINT('Ctrl Pts',(-10.3961839004773,15.2,1.6651821571638));
#257088=CARTESIAN_POINT('Ctrl Pts',(-10.3996477608152,15.2,1.66645058776564));
#257089=CARTESIAN_POINT('Ctrl Pts',(-10.4031492356743,15.2,1.66774383383719));
#257090=CARTESIAN_POINT('Ctrl Pts',(-10.4066507102154,15.2,1.66903707979128));
#257091=CARTESIAN_POINT('Ctrl Pts',(-10.4101897996955,15.2,1.67035514123376));
#257092=CARTESIAN_POINT('Ctrl Pts',(-10.4137658072484,15.2,1.671698221941));
#257093=CARTESIAN_POINT('Ctrl Pts',(-10.4173418148013,15.2,1.67304130264824));
#257094=CARTESIAN_POINT('Ctrl Pts',(-10.4209547402873,15.2,1.67440940080042));
#257095=CARTESIAN_POINT('Ctrl Pts',(-10.4246039011522,15.2,1.67580271658141));
#257096=CARTESIAN_POINT('Ctrl Pts',(-10.4282530623487,15.2,1.67719603248896));
#257097=CARTESIAN_POINT('Ctrl Pts',(-10.4319384591359,15.2,1.67861456248737));
#257098=CARTESIAN_POINT('Ctrl Pts',(-10.43565942236,15.2,1.68005849763969));
#257099=CARTESIAN_POINT('Ctrl Pts',(-10.4387602248778,15.2,1.6812617768677));
#257100=CARTESIAN_POINT('Ctrl Pts',(-10.4418857253989,15.2,1.6824826993383));
#257101=CARTESIAN_POINT('Ctrl Pts',(-10.4450355444287,15.2,1.68372137093697));
#257102=CARTESIAN_POINT('Ctrl Pts',(-10.4481853634584,15.2,1.68496004253563));
#257103=CARTESIAN_POINT('Ctrl Pts',(-10.4513595001386,15.2,1.68621646360405));
#257104=CARTESIAN_POINT('Ctrl Pts',(-10.4545575793766,15.2,1.68749073763329));
#257105=CARTESIAN_POINT('Ctrl Pts',(-10.4577556582661,15.2,1.68876501152363));
#257106=CARTESIAN_POINT('Ctrl Pts',(-10.4609776819034,15.2,1.69005713877285));
#257107=CARTESIAN_POINT('Ctrl Pts',(-10.4642232782838,15.2,1.69136722008692));
#257108=CARTESIAN_POINT('Ctrl Pts',(-10.4681179945771,15.2,1.69293931792085));
#257109=CARTESIAN_POINT('Ctrl Pts',(-10.4720466563404,15.2,1.69453726941559));
#257110=CARTESIAN_POINT('Ctrl Pts',(-10.4760086384744,15.2,1.69616124333856));
#257111=CARTESIAN_POINT('Ctrl Pts',(-10.4793102900728,15.2,1.69751455486727));
#257112=CARTESIAN_POINT('Ctrl Pts',(-10.4826350783087,15.2,1.69888593766284));
#257113=CARTESIAN_POINT('Ctrl Pts',(-10.4859826493804,15.2,1.70027548738631));
#257114=CARTESIAN_POINT('Ctrl Pts',(-10.489330220452,15.2,1.70166503710978));
#257115=CARTESIAN_POINT('Ctrl Pts',(-10.4927005713142,15.2,1.70307275317942));
#257116=CARTESIAN_POINT('Ctrl Pts',(-10.4960933524271,15.2,1.70449872790313));
#257117=CARTESIAN_POINT('Ctrl Pts',(-10.5001646896147,15.2,1.70620989750942));
#257118=CARTESIAN_POINT('Ctrl Pts',(-10.5042683258583,15.2,1.70794735808176));
#257119=CARTESIAN_POINT('Ctrl Pts',(-10.5084036609769,15.2,1.70971126577574));
#257120=CARTESIAN_POINT('Ctrl Pts',(-10.5125389960955,15.2,1.71147517346972));
#257121=CARTESIAN_POINT('Ctrl Pts',(-10.5167060311669,15.2,1.71326553015153));
#257122=CARTESIAN_POINT('Ctrl Pts',(-10.520904178263,15.2,1.71508248091769));
#257123=CARTESIAN_POINT('Ctrl Pts',(-10.5244026343035,15.2,1.71659660661117));
#257124=CARTESIAN_POINT('Ctrl Pts',(-10.5279226954474,15.2,1.71812920202735));
#257125=CARTESIAN_POINT('Ctrl Pts',(-10.5314640274602,15.2,1.71968035091527));
#257126=CARTESIAN_POINT('Ctrl Pts',(-10.5357136257212,15.2,1.72154172951316));
#257127=CARTESIAN_POINT('Ctrl Pts',(-10.5399938549055,15.2,1.72342982533764));
#257128=CARTESIAN_POINT('Ctrl Pts',(-10.5443041412469,15.2,1.72534477701621));
#257129=CARTESIAN_POINT('Ctrl Pts',(-10.5478960466618,15.2,1.72694057013968));
#257130=CARTESIAN_POINT('Ctrl Pts',(-10.5515088274653,15.2,1.72855501449341));
#257131=CARTESIAN_POINT('Ctrl Pts',(-10.5551421577414,15.2,1.73018818831133));
#257132=CARTESIAN_POINT('Ctrl Pts',(-10.5587754880175,15.2,1.73182136212924));
#257133=CARTESIAN_POINT('Ctrl Pts',(-10.5624293680322,15.2,1.73347326436629));
#257134=CARTESIAN_POINT('Ctrl Pts',(-10.5661034767111,15.2,1.73514397248975));
#257135=CARTESIAN_POINT('Ctrl Pts',(-10.5712472289416,15.2,1.737482963899));
#257136=CARTESIAN_POINT('Ctrl Pts',(-10.5764306300097,15.2,1.73985881671164));
#257137=CARTESIAN_POINT('Ctrl Pts',(-10.581652812698,15.2,1.742271730274));
#257138=CARTESIAN_POINT('Ctrl Pts',(-10.5853829431315,15.2,1.74399523993456));
#257139=CARTESIAN_POINT('Ctrl Pts',(-10.5891328619333,15.2,1.74573765824437));
#257140=CARTESIAN_POINT('Ctrl Pts',(-10.5929022565167,15.2,1.74749905775826));
#257141=CARTESIAN_POINT('Ctrl Pts',(-10.5966716511,15.2,1.74926045727215));
#257142=CARTESIAN_POINT('Ctrl Pts',(-10.6004605235403,15.2,1.75104083661492));
#257143=CARTESIAN_POINT('Ctrl Pts',(-10.6042685642521,15.2,1.75284026544259));
#257144=CARTESIAN_POINT('Ctrl Pts',(-10.6073149965725,15.2,1.75427980838704));
#257145=CARTESIAN_POINT('Ctrl Pts',(-10.6103736992141,15.2,1.75573154406763));
#257146=CARTESIAN_POINT('Ctrl Pts',(-10.6134445152396,15.2,1.75719550500225));
#257147=CARTESIAN_POINT('Ctrl Pts',(-10.6172830355853,15.2,1.75902545632013));
#257148=CARTESIAN_POINT('Ctrl Pts',(-10.6211404832112,15.2,1.76087451139604));
#257149=CARTESIAN_POINT('Ctrl Pts',(-10.6250165594597,15.2,1.76274273521391));
#257150=CARTESIAN_POINT('Ctrl Pts',(-10.6281174206274,15.2,1.76423731434966));
#257151=CARTESIAN_POINT('Ctrl Pts',(-10.6312302028204,15.2,1.76574416327235));
#257152=CARTESIAN_POINT('Ctrl Pts',(-10.6343547567271,15.2,1.76726331125097));
#257153=CARTESIAN_POINT('Ctrl Pts',(-10.6374793102082,15.2,1.76878245902261));
#257154=CARTESIAN_POINT('Ctrl Pts',(-10.6406156344022,15.2,1.77031390885556));
#257155=CARTESIAN_POINT('Ctrl Pts',(-10.643763577977,15.2,1.77185769100587));
#257156=CARTESIAN_POINT('Ctrl Pts',(-10.6469115219807,15.2,1.77340147336651));
#257157=CARTESIAN_POINT('Ctrl Pts',(-10.6500710867133,15.2,1.77495758991445));
#257158=CARTESIAN_POINT('Ctrl Pts',(-10.653242123275,15.2,1.77652606899993));
#257159=CARTESIAN_POINT('Ctrl Pts',(-10.6579986776855,15.2,1.77887878741445));
#257160=CARTESIAN_POINT('Ctrl Pts',(-10.662781040646,15.2,1.78125932488582));
#257161=CARTESIAN_POINT('Ctrl Pts',(-10.6675887212933,15.2,1.78366778525035));
#257162=CARTESIAN_POINT('Ctrl Pts',(-10.6723964023774,15.2,1.78607624583364));
#257163=CARTESIAN_POINT('Ctrl Pts',(-10.6772293960964,15.2,1.78851262710733));
#257164=CARTESIAN_POINT('Ctrl Pts',(-10.6820872180295,15.2,1.79097702699357));
#257165=CARTESIAN_POINT('Ctrl Pts',(-10.6861354027532,15.2,1.7930306934535));
#257166=CARTESIAN_POINT('Ctrl Pts',(-10.6902008280438,15.2,1.79510381956652));
#257167=CARTESIAN_POINT('Ctrl Pts',(-10.6942832152673,15.2,1.79719645824866));
#257168=CARTESIAN_POINT('Ctrl Pts',(-10.6983656020459,15.2,1.7992890967027));
#257169=CARTESIAN_POINT('Ctrl Pts',(-10.7024649500561,15.2,1.80140124834397));
#257170=CARTESIAN_POINT('Ctrl Pts',(-10.7065809837033,15.2,1.80353296672111));
#257171=CARTESIAN_POINT('Ctrl Pts',(-10.7098738111594,15.2,1.80523834170165));
#257172=CARTESIAN_POINT('Ctrl Pts',(-10.7131773185027,15.2,1.80695623840007));
#257173=CARTESIAN_POINT('Ctrl Pts',(-10.7164913640167,15.2,1.8086866847166));
#257174=CARTESIAN_POINT('Ctrl Pts',(-10.7198054095306,15.2,1.81041713103312));
#257175=CARTESIAN_POINT('Ctrl Pts',(-10.7231299947236,15.2,1.81216012539557));
#257176=CARTESIAN_POINT('Ctrl Pts',(-10.7264649807953,15.2,1.81391569627031));
#257177=CARTESIAN_POINT('Ctrl Pts',(-10.7306337127033,15.2,1.81611015950494));
#257178=CARTESIAN_POINT('Ctrl Pts',(-10.7348186963209,15.2,1.81832426840286));
#257179=CARTESIAN_POINT('Ctrl Pts',(-10.7390196624589,15.2,1.82055807669943));
#257180=CARTESIAN_POINT('Ctrl Pts',(-10.7432206290548,15.2,1.82279188523947));
#257181=CARTESIAN_POINT('Ctrl Pts',(-10.7474375781921,15.2,1.825045390332));
#257182=CARTESIAN_POINT('Ctrl Pts',(-10.7516702479131,15.2,1.8273186406776));
#257183=CARTESIAN_POINT('Ctrl Pts',(-10.7550563838744,15.2,1.8291372410532));
#257184=CARTESIAN_POINT('Ctrl Pts',(-10.7584525786929,15.2,1.83096847838395));
#257185=CARTESIAN_POINT('Ctrl Pts',(-10.7618587007273,15.2,1.83281237599286));
#257186=CARTESIAN_POINT('Ctrl Pts',(-10.766967883315,15.2,1.83557822215499));
#257187=CARTESIAN_POINT('Ctrl Pts',(-10.7720993974574,15.2,1.83837255355835));
#257188=CARTESIAN_POINT('Ctrl Pts',(-10.7772527972692,15.2,1.84119544787121));
#257189=CARTESIAN_POINT('Ctrl Pts',(-10.7806883974559,15.2,1.84307737758405));
#257190=CARTESIAN_POINT('Ctrl Pts',(-10.7841337237158,15.2,1.84497200279841));
#257191=CARTESIAN_POINT('Ctrl Pts',(-10.7875886470159,15.2,1.84687934318098));
#257192=CARTESIAN_POINT('Ctrl Pts',(-10.7910435698452,15.2,1.84878668330368));
#257193=CARTESIAN_POINT('Ctrl Pts',(-10.7945080870906,15.2,1.85070674124876));
#257194=CARTESIAN_POINT('Ctrl Pts',(-10.7979820709793,15.2,1.85263953618621));
#257195=CARTESIAN_POINT('Ctrl Pts',(-10.8014560553414,15.2,1.85457233138701));
#257196=CARTESIAN_POINT('Ctrl Pts',(-10.8049395044086,15.2,1.85651786550815));
#257197=CARTESIAN_POINT('Ctrl Pts',(-10.808432290544,15.2,1.85847615839348));
#257198=CARTESIAN_POINT('Ctrl Pts',(-10.8119250762035,15.2,1.86043445101199));
#257199=CARTESIAN_POINT('Ctrl Pts',(-10.8154271986306,15.2,1.86240550101407));
#257200=CARTESIAN_POINT('Ctrl Pts',(-10.8189385296759,15.2,1.86438933168391));
#257201=CARTESIAN_POINT('Ctrl Pts',(-10.8224498611997,15.2,1.86637316262406));
#257202=CARTESIAN_POINT('Ctrl Pts',(-10.8259704011216,15.2,1.86836977281543));
#257203=CARTESIAN_POINT('Ctrl Pts',(-10.8295000232584,15.2,1.87037918175827));
#257204=CARTESIAN_POINT('Ctrl Pts',(-10.8339120506889,15.2,1.87289094279992));
#257205=CARTESIAN_POINT('Ctrl Pts',(-10.8383382672322,15.2,1.87542270172858));
#257206=CARTESIAN_POINT('Ctrl Pts',(-10.8427784297524,15.2,1.877974497018));
#257207=CARTESIAN_POINT('Ctrl Pts',(-10.8463305594782,15.2,1.88001593308265));
#257208=CARTESIAN_POINT('Ctrl Pts',(-10.8498916145452,15.2,1.88207019220727));
#257209=CARTESIAN_POINT('Ctrl Pts',(-10.8534614696414,15.2,1.88413729220364));
#257210=CARTESIAN_POINT('Ctrl Pts',(-10.8579237888763,15.2,1.88672116741033));
#257211=CARTESIAN_POINT('Ctrl Pts',(-10.862399858275,15.2,1.88932510699725));
#257212=CARTESIAN_POINT('Ctrl Pts',(-10.8668894375794,15.2,1.89194914644005));
#257213=CARTESIAN_POINT('Ctrl Pts',(-10.8722769330384,15.2,1.89509799394301));
#257214=CARTESIAN_POINT('Ctrl Pts',(-10.8776838814571,15.2,1.89827578490691));
#257215=CARTESIAN_POINT('Ctrl Pts',(-10.883109874025,15.2,1.90148257657689));
#257216=CARTESIAN_POINT('Ctrl Pts',(-10.8867272019107,15.2,1.90362043739893));
#257217=CARTESIAN_POINT('Ctrl Pts',(-10.8903529927368,15.2,1.90577118816479));
#257218=CARTESIAN_POINT('Ctrl Pts',(-10.8939871264947,15.2,1.90793484359818));
#257219=CARTESIAN_POINT('Ctrl Pts',(-10.8976212607477,15.2,1.91009849932637));
#257220=CARTESIAN_POINT('Ctrl Pts',(-10.9012637372574,15.2,1.91227506161165));
#257221=CARTESIAN_POINT('Ctrl Pts',(-10.9049144362902,15.2,1.91446454645405));
#257222=CARTESIAN_POINT('Ctrl Pts',(-10.9085651348257,15.2,1.91665403099813));
#257223=CARTESIAN_POINT('Ctrl Pts',(-10.912224056838,15.2,1.91885643574456));
#257224=CARTESIAN_POINT('Ctrl Pts',(-10.915891083443,15.2,1.92107177789521));
#257225=CARTESIAN_POINT('Ctrl Pts',(-10.9195581105475,15.2,1.9232871203477));
#257226=CARTESIAN_POINT('Ctrl Pts',(-10.9232332416694,15.2,1.92551540136861));
#257227=CARTESIAN_POINT('Ctrl Pts',(-10.9269163592595,15.2,1.92775663365828));
#257228=CARTESIAN_POINT('Ctrl Pts',(-10.9305994763479,15.2,1.92999786564257));
#257229=CARTESIAN_POINT('Ctrl Pts',(-10.9342905786707,15.2,1.93225205087703));
#257230=CARTESIAN_POINT('Ctrl Pts',(-10.9379895511452,15.2,1.93451920157926));
#257231=CARTESIAN_POINT('Ctrl Pts',(-10.9416885241238,15.2,1.93678635259038));
#257232=CARTESIAN_POINT('Ctrl Pts',(-10.9453953661055,15.2,1.93906647141052));
#257233=CARTESIAN_POINT('Ctrl Pts',(-10.9491099617692,15.2,1.94135956976817));
#257234=CARTESIAN_POINT('Ctrl Pts',(-10.9528245569269,15.2,1.94365266781338));
#257235=CARTESIAN_POINT('Ctrl Pts',(-10.956546906807,15.2,1.94595874678667));
#257236=CARTESIAN_POINT('Ctrl Pts',(-10.9602768933902,15.2,1.94827782009577));
#257237=CARTESIAN_POINT('Ctrl Pts',(-10.9658718740273,15.2,1.95175643053337));
#257238=CARTESIAN_POINT('Ctrl Pts',(-10.9714840399244,15.2,1.95526427792379));
#257239=CARTESIAN_POINT('Ctrl Pts',(-10.9771130083152,15.2,1.95880140620116));
#257240=CARTESIAN_POINT('Ctrl Pts',(-10.9808656533978,15.2,1.96115949139812));
#257241=CARTESIAN_POINT('Ctrl Pts',(-10.9846257646821,15.2,1.96353059018655));
#257242=CARTESIAN_POINT('Ctrl Pts',(-10.9883932307284,15.2,1.96591471488739));
#257243=CARTESIAN_POINT('Ctrl Pts',(-10.9921606972879,15.2,1.96829883991306));
#257244=CARTESIAN_POINT('Ctrl Pts',(-10.9959355180971,15.2,1.9706959892621));
#257245=CARTESIAN_POINT('Ctrl Pts',(-10.999717580526,15.2,1.97310617867209));
#257246=CARTESIAN_POINT('Ctrl Pts',(-11.0025541270899,15.2,1.97491382056539));
#257247=CARTESIAN_POINT('Ctrl Pts',(-11.0053947483034,15.2,1.97672879453281));
#257248=CARTESIAN_POINT('Ctrl Pts',(-11.0082393957834,15.2,1.9785511084666));
#257249=CARTESIAN_POINT('Ctrl Pts',(-11.0110840432633,15.2,1.98037342240038));
#257250=CARTESIAN_POINT('Ctrl Pts',(-11.0139327165098,15.2,1.98220307505055));
#257251=CARTESIAN_POINT('Ctrl Pts',(-11.0167853709475,15.2,1.98404007056649));
#257252=CARTESIAN_POINT('Ctrl Pts',(-11.0196380253851,15.2,1.98587706608243));
#257253=CARTESIAN_POINT('Ctrl Pts',(-11.0224946585581,15.2,1.98772140453404));
#257254=CARTESIAN_POINT('Ctrl Pts',(-11.0253552261799,15.2,1.98957309160008));
#257255=CARTESIAN_POINT('Ctrl Pts',(-11.0282157938018,15.2,1.99142477866612));
#257256=CARTESIAN_POINT('Ctrl Pts',(-11.0310802943128,15.2,1.99328381362856));
#257257=CARTESIAN_POINT('Ctrl Pts',(-11.0339486823747,15.2,1.99515020064307));
#257258=CARTESIAN_POINT('Ctrl Pts',(-11.0368170709577,15.2,1.99701658799663));
#257259=CARTESIAN_POINT('Ctrl Pts',(-11.0396893477418,15.2,1.9988903280523));
#257260=CARTESIAN_POINT('Ctrl Pts',(-11.0425654648687,15.2,2.00077142441002));
#257261=CARTESIAN_POINT('Ctrl Pts',(-11.045441581473,15.2,2.002652520426));
#257262=CARTESIAN_POINT('Ctrl Pts',(-11.0483215400355,15.2,2.0045409724916));
#257263=CARTESIAN_POINT('Ctrl Pts',(-11.0512052935978,15.2,2.00643678596503));
#257264=CARTESIAN_POINT('Ctrl Pts',(-11.05408904716,15.2,2.00833259943846));
#257265=CARTESIAN_POINT('Ctrl Pts',(-11.0569765959779,15.2,2.01023577351237));
#257266=CARTESIAN_POINT('Ctrl Pts',(-11.059867896011,15.2,2.01214631249334));
#257267=CARTESIAN_POINT('Ctrl Pts',(-11.0627591960441,15.2,2.01405685147431));
#257268=CARTESIAN_POINT('Ctrl Pts',(-11.0656542461062,15.2,2.01597475507609));
#257269=CARTESIAN_POINT('Ctrl Pts',(-11.0685530007224,15.2,2.01790002801486));
#257270=CARTESIAN_POINT('Ctrl Pts',(-11.0714517553386,15.2,2.01982530095362));
#257271=CARTESIAN_POINT('Ctrl Pts',(-11.0743542155726,15.2,2.02175794254306));
#257272=CARTESIAN_POINT('Ctrl Pts',(-11.077260334675,15.2,2.02369795609693));
#257273=CARTESIAN_POINT('Ctrl Pts',(-11.0801664537774,15.2,2.02563796965079));
#257274=CARTESIAN_POINT('Ctrl Pts',(-11.0830762328546,15.2,2.02758535579583));
#257275=CARTESIAN_POINT('Ctrl Pts',(-11.0859896278732,15.2,2.02954011826547));
#257276=CARTESIAN_POINT('Ctrl Pts',(-11.0889030234212,15.2,2.03149488109022));
#257277=CARTESIAN_POINT('Ctrl Pts',(-11.0918200337784,15.2,2.03345701942539));
#257278=CARTESIAN_POINT('Ctrl Pts',(-11.0947406148701,15.2,2.03542653821263));
#257279=CARTESIAN_POINT('Ctrl Pts',(-11.0976611954311,15.2,2.03739605664208));
#257280=CARTESIAN_POINT('Ctrl Pts',(-11.1005853472429,15.2,2.03937295500602));
#257281=CARTESIAN_POINT('Ctrl Pts',(-11.1035130258665,15.2,2.04135723565892));
#257282=CARTESIAN_POINT('Ctrl Pts',(-11.1083924904165,15.2,2.04466437020056));
#257283=CARTESIAN_POINT('Ctrl Pts',(-11.1132817476734,15.2,2.04799201313066));
#257284=CARTESIAN_POINT('Ctrl Pts',(-11.1181805989241,15.2,2.05134017993789));
#257285=CARTESIAN_POINT('Ctrl Pts',(-11.1211199095678,15.2,2.05334907994923));
#257286=CARTESIAN_POINT('Ctrl Pts',(-11.1240626736446,15.2,2.05536536966019));
#257287=CARTESIAN_POINT('Ctrl Pts',(-11.1270088467879,15.2,2.05738904875397));
#257288=CARTESIAN_POINT('Ctrl Pts',(-11.1299550199311,15.2,2.05941272784775));
#257289=CARTESIAN_POINT('Ctrl Pts',(-11.1329046029407,15.2,2.061443798524));
#257290=CARTESIAN_POINT('Ctrl Pts',(-11.135857552,15.2,2.0634822644916));
#257291=CARTESIAN_POINT('Ctrl Pts',(-11.1388105010594,15.2,2.06552073045919));
#257292=CARTESIAN_POINT('Ctrl Pts',(-11.141766815602,15.2,2.0675665902015));
#257293=CARTESIAN_POINT('Ctrl Pts',(-11.1447264536608,15.2,2.06961984720959));
#257294=CARTESIAN_POINT('Ctrl Pts',(-11.1476860917197,15.2,2.07167310421767));
#257295=CARTESIAN_POINT('Ctrl Pts',(-11.1506490527028,15.2,2.07373375897259));
#257296=CARTESIAN_POINT('Ctrl Pts',(-11.1536152939512,15.2,2.07580181308322));
#257297=CARTESIAN_POINT('Ctrl Pts',(-11.1565815351995,15.2,2.07786986719385));
#257298=CARTESIAN_POINT('Ctrl Pts',(-11.1595510567104,15.2,2.07994532147257));
#257299=CARTESIAN_POINT('Ctrl Pts',(-11.162523814852,15.2,2.08202817752088));
#257300=CARTESIAN_POINT('Ctrl Pts',(-11.1664874927341,15.2,2.08480531917088));
#257301=CARTESIAN_POINT('Ctrl Pts',(-11.1704569258,15.2,2.0875956213777));
#257302=CARTESIAN_POINT('Ctrl Pts',(-11.1744320130167,15.2,2.09039908947493));
#257303=CARTESIAN_POINT('Ctrl Pts',(-11.1784071002334,15.2,2.09320255757216));
#257304=CARTESIAN_POINT('Ctrl Pts',(-11.1823878411951,15.2,2.0960191907293));
#257305=CARTESIAN_POINT('Ctrl Pts',(-11.1863741376351,15.2,2.09884899499595));
#257306=CARTESIAN_POINT('Ctrl Pts',(-11.1893638596936,15.2,2.10097134800316));
#257307=CARTESIAN_POINT('Ctrl Pts',(-11.1923567062552,15.2,2.10310111003352));
#257308=CARTESIAN_POINT('Ctrl Pts',(-11.1953526345464,15.2,2.10523828264683));
#257309=CARTESIAN_POINT('Ctrl Pts',(-11.1983485628375,15.2,2.10737545526014));
#257310=CARTESIAN_POINT('Ctrl Pts',(-11.2013475734695,15.2,2.1095200384955));
#257311=CARTESIAN_POINT('Ctrl Pts',(-11.204349624069,15.2,2.11167203495962));
#257312=CARTESIAN_POINT('Ctrl Pts',(-11.2073516746685,15.2,2.11382403142374));
#257313=CARTESIAN_POINT('Ctrl Pts',(-11.2103567648593,15.2,2.11598344101199));
#257314=CARTESIAN_POINT('Ctrl Pts',(-11.213364855,15.2,2.11815026497493));
#257315=CARTESIAN_POINT('Ctrl Pts',(-11.2163729451407,15.2,2.12031708893787));
#257316=CARTESIAN_POINT('Ctrl Pts',(-11.219384036048,15.2,2.12249132754217));
#257317=CARTESIAN_POINT('Ctrl Pts',(-11.2223980842299,15.2,2.12467298300392));
#257318=CARTESIAN_POINT('Ctrl Pts',(-11.2254121324118,15.2,2.12685463846567));
#257319=CARTESIAN_POINT('Ctrl Pts',(-11.2284291390583,15.2,2.12904371126263));
#257320=CARTESIAN_POINT('Ctrl Pts',(-11.2314490603908,15.2,2.13124020183337));
#257321=CARTESIAN_POINT('Ctrl Pts',(-11.2344689817233,15.2,2.13343669240411));
#257322=CARTESIAN_POINT('Ctrl Pts',(-11.2374918181841,15.2,2.13564060099922));
#257323=CARTESIAN_POINT('Ctrl Pts',(-11.2405175293654,15.2,2.13785192904286));
#257324=CARTESIAN_POINT('Ctrl Pts',(-11.2435432410964,15.2,2.14006325748823));
#257325=CARTESIAN_POINT('Ctrl Pts',(-11.2465718276033,15.2,2.14228200709404));
#257326=CARTESIAN_POINT('Ctrl Pts',(-11.2496032518776,15.2,2.14450817746025));
#257327=CARTESIAN_POINT('Ctrl Pts',(-11.2526346756011,15.2,2.14673434742203));
#257328=CARTESIAN_POINT('Ctrl Pts',(-11.2556689386246,15.2,2.14896793802511));
#257329=CARTESIAN_POINT('Ctrl Pts',(-11.2587059980978,15.2,2.151208951486));
#257330=CARTESIAN_POINT('Ctrl Pts',(-11.261743057571,15.2,2.1534499649469));
#257331=CARTESIAN_POINT('Ctrl Pts',(-11.2647829118995,15.2,2.15569840179033));
#257332=CARTESIAN_POINT('Ctrl Pts',(-11.2678255119695,15.2,2.15795426226032));
#257333=CARTESIAN_POINT('Ctrl Pts',(-11.2718823118785,15.2,2.1609620760837));
#257334=CARTESIAN_POINT('Ctrl Pts',(-11.2759439882014,15.2,2.16398308913101));
#257335=CARTESIAN_POINT('Ctrl Pts',(-11.2800104648685,15.2,2.16701730343717));
#257336=CARTESIAN_POINT('Ctrl Pts',(-11.2840769420896,15.2,2.17005151815675));
#257337=CARTESIAN_POINT('Ctrl Pts',(-11.288148224556,15.2,2.17309893949932));
#257338=CARTESIAN_POINT('Ctrl Pts',(-11.2922242990001,15.2,2.17615954699999));
#257339=CARTESIAN_POINT('Ctrl Pts',(-10.0330625580001,15.2,2.64164356399998));
#257340=CARTESIAN_POINT('Ctrl Pts',(-10.0330625580001,11.6,2.64164356399998));
#257341=CARTESIAN_POINT('Ctrl Pts',(-10.0332343610001,15.2,2.64167330399999));
#257342=CARTESIAN_POINT('Ctrl Pts',(-10.0332343610001,11.6,2.64167330399999));
#257343=CARTESIAN_POINT('Ctrl Pts',(-10.0335839820001,15.2,2.64173373799999));
#257344=CARTESIAN_POINT('Ctrl Pts',(-10.0335839820001,11.6,2.64173373799998));
#257345=CARTESIAN_POINT('Ctrl Pts',(-10.0341137860001,15.2,2.64182504799999));
#257346=CARTESIAN_POINT('Ctrl Pts',(-10.0341137860001,11.6,2.64182504799999));
#257347=CARTESIAN_POINT('Ctrl Pts',(-10.0348275720001,15.2,2.64194751899999));
#257348=CARTESIAN_POINT('Ctrl Pts',(-10.0348275720001,11.6,2.64194751899998));
#257349=CARTESIAN_POINT('Ctrl Pts',(-10.0357305600001,15.2,2.64210152599999));
#257350=CARTESIAN_POINT('Ctrl Pts',(-10.0357305600001,11.6,2.64210152599999));
#257351=CARTESIAN_POINT('Ctrl Pts',(-10.0366483400001,15.2,2.64225710799998));
#257352=CARTESIAN_POINT('Ctrl Pts',(-10.0366483400001,11.6,2.64225710799998));
#257353=CARTESIAN_POINT('Ctrl Pts',(-10.0375756570001,15.2,2.64241334899998));
#257354=CARTESIAN_POINT('Ctrl Pts',(-10.0375756570001,11.6,2.64241334899998));
#257355=CARTESIAN_POINT('Ctrl Pts',(-10.0385124890001,15.2,2.64257022899999));
#257356=CARTESIAN_POINT('Ctrl Pts',(-10.0385124890001,11.6,2.64257022899999));
#257357=CARTESIAN_POINT('Ctrl Pts',(-10.0394588120001,15.2,2.64272772499999));
#257358=CARTESIAN_POINT('Ctrl Pts',(-10.0394588120001,11.6,2.64272772499999));
#257359=CARTESIAN_POINT('Ctrl Pts',(-10.0404146010001,15.2,2.64288581199998));
#257360=CARTESIAN_POINT('Ctrl Pts',(-10.0404146010001,11.6,2.64288581199998));
#257361=CARTESIAN_POINT('Ctrl Pts',(-10.0413798350001,15.2,2.64304447199999));
#257362=CARTESIAN_POINT('Ctrl Pts',(-10.0413798350001,11.6,2.64304447199999));
#257363=CARTESIAN_POINT('Ctrl Pts',(-10.0423544890001,15.2,2.64320368099998));
#257364=CARTESIAN_POINT('Ctrl Pts',(-10.0423544890001,11.6,2.64320368099998));
#257365=CARTESIAN_POINT('Ctrl Pts',(-10.0433385410001,15.2,2.64336341799999));
#257366=CARTESIAN_POINT('Ctrl Pts',(-10.0433385410001,11.6,2.64336341799999));
#257367=CARTESIAN_POINT('Ctrl Pts',(-10.0443319680001,15.2,2.64352366099998));
#257368=CARTESIAN_POINT('Ctrl Pts',(-10.0443319680001,11.6,2.64352366099998));
#257369=CARTESIAN_POINT('Ctrl Pts',(-10.0453347470001,15.2,2.64368438699999));
#257370=CARTESIAN_POINT('Ctrl Pts',(-10.0453347470001,11.6,2.64368438699999));
#257371=CARTESIAN_POINT('Ctrl Pts',(-10.0463468550001,15.2,2.64384557699999));
#257372=CARTESIAN_POINT('Ctrl Pts',(-10.0463468550001,11.6,2.64384557699999));
#257373=CARTESIAN_POINT('Ctrl Pts',(-10.0473682690001,15.2,2.64400720799999));
#257374=CARTESIAN_POINT('Ctrl Pts',(-10.0473682690001,11.6,2.64400720799999));
#257375=CARTESIAN_POINT('Ctrl Pts',(-10.0483989660001,15.2,2.64416925999999));
#257376=CARTESIAN_POINT('Ctrl Pts',(-10.0483989660001,11.6,2.64416925999999));
#257377=CARTESIAN_POINT('Ctrl Pts',(-10.0494389260001,15.2,2.64433171099999));
#257378=CARTESIAN_POINT('Ctrl Pts',(-10.0494389260001,11.6,2.64433171099998));
#257379=CARTESIAN_POINT('Ctrl Pts',(-10.0504881240001,15.2,2.64449453999998));
#257380=CARTESIAN_POINT('Ctrl Pts',(-10.0504881240001,11.6,2.64449453999998));
#257381=CARTESIAN_POINT('Ctrl Pts',(-10.0515465390001,15.2,2.64465772599999));
#257382=CARTESIAN_POINT('Ctrl Pts',(-10.0515465390001,11.6,2.64465772599999));
#257383=CARTESIAN_POINT('Ctrl Pts',(-10.0526141480001,15.2,2.64482124899998));
#257384=CARTESIAN_POINT('Ctrl Pts',(-10.0526141480001,11.6,2.64482124899998));
#257385=CARTESIAN_POINT('Ctrl Pts',(-10.0536909300001,15.2,2.64498508799999));
#257386=CARTESIAN_POINT('Ctrl Pts',(-10.0536909300001,11.6,2.64498508799999));
#257387=CARTESIAN_POINT('Ctrl Pts',(-10.0547768630001,15.2,2.64514922199999));
#257388=CARTESIAN_POINT('Ctrl Pts',(-10.0547768630001,11.6,2.64514922199999));
#257389=CARTESIAN_POINT('Ctrl Pts',(-10.0558719240001,15.2,2.64531363099999));
#257390=CARTESIAN_POINT('Ctrl Pts',(-10.0558719240001,11.6,2.64531363099999));
#257391=CARTESIAN_POINT('Ctrl Pts',(-10.0569760920001,15.2,2.64547829499998));
#257392=CARTESIAN_POINT('Ctrl Pts',(-10.0569760920001,11.6,2.64547829499998));
#257393=CARTESIAN_POINT('Ctrl Pts',(-10.0580893450001,15.2,2.64564319399998));
#257394=CARTESIAN_POINT('Ctrl Pts',(-10.0580893450001,11.6,2.64564319399998));
#257395=CARTESIAN_POINT('Ctrl Pts',(-10.0592116610001,15.2,2.64580830499998));
#257396=CARTESIAN_POINT('Ctrl Pts',(-10.0592116610001,11.6,2.64580830499998));
#257397=CARTESIAN_POINT('Ctrl Pts',(-10.0603430200001,15.2,2.64597361199999));
#257398=CARTESIAN_POINT('Ctrl Pts',(-10.0603430200001,11.6,2.64597361199999));
#257399=CARTESIAN_POINT('Ctrl Pts',(-10.0614833980001,15.2,2.64613909299998));
#257400=CARTESIAN_POINT('Ctrl Pts',(-10.0614833980001,11.6,2.64613909299998));
#257401=CARTESIAN_POINT('Ctrl Pts',(-10.0626327760001,15.2,2.64630472799999));
#257402=CARTESIAN_POINT('Ctrl Pts',(-10.0626327760001,11.6,2.64630472799999));
#257403=CARTESIAN_POINT('Ctrl Pts',(-10.0637911310001,15.2,2.64647049799999));
#257404=CARTESIAN_POINT('Ctrl Pts',(-10.0637911310001,11.6,2.64647049799999));
#257405=CARTESIAN_POINT('Ctrl Pts',(-10.0649584440001,15.2,2.64663638399998));
#257406=CARTESIAN_POINT('Ctrl Pts',(-10.0649584440001,11.6,2.64663638399998));
#257407=CARTESIAN_POINT('Ctrl Pts',(-10.0661346930001,15.2,2.64680236399998));
#257408=CARTESIAN_POINT('Ctrl Pts',(-10.0661346930001,11.6,2.64680236399998));
#257409=CARTESIAN_POINT('Ctrl Pts',(-10.0673198560001,15.2,2.64696842199999));
#257410=CARTESIAN_POINT('Ctrl Pts',(-10.0673198560001,11.6,2.64696842199999));
#257411=CARTESIAN_POINT('Ctrl Pts',(-10.0685139130001,15.2,2.64713453499999));
#257412=CARTESIAN_POINT('Ctrl Pts',(-10.0685139130001,11.6,2.64713453499999));
#257413=CARTESIAN_POINT('Ctrl Pts',(-10.0697168420001,15.2,2.64730068599999));
#257414=CARTESIAN_POINT('Ctrl Pts',(-10.0697168420001,11.6,2.64730068599999));
#257415=CARTESIAN_POINT('Ctrl Pts',(-10.0709286240001,15.2,2.64746685699999));
#257416=CARTESIAN_POINT('Ctrl Pts',(-10.0709286240001,11.6,2.64746685699999));
#257417=CARTESIAN_POINT('Ctrl Pts',(-10.0721492380001,15.2,2.64763302599999));
#257418=CARTESIAN_POINT('Ctrl Pts',(-10.0721492380001,11.6,2.64763302599999));
#257419=CARTESIAN_POINT('Ctrl Pts',(-10.0733786630001,15.2,2.64779917599999));
#257420=CARTESIAN_POINT('Ctrl Pts',(-10.0733786630001,11.6,2.64779917599998));
#257421=CARTESIAN_POINT('Ctrl Pts',(-10.0746168780001,15.2,2.64796528799998));
#257422=CARTESIAN_POINT('Ctrl Pts',(-10.0746168780001,11.6,2.64796528799998));
#257423=CARTESIAN_POINT('Ctrl Pts',(-10.0758638630001,15.2,2.64813134199999));
#257424=CARTESIAN_POINT('Ctrl Pts',(-10.0758638630001,11.6,2.64813134199999));
#257425=CARTESIAN_POINT('Ctrl Pts',(-10.0771195980001,15.2,2.64829732099999));
#257426=CARTESIAN_POINT('Ctrl Pts',(-10.0771195980001,11.6,2.64829732099999));
#257427=CARTESIAN_POINT('Ctrl Pts',(-10.0783840630001,15.2,2.64846320699998));
#257428=CARTESIAN_POINT('Ctrl Pts',(-10.0783840630001,11.6,2.64846320699998));
#257429=CARTESIAN_POINT('Ctrl Pts',(-10.0796572370001,15.2,2.64862897899998));
#257430=CARTESIAN_POINT('Ctrl Pts',(-10.0796572370001,11.6,2.64862897899998));
#257431=CARTESIAN_POINT('Ctrl Pts',(-10.0809391000001,15.2,2.64879461899999));
#257432=CARTESIAN_POINT('Ctrl Pts',(-10.0809391000001,11.6,2.64879461899999));
#257433=CARTESIAN_POINT('Ctrl Pts',(-10.0822296340001,15.2,2.64896011099999));
#257434=CARTESIAN_POINT('Ctrl Pts',(-10.0822296340001,11.6,2.64896011099999));
#257435=CARTESIAN_POINT('Ctrl Pts',(-10.0835288160001,15.2,2.64912543499998));
#257436=CARTESIAN_POINT('Ctrl Pts',(-10.0835288160001,11.6,2.64912543499998));
#257437=CARTESIAN_POINT('Ctrl Pts',(-10.0848366280001,15.2,2.64929057399999));
#257438=CARTESIAN_POINT('Ctrl Pts',(-10.0848366280001,11.6,2.64929057399998));
#257439=CARTESIAN_POINT('Ctrl Pts',(-10.0861530500001,15.2,2.64945550899998));
#257440=CARTESIAN_POINT('Ctrl Pts',(-10.0861530500001,11.6,2.64945550899998));
#257441=CARTESIAN_POINT('Ctrl Pts',(-10.0874780620001,15.2,2.64962022099999));
#257442=CARTESIAN_POINT('Ctrl Pts',(-10.0874780620001,11.6,2.64962022099999));
#257443=CARTESIAN_POINT('Ctrl Pts',(-10.0888116440001,15.2,2.64978469499999));
#257444=CARTESIAN_POINT('Ctrl Pts',(-10.0888116440001,11.6,2.64978469499999));
#257445=CARTESIAN_POINT('Ctrl Pts',(-10.0901537780001,15.2,2.64994891199999));
#257446=CARTESIAN_POINT('Ctrl Pts',(-10.0901537780001,11.6,2.64994891199999));
#257447=CARTESIAN_POINT('Ctrl Pts',(-10.0915044430001,15.2,2.65011285399999));
#257448=CARTESIAN_POINT('Ctrl Pts',(-10.0915044430001,11.6,2.65011285399999));
#257449=CARTESIAN_POINT('Ctrl Pts',(-10.0928636200001,15.2,2.65027650399999));
#257450=CARTESIAN_POINT('Ctrl Pts',(-10.0928636200001,11.6,2.65027650399999));
#257451=CARTESIAN_POINT('Ctrl Pts',(-10.0942312910001,15.2,2.65043984299999));
#257452=CARTESIAN_POINT('Ctrl Pts',(-10.0942312910001,11.6,2.65043984299999));
#257453=CARTESIAN_POINT('Ctrl Pts',(-10.0956074340001,15.2,2.65060285499998));
#257454=CARTESIAN_POINT('Ctrl Pts',(-10.0956074340001,11.6,2.65060285499998));
#257455=CARTESIAN_POINT('Ctrl Pts',(-10.0969920330001,15.2,2.65076552299998));
#257456=CARTESIAN_POINT('Ctrl Pts',(-10.0969920330001,11.6,2.65076552299998));
#257457=CARTESIAN_POINT('Ctrl Pts',(-10.0983850660001,15.2,2.65092782899998));
#257458=CARTESIAN_POINT('Ctrl Pts',(-10.0983850660001,11.6,2.65092782899998));
#257459=CARTESIAN_POINT('Ctrl Pts',(-10.0997865150001,15.2,2.65108975499999));
#257460=CARTESIAN_POINT('Ctrl Pts',(-10.0997865150001,11.6,2.65108975499999));
#257461=CARTESIAN_POINT('Ctrl Pts',(-10.1011963620001,15.2,2.65125128599998));
#257462=CARTESIAN_POINT('Ctrl Pts',(-10.1011963620001,11.6,2.65125128599998));
#257463=CARTESIAN_POINT('Ctrl Pts',(-10.1026145880001,15.2,2.65141240299998));
#257464=CARTESIAN_POINT('Ctrl Pts',(-10.1026145880001,11.6,2.65141240299998));
#257465=CARTESIAN_POINT('Ctrl Pts',(-10.1040411730001,15.2,2.65157308999999));
#257466=CARTESIAN_POINT('Ctrl Pts',(-10.1040411730001,11.6,2.65157308999999));
#257467=CARTESIAN_POINT('Ctrl Pts',(-10.1054760990001,15.2,2.65173333099998));
#257468=CARTESIAN_POINT('Ctrl Pts',(-10.1054760990001,11.6,2.65173333099998));
#257469=CARTESIAN_POINT('Ctrl Pts',(-10.1069193480001,15.2,2.65189310799999));
#257470=CARTESIAN_POINT('Ctrl Pts',(-10.1069193480001,11.6,2.65189310799998));
#257471=CARTESIAN_POINT('Ctrl Pts',(-10.1083709000001,15.2,2.65205240499998));
#257472=CARTESIAN_POINT('Ctrl Pts',(-10.1083709000001,11.6,2.65205240499998));
#257473=CARTESIAN_POINT('Ctrl Pts',(-10.1098307370001,15.2,2.65221120399998));
#257474=CARTESIAN_POINT('Ctrl Pts',(-10.1098307370001,11.6,2.65221120399998));
#257475=CARTESIAN_POINT('Ctrl Pts',(-10.1112988410001,15.2,2.65236948899998));
#257476=CARTESIAN_POINT('Ctrl Pts',(-10.1112988410001,11.6,2.65236948899998));
#257477=CARTESIAN_POINT('Ctrl Pts',(-10.1127751920001,15.2,2.65252724599998));
#257478=CARTESIAN_POINT('Ctrl Pts',(-10.1127751920001,11.6,2.65252724599998));
#257479=CARTESIAN_POINT('Ctrl Pts',(-10.1142597750001,15.2,2.65268445599999));
#257480=CARTESIAN_POINT('Ctrl Pts',(-10.1142597750001,11.6,2.65268445599998));
#257481=CARTESIAN_POINT('Ctrl Pts',(-10.1157525680001,15.2,2.65284110399998));
#257482=CARTESIAN_POINT('Ctrl Pts',(-10.1157525680001,11.6,2.65284110399998));
#257483=CARTESIAN_POINT('Ctrl Pts',(-10.1172535550001,15.2,2.65299717299998));
#257484=CARTESIAN_POINT('Ctrl Pts',(-10.1172535550001,11.6,2.65299717299998));
#257485=CARTESIAN_POINT('Ctrl Pts',(-10.1187627170001,15.2,2.65315264699999));
#257486=CARTESIAN_POINT('Ctrl Pts',(-10.1187627170001,11.6,2.65315264699999));
#257487=CARTESIAN_POINT('Ctrl Pts',(-10.1202800360001,15.2,2.65330750999999));
#257488=CARTESIAN_POINT('Ctrl Pts',(-10.1202800360001,11.6,2.65330750999999));
#257489=CARTESIAN_POINT('Ctrl Pts',(-10.1218054950001,15.2,2.65346174599999));
#257490=CARTESIAN_POINT('Ctrl Pts',(-10.1218054950001,11.6,2.65346174599998));
#257491=CARTESIAN_POINT('Ctrl Pts',(-10.1233390740001,15.2,2.65361533999998));
#257492=CARTESIAN_POINT('Ctrl Pts',(-10.1233390740001,11.6,2.65361533999998));
#257493=CARTESIAN_POINT('Ctrl Pts',(-10.1248807580001,15.2,2.65376827399999));
#257494=CARTESIAN_POINT('Ctrl Pts',(-10.1248807580001,11.6,2.65376827399999));
#257495=CARTESIAN_POINT('Ctrl Pts',(-10.1264305260001,15.2,2.65392053499999));
#257496=CARTESIAN_POINT('Ctrl Pts',(-10.1264305260001,11.6,2.65392053499998));
#257497=CARTESIAN_POINT('Ctrl Pts',(-10.1279883630001,15.2,2.65407210499998));
#257498=CARTESIAN_POINT('Ctrl Pts',(-10.1279883630001,11.6,2.65407210499998));
#257499=CARTESIAN_POINT('Ctrl Pts',(-10.1295542490001,15.2,2.65422296899998));
#257500=CARTESIAN_POINT('Ctrl Pts',(-10.1295542490001,11.6,2.65422296899998));
#257501=CARTESIAN_POINT('Ctrl Pts',(-10.1311281680001,15.2,2.65437311199998));
#257502=CARTESIAN_POINT('Ctrl Pts',(-10.1311281680001,11.6,2.65437311199998));
#257503=CARTESIAN_POINT('Ctrl Pts',(-10.1327101010001,15.2,2.65452251899998));
#257504=CARTESIAN_POINT('Ctrl Pts',(-10.1327101010001,11.6,2.65452251899998));
#257505=CARTESIAN_POINT('Ctrl Pts',(-10.1343000320001,15.2,2.65467117299998));
#257506=CARTESIAN_POINT('Ctrl Pts',(-10.1343000320001,11.6,2.65467117299998));
#257507=CARTESIAN_POINT('Ctrl Pts',(-10.1358979420001,15.2,2.65481905899998));
#257508=CARTESIAN_POINT('Ctrl Pts',(-10.1358979420001,11.6,2.65481905899998));
#257509=CARTESIAN_POINT('Ctrl Pts',(-10.1375038160001,15.2,2.65496616399999));
#257510=CARTESIAN_POINT('Ctrl Pts',(-10.1375038160001,11.6,2.65496616399999));
#257511=CARTESIAN_POINT('Ctrl Pts',(-10.1391176340001,15.2,2.65511246899998));
#257512=CARTESIAN_POINT('Ctrl Pts',(-10.1391176340001,11.6,2.65511246899998));
#257513=CARTESIAN_POINT('Ctrl Pts',(-10.1407393800001,15.2,2.65525796199999));
#257514=CARTESIAN_POINT('Ctrl Pts',(-10.1407393800001,11.6,2.65525796199999));
#257515=CARTESIAN_POINT('Ctrl Pts',(-10.1423690360001,15.2,2.65540262599998));
#257516=CARTESIAN_POINT('Ctrl Pts',(-10.1423690360001,11.6,2.65540262599998));
#257517=CARTESIAN_POINT('Ctrl Pts',(-10.1440065870001,15.2,2.65554644699999));
#257518=CARTESIAN_POINT('Ctrl Pts',(-10.1440065870001,11.6,2.65554644699999));
#257519=CARTESIAN_POINT('Ctrl Pts',(-10.1456520130001,15.2,2.65568941099998));
#257520=CARTESIAN_POINT('Ctrl Pts',(-10.1456520130001,11.6,2.65568941099998));
#257521=CARTESIAN_POINT('Ctrl Pts',(-10.1473052990001,15.2,2.65583150099998));
#257522=CARTESIAN_POINT('Ctrl Pts',(-10.1473052990001,11.6,2.65583150099998));
#257523=CARTESIAN_POINT('Ctrl Pts',(-10.1489664270001,15.2,2.65597270399999));
#257524=CARTESIAN_POINT('Ctrl Pts',(-10.1489664270001,11.6,2.65597270399999));
#257525=CARTESIAN_POINT('Ctrl Pts',(-10.1506353810001,15.2,2.65611300399998));
#257526=CARTESIAN_POINT('Ctrl Pts',(-10.1506353810001,11.6,2.65611300399998));
#257527=CARTESIAN_POINT('Ctrl Pts',(-10.1523121420001,15.2,2.65625238599998));
#257528=CARTESIAN_POINT('Ctrl Pts',(-10.1523121420001,11.6,2.65625238599998));
#257529=CARTESIAN_POINT('Ctrl Pts',(-10.1539966950001,15.2,2.65639083799999));
#257530=CARTESIAN_POINT('Ctrl Pts',(-10.1539966950001,11.6,2.65639083799999));
#257531=CARTESIAN_POINT('Ctrl Pts',(-10.1556890250001,15.2,2.65652834299999));
#257532=CARTESIAN_POINT('Ctrl Pts',(-10.1556890250001,11.6,2.65652834299999));
#257533=CARTESIAN_POINT('Ctrl Pts',(-10.1573891100001,15.2,2.65666488699999));
#257534=CARTESIAN_POINT('Ctrl Pts',(-10.1573891100001,11.6,2.65666488699999));
#257535=CARTESIAN_POINT('Ctrl Pts',(-10.1590969390001,15.2,2.65680045599999));
#257536=CARTESIAN_POINT('Ctrl Pts',(-10.1590969390001,11.6,2.65680045599999));
#257537=CARTESIAN_POINT('Ctrl Pts',(-10.1608124920001,15.2,2.65693503499998));
#257538=CARTESIAN_POINT('Ctrl Pts',(-10.1608124920001,11.6,2.65693503499998));
#257539=CARTESIAN_POINT('Ctrl Pts',(-10.1625357530001,15.2,2.65706861099999));
#257540=CARTESIAN_POINT('Ctrl Pts',(-10.1625357530001,11.6,2.65706861099999));
#257541=CARTESIAN_POINT('Ctrl Pts',(-10.1642667060001,15.2,2.65720116799999));
#257542=CARTESIAN_POINT('Ctrl Pts',(-10.1642667060001,11.6,2.65720116799999));
#257543=CARTESIAN_POINT('Ctrl Pts',(-10.1660053350001,15.2,2.65733269399998));
#257544=CARTESIAN_POINT('Ctrl Pts',(-10.1660053350001,11.6,2.65733269399998));
#257545=CARTESIAN_POINT('Ctrl Pts',(-10.1677516220001,15.2,2.65746317399999));
#257546=CARTESIAN_POINT('Ctrl Pts',(-10.1677516220001,11.6,2.65746317399999));
#257547=CARTESIAN_POINT('Ctrl Pts',(-10.1695055520001,15.2,2.65759259199999));
#257548=CARTESIAN_POINT('Ctrl Pts',(-10.1695055520001,11.6,2.65759259199999));
#257549=CARTESIAN_POINT('Ctrl Pts',(-10.1712671090001,15.2,2.65772093799999));
#257550=CARTESIAN_POINT('Ctrl Pts',(-10.1712671090001,11.6,2.65772093799999));
#257551=CARTESIAN_POINT('Ctrl Pts',(-10.1730362760001,15.2,2.65784819299999));
#257552=CARTESIAN_POINT('Ctrl Pts',(-10.1730362760001,11.6,2.65784819299998));
#257553=CARTESIAN_POINT('Ctrl Pts',(-10.1748130360001,15.2,2.65797434899999));
#257554=CARTESIAN_POINT('Ctrl Pts',(-10.1748130360001,11.6,2.65797434899999));
#257555=CARTESIAN_POINT('Ctrl Pts',(-10.1765973750001,15.2,2.65809938799999));
#257556=CARTESIAN_POINT('Ctrl Pts',(-10.1765973750001,11.6,2.65809938799999));
#257557=CARTESIAN_POINT('Ctrl Pts',(-10.1783892740001,15.2,2.65822329699999));
#257558=CARTESIAN_POINT('Ctrl Pts',(-10.1783892740001,11.6,2.65822329699999));
#257559=CARTESIAN_POINT('Ctrl Pts',(-10.1801887200001,15.2,2.65834606199999));
#257560=CARTESIAN_POINT('Ctrl Pts',(-10.1801887200001,11.6,2.65834606199999));
#257561=CARTESIAN_POINT('Ctrl Pts',(-10.1819956950001,15.2,2.65846767299998));
#257562=CARTESIAN_POINT('Ctrl Pts',(-10.1819956950001,11.6,2.65846767299998));
#257563=CARTESIAN_POINT('Ctrl Pts',(-10.1838101840001,15.2,2.65858811199998));
#257564=CARTESIAN_POINT('Ctrl Pts',(-10.1838101840001,11.6,2.65858811199998));
#257565=CARTESIAN_POINT('Ctrl Pts',(-10.1856321710001,15.2,2.65870736699998));
#257566=CARTESIAN_POINT('Ctrl Pts',(-10.1856321710001,11.6,2.65870736699998));
#257567=CARTESIAN_POINT('Ctrl Pts',(-10.1874616400001,15.2,2.65882542499998));
#257568=CARTESIAN_POINT('Ctrl Pts',(-10.1874616400001,11.6,2.65882542499998));
#257569=CARTESIAN_POINT('Ctrl Pts',(-10.1892985750001,15.2,2.65894227199999));
#257570=CARTESIAN_POINT('Ctrl Pts',(-10.1892985750001,11.6,2.65894227199999));
#257571=CARTESIAN_POINT('Ctrl Pts',(-10.1911429610001,15.2,2.65905789599999));
#257572=CARTESIAN_POINT('Ctrl Pts',(-10.1911429610001,11.6,2.65905789599999));
#257573=CARTESIAN_POINT('Ctrl Pts',(-10.1929947820001,15.2,2.65917228199999));
#257574=CARTESIAN_POINT('Ctrl Pts',(-10.1929947820001,11.6,2.65917228199999));
#257575=CARTESIAN_POINT('Ctrl Pts',(-10.1948540200001,15.2,2.65928541799998));
#257576=CARTESIAN_POINT('Ctrl Pts',(-10.1948540200001,11.6,2.65928541799998));
#257577=CARTESIAN_POINT('Ctrl Pts',(-10.1967206650001,15.2,2.65939729099999));
#257578=CARTESIAN_POINT('Ctrl Pts',(-10.1967206650001,11.6,2.65939729099998));
#257579=CARTESIAN_POINT('Ctrl Pts',(-10.1985946950001,15.2,2.65950788699998));
#257580=CARTESIAN_POINT('Ctrl Pts',(-10.1985946950001,11.6,2.65950788699998));
#257581=CARTESIAN_POINT('Ctrl Pts',(-10.2004760990001,15.2,2.65961719299998));
#257582=CARTESIAN_POINT('Ctrl Pts',(-10.2004760990001,11.6,2.65961719299998));
#257583=CARTESIAN_POINT('Ctrl Pts',(-10.2023648590001,15.2,2.65972519599998));
#257584=CARTESIAN_POINT('Ctrl Pts',(-10.2023648590001,11.6,2.65972519599998));
#257585=CARTESIAN_POINT('Ctrl Pts',(-10.2042609620001,15.2,2.65983188399999));
#257586=CARTESIAN_POINT('Ctrl Pts',(-10.2042609620001,11.6,2.65983188399999));
#257587=CARTESIAN_POINT('Ctrl Pts',(-10.2061643900001,15.2,2.65993724299998));
#257588=CARTESIAN_POINT('Ctrl Pts',(-10.2061643900001,11.6,2.65993724299998));
#257589=CARTESIAN_POINT('Ctrl Pts',(-10.2080751300001,15.2,2.66004126199999));
#257590=CARTESIAN_POINT('Ctrl Pts',(-10.2080751300001,11.6,2.66004126199999));
#257591=CARTESIAN_POINT('Ctrl Pts',(-10.2099931640001,15.2,2.66014392599998));
#257592=CARTESIAN_POINT('Ctrl Pts',(-10.2099931640001,11.6,2.66014392599998));
#257593=CARTESIAN_POINT('Ctrl Pts',(-10.2119184800001,15.2,2.66024522299999));
#257594=CARTESIAN_POINT('Ctrl Pts',(-10.2119184800001,11.6,2.66024522299999));
#257595=CARTESIAN_POINT('Ctrl Pts',(-10.2138510600001,15.2,2.66034513999998));
#257596=CARTESIAN_POINT('Ctrl Pts',(-10.2138510600001,11.6,2.66034513999998));
#257597=CARTESIAN_POINT('Ctrl Pts',(-10.2157908920001,15.2,2.66044366699998));
#257598=CARTESIAN_POINT('Ctrl Pts',(-10.2157908920001,11.6,2.66044366699998));
#257599=CARTESIAN_POINT('Ctrl Pts',(-10.2177379570001,15.2,2.66054078699998));
#257600=CARTESIAN_POINT('Ctrl Pts',(-10.2177379570001,11.6,2.66054078699998));
#257601=CARTESIAN_POINT('Ctrl Pts',(-10.2196922430001,15.2,2.66063649199998));
#257602=CARTESIAN_POINT('Ctrl Pts',(-10.2196922430001,11.6,2.66063649199998));
#257603=CARTESIAN_POINT('Ctrl Pts',(-10.2216537340001,15.2,2.66073076599999));
#257604=CARTESIAN_POINT('Ctrl Pts',(-10.2216537340001,11.6,2.66073076599999));
#257605=CARTESIAN_POINT('Ctrl Pts',(-10.2236224150001,15.2,2.66082359899999));
#257606=CARTESIAN_POINT('Ctrl Pts',(-10.2236224150001,11.6,2.66082359899999));
#257607=CARTESIAN_POINT('Ctrl Pts',(-10.2255982700001,15.2,2.66091497699998));
#257608=CARTESIAN_POINT('Ctrl Pts',(-10.2255982700001,11.6,2.66091497699998));
#257609=CARTESIAN_POINT('Ctrl Pts',(-10.2275812850001,15.2,2.66100488799999));
#257610=CARTESIAN_POINT('Ctrl Pts',(-10.2275812850001,11.6,2.66100488799999));
#257611=CARTESIAN_POINT('Ctrl Pts',(-10.2295714460001,15.2,2.66109332199999));
#257612=CARTESIAN_POINT('Ctrl Pts',(-10.2295714460001,11.6,2.66109332199999));
#257613=CARTESIAN_POINT('Ctrl Pts',(-10.2315687380001,15.2,2.66118026399998));
#257614=CARTESIAN_POINT('Ctrl Pts',(-10.2315687380001,11.6,2.66118026399998));
#257615=CARTESIAN_POINT('Ctrl Pts',(-10.2335731450001,15.2,2.66126570199999));
#257616=CARTESIAN_POINT('Ctrl Pts',(-10.2335731450001,11.6,2.66126570199999));
#257617=CARTESIAN_POINT('Ctrl Pts',(-10.2355846530001,15.2,2.66134962599998));
#257618=CARTESIAN_POINT('Ctrl Pts',(-10.2355846530001,11.6,2.66134962599998));
#257619=CARTESIAN_POINT('Ctrl Pts',(-10.2376032480001,15.2,2.66143202199999));
#257620=CARTESIAN_POINT('Ctrl Pts',(-10.2376032480001,11.6,2.66143202199998));
#257621=CARTESIAN_POINT('Ctrl Pts',(-10.2396289140001,15.2,2.66151287899999));
#257622=CARTESIAN_POINT('Ctrl Pts',(-10.2396289140001,11.6,2.66151287899999));
#257623=CARTESIAN_POINT('Ctrl Pts',(-10.2416616380001,15.2,2.66159218399999));
#257624=CARTESIAN_POINT('Ctrl Pts',(-10.2416616380001,11.6,2.66159218399999));
#257625=CARTESIAN_POINT('Ctrl Pts',(-10.2437014030001,15.2,2.66166992699999));
#257626=CARTESIAN_POINT('Ctrl Pts',(-10.2437014030001,11.6,2.66166992699999));
#257627=CARTESIAN_POINT('Ctrl Pts',(-10.2457481980001,15.2,2.66174609399998));
#257628=CARTESIAN_POINT('Ctrl Pts',(-10.2457481980001,11.6,2.66174609399998));
#257629=CARTESIAN_POINT('Ctrl Pts',(-10.2478020060001,15.2,2.66182067599999));
#257630=CARTESIAN_POINT('Ctrl Pts',(-10.2478020060001,11.6,2.66182067599999));
#257631=CARTESIAN_POINT('Ctrl Pts',(-10.2498628120001,15.2,2.66189365799999));
#257632=CARTESIAN_POINT('Ctrl Pts',(-10.2498628120001,11.6,2.66189365799998));
#257633=CARTESIAN_POINT('Ctrl Pts',(-10.2519306040001,15.2,2.66196502999998));
#257634=CARTESIAN_POINT('Ctrl Pts',(-10.2519306040001,11.6,2.66196502999998));
#257635=CARTESIAN_POINT('Ctrl Pts',(-10.2540053660001,15.2,2.66203477999999));
#257636=CARTESIAN_POINT('Ctrl Pts',(-10.2540053660001,11.6,2.66203477999999));
#257637=CARTESIAN_POINT('Ctrl Pts',(-10.2560870840001,15.2,2.66210289699998));
#257638=CARTESIAN_POINT('Ctrl Pts',(-10.2560870840001,11.6,2.66210289699998));
#257639=CARTESIAN_POINT('Ctrl Pts',(-10.2581757450001,15.2,2.66216936899998));
#257640=CARTESIAN_POINT('Ctrl Pts',(-10.2581757450001,11.6,2.66216936899998));
#257641=CARTESIAN_POINT('Ctrl Pts',(-10.2602713320001,15.2,2.66223418299998));
#257642=CARTESIAN_POINT('Ctrl Pts',(-10.2602713320001,11.6,2.66223418299998));
#257643=CARTESIAN_POINT('Ctrl Pts',(-10.2623738330001,15.2,2.66229732999999));
#257644=CARTESIAN_POINT('Ctrl Pts',(-10.2623738330001,11.6,2.66229732999999));
#257645=CARTESIAN_POINT('Ctrl Pts',(-10.2644832330001,15.2,2.66235879699998));
#257646=CARTESIAN_POINT('Ctrl Pts',(-10.2644832330001,11.6,2.66235879699998));
#257647=CARTESIAN_POINT('Ctrl Pts',(-10.2665995190001,15.2,2.66241857399999));
#257648=CARTESIAN_POINT('Ctrl Pts',(-10.2665995190001,11.6,2.66241857399999));
#257649=CARTESIAN_POINT('Ctrl Pts',(-10.2687226760001,15.2,2.66247664899999));
#257650=CARTESIAN_POINT('Ctrl Pts',(-10.2687226760001,11.6,2.66247664899998));
#257651=CARTESIAN_POINT('Ctrl Pts',(-10.2708526900001,15.2,2.66253300899999));
#257652=CARTESIAN_POINT('Ctrl Pts',(-10.2708526900001,11.6,2.66253300899999));
#257653=CARTESIAN_POINT('Ctrl Pts',(-10.2729895460001,15.2,2.66258764499998));
#257654=CARTESIAN_POINT('Ctrl Pts',(-10.2729895460001,11.6,2.66258764499998));
#257655=CARTESIAN_POINT('Ctrl Pts',(-10.2751332320001,15.2,2.66264054599999));
#257656=CARTESIAN_POINT('Ctrl Pts',(-10.2751332320001,11.6,2.66264054599999));
#257657=CARTESIAN_POINT('Ctrl Pts',(-10.2772837330001,15.2,2.66269169899999));
#257658=CARTESIAN_POINT('Ctrl Pts',(-10.2772837330001,11.6,2.66269169899999));
#257659=CARTESIAN_POINT('Ctrl Pts',(-10.2794410340001,15.2,2.66274109399999));
#257660=CARTESIAN_POINT('Ctrl Pts',(-10.2794410340001,11.6,2.66274109399998));
#257661=CARTESIAN_POINT('Ctrl Pts',(-10.2816051240001,15.2,2.66278871999998));
#257662=CARTESIAN_POINT('Ctrl Pts',(-10.2816051240001,11.6,2.66278871999998));
#257663=CARTESIAN_POINT('Ctrl Pts',(-10.2837759870001,15.2,2.66283456499998));
#257664=CARTESIAN_POINT('Ctrl Pts',(-10.2837759870001,11.6,2.66283456499998));
#257665=CARTESIAN_POINT('Ctrl Pts',(-10.2859536100001,15.2,2.66287861899999));
#257666=CARTESIAN_POINT('Ctrl Pts',(-10.2859536100001,11.6,2.66287861899999));
#257667=CARTESIAN_POINT('Ctrl Pts',(-10.2881379790001,15.2,2.66292087099998));
#257668=CARTESIAN_POINT('Ctrl Pts',(-10.2881379790001,11.6,2.66292087099998));
#257669=CARTESIAN_POINT('Ctrl Pts',(-10.2903290790001,15.2,2.66296131099999));
#257670=CARTESIAN_POINT('Ctrl Pts',(-10.2903290790001,11.6,2.66296131099998));
#257671=CARTESIAN_POINT('Ctrl Pts',(-10.2925268990001,15.2,2.66299992599999));
#257672=CARTESIAN_POINT('Ctrl Pts',(-10.2925268990001,11.6,2.66299992599999));
#257673=CARTESIAN_POINT('Ctrl Pts',(-10.2947314240001,15.2,2.66303670599999));
#257674=CARTESIAN_POINT('Ctrl Pts',(-10.2947314240001,11.6,2.66303670599999));
#257675=CARTESIAN_POINT('Ctrl Pts',(-10.2969426400001,15.2,2.66307164099998));
#257676=CARTESIAN_POINT('Ctrl Pts',(-10.2969426400001,11.6,2.66307164099998));
#257677=CARTESIAN_POINT('Ctrl Pts',(-10.2991605340001,15.2,2.66310471999999));
#257678=CARTESIAN_POINT('Ctrl Pts',(-10.2991605340001,11.6,2.66310471999999));
#257679=CARTESIAN_POINT('Ctrl Pts',(-10.3013850920001,15.2,2.66313593099999));
#257680=CARTESIAN_POINT('Ctrl Pts',(-10.3013850920001,11.6,2.66313593099999));
#257681=CARTESIAN_POINT('Ctrl Pts',(-10.3036163000001,15.2,2.66316526499998));
#257682=CARTESIAN_POINT('Ctrl Pts',(-10.3036163000001,11.6,2.66316526499998));
#257683=CARTESIAN_POINT('Ctrl Pts',(-10.3058541460001,15.2,2.66319271199999));
#257684=CARTESIAN_POINT('Ctrl Pts',(-10.3058541460001,11.6,2.66319271199999));
#257685=CARTESIAN_POINT('Ctrl Pts',(-10.3080986170001,15.2,2.66321825899999));
#257686=CARTESIAN_POINT('Ctrl Pts',(-10.3080986170001,11.6,2.66321825899999));
#257687=CARTESIAN_POINT('Ctrl Pts',(-10.3103496970001,15.2,2.66324189799998));
#257688=CARTESIAN_POINT('Ctrl Pts',(-10.3103496970001,11.6,2.66324189799998));
#257689=CARTESIAN_POINT('Ctrl Pts',(-10.3126073740001,15.2,2.66326361599998));
#257690=CARTESIAN_POINT('Ctrl Pts',(-10.3126073740001,11.6,2.66326361599998));
#257691=CARTESIAN_POINT('Ctrl Pts',(-10.3148716350001,15.2,2.66328340499999));
#257692=CARTESIAN_POINT('Ctrl Pts',(-10.3148716350001,11.6,2.66328340499999));
#257693=CARTESIAN_POINT('Ctrl Pts',(-10.3171424670001,15.2,2.66330125299999));
#257694=CARTESIAN_POINT('Ctrl Pts',(-10.3171424670001,11.6,2.66330125299999));
#257695=CARTESIAN_POINT('Ctrl Pts',(-10.3194198560001,15.2,2.66331714999998));
#257696=CARTESIAN_POINT('Ctrl Pts',(-10.3194198560001,11.6,2.66331714999998));
#257697=CARTESIAN_POINT('Ctrl Pts',(-10.3217037880001,15.2,2.66333108599999));
#257698=CARTESIAN_POINT('Ctrl Pts',(-10.3217037880001,11.6,2.66333108599999));
#257699=CARTESIAN_POINT('Ctrl Pts',(-10.3239942520001,15.2,2.66334304999998));
#257700=CARTESIAN_POINT('Ctrl Pts',(-10.3239942520001,11.6,2.66334304999998));
#257701=CARTESIAN_POINT('Ctrl Pts',(-10.3262912330001,15.2,2.66335303299999));
#257702=CARTESIAN_POINT('Ctrl Pts',(-10.3262912330001,11.6,2.66335303299999));
#257703=CARTESIAN_POINT('Ctrl Pts',(-10.3285947190001,15.2,2.66336102499999));
#257704=CARTESIAN_POINT('Ctrl Pts',(-10.3285947190001,11.6,2.66336102499999));
#257705=CARTESIAN_POINT('Ctrl Pts',(-10.3309046950001,15.2,2.66336701399998));
#257706=CARTESIAN_POINT('Ctrl Pts',(-10.3309046950001,11.6,2.66336701399998));
#257707=CARTESIAN_POINT('Ctrl Pts',(-10.3332211510001,15.2,2.66337099099999));
#257708=CARTESIAN_POINT('Ctrl Pts',(-10.3332211510001,11.6,2.66337099099999));
#257709=CARTESIAN_POINT('Ctrl Pts',(-10.3355440700001,15.2,2.66337294499999));
#257710=CARTESIAN_POINT('Ctrl Pts',(-10.3355440700001,11.6,2.66337294499999));
#257711=CARTESIAN_POINT('Ctrl Pts',(-10.3378734430001,15.2,2.66337286799998));
#257712=CARTESIAN_POINT('Ctrl Pts',(-10.3378734430001,11.6,2.66337286799998));
#257713=CARTESIAN_POINT('Ctrl Pts',(-10.3402092540001,15.2,2.66337074899998));
#257714=CARTESIAN_POINT('Ctrl Pts',(-10.3402092540001,11.6,2.66337074899998));
#257715=CARTESIAN_POINT('Ctrl Pts',(-10.3425514920001,15.2,2.66336657699998));
#257716=CARTESIAN_POINT('Ctrl Pts',(-10.3425514920001,11.6,2.66336657699998));
#257717=CARTESIAN_POINT('Ctrl Pts',(-10.3449001440001,15.2,2.66336034399998));
#257718=CARTESIAN_POINT('Ctrl Pts',(-10.3449001440001,11.6,2.66336034399998));
#257719=CARTESIAN_POINT('Ctrl Pts',(-10.3472551960001,15.2,2.66335203799999));
#257720=CARTESIAN_POINT('Ctrl Pts',(-10.3472551960001,11.6,2.66335203799999));
#257721=CARTESIAN_POINT('Ctrl Pts',(-10.3496166340001,15.2,2.66334165099998));
#257722=CARTESIAN_POINT('Ctrl Pts',(-10.3496166340001,11.6,2.66334165099998));
#257723=CARTESIAN_POINT('Ctrl Pts',(-10.3519844490001,15.2,2.66332917099999));
#257724=CARTESIAN_POINT('Ctrl Pts',(-10.3519844490001,11.6,2.66332917099999));
#257725=CARTESIAN_POINT('Ctrl Pts',(-10.3543586250001,15.2,2.66331458999999));
#257726=CARTESIAN_POINT('Ctrl Pts',(-10.3543586250001,11.6,2.66331458999999));
#257727=CARTESIAN_POINT('Ctrl Pts',(-10.3567391510001,15.2,2.66329789899999));
#257728=CARTESIAN_POINT('Ctrl Pts',(-10.3567391510001,11.6,2.66329789899999));
#257729=CARTESIAN_POINT('Ctrl Pts',(-10.3591260120001,15.2,2.66327908699999));
#257730=CARTESIAN_POINT('Ctrl Pts',(-10.3591260120001,11.6,2.66327908699999));
#257731=CARTESIAN_POINT('Ctrl Pts',(-10.3615191980001,15.2,2.66325814399998));
#257732=CARTESIAN_POINT('Ctrl Pts',(-10.3615191980001,11.6,2.66325814399998));
#257733=CARTESIAN_POINT('Ctrl Pts',(-10.3639186950001,15.2,2.66323506099998));
#257734=CARTESIAN_POINT('Ctrl Pts',(-10.3639186950001,11.6,2.66323506099998));
#257735=CARTESIAN_POINT('Ctrl Pts',(-10.3663244900001,15.2,2.66320982799999));
#257736=CARTESIAN_POINT('Ctrl Pts',(-10.3663244900001,11.6,2.66320982799999));
#257737=CARTESIAN_POINT('Ctrl Pts',(-10.3687365710001,15.2,2.66318243599999));
#257738=CARTESIAN_POINT('Ctrl Pts',(-10.3687365710001,11.6,2.66318243599999));
#257739=CARTESIAN_POINT('Ctrl Pts',(-10.3711549250001,15.2,2.66315287599999));
#257740=CARTESIAN_POINT('Ctrl Pts',(-10.3711549250001,11.6,2.66315287599999));
#257741=CARTESIAN_POINT('Ctrl Pts',(-10.3735795410001,15.2,2.66312113599999));
#257742=CARTESIAN_POINT('Ctrl Pts',(-10.3735795410001,11.6,2.66312113599999));
#257743=CARTESIAN_POINT('Ctrl Pts',(-10.3760104050001,15.2,2.66308720999999));
#257744=CARTESIAN_POINT('Ctrl Pts',(-10.3760104050001,11.6,2.66308720999999));
#257745=CARTESIAN_POINT('Ctrl Pts',(-10.3784475030001,15.2,2.66305108599998));
#257746=CARTESIAN_POINT('Ctrl Pts',(-10.3784475030001,11.6,2.66305108599998));
#257747=CARTESIAN_POINT('Ctrl Pts',(-10.3808908260001,15.2,2.66301275499998));
#257748=CARTESIAN_POINT('Ctrl Pts',(-10.3808908260001,11.6,2.66301275499998));
#257749=CARTESIAN_POINT('Ctrl Pts',(-10.3833403590001,15.2,2.66297220899999));
#257750=CARTESIAN_POINT('Ctrl Pts',(-10.3833403590001,11.6,2.66297220899998));
#257751=CARTESIAN_POINT('Ctrl Pts',(-10.3857960910001,15.2,2.66292943799999));
#257752=CARTESIAN_POINT('Ctrl Pts',(-10.3857960910001,11.6,2.66292943799999));
#257753=CARTESIAN_POINT('Ctrl Pts',(-10.3882580090001,15.2,2.66288443299998));
#257754=CARTESIAN_POINT('Ctrl Pts',(-10.3882580090001,11.6,2.66288443299998));
#257755=CARTESIAN_POINT('Ctrl Pts',(-10.3907261000001,15.2,2.66283718399999));
#257756=CARTESIAN_POINT('Ctrl Pts',(-10.3907261000001,11.6,2.66283718399999));
#257757=CARTESIAN_POINT('Ctrl Pts',(-10.3932003530001,15.2,2.66278768199999));
#257758=CARTESIAN_POINT('Ctrl Pts',(-10.3932003530001,11.6,2.66278768199999));
#257759=CARTESIAN_POINT('Ctrl Pts',(-10.3956807540001,15.2,2.66273591899999));
#257760=CARTESIAN_POINT('Ctrl Pts',(-10.3956807540001,11.6,2.66273591899999));
#257761=CARTESIAN_POINT('Ctrl Pts',(-10.3981672930001,15.2,2.66268188399999));
#257762=CARTESIAN_POINT('Ctrl Pts',(-10.3981672930001,11.6,2.66268188399999));
#257763=CARTESIAN_POINT('Ctrl Pts',(-10.4006599560001,15.2,2.66262556899999));
#257764=CARTESIAN_POINT('Ctrl Pts',(-10.4006599560001,11.6,2.66262556899999));
#257765=CARTESIAN_POINT('Ctrl Pts',(-10.4031587310001,15.2,2.66256696399999));
#257766=CARTESIAN_POINT('Ctrl Pts',(-10.4031587310001,11.6,2.66256696399999));
#257767=CARTESIAN_POINT('Ctrl Pts',(-10.4056636070001,15.2,2.66250606099998));
#257768=CARTESIAN_POINT('Ctrl Pts',(-10.4056636070001,11.6,2.66250606099998));
#257769=CARTESIAN_POINT('Ctrl Pts',(-10.4081745700001,15.2,2.66244285099998));
#257770=CARTESIAN_POINT('Ctrl Pts',(-10.4081745700001,11.6,2.66244285099998));
#257771=CARTESIAN_POINT('Ctrl Pts',(-10.4106916090001,15.2,2.66237732499999));
#257772=CARTESIAN_POINT('Ctrl Pts',(-10.4106916090001,11.6,2.66237732499999));
#257773=CARTESIAN_POINT('Ctrl Pts',(-10.4132147120001,15.2,2.66230947299999));
#257774=CARTESIAN_POINT('Ctrl Pts',(-10.4132147120001,11.6,2.66230947299999));
#257775=CARTESIAN_POINT('Ctrl Pts',(-10.4157438670001,15.2,2.66223928799998));
#257776=CARTESIAN_POINT('Ctrl Pts',(-10.4157438670001,11.6,2.66223928799998));
#257777=CARTESIAN_POINT('Ctrl Pts',(-10.4182790610001,15.2,2.66216675899998));
#257778=CARTESIAN_POINT('Ctrl Pts',(-10.4182790610001,11.6,2.66216675899998));
#257779=CARTESIAN_POINT('Ctrl Pts',(-10.4208202830001,15.2,2.66209187899998));
#257780=CARTESIAN_POINT('Ctrl Pts',(-10.4208202830001,11.6,2.66209187899998));
#257781=CARTESIAN_POINT('Ctrl Pts',(-10.4233675200001,15.2,2.66201463899999));
#257782=CARTESIAN_POINT('Ctrl Pts',(-10.4233675200001,11.6,2.66201463899999));
#257783=CARTESIAN_POINT('Ctrl Pts',(-10.4259207610001,15.2,2.66193502899998));
#257784=CARTESIAN_POINT('Ctrl Pts',(-10.4259207610001,11.6,2.66193502899998));
#257785=CARTESIAN_POINT('Ctrl Pts',(-10.4284799940001,15.2,2.66185303999999));
#257786=CARTESIAN_POINT('Ctrl Pts',(-10.4284799940001,11.6,2.66185303999999));
#257787=CARTESIAN_POINT('Ctrl Pts',(-10.4310452060001,15.2,2.66176866499999));
#257788=CARTESIAN_POINT('Ctrl Pts',(-10.4310452060001,11.6,2.66176866499999));
#257789=CARTESIAN_POINT('Ctrl Pts',(-10.4336163860001,15.2,2.66168189499999));
#257790=CARTESIAN_POINT('Ctrl Pts',(-10.4336163860001,11.6,2.66168189499999));
#257791=CARTESIAN_POINT('Ctrl Pts',(-10.4361935220001,15.2,2.66159271999998));
#257792=CARTESIAN_POINT('Ctrl Pts',(-10.4361935220001,11.6,2.66159271999998));
#257793=CARTESIAN_POINT('Ctrl Pts',(-10.4387766020001,15.2,2.66150113299998));
#257794=CARTESIAN_POINT('Ctrl Pts',(-10.4387766020001,11.6,2.66150113299998));
#257795=CARTESIAN_POINT('Ctrl Pts',(-10.4413656150001,15.2,2.66140712399999));
#257796=CARTESIAN_POINT('Ctrl Pts',(-10.4413656150001,11.6,2.66140712399999));
#257797=CARTESIAN_POINT('Ctrl Pts',(-10.4439605480001,15.2,2.66131068599999));
#257798=CARTESIAN_POINT('Ctrl Pts',(-10.4439605480001,11.6,2.66131068599999));
#257799=CARTESIAN_POINT('Ctrl Pts',(-10.4465613900001,15.2,2.66121180899999));
#257800=CARTESIAN_POINT('Ctrl Pts',(-10.4465613900001,11.6,2.66121180899999));
#257801=CARTESIAN_POINT('Ctrl Pts',(-10.4491681290001,15.2,2.66111048599999));
#257802=CARTESIAN_POINT('Ctrl Pts',(-10.4491681290001,11.6,2.66111048599999));
#257803=CARTESIAN_POINT('Ctrl Pts',(-10.4517807530001,15.2,2.66100670699998));
#257804=CARTESIAN_POINT('Ctrl Pts',(-10.4517807530001,11.6,2.66100670699998));
#257805=CARTESIAN_POINT('Ctrl Pts',(-10.4543992500001,15.2,2.66090046499999));
#257806=CARTESIAN_POINT('Ctrl Pts',(-10.4543992500001,11.6,2.66090046499999));
#257807=CARTESIAN_POINT('Ctrl Pts',(-10.4570236090001,15.2,2.66079174999999));
#257808=CARTESIAN_POINT('Ctrl Pts',(-10.4570236090001,11.6,2.66079174999999));
#257809=CARTESIAN_POINT('Ctrl Pts',(-10.4596538190001,15.2,2.66068055499999));
#257810=CARTESIAN_POINT('Ctrl Pts',(-10.4596538190001,11.6,2.66068055499999));
#257811=CARTESIAN_POINT('Ctrl Pts',(-10.4622898670001,15.2,2.66056687199999));
#257812=CARTESIAN_POINT('Ctrl Pts',(-10.4622898670001,11.6,2.66056687199998));
#257813=CARTESIAN_POINT('Ctrl Pts',(-10.4649317430001,15.2,2.66045069099999));
#257814=CARTESIAN_POINT('Ctrl Pts',(-10.4649317430001,11.6,2.66045069099999));
#257815=CARTESIAN_POINT('Ctrl Pts',(-10.4675794330001,15.2,2.66033200499999));
#257816=CARTESIAN_POINT('Ctrl Pts',(-10.4675794330001,11.6,2.66033200499999));
#257817=CARTESIAN_POINT('Ctrl Pts',(-10.4702329280001,15.2,2.66021080599998));
#257818=CARTESIAN_POINT('Ctrl Pts',(-10.4702329280001,11.6,2.66021080599998));
#257819=CARTESIAN_POINT('Ctrl Pts',(-10.4728922150001,15.2,2.66008708399998));
#257820=CARTESIAN_POINT('Ctrl Pts',(-10.4728922150001,11.6,2.66008708399998));
#257821=CARTESIAN_POINT('Ctrl Pts',(-10.4755572830001,15.2,2.65996083299999));
#257822=CARTESIAN_POINT('Ctrl Pts',(-10.4755572830001,11.6,2.65996083299999));
#257823=CARTESIAN_POINT('Ctrl Pts',(-10.4782281200001,15.2,2.65983204299998));
#257824=CARTESIAN_POINT('Ctrl Pts',(-10.4782281200001,11.6,2.65983204299998));
#257825=CARTESIAN_POINT('Ctrl Pts',(-10.4809047160001,15.2,2.65970070699999));
#257826=CARTESIAN_POINT('Ctrl Pts',(-10.4809047160001,11.6,2.65970070699999));
#257827=CARTESIAN_POINT('Ctrl Pts',(-10.4835870570001,15.2,2.65956681699999));
#257828=CARTESIAN_POINT('Ctrl Pts',(-10.4835870570001,11.6,2.65956681699999));
#257829=CARTESIAN_POINT('Ctrl Pts',(-10.4862751350001,15.2,2.65943036399998));
#257830=CARTESIAN_POINT('Ctrl Pts',(-10.4862751350001,11.6,2.65943036399998));
#257831=CARTESIAN_POINT('Ctrl Pts',(-10.4889689350001,15.2,2.65929134099999));
#257832=CARTESIAN_POINT('Ctrl Pts',(-10.4889689350001,11.6,2.65929134099998));
#257833=CARTESIAN_POINT('Ctrl Pts',(-10.4916684480001,15.2,2.65914974099999));
#257834=CARTESIAN_POINT('Ctrl Pts',(-10.4916684480001,11.6,2.65914974099999));
#257835=CARTESIAN_POINT('Ctrl Pts',(-10.4943736620001,15.2,2.65900555299999));
#257836=CARTESIAN_POINT('Ctrl Pts',(-10.4943736620001,11.6,2.65900555299999));
#257837=CARTESIAN_POINT('Ctrl Pts',(-10.4970845660001,15.2,2.65885877099999));
#257838=CARTESIAN_POINT('Ctrl Pts',(-10.4970845660001,11.6,2.65885877099999));
#257839=CARTESIAN_POINT('Ctrl Pts',(-10.4998011490001,15.2,2.65870938599999));
#257840=CARTESIAN_POINT('Ctrl Pts',(-10.4998011490001,11.6,2.65870938599999));
#257841=CARTESIAN_POINT('Ctrl Pts',(-10.5025233980001,15.2,2.65855739099998));
#257842=CARTESIAN_POINT('Ctrl Pts',(-10.5025233980001,11.6,2.65855739099998));
#257843=CARTESIAN_POINT('Ctrl Pts',(-10.5052513030001,15.2,2.65840277799998));
#257844=CARTESIAN_POINT('Ctrl Pts',(-10.5052513030001,11.6,2.65840277799998));
#257845=CARTESIAN_POINT('Ctrl Pts',(-10.5079848540001,15.2,2.65824553999998));
#257846=CARTESIAN_POINT('Ctrl Pts',(-10.5079848540001,11.6,2.65824553999998));
#257847=CARTESIAN_POINT('Ctrl Pts',(-10.5107240380001,15.2,2.65808566799999));
#257848=CARTESIAN_POINT('Ctrl Pts',(-10.5107240380001,11.6,2.65808566799999));
#257849=CARTESIAN_POINT('Ctrl Pts',(-10.5134688430001,15.2,2.65792315499999));
#257850=CARTESIAN_POINT('Ctrl Pts',(-10.5134688430001,11.6,2.65792315499999));
#257851=CARTESIAN_POINT('Ctrl Pts',(-10.5162192600001,15.2,2.65775799199999));
#257852=CARTESIAN_POINT('Ctrl Pts',(-10.5162192600001,11.6,2.65775799199999));
#257853=CARTESIAN_POINT('Ctrl Pts',(-10.5189752770001,15.2,2.65759017199999));
#257854=CARTESIAN_POINT('Ctrl Pts',(-10.5189752770001,11.6,2.65759017199999));
#257855=CARTESIAN_POINT('Ctrl Pts',(-10.5217368840001,15.2,2.65741968699999));
#257856=CARTESIAN_POINT('Ctrl Pts',(-10.5217368840001,11.6,2.65741968699999));
#257857=CARTESIAN_POINT('Ctrl Pts',(-10.5245040670001,15.2,2.65724653099999));
#257858=CARTESIAN_POINT('Ctrl Pts',(-10.5245040670001,11.6,2.65724653099999));
#257859=CARTESIAN_POINT('Ctrl Pts',(-10.5272768180001,15.2,2.65707069399999));
#257860=CARTESIAN_POINT('Ctrl Pts',(-10.5272768180001,11.6,2.65707069399999));
#257861=CARTESIAN_POINT('Ctrl Pts',(-10.5300551240001,15.2,2.65689216899998));
#257862=CARTESIAN_POINT('Ctrl Pts',(-10.5300551240001,11.6,2.65689216899998));
#257863=CARTESIAN_POINT('Ctrl Pts',(-10.5328389750001,15.2,2.65671094999998));
#257864=CARTESIAN_POINT('Ctrl Pts',(-10.5328389750001,11.6,2.65671094999998));
#257865=CARTESIAN_POINT('Ctrl Pts',(-10.5356283600001,15.2,2.65652702799999));
#257866=CARTESIAN_POINT('Ctrl Pts',(-10.5356283600001,11.6,2.65652702799999));
#257867=CARTESIAN_POINT('Ctrl Pts',(-10.5384232670001,15.2,2.65634039599998));
#257868=CARTESIAN_POINT('Ctrl Pts',(-10.5384232670001,11.6,2.65634039599998));
#257869=CARTESIAN_POINT('Ctrl Pts',(-10.5412236860001,15.2,2.65615104599998));
#257870=CARTESIAN_POINT('Ctrl Pts',(-10.5412236860001,11.6,2.65615104599998));
#257871=CARTESIAN_POINT('Ctrl Pts',(-10.5440296060001,15.2,2.65595896999999));
#257872=CARTESIAN_POINT('Ctrl Pts',(-10.5440296060001,11.6,2.65595896999999));
#257873=CARTESIAN_POINT('Ctrl Pts',(-10.5468410160001,15.2,2.65576416199998));
#257874=CARTESIAN_POINT('Ctrl Pts',(-10.5468410160001,11.6,2.65576416199998));
#257875=CARTESIAN_POINT('Ctrl Pts',(-10.5496579050001,15.2,2.65556661399999));
#257876=CARTESIAN_POINT('Ctrl Pts',(-10.5496579050001,11.6,2.65556661399999));
#257877=CARTESIAN_POINT('Ctrl Pts',(-10.5524802620001,15.2,2.65536631799999));
#257878=CARTESIAN_POINT('Ctrl Pts',(-10.5524802620001,11.6,2.65536631799998));
#257879=CARTESIAN_POINT('Ctrl Pts',(-10.5553080750001,15.2,2.65516326799998));
#257880=CARTESIAN_POINT('Ctrl Pts',(-10.5553080750001,11.6,2.65516326799998));
#257881=CARTESIAN_POINT('Ctrl Pts',(-10.5581413360001,15.2,2.65495745499998));
#257882=CARTESIAN_POINT('Ctrl Pts',(-10.5581413360001,11.6,2.65495745499998));
#257883=CARTESIAN_POINT('Ctrl Pts',(-10.5609800320001,15.2,2.65474887199999));
#257884=CARTESIAN_POINT('Ctrl Pts',(-10.5609800320001,11.6,2.65474887199999));
#257885=CARTESIAN_POINT('Ctrl Pts',(-10.5638241530001,15.2,2.65453751199999));
#257886=CARTESIAN_POINT('Ctrl Pts',(-10.5638241530001,11.6,2.65453751199999));
#257887=CARTESIAN_POINT('Ctrl Pts',(-10.5666736870001,15.2,2.65432336899998));
#257888=CARTESIAN_POINT('Ctrl Pts',(-10.5666736870001,11.6,2.65432336899998));
#257889=CARTESIAN_POINT('Ctrl Pts',(-10.5695286260001,15.2,2.65410643399999));
#257890=CARTESIAN_POINT('Ctrl Pts',(-10.5695286260001,11.6,2.65410643399999));
#257891=CARTESIAN_POINT('Ctrl Pts',(-10.5723889570001,15.2,2.65388669999999));
#257892=CARTESIAN_POINT('Ctrl Pts',(-10.5723889570001,11.6,2.65388669999999));
#257893=CARTESIAN_POINT('Ctrl Pts',(-10.5752546690001,15.2,2.65366416099998));
#257894=CARTESIAN_POINT('Ctrl Pts',(-10.5752546690001,11.6,2.65366416099998));
#257895=CARTESIAN_POINT('Ctrl Pts',(-10.5781257530001,15.2,2.65343880799998));
#257896=CARTESIAN_POINT('Ctrl Pts',(-10.5781257530001,11.6,2.65343880799998));
#257897=CARTESIAN_POINT('Ctrl Pts',(-10.5810021970001,15.2,2.65321063499999));
#257898=CARTESIAN_POINT('Ctrl Pts',(-10.5810021970001,11.6,2.65321063499999));
#257899=CARTESIAN_POINT('Ctrl Pts',(-10.5838839910001,15.2,2.65297963599998));
#257900=CARTESIAN_POINT('Ctrl Pts',(-10.5838839910001,11.6,2.65297963599998));
#257901=CARTESIAN_POINT('Ctrl Pts',(-10.5867711240001,15.2,2.65274580099998));
#257902=CARTESIAN_POINT('Ctrl Pts',(-10.5867711240001,11.6,2.65274580099998));
#257903=CARTESIAN_POINT('Ctrl Pts',(-10.5896635860001,15.2,2.65250912599999));
#257904=CARTESIAN_POINT('Ctrl Pts',(-10.5896635860001,11.6,2.65250912599999));
#257905=CARTESIAN_POINT('Ctrl Pts',(-10.5925613650001,15.2,2.65226960099999));
#257906=CARTESIAN_POINT('Ctrl Pts',(-10.5925613650001,11.6,2.65226960099999));
#257907=CARTESIAN_POINT('Ctrl Pts',(-10.5954644520001,15.2,2.65202722099998));
#257908=CARTESIAN_POINT('Ctrl Pts',(-10.5954644520001,11.6,2.65202722099998));
#257909=CARTESIAN_POINT('Ctrl Pts',(-10.5983728360001,15.2,2.65178197799998));
#257910=CARTESIAN_POINT('Ctrl Pts',(-10.5983728360001,11.6,2.65178197799998));
#257911=CARTESIAN_POINT('Ctrl Pts',(-10.6012865070001,15.2,2.65153386599999));
#257912=CARTESIAN_POINT('Ctrl Pts',(-10.6012865070001,11.6,2.65153386599999));
#257913=CARTESIAN_POINT('Ctrl Pts',(-10.6042054530001,15.2,2.65128287899999));
#257914=CARTESIAN_POINT('Ctrl Pts',(-10.6042054530001,11.6,2.65128287899999));
#257915=CARTESIAN_POINT('Ctrl Pts',(-10.6071296640001,15.2,2.65102900599998));
#257916=CARTESIAN_POINT('Ctrl Pts',(-10.6071296640001,11.6,2.65102900599998));
#257917=CARTESIAN_POINT('Ctrl Pts',(-10.6100591290001,15.2,2.65077224399998));
#257918=CARTESIAN_POINT('Ctrl Pts',(-10.6100591290001,11.6,2.65077224399998));
#257919=CARTESIAN_POINT('Ctrl Pts',(-10.6129938410001,15.2,2.65051258599998));
#257920=CARTESIAN_POINT('Ctrl Pts',(-10.6129938410001,11.6,2.65051258599998));
#257921=CARTESIAN_POINT('Ctrl Pts',(-10.6159337850001,15.2,2.65025002199998));
#257922=CARTESIAN_POINT('Ctrl Pts',(-10.6159337850001,11.6,2.65025002199998));
#257923=CARTESIAN_POINT('Ctrl Pts',(-10.6188789520001,15.2,2.64998454799999));
#257924=CARTESIAN_POINT('Ctrl Pts',(-10.6188789520001,11.6,2.64998454799999));
#257925=CARTESIAN_POINT('Ctrl Pts',(-10.6218293330001,15.2,2.64971615699999));
#257926=CARTESIAN_POINT('Ctrl Pts',(-10.6218293330001,11.6,2.64971615699999));
#257927=CARTESIAN_POINT('Ctrl Pts',(-10.6247849170001,15.2,2.64944483999999));
#257928=CARTESIAN_POINT('Ctrl Pts',(-10.6247849170001,11.6,2.64944483999999));
#257929=CARTESIAN_POINT('Ctrl Pts',(-10.6277456920001,15.2,2.64917059199998));
#257930=CARTESIAN_POINT('Ctrl Pts',(-10.6277456920001,11.6,2.64917059199998));
#257931=CARTESIAN_POINT('Ctrl Pts',(-10.6307116510001,15.2,2.64889340699998));
#257932=CARTESIAN_POINT('Ctrl Pts',(-10.6307116510001,11.6,2.64889340699998));
#257933=CARTESIAN_POINT('Ctrl Pts',(-10.6336827810001,15.2,2.64861327699998));
#257934=CARTESIAN_POINT('Ctrl Pts',(-10.6336827810001,11.6,2.64861327699998));
#257935=CARTESIAN_POINT('Ctrl Pts',(-10.6366590710001,15.2,2.64833019599998));
#257936=CARTESIAN_POINT('Ctrl Pts',(-10.6366590710001,11.6,2.64833019599998));
#257937=CARTESIAN_POINT('Ctrl Pts',(-10.6396405130001,15.2,2.64804415599999));
#257938=CARTESIAN_POINT('Ctrl Pts',(-10.6396405130001,11.6,2.64804415599999));
#257939=CARTESIAN_POINT('Ctrl Pts',(-10.6426270960001,15.2,2.64775515199998));
#257940=CARTESIAN_POINT('Ctrl Pts',(-10.6426270960001,11.6,2.64775515199998));
#257941=CARTESIAN_POINT('Ctrl Pts',(-10.6456188090001,15.2,2.64746317599998));
#257942=CARTESIAN_POINT('Ctrl Pts',(-10.6456188090001,11.6,2.64746317599998));
#257943=CARTESIAN_POINT('Ctrl Pts',(-10.6486156430001,15.2,2.64716822299999));
#257944=CARTESIAN_POINT('Ctrl Pts',(-10.6486156430001,11.6,2.64716822299999));
#257945=CARTESIAN_POINT('Ctrl Pts',(-10.6516175860001,15.2,2.64687028499999));
#257946=CARTESIAN_POINT('Ctrl Pts',(-10.6516175860001,11.6,2.64687028499999));
#257947=CARTESIAN_POINT('Ctrl Pts',(-10.6546246300001,15.2,2.64656935599999));
#257948=CARTESIAN_POINT('Ctrl Pts',(-10.6546246300001,11.6,2.64656935599999));
#257949=CARTESIAN_POINT('Ctrl Pts',(-10.6576367620001,15.2,2.64626542899999));
#257950=CARTESIAN_POINT('Ctrl Pts',(-10.6576367620001,11.6,2.64626542899998));
#257951=CARTESIAN_POINT('Ctrl Pts',(-10.6606539750001,15.2,2.64595849899998));
#257952=CARTESIAN_POINT('Ctrl Pts',(-10.6606539750001,11.6,2.64595849899998));
#257953=CARTESIAN_POINT('Ctrl Pts',(-10.6636762580001,15.2,2.64564855699999));
#257954=CARTESIAN_POINT('Ctrl Pts',(-10.6636762580001,11.6,2.64564855699999));
#257955=CARTESIAN_POINT('Ctrl Pts',(-10.6667035990001,15.2,2.64533559999999));
#257956=CARTESIAN_POINT('Ctrl Pts',(-10.6667035990001,11.6,2.64533559999998));
#257957=CARTESIAN_POINT('Ctrl Pts',(-10.6697359890001,15.2,2.64501961799999));
#257958=CARTESIAN_POINT('Ctrl Pts',(-10.6697359890001,11.6,2.64501961799999));
#257959=CARTESIAN_POINT('Ctrl Pts',(-10.6727734180001,15.2,2.64470060699999));
#257960=CARTESIAN_POINT('Ctrl Pts',(-10.6727734180001,11.6,2.64470060699999));
#257961=CARTESIAN_POINT('Ctrl Pts',(-10.6758158770001,15.2,2.64437855899998));
#257962=CARTESIAN_POINT('Ctrl Pts',(-10.6758158770001,11.6,2.64437855899998));
#257963=CARTESIAN_POINT('Ctrl Pts',(-10.6788633540001,15.2,2.64405346799998));
#257964=CARTESIAN_POINT('Ctrl Pts',(-10.6788633540001,11.6,2.64405346799998));
#257965=CARTESIAN_POINT('Ctrl Pts',(-10.6819158400001,15.2,2.64372532899999));
#257966=CARTESIAN_POINT('Ctrl Pts',(-10.6819158400001,11.6,2.64372532899999));
#257967=CARTESIAN_POINT('Ctrl Pts',(-10.6849733260001,15.2,2.64339413399998));
#257968=CARTESIAN_POINT('Ctrl Pts',(-10.6849733260001,11.6,2.64339413399998));
#257969=CARTESIAN_POINT('Ctrl Pts',(-10.6880357990001,15.2,2.64305987699998));
#257970=CARTESIAN_POINT('Ctrl Pts',(-10.6880357990001,11.6,2.64305987699998));
#257971=CARTESIAN_POINT('Ctrl Pts',(-10.6911032520001,15.2,2.64272255199998));
#257972=CARTESIAN_POINT('Ctrl Pts',(-10.6911032520001,11.6,2.64272255199998));
#257973=CARTESIAN_POINT('Ctrl Pts',(-10.6941756740001,15.2,2.64238215299999));
#257974=CARTESIAN_POINT('Ctrl Pts',(-10.6941756740001,11.6,2.64238215299999));
#257975=CARTESIAN_POINT('Ctrl Pts',(-10.6972530540001,15.2,2.64203867399999));
#257976=CARTESIAN_POINT('Ctrl Pts',(-10.6972530540001,11.6,2.64203867399999));
#257977=CARTESIAN_POINT('Ctrl Pts',(-10.7003353830001,15.2,2.64169210799999));
#257978=CARTESIAN_POINT('Ctrl Pts',(-10.7003353830001,11.6,2.64169210799999));
#257979=CARTESIAN_POINT('Ctrl Pts',(-10.7034226510001,15.2,2.64134244899999));
#257980=CARTESIAN_POINT('Ctrl Pts',(-10.7034226510001,11.6,2.64134244899999));
#257981=CARTESIAN_POINT('Ctrl Pts',(-10.7065148490001,15.2,2.64098969099998));
#257982=CARTESIAN_POINT('Ctrl Pts',(-10.7065148490001,11.6,2.64098969099998));
#257983=CARTESIAN_POINT('Ctrl Pts',(-10.7096119650001,15.2,2.64063382799999));
#257984=CARTESIAN_POINT('Ctrl Pts',(-10.7096119650001,11.6,2.64063382799998));
#257985=CARTESIAN_POINT('Ctrl Pts',(-10.7127139910001,15.2,2.64027485299999));
#257986=CARTESIAN_POINT('Ctrl Pts',(-10.7127139910001,11.6,2.64027485299999));
#257987=CARTESIAN_POINT('Ctrl Pts',(-10.7158209160001,15.2,2.63991276099999));
#257988=CARTESIAN_POINT('Ctrl Pts',(-10.7158209160001,11.6,2.63991276099999));
#257989=CARTESIAN_POINT('Ctrl Pts',(-10.7189327310001,15.2,2.63954754399998));
#257990=CARTESIAN_POINT('Ctrl Pts',(-10.7189327310001,11.6,2.63954754399998));
#257991=CARTESIAN_POINT('Ctrl Pts',(-10.7220494270001,15.2,2.63917919899999));
#257992=CARTESIAN_POINT('Ctrl Pts',(-10.7220494270001,11.6,2.63917919899999));
#257993=CARTESIAN_POINT('Ctrl Pts',(-10.7251709920001,15.2,2.63880771699998));
#257994=CARTESIAN_POINT('Ctrl Pts',(-10.7251709920001,11.6,2.63880771699998));
#257995=CARTESIAN_POINT('Ctrl Pts',(-10.7282974160001,15.2,2.63843309399999));
#257996=CARTESIAN_POINT('Ctrl Pts',(-10.7282974160001,11.6,2.63843309399999));
#257997=CARTESIAN_POINT('Ctrl Pts',(-10.7314286920001,15.2,2.63805532299998));
#257998=CARTESIAN_POINT('Ctrl Pts',(-10.7314286920001,11.6,2.63805532299998));
#257999=CARTESIAN_POINT('Ctrl Pts',(-10.7345648080001,15.2,2.63767439799998));
#258000=CARTESIAN_POINT('Ctrl Pts',(-10.7345648080001,11.6,2.63767439799998));
#258001=CARTESIAN_POINT('Ctrl Pts',(-10.7377057560001,15.2,2.63729031299999));
#258002=CARTESIAN_POINT('Ctrl Pts',(-10.7377057560001,11.6,2.63729031299999));
#258003=CARTESIAN_POINT('Ctrl Pts',(-10.7408515230001,15.2,2.63690306299999));
#258004=CARTESIAN_POINT('Ctrl Pts',(-10.7408515230001,11.6,2.63690306299999));
#258005=CARTESIAN_POINT('Ctrl Pts',(-10.7440021030001,15.2,2.63651264099998));
#258006=CARTESIAN_POINT('Ctrl Pts',(-10.7440021030001,11.6,2.63651264099998));
#258007=CARTESIAN_POINT('Ctrl Pts',(-10.7471574850001,15.2,2.63611904099999));
#258008=CARTESIAN_POINT('Ctrl Pts',(-10.7471574850001,11.6,2.63611904099999));
#258009=CARTESIAN_POINT('Ctrl Pts',(-10.7503176590001,15.2,2.63572225799999));
#258010=CARTESIAN_POINT('Ctrl Pts',(-10.7503176590001,11.6,2.63572225799999));
#258011=CARTESIAN_POINT('Ctrl Pts',(-10.7534826150001,15.2,2.63532228399999));
#258012=CARTESIAN_POINT('Ctrl Pts',(-10.7534826150001,11.6,2.63532228399999));
#258013=CARTESIAN_POINT('Ctrl Pts',(-10.7566523440001,15.2,2.63491911599999));
#258014=CARTESIAN_POINT('Ctrl Pts',(-10.7566523440001,11.6,2.63491911599999));
#258015=CARTESIAN_POINT('Ctrl Pts',(-10.7598268370001,15.2,2.63451274799999));
#258016=CARTESIAN_POINT('Ctrl Pts',(-10.7598268370001,11.6,2.63451274799999));
#258017=CARTESIAN_POINT('Ctrl Pts',(-10.7630060830001,15.2,2.63410317099999));
#258018=CARTESIAN_POINT('Ctrl Pts',(-10.7630060830001,11.6,2.63410317099999));
#258019=CARTESIAN_POINT('Ctrl Pts',(-10.7661900720001,15.2,2.63369038299999));
#258020=CARTESIAN_POINT('Ctrl Pts',(-10.7661900720001,11.6,2.63369038299999));
#258021=CARTESIAN_POINT('Ctrl Pts',(-10.7693787950001,15.2,2.63327437599998));
#258022=CARTESIAN_POINT('Ctrl Pts',(-10.7693787950001,11.6,2.63327437599998));
#258023=CARTESIAN_POINT('Ctrl Pts',(-10.7725722440001,15.2,2.63285514399998));
#258024=CARTESIAN_POINT('Ctrl Pts',(-10.7725722440001,11.6,2.63285514399998));
#258025=CARTESIAN_POINT('Ctrl Pts',(-10.7757704090001,15.2,2.63243268299998));
#258026=CARTESIAN_POINT('Ctrl Pts',(-10.7757704090001,11.6,2.63243268299998));
#258027=CARTESIAN_POINT('Ctrl Pts',(-10.7789732780001,15.2,2.63200698499999));
#258028=CARTESIAN_POINT('Ctrl Pts',(-10.7789732780001,11.6,2.63200698499999));
#258029=CARTESIAN_POINT('Ctrl Pts',(-10.7821808440001,15.2,2.63157804699999));
#258030=CARTESIAN_POINT('Ctrl Pts',(-10.7821808440001,11.6,2.63157804699999));
#258031=CARTESIAN_POINT('Ctrl Pts',(-10.7853930960001,15.2,2.63114586099999));
#258032=CARTESIAN_POINT('Ctrl Pts',(-10.7853930960001,11.6,2.63114586099999));
#258033=CARTESIAN_POINT('Ctrl Pts',(-10.7886100260001,15.2,2.63071042299998));
#258034=CARTESIAN_POINT('Ctrl Pts',(-10.7886100260001,11.6,2.63071042299998));
#258035=CARTESIAN_POINT('Ctrl Pts',(-10.7918316230001,15.2,2.63027172599998));
#258036=CARTESIAN_POINT('Ctrl Pts',(-10.7918316230001,11.6,2.63027172599998));
#258037=CARTESIAN_POINT('Ctrl Pts',(-10.7950578790001,15.2,2.62982976599999));
#258038=CARTESIAN_POINT('Ctrl Pts',(-10.7950578790001,11.6,2.62982976599999));
#258039=CARTESIAN_POINT('Ctrl Pts',(-10.7982887820001,15.2,2.62938453599999));
#258040=CARTESIAN_POINT('Ctrl Pts',(-10.7982887820001,11.6,2.62938453599999));
#258041=CARTESIAN_POINT('Ctrl Pts',(-10.8015243260001,15.2,2.62893602899998));
#258042=CARTESIAN_POINT('Ctrl Pts',(-10.8015243260001,11.6,2.62893602899998));
#258043=CARTESIAN_POINT('Ctrl Pts',(-10.8047644990001,15.2,2.62848424299998));
#258044=CARTESIAN_POINT('Ctrl Pts',(-10.8047644990001,11.6,2.62848424299998));
#258045=CARTESIAN_POINT('Ctrl Pts',(-10.8080092930001,15.2,2.62802917099999));
#258046=CARTESIAN_POINT('Ctrl Pts',(-10.8080092930001,11.6,2.62802917099999));
#258047=CARTESIAN_POINT('Ctrl Pts',(-10.8112586980001,15.2,2.62757080599999));
#258048=CARTESIAN_POINT('Ctrl Pts',(-10.8112586980001,11.6,2.62757080599999));
#258049=CARTESIAN_POINT('Ctrl Pts',(-10.8145127050001,15.2,2.62710914399998));
#258050=CARTESIAN_POINT('Ctrl Pts',(-10.8145127050001,11.6,2.62710914399998));
#258051=CARTESIAN_POINT('Ctrl Pts',(-10.8177713030001,15.2,2.62664417899998));
#258052=CARTESIAN_POINT('Ctrl Pts',(-10.8177713030001,11.6,2.62664417899998));
#258053=CARTESIAN_POINT('Ctrl Pts',(-10.8210344850001,15.2,2.62617590599999));
#258054=CARTESIAN_POINT('Ctrl Pts',(-10.8210344850001,11.6,2.62617590599999));
#258055=CARTESIAN_POINT('Ctrl Pts',(-10.8243022400001,15.2,2.62570431899999));
#258056=CARTESIAN_POINT('Ctrl Pts',(-10.8243022400001,11.6,2.62570431899999));
#258057=CARTESIAN_POINT('Ctrl Pts',(-10.8275745600001,15.2,2.62522941199999));
#258058=CARTESIAN_POINT('Ctrl Pts',(-10.8275745600001,11.6,2.62522941199998));
#258059=CARTESIAN_POINT('Ctrl Pts',(-10.8308514350001,15.2,2.62475118099999));
#258060=CARTESIAN_POINT('Ctrl Pts',(-10.8308514350001,11.6,2.62475118099999));
#258061=CARTESIAN_POINT('Ctrl Pts',(-10.8341328550001,15.2,2.62426962099998));
#258062=CARTESIAN_POINT('Ctrl Pts',(-10.8341328550001,11.6,2.62426962099998));
#258063=CARTESIAN_POINT('Ctrl Pts',(-10.8374188130001,15.2,2.62378472399998));
#258064=CARTESIAN_POINT('Ctrl Pts',(-10.8374188130001,11.6,2.62378472399998));
#258065=CARTESIAN_POINT('Ctrl Pts',(-10.8407092960001,15.2,2.62329648699998));
#258066=CARTESIAN_POINT('Ctrl Pts',(-10.8407092960001,11.6,2.62329648699998));
#258067=CARTESIAN_POINT('Ctrl Pts',(-10.8440042990001,15.2,2.62280490399998));
#258068=CARTESIAN_POINT('Ctrl Pts',(-10.8440042990001,11.6,2.62280490399998));
#258069=CARTESIAN_POINT('Ctrl Pts',(-10.8473038090001,15.2,2.62230996899999));
#258070=CARTESIAN_POINT('Ctrl Pts',(-10.8473038090001,11.6,2.62230996899999));
#258071=CARTESIAN_POINT('Ctrl Pts',(-10.8506078190001,15.2,2.62181167699998));
#258072=CARTESIAN_POINT('Ctrl Pts',(-10.8506078190001,11.6,2.62181167699998));
#258073=CARTESIAN_POINT('Ctrl Pts',(-10.8539163200001,15.2,2.62131002399999));
#258074=CARTESIAN_POINT('Ctrl Pts',(-10.8539163200001,11.6,2.62131002399998));
#258075=CARTESIAN_POINT('Ctrl Pts',(-10.8572293010001,15.2,2.62080500299999));
#258076=CARTESIAN_POINT('Ctrl Pts',(-10.8572293010001,11.6,2.62080500299999));
#258077=CARTESIAN_POINT('Ctrl Pts',(-10.8605467540001,15.2,2.62029660899999));
#258078=CARTESIAN_POINT('Ctrl Pts',(-10.8605467540001,11.6,2.62029660899999));
#258079=CARTESIAN_POINT('Ctrl Pts',(-10.8638686700001,15.2,2.61978483699998));
#258080=CARTESIAN_POINT('Ctrl Pts',(-10.8638686700001,11.6,2.61978483699998));
#258081=CARTESIAN_POINT('Ctrl Pts',(-10.8671950400001,15.2,2.61926968199998));
#258082=CARTESIAN_POINT('Ctrl Pts',(-10.8671950400001,11.6,2.61926968199998));
#258083=CARTESIAN_POINT('Ctrl Pts',(-10.8705258540001,15.2,2.61875113999999));
#258084=CARTESIAN_POINT('Ctrl Pts',(-10.8705258540001,11.6,2.61875113999999));
#258085=CARTESIAN_POINT('Ctrl Pts',(-10.8738611030001,15.2,2.61822920299998));
#258086=CARTESIAN_POINT('Ctrl Pts',(-10.8738611030001,11.6,2.61822920299998));
#258087=CARTESIAN_POINT('Ctrl Pts',(-10.8772007790001,15.2,2.61770386799999));
#258088=CARTESIAN_POINT('Ctrl Pts',(-10.8772007790001,11.6,2.61770386799998));
#258089=CARTESIAN_POINT('Ctrl Pts',(-10.8805448720001,15.2,2.61717512899998));
#258090=CARTESIAN_POINT('Ctrl Pts',(-10.8805448720001,11.6,2.61717512899998));
#258091=CARTESIAN_POINT('Ctrl Pts',(-10.8838933720001,15.2,2.61664298099999));
#258092=CARTESIAN_POINT('Ctrl Pts',(-10.8838933720001,11.6,2.61664298099999));
#258093=CARTESIAN_POINT('Ctrl Pts',(-10.8872462720001,15.2,2.61610741899998));
#258094=CARTESIAN_POINT('Ctrl Pts',(-10.8872462720001,11.6,2.61610741899998));
#258095=CARTESIAN_POINT('Ctrl Pts',(-10.8906035620001,15.2,2.61556843799998));
#258096=CARTESIAN_POINT('Ctrl Pts',(-10.8906035620001,11.6,2.61556843799998));
#258097=CARTESIAN_POINT('Ctrl Pts',(-10.8939652320001,15.2,2.61502603199999));
#258098=CARTESIAN_POINT('Ctrl Pts',(-10.8939652320001,11.6,2.61502603199998));
#258099=CARTESIAN_POINT('Ctrl Pts',(-10.8973312750001,15.2,2.61448019799998));
#258100=CARTESIAN_POINT('Ctrl Pts',(-10.8973312750001,11.6,2.61448019799998));
#258101=CARTESIAN_POINT('Ctrl Pts',(-10.9007016800001,15.2,2.61393092799998));
#258102=CARTESIAN_POINT('Ctrl Pts',(-10.9007016800001,11.6,2.61393092799998));
#258103=CARTESIAN_POINT('Ctrl Pts',(-10.9040764380001,15.2,2.61337821999999));
#258104=CARTESIAN_POINT('Ctrl Pts',(-10.9040764380001,11.6,2.61337821999999));
#258105=CARTESIAN_POINT('Ctrl Pts',(-10.9074555420001,15.2,2.61282206699998));
#258106=CARTESIAN_POINT('Ctrl Pts',(-10.9074555420001,11.6,2.61282206699998));
#258107=CARTESIAN_POINT('Ctrl Pts',(-10.9108389810001,15.2,2.61226246499999));
#258108=CARTESIAN_POINT('Ctrl Pts',(-10.9108389810001,11.6,2.61226246499999));
#258109=CARTESIAN_POINT('Ctrl Pts',(-10.9142267470001,15.2,2.61169940799999));
#258110=CARTESIAN_POINT('Ctrl Pts',(-10.9142267470001,11.6,2.61169940799999));
#258111=CARTESIAN_POINT('Ctrl Pts',(-10.9176188310001,15.2,2.61113289199999));
#258112=CARTESIAN_POINT('Ctrl Pts',(-10.9176188310001,11.6,2.61113289199999));
#258113=CARTESIAN_POINT('Ctrl Pts',(-10.9210152230001,15.2,2.61056291099998));
#258114=CARTESIAN_POINT('Ctrl Pts',(-10.9210152230001,11.6,2.61056291099998));
#258115=CARTESIAN_POINT('Ctrl Pts',(-10.9244159170001,15.2,2.60998946099999));
#258116=CARTESIAN_POINT('Ctrl Pts',(-10.9244159170001,11.6,2.60998946099999));
#258117=CARTESIAN_POINT('Ctrl Pts',(-10.9278209010001,15.2,2.60941253699999));
#258118=CARTESIAN_POINT('Ctrl Pts',(-10.9278209010001,11.6,2.60941253699999));
#258119=CARTESIAN_POINT('Ctrl Pts',(-10.9312301670001,15.2,2.60883213399998));
#258120=CARTESIAN_POINT('Ctrl Pts',(-10.9312301670001,11.6,2.60883213399998));
#258121=CARTESIAN_POINT('Ctrl Pts',(-10.9346437070001,15.2,2.60824824699998));
#258122=CARTESIAN_POINT('Ctrl Pts',(-10.9346437070001,11.6,2.60824824699998));
#258123=CARTESIAN_POINT('Ctrl Pts',(-10.9380615100001,15.2,2.60766087099999));
#258124=CARTESIAN_POINT('Ctrl Pts',(-10.9380615100001,11.6,2.60766087099999));
#258125=CARTESIAN_POINT('Ctrl Pts',(-10.9414835700001,15.2,2.60707000099998));
#258126=CARTESIAN_POINT('Ctrl Pts',(-10.9414835700001,11.6,2.60707000099998));
#258127=CARTESIAN_POINT('Ctrl Pts',(-10.9449098760001,15.2,2.60647563299998));
#258128=CARTESIAN_POINT('Ctrl Pts',(-10.9449098760001,11.6,2.60647563299998));
#258129=CARTESIAN_POINT('Ctrl Pts',(-10.9483404200001,15.2,2.60587776099998));
#258130=CARTESIAN_POINT('Ctrl Pts',(-10.9483404200001,11.6,2.60587776099998));
#258131=CARTESIAN_POINT('Ctrl Pts',(-10.9517751930001,15.2,2.60527638199999));
#258132=CARTESIAN_POINT('Ctrl Pts',(-10.9517751930001,11.6,2.60527638199999));
#258133=CARTESIAN_POINT('Ctrl Pts',(-10.9552141870001,15.2,2.60467148899998));
#258134=CARTESIAN_POINT('Ctrl Pts',(-10.9552141870001,11.6,2.60467148899998));
#258135=CARTESIAN_POINT('Ctrl Pts',(-10.9586573930001,15.2,2.60406307899999));
#258136=CARTESIAN_POINT('Ctrl Pts',(-10.9586573930001,11.6,2.60406307899998));
#258137=CARTESIAN_POINT('Ctrl Pts',(-10.9621047990001,15.2,2.60345114599998));
#258138=CARTESIAN_POINT('Ctrl Pts',(-10.9621047990001,11.6,2.60345114599998));
#258139=CARTESIAN_POINT('Ctrl Pts',(-10.9655564020001,15.2,2.60283568599998));
#258140=CARTESIAN_POINT('Ctrl Pts',(-10.9655564020001,11.6,2.60283568599998));
#258141=CARTESIAN_POINT('Ctrl Pts',(-10.9690121870001,15.2,2.60221669399999));
#258142=CARTESIAN_POINT('Ctrl Pts',(-10.9690121870001,11.6,2.60221669399999));
#258143=CARTESIAN_POINT('Ctrl Pts',(-10.9724721500001,15.2,2.60159416599999));
#258144=CARTESIAN_POINT('Ctrl Pts',(-10.9724721500001,11.6,2.60159416599999));
#258145=CARTESIAN_POINT('Ctrl Pts',(-10.9759362810001,15.2,2.60096809599998));
#258146=CARTESIAN_POINT('Ctrl Pts',(-10.9759362810001,11.6,2.60096809599998));
#258147=CARTESIAN_POINT('Ctrl Pts',(-10.9794045700001,15.2,2.60033847899999));
#258148=CARTESIAN_POINT('Ctrl Pts',(-10.9794045700001,11.6,2.60033847899999));
#258149=CARTESIAN_POINT('Ctrl Pts',(-10.9828770100001,15.2,2.59970531199999));
#258150=CARTESIAN_POINT('Ctrl Pts',(-10.9828770100001,11.6,2.59970531199999));
#258151=CARTESIAN_POINT('Ctrl Pts',(-10.9863535920001,15.2,2.59906858999998));
#258152=CARTESIAN_POINT('Ctrl Pts',(-10.9863535920001,11.6,2.59906858999998));
#258153=CARTESIAN_POINT('Ctrl Pts',(-10.9898343060001,15.2,2.59842830899998));
#258154=CARTESIAN_POINT('Ctrl Pts',(-10.9898343060001,11.6,2.59842830899998));
#258155=CARTESIAN_POINT('Ctrl Pts',(-10.9933191440001,15.2,2.59778446199999));
#258156=CARTESIAN_POINT('Ctrl Pts',(-10.9933191440001,11.6,2.59778446199999));
#258157=CARTESIAN_POINT('Ctrl Pts',(-10.9968080970001,15.2,2.59713704699998));
#258158=CARTESIAN_POINT('Ctrl Pts',(-10.9968080970001,11.6,2.59713704699998));
#258159=CARTESIAN_POINT('Ctrl Pts',(-11.0003011580001,15.2,2.59648605699999));
#258160=CARTESIAN_POINT('Ctrl Pts',(-11.0003011580001,11.6,2.59648605699999));
#258161=CARTESIAN_POINT('Ctrl Pts',(-11.0037983160001,15.2,2.59583148899999));
#258162=CARTESIAN_POINT('Ctrl Pts',(-11.0037983160001,11.6,2.59583148899999));
#258163=CARTESIAN_POINT('Ctrl Pts',(-11.0072995640001,15.2,2.59517333899999));
#258164=CARTESIAN_POINT('Ctrl Pts',(-11.0072995640001,11.6,2.59517333899998));
#258165=CARTESIAN_POINT('Ctrl Pts',(-11.0108048930001,15.2,2.59451159999998));
#258166=CARTESIAN_POINT('Ctrl Pts',(-11.0108048930001,11.6,2.59451159999998));
#258167=CARTESIAN_POINT('Ctrl Pts',(-11.0143142940001,15.2,2.59384626999999));
#258168=CARTESIAN_POINT('Ctrl Pts',(-11.0143142940001,11.6,2.59384626999999));
#258169=CARTESIAN_POINT('Ctrl Pts',(-11.0178277600001,15.2,2.59317734299999));
#258170=CARTESIAN_POINT('Ctrl Pts',(-11.0178277600001,11.6,2.59317734299999));
#258171=CARTESIAN_POINT('Ctrl Pts',(-11.0213452790001,15.2,2.59250481599998));
#258172=CARTESIAN_POINT('Ctrl Pts',(-11.0213452790001,11.6,2.59250481599998));
#258173=CARTESIAN_POINT('Ctrl Pts',(-11.0248668450001,15.2,2.59182868299998));
#258174=CARTESIAN_POINT('Ctrl Pts',(-11.0248668450001,11.6,2.59182868299998));
#258175=CARTESIAN_POINT('Ctrl Pts',(-11.0283924510001,15.2,2.59114894099999));
#258176=CARTESIAN_POINT('Ctrl Pts',(-11.0283924510001,11.6,2.59114894099999));
#258177=CARTESIAN_POINT('Ctrl Pts',(-11.0319220850001,15.2,2.59046558299998));
#258178=CARTESIAN_POINT('Ctrl Pts',(-11.0319220850001,11.6,2.59046558299998));
#258179=CARTESIAN_POINT('Ctrl Pts',(-11.0354557400001,15.2,2.58977860699999));
#258180=CARTESIAN_POINT('Ctrl Pts',(-11.0354557400001,11.6,2.58977860699999));
#258181=CARTESIAN_POINT('Ctrl Pts',(-11.0389934070001,15.2,2.58908800799999));
#258182=CARTESIAN_POINT('Ctrl Pts',(-11.0389934070001,11.6,2.58908800799999));
#258183=CARTESIAN_POINT('Ctrl Pts',(-11.0425350780001,15.2,2.58839378199998));
#258184=CARTESIAN_POINT('Ctrl Pts',(-11.0425350780001,11.6,2.58839378199998));
#258185=CARTESIAN_POINT('Ctrl Pts',(-11.0460807450001,15.2,2.58769592199998));
#258186=CARTESIAN_POINT('Ctrl Pts',(-11.0460807450001,11.6,2.58769592199998));
#258187=CARTESIAN_POINT('Ctrl Pts',(-11.0496303980001,15.2,2.58699442799998));
#258188=CARTESIAN_POINT('Ctrl Pts',(-11.0496303980001,11.6,2.58699442799998));
#258189=CARTESIAN_POINT('Ctrl Pts',(-11.0531840300001,15.2,2.58628929099999));
#258190=CARTESIAN_POINT('Ctrl Pts',(-11.0531840300001,11.6,2.58628929099999));
#258191=CARTESIAN_POINT('Ctrl Pts',(-11.0567416320001,15.2,2.58558051099998));
#258192=CARTESIAN_POINT('Ctrl Pts',(-11.0567416320001,11.6,2.58558051099998));
#258193=CARTESIAN_POINT('Ctrl Pts',(-11.0603031950001,15.2,2.58486808099998));
#258194=CARTESIAN_POINT('Ctrl Pts',(-11.0603031950001,11.6,2.58486808099998));
#258195=CARTESIAN_POINT('Ctrl Pts',(-11.0638687110001,15.2,2.58415199699999));
#258196=CARTESIAN_POINT('Ctrl Pts',(-11.0638687110001,11.6,2.58415199699999));
#258197=CARTESIAN_POINT('Ctrl Pts',(-11.0674381720001,15.2,2.58343225399998));
#258198=CARTESIAN_POINT('Ctrl Pts',(-11.0674381720001,11.6,2.58343225399998));
#258199=CARTESIAN_POINT('Ctrl Pts',(-11.0710115690001,15.2,2.58270884999998));
#258200=CARTESIAN_POINT('Ctrl Pts',(-11.0710115690001,11.6,2.58270884999998));
#258201=CARTESIAN_POINT('Ctrl Pts',(-11.0745888930001,15.2,2.58198177899998));
#258202=CARTESIAN_POINT('Ctrl Pts',(-11.0745888930001,11.6,2.58198177899998));
#258203=CARTESIAN_POINT('Ctrl Pts',(-11.0781701370001,15.2,2.58125103699999));
#258204=CARTESIAN_POINT('Ctrl Pts',(-11.0781701370001,11.6,2.58125103699999));
#258205=CARTESIAN_POINT('Ctrl Pts',(-11.0817552930001,15.2,2.58051662099999));
#258206=CARTESIAN_POINT('Ctrl Pts',(-11.0817552930001,11.6,2.58051662099999));
#258207=CARTESIAN_POINT('Ctrl Pts',(-11.0853443500001,15.2,2.57977852499998));
#258208=CARTESIAN_POINT('Ctrl Pts',(-11.0853443500001,11.6,2.57977852499998));
#258209=CARTESIAN_POINT('Ctrl Pts',(-11.0889373030001,15.2,2.57903674599999));
#258210=CARTESIAN_POINT('Ctrl Pts',(-11.0889373030001,11.6,2.57903674599999));
#258211=CARTESIAN_POINT('Ctrl Pts',(-11.0925341410001,15.2,2.57829127899999));
#258212=CARTESIAN_POINT('Ctrl Pts',(-11.0925341410001,11.6,2.57829127899999));
#258213=CARTESIAN_POINT('Ctrl Pts',(-11.0961348560001,15.2,2.57754211899999));
#258214=CARTESIAN_POINT('Ctrl Pts',(-11.0961348560001,11.6,2.57754211899999));
#258215=CARTESIAN_POINT('Ctrl Pts',(-11.0997394400001,15.2,2.57678926399999));
#258216=CARTESIAN_POINT('Ctrl Pts',(-11.0997394400001,11.6,2.57678926399999));
#258217=CARTESIAN_POINT('Ctrl Pts',(-11.1033478850001,15.2,2.57603270799999));
#258218=CARTESIAN_POINT('Ctrl Pts',(-11.1033478850001,11.6,2.57603270799999));
#258219=CARTESIAN_POINT('Ctrl Pts',(-11.1069601830001,15.2,2.57527244799999));
#258220=CARTESIAN_POINT('Ctrl Pts',(-11.1069601830001,11.6,2.57527244799999));
#258221=CARTESIAN_POINT('Ctrl Pts',(-11.1105763250001,15.2,2.57450847999999));
#258222=CARTESIAN_POINT('Ctrl Pts',(-11.1105763250001,11.6,2.57450847999999));
#258223=CARTESIAN_POINT('Ctrl Pts',(-11.1141963030001,15.2,2.57374079699999));
#258224=CARTESIAN_POINT('Ctrl Pts',(-11.1141963030001,11.6,2.57374079699999));
#258225=CARTESIAN_POINT('Ctrl Pts',(-11.1178201080001,15.2,2.57296939999998));
#258226=CARTESIAN_POINT('Ctrl Pts',(-11.1178201080001,11.6,2.57296939999998));
#258227=CARTESIAN_POINT('Ctrl Pts',(-11.1214477320001,15.2,2.57219428099998));
#258228=CARTESIAN_POINT('Ctrl Pts',(-11.1214477320001,11.6,2.57219428099998));
#258229=CARTESIAN_POINT('Ctrl Pts',(-11.1250791700001,15.2,2.57141543699999));
#258230=CARTESIAN_POINT('Ctrl Pts',(-11.1250791700001,11.6,2.57141543699999));
#258231=CARTESIAN_POINT('Ctrl Pts',(-11.1287144100001,15.2,2.57063286499999));
#258232=CARTESIAN_POINT('Ctrl Pts',(-11.1287144100001,11.6,2.57063286499999));
#258233=CARTESIAN_POINT('Ctrl Pts',(-11.1323534440001,15.2,2.56984655999998));
#258234=CARTESIAN_POINT('Ctrl Pts',(-11.1323534440001,11.6,2.56984655999998));
#258235=CARTESIAN_POINT('Ctrl Pts',(-11.1359962660001,15.2,2.56905651699999));
#258236=CARTESIAN_POINT('Ctrl Pts',(-11.1359962660001,11.6,2.56905651699999));
#258237=CARTESIAN_POINT('Ctrl Pts',(-11.1396428650001,15.2,2.56826273399999));
#258238=CARTESIAN_POINT('Ctrl Pts',(-11.1396428650001,11.6,2.56826273399999));
#258239=CARTESIAN_POINT('Ctrl Pts',(-11.1432932330001,15.2,2.56746520399999));
#258240=CARTESIAN_POINT('Ctrl Pts',(-11.1432932330001,11.6,2.56746520399999));
#258241=CARTESIAN_POINT('Ctrl Pts',(-11.1469473610001,15.2,2.56666392599998));
#258242=CARTESIAN_POINT('Ctrl Pts',(-11.1469473610001,11.6,2.56666392599998));
#258243=CARTESIAN_POINT('Ctrl Pts',(-11.1506052430001,15.2,2.56585889299998));
#258244=CARTESIAN_POINT('Ctrl Pts',(-11.1506052430001,11.6,2.56585889299998));
#258245=CARTESIAN_POINT('Ctrl Pts',(-11.1542668700001,15.2,2.56505010399999));
#258246=CARTESIAN_POINT('Ctrl Pts',(-11.1542668700001,11.6,2.56505010399999));
#258247=CARTESIAN_POINT('Ctrl Pts',(-11.1579322340001,15.2,2.56423755399998));
#258248=CARTESIAN_POINT('Ctrl Pts',(-11.1579322340001,11.6,2.56423755399998));
#258249=CARTESIAN_POINT('Ctrl Pts',(-11.1616013300001,15.2,2.56342123899999));
#258250=CARTESIAN_POINT('Ctrl Pts',(-11.1616013300001,11.6,2.56342123899999));
#258251=CARTESIAN_POINT('Ctrl Pts',(-11.1652741470001,15.2,2.56260115599999));
#258252=CARTESIAN_POINT('Ctrl Pts',(-11.1652741470001,11.6,2.56260115599999));
#258253=CARTESIAN_POINT('Ctrl Pts',(-11.1689506800001,15.2,2.56177730199998));
#258254=CARTESIAN_POINT('Ctrl Pts',(-11.1689506800001,11.6,2.56177730199998));
#258255=CARTESIAN_POINT('Ctrl Pts',(-11.1726309200001,15.2,2.56094967199999));
#258256=CARTESIAN_POINT('Ctrl Pts',(-11.1726309200001,11.6,2.56094967199999));
#258257=CARTESIAN_POINT('Ctrl Pts',(-11.1763148560001,15.2,2.56011826199998));
#258258=CARTESIAN_POINT('Ctrl Pts',(-11.1763148560001,11.6,2.56011826199998));
#258259=CARTESIAN_POINT('Ctrl Pts',(-11.1800024800001,15.2,2.55928306599999));
#258260=CARTESIAN_POINT('Ctrl Pts',(-11.1800024800001,11.6,2.55928306599999));
#258261=CARTESIAN_POINT('Ctrl Pts',(-11.1836937810001,15.2,2.55844408099998));
#258262=CARTESIAN_POINT('Ctrl Pts',(-11.1836937810001,11.6,2.55844408099998));
#258263=CARTESIAN_POINT('Ctrl Pts',(-11.1873887500001,15.2,2.55760130099999));
#258264=CARTESIAN_POINT('Ctrl Pts',(-11.1873887500001,11.6,2.55760130099999));
#258265=CARTESIAN_POINT('Ctrl Pts',(-11.1910873770001,15.2,2.55675472199999));
#258266=CARTESIAN_POINT('Ctrl Pts',(-11.1910873770001,11.6,2.55675472199999));
#258267=CARTESIAN_POINT('Ctrl Pts',(-11.1947896560001,15.2,2.55590434099998));
#258268=CARTESIAN_POINT('Ctrl Pts',(-11.1947896560001,11.6,2.55590434099998));
#258269=CARTESIAN_POINT('Ctrl Pts',(-11.1984955800001,15.2,2.55505015599999));
#258270=CARTESIAN_POINT('Ctrl Pts',(-11.1984955800001,11.6,2.55505015599999));
#258271=CARTESIAN_POINT('Ctrl Pts',(-11.2022051470001,15.2,2.55419216399999));
#258272=CARTESIAN_POINT('Ctrl Pts',(-11.2022051470001,11.6,2.55419216399999));
#258273=CARTESIAN_POINT('Ctrl Pts',(-11.2059183540001,15.2,2.55333036499999));
#258274=CARTESIAN_POINT('Ctrl Pts',(-11.2059183540001,11.6,2.55333036499999));
#258275=CARTESIAN_POINT('Ctrl Pts',(-11.2088918300001,15.2,2.55263787899998));
#258276=CARTESIAN_POINT('Ctrl Pts',(-11.2088918300001,11.6,2.55263787899998));
#258277=CARTESIAN_POINT('Ctrl Pts',(-11.2111235750001,15.2,2.55211679999999));
#258278=CARTESIAN_POINT('Ctrl Pts',(-11.2111235750001,11.6,2.55211679999999));
#258279=CARTESIAN_POINT('Ctrl Pts',(-11.2126121320001,15.2,2.55176865399999));
#258280=CARTESIAN_POINT('Ctrl Pts',(-11.2126121320001,11.6,2.55176865399999));
#258281=CARTESIAN_POINT('Ctrl Pts',(-11.2133565920001,15.2,2.55159438999998));
#258282=CARTESIAN_POINT('Ctrl Pts',(-11.2133565920001,11.6,2.55159438999998));
#258283=CARTESIAN_POINT('Ctrl Pts',(-10.0330625580001,15.2,2.64164356399998));
#258284=CARTESIAN_POINT('Ctrl Pts',(-10.03482302717,15.2,2.64194831044285));
#258285=CARTESIAN_POINT('Ctrl Pts',(-10.0366407484416,15.2,2.64225751971682));
#258286=CARTESIAN_POINT('Ctrl Pts',(-10.0385148615364,15.2,2.64257038294905));
#258287=CARTESIAN_POINT('Ctrl Pts',(-10.0403980125518,15.2,2.64288475496593));
#258288=CARTESIAN_POINT('Ctrl Pts',(-10.0423381038147,15.2,2.64320281628067));
#258289=CARTESIAN_POINT('Ctrl Pts',(-10.0443343061932,15.2,2.64352378181437));
#258290=CARTESIAN_POINT('Ctrl Pts',(-10.0463305083903,15.2,2.64384474731891));
#258291=CARTESIAN_POINT('Ctrl Pts',(-10.0483828189766,15.2,2.64416861768683));
#258292=CARTESIAN_POINT('Ctrl Pts',(-10.0504904282333,15.2,2.64449462925831));
#258293=CARTESIAN_POINT('Ctrl Pts',(-10.05259803749,15.2,2.6448206408298));
#258294=CARTESIAN_POINT('Ctrl Pts',(-10.0547609456752,15.2,2.64514879427203));
#258295=CARTESIAN_POINT('Ctrl Pts',(-10.0569783630356,15.2,2.6454783536931));
#258296=CARTESIAN_POINT('Ctrl Pts',(-10.0591957805974,15.2,2.64580791314411));
#258297=CARTESIAN_POINT('Ctrl Pts',(-10.0614677060147,15.2,2.64613887440968));
#258298=CARTESIAN_POINT('Ctrl Pts',(-10.0637933707285,15.2,2.64647052701114));
#258299=CARTESIAN_POINT('Ctrl Pts',(-10.066506645911,15.2,2.64685745500097));
#258300=CARTESIAN_POINT('Ctrl Pts',(-10.0692930658019,15.2,2.64724531920595));
#258301=CARTESIAN_POINT('Ctrl Pts',(-10.0721514405131,15.2,2.64763302120117));
#258302=CARTESIAN_POINT('Ctrl Pts',(-10.0746014762659,15.2,2.64796533723589));
#258303=CARTESIAN_POINT('Ctrl Pts',(-10.077104375569,15.2,2.6482975368681));
#258304=CARTESIAN_POINT('Ctrl Pts',(-10.0796594095451,15.2,2.64862894605278));
#258305=CARTESIAN_POINT('Ctrl Pts',(-10.0826402821692,15.2,2.64901559005641));
#258306=CARTESIAN_POINT('Ctrl Pts',(-10.0856921168832,15.2,2.64940116149503));
#258307=CARTESIAN_POINT('Ctrl Pts',(-10.0888137817163,15.2,2.64978463072653));
#258308=CARTESIAN_POINT('Ctrl Pts',(-10.0914894947428,15.2,2.65011331867762));
#258309=CARTESIAN_POINT('Ctrl Pts',(-10.0942165130146,15.2,2.65044046151785));
#258310=CARTESIAN_POINT('Ctrl Pts',(-10.0969941418361,15.2,2.65076543253541));
#258311=CARTESIAN_POINT('Ctrl Pts',(-10.0997717704053,15.2,2.65109040352346));
#258312=CARTESIAN_POINT('Ctrl Pts',(-10.1026000079927,15.2,2.65141319986032));
#258313=CARTESIAN_POINT('Ctrl Pts',(-10.1054781797346,15.2,2.6517332150168));
#258314=CARTESIAN_POINT('Ctrl Pts',(-10.1083563514765,15.2,2.65205323017329));
#258315=CARTESIAN_POINT('Ctrl Pts',(-10.1112844546649,15.2,2.65237046014413));
#258316=CARTESIAN_POINT('Ctrl Pts',(-10.1142618273879,15.2,2.6526843154662));
#258317=CARTESIAN_POINT('Ctrl Pts',(-10.1172392003813,15.2,2.65299817081679));
#258318=CARTESIAN_POINT('Ctrl Pts',(-10.1202658403643,15.2,2.65330864964196));
#258319=CARTESIAN_POINT('Ctrl Pts',(-10.1233411005352,15.2,2.65361517507507));
#258320=CARTESIAN_POINT('Ctrl Pts',(-10.1264163604267,15.2,2.65392170048033));
#258321=CARTESIAN_POINT('Ctrl Pts',(-10.1295402396778,15.2,2.65422427246057));
#258322=CARTESIAN_POINT('Ctrl Pts',(-10.132712100648,15.2,2.65452233078288));
#258323=CARTESIAN_POINT('Ctrl Pts',(-10.1358839616182,15.2,2.6548203891052));
#258324=CARTESIAN_POINT('Ctrl Pts',(-10.1391038055679,15.2,2.65511393257785));
#258325=CARTESIAN_POINT('Ctrl Pts',(-10.1423710095304,15.2,2.65540241523425));
#258326=CARTESIAN_POINT('Ctrl Pts',(-10.1456382137898,15.2,2.65569089791686));
#258327=CARTESIAN_POINT('Ctrl Pts',(-10.14895277868,15.2,2.65597432189051));
#258328=CARTESIAN_POINT('Ctrl Pts',(-10.1523140903664,15.2,2.65625215348861));
#258329=CARTESIAN_POINT('Ctrl Pts',(-10.1556754017474,15.2,2.65652998506147));
#258330=CARTESIAN_POINT('Ctrl Pts',(-10.1590834649786,15.2,2.65680222564107));
#258331=CARTESIAN_POINT('Ctrl Pts',(-10.1625376761884,15.2,2.65706835629781));
#258332=CARTESIAN_POINT('Ctrl Pts',(-10.1659918873983,15.2,2.65733448695455));
#258333=CARTESIAN_POINT('Ctrl Pts',(-10.1694922497961,15.2,2.65759450932841));
#258334=CARTESIAN_POINT('Ctrl Pts',(-10.1730381740819,15.2,2.65784791815283));
#258335=CARTESIAN_POINT('Ctrl Pts',(-10.1771750859635,15.2,2.65814356179666));
#258336=CARTESIAN_POINT('Ctrl Pts',(-10.1813740127417,15.2,2.65843020520895));
#258337=CARTESIAN_POINT('Ctrl Pts',(-10.1856340416992,15.2,2.65870706775457));
#258338=CARTESIAN_POINT('Ctrl Pts',(-10.1892854949018,15.2,2.65894437849563));
#258339=CARTESIAN_POINT('Ctrl Pts',(-10.1929818390258,15.2,2.65917450500392));
#258340=CARTESIAN_POINT('Ctrl Pts',(-10.196722511138,15.2,2.65939697174618));
#258341=CARTESIAN_POINT('Ctrl Pts',(-10.2004631832501,15.2,2.65961943848842));
#258342=CARTESIAN_POINT('Ctrl Pts',(-10.2042481817748,15.2,2.65983424250942));
#258343=CARTESIAN_POINT('Ctrl Pts',(-10.2080769531327,15.2,2.66004092325247));
#258344=CARTESIAN_POINT('Ctrl Pts',(-10.2119057248383,15.2,2.66024760401429));
#258345=CARTESIAN_POINT('Ctrl Pts',(-10.2157782698399,15.2,2.660446157467));
#258346=CARTESIAN_POINT('Ctrl Pts',(-10.2196940444719,15.2,2.66063613431032));
#258347=CARTESIAN_POINT('Ctrl Pts',(-10.2242624476756,15.2,2.66085777393497));
#258348=CARTESIAN_POINT('Ctrl Pts',(-10.228889688663,15.2,2.66106773679313));
#258349=CARTESIAN_POINT('Ctrl Pts',(-10.2335749198123,15.2,2.66126532344821));
#258350=CARTESIAN_POINT('Ctrl Pts',(-10.2375908326949,15.2,2.66143468345806));
#258351=CARTESIAN_POINT('Ctrl Pts',(-10.2416493509317,15.2,2.66159495070038));
#258352=CARTESIAN_POINT('Ctrl Pts',(-10.2457499514903,15.2,2.66174569770818));
#258353=CARTESIAN_POINT('Ctrl Pts',(-10.2491671184363,15.2,2.66187132020783));
#258354=CARTESIAN_POINT('Ctrl Pts',(-10.2526135061945,15.2,2.66199032998565));
#258355=CARTESIAN_POINT('Ctrl Pts',(-10.2560888201202,15.2,2.66210248575466));
#258356=CARTESIAN_POINT('Ctrl Pts',(-10.2602591966794,15.2,2.66223707267259));
#258357=CARTESIAN_POINT('Ctrl Pts',(-10.2644712218128,15.2,2.66236178712083));
#258358=CARTESIAN_POINT('Ctrl Pts',(-10.2687243902416,15.2,2.66247622028334));
#258359=CARTESIAN_POINT('Ctrl Pts',(-10.2722686973944,15.2,2.66257158125556));
#258360=CARTESIAN_POINT('Ctrl Pts',(-10.2758415739022,15.2,2.66265980250525));
#258361=CARTESIAN_POINT('Ctrl Pts',(-10.2794427312103,15.2,2.66274065174171));
#258362=CARTESIAN_POINT('Ctrl Pts',(-10.283764119823,15.2,2.66283767082193));
#258363=CARTESIAN_POINT('Ctrl Pts',(-10.2881262325969,15.2,2.66292407391478));
#258364=CARTESIAN_POINT('Ctrl Pts',(-10.2925285750186,15.2,2.66299946724585));
#258365=CARTESIAN_POINT('Ctrl Pts',(-10.2961971938365,15.2,2.66306229502403));
#258366=CARTESIAN_POINT('Ctrl Pts',(-10.2998937493192,15.2,2.66311747731868));
#258367=CARTESIAN_POINT('Ctrl Pts',(-10.3036179592483,15.2,2.66316479322186));
#258368=CARTESIAN_POINT('Ctrl Pts',(-10.3088318532302,15.2,2.66323103548736));
#258369=CARTESIAN_POINT('Ctrl Pts',(-10.3140999532028,15.2,2.66328185661831));
#258370=CARTESIAN_POINT('Ctrl Pts',(-10.3194214920237,15.2,2.66331665974325));
#258371=CARTESIAN_POINT('Ctrl Pts',(-10.3262634701527,15.2,2.66336140661585));
#258372=CARTESIAN_POINT('Ctrl Pts',(-10.3331937896886,15.2,2.66337967464965));
#258373=CARTESIAN_POINT('Ctrl Pts',(-10.3402108602809,15.2,2.66337023577558));
#258374=CARTESIAN_POINT('Ctrl Pts',(-10.3441092329738,15.2,2.66336499195647));
#258375=CARTESIAN_POINT('Ctrl Pts',(-10.3480343817431,15.2,2.66335119775652));
#258376=CARTESIAN_POINT('Ctrl Pts',(-10.3519860390334,15.2,2.6633286457431));
#258377=CARTESIAN_POINT('Ctrl Pts',(-10.3559376963237,15.2,2.66330609372967));
#258378=CARTESIAN_POINT('Ctrl Pts',(-10.3599158609841,15.2,2.66327478816323));
#258379=CARTESIAN_POINT('Ctrl Pts',(-10.3639202692466,15.2,2.66323452351092));
#258380=CARTESIAN_POINT('Ctrl Pts',(-10.3679246775091,15.2,2.66319425885861));
#258381=CARTESIAN_POINT('Ctrl Pts',(-10.3719553298751,15.2,2.66314503698663));
#258382=CARTESIAN_POINT('Ctrl Pts',(-10.3760119632765,15.2,2.66308666052877));
#258383=CARTESIAN_POINT('Ctrl Pts',(-10.3800685966779,15.2,2.66302828407091));
#258384=CARTESIAN_POINT('Ctrl Pts',(-10.3841512130792,15.2,2.66296075166148));
#258385=CARTESIAN_POINT('Ctrl Pts',(-10.3882595522644,15.2,2.66288387200838));
#258386=CARTESIAN_POINT('Ctrl Pts',(-10.3948328948713,15.2,2.6627608645651));
#258387=CARTESIAN_POINT('Ctrl Pts',(-10.4014720887002,15.2,2.66261392210659));
#258388=CARTESIAN_POINT('Ctrl Pts',(-10.4081760887178,15.2,2.66244227199863));
#258389=CARTESIAN_POINT('Ctrl Pts',(-10.4115280889549,15.2,2.66235644693881));
#258390=CARTESIAN_POINT('Ctrl Pts',(-10.4148962921196,15.2,2.66226444478541));
#258391=CARTESIAN_POINT('Ctrl Pts',(-10.4182805684745,15.2,2.66216617121905));
#258392=CARTESIAN_POINT('Ctrl Pts',(-10.4216648443683,15.2,2.66206789766606));
#258393=CARTESIAN_POINT('Ctrl Pts',(-10.4250651934345,15.2,2.66196335370509));
#258394=CARTESIAN_POINT('Ctrl Pts',(-10.4284814884875,15.2,2.66185244349235));
#258395=CARTESIAN_POINT('Ctrl Pts',(-10.431897784006,15.2,2.6617415332645));
#258396=CARTESIAN_POINT('Ctrl Pts',(-10.4353300246598,15.2,2.66162425913311));
#258397=CARTESIAN_POINT('Ctrl Pts',(-10.4387780855154,15.2,2.66150052751483));
#258398=CARTESIAN_POINT('Ctrl Pts',(-10.44308816135,15.2,2.66134586300042));
#258399=CARTESIAN_POINT('Ctrl Pts',(-10.4474229556422,15.2,2.66118110989467));
#258400=CARTESIAN_POINT('Ctrl Pts',(-10.4517822217645,15.2,2.66100609120466));
#258401=CARTESIAN_POINT('Ctrl Pts',(-10.4552696343772,15.2,2.66086607626409));
#258402=CARTESIAN_POINT('Ctrl Pts',(-10.4587727093012,15.2,2.66071949113562));
#258403=CARTESIAN_POINT('Ctrl Pts',(-10.4622913236792,15.2,2.66056624753748));
#258404=CARTESIAN_POINT('Ctrl Pts',(-10.4658099385365,15.2,2.66041300391845));
#258405=CARTESIAN_POINT('Ctrl Pts',(-10.4693440916153,15.2,2.66025310126806));
#258406=CARTESIAN_POINT('Ctrl Pts',(-10.472893660532,15.2,2.66008645170299));
#258407=CARTESIAN_POINT('Ctrl Pts',(-10.476443228965,15.2,2.65991980216062));
#258408=CARTESIAN_POINT('Ctrl Pts',(-10.4800082127318,15.2,2.65974640584203));
#258409=CARTESIAN_POINT('Ctrl Pts',(-10.4835884906722,15.2,2.65956617629279));
#258410=CARTESIAN_POINT('Ctrl Pts',(-10.4880638384636,15.2,2.65934088933784));
#258411=CARTESIAN_POINT('Ctrl Pts',(-10.4925630812722,15.2,2.65910492722664));
#258412=CARTESIAN_POINT('Ctrl Pts',(-10.4970859854377,15.2,2.65885812028276));
#258413=CARTESIAN_POINT('Ctrl Pts',(-10.5016088896031,15.2,2.65861131333888));
#258414=CARTESIAN_POINT('Ctrl Pts',(-10.5061554536025,15.2,2.65835366302805));
#258415=CARTESIAN_POINT('Ctrl Pts',(-10.5107254429763,15.2,2.65808500775085));
#258416=CARTESIAN_POINT('Ctrl Pts',(-10.51529543235,15.2,2.65781635247365));
#258417=CARTESIAN_POINT('Ctrl Pts',(-10.5198888487266,15.2,2.65753668945702));
#258418=CARTESIAN_POINT('Ctrl Pts',(-10.5245054589558,15.2,2.65724586077517));
#258419=CARTESIAN_POINT('Ctrl Pts',(-10.5281987473405,15.2,2.65701319781701));
#258420=CARTESIAN_POINT('Ctrl Pts',(-10.5319068808099,15.2,2.65677338729882));
#258421=CARTESIAN_POINT('Ctrl Pts',(-10.5356297411254,15.2,2.65652635045129));
#258422=CARTESIAN_POINT('Ctrl Pts',(-10.5393526009336,15.2,2.65627931363741));
#258423=CARTESIAN_POINT('Ctrl Pts',(-10.54309018764,15.2,2.65602504855503));
#258424=CARTESIAN_POINT('Ctrl Pts',(-10.5468423854434,15.2,2.65576347702133));
#258425=CARTESIAN_POINT('Ctrl Pts',(-10.550594583758,15.2,2.65550190545199));
#258426=CARTESIAN_POINT('Ctrl Pts',(-10.5543613915386,15.2,2.65523302726716));
#258427=CARTESIAN_POINT('Ctrl Pts',(-10.5581426953238,15.2,2.65495676245988));
#258428=CARTESIAN_POINT('Ctrl Pts',(-10.5628693247976,15.2,2.6546114314696));
#258429=CARTESIAN_POINT('Ctrl Pts',(-10.5676186017778,15.2,2.65425456055276));
#258430=CARTESIAN_POINT('Ctrl Pts',(-10.5723903028908,15.2,2.6538859986768));
#258431=CARTESIAN_POINT('Ctrl Pts',(-10.5771620040038,15.2,2.65351743680084));
#258432=CARTESIAN_POINT('Ctrl Pts',(-10.5819561292227,15.2,2.65313718353857));
#258433=CARTESIAN_POINT('Ctrl Pts',(-10.5867724568633,15.2,2.65274509089872));
#258434=CARTESIAN_POINT('Ctrl Pts',(-10.591588783979,15.2,2.65235299830161));
#258435=CARTESIAN_POINT('Ctrl Pts',(-10.5964273130236,15.2,2.65194906423032));
#258436=CARTESIAN_POINT('Ctrl Pts',(-10.6012878251309,15.2,2.65153314726275));
#258437=CARTESIAN_POINT('Ctrl Pts',(-10.6080925429288,15.2,2.65095086343561));
#258438=CARTESIAN_POINT('Ctrl Pts',(-10.6149403430503,15.2,2.65034508626605));
#258439=CARTESIAN_POINT('Ctrl Pts',(-10.6218306334199,15.2,2.64971542556269));
#258440=CARTESIAN_POINT('Ctrl Pts',(-10.6267522693216,15.2,2.64926566792444));
#258441=CARTESIAN_POINT('Ctrl Pts',(-10.6316955836026,15.2,2.64880372468017));
#258442=CARTESIAN_POINT('Ctrl Pts',(-10.6366603589723,15.2,2.64832945627527));
#258443=CARTESIAN_POINT('Ctrl Pts',(-10.6406321794845,15.2,2.64795004153068));
#258444=CARTESIAN_POINT('Ctrl Pts',(-10.6446177371623,15.2,2.64756273816885));
#258445=CARTESIAN_POINT('Ctrl Pts',(-10.6486169209372,15.2,2.64716747670205));
#258446=CARTESIAN_POINT('Ctrl Pts',(-10.6526161041672,15.2,2.64677221528911));
#258447=CARTESIAN_POINT('Ctrl Pts',(-10.6566289131038,15.2,2.64636899471608));
#258448=CARTESIAN_POINT('Ctrl Pts',(-10.6606552421626,15.2,2.64595774608356));
#258449=CARTESIAN_POINT('Ctrl Pts',(-10.6656881538976,15.2,2.64544368525089));
#258450=CARTESIAN_POINT('Ctrl Pts',(-10.670742185986,15.2,2.64491708155677));
#258451=CARTESIAN_POINT('Ctrl Pts',(-10.6758171311932,15.2,2.64437779829354));
#258452=CARTESIAN_POINT('Ctrl Pts',(-10.6819070652207,15.2,2.64373065840118));
#258453=CARTESIAN_POINT('Ctrl Pts',(-10.6880271127384,15.2,2.64306526212345));
#258454=CARTESIAN_POINT('Ctrl Pts',(-10.6941769128464,15.2,2.64238138306622));
#258455=CARTESIAN_POINT('Ctrl Pts',(-10.6982767799574,15.2,2.64192546365333));
#258456=CARTESIAN_POINT('Ctrl Pts',(-10.7023898700862,15.2,2.64146132948965));
#258457=CARTESIAN_POINT('Ctrl Pts',(-10.7065160785333,15.2,2.64098891474169));
#258458=CARTESIAN_POINT('Ctrl Pts',(-10.7106422869804,15.2,2.64051649999372));
#258459=CARTESIAN_POINT('Ctrl Pts',(-10.7147816121763,15.2,2.64003580389756));
#258460=CARTESIAN_POINT('Ctrl Pts',(-10.7189339519039,15.2,2.63954676187006));
#258461=CARTESIAN_POINT('Ctrl Pts',(-10.7230862910658,15.2,2.63905771990918));
#258462=CARTESIAN_POINT('Ctrl Pts',(-10.7272516421309,15.2,2.63856033246128));
#258463=CARTESIAN_POINT('Ctrl Pts',(-10.7314299020305,15.2,2.63805453450036));
#258464=CARTESIAN_POINT('Ctrl Pts',(-10.7356081624993,15.2,2.63754873647052));
#258465=CARTESIAN_POINT('Ctrl Pts',(-10.7397993304653,15.2,2.63703452839668));
#258466=CARTESIAN_POINT('Ctrl Pts',(-10.7440033041957,15.2,2.63651184642289));
#258467=CARTESIAN_POINT('Ctrl Pts',(-10.7482072773533,15.2,2.6359891645203));
#258468=CARTESIAN_POINT('Ctrl Pts',(-10.7524240547621,15.2,2.63545800747438));
#258469=CARTESIAN_POINT('Ctrl Pts',(-10.7566535346377,15.2,2.63491831601906));
#258470=CARTESIAN_POINT('Ctrl Pts',(-10.7619403849144,15.2,2.63424370164476));
#258471=CARTESIAN_POINT('Ctrl Pts',(-10.7672470794841,15.2,2.63355574838688));
#258472=CARTESIAN_POINT('Ctrl Pts',(-10.7725734229804,15.2,2.63285433671706));
#258473=CARTESIAN_POINT('Ctrl Pts',(-10.7768344980098,15.2,2.63229320735063));
#258474=CARTESIAN_POINT('Ctrl Pts',(-10.7811081456632,15.2,2.63172346452397));
#258475=CARTESIAN_POINT('Ctrl Pts',(-10.7853942661758,15.2,2.63114504788044));
#258476=CARTESIAN_POINT('Ctrl Pts',(-10.7896803861045,15.2,2.63056663131573));
#258477=CARTESIAN_POINT('Ctrl Pts',(-10.7939789785343,15.2,2.6299795419577));
#258478=CARTESIAN_POINT('Ctrl Pts',(-10.7982899418477,15.2,2.62938371684031));
#258479=CARTESIAN_POINT('Ctrl Pts',(-10.80367864643,15.2,2.62863893538269));
#258480=CARTESIAN_POINT('Ctrl Pts',(-10.8090866831725,15.2,2.6278805081928));
#258481=CARTESIAN_POINT('Ctrl Pts',(-10.8145138527804,15.2,2.62710831825877));
#258482=CARTESIAN_POINT('Ctrl Pts',(-10.8188555887034,15.2,2.62649056627788));
#258483=CARTESIAN_POINT('Ctrl Pts',(-10.8232095703358,15.2,2.62586400675666));
#258484=CARTESIAN_POINT('Ctrl Pts',(-10.8275756994639,15.2,2.62522858088779));
#258485=CARTESIAN_POINT('Ctrl Pts',(-10.8330333605766,15.2,2.62443429859499));
#258486=CARTESIAN_POINT('Ctrl Pts',(-10.8385100004062,15.2,2.62362616499918));
#258487=CARTESIAN_POINT('Ctrl Pts',(-10.8440054265188,15.2,2.62280406590082));
#258488=CARTESIAN_POINT('Ctrl Pts',(-10.8473026820666,15.2,2.62231080645972));
#258489=CARTESIAN_POINT('Ctrl Pts',(-10.8506067004114,15.2,2.62181251942669));
#258490=CARTESIAN_POINT('Ctrl Pts',(-10.8539174406656,15.2,2.62130918191925));
#258491=CARTESIAN_POINT('Ctrl Pts',(-10.8572281809198,15.2,2.62080584441181));
#258492=CARTESIAN_POINT('Ctrl Pts',(-10.860545641766,15.2,2.62029745505909));
#258493=CARTESIAN_POINT('Ctrl Pts',(-10.8638697838541,15.2,2.6197839912023));
#258494=CARTESIAN_POINT('Ctrl Pts',(-10.8683019731037,15.2,2.61909937275767));
#258495=CARTESIAN_POINT('Ctrl Pts',(-10.8727460379981,15.2,2.61840573367598));
#258496=CARTESIAN_POINT('Ctrl Pts',(-10.8772018825215,15.2,2.61770301712324));
#258497=CARTESIAN_POINT('Ctrl Pts',(-10.8805437666729,15.2,2.61717597958901));
#258498=CARTESIAN_POINT('Ctrl Pts',(-10.8838922755763,15.2,2.61664383616167));
#258499=CARTESIAN_POINT('Ctrl Pts',(-10.8872473702314,15.2,2.61610656412456));
#258500=CARTESIAN_POINT('Ctrl Pts',(-10.8906024642771,15.2,2.61556929218505));
#258501=CARTESIAN_POINT('Ctrl Pts',(-10.8939641429551,15.2,2.61502689136876));
#258502=CARTESIAN_POINT('Ctrl Pts',(-10.8973323661684,15.2,2.61447933894403));
#258503=CARTESIAN_POINT('Ctrl Pts',(-10.9007005893817,15.2,2.6139317865193));
#258504=CARTESIAN_POINT('Ctrl Pts',(-10.9040753555576,15.2,2.61337908256931));
#258505=CARTESIAN_POINT('Ctrl Pts',(-10.9074566261437,15.2,2.61282120467246));
#258506=CARTESIAN_POINT('Ctrl Pts',(-10.9130920773252,15.2,2.61189140814393));
#258507=CARTESIAN_POINT('Ctrl Pts',(-10.918745592959,15.2,2.61094723813244));
#258508=CARTESIAN_POINT('Ctrl Pts',(-10.9244169899044,15.2,2.60998859243724));
#258509=CARTESIAN_POINT('Ctrl Pts',(-10.927819827948,15.2,2.60941340504101));
#258510=CARTESIAN_POINT('Ctrl Pts',(-10.9312291021117,15.2,2.60883300664756));
#258511=CARTESIAN_POINT('Ctrl Pts',(-10.9346447727948,15.2,2.60824737474949));
#258512=CARTESIAN_POINT('Ctrl Pts',(-10.9391990001654,15.2,2.60746653225419));
#258513=CARTESIAN_POINT('Ctrl Pts',(-10.9437645998298,15.2,2.6066763855033));
#258514=CARTESIAN_POINT('Ctrl Pts',(-10.94834147651,15.2,2.6058768843474));
#258515=CARTESIAN_POINT('Ctrl Pts',(-10.954062572828,15.2,2.60487750782083));
#258516=CARTESIAN_POINT('Ctrl Pts',(-10.959801291493,15.2,2.6038635137667));
#258517=CARTESIAN_POINT('Ctrl Pts',(-10.9655574468388,15.2,2.60283480314291));
#258518=CARTESIAN_POINT('Ctrl Pts',(-10.9690111405482,15.2,2.60221757667892));
#258519=CARTESIAN_POINT('Ctrl Pts',(-10.9724711114844,15.2,2.60159505305512));
#258520=CARTESIAN_POINT('Ctrl Pts',(-10.9759373212807,15.2,2.60096720912981));
#258521=CARTESIAN_POINT('Ctrl Pts',(-10.9817143361385,15.2,2.59992080285378));
#258522=CARTESIAN_POINT('Ctrl Pts',(-10.9875086812525,15.2,2.59885962227225));
#258523=CARTESIAN_POINT('Ctrl Pts',(-10.9933201720065,15.2,2.5977835700991));
#258524=CARTESIAN_POINT('Ctrl Pts',(-10.9968070673458,15.2,2.597137938631));
#258525=CARTESIAN_POINT('Ctrl Pts',(-11.0003001364035,15.2,2.59648695288639));
#258526=CARTESIAN_POINT('Ctrl Pts',(-11.0037993392462,15.2,2.59583059333193));
#258527=CARTESIAN_POINT('Ctrl Pts',(-11.008464941977,15.2,2.59495544745805));
#258528=CARTESIAN_POINT('Ctrl Pts',(-11.0131414509675,15.2,2.59407074614098));
#258529=CARTESIAN_POINT('Ctrl Pts',(-11.0178287729169,15.2,2.59317644304804));
#258530=CARTESIAN_POINT('Ctrl Pts',(-11.022516095505,15.2,2.59228213983327));
#258531=CARTESIAN_POINT('Ctrl Pts',(-11.0272142319166,15.2,2.59137823483956));
#258532=CARTESIAN_POINT('Ctrl Pts',(-11.0319230906184,15.2,2.59046467840025));
#258533=CARTESIAN_POINT('Ctrl Pts',(-11.0366319486786,15.2,2.58955112208541));
#258534=CARTESIAN_POINT('Ctrl Pts',(-11.0413515286011,15.2,2.5886279166965));
#258535=CARTESIAN_POINT('Ctrl Pts',(-11.0460817408387,15.2,2.58769501356034));
#258536=CARTESIAN_POINT('Ctrl Pts',(-11.0508119537207,15.2,2.58676211029707));
#258537=CARTESIAN_POINT('Ctrl Pts',(-11.0555527982678,15.2,2.58581951063295));
#258538=CARTESIAN_POINT('Ctrl Pts',(-11.0603041836385,15.2,2.58486716741374));
#258539=CARTESIAN_POINT('Ctrl Pts',(-11.0650555683619,15.2,2.58391482432429));
#258540=CARTESIAN_POINT('Ctrl Pts',(-11.0698174947693,15.2,2.58295273705902));
#258541=CARTESIAN_POINT('Ctrl Pts',(-11.0745898722114,15.2,2.58198086141725));
#258542=CARTESIAN_POINT('Ctrl Pts',(-11.0805553445017,15.2,2.58076601676573));
#258543=CARTESIAN_POINT('Ctrl Pts',(-11.086537149533,15.2,2.57953587896683));
#258544=CARTESIAN_POINT('Ctrl Pts',(-11.0925351095538,15.2,2.57829035591956));
#258545=CARTESIAN_POINT('Ctrl Pts',(-11.0961338854355,15.2,2.57754304211835));
#258546=CARTESIAN_POINT('Ctrl Pts',(-11.0997384767949,15.2,2.57679019042038));
#258547=CARTESIAN_POINT('Ctrl Pts',(-11.1033488474546,15.2,2.57603178215702));
#258548=CARTESIAN_POINT('Ctrl Pts',(-11.1069592187702,15.2,2.57527337375588));
#258549=CARTESIAN_POINT('Ctrl Pts',(-11.1105753692291,15.2,2.57450940866153));
#258550=CARTESIAN_POINT('Ctrl Pts',(-11.1141972605479,15.2,2.57373986825726));
#258551=CARTESIAN_POINT('Ctrl Pts',(-11.1178191512088,15.2,2.57297032799279));
#258552=CARTESIAN_POINT('Ctrl Pts',(-11.1214467828943,15.2,2.57219521320362));
#258553=CARTESIAN_POINT('Ctrl Pts',(-11.1250801209295,15.2,2.57141450489817));
#258554=CARTESIAN_POINT('Ctrl Pts',(-11.1287134589646,15.2,2.57063379659272));
#258555=CARTESIAN_POINT('Ctrl Pts',(-11.1323525006858,15.2,2.56984749530749));
#258556=CARTESIAN_POINT('Ctrl Pts',(-11.1359972102783,15.2,2.56905558195764));
#258557=CARTESIAN_POINT('Ctrl Pts',(-11.1396419198708,15.2,2.56826366860779));
#258558=CARTESIAN_POINT('Ctrl Pts',(-11.1432922952129,15.2,2.56746614310853));
#258559=CARTESIAN_POINT('Ctrl Pts',(-11.1469482994717,15.2,2.56666298730075));
#258560=CARTESIAN_POINT('Ctrl Pts',(-11.1518229722595,15.2,2.56559211279311));
#258561=CARTESIAN_POINT('Ctrl Pts',(-11.1567076530547,15.2,2.56451122921546));
#258562=CARTESIAN_POINT('Ctrl Pts',(-11.1616022611003,15.2,2.56342029682165));
#258563=CARTESIAN_POINT('Ctrl Pts',(-11.1664968684789,15.2,2.56232936457648));
#258564=CARTESIAN_POINT('Ctrl Pts',(-11.171401405698,15.2,2.56122838669093));
#258565=CARTESIAN_POINT('Ctrl Pts',(-11.1763157775734,15.2,2.56011731561576));
#258566=CARTESIAN_POINT('Ctrl Pts',(-11.1812301501183,15.2,2.5590062443892));
#258567=CARTESIAN_POINT('Ctrl Pts',(-11.1861543535804,15.2,2.55788507840765));
#258568=CARTESIAN_POINT('Ctrl Pts',(-11.1910882907077,15.2,2.55675377134414));
#258569=CARTESIAN_POINT('Ctrl Pts',(-11.1947887432171,15.2,2.55590529112359));
#258570=CARTESIAN_POINT('Ctrl Pts',(-11.1984946707624,15.2,2.55505110767388));
#258571=CARTESIAN_POINT('Ctrl Pts',(-11.2022060574113,15.2,2.5541912121441));
#258572=CARTESIAN_POINT('Ctrl Pts',(-11.2059174440601,15.2,2.55333131661431));
#258573=CARTESIAN_POINT('Ctrl Pts',(-11.209634289429,15.2,2.55246571060184));
#258574=CARTESIAN_POINT('Ctrl Pts',(-11.2133565920001,15.2,2.55159438999998));
#258575=CARTESIAN_POINT('Ctrl Pts',(-10.0330625580001,12.2,2.64164356399998));
#258576=CARTESIAN_POINT('Ctrl Pts',(-10.03482302717,12.2,2.64194831044285));
#258577=CARTESIAN_POINT('Ctrl Pts',(-10.0366407484416,12.2,2.64225751971682));
#258578=CARTESIAN_POINT('Ctrl Pts',(-10.0385148615364,12.2,2.64257038294905));
#258579=CARTESIAN_POINT('Ctrl Pts',(-10.0403980125518,12.2,2.64288475496593));
#258580=CARTESIAN_POINT('Ctrl Pts',(-10.0423381038147,12.2,2.64320281628067));
#258581=CARTESIAN_POINT('Ctrl Pts',(-10.0443343061932,12.2,2.64352378181437));
#258582=CARTESIAN_POINT('Ctrl Pts',(-10.0463305083903,12.2,2.64384474731891));
#258583=CARTESIAN_POINT('Ctrl Pts',(-10.0483828189766,12.2,2.64416861768683));
#258584=CARTESIAN_POINT('Ctrl Pts',(-10.0504904282333,12.2,2.64449462925831));
#258585=CARTESIAN_POINT('Ctrl Pts',(-10.05259803749,12.2,2.6448206408298));
#258586=CARTESIAN_POINT('Ctrl Pts',(-10.0547609456752,12.2,2.64514879427203));
#258587=CARTESIAN_POINT('Ctrl Pts',(-10.0569783630356,12.2,2.6454783536931));
#258588=CARTESIAN_POINT('Ctrl Pts',(-10.0591957805974,12.2,2.64580791314411));
#258589=CARTESIAN_POINT('Ctrl Pts',(-10.0614677060147,12.2,2.64613887440968));
#258590=CARTESIAN_POINT('Ctrl Pts',(-10.0637933707285,12.2,2.64647052701114));
#258591=CARTESIAN_POINT('Ctrl Pts',(-10.066119035231,12.2,2.64680217958246));
#258592=CARTESIAN_POINT('Ctrl Pts',(-10.0684984395783,12.2,2.64713451980237));
#258593=CARTESIAN_POINT('Ctrl Pts',(-10.0709308320011,12.2,2.6474668565418));
#258594=CARTESIAN_POINT('Ctrl Pts',(-10.0733632244239,12.2,2.64779919328124));
#258595=CARTESIAN_POINT('Ctrl Pts',(-10.0758486046314,12.2,2.64813152376893));
#258596=CARTESIAN_POINT('Ctrl Pts',(-10.0783862401202,12.2,2.64846317850691));
#258597=CARTESIAN_POINT('Ctrl Pts',(-10.0809238758396,12.2,2.648794833275));
#258598=CARTESIAN_POINT('Ctrl Pts',(-10.0835137669738,12.2,2.64912580913471));
#258599=CARTESIAN_POINT('Ctrl Pts',(-10.0861551977879,12.2,2.64945545331925));
#258600=CARTESIAN_POINT('Ctrl Pts',(-10.0892368667112,12.2,2.64984003815631));
#258601=CARTESIAN_POINT('Ctrl Pts',(-10.0923886860307,12.2,2.65022281240024));
#258602=CARTESIAN_POINT('Ctrl Pts',(-10.0956095477997,12.2,2.6506027689739));
#258603=CARTESIAN_POINT('Ctrl Pts',(-10.0983702867813,12.2,2.65092844607506));
#258604=CARTESIAN_POINT('Ctrl Pts',(-10.1011817504025,12.2,2.65125205333433));
#258605=CARTESIAN_POINT('Ctrl Pts',(-10.1040432585619,12.2,2.6515729785183));
#258606=CARTESIAN_POINT('Ctrl Pts',(-10.1069047664613,12.2,2.65189390367312));
#258607=CARTESIAN_POINT('Ctrl Pts',(-10.109816319292,12.2,2.6522121451454));
#258608=CARTESIAN_POINT('Ctrl Pts',(-10.1127772501032,12.2,2.65252710930047));
#258609=CARTESIAN_POINT('Ctrl Pts',(-10.1157381809144,12.2,2.65284207345556));
#258610=CARTESIAN_POINT('Ctrl Pts',(-10.118748489905,12.2,2.65315375821922));
#258611=CARTESIAN_POINT('Ctrl Pts',(-10.1218075248751,12.2,2.6534615854582));
#258612=CARTESIAN_POINT('Ctrl Pts',(-10.1248665598452,12.2,2.65376941269718));
#258613=CARTESIAN_POINT('Ctrl Pts',(-10.1279743222156,12.2,2.65407338062792));
#258614=CARTESIAN_POINT('Ctrl Pts',(-10.131130171181,12.2,2.65437292795067));
#258615=CARTESIAN_POINT('Ctrl Pts',(-10.1342860204331,12.2,2.65467247530064));
#258616=CARTESIAN_POINT('Ctrl Pts',(-10.1374899582731,12.2,2.65496760035852));
#258617=CARTESIAN_POINT('Ctrl Pts',(-10.1407413577024,12.2,2.65525775479079));
#258618=CARTESIAN_POINT('Ctrl Pts',(-10.1439927568363,12.2,2.65554790919669));
#258619=CARTESIAN_POINT('Ctrl Pts',(-10.1472916205581,12.2,2.65583309476966));
#258620=CARTESIAN_POINT('Ctrl Pts',(-10.1506373326012,12.2,2.65611277450973));
#258621=CARTESIAN_POINT('Ctrl Pts',(-10.1539830446442,12.2,2.6563924542498));
#258622=CARTESIAN_POINT('Ctrl Pts',(-10.1573756074199,12.2,2.65666663162176));
#258623=CARTESIAN_POINT('Ctrl Pts',(-10.1608144186252,12.2,2.65693478419576));
#258624=CARTESIAN_POINT('Ctrl Pts',(-10.1642532301428,12.2,2.65720293679412));
#258625=CARTESIAN_POINT('Ctrl Pts',(-10.1677382903315,12.2,2.65746506659192));
#258626=CARTESIAN_POINT('Ctrl Pts',(-10.1712690116926,12.2,2.65772066535557));
#258627=CARTESIAN_POINT('Ctrl Pts',(-10.1747997327329,12.2,2.65797626409599));
#258628=CARTESIAN_POINT('Ctrl Pts',(-10.1783761121886,12.2,2.65822533255757));
#258629=CARTESIAN_POINT('Ctrl Pts',(-10.18199757349,12.2,2.65846738004989));
#258630=CARTESIAN_POINT('Ctrl Pts',(-10.1862226118943,12.2,2.65874976880558));
#258631=CARTESIAN_POINT('Ctrl Pts',(-10.1905090113944,12.2,2.6590225943752));
#258632=CARTESIAN_POINT('Ctrl Pts',(-10.1948558718532,12.2,2.6592851022539));
#258633=CARTESIAN_POINT('Ctrl Pts',(-10.1992027319736,12.2,2.65954761011216));
#258634=CARTESIAN_POINT('Ctrl Pts',(-10.203610053331,12.2,2.65979979572518));
#258635=CARTESIAN_POINT('Ctrl Pts',(-10.2080769531326,12.2,2.66004092325247));
#258636=CARTESIAN_POINT('Ctrl Pts',(-10.2119057248383,12.2,2.66024760401429));
#258637=CARTESIAN_POINT('Ctrl Pts',(-10.2157782698399,12.2,2.660446157467));
#258638=CARTESIAN_POINT('Ctrl Pts',(-10.2196940444719,12.2,2.66063613431031));
#258639=CARTESIAN_POINT('Ctrl Pts',(-10.2242624476756,12.2,2.66085777393497));
#258640=CARTESIAN_POINT('Ctrl Pts',(-10.228889688663,12.2,2.66106773679313));
#258641=CARTESIAN_POINT('Ctrl Pts',(-10.2335749198123,12.2,2.66126532344821));
#258642=CARTESIAN_POINT('Ctrl Pts',(-10.2369215136987,12.2,2.66140645678205));
#258643=CARTESIAN_POINT('Ctrl Pts',(-10.2402976952847,12.2,2.66154127628825));
#258644=CARTESIAN_POINT('Ctrl Pts',(-10.2437031600046,12.2,2.66166953302489));
#258645=CARTESIAN_POINT('Ctrl Pts',(-10.2471086247244,12.2,2.66179778976154));
#258646=CARTESIAN_POINT('Ctrl Pts',(-10.250543372977,12.2,2.66191948415265));
#258647=CARTESIAN_POINT('Ctrl Pts',(-10.2540071046063,12.2,2.66203437172831));
#258648=CARTESIAN_POINT('Ctrl Pts',(-10.2574708362357,12.2,2.66214925930396));
#258649=CARTESIAN_POINT('Ctrl Pts',(-10.2609635511991,12.2,2.66225733933743));
#258650=CARTESIAN_POINT('Ctrl Pts',(-10.2644849542532,12.2,2.66235837447669));
#258651=CARTESIAN_POINT('Ctrl Pts',(-10.2680063573072,12.2,2.66245940961594));
#258652=CARTESIAN_POINT('Ctrl Pts',(-10.2715564484343,12.2,2.66255339894946));
#258653=CARTESIAN_POINT('Ctrl Pts',(-10.2751349355161,12.2,2.66264010901929));
#258654=CARTESIAN_POINT('Ctrl Pts',(-10.278713422598,12.2,2.66272681908912));
#258655=CARTESIAN_POINT('Ctrl Pts',(-10.2823203051538,12.2,2.66280624829962));
#258656=CARTESIAN_POINT('Ctrl Pts',(-10.2859552964897,12.2,2.6628781685083));
#258657=CARTESIAN_POINT('Ctrl Pts',(-10.2895902878256,12.2,2.66295008871698));
#258658=CARTESIAN_POINT('Ctrl Pts',(-10.2932533863666,12.2,2.66301450025556));
#258659=CARTESIAN_POINT('Ctrl Pts',(-10.2969443094916,12.2,2.66307117699167));
#258660=CARTESIAN_POINT('Ctrl Pts',(-10.3006352326166,12.2,2.66312785372779));
#258661=CARTESIAN_POINT('Ctrl Pts',(-10.3043539787127,12.2,2.6631767950832));
#258662=CARTESIAN_POINT('Ctrl Pts',(-10.3081002692854,12.2,2.66321778195836));
#258663=CARTESIAN_POINT('Ctrl Pts',(-10.311846559858,12.2,2.66325876883353));
#258664=CARTESIAN_POINT('Ctrl Pts',(-10.3156203929251,12.2,2.66329180036868));
#258665=CARTESIAN_POINT('Ctrl Pts',(-10.3194214920237,12.2,2.66331665974325));
#258666=CARTESIAN_POINT('Ctrl Pts',(-10.3232225911224,12.2,2.66334151911782));
#258667=CARTESIAN_POINT('Ctrl Pts',(-10.3270509570675,12.2,2.66335820737315));
#258668=CARTESIAN_POINT('Ctrl Pts',(-10.330906315194,12.2,2.66336651098383));
#258669=CARTESIAN_POINT('Ctrl Pts',(-10.3347616733204,12.2,2.66337481459451));
#258670=CARTESIAN_POINT('Ctrl Pts',(-10.3386440226234,12.2,2.66337473393888));
#258671=CARTESIAN_POINT('Ctrl Pts',(-10.3425530959455,12.2,2.66336606171563));
#258672=CARTESIAN_POINT('Ctrl Pts',(-10.3464621692677,12.2,2.66335738949238));
#258673=CARTESIAN_POINT('Ctrl Pts',(-10.3503979631216,12.2,2.66334012386954));
#258674=CARTESIAN_POINT('Ctrl Pts',(-10.3543602129849,12.2,2.66331406247993));
#258675=CARTESIAN_POINT('Ctrl Pts',(-10.3583224628482,12.2,2.66328800109032));
#258676=CARTESIAN_POINT('Ctrl Pts',(-10.3623111670841,12.2,2.66325314366167));
#258677=CARTESIAN_POINT('Ctrl Pts',(-10.3663260620168,12.2,2.66320928824427));
#258678=CARTESIAN_POINT('Ctrl Pts',(-10.3703409569495,12.2,2.66316543282687));
#258679=CARTESIAN_POINT('Ctrl Pts',(-10.3743820438965,12.2,2.66311258126487));
#258680=CARTESIAN_POINT('Ctrl Pts',(-10.378449059732,12.2,2.66305053425022));
#258681=CARTESIAN_POINT('Ctrl Pts',(-10.3825160751241,12.2,2.66298848724234));
#258682=CARTESIAN_POINT('Ctrl Pts',(-10.3866090221234,12.2,2.66291724777322));
#258683=CARTESIAN_POINT('Ctrl Pts',(-10.3907276399363,12.2,2.66283662076889));
#258684=CARTESIAN_POINT('Ctrl Pts',(-10.3948462581981,12.2,2.66275599375577));
#258685=CARTESIAN_POINT('Ctrl Pts',(-10.3989905482511,12.2,2.66266598068448));
#258686=CARTESIAN_POINT('Ctrl Pts',(-10.4031602556796,12.2,2.6625663895047));
#258687=CARTESIAN_POINT('Ctrl Pts',(-10.4064960218042,12.2,2.66248671655653));
#258688=CARTESIAN_POINT('Ctrl Pts',(-10.4098480541839,12.2,2.66240091538874));
#258689=CARTESIAN_POINT('Ctrl Pts',(-10.413216224994,12.2,2.66230888971661));
#258690=CARTESIAN_POINT('Ctrl Pts',(-10.417426438277,12.2,2.66219385763273));
#258691=CARTESIAN_POINT('Ctrl Pts',(-10.4216618660052,12.2,2.66206910120277));
#258692=CARTESIAN_POINT('Ctrl Pts',(-10.4259222592704,12.2,2.66193443425781));
#258693=CARTESIAN_POINT('Ctrl Pts',(-10.429330573604,12.2,2.66182670071065));
#258694=CARTESIAN_POINT('Ctrl Pts',(-10.4327548650065,12.2,2.66171262592865));
#258695=CARTESIAN_POINT('Ctrl Pts',(-10.4361950074459,12.2,2.66159211699471));
#258696=CARTESIAN_POINT('Ctrl Pts',(-10.439635150354,12.2,2.66147160804435));
#258697=CARTESIAN_POINT('Ctrl Pts',(-10.443091144714,12.2,2.66134466509394));
#258698=CARTESIAN_POINT('Ctrl Pts',(-10.4465628642524,12.2,2.66121119747492));
#258699=CARTESIAN_POINT('Ctrl Pts',(-10.4500345833177,12.2,2.66107772987409));
#258700=CARTESIAN_POINT('Ctrl Pts',(-10.4535220267819,12.2,2.66093773750299));
#258701=CARTESIAN_POINT('Ctrl Pts',(-10.4570250711606,12.2,2.66079113001565));
#258702=CARTESIAN_POINT('Ctrl Pts',(-10.4605281160166,12.2,2.66064452250833));
#258703=CARTESIAN_POINT('Ctrl Pts',(-10.4640467619129,12.2,2.6604913010754));
#258704=CARTESIAN_POINT('Ctrl Pts',(-10.4675808842167,12.2,2.66033137673335));
#258705=CARTESIAN_POINT('Ctrl Pts',(-10.4711150065204,12.2,2.6601714523913));
#258706=CARTESIAN_POINT('Ctrl Pts',(-10.4746646061037,12.2,2.66000482464013));
#258707=CARTESIAN_POINT('Ctrl Pts',(-10.4782295602995,12.2,2.65983140646332));
#258708=CARTESIAN_POINT('Ctrl Pts',(-10.4817945140097,12.2,2.65965798831013));
#258709=CARTESIAN_POINT('Ctrl Pts',(-10.4853748226669,12.2,2.65947777970233));
#258710=CARTESIAN_POINT('Ctrl Pts',(-10.4889703632225,12.2,2.65929069671681));
#258711=CARTESIAN_POINT('Ctrl Pts',(-10.4934647892845,12.2,2.65905684296577));
#258712=CARTESIAN_POINT('Ctrl Pts',(-10.4979830183889,12.2,2.65881224421668));
#258713=CARTESIAN_POINT('Ctrl Pts',(-10.502524812,12.2,2.65855673650835));
#258714=CARTESIAN_POINT('Ctrl Pts',(-10.5061582470869,12.2,2.65835233033054));
#258715=CARTESIAN_POINT('Ctrl Pts',(-10.5098067662061,12.2,2.65814094404915));
#258716=CARTESIAN_POINT('Ctrl Pts',(-10.513470246574,12.2,2.65792249248096));
#258717=CARTESIAN_POINT('Ctrl Pts',(-10.5171337264427,12.2,2.65770404094254));
#258718=CARTESIAN_POINT('Ctrl Pts',(-10.5208121710743,12.2,2.65747852370163));
#258719=CARTESIAN_POINT('Ctrl Pts',(-10.5245054589558,12.2,2.65724586077517));
#258720=CARTESIAN_POINT('Ctrl Pts',(-10.5281987473405,12.2,2.65701319781701));
#258721=CARTESIAN_POINT('Ctrl Pts',(-10.5319068808099,12.2,2.65677338729882));
#258722=CARTESIAN_POINT('Ctrl Pts',(-10.5356297411254,12.2,2.65652635045129));
#258723=CARTESIAN_POINT('Ctrl Pts',(-10.5393526009336,12.2,2.65627931363741));
#258724=CARTESIAN_POINT('Ctrl Pts',(-10.54309018764,12.2,2.65602504855502));
#258725=CARTESIAN_POINT('Ctrl Pts',(-10.5468423854434,12.2,2.65576347702133));
#258726=CARTESIAN_POINT('Ctrl Pts',(-10.550594583758,12.2,2.65550190545199));
#258727=CARTESIAN_POINT('Ctrl Pts',(-10.5543613915386,12.2,2.65523302726716));
#258728=CARTESIAN_POINT('Ctrl Pts',(-10.5581426953238,12.2,2.65495676245988));
#258729=CARTESIAN_POINT('Ctrl Pts',(-10.5619239985937,12.2,2.65468049769025));
#258730=CARTESIAN_POINT('Ctrl Pts',(-10.5657197953511,12.2,2.65439684764667));
#258731=CARTESIAN_POINT('Ctrl Pts',(-10.5695299737053,12.2,2.65410573428208));
#258732=CARTESIAN_POINT('Ctrl Pts',(-10.5733401525787,12.2,2.65381462087781));
#258733=CARTESIAN_POINT('Ctrl Pts',(-10.5771647104288,12.2,2.65351604401432));
#258734=CARTESIAN_POINT('Ctrl Pts',(-10.5810035348056,12.2,2.65320992844158));
#258735=CARTESIAN_POINT('Ctrl Pts',(-10.5848423586594,12.2,2.65290381291056));
#258736=CARTESIAN_POINT('Ctrl Pts',(-10.5886954486575,12.2,2.65259015798294));
#258737=CARTESIAN_POINT('Ctrl Pts',(-10.5925626914223,12.2,2.65226888727159));
#258738=CARTESIAN_POINT('Ctrl Pts',(-10.5973967452733,12.2,2.65186729884958));
#258739=CARTESIAN_POINT('Ctrl Pts',(-10.6022529151322,12.2,2.65145381360492));
#258740=CARTESIAN_POINT('Ctrl Pts',(-10.6071309772144,12.2,2.65102828374444));
#258741=CARTESIAN_POINT('Ctrl Pts',(-10.6110334270929,12.2,2.65068785983749));
#258742=CARTESIAN_POINT('Ctrl Pts',(-10.6149498913674,12.2,2.65033972961297));
#258743=CARTESIAN_POINT('Ctrl Pts',(-10.6188802558048,12.2,2.64998381870418));
#258744=CARTESIAN_POINT('Ctrl Pts',(-10.6228106197066,12.2,2.64962790784388));
#258745=CARTESIAN_POINT('Ctrl Pts',(-10.6267548853194,12.2,2.64926421491916));
#258746=CARTESIAN_POINT('Ctrl Pts',(-10.6307129431924,12.2,2.64889267082055));
#258747=CARTESIAN_POINT('Ctrl Pts',(-10.6346710016047,12.2,2.64852112667131));
#258748=CARTESIAN_POINT('Ctrl Pts',(-10.638642849069,12.2,2.64814172973713));
#258749=CARTESIAN_POINT('Ctrl Pts',(-10.6426283788426,12.2,2.64775440899328));
#258750=CARTESIAN_POINT('Ctrl Pts',(-10.6466139080733,12.2,2.6473670883022));
#258751=CARTESIAN_POINT('Ctrl Pts',(-10.6506131188344,12.2,2.64697184454883));
#258752=CARTESIAN_POINT('Ctrl Pts',(-10.6546259013939,12.2,2.64656860658261));
#258753=CARTESIAN_POINT('Ctrl Pts',(-10.6586386845001,12.2,2.64616536856145));
#258754=CARTESIAN_POINT('Ctrl Pts',(-10.6626650414104,12.2,2.64575413726732));
#258755=CARTESIAN_POINT('Ctrl Pts',(-10.6667048612417,12.2,2.64533484380002));
#258756=CARTESIAN_POINT('Ctrl Pts',(-10.670744681073,12.2,2.64491555033272));
#258757=CARTESIAN_POINT('Ctrl Pts',(-10.6747979656919,12.2,2.64448819331727));
#258758=CARTESIAN_POINT('Ctrl Pts',(-10.6788646069149,12.2,2.64405270590381));
#258759=CARTESIAN_POINT('Ctrl Pts',(-10.6829312475838,12.2,2.64361721854969));
#258760=CARTESIAN_POINT('Ctrl Pts',(-10.6870112457855,12.2,2.64317360013207));
#258761=CARTESIAN_POINT('Ctrl Pts',(-10.6911044942472,12.2,2.64272178350032));
#258762=CARTESIAN_POINT('Ctrl Pts',(-10.6951977432666,12.2,2.64226996680701));
#258763=CARTESIAN_POINT('Ctrl Pts',(-10.6993042410894,12.2,2.64180995286649));
#258764=CARTESIAN_POINT('Ctrl Pts',(-10.7034238841486,12.2,2.64134167417345));
#258765=CARTESIAN_POINT('Ctrl Pts',(-10.7075435266465,12.2,2.64087339554422));
#258766=CARTESIAN_POINT('Ctrl Pts',(-10.7116763128343,12.2,2.64039685306885));
#258767=CARTESIAN_POINT('Ctrl Pts',(-10.7158221381612,12.2,2.63991197983125));
#258768=CARTESIAN_POINT('Ctrl Pts',(-10.7210044202435,12.2,2.6393058882347));
#258769=CARTESIAN_POINT('Ctrl Pts',(-10.7262070767291,12.2,2.6386867820032));
#258770=CARTESIAN_POINT('Ctrl Pts',(-10.7314299020305,12.2,2.63805453450036));
#258771=CARTESIAN_POINT('Ctrl Pts',(-10.7356081624994,12.2,2.63754873647052));
#258772=CARTESIAN_POINT('Ctrl Pts',(-10.7397993304653,12.2,2.63703452839668));
#258773=CARTESIAN_POINT('Ctrl Pts',(-10.7440033041957,12.2,2.63651184642289));
#258774=CARTESIAN_POINT('Ctrl Pts',(-10.7482072773534,12.2,2.6359891645203));
#258775=CARTESIAN_POINT('Ctrl Pts',(-10.7524240547621,12.2,2.63545800747438));
#258776=CARTESIAN_POINT('Ctrl Pts',(-10.7566535346377,12.2,2.63491831601906));
#258777=CARTESIAN_POINT('Ctrl Pts',(-10.7608830150896,12.2,2.63437862449021));
#258778=CARTESIAN_POINT('Ctrl Pts',(-10.7651251963219,12.2,2.63383039630031));
#258779=CARTESIAN_POINT('Ctrl Pts',(-10.7693799771008,12.2,2.63327356968584));
#258780=CARTESIAN_POINT('Ctrl Pts',(-10.7736347573,12.2,2.63271674314724));
#258781=CARTESIAN_POINT('Ctrl Pts',(-10.7779021379148,12.2,2.63215131836604));
#258782=CARTESIAN_POINT('Ctrl Pts',(-10.7821820151752,12.2,2.6315772350802));
#258783=CARTESIAN_POINT('Ctrl Pts',(-10.7864618930188,12.2,2.63100315171615));
#258784=CARTESIAN_POINT('Ctrl Pts',(-10.79075426925,12.2,2.63042040926217));
#258785=CARTESIAN_POINT('Ctrl Pts',(-10.795059041152,12.2,2.62982894845158));
#258786=CARTESIAN_POINT('Ctrl Pts',(-10.7993638124676,12.2,2.62923748772159));
#258787=CARTESIAN_POINT('Ctrl Pts',(-10.8036809803244,12.2,2.62863730645432));
#258788=CARTESIAN_POINT('Ctrl Pts',(-10.8080104451302,12.2,2.62802834786334));
#258789=CARTESIAN_POINT('Ctrl Pts',(-10.8123399105258,12.2,2.62741938918938));
#258790=CARTESIAN_POINT('Ctrl Pts',(-10.8166816714485,12.2,2.62680165148344));
#258791=CARTESIAN_POINT('Ctrl Pts',(-10.8210356286311,12.2,2.62617507744871));
#258792=CARTESIAN_POINT('Ctrl Pts',(-10.8253895852204,12.2,2.62554850349936));
#258793=CARTESIAN_POINT('Ctrl Pts',(-10.8297557382045,12.2,2.62491309212122));
#258794=CARTESIAN_POINT('Ctrl Pts',(-10.8341339887342,12.2,2.62426878689703));
#258795=CARTESIAN_POINT('Ctrl Pts',(-10.8385122398604,12.2,2.62362448158504));
#258796=CARTESIAN_POINT('Ctrl Pts',(-10.8429025879486,12.2,2.62297128163036));
#258797=CARTESIAN_POINT('Ctrl Pts',(-10.8473049339863,12.2,2.6223091297579));
#258798=CARTESIAN_POINT('Ctrl Pts',(-10.8517072794243,12.2,2.62164697797566));
#258799=CARTESIAN_POINT('Ctrl Pts',(-10.8561216243894,12.2,2.62097587577692));
#258800=CARTESIAN_POINT('Ctrl Pts',(-10.8605478690263,12.2,2.62029576461122));
#258801=CARTESIAN_POINT('Ctrl Pts',(-10.8638675532579,12.2,2.61978568112111));
#258802=CARTESIAN_POINT('Ctrl Pts',(-10.867193932208,12.2,2.6192705312129));
#258803=CARTESIAN_POINT('Ctrl Pts',(-10.870526963485,12.2,2.61875029117827));
#258804=CARTESIAN_POINT('Ctrl Pts',(-10.8738599941564,12.2,2.61823005123815));
#258805=CARTESIAN_POINT('Ctrl Pts',(-10.8771996784692,12.2,2.61770472058996));
#258806=CARTESIAN_POINT('Ctrl Pts',(-10.8805459741399,12.2,2.61717427669212));
#258807=CARTESIAN_POINT('Ctrl Pts',(-10.8838922698105,12.2,2.61664383279428));
#258808=CARTESIAN_POINT('Ctrl Pts',(-10.8872451778432,12.2,2.61610827563236));
#258809=CARTESIAN_POINT('Ctrl Pts',(-10.8906046570281,12.2,2.61556758177453));
#258810=CARTESIAN_POINT('Ctrl Pts',(-10.893964136213,12.2,2.61502688791669));
#258811=CARTESIAN_POINT('Ctrl Pts',(-10.8973301875375,12.2,2.61448105781631));
#258812=CARTESIAN_POINT('Ctrl Pts',(-10.9007027682636,12.2,2.61393006845885));
#258813=CARTESIAN_POINT('Ctrl Pts',(-10.9040753489897,12.2,2.61337907910139));
#258814=CARTESIAN_POINT('Ctrl Pts',(-10.9074544607047,12.2,2.6128229312236));
#258815=CARTESIAN_POINT('Ctrl Pts',(-10.9108400623728,12.2,2.61226160132779));
#258816=CARTESIAN_POINT('Ctrl Pts',(-10.9142256640408,12.2,2.61170027143197));
#258817=CARTESIAN_POINT('Ctrl Pts',(-10.9176177555835,12.2,2.61113375971984));
#258818=CARTESIAN_POINT('Ctrl Pts',(-10.9210162977091,12.2,2.61056204386632));
#258819=CARTESIAN_POINT('Ctrl Pts',(-10.9244148404522,12.2,2.60999032790894));
#258820=CARTESIAN_POINT('Ctrl Pts',(-10.9278198335137,12.2,2.60941340837509));
#258821=CARTESIAN_POINT('Ctrl Pts',(-10.9312312362187,12.2,2.60883126287311));
#258822=CARTESIAN_POINT('Ctrl Pts',(-10.9346426383039,12.2,2.60824911747688));
#258823=CARTESIAN_POINT('Ctrl Pts',(-10.9380604499318,12.2,2.60766174579399));
#258824=CARTESIAN_POINT('Ctrl Pts',(-10.9414846321876,12.2,2.60706912636864));
#258825=CARTESIAN_POINT('Ctrl Pts',(-10.9449088144433,12.2,2.60647650694329));
#258826=CARTESIAN_POINT('Ctrl Pts',(-10.948339365949,12.2,2.60587863986274));
#258827=CARTESIAN_POINT('Ctrl Pts',(-10.9517762486164,12.2,2.60527550346752));
#258828=CARTESIAN_POINT('Ctrl Pts',(-10.9552131312838,12.2,2.60467236707231));
#258829=CARTESIAN_POINT('Ctrl Pts',(-10.9586563445253,12.2,2.60406396109439));
#258830=CARTESIAN_POINT('Ctrl Pts',(-10.96210584815,12.2,2.60345026424169));
#258831=CARTESIAN_POINT('Ctrl Pts',(-10.9655553517747,12.2,2.60283656738899));
#258832=CARTESIAN_POINT('Ctrl Pts',(-10.9690111455824,12.2,2.6022175800115));
#258833=CARTESIAN_POINT('Ctrl Pts',(-10.9724731916228,12.2,2.60159328057632));
#258834=CARTESIAN_POINT('Ctrl Pts',(-10.9759352376631,12.2,2.60096898114113));
#258835=CARTESIAN_POINT('Ctrl Pts',(-10.9794035345646,12.2,2.60033936826418));
#258836=CARTESIAN_POINT('Ctrl Pts',(-10.9828780448195,12.2,2.59970442338115));
#258837=CARTESIAN_POINT('Ctrl Pts',(-10.9863525550745,12.2,2.59906947849812));
#258838=CARTESIAN_POINT('Ctrl Pts',(-10.9898332773007,12.2,2.59842920144991));
#258839=CARTESIAN_POINT('Ctrl Pts',(-10.9933201720065,12.2,2.5977835700991));
#258840=CARTESIAN_POINT('Ctrl Pts',(-10.9968070673458,12.2,2.597137938631));
#258841=CARTESIAN_POINT('Ctrl Pts',(-11.0003001364035,12.2,2.59648695288639));
#258842=CARTESIAN_POINT('Ctrl Pts',(-11.0037993392462,12.2,2.59583059333193));
#258843=CARTESIAN_POINT('Ctrl Pts',(-11.0072985414532,12.2,2.59517423389671));
#258844=CARTESIAN_POINT('Ctrl Pts',(-11.0108038780099,12.2,2.59451249955344));
#258845=CARTESIAN_POINT('Ctrl Pts',(-11.0143153105912,12.2,2.59384537070222));
#258846=CARTESIAN_POINT('Ctrl Pts',(-11.0178267431725,12.2,2.59317824185099));
#258847=CARTESIAN_POINT('Ctrl Pts',(-11.021344269878,12.2,2.59250571860873));
#258848=CARTESIAN_POINT('Ctrl Pts',(-11.0248678549583,12.2,2.59182778071669));
#258849=CARTESIAN_POINT('Ctrl Pts',(-11.0283914400387,12.2,2.59114984282466));
#258850=CARTESIAN_POINT('Ctrl Pts',(-11.0319210824604,12.2,2.59046648918284));
#258851=CARTESIAN_POINT('Ctrl Pts',(-11.0354567426231,12.2,2.58977770133334));
#258852=CARTESIAN_POINT('Ctrl Pts',(-11.0389924027857,12.2,2.58908891348384));
#258853=CARTESIAN_POINT('Ctrl Pts',(-11.0425340814994,12.2,2.58839469094423));
#258854=CARTESIAN_POINT('Ctrl Pts',(-11.0460817408387,12.2,2.58769501356034));
#258855=CARTESIAN_POINT('Ctrl Pts',(-11.049629400178,12.2,2.58699533617644));
#258856=CARTESIAN_POINT('Ctrl Pts',(-11.0531830398208,12.2,2.5862902041117));
#258857=CARTESIAN_POINT('Ctrl Pts',(-11.0567426214824,12.2,2.58557959867993));
#258858=CARTESIAN_POINT('Ctrl Pts',(-11.0614887307955,12.2,2.58463212468484));
#258859=CARTESIAN_POINT('Ctrl Pts',(-11.0662454040624,12.2,2.58367491720828));
#258860=CARTESIAN_POINT('Ctrl Pts',(-11.0710125507667,12.2,2.58270793326669));
#258861=CARTESIAN_POINT('Ctrl Pts',(-11.0745879104701,12.2,2.58198269537637));
#258862=CARTESIAN_POINT('Ctrl Pts',(-11.0781691622066,12.2,2.58125195745296));
#258863=CARTESIAN_POINT('Ctrl Pts',(-11.0817562679091,12.2,2.58051570110518));
#258864=CARTESIAN_POINT('Ctrl Pts',(-11.0853433736116,12.2,2.57977944475741));
#258865=CARTESIAN_POINT('Ctrl Pts',(-11.0889363336721,12.2,2.57903766972076));
#258866=CARTESIAN_POINT('Ctrl Pts',(-11.0925351095538,12.2,2.57829035591956));
#258867=CARTESIAN_POINT('Ctrl Pts',(-11.0961338854355,12.2,2.57754304211835));
#258868=CARTESIAN_POINT('Ctrl Pts',(-11.0997384767949,12.2,2.57679019042038));
#258869=CARTESIAN_POINT('Ctrl Pts',(-11.1033488474546,12.2,2.57603178215702));
#258870=CARTESIAN_POINT('Ctrl Pts',(-11.1069592187702,12.2,2.57527337375588));
#258871=CARTESIAN_POINT('Ctrl Pts',(-11.1105753692291,12.2,2.57450940866153));
#258872=CARTESIAN_POINT('Ctrl Pts',(-11.1141972605479,12.2,2.57373986825726));
#258873=CARTESIAN_POINT('Ctrl Pts',(-11.1178191512088,12.2,2.57297032799279));
#258874=CARTESIAN_POINT('Ctrl Pts',(-11.1214467828943,12.2,2.57219521320362));
#258875=CARTESIAN_POINT('Ctrl Pts',(-11.1250801209295,12.2,2.57141450489817));
#258876=CARTESIAN_POINT('Ctrl Pts',(-11.1287134589646,12.2,2.57063379659272));
#258877=CARTESIAN_POINT('Ctrl Pts',(-11.1323525006858,12.2,2.56984749530749));
#258878=CARTESIAN_POINT('Ctrl Pts',(-11.1359972102783,12.2,2.56905558195764));
#258879=CARTESIAN_POINT('Ctrl Pts',(-11.1396419198708,12.2,2.56826366860779));
#258880=CARTESIAN_POINT('Ctrl Pts',(-11.1432922952129,12.2,2.56746614310853));
#258881=CARTESIAN_POINT('Ctrl Pts',(-11.1469482994717,12.2,2.56666298730075));
#258882=CARTESIAN_POINT('Ctrl Pts',(-11.1506043037305,12.2,2.56585983149297));
#258883=CARTESIAN_POINT('Ctrl Pts',(-11.1542659373508,12.2,2.56505104560862));
#258884=CARTESIAN_POINT('Ctrl Pts',(-11.1579331665504,12.2,2.56423661284704));
#258885=CARTESIAN_POINT('Ctrl Pts',(-11.1628228059273,12.2,2.56315070239962));
#258886=CARTESIAN_POINT('Ctrl Pts',(-11.1677223945472,12.2,2.562054754176));
#258887=CARTESIAN_POINT('Ctrl Pts',(-11.1726318444265,12.2,2.56094872689285));
#258888=CARTESIAN_POINT('Ctrl Pts',(-11.1775412936369,12.2,2.55984269976039));
#258889=CARTESIAN_POINT('Ctrl Pts',(-11.1824606008646,12.2,2.55872659110727));
#258890=CARTESIAN_POINT('Ctrl Pts',(-11.1873896638182,12.2,2.55760035142173));
#258891=CARTESIAN_POINT('Ctrl Pts',(-11.1910864612012,12.2,2.55675567161921));
#258892=CARTESIAN_POINT('Ctrl Pts',(-11.1947887447772,12.2,2.55590529305476));
#258893=CARTESIAN_POINT('Ctrl Pts',(-11.1984964899334,12.2,2.55504920446165));
#258894=CARTESIAN_POINT('Ctrl Pts',(-11.2034401505907,12.2,2.55390775290048));
#258895=CARTESIAN_POINT('Ctrl Pts',(-11.2083935214545,12.2,2.55275615090798));
#258896=CARTESIAN_POINT('Ctrl Pts',(-11.2133565920001,12.2,2.55159438999998));
#258897=CARTESIAN_POINT('Origin',(-5.66257110645729E-14,15.2,-1.77635683940025E-14));
#258898=CARTESIAN_POINT('',(-10.3068855240001,15.2,1.18690176599999));
#258899=CARTESIAN_POINT('',(-10.3068855240001,12.2,1.18690176599999));
#258900=CARTESIAN_POINT('',(-10.3068855240001,15.2,1.18690176599999));
#258901=CARTESIAN_POINT('Origin',(-5.66257110645729E-14,12.2,-1.77635683940025E-14));
#258902=CARTESIAN_POINT('Origin',(-5.66257110645729E-14,15.2,-1.77635683940025E-14));
#258903=CARTESIAN_POINT('Origin',(-5.66257110645729E-14,15.2,-1.77635683940025E-14));
#258904=CARTESIAN_POINT('',(-11.4623505340001,15.2,0.929795807999985));
#258905=CARTESIAN_POINT('',(-11.4869855320001,15.2,0.546958305999983));
#258906=CARTESIAN_POINT('Origin',(-5.66257110645729E-14,15.2,-1.77635683940025E-14));
#258907=CARTESIAN_POINT('',(-11.4869855320001,12.2,0.546958305999983));
#258908=CARTESIAN_POINT('',(-11.4869855320001,15.2,0.546958305999983));
#258909=CARTESIAN_POINT('',(-11.4623505340001,12.2,0.929795807999985));
#258910=CARTESIAN_POINT('Origin',(-5.66257110645729E-14,12.2,-1.77635683940025E-14));
#258911=CARTESIAN_POINT('',(-11.4623505340001,15.2,0.929795807999985));
#258912=CARTESIAN_POINT('Ctrl Pts',(-10.3068855240001,15.2,1.18690176599999));
#258913=CARTESIAN_POINT('Ctrl Pts',(-10.3068855240001,11.6,1.18690176599999));
#258914=CARTESIAN_POINT('Ctrl Pts',(-10.3070598110001,15.2,1.18690675299999));
#258915=CARTESIAN_POINT('Ctrl Pts',(-10.3070598110001,11.6,1.18690675299999));
#258916=CARTESIAN_POINT('Ctrl Pts',(-10.3074144740001,15.2,1.18691681599998));
#258917=CARTESIAN_POINT('Ctrl Pts',(-10.3074144740001,11.6,1.18691681599998));
#258918=CARTESIAN_POINT('Ctrl Pts',(-10.3079518810001,15.2,1.18693179799998));
#258919=CARTESIAN_POINT('Ctrl Pts',(-10.3079518810001,11.6,1.18693179799998));
#258920=CARTESIAN_POINT('Ctrl Pts',(-10.3086758300001,15.2,1.18695143999998));
#258921=CARTESIAN_POINT('Ctrl Pts',(-10.3086758300001,11.6,1.18695143999998));
#258922=CARTESIAN_POINT('Ctrl Pts',(-10.3095915440001,15.2,1.18697537099999));
#258923=CARTESIAN_POINT('Ctrl Pts',(-10.3095915440001,11.6,1.18697537099999));
#258924=CARTESIAN_POINT('Ctrl Pts',(-10.3105221240001,15.2,1.18699875499999));
#258925=CARTESIAN_POINT('Ctrl Pts',(-10.3105221240001,11.6,1.18699875499999));
#258926=CARTESIAN_POINT('Ctrl Pts',(-10.3114622390001,15.2,1.18702143499998));
#258927=CARTESIAN_POINT('Ctrl Pts',(-10.3114622390001,11.6,1.18702143499998));
#258928=CARTESIAN_POINT('Ctrl Pts',(-10.3124118610001,15.2,1.18704339399998));
#258929=CARTESIAN_POINT('Ctrl Pts',(-10.3124118610001,11.6,1.18704339399998));
#258930=CARTESIAN_POINT('Ctrl Pts',(-10.3133709660001,15.2,1.18706460899999));
#258931=CARTESIAN_POINT('Ctrl Pts',(-10.3133709660001,11.6,1.18706460899999));
#258932=CARTESIAN_POINT('Ctrl Pts',(-10.3143395250001,15.2,1.18708506599999));
#258933=CARTESIAN_POINT('Ctrl Pts',(-10.3143395250001,11.6,1.18708506599999));
#258934=CARTESIAN_POINT('Ctrl Pts',(-10.3153175130001,15.2,1.18710474299998));
#258935=CARTESIAN_POINT('Ctrl Pts',(-10.3153175130001,11.6,1.18710474299998));
#258936=CARTESIAN_POINT('Ctrl Pts',(-10.3163049050001,15.2,1.18712362399998));
#258937=CARTESIAN_POINT('Ctrl Pts',(-10.3163049050001,11.6,1.18712362399998));
#258938=CARTESIAN_POINT('Ctrl Pts',(-10.3173016730001,15.2,1.18714168899999));
#258939=CARTESIAN_POINT('Ctrl Pts',(-10.3173016730001,11.6,1.18714168899999));
#258940=CARTESIAN_POINT('Ctrl Pts',(-10.3183077930001,15.2,1.18715892099999));
#258941=CARTESIAN_POINT('Ctrl Pts',(-10.3183077930001,11.6,1.18715892099999));
#258942=CARTESIAN_POINT('Ctrl Pts',(-10.3193232400001,15.2,1.18717530199998));
#258943=CARTESIAN_POINT('Ctrl Pts',(-10.3193232400001,11.6,1.18717530199998));
#258944=CARTESIAN_POINT('Ctrl Pts',(-10.3203479850001,15.2,1.18719081299998));
#258945=CARTESIAN_POINT('Ctrl Pts',(-10.3203479850001,11.6,1.18719081299998));
#258946=CARTESIAN_POINT('Ctrl Pts',(-10.3213820050001,15.2,1.18720543699999));
#258947=CARTESIAN_POINT('Ctrl Pts',(-10.3213820050001,11.6,1.18720543699998));
#258948=CARTESIAN_POINT('Ctrl Pts',(-10.3224252740001,15.2,1.18721915599998));
#258949=CARTESIAN_POINT('Ctrl Pts',(-10.3224252740001,11.6,1.18721915599998));
#258950=CARTESIAN_POINT('Ctrl Pts',(-10.3234777680001,15.2,1.18723195099999));
#258951=CARTESIAN_POINT('Ctrl Pts',(-10.3234777680001,11.6,1.18723195099998));
#258952=CARTESIAN_POINT('Ctrl Pts',(-10.3245394590001,15.2,1.18724380599998));
#258953=CARTESIAN_POINT('Ctrl Pts',(-10.3245394590001,11.6,1.18724380599998));
#258954=CARTESIAN_POINT('Ctrl Pts',(-10.3256103250001,15.2,1.18725470399998));
#258955=CARTESIAN_POINT('Ctrl Pts',(-10.3256103250001,11.6,1.18725470399998));
#258956=CARTESIAN_POINT('Ctrl Pts',(-10.3266903400001,15.2,1.18726462499998));
#258957=CARTESIAN_POINT('Ctrl Pts',(-10.3266903400001,11.6,1.18726462499998));
#258958=CARTESIAN_POINT('Ctrl Pts',(-10.3277794780001,15.2,1.18727355499999));
#258959=CARTESIAN_POINT('Ctrl Pts',(-10.3277794780001,11.6,1.18727355499999));
#258960=CARTESIAN_POINT('Ctrl Pts',(-10.3288777160001,15.2,1.18728147399999));
#258961=CARTESIAN_POINT('Ctrl Pts',(-10.3288777160001,11.6,1.18728147399999));
#258962=CARTESIAN_POINT('Ctrl Pts',(-10.3299850290001,15.2,1.18728836599999));
#258963=CARTESIAN_POINT('Ctrl Pts',(-10.3299850290001,11.6,1.18728836599999));
#258964=CARTESIAN_POINT('Ctrl Pts',(-10.3311013920001,15.2,1.18729421399999));
#258965=CARTESIAN_POINT('Ctrl Pts',(-10.3311013920001,11.6,1.18729421399998));
#258966=CARTESIAN_POINT('Ctrl Pts',(-10.3322267810001,15.2,1.18729900199999));
#258967=CARTESIAN_POINT('Ctrl Pts',(-10.3322267810001,11.6,1.18729900199999));
#258968=CARTESIAN_POINT('Ctrl Pts',(-10.3333611710001,15.2,1.18730271099999));
#258969=CARTESIAN_POINT('Ctrl Pts',(-10.3333611710001,11.6,1.18730271099999));
#258970=CARTESIAN_POINT('Ctrl Pts',(-10.3345045400001,15.2,1.18730532599999));
#258971=CARTESIAN_POINT('Ctrl Pts',(-10.3345045400001,11.6,1.18730532599999));
#258972=CARTESIAN_POINT('Ctrl Pts',(-10.3356568620001,15.2,1.18730682999999));
#258973=CARTESIAN_POINT('Ctrl Pts',(-10.3356568620001,11.6,1.18730682999999));
#258974=CARTESIAN_POINT('Ctrl Pts',(-10.3368181130001,15.2,1.18730720599999));
#258975=CARTESIAN_POINT('Ctrl Pts',(-10.3368181130001,11.6,1.18730720599999));
#258976=CARTESIAN_POINT('Ctrl Pts',(-10.3379882700001,15.2,1.18730643699998));
#258977=CARTESIAN_POINT('Ctrl Pts',(-10.3379882700001,11.6,1.18730643699998));
#258978=CARTESIAN_POINT('Ctrl Pts',(-10.3391673090001,15.2,1.18730450799998));
#258979=CARTESIAN_POINT('Ctrl Pts',(-10.3391673090001,11.6,1.18730450799998));
#258980=CARTESIAN_POINT('Ctrl Pts',(-10.3403552060001,15.2,1.18730140199999));
#258981=CARTESIAN_POINT('Ctrl Pts',(-10.3403552060001,11.6,1.18730140199998));
#258982=CARTESIAN_POINT('Ctrl Pts',(-10.3415519380001,15.2,1.18729710199998));
#258983=CARTESIAN_POINT('Ctrl Pts',(-10.3415519380001,11.6,1.18729710199998));
#258984=CARTESIAN_POINT('Ctrl Pts',(-10.3427574820001,15.2,1.18729159399999));
#258985=CARTESIAN_POINT('Ctrl Pts',(-10.3427574820001,11.6,1.18729159399999));
#258986=CARTESIAN_POINT('Ctrl Pts',(-10.3439718130001,15.2,1.18728485899998));
#258987=CARTESIAN_POINT('Ctrl Pts',(-10.3439718130001,11.6,1.18728485899998));
#258988=CARTESIAN_POINT('Ctrl Pts',(-10.3451949090001,15.2,1.18727688299999));
#258989=CARTESIAN_POINT('Ctrl Pts',(-10.3451949090001,11.6,1.18727688299999));
#258990=CARTESIAN_POINT('Ctrl Pts',(-10.3464267470001,15.2,1.18726764999999));
#258991=CARTESIAN_POINT('Ctrl Pts',(-10.3464267470001,11.6,1.18726764999999));
#258992=CARTESIAN_POINT('Ctrl Pts',(-10.3476673040001,15.2,1.18725714299998));
#258993=CARTESIAN_POINT('Ctrl Pts',(-10.3476673040001,11.6,1.18725714299998));
#258994=CARTESIAN_POINT('Ctrl Pts',(-10.3489165560001,15.2,1.18724534699998));
#258995=CARTESIAN_POINT('Ctrl Pts',(-10.3489165560001,11.6,1.18724534699998));
#258996=CARTESIAN_POINT('Ctrl Pts',(-10.3501744810001,15.2,1.18723224699998));
#258997=CARTESIAN_POINT('Ctrl Pts',(-10.3501744810001,11.6,1.18723224699998));
#258998=CARTESIAN_POINT('Ctrl Pts',(-10.3514410560001,15.2,1.18721782799998));
#258999=CARTESIAN_POINT('Ctrl Pts',(-10.3514410560001,11.6,1.18721782799998));
#259000=CARTESIAN_POINT('Ctrl Pts',(-10.3527162580001,15.2,1.18720207199999));
#259001=CARTESIAN_POINT('Ctrl Pts',(-10.3527162580001,11.6,1.18720207199999));
#259002=CARTESIAN_POINT('Ctrl Pts',(-10.3540000650001,15.2,1.18718496499998));
#259003=CARTESIAN_POINT('Ctrl Pts',(-10.3540000650001,11.6,1.18718496499998));
#259004=CARTESIAN_POINT('Ctrl Pts',(-10.3552924550001,15.2,1.18716649199999));
#259005=CARTESIAN_POINT('Ctrl Pts',(-10.3552924550001,11.6,1.18716649199999));
#259006=CARTESIAN_POINT('Ctrl Pts',(-10.3565934040001,15.2,1.18714663699999));
#259007=CARTESIAN_POINT('Ctrl Pts',(-10.3565934040001,11.6,1.18714663699999));
#259008=CARTESIAN_POINT('Ctrl Pts',(-10.3579028900001,15.2,1.18712538499999));
#259009=CARTESIAN_POINT('Ctrl Pts',(-10.3579028900001,11.6,1.18712538499999));
#259010=CARTESIAN_POINT('Ctrl Pts',(-10.3592208920001,15.2,1.18710272199999));
#259011=CARTESIAN_POINT('Ctrl Pts',(-10.3592208920001,11.6,1.18710272199999));
#259012=CARTESIAN_POINT('Ctrl Pts',(-10.3605473870001,15.2,1.18707863099999));
#259013=CARTESIAN_POINT('Ctrl Pts',(-10.3605473870001,11.6,1.18707863099999));
#259014=CARTESIAN_POINT('Ctrl Pts',(-10.3618823540001,15.2,1.18705309899998));
#259015=CARTESIAN_POINT('Ctrl Pts',(-10.3618823540001,11.6,1.18705309899998));
#259016=CARTESIAN_POINT('Ctrl Pts',(-10.3632257690001,15.2,1.18702610999998));
#259017=CARTESIAN_POINT('Ctrl Pts',(-10.3632257690001,11.6,1.18702610999998));
#259018=CARTESIAN_POINT('Ctrl Pts',(-10.3645776120001,15.2,1.18699765099999));
#259019=CARTESIAN_POINT('Ctrl Pts',(-10.3645776120001,11.6,1.18699765099999));
#259020=CARTESIAN_POINT('Ctrl Pts',(-10.3659378610001,15.2,1.18696770399998));
#259021=CARTESIAN_POINT('Ctrl Pts',(-10.3659378610001,11.6,1.18696770399998));
#259022=CARTESIAN_POINT('Ctrl Pts',(-10.3673064940001,15.2,1.18693625599999));
#259023=CARTESIAN_POINT('Ctrl Pts',(-10.3673064940001,11.6,1.18693625599999));
#259024=CARTESIAN_POINT('Ctrl Pts',(-10.3686834880001,15.2,1.18690329399998));
#259025=CARTESIAN_POINT('Ctrl Pts',(-10.3686834880001,11.6,1.18690329399998));
#259026=CARTESIAN_POINT('Ctrl Pts',(-10.3700688240001,15.2,1.18686880099999));
#259027=CARTESIAN_POINT('Ctrl Pts',(-10.3700688240001,11.6,1.18686880099998));
#259028=CARTESIAN_POINT('Ctrl Pts',(-10.3714624790001,15.2,1.18683276399999));
#259029=CARTESIAN_POINT('Ctrl Pts',(-10.3714624790001,11.6,1.18683276399999));
#259030=CARTESIAN_POINT('Ctrl Pts',(-10.3728644310001,15.2,1.18679516799999));
#259031=CARTESIAN_POINT('Ctrl Pts',(-10.3728644310001,11.6,1.18679516799999));
#259032=CARTESIAN_POINT('Ctrl Pts',(-10.3742746610001,15.2,1.18675599899999));
#259033=CARTESIAN_POINT('Ctrl Pts',(-10.3742746610001,11.6,1.18675599899999));
#259034=CARTESIAN_POINT('Ctrl Pts',(-10.3756931460001,15.2,1.18671524399999));
#259035=CARTESIAN_POINT('Ctrl Pts',(-10.3756931460001,11.6,1.18671524399998));
#259036=CARTESIAN_POINT('Ctrl Pts',(-10.3771198660001,15.2,1.18667288599998));
#259037=CARTESIAN_POINT('Ctrl Pts',(-10.3771198660001,11.6,1.18667288599998));
#259038=CARTESIAN_POINT('Ctrl Pts',(-10.3785547980001,15.2,1.18662891399998));
#259039=CARTESIAN_POINT('Ctrl Pts',(-10.3785547980001,11.6,1.18662891399998));
#259040=CARTESIAN_POINT('Ctrl Pts',(-10.3799979240001,15.2,1.18658331299998));
#259041=CARTESIAN_POINT('Ctrl Pts',(-10.3799979240001,11.6,1.18658331299998));
#259042=CARTESIAN_POINT('Ctrl Pts',(-10.3814492210001,15.2,1.18653606699999));
#259043=CARTESIAN_POINT('Ctrl Pts',(-10.3814492210001,11.6,1.18653606699999));
#259044=CARTESIAN_POINT('Ctrl Pts',(-10.3829086680001,15.2,1.18648716499999));
#259045=CARTESIAN_POINT('Ctrl Pts',(-10.3829086680001,11.6,1.18648716499999));
#259046=CARTESIAN_POINT('Ctrl Pts',(-10.3843762450001,15.2,1.18643659199998));
#259047=CARTESIAN_POINT('Ctrl Pts',(-10.3843762450001,11.6,1.18643659199998));
#259048=CARTESIAN_POINT('Ctrl Pts',(-10.3858519330001,15.2,1.18638433399999));
#259049=CARTESIAN_POINT('Ctrl Pts',(-10.3858519330001,11.6,1.18638433399999));
#259050=CARTESIAN_POINT('Ctrl Pts',(-10.3873357080001,15.2,1.18633037799999));
#259051=CARTESIAN_POINT('Ctrl Pts',(-10.3873357080001,11.6,1.18633037799999));
#259052=CARTESIAN_POINT('Ctrl Pts',(-10.3888275530001,15.2,1.18627470999999));
#259053=CARTESIAN_POINT('Ctrl Pts',(-10.3888275530001,11.6,1.18627470999999));
#259054=CARTESIAN_POINT('Ctrl Pts',(-10.3903274450001,15.2,1.18621731599998));
#259055=CARTESIAN_POINT('Ctrl Pts',(-10.3903274450001,11.6,1.18621731599998));
#259056=CARTESIAN_POINT('Ctrl Pts',(-10.3918353650001,15.2,1.18615818399999));
#259057=CARTESIAN_POINT('Ctrl Pts',(-10.3918353650001,11.6,1.18615818399999));
#259058=CARTESIAN_POINT('Ctrl Pts',(-10.3933512920001,15.2,1.18609729999998));
#259059=CARTESIAN_POINT('Ctrl Pts',(-10.3933512920001,11.6,1.18609729999998));
#259060=CARTESIAN_POINT('Ctrl Pts',(-10.3948752070001,15.2,1.18603464899998));
#259061=CARTESIAN_POINT('Ctrl Pts',(-10.3948752070001,11.6,1.18603464899998));
#259062=CARTESIAN_POINT('Ctrl Pts',(-10.3964070880001,15.2,1.18597021999999));
#259063=CARTESIAN_POINT('Ctrl Pts',(-10.3964070880001,11.6,1.18597021999999));
#259064=CARTESIAN_POINT('Ctrl Pts',(-10.3979469170001,15.2,1.18590399899999));
#259065=CARTESIAN_POINT('Ctrl Pts',(-10.3979469170001,11.6,1.18590399899999));
#259066=CARTESIAN_POINT('Ctrl Pts',(-10.3994946730001,15.2,1.18583597199999));
#259067=CARTESIAN_POINT('Ctrl Pts',(-10.3994946730001,11.6,1.18583597199999));
#259068=CARTESIAN_POINT('Ctrl Pts',(-10.4010503360001,15.2,1.18576612699998));
#259069=CARTESIAN_POINT('Ctrl Pts',(-10.4010503360001,11.6,1.18576612699998));
#259070=CARTESIAN_POINT('Ctrl Pts',(-10.4026138870001,15.2,1.18569445199999));
#259071=CARTESIAN_POINT('Ctrl Pts',(-10.4026138870001,11.6,1.18569445199999));
#259072=CARTESIAN_POINT('Ctrl Pts',(-10.4041853050001,15.2,1.18562093199999));
#259073=CARTESIAN_POINT('Ctrl Pts',(-10.4041853050001,11.6,1.18562093199999));
#259074=CARTESIAN_POINT('Ctrl Pts',(-10.4057645710001,15.2,1.18554555499998));
#259075=CARTESIAN_POINT('Ctrl Pts',(-10.4057645710001,11.6,1.18554555499998));
#259076=CARTESIAN_POINT('Ctrl Pts',(-10.4073516650001,15.2,1.18546830799998));
#259077=CARTESIAN_POINT('Ctrl Pts',(-10.4073516650001,11.6,1.18546830799998));
#259078=CARTESIAN_POINT('Ctrl Pts',(-10.4089465690001,15.2,1.18538917799999));
#259079=CARTESIAN_POINT('Ctrl Pts',(-10.4089465690001,11.6,1.18538917799999));
#259080=CARTESIAN_POINT('Ctrl Pts',(-10.4105492620001,15.2,1.18530815299998));
#259081=CARTESIAN_POINT('Ctrl Pts',(-10.4105492620001,11.6,1.18530815299998));
#259082=CARTESIAN_POINT('Ctrl Pts',(-10.4121597240001,15.2,1.18522521999999));
#259083=CARTESIAN_POINT('Ctrl Pts',(-10.4121597240001,11.6,1.18522521999999));
#259084=CARTESIAN_POINT('Ctrl Pts',(-10.4137779370001,15.2,1.18514036599999));
#259085=CARTESIAN_POINT('Ctrl Pts',(-10.4137779370001,11.6,1.18514036599999));
#259086=CARTESIAN_POINT('Ctrl Pts',(-10.4154038820001,15.2,1.18505357999998));
#259087=CARTESIAN_POINT('Ctrl Pts',(-10.4154038820001,11.6,1.18505357999998));
#259088=CARTESIAN_POINT('Ctrl Pts',(-10.4170375390001,15.2,1.18496484799998));
#259089=CARTESIAN_POINT('Ctrl Pts',(-10.4170375390001,11.6,1.18496484799998));
#259090=CARTESIAN_POINT('Ctrl Pts',(-10.4186788900001,15.2,1.18487415599999));
#259091=CARTESIAN_POINT('Ctrl Pts',(-10.4186788900001,11.6,1.18487415599999));
#259092=CARTESIAN_POINT('Ctrl Pts',(-10.4203279130001,15.2,1.18478149699999));
#259093=CARTESIAN_POINT('Ctrl Pts',(-10.4203279130001,11.6,1.18478149699999));
#259094=CARTESIAN_POINT('Ctrl Pts',(-10.4219845930001,15.2,1.18468685399999));
#259095=CARTESIAN_POINT('Ctrl Pts',(-10.4219845930001,11.6,1.18468685399999));
#259096=CARTESIAN_POINT('Ctrl Pts',(-10.4236489080001,15.2,1.18459021499998));
#259097=CARTESIAN_POINT('Ctrl Pts',(-10.4236489080001,11.6,1.18459021499998));
#259098=CARTESIAN_POINT('Ctrl Pts',(-10.4253208410001,15.2,1.18449156999999));
#259099=CARTESIAN_POINT('Ctrl Pts',(-10.4253208410001,11.6,1.18449156999999));
#259100=CARTESIAN_POINT('Ctrl Pts',(-10.4270003720001,15.2,1.18439090599999));
#259101=CARTESIAN_POINT('Ctrl Pts',(-10.4270003720001,11.6,1.18439090599999));
#259102=CARTESIAN_POINT('Ctrl Pts',(-10.4286874830001,15.2,1.18428821199998));
#259103=CARTESIAN_POINT('Ctrl Pts',(-10.4286874830001,11.6,1.18428821199998));
#259104=CARTESIAN_POINT('Ctrl Pts',(-10.4303821540001,15.2,1.18418347399999));
#259105=CARTESIAN_POINT('Ctrl Pts',(-10.4303821540001,11.6,1.18418347399999));
#259106=CARTESIAN_POINT('Ctrl Pts',(-10.4320843690001,15.2,1.18407667999998));
#259107=CARTESIAN_POINT('Ctrl Pts',(-10.4320843690001,11.6,1.18407667999998));
#259108=CARTESIAN_POINT('Ctrl Pts',(-10.4337941070001,15.2,1.18396781999999));
#259109=CARTESIAN_POINT('Ctrl Pts',(-10.4337941070001,11.6,1.18396781999999));
#259110=CARTESIAN_POINT('Ctrl Pts',(-10.4355113520001,15.2,1.18385688099998));
#259111=CARTESIAN_POINT('Ctrl Pts',(-10.4355113520001,11.6,1.18385688099998));
#259112=CARTESIAN_POINT('Ctrl Pts',(-10.4372360820001,15.2,1.18374385099999));
#259113=CARTESIAN_POINT('Ctrl Pts',(-10.4372360820001,11.6,1.18374385099999));
#259114=CARTESIAN_POINT('Ctrl Pts',(-10.4389682810001,15.2,1.18362871999999));
#259115=CARTESIAN_POINT('Ctrl Pts',(-10.4389682810001,11.6,1.18362871999999));
#259116=CARTESIAN_POINT('Ctrl Pts',(-10.4407079310001,15.2,1.18351147399999));
#259117=CARTESIAN_POINT('Ctrl Pts',(-10.4407079310001,11.6,1.18351147399998));
#259118=CARTESIAN_POINT('Ctrl Pts',(-10.4424550130001,15.2,1.18339210299998));
#259119=CARTESIAN_POINT('Ctrl Pts',(-10.4424550130001,11.6,1.18339210299998));
#259120=CARTESIAN_POINT('Ctrl Pts',(-10.4442095090001,15.2,1.18327059399999));
#259121=CARTESIAN_POINT('Ctrl Pts',(-10.4442095090001,11.6,1.18327059399999));
#259122=CARTESIAN_POINT('Ctrl Pts',(-10.4459714000001,15.2,1.18314693699999));
#259123=CARTESIAN_POINT('Ctrl Pts',(-10.4459714000001,11.6,1.18314693699999));
#259124=CARTESIAN_POINT('Ctrl Pts',(-10.4477406700001,15.2,1.18302111899999));
#259125=CARTESIAN_POINT('Ctrl Pts',(-10.4477406700001,11.6,1.18302111899998));
#259126=CARTESIAN_POINT('Ctrl Pts',(-10.4495173000001,15.2,1.18289313099998));
#259127=CARTESIAN_POINT('Ctrl Pts',(-10.4495173000001,11.6,1.18289313099998));
#259128=CARTESIAN_POINT('Ctrl Pts',(-10.4513012710001,15.2,1.18276295899999));
#259129=CARTESIAN_POINT('Ctrl Pts',(-10.4513012710001,11.6,1.18276295899999));
#259130=CARTESIAN_POINT('Ctrl Pts',(-10.4530925660001,15.2,1.18263059399998));
#259131=CARTESIAN_POINT('Ctrl Pts',(-10.4530925660001,11.6,1.18263059399998));
#259132=CARTESIAN_POINT('Ctrl Pts',(-10.4548911670001,15.2,1.18249602199999));
#259133=CARTESIAN_POINT('Ctrl Pts',(-10.4548911670001,11.6,1.18249602199999));
#259134=CARTESIAN_POINT('Ctrl Pts',(-10.4566970570001,15.2,1.18235923399999));
#259135=CARTESIAN_POINT('Ctrl Pts',(-10.4566970570001,11.6,1.18235923399999));
#259136=CARTESIAN_POINT('Ctrl Pts',(-10.4585102170001,15.2,1.18222021899999));
#259137=CARTESIAN_POINT('Ctrl Pts',(-10.4585102170001,11.6,1.18222021899998));
#259138=CARTESIAN_POINT('Ctrl Pts',(-10.4603306310001,15.2,1.18207896399999));
#259139=CARTESIAN_POINT('Ctrl Pts',(-10.4603306310001,11.6,1.18207896399999));
#259140=CARTESIAN_POINT('Ctrl Pts',(-10.4621582800001,15.2,1.18193545999999));
#259141=CARTESIAN_POINT('Ctrl Pts',(-10.4621582800001,11.6,1.18193545999999));
#259142=CARTESIAN_POINT('Ctrl Pts',(-10.4639931470001,15.2,1.18178969599999));
#259143=CARTESIAN_POINT('Ctrl Pts',(-10.4639931470001,11.6,1.18178969599999));
#259144=CARTESIAN_POINT('Ctrl Pts',(-10.4658352150001,15.2,1.18164165899998));
#259145=CARTESIAN_POINT('Ctrl Pts',(-10.4658352150001,11.6,1.18164165899998));
#259146=CARTESIAN_POINT('Ctrl Pts',(-10.4676844650001,15.2,1.18149133999998));
#259147=CARTESIAN_POINT('Ctrl Pts',(-10.4676844650001,11.6,1.18149133999998));
#259148=CARTESIAN_POINT('Ctrl Pts',(-10.4695408810001,15.2,1.18133872599998));
#259149=CARTESIAN_POINT('Ctrl Pts',(-10.4695408810001,11.6,1.18133872599998));
#259150=CARTESIAN_POINT('Ctrl Pts',(-10.4714044460001,15.2,1.18118380899999));
#259151=CARTESIAN_POINT('Ctrl Pts',(-10.4714044460001,11.6,1.18118380899999));
#259152=CARTESIAN_POINT('Ctrl Pts',(-10.4732751410001,15.2,1.18102657599998));
#259153=CARTESIAN_POINT('Ctrl Pts',(-10.4732751410001,11.6,1.18102657599998));
#259154=CARTESIAN_POINT('Ctrl Pts',(-10.4751529500001,15.2,1.18086701799998));
#259155=CARTESIAN_POINT('Ctrl Pts',(-10.4751529500001,11.6,1.18086701799998));
#259156=CARTESIAN_POINT('Ctrl Pts',(-10.4770378570001,15.2,1.18070512399999));
#259157=CARTESIAN_POINT('Ctrl Pts',(-10.4770378570001,11.6,1.18070512399999));
#259158=CARTESIAN_POINT('Ctrl Pts',(-10.4789298430001,15.2,1.18054088199999));
#259159=CARTESIAN_POINT('Ctrl Pts',(-10.4789298430001,11.6,1.18054088199999));
#259160=CARTESIAN_POINT('Ctrl Pts',(-10.4808288920001,15.2,1.18037428299999));
#259161=CARTESIAN_POINT('Ctrl Pts',(-10.4808288920001,11.6,1.18037428299999));
#259162=CARTESIAN_POINT('Ctrl Pts',(-10.4827349850001,15.2,1.18020531599999));
#259163=CARTESIAN_POINT('Ctrl Pts',(-10.4827349850001,11.6,1.18020531599999));
#259164=CARTESIAN_POINT('Ctrl Pts',(-10.4846481080001,15.2,1.18003396999999));
#259165=CARTESIAN_POINT('Ctrl Pts',(-10.4846481080001,11.6,1.18003396999998));
#259166=CARTESIAN_POINT('Ctrl Pts',(-10.4865682440001,15.2,1.17986023499999));
#259167=CARTESIAN_POINT('Ctrl Pts',(-10.4865682440001,11.6,1.17986023499998));
#259168=CARTESIAN_POINT('Ctrl Pts',(-10.4884953720001,15.2,1.17968410099999));
#259169=CARTESIAN_POINT('Ctrl Pts',(-10.4884953720001,11.6,1.17968410099999));
#259170=CARTESIAN_POINT('Ctrl Pts',(-10.4904294800001,15.2,1.17950555699998));
#259171=CARTESIAN_POINT('Ctrl Pts',(-10.4904294800001,11.6,1.17950555699998));
#259172=CARTESIAN_POINT('Ctrl Pts',(-10.4923705490001,15.2,1.17932459399999));
#259173=CARTESIAN_POINT('Ctrl Pts',(-10.4923705490001,11.6,1.17932459399999));
#259174=CARTESIAN_POINT('Ctrl Pts',(-10.4943185630001,15.2,1.17914119999998));
#259175=CARTESIAN_POINT('Ctrl Pts',(-10.4943185630001,11.6,1.17914119999998));
#259176=CARTESIAN_POINT('Ctrl Pts',(-10.4962735060001,15.2,1.17895536499999));
#259177=CARTESIAN_POINT('Ctrl Pts',(-10.4962735060001,11.6,1.17895536499998));
#259178=CARTESIAN_POINT('Ctrl Pts',(-10.4982353590001,15.2,1.17876708099999));
#259179=CARTESIAN_POINT('Ctrl Pts',(-10.4982353590001,11.6,1.17876708099998));
#259180=CARTESIAN_POINT('Ctrl Pts',(-10.5002041080001,15.2,1.17857633499999));
#259181=CARTESIAN_POINT('Ctrl Pts',(-10.5002041080001,11.6,1.17857633499999));
#259182=CARTESIAN_POINT('Ctrl Pts',(-10.5021797350001,15.2,1.17838311899999));
#259183=CARTESIAN_POINT('Ctrl Pts',(-10.5021797350001,11.6,1.17838311899999));
#259184=CARTESIAN_POINT('Ctrl Pts',(-10.5041622250001,15.2,1.17818742199999));
#259185=CARTESIAN_POINT('Ctrl Pts',(-10.5041622250001,11.6,1.17818742199999));
#259186=CARTESIAN_POINT('Ctrl Pts',(-10.5061515600001,15.2,1.17798923599999));
#259187=CARTESIAN_POINT('Ctrl Pts',(-10.5061515600001,11.6,1.17798923599999));
#259188=CARTESIAN_POINT('Ctrl Pts',(-10.5081477230001,15.2,1.17778854799999));
#259189=CARTESIAN_POINT('Ctrl Pts',(-10.5081477230001,11.6,1.17778854799999));
#259190=CARTESIAN_POINT('Ctrl Pts',(-10.5101507010001,15.2,1.17758534999998));
#259191=CARTESIAN_POINT('Ctrl Pts',(-10.5101507010001,11.6,1.17758534999998));
#259192=CARTESIAN_POINT('Ctrl Pts',(-10.5121604750001,15.2,1.17737963099998));
#259193=CARTESIAN_POINT('Ctrl Pts',(-10.5121604750001,11.6,1.17737963099998));
#259194=CARTESIAN_POINT('Ctrl Pts',(-10.5141770310001,15.2,1.17717138199998));
#259195=CARTESIAN_POINT('Ctrl Pts',(-10.5141770310001,11.6,1.17717138199998));
#259196=CARTESIAN_POINT('Ctrl Pts',(-10.5162003510001,15.2,1.17696059399998));
#259197=CARTESIAN_POINT('Ctrl Pts',(-10.5162003510001,11.6,1.17696059399998));
#259198=CARTESIAN_POINT('Ctrl Pts',(-10.5182304190001,15.2,1.17674725699999));
#259199=CARTESIAN_POINT('Ctrl Pts',(-10.5182304190001,11.6,1.17674725699999));
#259200=CARTESIAN_POINT('Ctrl Pts',(-10.5202672190001,15.2,1.17653135999999));
#259201=CARTESIAN_POINT('Ctrl Pts',(-10.5202672190001,11.6,1.17653135999999));
#259202=CARTESIAN_POINT('Ctrl Pts',(-10.5223107360001,15.2,1.17631289399998));
#259203=CARTESIAN_POINT('Ctrl Pts',(-10.5223107360001,11.6,1.17631289399998));
#259204=CARTESIAN_POINT('Ctrl Pts',(-10.5243609530001,15.2,1.17609184999999));
#259205=CARTESIAN_POINT('Ctrl Pts',(-10.5243609530001,11.6,1.17609184999999));
#259206=CARTESIAN_POINT('Ctrl Pts',(-10.5264178550001,15.2,1.17586821899998));
#259207=CARTESIAN_POINT('Ctrl Pts',(-10.5264178550001,11.6,1.17586821899998));
#259208=CARTESIAN_POINT('Ctrl Pts',(-10.5284814260001,15.2,1.17564198999998));
#259209=CARTESIAN_POINT('Ctrl Pts',(-10.5284814260001,11.6,1.17564198999998));
#259210=CARTESIAN_POINT('Ctrl Pts',(-10.5305516490001,15.2,1.17541315299999));
#259211=CARTESIAN_POINT('Ctrl Pts',(-10.5305516490001,11.6,1.17541315299999));
#259212=CARTESIAN_POINT('Ctrl Pts',(-10.5326285090001,15.2,1.17518170099999));
#259213=CARTESIAN_POINT('Ctrl Pts',(-10.5326285090001,11.6,1.17518170099998));
#259214=CARTESIAN_POINT('Ctrl Pts',(-10.5347119910001,15.2,1.17494762299998));
#259215=CARTESIAN_POINT('Ctrl Pts',(-10.5347119910001,11.6,1.17494762299998));
#259216=CARTESIAN_POINT('Ctrl Pts',(-10.5368020780001,15.2,1.17471090999999));
#259217=CARTESIAN_POINT('Ctrl Pts',(-10.5368020780001,11.6,1.17471090999999));
#259218=CARTESIAN_POINT('Ctrl Pts',(-10.5388987570001,15.2,1.17447155299998));
#259219=CARTESIAN_POINT('Ctrl Pts',(-10.5388987570001,11.6,1.17447155299998));
#259220=CARTESIAN_POINT('Ctrl Pts',(-10.5410020080001,15.2,1.17422954199998));
#259221=CARTESIAN_POINT('Ctrl Pts',(-10.5410020080001,11.6,1.17422954199998));
#259222=CARTESIAN_POINT('Ctrl Pts',(-10.5431118190001,15.2,1.17398486899999));
#259223=CARTESIAN_POINT('Ctrl Pts',(-10.5431118190001,11.6,1.17398486899999));
#259224=CARTESIAN_POINT('Ctrl Pts',(-10.5452281730001,15.2,1.17373752299998));
#259225=CARTESIAN_POINT('Ctrl Pts',(-10.5452281730001,11.6,1.17373752299998));
#259226=CARTESIAN_POINT('Ctrl Pts',(-10.5473510550001,15.2,1.17348749699998));
#259227=CARTESIAN_POINT('Ctrl Pts',(-10.5473510550001,11.6,1.17348749699998));
#259228=CARTESIAN_POINT('Ctrl Pts',(-10.5494804500001,15.2,1.17323477999999));
#259229=CARTESIAN_POINT('Ctrl Pts',(-10.5494804500001,11.6,1.17323477999998));
#259230=CARTESIAN_POINT('Ctrl Pts',(-10.5516163410001,15.2,1.17297936399999));
#259231=CARTESIAN_POINT('Ctrl Pts',(-10.5516163410001,11.6,1.17297936399999));
#259232=CARTESIAN_POINT('Ctrl Pts',(-10.5537587150001,15.2,1.17272124099999));
#259233=CARTESIAN_POINT('Ctrl Pts',(-10.5537587150001,11.6,1.17272124099998));
#259234=CARTESIAN_POINT('Ctrl Pts',(-10.5559075550001,15.2,1.17246039999999));
#259235=CARTESIAN_POINT('Ctrl Pts',(-10.5559075550001,11.6,1.17246039999999));
#259236=CARTESIAN_POINT('Ctrl Pts',(-10.5580628460001,15.2,1.17219683299998));
#259237=CARTESIAN_POINT('Ctrl Pts',(-10.5580628460001,11.6,1.17219683299998));
#259238=CARTESIAN_POINT('Ctrl Pts',(-10.5602245730001,15.2,1.17193052999998));
#259239=CARTESIAN_POINT('Ctrl Pts',(-10.5602245730001,11.6,1.17193052999998));
#259240=CARTESIAN_POINT('Ctrl Pts',(-10.5623927210001,15.2,1.17166148499999));
#259241=CARTESIAN_POINT('Ctrl Pts',(-10.5623927210001,11.6,1.17166148499999));
#259242=CARTESIAN_POINT('Ctrl Pts',(-10.5645672750001,15.2,1.17138968599999));
#259243=CARTESIAN_POINT('Ctrl Pts',(-10.5645672750001,11.6,1.17138968599999));
#259244=CARTESIAN_POINT('Ctrl Pts',(-10.5667482200001,15.2,1.17111512499998));
#259245=CARTESIAN_POINT('Ctrl Pts',(-10.5667482200001,11.6,1.17111512499998));
#259246=CARTESIAN_POINT('Ctrl Pts',(-10.5689355400001,15.2,1.17083779399998));
#259247=CARTESIAN_POINT('Ctrl Pts',(-10.5689355400001,11.6,1.17083779399998));
#259248=CARTESIAN_POINT('Ctrl Pts',(-10.5711292210001,15.2,1.17055768399998));
#259249=CARTESIAN_POINT('Ctrl Pts',(-10.5711292210001,11.6,1.17055768399998));
#259250=CARTESIAN_POINT('Ctrl Pts',(-10.5733292470001,15.2,1.17027478699999));
#259251=CARTESIAN_POINT('Ctrl Pts',(-10.5733292470001,11.6,1.17027478699998));
#259252=CARTESIAN_POINT('Ctrl Pts',(-10.5755356040001,15.2,1.16998909399999));
#259253=CARTESIAN_POINT('Ctrl Pts',(-10.5755356040001,11.6,1.16998909399999));
#259254=CARTESIAN_POINT('Ctrl Pts',(-10.5777482770001,15.2,1.16970059599999));
#259255=CARTESIAN_POINT('Ctrl Pts',(-10.5777482770001,11.6,1.16970059599998));
#259256=CARTESIAN_POINT('Ctrl Pts',(-10.5799672510001,15.2,1.16940928399998));
#259257=CARTESIAN_POINT('Ctrl Pts',(-10.5799672510001,11.6,1.16940928399998));
#259258=CARTESIAN_POINT('Ctrl Pts',(-10.5821925120001,15.2,1.16911514999999));
#259259=CARTESIAN_POINT('Ctrl Pts',(-10.5821925120001,11.6,1.16911514999999));
#259260=CARTESIAN_POINT('Ctrl Pts',(-10.5844240430001,15.2,1.16881818499999));
#259261=CARTESIAN_POINT('Ctrl Pts',(-10.5844240430001,11.6,1.16881818499999));
#259262=CARTESIAN_POINT('Ctrl Pts',(-10.5866618310001,15.2,1.16851838199999));
#259263=CARTESIAN_POINT('Ctrl Pts',(-10.5866618310001,11.6,1.16851838199999));
#259264=CARTESIAN_POINT('Ctrl Pts',(-10.5889058620001,15.2,1.16821573099998));
#259265=CARTESIAN_POINT('Ctrl Pts',(-10.5889058620001,11.6,1.16821573099998));
#259266=CARTESIAN_POINT('Ctrl Pts',(-10.5911561200001,15.2,1.16791022399998));
#259267=CARTESIAN_POINT('Ctrl Pts',(-10.5911561200001,11.6,1.16791022399998));
#259268=CARTESIAN_POINT('Ctrl Pts',(-10.5934125910001,15.2,1.16760185399999));
#259269=CARTESIAN_POINT('Ctrl Pts',(-10.5934125910001,11.6,1.16760185399999));
#259270=CARTESIAN_POINT('Ctrl Pts',(-10.5956752600001,15.2,1.16729060999999));
#259271=CARTESIAN_POINT('Ctrl Pts',(-10.5956752600001,11.6,1.16729060999999));
#259272=CARTESIAN_POINT('Ctrl Pts',(-10.5979441110001,15.2,1.16697648599999));
#259273=CARTESIAN_POINT('Ctrl Pts',(-10.5979441110001,11.6,1.16697648599999));
#259274=CARTESIAN_POINT('Ctrl Pts',(-10.6002191330001,15.2,1.16665947299999));
#259275=CARTESIAN_POINT('Ctrl Pts',(-10.6002191330001,11.6,1.16665947299999));
#259276=CARTESIAN_POINT('Ctrl Pts',(-10.6025003100001,15.2,1.16633956299999));
#259277=CARTESIAN_POINT('Ctrl Pts',(-10.6025003100001,11.6,1.16633956299998));
#259278=CARTESIAN_POINT('Ctrl Pts',(-10.6047876270001,15.2,1.16601674699998));
#259279=CARTESIAN_POINT('Ctrl Pts',(-10.6047876270001,11.6,1.16601674699998));
#259280=CARTESIAN_POINT('Ctrl Pts',(-10.6070810700001,15.2,1.16569101799998));
#259281=CARTESIAN_POINT('Ctrl Pts',(-10.6070810700001,11.6,1.16569101799998));
#259282=CARTESIAN_POINT('Ctrl Pts',(-10.6093806240001,15.2,1.16536236699998));
#259283=CARTESIAN_POINT('Ctrl Pts',(-10.6093806240001,11.6,1.16536236699998));
#259284=CARTESIAN_POINT('Ctrl Pts',(-10.6116862760001,15.2,1.16503078599999));
#259285=CARTESIAN_POINT('Ctrl Pts',(-10.6116862760001,11.6,1.16503078599999));
#259286=CARTESIAN_POINT('Ctrl Pts',(-10.6139980110001,15.2,1.16469626699998));
#259287=CARTESIAN_POINT('Ctrl Pts',(-10.6139980110001,11.6,1.16469626699998));
#259288=CARTESIAN_POINT('Ctrl Pts',(-10.6163158140001,15.2,1.16435880299999));
#259289=CARTESIAN_POINT('Ctrl Pts',(-10.6163158140001,11.6,1.16435880299999));
#259290=CARTESIAN_POINT('Ctrl Pts',(-10.6186396720001,15.2,1.16401838499999));
#259291=CARTESIAN_POINT('Ctrl Pts',(-10.6186396720001,11.6,1.16401838499998));
#259292=CARTESIAN_POINT('Ctrl Pts',(-10.6209695720001,15.2,1.16367500499999));
#259293=CARTESIAN_POINT('Ctrl Pts',(-10.6209695720001,11.6,1.16367500499999));
#259294=CARTESIAN_POINT('Ctrl Pts',(-10.6233054970001,15.2,1.16332865499999));
#259295=CARTESIAN_POINT('Ctrl Pts',(-10.6233054970001,11.6,1.16332865499999));
#259296=CARTESIAN_POINT('Ctrl Pts',(-10.6256474340001,15.2,1.16297932799998));
#259297=CARTESIAN_POINT('Ctrl Pts',(-10.6256474340001,11.6,1.16297932799998));
#259298=CARTESIAN_POINT('Ctrl Pts',(-10.6279953690001,15.2,1.16262701499998));
#259299=CARTESIAN_POINT('Ctrl Pts',(-10.6279953690001,11.6,1.16262701499998));
#259300=CARTESIAN_POINT('Ctrl Pts',(-10.6303492890001,15.2,1.16227170999998));
#259301=CARTESIAN_POINT('Ctrl Pts',(-10.6303492890001,11.6,1.16227170999998));
#259302=CARTESIAN_POINT('Ctrl Pts',(-10.6327091780001,15.2,1.16191340299999));
#259303=CARTESIAN_POINT('Ctrl Pts',(-10.6327091780001,11.6,1.16191340299999));
#259304=CARTESIAN_POINT('Ctrl Pts',(-10.6350750250001,15.2,1.16155208699999));
#259305=CARTESIAN_POINT('Ctrl Pts',(-10.6350750250001,11.6,1.16155208699999));
#259306=CARTESIAN_POINT('Ctrl Pts',(-10.6374468130001,15.2,1.16118775499999));
#259307=CARTESIAN_POINT('Ctrl Pts',(-10.6374468130001,11.6,1.16118775499999));
#259308=CARTESIAN_POINT('Ctrl Pts',(-10.6398245300001,15.2,1.16082039899998));
#259309=CARTESIAN_POINT('Ctrl Pts',(-10.6398245300001,11.6,1.16082039899998));
#259310=CARTESIAN_POINT('Ctrl Pts',(-10.6422081610001,15.2,1.16045001099998));
#259311=CARTESIAN_POINT('Ctrl Pts',(-10.6422081610001,11.6,1.16045001099998));
#259312=CARTESIAN_POINT('Ctrl Pts',(-10.6445976930001,15.2,1.16007658299999));
#259313=CARTESIAN_POINT('Ctrl Pts',(-10.6445976930001,11.6,1.16007658299999));
#259314=CARTESIAN_POINT('Ctrl Pts',(-10.6469931120001,15.2,1.15970010799999));
#259315=CARTESIAN_POINT('Ctrl Pts',(-10.6469931120001,11.6,1.15970010799999));
#259316=CARTESIAN_POINT('Ctrl Pts',(-10.6493944050001,15.2,1.15932057999999));
#259317=CARTESIAN_POINT('Ctrl Pts',(-10.6493944050001,11.6,1.15932057999998));
#259318=CARTESIAN_POINT('Ctrl Pts',(-10.6518015570001,15.2,1.15893798799998));
#259319=CARTESIAN_POINT('Ctrl Pts',(-10.6518015570001,11.6,1.15893798799998));
#259320=CARTESIAN_POINT('Ctrl Pts',(-10.6542145550001,15.2,1.15855232699999));
#259321=CARTESIAN_POINT('Ctrl Pts',(-10.6542145550001,11.6,1.15855232699999));
#259322=CARTESIAN_POINT('Ctrl Pts',(-10.6566333850001,15.2,1.15816358799998));
#259323=CARTESIAN_POINT('Ctrl Pts',(-10.6566333850001,11.6,1.15816358799998));
#259324=CARTESIAN_POINT('Ctrl Pts',(-10.6590580340001,15.2,1.15777176599998));
#259325=CARTESIAN_POINT('Ctrl Pts',(-10.6590580340001,11.6,1.15777176599998));
#259326=CARTESIAN_POINT('Ctrl Pts',(-10.6614884880001,15.2,1.15737684999999));
#259327=CARTESIAN_POINT('Ctrl Pts',(-10.6614884880001,11.6,1.15737684999999));
#259328=CARTESIAN_POINT('Ctrl Pts',(-10.6639247340001,15.2,1.15697883699998));
#259329=CARTESIAN_POINT('Ctrl Pts',(-10.6639247340001,11.6,1.15697883699998));
#259330=CARTESIAN_POINT('Ctrl Pts',(-10.6663667570001,15.2,1.15657771499999));
#259331=CARTESIAN_POINT('Ctrl Pts',(-10.6663667570001,11.6,1.15657771499999));
#259332=CARTESIAN_POINT('Ctrl Pts',(-10.6688145450001,15.2,1.15617348099998));
#259333=CARTESIAN_POINT('Ctrl Pts',(-10.6688145450001,11.6,1.15617348099998));
#259334=CARTESIAN_POINT('Ctrl Pts',(-10.6712680840001,15.2,1.15576612499999));
#259335=CARTESIAN_POINT('Ctrl Pts',(-10.6712680840001,11.6,1.15576612499999));
#259336=CARTESIAN_POINT('Ctrl Pts',(-10.6737273610001,15.2,1.15535563899998));
#259337=CARTESIAN_POINT('Ctrl Pts',(-10.6737273610001,11.6,1.15535563899998));
#259338=CARTESIAN_POINT('Ctrl Pts',(-10.6761923620001,15.2,1.15494201899998));
#259339=CARTESIAN_POINT('Ctrl Pts',(-10.6761923620001,11.6,1.15494201899998));
#259340=CARTESIAN_POINT('Ctrl Pts',(-10.6786630740001,15.2,1.15452525499999));
#259341=CARTESIAN_POINT('Ctrl Pts',(-10.6786630740001,11.6,1.15452525499998));
#259342=CARTESIAN_POINT('Ctrl Pts',(-10.6811394830001,15.2,1.15410534099999));
#259343=CARTESIAN_POINT('Ctrl Pts',(-10.6811394830001,11.6,1.15410534099999));
#259344=CARTESIAN_POINT('Ctrl Pts',(-10.6836215780001,15.2,1.15368226999998));
#259345=CARTESIAN_POINT('Ctrl Pts',(-10.6836215780001,11.6,1.15368226999998));
#259346=CARTESIAN_POINT('Ctrl Pts',(-10.6861093440001,15.2,1.15325603399999));
#259347=CARTESIAN_POINT('Ctrl Pts',(-10.6861093440001,11.6,1.15325603399999));
#259348=CARTESIAN_POINT('Ctrl Pts',(-10.6886027670001,15.2,1.15282662699999));
#259349=CARTESIAN_POINT('Ctrl Pts',(-10.6886027670001,11.6,1.15282662699998));
#259350=CARTESIAN_POINT('Ctrl Pts',(-10.6911018330001,15.2,1.15239403999999));
#259351=CARTESIAN_POINT('Ctrl Pts',(-10.6911018330001,11.6,1.15239403999999));
#259352=CARTESIAN_POINT('Ctrl Pts',(-10.6936065330001,15.2,1.15195826999999));
#259353=CARTESIAN_POINT('Ctrl Pts',(-10.6936065330001,11.6,1.15195826999999));
#259354=CARTESIAN_POINT('Ctrl Pts',(-10.6961168510001,15.2,1.15151930499998));
#259355=CARTESIAN_POINT('Ctrl Pts',(-10.6961168510001,11.6,1.15151930499998));
#259356=CARTESIAN_POINT('Ctrl Pts',(-10.6986327730001,15.2,1.15107714099999));
#259357=CARTESIAN_POINT('Ctrl Pts',(-10.6986327730001,11.6,1.15107714099999));
#259358=CARTESIAN_POINT('Ctrl Pts',(-10.7011542890001,15.2,1.15063176999998));
#259359=CARTESIAN_POINT('Ctrl Pts',(-10.7011542890001,11.6,1.15063176999998));
#259360=CARTESIAN_POINT('Ctrl Pts',(-10.7036813830001,15.2,1.15018318599999));
#259361=CARTESIAN_POINT('Ctrl Pts',(-10.7036813830001,11.6,1.15018318599999));
#259362=CARTESIAN_POINT('Ctrl Pts',(-10.7062140430001,15.2,1.14973138199999));
#259363=CARTESIAN_POINT('Ctrl Pts',(-10.7062140430001,11.6,1.14973138199999));
#259364=CARTESIAN_POINT('Ctrl Pts',(-10.7087522570001,15.2,1.14927634999999));
#259365=CARTESIAN_POINT('Ctrl Pts',(-10.7087522570001,11.6,1.14927634999999));
#259366=CARTESIAN_POINT('Ctrl Pts',(-10.7112960120001,15.2,1.14881808499999));
#259367=CARTESIAN_POINT('Ctrl Pts',(-10.7112960120001,11.6,1.14881808499998));
#259368=CARTESIAN_POINT('Ctrl Pts',(-10.7138452930001,15.2,1.14835657899999));
#259369=CARTESIAN_POINT('Ctrl Pts',(-10.7138452930001,11.6,1.14835657899999));
#259370=CARTESIAN_POINT('Ctrl Pts',(-10.7164000880001,15.2,1.14789182399999));
#259371=CARTESIAN_POINT('Ctrl Pts',(-10.7164000880001,11.6,1.14789182399999));
#259372=CARTESIAN_POINT('Ctrl Pts',(-10.7189603860001,15.2,1.14742381499998));
#259373=CARTESIAN_POINT('Ctrl Pts',(-10.7189603860001,11.6,1.14742381499998));
#259374=CARTESIAN_POINT('Ctrl Pts',(-10.7215261720001,15.2,1.14695254599999));
#259375=CARTESIAN_POINT('Ctrl Pts',(-10.7215261720001,11.6,1.14695254599999));
#259376=CARTESIAN_POINT('Ctrl Pts',(-10.7240974330001,15.2,1.14647800799998));
#259377=CARTESIAN_POINT('Ctrl Pts',(-10.7240974330001,11.6,1.14647800799998));
#259378=CARTESIAN_POINT('Ctrl Pts',(-10.7266741590001,15.2,1.14600019699999));
#259379=CARTESIAN_POINT('Ctrl Pts',(-10.7266741590001,11.6,1.14600019699999));
#259380=CARTESIAN_POINT('Ctrl Pts',(-10.7292563340001,15.2,1.14551910299999));
#259381=CARTESIAN_POINT('Ctrl Pts',(-10.7292563340001,11.6,1.14551910299999));
#259382=CARTESIAN_POINT('Ctrl Pts',(-10.7318439480001,15.2,1.14503472299999));
#259383=CARTESIAN_POINT('Ctrl Pts',(-10.7318439480001,11.6,1.14503472299999));
#259384=CARTESIAN_POINT('Ctrl Pts',(-10.7344369860001,15.2,1.14454704699999));
#259385=CARTESIAN_POINT('Ctrl Pts',(-10.7344369860001,11.6,1.14454704699999));
#259386=CARTESIAN_POINT('Ctrl Pts',(-10.7370354360001,15.2,1.14405607099998));
#259387=CARTESIAN_POINT('Ctrl Pts',(-10.7370354360001,11.6,1.14405607099998));
#259388=CARTESIAN_POINT('Ctrl Pts',(-10.7396392860001,15.2,1.14356178699999));
#259389=CARTESIAN_POINT('Ctrl Pts',(-10.7396392860001,11.6,1.14356178699999));
#259390=CARTESIAN_POINT('Ctrl Pts',(-10.7422485240001,15.2,1.14306418899998));
#259391=CARTESIAN_POINT('Ctrl Pts',(-10.7422485240001,11.6,1.14306418899998));
#259392=CARTESIAN_POINT('Ctrl Pts',(-10.7448631370001,15.2,1.14256327099998));
#259393=CARTESIAN_POINT('Ctrl Pts',(-10.7448631370001,11.6,1.14256327099998));
#259394=CARTESIAN_POINT('Ctrl Pts',(-10.7474831100001,15.2,1.14205902499998));
#259395=CARTESIAN_POINT('Ctrl Pts',(-10.7474831100001,11.6,1.14205902499998));
#259396=CARTESIAN_POINT('Ctrl Pts',(-10.7501084340001,15.2,1.14155144699998));
#259397=CARTESIAN_POINT('Ctrl Pts',(-10.7501084340001,11.6,1.14155144699998));
#259398=CARTESIAN_POINT('Ctrl Pts',(-10.7527390940001,15.2,1.14104052899998));
#259399=CARTESIAN_POINT('Ctrl Pts',(-10.7527390940001,11.6,1.14104052899998));
#259400=CARTESIAN_POINT('Ctrl Pts',(-10.7553750790001,15.2,1.14052626499999));
#259401=CARTESIAN_POINT('Ctrl Pts',(-10.7553750790001,11.6,1.14052626499999));
#259402=CARTESIAN_POINT('Ctrl Pts',(-10.7580163760001,15.2,1.14000864899999));
#259403=CARTESIAN_POINT('Ctrl Pts',(-10.7580163760001,11.6,1.14000864899999));
#259404=CARTESIAN_POINT('Ctrl Pts',(-10.7606629730001,15.2,1.13948767199998));
#259405=CARTESIAN_POINT('Ctrl Pts',(-10.7606629730001,11.6,1.13948767199998));
#259406=CARTESIAN_POINT('Ctrl Pts',(-10.7633148570001,15.2,1.13896333199999));
#259407=CARTESIAN_POINT('Ctrl Pts',(-10.7633148570001,11.6,1.13896333199999));
#259408=CARTESIAN_POINT('Ctrl Pts',(-10.7659720160001,15.2,1.13843561899999));
#259409=CARTESIAN_POINT('Ctrl Pts',(-10.7659720160001,11.6,1.13843561899999));
#259410=CARTESIAN_POINT('Ctrl Pts',(-10.7686344370001,15.2,1.13790452999998));
#259411=CARTESIAN_POINT('Ctrl Pts',(-10.7686344370001,11.6,1.13790452999998));
#259412=CARTESIAN_POINT('Ctrl Pts',(-10.7713021080001,15.2,1.13737005599999));
#259413=CARTESIAN_POINT('Ctrl Pts',(-10.7713021080001,11.6,1.13737005599999));
#259414=CARTESIAN_POINT('Ctrl Pts',(-10.7739750180001,15.2,1.13683219199999));
#259415=CARTESIAN_POINT('Ctrl Pts',(-10.7739750180001,11.6,1.13683219199999));
#259416=CARTESIAN_POINT('Ctrl Pts',(-10.7766531540001,15.2,1.13629093099998));
#259417=CARTESIAN_POINT('Ctrl Pts',(-10.7766531540001,11.6,1.13629093099998));
#259418=CARTESIAN_POINT('Ctrl Pts',(-10.7793365030001,15.2,1.13574626899998));
#259419=CARTESIAN_POINT('Ctrl Pts',(-10.7793365030001,11.6,1.13574626899998));
#259420=CARTESIAN_POINT('Ctrl Pts',(-10.7820250540001,15.2,1.13519819699999));
#259421=CARTESIAN_POINT('Ctrl Pts',(-10.7820250540001,11.6,1.13519819699999));
#259422=CARTESIAN_POINT('Ctrl Pts',(-10.7847187940001,15.2,1.13464671099999));
#259423=CARTESIAN_POINT('Ctrl Pts',(-10.7847187940001,11.6,1.13464671099999));
#259424=CARTESIAN_POINT('Ctrl Pts',(-10.7874177100001,15.2,1.13409180499998));
#259425=CARTESIAN_POINT('Ctrl Pts',(-10.7874177100001,11.6,1.13409180499998));
#259426=CARTESIAN_POINT('Ctrl Pts',(-10.7901217920001,15.2,1.13353347099999));
#259427=CARTESIAN_POINT('Ctrl Pts',(-10.7901217920001,11.6,1.13353347099999));
#259428=CARTESIAN_POINT('Ctrl Pts',(-10.7928310260001,15.2,1.13297170399999));
#259429=CARTESIAN_POINT('Ctrl Pts',(-10.7928310260001,11.6,1.13297170399999));
#259430=CARTESIAN_POINT('Ctrl Pts',(-10.7955454010001,15.2,1.13240649799998));
#259431=CARTESIAN_POINT('Ctrl Pts',(-10.7955454010001,11.6,1.13240649799998));
#259432=CARTESIAN_POINT('Ctrl Pts',(-10.7982649040001,15.2,1.13183784699999));
#259433=CARTESIAN_POINT('Ctrl Pts',(-10.7982649040001,11.6,1.13183784699999));
#259434=CARTESIAN_POINT('Ctrl Pts',(-10.8009895250001,15.2,1.13126574599999));
#259435=CARTESIAN_POINT('Ctrl Pts',(-10.8009895250001,11.6,1.13126574599998));
#259436=CARTESIAN_POINT('Ctrl Pts',(-10.8037192500001,15.2,1.13069018799999));
#259437=CARTESIAN_POINT('Ctrl Pts',(-10.8037192500001,11.6,1.13069018799999));
#259438=CARTESIAN_POINT('Ctrl Pts',(-10.8064540680001,15.2,1.13011116799999));
#259439=CARTESIAN_POINT('Ctrl Pts',(-10.8064540680001,11.6,1.13011116799999));
#259440=CARTESIAN_POINT('Ctrl Pts',(-10.8091939670001,15.2,1.12952867799998));
#259441=CARTESIAN_POINT('Ctrl Pts',(-10.8091939670001,11.6,1.12952867799998));
#259442=CARTESIAN_POINT('Ctrl Pts',(-10.8119389340001,15.2,1.12894271399998));
#259443=CARTESIAN_POINT('Ctrl Pts',(-10.8119389340001,11.6,1.12894271399998));
#259444=CARTESIAN_POINT('Ctrl Pts',(-10.8146889590001,15.2,1.12835326899999));
#259445=CARTESIAN_POINT('Ctrl Pts',(-10.8146889590001,11.6,1.12835326899999));
#259446=CARTESIAN_POINT('Ctrl Pts',(-10.8174440290001,15.2,1.12776033899999));
#259447=CARTESIAN_POINT('Ctrl Pts',(-10.8174440290001,11.6,1.12776033899999));
#259448=CARTESIAN_POINT('Ctrl Pts',(-10.8202041310001,15.2,1.12716391599998));
#259449=CARTESIAN_POINT('Ctrl Pts',(-10.8202041310001,11.6,1.12716391599998));
#259450=CARTESIAN_POINT('Ctrl Pts',(-10.8229692560001,15.2,1.12656399699999));
#259451=CARTESIAN_POINT('Ctrl Pts',(-10.8229692560001,11.6,1.12656399699999));
#259452=CARTESIAN_POINT('Ctrl Pts',(-10.8257393900001,15.2,1.12596057199998));
#259453=CARTESIAN_POINT('Ctrl Pts',(-10.8257393900001,11.6,1.12596057199998));
#259454=CARTESIAN_POINT('Ctrl Pts',(-10.8285145220001,15.2,1.12535363899998));
#259455=CARTESIAN_POINT('Ctrl Pts',(-10.8285145220001,11.6,1.12535363899998));
#259456=CARTESIAN_POINT('Ctrl Pts',(-10.8312946400001,15.2,1.12474319099999));
#259457=CARTESIAN_POINT('Ctrl Pts',(-10.8312946400001,11.6,1.12474319099999));
#259458=CARTESIAN_POINT('Ctrl Pts',(-10.8340797320001,15.2,1.12412922199999));
#259459=CARTESIAN_POINT('Ctrl Pts',(-10.8340797320001,11.6,1.12412922199998));
#259460=CARTESIAN_POINT('Ctrl Pts',(-10.8368697870001,15.2,1.12351172799999));
#259461=CARTESIAN_POINT('Ctrl Pts',(-10.8368697870001,11.6,1.12351172799999));
#259462=CARTESIAN_POINT('Ctrl Pts',(-10.8396647920001,15.2,1.12289069999999));
#259463=CARTESIAN_POINT('Ctrl Pts',(-10.8396647920001,11.6,1.12289069999999));
#259464=CARTESIAN_POINT('Ctrl Pts',(-10.8424647370001,15.2,1.12226613499999));
#259465=CARTESIAN_POINT('Ctrl Pts',(-10.8424647370001,11.6,1.12226613499998));
#259466=CARTESIAN_POINT('Ctrl Pts',(-10.8452696110001,15.2,1.12163802799999));
#259467=CARTESIAN_POINT('Ctrl Pts',(-10.8452696110001,11.6,1.12163802799999));
#259468=CARTESIAN_POINT('Ctrl Pts',(-10.8480794000001,15.2,1.12100637199998));
#259469=CARTESIAN_POINT('Ctrl Pts',(-10.8480794000001,11.6,1.12100637199998));
#259470=CARTESIAN_POINT('Ctrl Pts',(-10.8508940940001,15.2,1.12037116099998));
#259471=CARTESIAN_POINT('Ctrl Pts',(-10.8508940940001,11.6,1.12037116099998));
#259472=CARTESIAN_POINT('Ctrl Pts',(-10.8537136800001,15.2,1.11973238999999));
#259473=CARTESIAN_POINT('Ctrl Pts',(-10.8537136800001,11.6,1.11973238999999));
#259474=CARTESIAN_POINT('Ctrl Pts',(-10.8565381480001,15.2,1.11909005299998));
#259475=CARTESIAN_POINT('Ctrl Pts',(-10.8565381480001,11.6,1.11909005299998));
#259476=CARTESIAN_POINT('Ctrl Pts',(-10.8593674860001,15.2,1.11844414699998));
#259477=CARTESIAN_POINT('Ctrl Pts',(-10.8593674860001,11.6,1.11844414699998));
#259478=CARTESIAN_POINT('Ctrl Pts',(-10.8622016830001,15.2,1.11779466399998));
#259479=CARTESIAN_POINT('Ctrl Pts',(-10.8622016830001,11.6,1.11779466399998));
#259480=CARTESIAN_POINT('Ctrl Pts',(-10.8650407270001,15.2,1.11714159799998));
#259481=CARTESIAN_POINT('Ctrl Pts',(-10.8650407270001,11.6,1.11714159799998));
#259482=CARTESIAN_POINT('Ctrl Pts',(-10.8678846060001,15.2,1.11648494599998));
#259483=CARTESIAN_POINT('Ctrl Pts',(-10.8678846060001,11.6,1.11648494599998));
#259484=CARTESIAN_POINT('Ctrl Pts',(-10.8707333090001,15.2,1.11582469999998));
#259485=CARTESIAN_POINT('Ctrl Pts',(-10.8707333090001,11.6,1.11582469999998));
#259486=CARTESIAN_POINT('Ctrl Pts',(-10.8735868260001,15.2,1.11516085799999));
#259487=CARTESIAN_POINT('Ctrl Pts',(-10.8735868260001,11.6,1.11516085799999));
#259488=CARTESIAN_POINT('Ctrl Pts',(-10.8764451420001,15.2,1.11449341099998));
#259489=CARTESIAN_POINT('Ctrl Pts',(-10.8764451420001,11.6,1.11449341099998));
#259490=CARTESIAN_POINT('Ctrl Pts',(-10.8793082490001,15.2,1.11382235599998));
#259491=CARTESIAN_POINT('Ctrl Pts',(-10.8793082490001,11.6,1.11382235599998));
#259492=CARTESIAN_POINT('Ctrl Pts',(-10.8821761360001,15.2,1.11314768799998));
#259493=CARTESIAN_POINT('Ctrl Pts',(-10.8821761360001,11.6,1.11314768799998));
#259494=CARTESIAN_POINT('Ctrl Pts',(-10.8850487880001,15.2,1.11246939899999));
#259495=CARTESIAN_POINT('Ctrl Pts',(-10.8850487880001,11.6,1.11246939899999));
#259496=CARTESIAN_POINT('Ctrl Pts',(-10.8879261980001,15.2,1.11178748499999));
#259497=CARTESIAN_POINT('Ctrl Pts',(-10.8879261980001,11.6,1.11178748499999));
#259498=CARTESIAN_POINT('Ctrl Pts',(-10.8908083520001,15.2,1.11110194299998));
#259499=CARTESIAN_POINT('Ctrl Pts',(-10.8908083520001,11.6,1.11110194299998));
#259500=CARTESIAN_POINT('Ctrl Pts',(-10.8936952400001,15.2,1.11041276499999));
#259501=CARTESIAN_POINT('Ctrl Pts',(-10.8936952400001,11.6,1.11041276499999));
#259502=CARTESIAN_POINT('Ctrl Pts',(-10.8965868490001,15.2,1.10971994599999));
#259503=CARTESIAN_POINT('Ctrl Pts',(-10.8965868490001,11.6,1.10971994599998));
#259504=CARTESIAN_POINT('Ctrl Pts',(-10.8994831710001,15.2,1.10902348199998));
#259505=CARTESIAN_POINT('Ctrl Pts',(-10.8994831710001,11.6,1.10902348199998));
#259506=CARTESIAN_POINT('Ctrl Pts',(-10.9023841920001,15.2,1.10832336799998));
#259507=CARTESIAN_POINT('Ctrl Pts',(-10.9023841920001,11.6,1.10832336799998));
#259508=CARTESIAN_POINT('Ctrl Pts',(-10.9052899020001,15.2,1.10761959699999));
#259509=CARTESIAN_POINT('Ctrl Pts',(-10.9052899020001,11.6,1.10761959699999));
#259510=CARTESIAN_POINT('Ctrl Pts',(-10.9082002890001,15.2,1.10691216599998));
#259511=CARTESIAN_POINT('Ctrl Pts',(-10.9082002890001,11.6,1.10691216599998));
#259512=CARTESIAN_POINT('Ctrl Pts',(-10.9111153440001,15.2,1.10620106799999));
#259513=CARTESIAN_POINT('Ctrl Pts',(-10.9111153440001,11.6,1.10620106799999));
#259514=CARTESIAN_POINT('Ctrl Pts',(-10.9140350530001,15.2,1.10548629899998));
#259515=CARTESIAN_POINT('Ctrl Pts',(-10.9140350530001,11.6,1.10548629899998));
#259516=CARTESIAN_POINT('Ctrl Pts',(-10.9169594070001,15.2,1.10476785399999));
#259517=CARTESIAN_POINT('Ctrl Pts',(-10.9169594070001,11.6,1.10476785399999));
#259518=CARTESIAN_POINT('Ctrl Pts',(-10.9198883940001,15.2,1.10404572799998));
#259519=CARTESIAN_POINT('Ctrl Pts',(-10.9198883940001,11.6,1.10404572799998));
#259520=CARTESIAN_POINT('Ctrl Pts',(-10.9228220030001,15.2,1.10331991499999));
#259521=CARTESIAN_POINT('Ctrl Pts',(-10.9228220030001,11.6,1.10331991499998));
#259522=CARTESIAN_POINT('Ctrl Pts',(-10.9257602240001,15.2,1.10259041099999));
#259523=CARTESIAN_POINT('Ctrl Pts',(-10.9257602240001,11.6,1.10259041099999));
#259524=CARTESIAN_POINT('Ctrl Pts',(-10.9287030450001,15.2,1.10185720999999));
#259525=CARTESIAN_POINT('Ctrl Pts',(-10.9287030450001,11.6,1.10185720999999));
#259526=CARTESIAN_POINT('Ctrl Pts',(-10.9316504550001,15.2,1.10112030799999));
#259527=CARTESIAN_POINT('Ctrl Pts',(-10.9316504550001,11.6,1.10112030799998));
#259528=CARTESIAN_POINT('Ctrl Pts',(-10.9346024440001,15.2,1.10037969999999));
#259529=CARTESIAN_POINT('Ctrl Pts',(-10.9346024440001,11.6,1.10037969999999));
#259530=CARTESIAN_POINT('Ctrl Pts',(-10.9375590010001,15.2,1.09963537999999));
#259531=CARTESIAN_POINT('Ctrl Pts',(-10.9375590010001,11.6,1.09963537999999));
#259532=CARTESIAN_POINT('Ctrl Pts',(-10.9405201130001,15.2,1.09888734399998));
#259533=CARTESIAN_POINT('Ctrl Pts',(-10.9405201130001,11.6,1.09888734399998));
#259534=CARTESIAN_POINT('Ctrl Pts',(-10.9434857720001,15.2,1.09813558799999));
#259535=CARTESIAN_POINT('Ctrl Pts',(-10.9434857720001,11.6,1.09813558799999));
#259536=CARTESIAN_POINT('Ctrl Pts',(-10.9464559650001,15.2,1.09738010499999));
#259537=CARTESIAN_POINT('Ctrl Pts',(-10.9464559650001,11.6,1.09738010499999));
#259538=CARTESIAN_POINT('Ctrl Pts',(-10.9494306820001,15.2,1.09662089099999));
#259539=CARTESIAN_POINT('Ctrl Pts',(-10.9494306820001,11.6,1.09662089099999));
#259540=CARTESIAN_POINT('Ctrl Pts',(-10.9524099120001,15.2,1.09585794199999));
#259541=CARTESIAN_POINT('Ctrl Pts',(-10.9524099120001,11.6,1.09585794199999));
#259542=CARTESIAN_POINT('Ctrl Pts',(-10.9553936450001,15.2,1.09509125199999));
#259543=CARTESIAN_POINT('Ctrl Pts',(-10.9553936450001,11.6,1.09509125199999));
#259544=CARTESIAN_POINT('Ctrl Pts',(-10.9583818690001,15.2,1.09432081699998));
#259545=CARTESIAN_POINT('Ctrl Pts',(-10.9583818690001,11.6,1.09432081699998));
#259546=CARTESIAN_POINT('Ctrl Pts',(-10.9613745740001,15.2,1.09354663099999));
#259547=CARTESIAN_POINT('Ctrl Pts',(-10.9613745740001,11.6,1.09354663099999));
#259548=CARTESIAN_POINT('Ctrl Pts',(-10.9643717480001,15.2,1.09276869099999));
#259549=CARTESIAN_POINT('Ctrl Pts',(-10.9643717480001,11.6,1.09276869099999));
#259550=CARTESIAN_POINT('Ctrl Pts',(-10.9673733820001,15.2,1.09198699199998));
#259551=CARTESIAN_POINT('Ctrl Pts',(-10.9673733820001,11.6,1.09198699199998));
#259552=CARTESIAN_POINT('Ctrl Pts',(-10.9703794650001,15.2,1.09120152799999));
#259553=CARTESIAN_POINT('Ctrl Pts',(-10.9703794650001,11.6,1.09120152799999));
#259554=CARTESIAN_POINT('Ctrl Pts',(-10.9733899850001,15.2,1.09041229499999));
#259555=CARTESIAN_POINT('Ctrl Pts',(-10.9733899850001,11.6,1.09041229499998));
#259556=CARTESIAN_POINT('Ctrl Pts',(-10.9764049340001,15.2,1.08961928699999));
#259557=CARTESIAN_POINT('Ctrl Pts',(-10.9764049340001,11.6,1.08961928699999));
#259558=CARTESIAN_POINT('Ctrl Pts',(-10.9794242980001,15.2,1.08882250199999));
#259559=CARTESIAN_POINT('Ctrl Pts',(-10.9794242980001,11.6,1.08882250199999));
#259560=CARTESIAN_POINT('Ctrl Pts',(-10.9824480680001,15.2,1.08802193399999));
#259561=CARTESIAN_POINT('Ctrl Pts',(-10.9824480680001,11.6,1.08802193399998));
#259562=CARTESIAN_POINT('Ctrl Pts',(-10.9854762340001,15.2,1.08721757799998));
#259563=CARTESIAN_POINT('Ctrl Pts',(-10.9854762340001,11.6,1.08721757799998));
#259564=CARTESIAN_POINT('Ctrl Pts',(-10.9885087840001,15.2,1.08640942999998));
#259565=CARTESIAN_POINT('Ctrl Pts',(-10.9885087840001,11.6,1.08640942999998));
#259566=CARTESIAN_POINT('Ctrl Pts',(-10.9915457090001,15.2,1.08559748499998));
#259567=CARTESIAN_POINT('Ctrl Pts',(-10.9915457090001,11.6,1.08559748499998));
#259568=CARTESIAN_POINT('Ctrl Pts',(-10.9945869970001,15.2,1.08478173799998));
#259569=CARTESIAN_POINT('Ctrl Pts',(-10.9945869970001,11.6,1.08478173799998));
#259570=CARTESIAN_POINT('Ctrl Pts',(-10.9976326380001,15.2,1.08396218499998));
#259571=CARTESIAN_POINT('Ctrl Pts',(-10.9976326380001,11.6,1.08396218499998));
#259572=CARTESIAN_POINT('Ctrl Pts',(-11.0006826220001,15.2,1.08313882099999));
#259573=CARTESIAN_POINT('Ctrl Pts',(-11.0006826220001,11.6,1.08313882099999));
#259574=CARTESIAN_POINT('Ctrl Pts',(-11.0037369370001,15.2,1.08231164299998));
#259575=CARTESIAN_POINT('Ctrl Pts',(-11.0037369370001,11.6,1.08231164299998));
#259576=CARTESIAN_POINT('Ctrl Pts',(-11.0067955760001,15.2,1.08148064399999));
#259577=CARTESIAN_POINT('Ctrl Pts',(-11.0067955760001,11.6,1.08148064399999));
#259578=CARTESIAN_POINT('Ctrl Pts',(-11.0098585240001,15.2,1.08064582099999));
#259579=CARTESIAN_POINT('Ctrl Pts',(-11.0098585240001,11.6,1.08064582099999));
#259580=CARTESIAN_POINT('Ctrl Pts',(-11.0129257730001,15.2,1.07980717099998));
#259581=CARTESIAN_POINT('Ctrl Pts',(-11.0129257730001,11.6,1.07980717099998));
#259582=CARTESIAN_POINT('Ctrl Pts',(-11.0159973130001,15.2,1.07896468599999));
#259583=CARTESIAN_POINT('Ctrl Pts',(-11.0159973130001,11.6,1.07896468599999));
#259584=CARTESIAN_POINT('Ctrl Pts',(-11.0190731330001,15.2,1.07811836399998));
#259585=CARTESIAN_POINT('Ctrl Pts',(-11.0190731330001,11.6,1.07811836399998));
#259586=CARTESIAN_POINT('Ctrl Pts',(-11.0221532220001,15.2,1.07726820099999));
#259587=CARTESIAN_POINT('Ctrl Pts',(-11.0221532220001,11.6,1.07726820099999));
#259588=CARTESIAN_POINT('Ctrl Pts',(-11.0252375700001,15.2,1.07641418999998));
#259589=CARTESIAN_POINT('Ctrl Pts',(-11.0252375700001,11.6,1.07641418999998));
#259590=CARTESIAN_POINT('Ctrl Pts',(-11.0283261660001,15.2,1.07555632999999));
#259591=CARTESIAN_POINT('Ctrl Pts',(-11.0283261660001,11.6,1.07555632999999));
#259592=CARTESIAN_POINT('Ctrl Pts',(-11.0314190020001,15.2,1.07469461299999));
#259593=CARTESIAN_POINT('Ctrl Pts',(-11.0314190020001,11.6,1.07469461299999));
#259594=CARTESIAN_POINT('Ctrl Pts',(-11.0345160640001,15.2,1.07382903799999));
#259595=CARTESIAN_POINT('Ctrl Pts',(-11.0345160640001,11.6,1.07382903799999));
#259596=CARTESIAN_POINT('Ctrl Pts',(-11.0376173460001,15.2,1.07295959799998));
#259597=CARTESIAN_POINT('Ctrl Pts',(-11.0376173460001,11.6,1.07295959799998));
#259598=CARTESIAN_POINT('Ctrl Pts',(-11.0407228350001,15.2,1.07208629099999));
#259599=CARTESIAN_POINT('Ctrl Pts',(-11.0407228350001,11.6,1.07208629099999));
#259600=CARTESIAN_POINT('Ctrl Pts',(-11.0438325210001,15.2,1.07120911099999));
#259601=CARTESIAN_POINT('Ctrl Pts',(-11.0438325210001,11.6,1.07120911099999));
#259602=CARTESIAN_POINT('Ctrl Pts',(-11.0469463940001,15.2,1.07032805399998));
#259603=CARTESIAN_POINT('Ctrl Pts',(-11.0469463940001,11.6,1.07032805399998));
#259604=CARTESIAN_POINT('Ctrl Pts',(-11.0500644440001,15.2,1.06944311599999));
#259605=CARTESIAN_POINT('Ctrl Pts',(-11.0500644440001,11.6,1.06944311599999));
#259606=CARTESIAN_POINT('Ctrl Pts',(-11.0531866600001,15.2,1.06855429399999));
#259607=CARTESIAN_POINT('Ctrl Pts',(-11.0531866600001,11.6,1.06855429399999));
#259608=CARTESIAN_POINT('Ctrl Pts',(-11.0563130330001,15.2,1.06766158099999));
#259609=CARTESIAN_POINT('Ctrl Pts',(-11.0563130330001,11.6,1.06766158099999));
#259610=CARTESIAN_POINT('Ctrl Pts',(-11.0594435520001,15.2,1.06676497499999));
#259611=CARTESIAN_POINT('Ctrl Pts',(-11.0594435520001,11.6,1.06676497499999));
#259612=CARTESIAN_POINT('Ctrl Pts',(-11.0625782070001,15.2,1.06586446999998));
#259613=CARTESIAN_POINT('Ctrl Pts',(-11.0625782070001,11.6,1.06586446999998));
#259614=CARTESIAN_POINT('Ctrl Pts',(-11.0657169880001,15.2,1.06496006399999));
#259615=CARTESIAN_POINT('Ctrl Pts',(-11.0657169880001,11.6,1.06496006399999));
#259616=CARTESIAN_POINT('Ctrl Pts',(-11.0688598860001,15.2,1.06405175099999));
#259617=CARTESIAN_POINT('Ctrl Pts',(-11.0688598860001,11.6,1.06405175099999));
#259618=CARTESIAN_POINT('Ctrl Pts',(-11.0720068880001,15.2,1.06313952799999));
#259619=CARTESIAN_POINT('Ctrl Pts',(-11.0720068880001,11.6,1.06313952799999));
#259620=CARTESIAN_POINT('Ctrl Pts',(-11.0751579870001,15.2,1.06222338999999));
#259621=CARTESIAN_POINT('Ctrl Pts',(-11.0751579870001,11.6,1.06222338999999));
#259622=CARTESIAN_POINT('Ctrl Pts',(-11.0783131710001,15.2,1.06130333499999));
#259623=CARTESIAN_POINT('Ctrl Pts',(-11.0783131710001,11.6,1.06130333499999));
#259624=CARTESIAN_POINT('Ctrl Pts',(-11.0814724300001,15.2,1.06037935499999));
#259625=CARTESIAN_POINT('Ctrl Pts',(-11.0814724300001,11.6,1.06037935499998));
#259626=CARTESIAN_POINT('Ctrl Pts',(-11.0846357550001,15.2,1.05945144899998));
#259627=CARTESIAN_POINT('Ctrl Pts',(-11.0846357550001,11.6,1.05945144899998));
#259628=CARTESIAN_POINT('Ctrl Pts',(-11.0878031360001,15.2,1.05851961199999));
#259629=CARTESIAN_POINT('Ctrl Pts',(-11.0878031360001,11.6,1.05851961199999));
#259630=CARTESIAN_POINT('Ctrl Pts',(-11.0909745620001,15.2,1.05758383999999));
#259631=CARTESIAN_POINT('Ctrl Pts',(-11.0909745620001,11.6,1.05758383999999));
#259632=CARTESIAN_POINT('Ctrl Pts',(-11.0941500240001,15.2,1.05664412899999));
#259633=CARTESIAN_POINT('Ctrl Pts',(-11.0941500240001,11.6,1.05664412899999));
#259634=CARTESIAN_POINT('Ctrl Pts',(-11.0973295110001,15.2,1.05570047499999));
#259635=CARTESIAN_POINT('Ctrl Pts',(-11.0973295110001,11.6,1.05570047499999));
#259636=CARTESIAN_POINT('Ctrl Pts',(-11.1005130140001,15.2,1.05475287299999));
#259637=CARTESIAN_POINT('Ctrl Pts',(-11.1005130140001,11.6,1.05475287299999));
#259638=CARTESIAN_POINT('Ctrl Pts',(-11.1037005220001,15.2,1.05380132099999));
#259639=CARTESIAN_POINT('Ctrl Pts',(-11.1037005220001,11.6,1.05380132099999));
#259640=CARTESIAN_POINT('Ctrl Pts',(-11.1068920250001,15.2,1.05284581399999));
#259641=CARTESIAN_POINT('Ctrl Pts',(-11.1068920250001,11.6,1.05284581399998));
#259642=CARTESIAN_POINT('Ctrl Pts',(-11.1100875160001,15.2,1.05188634799998));
#259643=CARTESIAN_POINT('Ctrl Pts',(-11.1100875160001,11.6,1.05188634799998));
#259644=CARTESIAN_POINT('Ctrl Pts',(-11.1132869810001,15.2,1.05092291799998));
#259645=CARTESIAN_POINT('Ctrl Pts',(-11.1132869810001,11.6,1.05092291799998));
#259646=CARTESIAN_POINT('Ctrl Pts',(-11.1164904140001,15.2,1.04995552199998));
#259647=CARTESIAN_POINT('Ctrl Pts',(-11.1164904140001,11.6,1.04995552199998));
#259648=CARTESIAN_POINT('Ctrl Pts',(-11.1196978020001,15.2,1.04898415499999));
#259649=CARTESIAN_POINT('Ctrl Pts',(-11.1196978020001,11.6,1.04898415499999));
#259650=CARTESIAN_POINT('Ctrl Pts',(-11.1229091360001,15.2,1.04800881199999));
#259651=CARTESIAN_POINT('Ctrl Pts',(-11.1229091360001,11.6,1.04800881199999));
#259652=CARTESIAN_POINT('Ctrl Pts',(-11.1261244080001,15.2,1.04702949099998));
#259653=CARTESIAN_POINT('Ctrl Pts',(-11.1261244080001,11.6,1.04702949099998));
#259654=CARTESIAN_POINT('Ctrl Pts',(-11.1293436050001,15.2,1.04604618899999));
#259655=CARTESIAN_POINT('Ctrl Pts',(-11.1293436050001,11.6,1.04604618899998));
#259656=CARTESIAN_POINT('Ctrl Pts',(-11.1325667200001,15.2,1.04505889899999));
#259657=CARTESIAN_POINT('Ctrl Pts',(-11.1325667200001,11.6,1.04505889899999));
#259658=CARTESIAN_POINT('Ctrl Pts',(-11.1357937420001,15.2,1.04406762099998));
#259659=CARTESIAN_POINT('Ctrl Pts',(-11.1357937420001,11.6,1.04406762099998));
#259660=CARTESIAN_POINT('Ctrl Pts',(-11.1390246620001,15.2,1.04307234699998));
#259661=CARTESIAN_POINT('Ctrl Pts',(-11.1390246620001,11.6,1.04307234699998));
#259662=CARTESIAN_POINT('Ctrl Pts',(-11.1422594690001,15.2,1.04207307599999));
#259663=CARTESIAN_POINT('Ctrl Pts',(-11.1422594690001,11.6,1.04207307599998));
#259664=CARTESIAN_POINT('Ctrl Pts',(-11.1454981540001,15.2,1.04106980299999));
#259665=CARTESIAN_POINT('Ctrl Pts',(-11.1454981540001,11.6,1.04106980299999));
#259666=CARTESIAN_POINT('Ctrl Pts',(-11.1487407070001,15.2,1.04006252499998));
#259667=CARTESIAN_POINT('Ctrl Pts',(-11.1487407070001,11.6,1.04006252499998));
#259668=CARTESIAN_POINT('Ctrl Pts',(-11.1519871190001,15.2,1.03905123799999));
#259669=CARTESIAN_POINT('Ctrl Pts',(-11.1519871190001,11.6,1.03905123799999));
#259670=CARTESIAN_POINT('Ctrl Pts',(-11.1552373810001,15.2,1.03803593699999));
#259671=CARTESIAN_POINT('Ctrl Pts',(-11.1552373810001,11.6,1.03803593699999));
#259672=CARTESIAN_POINT('Ctrl Pts',(-11.1584914810001,15.2,1.03701662199999));
#259673=CARTESIAN_POINT('Ctrl Pts',(-11.1584914810001,11.6,1.03701662199999));
#259674=CARTESIAN_POINT('Ctrl Pts',(-11.1617494110001,15.2,1.03599328399998));
#259675=CARTESIAN_POINT('Ctrl Pts',(-11.1617494110001,11.6,1.03599328399998));
#259676=CARTESIAN_POINT('Ctrl Pts',(-11.1650111610001,15.2,1.03496592399999));
#259677=CARTESIAN_POINT('Ctrl Pts',(-11.1650111610001,11.6,1.03496592399999));
#259678=CARTESIAN_POINT('Ctrl Pts',(-11.1682767210001,15.2,1.03393453499999));
#259679=CARTESIAN_POINT('Ctrl Pts',(-11.1682767210001,11.6,1.03393453499998));
#259680=CARTESIAN_POINT('Ctrl Pts',(-11.1715460820001,15.2,1.03289911399999));
#259681=CARTESIAN_POINT('Ctrl Pts',(-11.1715460820001,11.6,1.03289911399999));
#259682=CARTESIAN_POINT('Ctrl Pts',(-11.1748192350001,15.2,1.03185965899999));
#259683=CARTESIAN_POINT('Ctrl Pts',(-11.1748192350001,11.6,1.03185965899998));
#259684=CARTESIAN_POINT('Ctrl Pts',(-11.1780961680001,15.2,1.03081616499999));
#259685=CARTESIAN_POINT('Ctrl Pts',(-11.1780961680001,11.6,1.03081616499999));
#259686=CARTESIAN_POINT('Ctrl Pts',(-11.1813768730001,15.2,1.02976862899999));
#259687=CARTESIAN_POINT('Ctrl Pts',(-11.1813768730001,11.6,1.02976862899998));
#259688=CARTESIAN_POINT('Ctrl Pts',(-11.1846613420001,15.2,1.02871704699998));
#259689=CARTESIAN_POINT('Ctrl Pts',(-11.1846613420001,11.6,1.02871704699998));
#259690=CARTESIAN_POINT('Ctrl Pts',(-11.1879495640001,15.2,1.02766141599998));
#259691=CARTESIAN_POINT('Ctrl Pts',(-11.1879495640001,11.6,1.02766141599998));
#259692=CARTESIAN_POINT('Ctrl Pts',(-11.1912415290001,15.2,1.02660173099999));
#259693=CARTESIAN_POINT('Ctrl Pts',(-11.1912415290001,11.6,1.02660173099998));
#259694=CARTESIAN_POINT('Ctrl Pts',(-11.1945372270001,15.2,1.02553798999999));
#259695=CARTESIAN_POINT('Ctrl Pts',(-11.1945372270001,11.6,1.02553798999998));
#259696=CARTESIAN_POINT('Ctrl Pts',(-11.1978366510001,15.2,1.02447018799999));
#259697=CARTESIAN_POINT('Ctrl Pts',(-11.1978366510001,11.6,1.02447018799999));
#259698=CARTESIAN_POINT('Ctrl Pts',(-11.2011397890001,15.2,1.02339832299998));
#259699=CARTESIAN_POINT('Ctrl Pts',(-11.2011397890001,11.6,1.02339832299998));
#259700=CARTESIAN_POINT('Ctrl Pts',(-11.2044466330001,15.2,1.02232238999999));
#259701=CARTESIAN_POINT('Ctrl Pts',(-11.2044466330001,11.6,1.02232238999999));
#259702=CARTESIAN_POINT('Ctrl Pts',(-11.2077571730001,15.2,1.02124238699998));
#259703=CARTESIAN_POINT('Ctrl Pts',(-11.2077571730001,11.6,1.02124238699998));
#259704=CARTESIAN_POINT('Ctrl Pts',(-11.2110714010001,15.2,1.02015830899999));
#259705=CARTESIAN_POINT('Ctrl Pts',(-11.2110714010001,11.6,1.02015830899999));
#259706=CARTESIAN_POINT('Ctrl Pts',(-11.2143893040001,15.2,1.01907015299998));
#259707=CARTESIAN_POINT('Ctrl Pts',(-11.2143893040001,11.6,1.01907015299998));
#259708=CARTESIAN_POINT('Ctrl Pts',(-11.2177108770001,15.2,1.01797791699999));
#259709=CARTESIAN_POINT('Ctrl Pts',(-11.2177108770001,11.6,1.01797791699999));
#259710=CARTESIAN_POINT('Ctrl Pts',(-11.2210361080001,15.2,1.01688159599998));
#259711=CARTESIAN_POINT('Ctrl Pts',(-11.2210361080001,11.6,1.01688159599998));
#259712=CARTESIAN_POINT('Ctrl Pts',(-11.2243649880001,15.2,1.01578118599999));
#259713=CARTESIAN_POINT('Ctrl Pts',(-11.2243649880001,11.6,1.01578118599999));
#259714=CARTESIAN_POINT('Ctrl Pts',(-11.2276975070001,15.2,1.01467668399998));
#259715=CARTESIAN_POINT('Ctrl Pts',(-11.2276975070001,11.6,1.01467668399998));
#259716=CARTESIAN_POINT('Ctrl Pts',(-11.2310336580001,15.2,1.01356808799999));
#259717=CARTESIAN_POINT('Ctrl Pts',(-11.2310336580001,11.6,1.01356808799998));
#259718=CARTESIAN_POINT('Ctrl Pts',(-11.2343734290001,15.2,1.01245539299998));
#259719=CARTESIAN_POINT('Ctrl Pts',(-11.2343734290001,11.6,1.01245539299998));
#259720=CARTESIAN_POINT('Ctrl Pts',(-11.2377168140001,15.2,1.01133859799999));
#259721=CARTESIAN_POINT('Ctrl Pts',(-11.2377168140001,11.6,1.01133859799999));
#259722=CARTESIAN_POINT('Ctrl Pts',(-11.2410637990001,15.2,1.01021769499999));
#259723=CARTESIAN_POINT('Ctrl Pts',(-11.2410637990001,11.6,1.01021769499999));
#259724=CARTESIAN_POINT('Ctrl Pts',(-11.2444143790001,15.2,1.00909268499999));
#259725=CARTESIAN_POINT('Ctrl Pts',(-11.2444143790001,11.6,1.00909268499999));
#259726=CARTESIAN_POINT('Ctrl Pts',(-11.2477685430001,15.2,1.00796356299998));
#259727=CARTESIAN_POINT('Ctrl Pts',(-11.2477685430001,11.6,1.00796356299998));
#259728=CARTESIAN_POINT('Ctrl Pts',(-11.2511262810001,15.2,1.00683032499999));
#259729=CARTESIAN_POINT('Ctrl Pts',(-11.2511262810001,11.6,1.00683032499999));
#259730=CARTESIAN_POINT('Ctrl Pts',(-11.2544875850001,15.2,1.00569296999999));
#259731=CARTESIAN_POINT('Ctrl Pts',(-11.2544875850001,11.6,1.00569296999998));
#259732=CARTESIAN_POINT('Ctrl Pts',(-11.2578524460001,15.2,1.00455149199998));
#259733=CARTESIAN_POINT('Ctrl Pts',(-11.2578524460001,11.6,1.00455149199998));
#259734=CARTESIAN_POINT('Ctrl Pts',(-11.2612208540001,15.2,1.00340588999998));
#259735=CARTESIAN_POINT('Ctrl Pts',(-11.2612208540001,11.6,1.00340588999998));
#259736=CARTESIAN_POINT('Ctrl Pts',(-11.2645927990001,15.2,1.00225615799999));
#259737=CARTESIAN_POINT('Ctrl Pts',(-11.2645927990001,11.6,1.00225615799999));
#259738=CARTESIAN_POINT('Ctrl Pts',(-11.2679682740001,15.2,1.00110229499998));
#259739=CARTESIAN_POINT('Ctrl Pts',(-11.2679682740001,11.6,1.00110229499998));
#259740=CARTESIAN_POINT('Ctrl Pts',(-11.2713472680001,15.2,0.999944296999988));
#259741=CARTESIAN_POINT('Ctrl Pts',(-11.2713472680001,11.6,0.999944296999988));
#259742=CARTESIAN_POINT('Ctrl Pts',(-11.2747297730001,15.2,0.998782160999987));
#259743=CARTESIAN_POINT('Ctrl Pts',(-11.2747297730001,11.6,0.998782160999987));
#259744=CARTESIAN_POINT('Ctrl Pts',(-11.2781157800001,15.2,0.997615882999985));
#259745=CARTESIAN_POINT('Ctrl Pts',(-11.2781157800001,11.6,0.997615882999984));
#259746=CARTESIAN_POINT('Ctrl Pts',(-11.2815052780001,15.2,0.996445461999986));
#259747=CARTESIAN_POINT('Ctrl Pts',(-11.2815052780001,11.6,0.996445461999986));
#259748=CARTESIAN_POINT('Ctrl Pts',(-11.2848982590001,15.2,0.995270892999987));
#259749=CARTESIAN_POINT('Ctrl Pts',(-11.2848982590001,11.6,0.995270892999986));
#259750=CARTESIAN_POINT('Ctrl Pts',(-11.2882947150001,15.2,0.994092171999985));
#259751=CARTESIAN_POINT('Ctrl Pts',(-11.2882947150001,11.6,0.994092171999985));
#259752=CARTESIAN_POINT('Ctrl Pts',(-11.2916946350001,15.2,0.992909295999986));
#259753=CARTESIAN_POINT('Ctrl Pts',(-11.2916946350001,11.6,0.992909295999986));
#259754=CARTESIAN_POINT('Ctrl Pts',(-11.2950980120001,15.2,0.991722263999986));
#259755=CARTESIAN_POINT('Ctrl Pts',(-11.2950980120001,11.6,0.991722263999985));
#259756=CARTESIAN_POINT('Ctrl Pts',(-11.2985048360001,15.2,0.990531070999987));
#259757=CARTESIAN_POINT('Ctrl Pts',(-11.2985048360001,11.6,0.990531070999987));
#259758=CARTESIAN_POINT('Ctrl Pts',(-11.3019150960001,15.2,0.989335713999986));
#259759=CARTESIAN_POINT('Ctrl Pts',(-11.3019150960001,11.6,0.989335713999985));
#259760=CARTESIAN_POINT('Ctrl Pts',(-11.3053287860001,15.2,0.988136191999986));
#259761=CARTESIAN_POINT('Ctrl Pts',(-11.3053287860001,11.6,0.988136191999986));
#259762=CARTESIAN_POINT('Ctrl Pts',(-11.3087458960001,15.2,0.986932498999984));
#259763=CARTESIAN_POINT('Ctrl Pts',(-11.3087458960001,11.6,0.986932498999983));
#259764=CARTESIAN_POINT('Ctrl Pts',(-11.3121664170001,15.2,0.985724631999982));
#259765=CARTESIAN_POINT('Ctrl Pts',(-11.3121664170001,11.6,0.985724631999982));
#259766=CARTESIAN_POINT('Ctrl Pts',(-11.3155903390001,15.2,0.984512589999986));
#259767=CARTESIAN_POINT('Ctrl Pts',(-11.3155903390001,11.6,0.984512589999986));
#259768=CARTESIAN_POINT('Ctrl Pts',(-11.3190176540001,15.2,0.983296368999986));
#259769=CARTESIAN_POINT('Ctrl Pts',(-11.3190176540001,11.6,0.983296368999986));
#259770=CARTESIAN_POINT('Ctrl Pts',(-11.3224483530001,15.2,0.982075965999982));
#259771=CARTESIAN_POINT('Ctrl Pts',(-11.3224483530001,11.6,0.982075965999982));
#259772=CARTESIAN_POINT('Ctrl Pts',(-11.3258824260001,15.2,0.980851377999983));
#259773=CARTESIAN_POINT('Ctrl Pts',(-11.3258824260001,11.6,0.980851377999982));
#259774=CARTESIAN_POINT('Ctrl Pts',(-11.3293198660001,15.2,0.979622600999988));
#259775=CARTESIAN_POINT('Ctrl Pts',(-11.3293198660001,11.6,0.979622600999987));
#259776=CARTESIAN_POINT('Ctrl Pts',(-11.3327606630001,15.2,0.978389632999987));
#259777=CARTESIAN_POINT('Ctrl Pts',(-11.3327606630001,11.6,0.978389632999987));
#259778=CARTESIAN_POINT('Ctrl Pts',(-11.3362048080001,15.2,0.977152470999982));
#259779=CARTESIAN_POINT('Ctrl Pts',(-11.3362048080001,11.6,0.977152470999982));
#259780=CARTESIAN_POINT('Ctrl Pts',(-11.3396522920001,15.2,0.975911110999985));
#259781=CARTESIAN_POINT('Ctrl Pts',(-11.3396522920001,11.6,0.975911110999985));
#259782=CARTESIAN_POINT('Ctrl Pts',(-11.3431031070001,15.2,0.974665550999987));
#259783=CARTESIAN_POINT('Ctrl Pts',(-11.3431031070001,11.6,0.974665550999986));
#259784=CARTESIAN_POINT('Ctrl Pts',(-11.3465572430001,15.2,0.973415788999983));
#259785=CARTESIAN_POINT('Ctrl Pts',(-11.3465572430001,11.6,0.973415788999982));
#259786=CARTESIAN_POINT('Ctrl Pts',(-11.3500146920001,15.2,0.972161818999986));
#259787=CARTESIAN_POINT('Ctrl Pts',(-11.3500146920001,11.6,0.972161818999985));
#259788=CARTESIAN_POINT('Ctrl Pts',(-11.3534754440001,15.2,0.970903640999987));
#259789=CARTESIAN_POINT('Ctrl Pts',(-11.3534754440001,11.6,0.970903640999987));
#259790=CARTESIAN_POINT('Ctrl Pts',(-11.3569394920001,15.2,0.969641250999986));
#259791=CARTESIAN_POINT('Ctrl Pts',(-11.3569394920001,11.6,0.969641250999986));
#259792=CARTESIAN_POINT('Ctrl Pts',(-11.3604068260001,15.2,0.968374645999983));
#259793=CARTESIAN_POINT('Ctrl Pts',(-11.3604068260001,11.6,0.968374645999983));
#259794=CARTESIAN_POINT('Ctrl Pts',(-11.3638774360001,15.2,0.967103821999986));
#259795=CARTESIAN_POINT('Ctrl Pts',(-11.3638774360001,11.6,0.967103821999986));
#259796=CARTESIAN_POINT('Ctrl Pts',(-11.3673513150001,15.2,0.965828777999986));
#259797=CARTESIAN_POINT('Ctrl Pts',(-11.3673513150001,11.6,0.965828777999986));
#259798=CARTESIAN_POINT('Ctrl Pts',(-11.3708284530001,15.2,0.964549509999983));
#259799=CARTESIAN_POINT('Ctrl Pts',(-11.3708284530001,11.6,0.964549509999983));
#259800=CARTESIAN_POINT('Ctrl Pts',(-11.3743088440001,15.2,0.963266015999986));
#259801=CARTESIAN_POINT('Ctrl Pts',(-11.3743088440001,11.6,0.963266015999986));
#259802=CARTESIAN_POINT('Ctrl Pts',(-11.3777924770001,15.2,0.961978291999985));
#259803=CARTESIAN_POINT('Ctrl Pts',(-11.3777924770001,11.6,0.961978291999985));
#259804=CARTESIAN_POINT('Ctrl Pts',(-11.3812793430001,15.2,0.960686337999985));
#259805=CARTESIAN_POINT('Ctrl Pts',(-11.3812793430001,11.6,0.960686337999985));
#259806=CARTESIAN_POINT('Ctrl Pts',(-11.3847694350001,15.2,0.959390146999985));
#259807=CARTESIAN_POINT('Ctrl Pts',(-11.3847694350001,11.6,0.959390146999985));
#259808=CARTESIAN_POINT('Ctrl Pts',(-11.3882627430001,15.2,0.958089718999986));
#259809=CARTESIAN_POINT('Ctrl Pts',(-11.3882627430001,11.6,0.958089718999986));
#259810=CARTESIAN_POINT('Ctrl Pts',(-11.3917592580001,15.2,0.956785048999986));
#259811=CARTESIAN_POINT('Ctrl Pts',(-11.3917592580001,11.6,0.956785048999986));
#259812=CARTESIAN_POINT('Ctrl Pts',(-11.3952589700001,15.2,0.955476136999986));
#259813=CARTESIAN_POINT('Ctrl Pts',(-11.3952589700001,11.6,0.955476136999986));
#259814=CARTESIAN_POINT('Ctrl Pts',(-11.3987618720001,15.2,0.954162976999986));
#259815=CARTESIAN_POINT('Ctrl Pts',(-11.3987618720001,11.6,0.954162976999986));
#259816=CARTESIAN_POINT('Ctrl Pts',(-11.4022679530001,15.2,0.952845567999985));
#259817=CARTESIAN_POINT('Ctrl Pts',(-11.4022679530001,11.6,0.952845567999984));
#259818=CARTESIAN_POINT('Ctrl Pts',(-11.4057772070001,15.2,0.951523905999987));
#259819=CARTESIAN_POINT('Ctrl Pts',(-11.4057772070001,11.6,0.951523905999986));
#259820=CARTESIAN_POINT('Ctrl Pts',(-11.4092896250001,15.2,0.950197990999988));
#259821=CARTESIAN_POINT('Ctrl Pts',(-11.4092896250001,11.6,0.950197990999988));
#259822=CARTESIAN_POINT('Ctrl Pts',(-11.4128052000001,15.2,0.948867817999983));
#259823=CARTESIAN_POINT('Ctrl Pts',(-11.4128052000001,11.6,0.948867817999983));
#259824=CARTESIAN_POINT('Ctrl Pts',(-11.4163239240001,15.2,0.947533386999986));
#259825=CARTESIAN_POINT('Ctrl Pts',(-11.4163239240001,11.6,0.947533386999985));
#259826=CARTESIAN_POINT('Ctrl Pts',(-11.4198457890001,15.2,0.946194692999986));
#259827=CARTESIAN_POINT('Ctrl Pts',(-11.4198457890001,11.6,0.946194692999986));
#259828=CARTESIAN_POINT('Ctrl Pts',(-11.4233707840001,15.2,0.944851733999985));
#259829=CARTESIAN_POINT('Ctrl Pts',(-11.4233707840001,11.6,0.944851733999985));
#259830=CARTESIAN_POINT('Ctrl Pts',(-11.4268989030001,15.2,0.943504507999986));
#259831=CARTESIAN_POINT('Ctrl Pts',(-11.4268989030001,11.6,0.943504507999986));
#259832=CARTESIAN_POINT('Ctrl Pts',(-11.4304301310001,15.2,0.942153010999984));
#259833=CARTESIAN_POINT('Ctrl Pts',(-11.4304301310001,11.6,0.942153010999984));
#259834=CARTESIAN_POINT('Ctrl Pts',(-11.4339644600001,15.2,0.940797237999984));
#259835=CARTESIAN_POINT('Ctrl Pts',(-11.4339644600001,11.6,0.940797237999984));
#259836=CARTESIAN_POINT('Ctrl Pts',(-11.4375018800001,15.2,0.939437186999985));
#259837=CARTESIAN_POINT('Ctrl Pts',(-11.4375018800001,11.6,0.939437186999985));
#259838=CARTESIAN_POINT('Ctrl Pts',(-11.4410423790001,15.2,0.938072855999987));
#259839=CARTESIAN_POINT('Ctrl Pts',(-11.4410423790001,11.6,0.938072855999987));
#259840=CARTESIAN_POINT('Ctrl Pts',(-11.4445859520001,15.2,0.936704240999986));
#259841=CARTESIAN_POINT('Ctrl Pts',(-11.4445859520001,11.6,0.936704240999986));
#259842=CARTESIAN_POINT('Ctrl Pts',(-11.4481325920001,15.2,0.935331340999985));
#259843=CARTESIAN_POINT('Ctrl Pts',(-11.4481325920001,11.6,0.935331340999985));
#259844=CARTESIAN_POINT('Ctrl Pts',(-11.4516822960001,15.2,0.933954156999985));
#259845=CARTESIAN_POINT('Ctrl Pts',(-11.4516822960001,11.6,0.933954156999985));
#259846=CARTESIAN_POINT('Ctrl Pts',(-11.4552350600001,15.2,0.932572684999986));
#259847=CARTESIAN_POINT('Ctrl Pts',(-11.4552350600001,11.6,0.932572684999986));
#259848=CARTESIAN_POINT('Ctrl Pts',(-11.4580797200001,15.2,0.931464077999986));
#259849=CARTESIAN_POINT('Ctrl Pts',(-11.4580797200001,11.6,0.931464077999986));
#259850=CARTESIAN_POINT('Ctrl Pts',(-11.4602145910001,15.2,0.930630692999985));
#259851=CARTESIAN_POINT('Ctrl Pts',(-11.4602145910001,11.6,0.930630692999985));
#259852=CARTESIAN_POINT('Ctrl Pts',(-11.4616384500001,15.2,0.930074245999983));
#259853=CARTESIAN_POINT('Ctrl Pts',(-11.4616384500001,11.6,0.930074245999983));
#259854=CARTESIAN_POINT('Ctrl Pts',(-11.4623505340001,15.2,0.929795807999985));
#259855=CARTESIAN_POINT('Ctrl Pts',(-11.4623505340001,11.6,0.929795807999984));
#259856=CARTESIAN_POINT('Ctrl Pts',(-10.3068855240001,15.2,1.18690176599999));
#259857=CARTESIAN_POINT('Ctrl Pts',(-10.3070598110001,15.2,1.18690675299999));
#259858=CARTESIAN_POINT('Ctrl Pts',(-10.3074144740001,15.2,1.18691681599998));
#259859=CARTESIAN_POINT('Ctrl Pts',(-10.3079518800001,15.2,1.18693179799998));
#259860=CARTESIAN_POINT('Ctrl Pts',(-10.3086758300001,15.2,1.18695143999998));
#259861=CARTESIAN_POINT('Ctrl Pts',(-10.3095915440001,15.2,1.18697537099999));
#259862=CARTESIAN_POINT('Ctrl Pts',(-10.3105221240001,15.2,1.18699875499999));
#259863=CARTESIAN_POINT('Ctrl Pts',(-10.3114622390001,15.2,1.18702143499998));
#259864=CARTESIAN_POINT('Ctrl Pts',(-10.3124118610001,15.2,1.18704339399998));
#259865=CARTESIAN_POINT('Ctrl Pts',(-10.3133709660001,15.2,1.18706460899999));
#259866=CARTESIAN_POINT('Ctrl Pts',(-10.3143395250001,15.2,1.18708506599999));
#259867=CARTESIAN_POINT('Ctrl Pts',(-10.3153175130001,15.2,1.18710474299998));
#259868=CARTESIAN_POINT('Ctrl Pts',(-10.3163049050001,15.2,1.18712362399998));
#259869=CARTESIAN_POINT('Ctrl Pts',(-10.3173016730001,15.2,1.18714168899999));
#259870=CARTESIAN_POINT('Ctrl Pts',(-10.3183077930001,15.2,1.18715892099999));
#259871=CARTESIAN_POINT('Ctrl Pts',(-10.3193232400001,15.2,1.18717530199998));
#259872=CARTESIAN_POINT('Ctrl Pts',(-10.3203479850001,15.2,1.18719081299998));
#259873=CARTESIAN_POINT('Ctrl Pts',(-10.3213820050001,15.2,1.18720543699999));
#259874=CARTESIAN_POINT('Ctrl Pts',(-10.3224252740001,15.2,1.18721915599998));
#259875=CARTESIAN_POINT('Ctrl Pts',(-10.3234777680001,15.2,1.18723195099999));
#259876=CARTESIAN_POINT('Ctrl Pts',(-10.3245394590001,15.2,1.18724380599998));
#259877=CARTESIAN_POINT('Ctrl Pts',(-10.3256103250001,15.2,1.18725470399998));
#259878=CARTESIAN_POINT('Ctrl Pts',(-10.3266903400001,15.2,1.18726462499998));
#259879=CARTESIAN_POINT('Ctrl Pts',(-10.3277794780001,15.2,1.18727355499999));
#259880=CARTESIAN_POINT('Ctrl Pts',(-10.3288777160001,15.2,1.18728147399999));
#259881=CARTESIAN_POINT('Ctrl Pts',(-10.3299850290001,15.2,1.18728836599999));
#259882=CARTESIAN_POINT('Ctrl Pts',(-10.3311013920001,15.2,1.18729421399999));
#259883=CARTESIAN_POINT('Ctrl Pts',(-10.3322267810001,15.2,1.18729900199999));
#259884=CARTESIAN_POINT('Ctrl Pts',(-10.3333611710001,15.2,1.18730271099999));
#259885=CARTESIAN_POINT('Ctrl Pts',(-10.3345045400001,15.2,1.18730532599999));
#259886=CARTESIAN_POINT('Ctrl Pts',(-10.3356568620001,15.2,1.18730682999999));
#259887=CARTESIAN_POINT('Ctrl Pts',(-10.3368181130001,15.2,1.18730720599999));
#259888=CARTESIAN_POINT('Ctrl Pts',(-10.3379882700001,15.2,1.18730643699998));
#259889=CARTESIAN_POINT('Ctrl Pts',(-10.3391673090001,15.2,1.18730450799998));
#259890=CARTESIAN_POINT('Ctrl Pts',(-10.3403552060001,15.2,1.18730140199999));
#259891=CARTESIAN_POINT('Ctrl Pts',(-10.3415519380001,15.2,1.18729710199998));
#259892=CARTESIAN_POINT('Ctrl Pts',(-10.3427574820001,15.2,1.18729159399999));
#259893=CARTESIAN_POINT('Ctrl Pts',(-10.3439718130001,15.2,1.18728485899998));
#259894=CARTESIAN_POINT('Ctrl Pts',(-10.3451949090001,15.2,1.18727688299999));
#259895=CARTESIAN_POINT('Ctrl Pts',(-10.3464267470001,15.2,1.18726764999999));
#259896=CARTESIAN_POINT('Ctrl Pts',(-10.3476673040001,15.2,1.18725714299998));
#259897=CARTESIAN_POINT('Ctrl Pts',(-10.3489165560001,15.2,1.18724534699998));
#259898=CARTESIAN_POINT('Ctrl Pts',(-10.3501744810001,15.2,1.18723224699998));
#259899=CARTESIAN_POINT('Ctrl Pts',(-10.3514410560001,15.2,1.18721782799998));
#259900=CARTESIAN_POINT('Ctrl Pts',(-10.3527162580001,15.2,1.18720207199999));
#259901=CARTESIAN_POINT('Ctrl Pts',(-10.3540000650001,15.2,1.18718496499998));
#259902=CARTESIAN_POINT('Ctrl Pts',(-10.3552924550001,15.2,1.18716649199999));
#259903=CARTESIAN_POINT('Ctrl Pts',(-10.3565934040001,15.2,1.18714663699999));
#259904=CARTESIAN_POINT('Ctrl Pts',(-10.3579028900001,15.2,1.18712538499999));
#259905=CARTESIAN_POINT('Ctrl Pts',(-10.3592208920001,15.2,1.18710272199999));
#259906=CARTESIAN_POINT('Ctrl Pts',(-10.3605473870001,15.2,1.18707863099999));
#259907=CARTESIAN_POINT('Ctrl Pts',(-10.3618823540001,15.2,1.18705309899998));
#259908=CARTESIAN_POINT('Ctrl Pts',(-10.3632257690001,15.2,1.18702610999998));
#259909=CARTESIAN_POINT('Ctrl Pts',(-10.3645776120001,15.2,1.18699765099999));
#259910=CARTESIAN_POINT('Ctrl Pts',(-10.3659378610001,15.2,1.18696770399998));
#259911=CARTESIAN_POINT('Ctrl Pts',(-10.3673064940001,15.2,1.18693625599999));
#259912=CARTESIAN_POINT('Ctrl Pts',(-10.3686834880001,15.2,1.18690329399998));
#259913=CARTESIAN_POINT('Ctrl Pts',(-10.3700688240001,15.2,1.18686880099999));
#259914=CARTESIAN_POINT('Ctrl Pts',(-10.3714624790001,15.2,1.18683276399999));
#259915=CARTESIAN_POINT('Ctrl Pts',(-10.3728644310001,15.2,1.18679516799999));
#259916=CARTESIAN_POINT('Ctrl Pts',(-10.3742746610001,15.2,1.18675599899999));
#259917=CARTESIAN_POINT('Ctrl Pts',(-10.3756931460001,15.2,1.18671524399999));
#259918=CARTESIAN_POINT('Ctrl Pts',(-10.3771198660001,15.2,1.18667288599998));
#259919=CARTESIAN_POINT('Ctrl Pts',(-10.3785547980001,15.2,1.18662891399998));
#259920=CARTESIAN_POINT('Ctrl Pts',(-10.3799979240001,15.2,1.18658331299998));
#259921=CARTESIAN_POINT('Ctrl Pts',(-10.3814492210001,15.2,1.18653606699999));
#259922=CARTESIAN_POINT('Ctrl Pts',(-10.3829086680001,15.2,1.18648716499999));
#259923=CARTESIAN_POINT('Ctrl Pts',(-10.3843762450001,15.2,1.18643659199998));
#259924=CARTESIAN_POINT('Ctrl Pts',(-10.3858519330001,15.2,1.18638433399999));
#259925=CARTESIAN_POINT('Ctrl Pts',(-10.3873357080001,15.2,1.18633037799999));
#259926=CARTESIAN_POINT('Ctrl Pts',(-10.3888275530001,15.2,1.18627470999999));
#259927=CARTESIAN_POINT('Ctrl Pts',(-10.3903274450001,15.2,1.18621731599998));
#259928=CARTESIAN_POINT('Ctrl Pts',(-10.3918353650001,15.2,1.18615818399999));
#259929=CARTESIAN_POINT('Ctrl Pts',(-10.3933512920001,15.2,1.18609729999998));
#259930=CARTESIAN_POINT('Ctrl Pts',(-10.3948752070001,15.2,1.18603464899998));
#259931=CARTESIAN_POINT('Ctrl Pts',(-10.3964070880001,15.2,1.18597021999999));
#259932=CARTESIAN_POINT('Ctrl Pts',(-10.3979469170001,15.2,1.18590399899999));
#259933=CARTESIAN_POINT('Ctrl Pts',(-10.3994946730001,15.2,1.18583597199999));
#259934=CARTESIAN_POINT('Ctrl Pts',(-10.4010503360001,15.2,1.18576612699998));
#259935=CARTESIAN_POINT('Ctrl Pts',(-10.4026138870001,15.2,1.18569445199999));
#259936=CARTESIAN_POINT('Ctrl Pts',(-10.4041853050001,15.2,1.18562093199999));
#259937=CARTESIAN_POINT('Ctrl Pts',(-10.4057645710001,15.2,1.18554555499998));
#259938=CARTESIAN_POINT('Ctrl Pts',(-10.4073516650001,15.2,1.18546830799998));
#259939=CARTESIAN_POINT('Ctrl Pts',(-10.4089465690001,15.2,1.18538917799999));
#259940=CARTESIAN_POINT('Ctrl Pts',(-10.4105492620001,15.2,1.18530815299998));
#259941=CARTESIAN_POINT('Ctrl Pts',(-10.4121597240001,15.2,1.18522521999999));
#259942=CARTESIAN_POINT('Ctrl Pts',(-10.4137779370001,15.2,1.18514036599999));
#259943=CARTESIAN_POINT('Ctrl Pts',(-10.4154038820001,15.2,1.18505357999998));
#259944=CARTESIAN_POINT('Ctrl Pts',(-10.4170375390001,15.2,1.18496484799998));
#259945=CARTESIAN_POINT('Ctrl Pts',(-10.4186788900001,15.2,1.18487415599999));
#259946=CARTESIAN_POINT('Ctrl Pts',(-10.4203279130001,15.2,1.18478149699999));
#259947=CARTESIAN_POINT('Ctrl Pts',(-10.4219845930001,15.2,1.18468685399999));
#259948=CARTESIAN_POINT('Ctrl Pts',(-10.4236489080001,15.2,1.18459021499998));
#259949=CARTESIAN_POINT('Ctrl Pts',(-10.4253208410001,15.2,1.18449156999999));
#259950=CARTESIAN_POINT('Ctrl Pts',(-10.4270003720001,15.2,1.18439090599999));
#259951=CARTESIAN_POINT('Ctrl Pts',(-10.4286874830001,15.2,1.18428821199998));
#259952=CARTESIAN_POINT('Ctrl Pts',(-10.4303821540001,15.2,1.18418347399999));
#259953=CARTESIAN_POINT('Ctrl Pts',(-10.4320843690001,15.2,1.18407667999998));
#259954=CARTESIAN_POINT('Ctrl Pts',(-10.4337941070001,15.2,1.18396781999999));
#259955=CARTESIAN_POINT('Ctrl Pts',(-10.4355113520001,15.2,1.18385688099998));
#259956=CARTESIAN_POINT('Ctrl Pts',(-10.4372360820001,15.2,1.18374385099999));
#259957=CARTESIAN_POINT('Ctrl Pts',(-10.4389682810001,15.2,1.18362871999999));
#259958=CARTESIAN_POINT('Ctrl Pts',(-10.4407079310001,15.2,1.18351147399999));
#259959=CARTESIAN_POINT('Ctrl Pts',(-10.4424550130001,15.2,1.18339210299998));
#259960=CARTESIAN_POINT('Ctrl Pts',(-10.4442095090001,15.2,1.18327059399999));
#259961=CARTESIAN_POINT('Ctrl Pts',(-10.4459714000001,15.2,1.18314693699999));
#259962=CARTESIAN_POINT('Ctrl Pts',(-10.4477406700001,15.2,1.18302111899999));
#259963=CARTESIAN_POINT('Ctrl Pts',(-10.4495173000001,15.2,1.18289313099998));
#259964=CARTESIAN_POINT('Ctrl Pts',(-10.4513012710001,15.2,1.18276295899999));
#259965=CARTESIAN_POINT('Ctrl Pts',(-10.4530925660001,15.2,1.18263059399998));
#259966=CARTESIAN_POINT('Ctrl Pts',(-10.4548911670001,15.2,1.18249602199999));
#259967=CARTESIAN_POINT('Ctrl Pts',(-10.4566970570001,15.2,1.18235923399999));
#259968=CARTESIAN_POINT('Ctrl Pts',(-10.4585102170001,15.2,1.18222021899999));
#259969=CARTESIAN_POINT('Ctrl Pts',(-10.4603306310001,15.2,1.18207896399999));
#259970=CARTESIAN_POINT('Ctrl Pts',(-10.4621582800001,15.2,1.18193545999999));
#259971=CARTESIAN_POINT('Ctrl Pts',(-10.4639931470001,15.2,1.18178969599999));
#259972=CARTESIAN_POINT('Ctrl Pts',(-10.4658352150001,15.2,1.18164165899998));
#259973=CARTESIAN_POINT('Ctrl Pts',(-10.4676844650001,15.2,1.18149133999998));
#259974=CARTESIAN_POINT('Ctrl Pts',(-10.4695408810001,15.2,1.18133872599998));
#259975=CARTESIAN_POINT('Ctrl Pts',(-10.4714044460001,15.2,1.18118380899999));
#259976=CARTESIAN_POINT('Ctrl Pts',(-10.4732751410001,15.2,1.18102657599998));
#259977=CARTESIAN_POINT('Ctrl Pts',(-10.4751529500001,15.2,1.18086701799998));
#259978=CARTESIAN_POINT('Ctrl Pts',(-10.4770378570001,15.2,1.18070512399999));
#259979=CARTESIAN_POINT('Ctrl Pts',(-10.4789298430001,15.2,1.18054088199999));
#259980=CARTESIAN_POINT('Ctrl Pts',(-10.4808288920001,15.2,1.18037428299999));
#259981=CARTESIAN_POINT('Ctrl Pts',(-10.4827349850001,15.2,1.18020531599999));
#259982=CARTESIAN_POINT('Ctrl Pts',(-10.4846481080001,15.2,1.18003396999999));
#259983=CARTESIAN_POINT('Ctrl Pts',(-10.4865682440001,15.2,1.17986023499999));
#259984=CARTESIAN_POINT('Ctrl Pts',(-10.4884953720001,15.2,1.17968410099999));
#259985=CARTESIAN_POINT('Ctrl Pts',(-10.4904294800001,15.2,1.17950555699998));
#259986=CARTESIAN_POINT('Ctrl Pts',(-10.4923705490001,15.2,1.17932459399999));
#259987=CARTESIAN_POINT('Ctrl Pts',(-10.4943185630001,15.2,1.17914119999998));
#259988=CARTESIAN_POINT('Ctrl Pts',(-10.4962735060001,15.2,1.17895536499999));
#259989=CARTESIAN_POINT('Ctrl Pts',(-10.4982353590001,15.2,1.17876708099999));
#259990=CARTESIAN_POINT('Ctrl Pts',(-10.5002041080001,15.2,1.17857633499999));
#259991=CARTESIAN_POINT('Ctrl Pts',(-10.5021797350001,15.2,1.17838311899999));
#259992=CARTESIAN_POINT('Ctrl Pts',(-10.5041622250001,15.2,1.17818742199999));
#259993=CARTESIAN_POINT('Ctrl Pts',(-10.5061515600001,15.2,1.17798923599999));
#259994=CARTESIAN_POINT('Ctrl Pts',(-10.5081477230001,15.2,1.17778854799999));
#259995=CARTESIAN_POINT('Ctrl Pts',(-10.5101507010001,15.2,1.17758534999998));
#259996=CARTESIAN_POINT('Ctrl Pts',(-10.5121604750001,15.2,1.17737963099998));
#259997=CARTESIAN_POINT('Ctrl Pts',(-10.5141770310001,15.2,1.17717138199998));
#259998=CARTESIAN_POINT('Ctrl Pts',(-10.5162003510001,15.2,1.17696059399998));
#259999=CARTESIAN_POINT('Ctrl Pts',(-10.5182304190001,15.2,1.17674725699999));
#260000=CARTESIAN_POINT('Ctrl Pts',(-10.5202672190001,15.2,1.17653135999999));
#260001=CARTESIAN_POINT('Ctrl Pts',(-10.5223107360001,15.2,1.17631289399998));
#260002=CARTESIAN_POINT('Ctrl Pts',(-10.5243609530001,15.2,1.17609184999999));
#260003=CARTESIAN_POINT('Ctrl Pts',(-10.5264178550001,15.2,1.17586821899998));
#260004=CARTESIAN_POINT('Ctrl Pts',(-10.5284814260001,15.2,1.17564198999998));
#260005=CARTESIAN_POINT('Ctrl Pts',(-10.5305516490001,15.2,1.17541315299999));
#260006=CARTESIAN_POINT('Ctrl Pts',(-10.5326285090001,15.2,1.17518170099999));
#260007=CARTESIAN_POINT('Ctrl Pts',(-10.5347119910001,15.2,1.17494762299998));
#260008=CARTESIAN_POINT('Ctrl Pts',(-10.5368020780001,15.2,1.17471090999999));
#260009=CARTESIAN_POINT('Ctrl Pts',(-10.5388987570001,15.2,1.17447155299998));
#260010=CARTESIAN_POINT('Ctrl Pts',(-10.5410020080001,15.2,1.17422954199998));
#260011=CARTESIAN_POINT('Ctrl Pts',(-10.5431118190001,15.2,1.17398486899999));
#260012=CARTESIAN_POINT('Ctrl Pts',(-10.5452281730001,15.2,1.17373752299998));
#260013=CARTESIAN_POINT('Ctrl Pts',(-10.5473510550001,15.2,1.17348749699998));
#260014=CARTESIAN_POINT('Ctrl Pts',(-10.5494804500001,15.2,1.17323477999999));
#260015=CARTESIAN_POINT('Ctrl Pts',(-10.5516163410001,15.2,1.17297936399999));
#260016=CARTESIAN_POINT('Ctrl Pts',(-10.5537587150001,15.2,1.17272124099999));
#260017=CARTESIAN_POINT('Ctrl Pts',(-10.5559075550001,15.2,1.17246039999999));
#260018=CARTESIAN_POINT('Ctrl Pts',(-10.5580628460001,15.2,1.17219683299998));
#260019=CARTESIAN_POINT('Ctrl Pts',(-10.5602245730001,15.2,1.17193052999998));
#260020=CARTESIAN_POINT('Ctrl Pts',(-10.5623927210001,15.2,1.17166148499999));
#260021=CARTESIAN_POINT('Ctrl Pts',(-10.5645672750001,15.2,1.17138968599999));
#260022=CARTESIAN_POINT('Ctrl Pts',(-10.5667482200001,15.2,1.17111512499998));
#260023=CARTESIAN_POINT('Ctrl Pts',(-10.5689355400001,15.2,1.17083779399998));
#260024=CARTESIAN_POINT('Ctrl Pts',(-10.5711292210001,15.2,1.17055768399998));
#260025=CARTESIAN_POINT('Ctrl Pts',(-10.5733292470001,15.2,1.17027478699999));
#260026=CARTESIAN_POINT('Ctrl Pts',(-10.5755356040001,15.2,1.16998909399999));
#260027=CARTESIAN_POINT('Ctrl Pts',(-10.5777482770001,15.2,1.16970059599999));
#260028=CARTESIAN_POINT('Ctrl Pts',(-10.5799672510001,15.2,1.16940928399998));
#260029=CARTESIAN_POINT('Ctrl Pts',(-10.5821925120001,15.2,1.16911514999999));
#260030=CARTESIAN_POINT('Ctrl Pts',(-10.5844240430001,15.2,1.16881818499999));
#260031=CARTESIAN_POINT('Ctrl Pts',(-10.5866618310001,15.2,1.16851838199999));
#260032=CARTESIAN_POINT('Ctrl Pts',(-10.5889058620001,15.2,1.16821573099998));
#260033=CARTESIAN_POINT('Ctrl Pts',(-10.5911561200001,15.2,1.16791022399998));
#260034=CARTESIAN_POINT('Ctrl Pts',(-10.5934125910001,15.2,1.16760185399999));
#260035=CARTESIAN_POINT('Ctrl Pts',(-10.5956752600001,15.2,1.16729060999999));
#260036=CARTESIAN_POINT('Ctrl Pts',(-10.5979441110001,15.2,1.16697648599999));
#260037=CARTESIAN_POINT('Ctrl Pts',(-10.6002191330001,15.2,1.16665947299999));
#260038=CARTESIAN_POINT('Ctrl Pts',(-10.6025003100001,15.2,1.16633956299999));
#260039=CARTESIAN_POINT('Ctrl Pts',(-10.6047876270001,15.2,1.16601674699998));
#260040=CARTESIAN_POINT('Ctrl Pts',(-10.6070810700001,15.2,1.16569101799998));
#260041=CARTESIAN_POINT('Ctrl Pts',(-10.6093806240001,15.2,1.16536236699998));
#260042=CARTESIAN_POINT('Ctrl Pts',(-10.6116862760001,15.2,1.16503078599999));
#260043=CARTESIAN_POINT('Ctrl Pts',(-10.6139980110001,15.2,1.16469626699998));
#260044=CARTESIAN_POINT('Ctrl Pts',(-10.6163158140001,15.2,1.16435880299999));
#260045=CARTESIAN_POINT('Ctrl Pts',(-10.6186396720001,15.2,1.16401838499999));
#260046=CARTESIAN_POINT('Ctrl Pts',(-10.6209695720001,15.2,1.16367500499999));
#260047=CARTESIAN_POINT('Ctrl Pts',(-10.6233054970001,15.2,1.16332865499999));
#260048=CARTESIAN_POINT('Ctrl Pts',(-10.6256474340001,15.2,1.16297932799998));
#260049=CARTESIAN_POINT('Ctrl Pts',(-10.6279953690001,15.2,1.16262701499998));
#260050=CARTESIAN_POINT('Ctrl Pts',(-10.6303492890001,15.2,1.16227170999998));
#260051=CARTESIAN_POINT('Ctrl Pts',(-10.6327091780001,15.2,1.16191340299999));
#260052=CARTESIAN_POINT('Ctrl Pts',(-10.6350750250001,15.2,1.16155208699999));
#260053=CARTESIAN_POINT('Ctrl Pts',(-10.6374468130001,15.2,1.16118775499999));
#260054=CARTESIAN_POINT('Ctrl Pts',(-10.6398245300001,15.2,1.16082039899998));
#260055=CARTESIAN_POINT('Ctrl Pts',(-10.6422081610001,15.2,1.16045001099998));
#260056=CARTESIAN_POINT('Ctrl Pts',(-10.6445976930001,15.2,1.16007658299999));
#260057=CARTESIAN_POINT('Ctrl Pts',(-10.6469931120001,15.2,1.15970010799999));
#260058=CARTESIAN_POINT('Ctrl Pts',(-10.6493944050001,15.2,1.15932057999999));
#260059=CARTESIAN_POINT('Ctrl Pts',(-10.6518015570001,15.2,1.15893798799998));
#260060=CARTESIAN_POINT('Ctrl Pts',(-10.6542145550001,15.2,1.15855232699999));
#260061=CARTESIAN_POINT('Ctrl Pts',(-10.6566333850001,15.2,1.15816358799998));
#260062=CARTESIAN_POINT('Ctrl Pts',(-10.6590580340001,15.2,1.15777176599998));
#260063=CARTESIAN_POINT('Ctrl Pts',(-10.6614884880001,15.2,1.15737684999999));
#260064=CARTESIAN_POINT('Ctrl Pts',(-10.6639247340001,15.2,1.15697883699998));
#260065=CARTESIAN_POINT('Ctrl Pts',(-10.6663667570001,15.2,1.15657771499999));
#260066=CARTESIAN_POINT('Ctrl Pts',(-10.6688145450001,15.2,1.15617348099998));
#260067=CARTESIAN_POINT('Ctrl Pts',(-10.6712680840001,15.2,1.15576612499999));
#260068=CARTESIAN_POINT('Ctrl Pts',(-10.6737273610001,15.2,1.15535563899998));
#260069=CARTESIAN_POINT('Ctrl Pts',(-10.6761923620001,15.2,1.15494201899998));
#260070=CARTESIAN_POINT('Ctrl Pts',(-10.6786630740001,15.2,1.15452525499999));
#260071=CARTESIAN_POINT('Ctrl Pts',(-10.6811394830001,15.2,1.15410534099999));
#260072=CARTESIAN_POINT('Ctrl Pts',(-10.6836215780001,15.2,1.15368226999998));
#260073=CARTESIAN_POINT('Ctrl Pts',(-10.6861093440001,15.2,1.15325603399999));
#260074=CARTESIAN_POINT('Ctrl Pts',(-10.6886027670001,15.2,1.15282662699999));
#260075=CARTESIAN_POINT('Ctrl Pts',(-10.6911018330001,15.2,1.15239403999999));
#260076=CARTESIAN_POINT('Ctrl Pts',(-10.6936065330001,15.2,1.15195826999999));
#260077=CARTESIAN_POINT('Ctrl Pts',(-10.6961168510001,15.2,1.15151930499998));
#260078=CARTESIAN_POINT('Ctrl Pts',(-10.6986327730001,15.2,1.15107714099999));
#260079=CARTESIAN_POINT('Ctrl Pts',(-10.7011542890001,15.2,1.15063176999998));
#260080=CARTESIAN_POINT('Ctrl Pts',(-10.7036813830001,15.2,1.15018318599999));
#260081=CARTESIAN_POINT('Ctrl Pts',(-10.7062140430001,15.2,1.14973138199999));
#260082=CARTESIAN_POINT('Ctrl Pts',(-10.7087522570001,15.2,1.14927634999999));
#260083=CARTESIAN_POINT('Ctrl Pts',(-10.7112960120001,15.2,1.14881808499999));
#260084=CARTESIAN_POINT('Ctrl Pts',(-10.7138452930001,15.2,1.14835657899999));
#260085=CARTESIAN_POINT('Ctrl Pts',(-10.7164000880001,15.2,1.14789182399999));
#260086=CARTESIAN_POINT('Ctrl Pts',(-10.7189603860001,15.2,1.14742381499998));
#260087=CARTESIAN_POINT('Ctrl Pts',(-10.7215261720001,15.2,1.14695254599999));
#260088=CARTESIAN_POINT('Ctrl Pts',(-10.7240974330001,15.2,1.14647800799998));
#260089=CARTESIAN_POINT('Ctrl Pts',(-10.7266741590001,15.2,1.14600019699999));
#260090=CARTESIAN_POINT('Ctrl Pts',(-10.7292563340001,15.2,1.14551910299999));
#260091=CARTESIAN_POINT('Ctrl Pts',(-10.7318439480001,15.2,1.14503472299999));
#260092=CARTESIAN_POINT('Ctrl Pts',(-10.734955593487,15.2,1.14444951182125));
#260093=CARTESIAN_POINT('Ctrl Pts',(-10.7380753572566,15.2,1.14385935058935));
#260094=CARTESIAN_POINT('Ctrl Pts',(-10.7412032147435,15.2,1.14326422341062));
#260095=CARTESIAN_POINT('Ctrl Pts',(-10.7443391425131,15.2,1.1426641201787));
#260096=CARTESIAN_POINT('Ctrl Pts',(-10.7474831100001,15.2,1.14205902499998));
#260097=CARTESIAN_POINT('Ctrl Pts',(-10.7501084340001,15.2,1.14155144699998));
#260098=CARTESIAN_POINT('Ctrl Pts',(-10.7527390940001,15.2,1.14104052899998));
#260099=CARTESIAN_POINT('Ctrl Pts',(-10.7553750790001,15.2,1.14052626499999));
#260100=CARTESIAN_POINT('Ctrl Pts',(-10.7580163760001,15.2,1.14000864899999));
#260101=CARTESIAN_POINT('Ctrl Pts',(-10.7606629730001,15.2,1.13948767199998));
#260102=CARTESIAN_POINT('Ctrl Pts',(-10.7633148570001,15.2,1.13896333199999));
#260103=CARTESIAN_POINT('Ctrl Pts',(-10.7659720160001,15.2,1.13843561899999));
#260104=CARTESIAN_POINT('Ctrl Pts',(-10.7686344370001,15.2,1.13790452999998));
#260105=CARTESIAN_POINT('Ctrl Pts',(-10.7713021080001,15.2,1.13737005599999));
#260106=CARTESIAN_POINT('Ctrl Pts',(-10.7739750180001,15.2,1.13683219199999));
#260107=CARTESIAN_POINT('Ctrl Pts',(-10.7766531540001,15.2,1.13629093099998));
#260108=CARTESIAN_POINT('Ctrl Pts',(-10.7793365030001,15.2,1.13574626899998));
#260109=CARTESIAN_POINT('Ctrl Pts',(-10.7820250540001,15.2,1.13519819699999));
#260110=CARTESIAN_POINT('Ctrl Pts',(-10.7847187940001,15.2,1.13464671099999));
#260111=CARTESIAN_POINT('Ctrl Pts',(-10.7874177100001,15.2,1.13409180499998));
#260112=CARTESIAN_POINT('Ctrl Pts',(-10.7901217920001,15.2,1.13353347099999));
#260113=CARTESIAN_POINT('Ctrl Pts',(-10.7928310260001,15.2,1.13297170399999));
#260114=CARTESIAN_POINT('Ctrl Pts',(-10.7955454010001,15.2,1.13240649799998));
#260115=CARTESIAN_POINT('Ctrl Pts',(-10.7982649040001,15.2,1.13183784699999));
#260116=CARTESIAN_POINT('Ctrl Pts',(-10.8009895250001,15.2,1.13126574599999));
#260117=CARTESIAN_POINT('Ctrl Pts',(-10.8037192500001,15.2,1.13069018799999));
#260118=CARTESIAN_POINT('Ctrl Pts',(-10.8064540680001,15.2,1.13011116799999));
#260119=CARTESIAN_POINT('Ctrl Pts',(-10.8091939670001,15.2,1.12952867799998));
#260120=CARTESIAN_POINT('Ctrl Pts',(-10.8119389340001,15.2,1.12894271399998));
#260121=CARTESIAN_POINT('Ctrl Pts',(-10.8146889590001,15.2,1.12835326899999));
#260122=CARTESIAN_POINT('Ctrl Pts',(-10.8174440290001,15.2,1.12776033899999));
#260123=CARTESIAN_POINT('Ctrl Pts',(-10.8202041310001,15.2,1.12716391599998));
#260124=CARTESIAN_POINT('Ctrl Pts',(-10.8229692560001,15.2,1.12656399699999));
#260125=CARTESIAN_POINT('Ctrl Pts',(-10.8257393900001,15.2,1.12596057199998));
#260126=CARTESIAN_POINT('Ctrl Pts',(-10.8285145220001,15.2,1.12535363899998));
#260127=CARTESIAN_POINT('Ctrl Pts',(-10.8312946400001,15.2,1.12474319099999));
#260128=CARTESIAN_POINT('Ctrl Pts',(-10.8340797320001,15.2,1.12412922199999));
#260129=CARTESIAN_POINT('Ctrl Pts',(-10.8368697870001,15.2,1.12351172799999));
#260130=CARTESIAN_POINT('Ctrl Pts',(-10.8396647920001,15.2,1.12289069999999));
#260131=CARTESIAN_POINT('Ctrl Pts',(-10.8424647370001,15.2,1.12226613499999));
#260132=CARTESIAN_POINT('Ctrl Pts',(-10.8452696110001,15.2,1.12163802799999));
#260133=CARTESIAN_POINT('Ctrl Pts',(-10.8480794000001,15.2,1.12100637199998));
#260134=CARTESIAN_POINT('Ctrl Pts',(-10.8508940940001,15.2,1.12037116099998));
#260135=CARTESIAN_POINT('Ctrl Pts',(-10.8537136800001,15.2,1.11973238999999));
#260136=CARTESIAN_POINT('Ctrl Pts',(-10.8565381480001,15.2,1.11909005299998));
#260137=CARTESIAN_POINT('Ctrl Pts',(-10.8593674860001,15.2,1.11844414699998));
#260138=CARTESIAN_POINT('Ctrl Pts',(-10.8622016830001,15.2,1.11779466399998));
#260139=CARTESIAN_POINT('Ctrl Pts',(-10.8650407270001,15.2,1.11714159799998));
#260140=CARTESIAN_POINT('Ctrl Pts',(-10.8678846060001,15.2,1.11648494599998));
#260141=CARTESIAN_POINT('Ctrl Pts',(-10.8707333090001,15.2,1.11582469999998));
#260142=CARTESIAN_POINT('Ctrl Pts',(-10.8735868260001,15.2,1.11516085799999));
#260143=CARTESIAN_POINT('Ctrl Pts',(-10.8764451420001,15.2,1.11449341099998));
#260144=CARTESIAN_POINT('Ctrl Pts',(-10.8793082490001,15.2,1.11382235599998));
#260145=CARTESIAN_POINT('Ctrl Pts',(-10.8821761360001,15.2,1.11314768799998));
#260146=CARTESIAN_POINT('Ctrl Pts',(-10.8850487880001,15.2,1.11246939899999));
#260147=CARTESIAN_POINT('Ctrl Pts',(-10.8879261980001,15.2,1.11178748499999));
#260148=CARTESIAN_POINT('Ctrl Pts',(-10.8908083520001,15.2,1.11110194299998));
#260149=CARTESIAN_POINT('Ctrl Pts',(-10.8936952400001,15.2,1.11041276499999));
#260150=CARTESIAN_POINT('Ctrl Pts',(-10.8965868490001,15.2,1.10971994599999));
#260151=CARTESIAN_POINT('Ctrl Pts',(-10.8994831710001,15.2,1.10902348199998));
#260152=CARTESIAN_POINT('Ctrl Pts',(-10.9023841920001,15.2,1.10832336799998));
#260153=CARTESIAN_POINT('Ctrl Pts',(-10.9052899020001,15.2,1.10761959699999));
#260154=CARTESIAN_POINT('Ctrl Pts',(-10.9082002890001,15.2,1.10691216599998));
#260155=CARTESIAN_POINT('Ctrl Pts',(-10.9111153440001,15.2,1.10620106799999));
#260156=CARTESIAN_POINT('Ctrl Pts',(-10.9140350530001,15.2,1.10548629899998));
#260157=CARTESIAN_POINT('Ctrl Pts',(-10.9169594070001,15.2,1.10476785399999));
#260158=CARTESIAN_POINT('Ctrl Pts',(-10.9198883940001,15.2,1.10404572799998));
#260159=CARTESIAN_POINT('Ctrl Pts',(-10.9228220030001,15.2,1.10331991499999));
#260160=CARTESIAN_POINT('Ctrl Pts',(-10.9257602240001,15.2,1.10259041099999));
#260161=CARTESIAN_POINT('Ctrl Pts',(-10.9287030450001,15.2,1.10185720999999));
#260162=CARTESIAN_POINT('Ctrl Pts',(-10.9316504550001,15.2,1.10112030799999));
#260163=CARTESIAN_POINT('Ctrl Pts',(-10.9346024440001,15.2,1.10037969999999));
#260164=CARTESIAN_POINT('Ctrl Pts',(-10.9375590010001,15.2,1.09963537999999));
#260165=CARTESIAN_POINT('Ctrl Pts',(-10.9405201130001,15.2,1.09888734399998));
#260166=CARTESIAN_POINT('Ctrl Pts',(-10.9434857720001,15.2,1.09813558799999));
#260167=CARTESIAN_POINT('Ctrl Pts',(-10.9464559650001,15.2,1.09738010499999));
#260168=CARTESIAN_POINT('Ctrl Pts',(-10.9494306820001,15.2,1.09662089099999));
#260169=CARTESIAN_POINT('Ctrl Pts',(-10.9524099120001,15.2,1.09585794199999));
#260170=CARTESIAN_POINT('Ctrl Pts',(-10.9553936450001,15.2,1.09509125199999));
#260171=CARTESIAN_POINT('Ctrl Pts',(-10.9583818690001,15.2,1.09432081699998));
#260172=CARTESIAN_POINT('Ctrl Pts',(-10.9613745740001,15.2,1.09354663099999));
#260173=CARTESIAN_POINT('Ctrl Pts',(-10.9643717480001,15.2,1.09276869099999));
#260174=CARTESIAN_POINT('Ctrl Pts',(-10.9673733820001,15.2,1.09198699199998));
#260175=CARTESIAN_POINT('Ctrl Pts',(-10.9703794650001,15.2,1.09120152799999));
#260176=CARTESIAN_POINT('Ctrl Pts',(-10.9733899850001,15.2,1.09041229499999));
#260177=CARTESIAN_POINT('Ctrl Pts',(-10.9764049340001,15.2,1.08961928699999));
#260178=CARTESIAN_POINT('Ctrl Pts',(-10.9794242980001,15.2,1.08882250199999));
#260179=CARTESIAN_POINT('Ctrl Pts',(-10.9824480680001,15.2,1.08802193399999));
#260180=CARTESIAN_POINT('Ctrl Pts',(-10.9854762340001,15.2,1.08721757799998));
#260181=CARTESIAN_POINT('Ctrl Pts',(-10.9885087840001,15.2,1.08640942999998));
#260182=CARTESIAN_POINT('Ctrl Pts',(-10.9915457090001,15.2,1.08559748499998));
#260183=CARTESIAN_POINT('Ctrl Pts',(-10.9945869970001,15.2,1.08478173799998));
#260184=CARTESIAN_POINT('Ctrl Pts',(-10.9976326380001,15.2,1.08396218499998));
#260185=CARTESIAN_POINT('Ctrl Pts',(-11.0006826220001,15.2,1.08313882099999));
#260186=CARTESIAN_POINT('Ctrl Pts',(-11.0037369370001,15.2,1.08231164299998));
#260187=CARTESIAN_POINT('Ctrl Pts',(-11.0067955760001,15.2,1.08148064399999));
#260188=CARTESIAN_POINT('Ctrl Pts',(-11.0098585240001,15.2,1.08064582099999));
#260189=CARTESIAN_POINT('Ctrl Pts',(-11.0129257730001,15.2,1.07980717099998));
#260190=CARTESIAN_POINT('Ctrl Pts',(-11.0159973130001,15.2,1.07896468599999));
#260191=CARTESIAN_POINT('Ctrl Pts',(-11.0190731330001,15.2,1.07811836399998));
#260192=CARTESIAN_POINT('Ctrl Pts',(-11.0221532220001,15.2,1.07726820099999));
#260193=CARTESIAN_POINT('Ctrl Pts',(-11.0252375700001,15.2,1.07641418999998));
#260194=CARTESIAN_POINT('Ctrl Pts',(-11.0283261660001,15.2,1.07555632999999));
#260195=CARTESIAN_POINT('Ctrl Pts',(-11.0314190020001,15.2,1.07469461299999));
#260196=CARTESIAN_POINT('Ctrl Pts',(-11.0345160640001,15.2,1.07382903799999));
#260197=CARTESIAN_POINT('Ctrl Pts',(-11.0376173460001,15.2,1.07295959799998));
#260198=CARTESIAN_POINT('Ctrl Pts',(-11.0407228350001,15.2,1.07208629099999));
#260199=CARTESIAN_POINT('Ctrl Pts',(-11.0438325210001,15.2,1.07120911099999));
#260200=CARTESIAN_POINT('Ctrl Pts',(-11.0469463940001,15.2,1.07032805399998));
#260201=CARTESIAN_POINT('Ctrl Pts',(-11.0500644440001,15.2,1.06944311599999));
#260202=CARTESIAN_POINT('Ctrl Pts',(-11.0531866600001,15.2,1.06855429399999));
#260203=CARTESIAN_POINT('Ctrl Pts',(-11.0563130330001,15.2,1.06766158099999));
#260204=CARTESIAN_POINT('Ctrl Pts',(-11.0594435520001,15.2,1.06676497499999));
#260205=CARTESIAN_POINT('Ctrl Pts',(-11.0625782070001,15.2,1.06586446999998));
#260206=CARTESIAN_POINT('Ctrl Pts',(-11.0657169880001,15.2,1.06496006399999));
#260207=CARTESIAN_POINT('Ctrl Pts',(-11.0688598860001,15.2,1.06405175099999));
#260208=CARTESIAN_POINT('Ctrl Pts',(-11.0720068880001,15.2,1.06313952799999));
#260209=CARTESIAN_POINT('Ctrl Pts',(-11.0751579870001,15.2,1.06222338999999));
#260210=CARTESIAN_POINT('Ctrl Pts',(-11.0783131710001,15.2,1.06130333499999));
#260211=CARTESIAN_POINT('Ctrl Pts',(-11.0814724300001,15.2,1.06037935499999));
#260212=CARTESIAN_POINT('Ctrl Pts',(-11.0846357550001,15.2,1.05945144899998));
#260213=CARTESIAN_POINT('Ctrl Pts',(-11.0878031360001,15.2,1.05851961199999));
#260214=CARTESIAN_POINT('Ctrl Pts',(-11.0909745620001,15.2,1.05758383999999));
#260215=CARTESIAN_POINT('Ctrl Pts',(-11.0941500240001,15.2,1.05664412899999));
#260216=CARTESIAN_POINT('Ctrl Pts',(-11.0973295110001,15.2,1.05570047499999));
#260217=CARTESIAN_POINT('Ctrl Pts',(-11.1005130140001,15.2,1.05475287299999));
#260218=CARTESIAN_POINT('Ctrl Pts',(-11.1037005220001,15.2,1.05380132099999));
#260219=CARTESIAN_POINT('Ctrl Pts',(-11.1068920250001,15.2,1.05284581399999));
#260220=CARTESIAN_POINT('Ctrl Pts',(-11.1100875160001,15.2,1.05188634799998));
#260221=CARTESIAN_POINT('Ctrl Pts',(-11.1132869810001,15.2,1.05092291799998));
#260222=CARTESIAN_POINT('Ctrl Pts',(-11.1164904140001,15.2,1.04995552199998));
#260223=CARTESIAN_POINT('Ctrl Pts',(-11.1196978020001,15.2,1.04898415499999));
#260224=CARTESIAN_POINT('Ctrl Pts',(-11.1229091360001,15.2,1.04800881199999));
#260225=CARTESIAN_POINT('Ctrl Pts',(-11.1261244080001,15.2,1.04702949099998));
#260226=CARTESIAN_POINT('Ctrl Pts',(-11.1293436050001,15.2,1.04604618899999));
#260227=CARTESIAN_POINT('Ctrl Pts',(-11.1325667200001,15.2,1.04505889899999));
#260228=CARTESIAN_POINT('Ctrl Pts',(-11.1357937420001,15.2,1.04406762099998));
#260229=CARTESIAN_POINT('Ctrl Pts',(-11.1390246620001,15.2,1.04307234699998));
#260230=CARTESIAN_POINT('Ctrl Pts',(-11.1422594690001,15.2,1.04207307599999));
#260231=CARTESIAN_POINT('Ctrl Pts',(-11.1454981540001,15.2,1.04106980299999));
#260232=CARTESIAN_POINT('Ctrl Pts',(-11.1487407070001,15.2,1.04006252499998));
#260233=CARTESIAN_POINT('Ctrl Pts',(-11.1519871190001,15.2,1.03905123799999));
#260234=CARTESIAN_POINT('Ctrl Pts',(-11.1552373810001,15.2,1.03803593699999));
#260235=CARTESIAN_POINT('Ctrl Pts',(-11.1584914810001,15.2,1.03701662199999));
#260236=CARTESIAN_POINT('Ctrl Pts',(-11.1617494110001,15.2,1.03599328399998));
#260237=CARTESIAN_POINT('Ctrl Pts',(-11.1650111610001,15.2,1.03496592399999));
#260238=CARTESIAN_POINT('Ctrl Pts',(-11.1682767210001,15.2,1.03393453499999));
#260239=CARTESIAN_POINT('Ctrl Pts',(-11.1715460820001,15.2,1.03289911399999));
#260240=CARTESIAN_POINT('Ctrl Pts',(-11.1748192350001,15.2,1.03185965899999));
#260241=CARTESIAN_POINT('Ctrl Pts',(-11.1780961680001,15.2,1.03081616499999));
#260242=CARTESIAN_POINT('Ctrl Pts',(-11.1813768730001,15.2,1.02976862899999));
#260243=CARTESIAN_POINT('Ctrl Pts',(-11.1846613420001,15.2,1.02871704699998));
#260244=CARTESIAN_POINT('Ctrl Pts',(-11.1879495640001,15.2,1.02766141599998));
#260245=CARTESIAN_POINT('Ctrl Pts',(-11.1912415290001,15.2,1.02660173099999));
#260246=CARTESIAN_POINT('Ctrl Pts',(-11.1945372270001,15.2,1.02553798999999));
#260247=CARTESIAN_POINT('Ctrl Pts',(-11.1978366510001,15.2,1.02447018799999));
#260248=CARTESIAN_POINT('Ctrl Pts',(-11.2011397890001,15.2,1.02339832299998));
#260249=CARTESIAN_POINT('Ctrl Pts',(-11.2044466330001,15.2,1.02232238999999));
#260250=CARTESIAN_POINT('Ctrl Pts',(-11.2077571730001,15.2,1.02124238699998));
#260251=CARTESIAN_POINT('Ctrl Pts',(-11.2110714010001,15.2,1.02015830899999));
#260252=CARTESIAN_POINT('Ctrl Pts',(-11.2143893040001,15.2,1.01907015299998));
#260253=CARTESIAN_POINT('Ctrl Pts',(-11.2177108770001,15.2,1.01797791699999));
#260254=CARTESIAN_POINT('Ctrl Pts',(-11.2210361080001,15.2,1.01688159599998));
#260255=CARTESIAN_POINT('Ctrl Pts',(-11.2243649880001,15.2,1.01578118599999));
#260256=CARTESIAN_POINT('Ctrl Pts',(-11.2276975070001,15.2,1.01467668399998));
#260257=CARTESIAN_POINT('Ctrl Pts',(-11.2310336580001,15.2,1.01356808799999));
#260258=CARTESIAN_POINT('Ctrl Pts',(-11.2343734290001,15.2,1.01245539299998));
#260259=CARTESIAN_POINT('Ctrl Pts',(-11.2377168140001,15.2,1.01133859799999));
#260260=CARTESIAN_POINT('Ctrl Pts',(-11.2410637990001,15.2,1.01021769499999));
#260261=CARTESIAN_POINT('Ctrl Pts',(-11.2444143790001,15.2,1.00909268499999));
#260262=CARTESIAN_POINT('Ctrl Pts',(-11.2477685430001,15.2,1.00796356299998));
#260263=CARTESIAN_POINT('Ctrl Pts',(-11.2511262810001,15.2,1.00683032499999));
#260264=CARTESIAN_POINT('Ctrl Pts',(-11.2544875850001,15.2,1.00569296999999));
#260265=CARTESIAN_POINT('Ctrl Pts',(-11.2578524460001,15.2,1.00455149199998));
#260266=CARTESIAN_POINT('Ctrl Pts',(-11.2612208540001,15.2,1.00340588999998));
#260267=CARTESIAN_POINT('Ctrl Pts',(-11.2645927990001,15.2,1.00225615799999));
#260268=CARTESIAN_POINT('Ctrl Pts',(-11.2679682740001,15.2,1.00110229499998));
#260269=CARTESIAN_POINT('Ctrl Pts',(-11.2713472680001,15.2,0.999944296999988));
#260270=CARTESIAN_POINT('Ctrl Pts',(-11.2747297730001,15.2,0.998782160999987));
#260271=CARTESIAN_POINT('Ctrl Pts',(-11.2781157800001,15.2,0.997615882999985));
#260272=CARTESIAN_POINT('Ctrl Pts',(-11.2815052780001,15.2,0.996445461999986));
#260273=CARTESIAN_POINT('Ctrl Pts',(-11.2848982590001,15.2,0.995270892999987));
#260274=CARTESIAN_POINT('Ctrl Pts',(-11.2882947150001,15.2,0.994092171999985));
#260275=CARTESIAN_POINT('Ctrl Pts',(-11.2916946350001,15.2,0.992909295999986));
#260276=CARTESIAN_POINT('Ctrl Pts',(-11.2950980120001,15.2,0.991722263999986));
#260277=CARTESIAN_POINT('Ctrl Pts',(-11.2985048360001,15.2,0.990531070999987));
#260278=CARTESIAN_POINT('Ctrl Pts',(-11.3019150960001,15.2,0.989335713999986));
#260279=CARTESIAN_POINT('Ctrl Pts',(-11.3053287860001,15.2,0.988136191999986));
#260280=CARTESIAN_POINT('Ctrl Pts',(-11.3087458960001,15.2,0.986932498999984));
#260281=CARTESIAN_POINT('Ctrl Pts',(-11.3121664170001,15.2,0.985724631999982));
#260282=CARTESIAN_POINT('Ctrl Pts',(-11.3155903390001,15.2,0.984512589999986));
#260283=CARTESIAN_POINT('Ctrl Pts',(-11.3190176540001,15.2,0.983296368999986));
#260284=CARTESIAN_POINT('Ctrl Pts',(-11.3224483530001,15.2,0.982075965999982));
#260285=CARTESIAN_POINT('Ctrl Pts',(-11.3258824260001,15.2,0.980851377999983));
#260286=CARTESIAN_POINT('Ctrl Pts',(-11.3293198660001,15.2,0.979622600999988));
#260287=CARTESIAN_POINT('Ctrl Pts',(-11.3327606630001,15.2,0.978389632999987));
#260288=CARTESIAN_POINT('Ctrl Pts',(-11.3362048080001,15.2,0.977152470999982));
#260289=CARTESIAN_POINT('Ctrl Pts',(-11.3396522920001,15.2,0.975911110999985));
#260290=CARTESIAN_POINT('Ctrl Pts',(-11.3431031070001,15.2,0.974665550999987));
#260291=CARTESIAN_POINT('Ctrl Pts',(-11.3465572430001,15.2,0.973415788999983));
#260292=CARTESIAN_POINT('Ctrl Pts',(-11.3500146920001,15.2,0.972161818999986));
#260293=CARTESIAN_POINT('Ctrl Pts',(-11.3534754440001,15.2,0.970903640999987));
#260294=CARTESIAN_POINT('Ctrl Pts',(-11.3569394920001,15.2,0.969641250999986));
#260295=CARTESIAN_POINT('Ctrl Pts',(-11.3604068260001,15.2,0.968374645999983));
#260296=CARTESIAN_POINT('Ctrl Pts',(-11.3638774360001,15.2,0.967103821999986));
#260297=CARTESIAN_POINT('Ctrl Pts',(-11.3673513150001,15.2,0.965828777999986));
#260298=CARTESIAN_POINT('Ctrl Pts',(-11.3708284530001,15.2,0.964549509999983));
#260299=CARTESIAN_POINT('Ctrl Pts',(-11.3743088440001,15.2,0.963266015999986));
#260300=CARTESIAN_POINT('Ctrl Pts',(-11.3777924770001,15.2,0.961978291999985));
#260301=CARTESIAN_POINT('Ctrl Pts',(-11.3812793430001,15.2,0.960686337999985));
#260302=CARTESIAN_POINT('Ctrl Pts',(-11.3847694350001,15.2,0.959390146999985));
#260303=CARTESIAN_POINT('Ctrl Pts',(-11.3882627430001,15.2,0.958089718999986));
#260304=CARTESIAN_POINT('Ctrl Pts',(-11.3917592580001,15.2,0.956785048999986));
#260305=CARTESIAN_POINT('Ctrl Pts',(-11.3952589700001,15.2,0.955476136999986));
#260306=CARTESIAN_POINT('Ctrl Pts',(-11.3987618720001,15.2,0.954162976999986));
#260307=CARTESIAN_POINT('Ctrl Pts',(-11.4022679530001,15.2,0.952845567999985));
#260308=CARTESIAN_POINT('Ctrl Pts',(-11.4057772070001,15.2,0.951523905999987));
#260309=CARTESIAN_POINT('Ctrl Pts',(-11.4092896250001,15.2,0.950197990999988));
#260310=CARTESIAN_POINT('Ctrl Pts',(-11.4128052000001,15.2,0.948867817999983));
#260311=CARTESIAN_POINT('Ctrl Pts',(-11.4163239240001,15.2,0.947533386999986));
#260312=CARTESIAN_POINT('Ctrl Pts',(-11.4198457890001,15.2,0.946194692999986));
#260313=CARTESIAN_POINT('Ctrl Pts',(-11.4233707840001,15.2,0.944851733999985));
#260314=CARTESIAN_POINT('Ctrl Pts',(-11.4268989030001,15.2,0.943504507999986));
#260315=CARTESIAN_POINT('Ctrl Pts',(-11.4304301310001,15.2,0.942153010999984));
#260316=CARTESIAN_POINT('Ctrl Pts',(-11.4339644600001,15.2,0.940797237999984));
#260317=CARTESIAN_POINT('Ctrl Pts',(-11.4375018800001,15.2,0.939437186999985));
#260318=CARTESIAN_POINT('Ctrl Pts',(-11.4410423790001,15.2,0.938072855999987));
#260319=CARTESIAN_POINT('Ctrl Pts',(-11.4445859520001,15.2,0.936704240999986));
#260320=CARTESIAN_POINT('Ctrl Pts',(-11.4481325920001,15.2,0.935331340999985));
#260321=CARTESIAN_POINT('Ctrl Pts',(-11.4516822960001,15.2,0.933954156999985));
#260322=CARTESIAN_POINT('Ctrl Pts',(-11.4552350600001,15.2,0.932572684999986));
#260323=CARTESIAN_POINT('Ctrl Pts',(-11.4580797200001,15.2,0.931464077999986));
#260324=CARTESIAN_POINT('Ctrl Pts',(-11.4602145910001,15.2,0.930630692999985));
#260325=CARTESIAN_POINT('Ctrl Pts',(-11.4616384500001,15.2,0.930074245999983));
#260326=CARTESIAN_POINT('Ctrl Pts',(-11.4623505340001,15.2,0.929795807999985));
#260327=CARTESIAN_POINT('Ctrl Pts',(-10.3068855240001,12.2,1.18690176599999));
#260328=CARTESIAN_POINT('Ctrl Pts',(-10.3070598110001,12.2,1.18690675299999));
#260329=CARTESIAN_POINT('Ctrl Pts',(-10.3074144740001,12.2,1.18691681599998));
#260330=CARTESIAN_POINT('Ctrl Pts',(-10.3079518800001,12.2,1.18693179799998));
#260331=CARTESIAN_POINT('Ctrl Pts',(-10.3086758300001,12.2,1.18695143999998));
#260332=CARTESIAN_POINT('Ctrl Pts',(-10.3095915440001,12.2,1.18697537099999));
#260333=CARTESIAN_POINT('Ctrl Pts',(-10.3105221240001,12.2,1.18699875499999));
#260334=CARTESIAN_POINT('Ctrl Pts',(-10.3114622390001,12.2,1.18702143499998));
#260335=CARTESIAN_POINT('Ctrl Pts',(-10.3124118610001,12.2,1.18704339399998));
#260336=CARTESIAN_POINT('Ctrl Pts',(-10.3133709660001,12.2,1.18706460899999));
#260337=CARTESIAN_POINT('Ctrl Pts',(-10.3143395250001,12.2,1.18708506599999));
#260338=CARTESIAN_POINT('Ctrl Pts',(-10.3153175130001,12.2,1.18710474299998));
#260339=CARTESIAN_POINT('Ctrl Pts',(-10.3163049050001,12.2,1.18712362399998));
#260340=CARTESIAN_POINT('Ctrl Pts',(-10.3173016730001,12.2,1.18714168899999));
#260341=CARTESIAN_POINT('Ctrl Pts',(-10.3183077930001,12.2,1.18715892099999));
#260342=CARTESIAN_POINT('Ctrl Pts',(-10.3193232400001,12.2,1.18717530199998));
#260343=CARTESIAN_POINT('Ctrl Pts',(-10.3203479850001,12.2,1.18719081299998));
#260344=CARTESIAN_POINT('Ctrl Pts',(-10.3213820050001,12.2,1.18720543699999));
#260345=CARTESIAN_POINT('Ctrl Pts',(-10.3224252740001,12.2,1.18721915599998));
#260346=CARTESIAN_POINT('Ctrl Pts',(-10.3234777680001,12.2,1.18723195099999));
#260347=CARTESIAN_POINT('Ctrl Pts',(-10.3245394590001,12.2,1.18724380599998));
#260348=CARTESIAN_POINT('Ctrl Pts',(-10.3256103250001,12.2,1.18725470399998));
#260349=CARTESIAN_POINT('Ctrl Pts',(-10.3266903400001,12.2,1.18726462499998));
#260350=CARTESIAN_POINT('Ctrl Pts',(-10.3277794780001,12.2,1.18727355499999));
#260351=CARTESIAN_POINT('Ctrl Pts',(-10.3288777160001,12.2,1.18728147399999));
#260352=CARTESIAN_POINT('Ctrl Pts',(-10.3299850290001,12.2,1.18728836599999));
#260353=CARTESIAN_POINT('Ctrl Pts',(-10.3311013920001,12.2,1.18729421399999));
#260354=CARTESIAN_POINT('Ctrl Pts',(-10.3322267810001,12.2,1.18729900199999));
#260355=CARTESIAN_POINT('Ctrl Pts',(-10.3333611710001,12.2,1.18730271099999));
#260356=CARTESIAN_POINT('Ctrl Pts',(-10.3345045400001,12.2,1.18730532599999));
#260357=CARTESIAN_POINT('Ctrl Pts',(-10.3356568620001,12.2,1.18730682999999));
#260358=CARTESIAN_POINT('Ctrl Pts',(-10.3368181130001,12.2,1.18730720599999));
#260359=CARTESIAN_POINT('Ctrl Pts',(-10.3379882700001,12.2,1.18730643699998));
#260360=CARTESIAN_POINT('Ctrl Pts',(-10.3391673090001,12.2,1.18730450799998));
#260361=CARTESIAN_POINT('Ctrl Pts',(-10.3403552060001,12.2,1.18730140199999));
#260362=CARTESIAN_POINT('Ctrl Pts',(-10.3415519380001,12.2,1.18729710199998));
#260363=CARTESIAN_POINT('Ctrl Pts',(-10.3427574820001,12.2,1.18729159399999));
#260364=CARTESIAN_POINT('Ctrl Pts',(-10.3439718130001,12.2,1.18728485899998));
#260365=CARTESIAN_POINT('Ctrl Pts',(-10.3451949090001,12.2,1.18727688299999));
#260366=CARTESIAN_POINT('Ctrl Pts',(-10.3464267470001,12.2,1.18726764999999));
#260367=CARTESIAN_POINT('Ctrl Pts',(-10.3476673040001,12.2,1.18725714299998));
#260368=CARTESIAN_POINT('Ctrl Pts',(-10.3489165560001,12.2,1.18724534699998));
#260369=CARTESIAN_POINT('Ctrl Pts',(-10.3501744810001,12.2,1.18723224699998));
#260370=CARTESIAN_POINT('Ctrl Pts',(-10.3514410560001,12.2,1.18721782799998));
#260371=CARTESIAN_POINT('Ctrl Pts',(-10.3527162580001,12.2,1.18720207199999));
#260372=CARTESIAN_POINT('Ctrl Pts',(-10.3540000650001,12.2,1.18718496499998));
#260373=CARTESIAN_POINT('Ctrl Pts',(-10.3552924550001,12.2,1.18716649199999));
#260374=CARTESIAN_POINT('Ctrl Pts',(-10.3565934040001,12.2,1.18714663699999));
#260375=CARTESIAN_POINT('Ctrl Pts',(-10.3579028900001,12.2,1.18712538499999));
#260376=CARTESIAN_POINT('Ctrl Pts',(-10.3592208920001,12.2,1.18710272199999));
#260377=CARTESIAN_POINT('Ctrl Pts',(-10.3605473870001,12.2,1.18707863099999));
#260378=CARTESIAN_POINT('Ctrl Pts',(-10.3618823540001,12.2,1.18705309899998));
#260379=CARTESIAN_POINT('Ctrl Pts',(-10.3632257690001,12.2,1.18702610999998));
#260380=CARTESIAN_POINT('Ctrl Pts',(-10.3645776120001,12.2,1.18699765099999));
#260381=CARTESIAN_POINT('Ctrl Pts',(-10.3659378610001,12.2,1.18696770399998));
#260382=CARTESIAN_POINT('Ctrl Pts',(-10.3673064940001,12.2,1.18693625599999));
#260383=CARTESIAN_POINT('Ctrl Pts',(-10.3686834880001,12.2,1.18690329399998));
#260384=CARTESIAN_POINT('Ctrl Pts',(-10.3700688240001,12.2,1.18686880099999));
#260385=CARTESIAN_POINT('Ctrl Pts',(-10.3714624790001,12.2,1.18683276399999));
#260386=CARTESIAN_POINT('Ctrl Pts',(-10.3728644310001,12.2,1.18679516799999));
#260387=CARTESIAN_POINT('Ctrl Pts',(-10.3742746610001,12.2,1.18675599899999));
#260388=CARTESIAN_POINT('Ctrl Pts',(-10.3756931460001,12.2,1.18671524399999));
#260389=CARTESIAN_POINT('Ctrl Pts',(-10.3771198660001,12.2,1.18667288599998));
#260390=CARTESIAN_POINT('Ctrl Pts',(-10.3785547980001,12.2,1.18662891399998));
#260391=CARTESIAN_POINT('Ctrl Pts',(-10.3799979240001,12.2,1.18658331299998));
#260392=CARTESIAN_POINT('Ctrl Pts',(-10.3814492210001,12.2,1.18653606699999));
#260393=CARTESIAN_POINT('Ctrl Pts',(-10.3829086680001,12.2,1.18648716499999));
#260394=CARTESIAN_POINT('Ctrl Pts',(-10.3843762450001,12.2,1.18643659199998));
#260395=CARTESIAN_POINT('Ctrl Pts',(-10.3858519330001,12.2,1.18638433399999));
#260396=CARTESIAN_POINT('Ctrl Pts',(-10.3873357080001,12.2,1.18633037799999));
#260397=CARTESIAN_POINT('Ctrl Pts',(-10.3888275530001,12.2,1.18627470999999));
#260398=CARTESIAN_POINT('Ctrl Pts',(-10.3903274450001,12.2,1.18621731599998));
#260399=CARTESIAN_POINT('Ctrl Pts',(-10.3918353650001,12.2,1.18615818399999));
#260400=CARTESIAN_POINT('Ctrl Pts',(-10.3933512920001,12.2,1.18609729999998));
#260401=CARTESIAN_POINT('Ctrl Pts',(-10.3948752070001,12.2,1.18603464899998));
#260402=CARTESIAN_POINT('Ctrl Pts',(-10.3964070880001,12.2,1.18597021999999));
#260403=CARTESIAN_POINT('Ctrl Pts',(-10.3979469170001,12.2,1.18590399899999));
#260404=CARTESIAN_POINT('Ctrl Pts',(-10.3994946730001,12.2,1.18583597199999));
#260405=CARTESIAN_POINT('Ctrl Pts',(-10.4010503360001,12.2,1.18576612699998));
#260406=CARTESIAN_POINT('Ctrl Pts',(-10.4026138870001,12.2,1.18569445199999));
#260407=CARTESIAN_POINT('Ctrl Pts',(-10.4041853050001,12.2,1.18562093199999));
#260408=CARTESIAN_POINT('Ctrl Pts',(-10.4057645710001,12.2,1.18554555499998));
#260409=CARTESIAN_POINT('Ctrl Pts',(-10.4073516650001,12.2,1.18546830799998));
#260410=CARTESIAN_POINT('Ctrl Pts',(-10.4089465690001,12.2,1.18538917799999));
#260411=CARTESIAN_POINT('Ctrl Pts',(-10.4105492620001,12.2,1.18530815299998));
#260412=CARTESIAN_POINT('Ctrl Pts',(-10.4121597240001,12.2,1.18522521999999));
#260413=CARTESIAN_POINT('Ctrl Pts',(-10.4137779370001,12.2,1.18514036599999));
#260414=CARTESIAN_POINT('Ctrl Pts',(-10.4154038820001,12.2,1.18505357999998));
#260415=CARTESIAN_POINT('Ctrl Pts',(-10.4170375390001,12.2,1.18496484799998));
#260416=CARTESIAN_POINT('Ctrl Pts',(-10.4186788900001,12.2,1.18487415599999));
#260417=CARTESIAN_POINT('Ctrl Pts',(-10.4203279130001,12.2,1.18478149699999));
#260418=CARTESIAN_POINT('Ctrl Pts',(-10.4219845930001,12.2,1.18468685399999));
#260419=CARTESIAN_POINT('Ctrl Pts',(-10.4236489080001,12.2,1.18459021499998));
#260420=CARTESIAN_POINT('Ctrl Pts',(-10.4253208410001,12.2,1.18449156999999));
#260421=CARTESIAN_POINT('Ctrl Pts',(-10.4270003720001,12.2,1.18439090599999));
#260422=CARTESIAN_POINT('Ctrl Pts',(-10.4286874830001,12.2,1.18428821199998));
#260423=CARTESIAN_POINT('Ctrl Pts',(-10.4303821540001,12.2,1.18418347399999));
#260424=CARTESIAN_POINT('Ctrl Pts',(-10.4320843690001,12.2,1.18407667999998));
#260425=CARTESIAN_POINT('Ctrl Pts',(-10.4337941070001,12.2,1.18396781999999));
#260426=CARTESIAN_POINT('Ctrl Pts',(-10.4355113520001,12.2,1.18385688099998));
#260427=CARTESIAN_POINT('Ctrl Pts',(-10.4372360820001,12.2,1.18374385099999));
#260428=CARTESIAN_POINT('Ctrl Pts',(-10.4389682810001,12.2,1.18362871999999));
#260429=CARTESIAN_POINT('Ctrl Pts',(-10.4407079310001,12.2,1.18351147399999));
#260430=CARTESIAN_POINT('Ctrl Pts',(-10.4424550130001,12.2,1.18339210299998));
#260431=CARTESIAN_POINT('Ctrl Pts',(-10.4442095090001,12.2,1.18327059399999));
#260432=CARTESIAN_POINT('Ctrl Pts',(-10.4459714000001,12.2,1.18314693699999));
#260433=CARTESIAN_POINT('Ctrl Pts',(-10.4477406700001,12.2,1.18302111899999));
#260434=CARTESIAN_POINT('Ctrl Pts',(-10.4495173000001,12.2,1.18289313099998));
#260435=CARTESIAN_POINT('Ctrl Pts',(-10.4513012710001,12.2,1.18276295899999));
#260436=CARTESIAN_POINT('Ctrl Pts',(-10.4530925660001,12.2,1.18263059399998));
#260437=CARTESIAN_POINT('Ctrl Pts',(-10.4548911670001,12.2,1.18249602199999));
#260438=CARTESIAN_POINT('Ctrl Pts',(-10.4566970570001,12.2,1.18235923399999));
#260439=CARTESIAN_POINT('Ctrl Pts',(-10.4585102170001,12.2,1.18222021899999));
#260440=CARTESIAN_POINT('Ctrl Pts',(-10.4603306310001,12.2,1.18207896399999));
#260441=CARTESIAN_POINT('Ctrl Pts',(-10.4621582800001,12.2,1.18193545999999));
#260442=CARTESIAN_POINT('Ctrl Pts',(-10.4639931470001,12.2,1.18178969599999));
#260443=CARTESIAN_POINT('Ctrl Pts',(-10.4658352150001,12.2,1.18164165899998));
#260444=CARTESIAN_POINT('Ctrl Pts',(-10.4676844650001,12.2,1.18149133999998));
#260445=CARTESIAN_POINT('Ctrl Pts',(-10.4695408810001,12.2,1.18133872599998));
#260446=CARTESIAN_POINT('Ctrl Pts',(-10.4714044460001,12.2,1.18118380899999));
#260447=CARTESIAN_POINT('Ctrl Pts',(-10.4732751410001,12.2,1.18102657599998));
#260448=CARTESIAN_POINT('Ctrl Pts',(-10.4751529500001,12.2,1.18086701799998));
#260449=CARTESIAN_POINT('Ctrl Pts',(-10.4770378570001,12.2,1.18070512399999));
#260450=CARTESIAN_POINT('Ctrl Pts',(-10.4789298430001,12.2,1.18054088199999));
#260451=CARTESIAN_POINT('Ctrl Pts',(-10.4808288920001,12.2,1.18037428299999));
#260452=CARTESIAN_POINT('Ctrl Pts',(-10.4827349850001,12.2,1.18020531599999));
#260453=CARTESIAN_POINT('Ctrl Pts',(-10.4846481080001,12.2,1.18003396999999));
#260454=CARTESIAN_POINT('Ctrl Pts',(-10.4865682440001,12.2,1.17986023499999));
#260455=CARTESIAN_POINT('Ctrl Pts',(-10.4884953720001,12.2,1.17968410099999));
#260456=CARTESIAN_POINT('Ctrl Pts',(-10.4904294800001,12.2,1.17950555699998));
#260457=CARTESIAN_POINT('Ctrl Pts',(-10.4923705490001,12.2,1.17932459399999));
#260458=CARTESIAN_POINT('Ctrl Pts',(-10.4943185630001,12.2,1.17914119999998));
#260459=CARTESIAN_POINT('Ctrl Pts',(-10.4962735060001,12.2,1.17895536499999));
#260460=CARTESIAN_POINT('Ctrl Pts',(-10.4982353590001,12.2,1.17876708099999));
#260461=CARTESIAN_POINT('Ctrl Pts',(-10.5002041080001,12.2,1.17857633499999));
#260462=CARTESIAN_POINT('Ctrl Pts',(-10.5021797350001,12.2,1.17838311899999));
#260463=CARTESIAN_POINT('Ctrl Pts',(-10.5041622250001,12.2,1.17818742199999));
#260464=CARTESIAN_POINT('Ctrl Pts',(-10.5061515600001,12.2,1.17798923599999));
#260465=CARTESIAN_POINT('Ctrl Pts',(-10.5081477230001,12.2,1.17778854799999));
#260466=CARTESIAN_POINT('Ctrl Pts',(-10.5101507010001,12.2,1.17758534999998));
#260467=CARTESIAN_POINT('Ctrl Pts',(-10.5121604750001,12.2,1.17737963099998));
#260468=CARTESIAN_POINT('Ctrl Pts',(-10.5141770310001,12.2,1.17717138199998));
#260469=CARTESIAN_POINT('Ctrl Pts',(-10.5162003510001,12.2,1.17696059399998));
#260470=CARTESIAN_POINT('Ctrl Pts',(-10.5182304190001,12.2,1.17674725699999));
#260471=CARTESIAN_POINT('Ctrl Pts',(-10.5202672190001,12.2,1.17653135999999));
#260472=CARTESIAN_POINT('Ctrl Pts',(-10.5223107360001,12.2,1.17631289399998));
#260473=CARTESIAN_POINT('Ctrl Pts',(-10.5243609530001,12.2,1.17609184999999));
#260474=CARTESIAN_POINT('Ctrl Pts',(-10.5264178550001,12.2,1.17586821899998));
#260475=CARTESIAN_POINT('Ctrl Pts',(-10.5284814260001,12.2,1.17564198999998));
#260476=CARTESIAN_POINT('Ctrl Pts',(-10.5305516490001,12.2,1.17541315299999));
#260477=CARTESIAN_POINT('Ctrl Pts',(-10.5326285090001,12.2,1.17518170099999));
#260478=CARTESIAN_POINT('Ctrl Pts',(-10.5347119910001,12.2,1.17494762299998));
#260479=CARTESIAN_POINT('Ctrl Pts',(-10.5368020780001,12.2,1.17471090999999));
#260480=CARTESIAN_POINT('Ctrl Pts',(-10.5388987570001,12.2,1.17447155299998));
#260481=CARTESIAN_POINT('Ctrl Pts',(-10.5410020080001,12.2,1.17422954199998));
#260482=CARTESIAN_POINT('Ctrl Pts',(-10.5431118190001,12.2,1.17398486899999));
#260483=CARTESIAN_POINT('Ctrl Pts',(-10.5452281730001,12.2,1.17373752299998));
#260484=CARTESIAN_POINT('Ctrl Pts',(-10.5473510550001,12.2,1.17348749699998));
#260485=CARTESIAN_POINT('Ctrl Pts',(-10.5494804500001,12.2,1.17323477999999));
#260486=CARTESIAN_POINT('Ctrl Pts',(-10.5516163410001,12.2,1.17297936399999));
#260487=CARTESIAN_POINT('Ctrl Pts',(-10.5537587150001,12.2,1.17272124099999));
#260488=CARTESIAN_POINT('Ctrl Pts',(-10.5559075550001,12.2,1.17246039999999));
#260489=CARTESIAN_POINT('Ctrl Pts',(-10.5580628460001,12.2,1.17219683299998));
#260490=CARTESIAN_POINT('Ctrl Pts',(-10.5602245730001,12.2,1.17193052999998));
#260491=CARTESIAN_POINT('Ctrl Pts',(-10.5623927210001,12.2,1.17166148499999));
#260492=CARTESIAN_POINT('Ctrl Pts',(-10.5645672750001,12.2,1.17138968599999));
#260493=CARTESIAN_POINT('Ctrl Pts',(-10.5667482200001,12.2,1.17111512499998));
#260494=CARTESIAN_POINT('Ctrl Pts',(-10.5689355400001,12.2,1.17083779399998));
#260495=CARTESIAN_POINT('Ctrl Pts',(-10.5711292210001,12.2,1.17055768399998));
#260496=CARTESIAN_POINT('Ctrl Pts',(-10.5733292470001,12.2,1.17027478699999));
#260497=CARTESIAN_POINT('Ctrl Pts',(-10.5755356040001,12.2,1.16998909399999));
#260498=CARTESIAN_POINT('Ctrl Pts',(-10.5777482770001,12.2,1.16970059599999));
#260499=CARTESIAN_POINT('Ctrl Pts',(-10.5799672510001,12.2,1.16940928399998));
#260500=CARTESIAN_POINT('Ctrl Pts',(-10.5821925120001,12.2,1.16911514999999));
#260501=CARTESIAN_POINT('Ctrl Pts',(-10.5844240430001,12.2,1.16881818499999));
#260502=CARTESIAN_POINT('Ctrl Pts',(-10.5866618310001,12.2,1.16851838199999));
#260503=CARTESIAN_POINT('Ctrl Pts',(-10.5889058620001,12.2,1.16821573099998));
#260504=CARTESIAN_POINT('Ctrl Pts',(-10.5911561200001,12.2,1.16791022399998));
#260505=CARTESIAN_POINT('Ctrl Pts',(-10.5934125910001,12.2,1.16760185399999));
#260506=CARTESIAN_POINT('Ctrl Pts',(-10.5956752600001,12.2,1.16729060999999));
#260507=CARTESIAN_POINT('Ctrl Pts',(-10.5979441110001,12.2,1.16697648599999));
#260508=CARTESIAN_POINT('Ctrl Pts',(-10.6002191330001,12.2,1.16665947299999));
#260509=CARTESIAN_POINT('Ctrl Pts',(-10.6025003100001,12.2,1.16633956299999));
#260510=CARTESIAN_POINT('Ctrl Pts',(-10.6047876270001,12.2,1.16601674699998));
#260511=CARTESIAN_POINT('Ctrl Pts',(-10.6070810700001,12.2,1.16569101799998));
#260512=CARTESIAN_POINT('Ctrl Pts',(-10.6093806240001,12.2,1.16536236699998));
#260513=CARTESIAN_POINT('Ctrl Pts',(-10.6116862760001,12.2,1.16503078599999));
#260514=CARTESIAN_POINT('Ctrl Pts',(-10.6139980110001,12.2,1.16469626699998));
#260515=CARTESIAN_POINT('Ctrl Pts',(-10.6163158140001,12.2,1.16435880299999));
#260516=CARTESIAN_POINT('Ctrl Pts',(-10.6186396720001,12.2,1.16401838499999));
#260517=CARTESIAN_POINT('Ctrl Pts',(-10.6209695720001,12.2,1.16367500499999));
#260518=CARTESIAN_POINT('Ctrl Pts',(-10.6233054970001,12.2,1.16332865499999));
#260519=CARTESIAN_POINT('Ctrl Pts',(-10.6256474340001,12.2,1.16297932799998));
#260520=CARTESIAN_POINT('Ctrl Pts',(-10.6279953690001,12.2,1.16262701499998));
#260521=CARTESIAN_POINT('Ctrl Pts',(-10.6303492890001,12.2,1.16227170999998));
#260522=CARTESIAN_POINT('Ctrl Pts',(-10.6327091780001,12.2,1.16191340299999));
#260523=CARTESIAN_POINT('Ctrl Pts',(-10.6350750250001,12.2,1.16155208699999));
#260524=CARTESIAN_POINT('Ctrl Pts',(-10.6374468130001,12.2,1.16118775499999));
#260525=CARTESIAN_POINT('Ctrl Pts',(-10.6398245300001,12.2,1.16082039899998));
#260526=CARTESIAN_POINT('Ctrl Pts',(-10.6422081610001,12.2,1.16045001099998));
#260527=CARTESIAN_POINT('Ctrl Pts',(-10.6445976930001,12.2,1.16007658299999));
#260528=CARTESIAN_POINT('Ctrl Pts',(-10.6469931120001,12.2,1.15970010799999));
#260529=CARTESIAN_POINT('Ctrl Pts',(-10.6493944050001,12.2,1.15932057999999));
#260530=CARTESIAN_POINT('Ctrl Pts',(-10.6518015570001,12.2,1.15893798799998));
#260531=CARTESIAN_POINT('Ctrl Pts',(-10.6542145550001,12.2,1.15855232699999));
#260532=CARTESIAN_POINT('Ctrl Pts',(-10.6566333850001,12.2,1.15816358799998));
#260533=CARTESIAN_POINT('Ctrl Pts',(-10.6590580340001,12.2,1.15777176599998));
#260534=CARTESIAN_POINT('Ctrl Pts',(-10.6614884880001,12.2,1.15737684999999));
#260535=CARTESIAN_POINT('Ctrl Pts',(-10.6639247340001,12.2,1.15697883699998));
#260536=CARTESIAN_POINT('Ctrl Pts',(-10.6663667570001,12.2,1.15657771499999));
#260537=CARTESIAN_POINT('Ctrl Pts',(-10.6688145450001,12.2,1.15617348099998));
#260538=CARTESIAN_POINT('Ctrl Pts',(-10.6712680840001,12.2,1.15576612499999));
#260539=CARTESIAN_POINT('Ctrl Pts',(-10.6737273610001,12.2,1.15535563899998));
#260540=CARTESIAN_POINT('Ctrl Pts',(-10.6761923620001,12.2,1.15494201899998));
#260541=CARTESIAN_POINT('Ctrl Pts',(-10.6786630740001,12.2,1.15452525499999));
#260542=CARTESIAN_POINT('Ctrl Pts',(-10.6811394830001,12.2,1.15410534099999));
#260543=CARTESIAN_POINT('Ctrl Pts',(-10.6836215780001,12.2,1.15368226999998));
#260544=CARTESIAN_POINT('Ctrl Pts',(-10.6861093440001,12.2,1.15325603399999));
#260545=CARTESIAN_POINT('Ctrl Pts',(-10.6886027670001,12.2,1.15282662699999));
#260546=CARTESIAN_POINT('Ctrl Pts',(-10.6911018330001,12.2,1.15239403999999));
#260547=CARTESIAN_POINT('Ctrl Pts',(-10.6936065330001,12.2,1.15195826999999));
#260548=CARTESIAN_POINT('Ctrl Pts',(-10.6961168510001,12.2,1.15151930499998));
#260549=CARTESIAN_POINT('Ctrl Pts',(-10.6986327730001,12.2,1.15107714099999));
#260550=CARTESIAN_POINT('Ctrl Pts',(-10.7011542890001,12.2,1.15063176999998));
#260551=CARTESIAN_POINT('Ctrl Pts',(-10.7036813830001,12.2,1.15018318599999));
#260552=CARTESIAN_POINT('Ctrl Pts',(-10.7062140430001,12.2,1.14973138199999));
#260553=CARTESIAN_POINT('Ctrl Pts',(-10.7087522570001,12.2,1.14927634999999));
#260554=CARTESIAN_POINT('Ctrl Pts',(-10.7112960120001,12.2,1.14881808499999));
#260555=CARTESIAN_POINT('Ctrl Pts',(-10.7138452930001,12.2,1.14835657899999));
#260556=CARTESIAN_POINT('Ctrl Pts',(-10.7164000880001,12.2,1.14789182399999));
#260557=CARTESIAN_POINT('Ctrl Pts',(-10.7189603860001,12.2,1.14742381499998));
#260558=CARTESIAN_POINT('Ctrl Pts',(-10.7215261720001,12.2,1.14695254599999));
#260559=CARTESIAN_POINT('Ctrl Pts',(-10.7240974330001,12.2,1.14647800799998));
#260560=CARTESIAN_POINT('Ctrl Pts',(-10.7266741590001,12.2,1.14600019699999));
#260561=CARTESIAN_POINT('Ctrl Pts',(-10.7292563340001,12.2,1.14551910299999));
#260562=CARTESIAN_POINT('Ctrl Pts',(-10.7318439480001,12.2,1.14503472299999));
#260563=CARTESIAN_POINT('Ctrl Pts',(-10.734955593487,12.2,1.14444951182125));
#260564=CARTESIAN_POINT('Ctrl Pts',(-10.7380753572566,12.2,1.14385935058935));
#260565=CARTESIAN_POINT('Ctrl Pts',(-10.7412032147435,12.2,1.14326422341062));
#260566=CARTESIAN_POINT('Ctrl Pts',(-10.7443391425131,12.2,1.1426641201787));
#260567=CARTESIAN_POINT('Ctrl Pts',(-10.7474831100001,12.2,1.14205902499998));
#260568=CARTESIAN_POINT('Ctrl Pts',(-10.7501084340001,12.2,1.14155144699998));
#260569=CARTESIAN_POINT('Ctrl Pts',(-10.7527390940001,12.2,1.14104052899998));
#260570=CARTESIAN_POINT('Ctrl Pts',(-10.7553750790001,12.2,1.14052626499999));
#260571=CARTESIAN_POINT('Ctrl Pts',(-10.7580163760001,12.2,1.14000864899999));
#260572=CARTESIAN_POINT('Ctrl Pts',(-10.7606629730001,12.2,1.13948767199998));
#260573=CARTESIAN_POINT('Ctrl Pts',(-10.7633148570001,12.2,1.13896333199999));
#260574=CARTESIAN_POINT('Ctrl Pts',(-10.7659720160001,12.2,1.13843561899999));
#260575=CARTESIAN_POINT('Ctrl Pts',(-10.7686344370001,12.2,1.13790452999998));
#260576=CARTESIAN_POINT('Ctrl Pts',(-10.7713021080001,12.2,1.13737005599999));
#260577=CARTESIAN_POINT('Ctrl Pts',(-10.7739750180001,12.2,1.13683219199999));
#260578=CARTESIAN_POINT('Ctrl Pts',(-10.7766531540001,12.2,1.13629093099998));
#260579=CARTESIAN_POINT('Ctrl Pts',(-10.7793365030001,12.2,1.13574626899998));
#260580=CARTESIAN_POINT('Ctrl Pts',(-10.7820250540001,12.2,1.13519819699999));
#260581=CARTESIAN_POINT('Ctrl Pts',(-10.7847187940001,12.2,1.13464671099999));
#260582=CARTESIAN_POINT('Ctrl Pts',(-10.7874177100001,12.2,1.13409180499998));
#260583=CARTESIAN_POINT('Ctrl Pts',(-10.7901217920001,12.2,1.13353347099999));
#260584=CARTESIAN_POINT('Ctrl Pts',(-10.7928310260001,12.2,1.13297170399999));
#260585=CARTESIAN_POINT('Ctrl Pts',(-10.7955454010001,12.2,1.13240649799998));
#260586=CARTESIAN_POINT('Ctrl Pts',(-10.7982649040001,12.2,1.13183784699999));
#260587=CARTESIAN_POINT('Ctrl Pts',(-10.8009895250001,12.2,1.13126574599999));
#260588=CARTESIAN_POINT('Ctrl Pts',(-10.8037192500001,12.2,1.13069018799999));
#260589=CARTESIAN_POINT('Ctrl Pts',(-10.8064540680001,12.2,1.13011116799999));
#260590=CARTESIAN_POINT('Ctrl Pts',(-10.8091939670001,12.2,1.12952867799998));
#260591=CARTESIAN_POINT('Ctrl Pts',(-10.8119389340001,12.2,1.12894271399998));
#260592=CARTESIAN_POINT('Ctrl Pts',(-10.8146889590001,12.2,1.12835326899999));
#260593=CARTESIAN_POINT('Ctrl Pts',(-10.8174440290001,12.2,1.12776033899999));
#260594=CARTESIAN_POINT('Ctrl Pts',(-10.8202041310001,12.2,1.12716391599998));
#260595=CARTESIAN_POINT('Ctrl Pts',(-10.8229692560001,12.2,1.12656399699999));
#260596=CARTESIAN_POINT('Ctrl Pts',(-10.8257393900001,12.2,1.12596057199998));
#260597=CARTESIAN_POINT('Ctrl Pts',(-10.8285145220001,12.2,1.12535363899998));
#260598=CARTESIAN_POINT('Ctrl Pts',(-10.8312946400001,12.2,1.12474319099999));
#260599=CARTESIAN_POINT('Ctrl Pts',(-10.8340797320001,12.2,1.12412922199999));
#260600=CARTESIAN_POINT('Ctrl Pts',(-10.8368697870001,12.2,1.12351172799999));
#260601=CARTESIAN_POINT('Ctrl Pts',(-10.8396647920001,12.2,1.12289069999999));
#260602=CARTESIAN_POINT('Ctrl Pts',(-10.8424647370001,12.2,1.12226613499999));
#260603=CARTESIAN_POINT('Ctrl Pts',(-10.8452696110001,12.2,1.12163802799999));
#260604=CARTESIAN_POINT('Ctrl Pts',(-10.8480794000001,12.2,1.12100637199998));
#260605=CARTESIAN_POINT('Ctrl Pts',(-10.8508940940001,12.2,1.12037116099998));
#260606=CARTESIAN_POINT('Ctrl Pts',(-10.8537136800001,12.2,1.11973238999999));
#260607=CARTESIAN_POINT('Ctrl Pts',(-10.8565381480001,12.2,1.11909005299998));
#260608=CARTESIAN_POINT('Ctrl Pts',(-10.8593674860001,12.2,1.11844414699998));
#260609=CARTESIAN_POINT('Ctrl Pts',(-10.8622016830001,12.2,1.11779466399998));
#260610=CARTESIAN_POINT('Ctrl Pts',(-10.8650407270001,12.2,1.11714159799998));
#260611=CARTESIAN_POINT('Ctrl Pts',(-10.8678846060001,12.2,1.11648494599998));
#260612=CARTESIAN_POINT('Ctrl Pts',(-10.8707333090001,12.2,1.11582469999998));
#260613=CARTESIAN_POINT('Ctrl Pts',(-10.8735868260001,12.2,1.11516085799999));
#260614=CARTESIAN_POINT('Ctrl Pts',(-10.8764451420001,12.2,1.11449341099998));
#260615=CARTESIAN_POINT('Ctrl Pts',(-10.8793082490001,12.2,1.11382235599998));
#260616=CARTESIAN_POINT('Ctrl Pts',(-10.8821761360001,12.2,1.11314768799998));
#260617=CARTESIAN_POINT('Ctrl Pts',(-10.8850487880001,12.2,1.11246939899999));
#260618=CARTESIAN_POINT('Ctrl Pts',(-10.8879261980001,12.2,1.11178748499999));
#260619=CARTESIAN_POINT('Ctrl Pts',(-10.8908083520001,12.2,1.11110194299998));
#260620=CARTESIAN_POINT('Ctrl Pts',(-10.8936952400001,12.2,1.11041276499999));
#260621=CARTESIAN_POINT('Ctrl Pts',(-10.8965868490001,12.2,1.10971994599999));
#260622=CARTESIAN_POINT('Ctrl Pts',(-10.8994831710001,12.2,1.10902348199998));
#260623=CARTESIAN_POINT('Ctrl Pts',(-10.9023841920001,12.2,1.10832336799998));
#260624=CARTESIAN_POINT('Ctrl Pts',(-10.9052899020001,12.2,1.10761959699999));
#260625=CARTESIAN_POINT('Ctrl Pts',(-10.9082002890001,12.2,1.10691216599998));
#260626=CARTESIAN_POINT('Ctrl Pts',(-10.9111153440001,12.2,1.10620106799999));
#260627=CARTESIAN_POINT('Ctrl Pts',(-10.9140350530001,12.2,1.10548629899998));
#260628=CARTESIAN_POINT('Ctrl Pts',(-10.9169594070001,12.2,1.10476785399999));
#260629=CARTESIAN_POINT('Ctrl Pts',(-10.9198883940001,12.2,1.10404572799998));
#260630=CARTESIAN_POINT('Ctrl Pts',(-10.9228220030001,12.2,1.10331991499999));
#260631=CARTESIAN_POINT('Ctrl Pts',(-10.9257602240001,12.2,1.10259041099999));
#260632=CARTESIAN_POINT('Ctrl Pts',(-10.9287030450001,12.2,1.10185720999999));
#260633=CARTESIAN_POINT('Ctrl Pts',(-10.9316504550001,12.2,1.10112030799999));
#260634=CARTESIAN_POINT('Ctrl Pts',(-10.9346024440001,12.2,1.10037969999999));
#260635=CARTESIAN_POINT('Ctrl Pts',(-10.9375590010001,12.2,1.09963537999999));
#260636=CARTESIAN_POINT('Ctrl Pts',(-10.9405201130001,12.2,1.09888734399998));
#260637=CARTESIAN_POINT('Ctrl Pts',(-10.9434857720001,12.2,1.09813558799999));
#260638=CARTESIAN_POINT('Ctrl Pts',(-10.9464559650001,12.2,1.09738010499999));
#260639=CARTESIAN_POINT('Ctrl Pts',(-10.9494306820001,12.2,1.09662089099999));
#260640=CARTESIAN_POINT('Ctrl Pts',(-10.9524099120001,12.2,1.09585794199999));
#260641=CARTESIAN_POINT('Ctrl Pts',(-10.9553936450001,12.2,1.09509125199999));
#260642=CARTESIAN_POINT('Ctrl Pts',(-10.9583818690001,12.2,1.09432081699998));
#260643=CARTESIAN_POINT('Ctrl Pts',(-10.9613745740001,12.2,1.09354663099999));
#260644=CARTESIAN_POINT('Ctrl Pts',(-10.9643717480001,12.2,1.09276869099999));
#260645=CARTESIAN_POINT('Ctrl Pts',(-10.9673733820001,12.2,1.09198699199998));
#260646=CARTESIAN_POINT('Ctrl Pts',(-10.9703794650001,12.2,1.09120152799999));
#260647=CARTESIAN_POINT('Ctrl Pts',(-10.9733899850001,12.2,1.09041229499999));
#260648=CARTESIAN_POINT('Ctrl Pts',(-10.9764049340001,12.2,1.08961928699999));
#260649=CARTESIAN_POINT('Ctrl Pts',(-10.9794242980001,12.2,1.08882250199999));
#260650=CARTESIAN_POINT('Ctrl Pts',(-10.9824480680001,12.2,1.08802193399999));
#260651=CARTESIAN_POINT('Ctrl Pts',(-10.9854762340001,12.2,1.08721757799998));
#260652=CARTESIAN_POINT('Ctrl Pts',(-10.9885087840001,12.2,1.08640942999998));
#260653=CARTESIAN_POINT('Ctrl Pts',(-10.9915457090001,12.2,1.08559748499998));
#260654=CARTESIAN_POINT('Ctrl Pts',(-10.9945869970001,12.2,1.08478173799998));
#260655=CARTESIAN_POINT('Ctrl Pts',(-10.9976326380001,12.2,1.08396218499998));
#260656=CARTESIAN_POINT('Ctrl Pts',(-11.0006826220001,12.2,1.08313882099999));
#260657=CARTESIAN_POINT('Ctrl Pts',(-11.0037369370001,12.2,1.08231164299998));
#260658=CARTESIAN_POINT('Ctrl Pts',(-11.0067955760001,12.2,1.08148064399999));
#260659=CARTESIAN_POINT('Ctrl Pts',(-11.0098585240001,12.2,1.08064582099999));
#260660=CARTESIAN_POINT('Ctrl Pts',(-11.0129257730001,12.2,1.07980717099998));
#260661=CARTESIAN_POINT('Ctrl Pts',(-11.0159973130001,12.2,1.07896468599999));
#260662=CARTESIAN_POINT('Ctrl Pts',(-11.0190731330001,12.2,1.07811836399998));
#260663=CARTESIAN_POINT('Ctrl Pts',(-11.0221532220001,12.2,1.07726820099999));
#260664=CARTESIAN_POINT('Ctrl Pts',(-11.0252375700001,12.2,1.07641418999998));
#260665=CARTESIAN_POINT('Ctrl Pts',(-11.0283261660001,12.2,1.07555632999999));
#260666=CARTESIAN_POINT('Ctrl Pts',(-11.0314190020001,12.2,1.07469461299999));
#260667=CARTESIAN_POINT('Ctrl Pts',(-11.0345160640001,12.2,1.07382903799999));
#260668=CARTESIAN_POINT('Ctrl Pts',(-11.0376173460001,12.2,1.07295959799998));
#260669=CARTESIAN_POINT('Ctrl Pts',(-11.0407228350001,12.2,1.07208629099999));
#260670=CARTESIAN_POINT('Ctrl Pts',(-11.0438325210001,12.2,1.07120911099999));
#260671=CARTESIAN_POINT('Ctrl Pts',(-11.0469463940001,12.2,1.07032805399998));
#260672=CARTESIAN_POINT('Ctrl Pts',(-11.0500644440001,12.2,1.06944311599999));
#260673=CARTESIAN_POINT('Ctrl Pts',(-11.0531866600001,12.2,1.06855429399999));
#260674=CARTESIAN_POINT('Ctrl Pts',(-11.0563130330001,12.2,1.06766158099999));
#260675=CARTESIAN_POINT('Ctrl Pts',(-11.0594435520001,12.2,1.06676497499999));
#260676=CARTESIAN_POINT('Ctrl Pts',(-11.0625782070001,12.2,1.06586446999998));
#260677=CARTESIAN_POINT('Ctrl Pts',(-11.0657169880001,12.2,1.06496006399999));
#260678=CARTESIAN_POINT('Ctrl Pts',(-11.0688598860001,12.2,1.06405175099999));
#260679=CARTESIAN_POINT('Ctrl Pts',(-11.0720068880001,12.2,1.06313952799999));
#260680=CARTESIAN_POINT('Ctrl Pts',(-11.0751579870001,12.2,1.06222338999999));
#260681=CARTESIAN_POINT('Ctrl Pts',(-11.0783131710001,12.2,1.06130333499999));
#260682=CARTESIAN_POINT('Ctrl Pts',(-11.0814724300001,12.2,1.06037935499999));
#260683=CARTESIAN_POINT('Ctrl Pts',(-11.0846357550001,12.2,1.05945144899998));
#260684=CARTESIAN_POINT('Ctrl Pts',(-11.0878031360001,12.2,1.05851961199999));
#260685=CARTESIAN_POINT('Ctrl Pts',(-11.0909745620001,12.2,1.05758383999999));
#260686=CARTESIAN_POINT('Ctrl Pts',(-11.0941500240001,12.2,1.05664412899999));
#260687=CARTESIAN_POINT('Ctrl Pts',(-11.0973295110001,12.2,1.05570047499999));
#260688=CARTESIAN_POINT('Ctrl Pts',(-11.1005130140001,12.2,1.05475287299999));
#260689=CARTESIAN_POINT('Ctrl Pts',(-11.1037005220001,12.2,1.05380132099999));
#260690=CARTESIAN_POINT('Ctrl Pts',(-11.1068920250001,12.2,1.05284581399999));
#260691=CARTESIAN_POINT('Ctrl Pts',(-11.1100875160001,12.2,1.05188634799998));
#260692=CARTESIAN_POINT('Ctrl Pts',(-11.1132869810001,12.2,1.05092291799998));
#260693=CARTESIAN_POINT('Ctrl Pts',(-11.1164904140001,12.2,1.04995552199998));
#260694=CARTESIAN_POINT('Ctrl Pts',(-11.1196978020001,12.2,1.04898415499999));
#260695=CARTESIAN_POINT('Ctrl Pts',(-11.1229091360001,12.2,1.04800881199999));
#260696=CARTESIAN_POINT('Ctrl Pts',(-11.1261244080001,12.2,1.04702949099998));
#260697=CARTESIAN_POINT('Ctrl Pts',(-11.1293436050001,12.2,1.04604618899999));
#260698=CARTESIAN_POINT('Ctrl Pts',(-11.1325667200001,12.2,1.04505889899999));
#260699=CARTESIAN_POINT('Ctrl Pts',(-11.1357937420001,12.2,1.04406762099998));
#260700=CARTESIAN_POINT('Ctrl Pts',(-11.1390246620001,12.2,1.04307234699998));
#260701=CARTESIAN_POINT('Ctrl Pts',(-11.1422594690001,12.2,1.04207307599999));
#260702=CARTESIAN_POINT('Ctrl Pts',(-11.1454981540001,12.2,1.04106980299999));
#260703=CARTESIAN_POINT('Ctrl Pts',(-11.1487407070001,12.2,1.04006252499998));
#260704=CARTESIAN_POINT('Ctrl Pts',(-11.1519871190001,12.2,1.03905123799999));
#260705=CARTESIAN_POINT('Ctrl Pts',(-11.1552373810001,12.2,1.03803593699999));
#260706=CARTESIAN_POINT('Ctrl Pts',(-11.1584914810001,12.2,1.03701662199999));
#260707=CARTESIAN_POINT('Ctrl Pts',(-11.1617494110001,12.2,1.03599328399998));
#260708=CARTESIAN_POINT('Ctrl Pts',(-11.1650111610001,12.2,1.03496592399999));
#260709=CARTESIAN_POINT('Ctrl Pts',(-11.1682767210001,12.2,1.03393453499999));
#260710=CARTESIAN_POINT('Ctrl Pts',(-11.1715460820001,12.2,1.03289911399999));
#260711=CARTESIAN_POINT('Ctrl Pts',(-11.1748192350001,12.2,1.03185965899999));
#260712=CARTESIAN_POINT('Ctrl Pts',(-11.1780961680001,12.2,1.03081616499999));
#260713=CARTESIAN_POINT('Ctrl Pts',(-11.1813768730001,12.2,1.02976862899999));
#260714=CARTESIAN_POINT('Ctrl Pts',(-11.1846613420001,12.2,1.02871704699998));
#260715=CARTESIAN_POINT('Ctrl Pts',(-11.1879495640001,12.2,1.02766141599998));
#260716=CARTESIAN_POINT('Ctrl Pts',(-11.1912415290001,12.2,1.02660173099999));
#260717=CARTESIAN_POINT('Ctrl Pts',(-11.1945372270001,12.2,1.02553798999999));
#260718=CARTESIAN_POINT('Ctrl Pts',(-11.1978366510001,12.2,1.02447018799999));
#260719=CARTESIAN_POINT('Ctrl Pts',(-11.2011397890001,12.2,1.02339832299998));
#260720=CARTESIAN_POINT('Ctrl Pts',(-11.2044466330001,12.2,1.02232238999999));
#260721=CARTESIAN_POINT('Ctrl Pts',(-11.2077571730001,12.2,1.02124238699998));
#260722=CARTESIAN_POINT('Ctrl Pts',(-11.2110714010001,12.2,1.02015830899999));
#260723=CARTESIAN_POINT('Ctrl Pts',(-11.2143893040001,12.2,1.01907015299998));
#260724=CARTESIAN_POINT('Ctrl Pts',(-11.2177108770001,12.2,1.01797791699999));
#260725=CARTESIAN_POINT('Ctrl Pts',(-11.2210361080001,12.2,1.01688159599998));
#260726=CARTESIAN_POINT('Ctrl Pts',(-11.2243649880001,12.2,1.01578118599999));
#260727=CARTESIAN_POINT('Ctrl Pts',(-11.2276975070001,12.2,1.01467668399998));
#260728=CARTESIAN_POINT('Ctrl Pts',(-11.2310336580001,12.2,1.01356808799999));
#260729=CARTESIAN_POINT('Ctrl Pts',(-11.2343734290001,12.2,1.01245539299998));
#260730=CARTESIAN_POINT('Ctrl Pts',(-11.2377168140001,12.2,1.01133859799999));
#260731=CARTESIAN_POINT('Ctrl Pts',(-11.2410637990001,12.2,1.01021769499999));
#260732=CARTESIAN_POINT('Ctrl Pts',(-11.2444143790001,12.2,1.00909268499999));
#260733=CARTESIAN_POINT('Ctrl Pts',(-11.2477685430001,12.2,1.00796356299998));
#260734=CARTESIAN_POINT('Ctrl Pts',(-11.2511262810001,12.2,1.00683032499999));
#260735=CARTESIAN_POINT('Ctrl Pts',(-11.2544875850001,12.2,1.00569296999999));
#260736=CARTESIAN_POINT('Ctrl Pts',(-11.2578524460001,12.2,1.00455149199998));
#260737=CARTESIAN_POINT('Ctrl Pts',(-11.2612208540001,12.2,1.00340588999998));
#260738=CARTESIAN_POINT('Ctrl Pts',(-11.2645927990001,12.2,1.00225615799999));
#260739=CARTESIAN_POINT('Ctrl Pts',(-11.2679682740001,12.2,1.00110229499998));
#260740=CARTESIAN_POINT('Ctrl Pts',(-11.2713472680001,12.2,0.999944296999988));
#260741=CARTESIAN_POINT('Ctrl Pts',(-11.2747297730001,12.2,0.998782160999987));
#260742=CARTESIAN_POINT('Ctrl Pts',(-11.2781157800001,12.2,0.997615882999985));
#260743=CARTESIAN_POINT('Ctrl Pts',(-11.2815052780001,12.2,0.996445461999986));
#260744=CARTESIAN_POINT('Ctrl Pts',(-11.2848982590001,12.2,0.995270892999987));
#260745=CARTESIAN_POINT('Ctrl Pts',(-11.2882947150001,12.2,0.994092171999985));
#260746=CARTESIAN_POINT('Ctrl Pts',(-11.2916946350001,12.2,0.992909295999986));
#260747=CARTESIAN_POINT('Ctrl Pts',(-11.2950980120001,12.2,0.991722263999986));
#260748=CARTESIAN_POINT('Ctrl Pts',(-11.2985048360001,12.2,0.990531070999987));
#260749=CARTESIAN_POINT('Ctrl Pts',(-11.3019150960001,12.2,0.989335713999986));
#260750=CARTESIAN_POINT('Ctrl Pts',(-11.3053287860001,12.2,0.988136191999986));
#260751=CARTESIAN_POINT('Ctrl Pts',(-11.3087458960001,12.2,0.986932498999984));
#260752=CARTESIAN_POINT('Ctrl Pts',(-11.3121664170001,12.2,0.985724631999982));
#260753=CARTESIAN_POINT('Ctrl Pts',(-11.3155903390001,12.2,0.984512589999986));
#260754=CARTESIAN_POINT('Ctrl Pts',(-11.3190176540001,12.2,0.983296368999986));
#260755=CARTESIAN_POINT('Ctrl Pts',(-11.3224483530001,12.2,0.982075965999982));
#260756=CARTESIAN_POINT('Ctrl Pts',(-11.3258824260001,12.2,0.980851377999983));
#260757=CARTESIAN_POINT('Ctrl Pts',(-11.3293198660001,12.2,0.979622600999988));
#260758=CARTESIAN_POINT('Ctrl Pts',(-11.3327606630001,12.2,0.978389632999987));
#260759=CARTESIAN_POINT('Ctrl Pts',(-11.3362048080001,12.2,0.977152470999982));
#260760=CARTESIAN_POINT('Ctrl Pts',(-11.3396522920001,12.2,0.975911110999985));
#260761=CARTESIAN_POINT('Ctrl Pts',(-11.3431031070001,12.2,0.974665550999987));
#260762=CARTESIAN_POINT('Ctrl Pts',(-11.3465572430001,12.2,0.973415788999983));
#260763=CARTESIAN_POINT('Ctrl Pts',(-11.3500146920001,12.2,0.972161818999986));
#260764=CARTESIAN_POINT('Ctrl Pts',(-11.3534754440001,12.2,0.970903640999987));
#260765=CARTESIAN_POINT('Ctrl Pts',(-11.3569394920001,12.2,0.969641250999986));
#260766=CARTESIAN_POINT('Ctrl Pts',(-11.3604068260001,12.2,0.968374645999983));
#260767=CARTESIAN_POINT('Ctrl Pts',(-11.3638774360001,12.2,0.967103821999986));
#260768=CARTESIAN_POINT('Ctrl Pts',(-11.3673513150001,12.2,0.965828777999986));
#260769=CARTESIAN_POINT('Ctrl Pts',(-11.3708284530001,12.2,0.964549509999983));
#260770=CARTESIAN_POINT('Ctrl Pts',(-11.3743088440001,12.2,0.963266015999986));
#260771=CARTESIAN_POINT('Ctrl Pts',(-11.3777924770001,12.2,0.961978291999985));
#260772=CARTESIAN_POINT('Ctrl Pts',(-11.3812793430001,12.2,0.960686337999985));
#260773=CARTESIAN_POINT('Ctrl Pts',(-11.3847694350001,12.2,0.959390146999985));
#260774=CARTESIAN_POINT('Ctrl Pts',(-11.3882627430001,12.2,0.958089718999986));
#260775=CARTESIAN_POINT('Ctrl Pts',(-11.3917592580001,12.2,0.956785048999986));
#260776=CARTESIAN_POINT('Ctrl Pts',(-11.3952589700001,12.2,0.955476136999986));
#260777=CARTESIAN_POINT('Ctrl Pts',(-11.3987618720001,12.2,0.954162976999986));
#260778=CARTESIAN_POINT('Ctrl Pts',(-11.4022679530001,12.2,0.952845567999985));
#260779=CARTESIAN_POINT('Ctrl Pts',(-11.4057772070001,12.2,0.951523905999987));
#260780=CARTESIAN_POINT('Ctrl Pts',(-11.4092896250001,12.2,0.950197990999988));
#260781=CARTESIAN_POINT('Ctrl Pts',(-11.4128052000001,12.2,0.948867817999983));
#260782=CARTESIAN_POINT('Ctrl Pts',(-11.4163239240001,12.2,0.947533386999986));
#260783=CARTESIAN_POINT('Ctrl Pts',(-11.4198457890001,12.2,0.946194692999986));
#260784=CARTESIAN_POINT('Ctrl Pts',(-11.4233707840001,12.2,0.944851733999985));
#260785=CARTESIAN_POINT('Ctrl Pts',(-11.4268989030001,12.2,0.943504507999986));
#260786=CARTESIAN_POINT('Ctrl Pts',(-11.4304301310001,12.2,0.942153010999984));
#260787=CARTESIAN_POINT('Ctrl Pts',(-11.4339644600001,12.2,0.940797237999984));
#260788=CARTESIAN_POINT('Ctrl Pts',(-11.4375018800001,12.2,0.939437186999985));
#260789=CARTESIAN_POINT('Ctrl Pts',(-11.4410423790001,12.2,0.938072855999987));
#260790=CARTESIAN_POINT('Ctrl Pts',(-11.4445859520001,12.2,0.936704240999986));
#260791=CARTESIAN_POINT('Ctrl Pts',(-11.4481325920001,12.2,0.935331340999985));
#260792=CARTESIAN_POINT('Ctrl Pts',(-11.4516822960001,12.2,0.933954156999985));
#260793=CARTESIAN_POINT('Ctrl Pts',(-11.4552350600001,12.2,0.932572684999986));
#260794=CARTESIAN_POINT('Ctrl Pts',(-11.4580797200001,12.2,0.931464077999986));
#260795=CARTESIAN_POINT('Ctrl Pts',(-11.4602145910001,12.2,0.930630692999985));
#260796=CARTESIAN_POINT('Ctrl Pts',(-11.4616384500001,12.2,0.930074245999983));
#260797=CARTESIAN_POINT('Ctrl Pts',(-11.4623505340001,12.2,0.929795807999985));
#260798=CARTESIAN_POINT('Ctrl Pts',(-11.4869855320001,15.2,0.546958305999983));
#260799=CARTESIAN_POINT('Ctrl Pts',(-11.4869855320001,11.6,0.546958305999982));
#260800=CARTESIAN_POINT('Ctrl Pts',(-11.4863150090001,15.2,0.546590898999986));
#260801=CARTESIAN_POINT('Ctrl Pts',(-11.4863150090001,11.6,0.546590898999985));
#260802=CARTESIAN_POINT('Ctrl Pts',(-11.4849742100001,15.2,0.545856550999986));
#260803=CARTESIAN_POINT('Ctrl Pts',(-11.4849742100001,11.6,0.545856550999985));
#260804=CARTESIAN_POINT('Ctrl Pts',(-11.4829637560001,15.2,0.544756421999986));
#260805=CARTESIAN_POINT('Ctrl Pts',(-11.4829637560001,11.6,0.544756421999985));
#260806=CARTESIAN_POINT('Ctrl Pts',(-11.4802846430001,15.2,0.543292367999988));
#260807=CARTESIAN_POINT('Ctrl Pts',(-11.4802846430001,11.6,0.543292367999987));
#260808=CARTESIAN_POINT('Ctrl Pts',(-11.4769382380001,15.2,0.541466945999982));
#260809=CARTESIAN_POINT('Ctrl Pts',(-11.4769382380001,11.6,0.541466945999982));
#260810=CARTESIAN_POINT('Ctrl Pts',(-11.4735943180001,15.2,0.539646165999983));
#260811=CARTESIAN_POINT('Ctrl Pts',(-11.4735943180001,11.6,0.539646165999982));
#260812=CARTESIAN_POINT('Ctrl Pts',(-11.4702528880001,15.2,0.537830029999986));
#260813=CARTESIAN_POINT('Ctrl Pts',(-11.4702528880001,11.6,0.537830029999986));
#260814=CARTESIAN_POINT('Ctrl Pts',(-11.4669139500001,15.2,0.536018536999983));
#260815=CARTESIAN_POINT('Ctrl Pts',(-11.4669139500001,11.6,0.536018536999982));
#260816=CARTESIAN_POINT('Ctrl Pts',(-11.4635775100001,15.2,0.534211684999986));
#260817=CARTESIAN_POINT('Ctrl Pts',(-11.4635775100001,11.6,0.534211684999985));
#260818=CARTESIAN_POINT('Ctrl Pts',(-11.4602435780001,15.2,0.532409473999986));
#260819=CARTESIAN_POINT('Ctrl Pts',(-11.4602435780001,11.6,0.532409473999986));
#260820=CARTESIAN_POINT('Ctrl Pts',(-11.4569121620001,15.2,0.530611900999984));
#260821=CARTESIAN_POINT('Ctrl Pts',(-11.4569121620001,11.6,0.530611900999984));
#260822=CARTESIAN_POINT('Ctrl Pts',(-11.4535832720001,15.2,0.528818965999989));
#260823=CARTESIAN_POINT('Ctrl Pts',(-11.4535832720001,11.6,0.528818965999988));
#260824=CARTESIAN_POINT('Ctrl Pts',(-11.4502569220001,15.2,0.527030663999986));
#260825=CARTESIAN_POINT('Ctrl Pts',(-11.4502569220001,11.6,0.527030663999985));
#260826=CARTESIAN_POINT('Ctrl Pts',(-11.4469331180001,15.2,0.525246995999984));
#260827=CARTESIAN_POINT('Ctrl Pts',(-11.4469331180001,11.6,0.525246995999983));
#260828=CARTESIAN_POINT('Ctrl Pts',(-11.4436118760001,15.2,0.523467958999984));
#260829=CARTESIAN_POINT('Ctrl Pts',(-11.4436118760001,11.6,0.523467958999983));
#260830=CARTESIAN_POINT('Ctrl Pts',(-11.4402932010001,15.2,0.521693550999984));
#260831=CARTESIAN_POINT('Ctrl Pts',(-11.4402932010001,11.6,0.521693550999984));
#260832=CARTESIAN_POINT('Ctrl Pts',(-11.4369771030001,15.2,0.519923770999986));
#260833=CARTESIAN_POINT('Ctrl Pts',(-11.4369771030001,11.6,0.519923770999986));
#260834=CARTESIAN_POINT('Ctrl Pts',(-11.4336635900001,15.2,0.518158617999984));
#260835=CARTESIAN_POINT('Ctrl Pts',(-11.4336635900001,11.6,0.518158617999984));
#260836=CARTESIAN_POINT('Ctrl Pts',(-11.4303526710001,15.2,0.516398088999988));
#260837=CARTESIAN_POINT('Ctrl Pts',(-11.4303526710001,11.6,0.516398088999987));
#260838=CARTESIAN_POINT('Ctrl Pts',(-11.4270443520001,15.2,0.514642183999987));
#260839=CARTESIAN_POINT('Ctrl Pts',(-11.4270443520001,11.6,0.514642183999987));
#260840=CARTESIAN_POINT('Ctrl Pts',(-11.4237386430001,15.2,0.512890900999987));
#260841=CARTESIAN_POINT('Ctrl Pts',(-11.4237386430001,11.6,0.512890900999987));
#260842=CARTESIAN_POINT('Ctrl Pts',(-11.4204355510001,15.2,0.511144238999983));
#260843=CARTESIAN_POINT('Ctrl Pts',(-11.4204355510001,11.6,0.511144238999983));
#260844=CARTESIAN_POINT('Ctrl Pts',(-11.4171350880001,15.2,0.509402193999984));
#260845=CARTESIAN_POINT('Ctrl Pts',(-11.4171350880001,11.6,0.509402193999983));
#260846=CARTESIAN_POINT('Ctrl Pts',(-11.4138372610001,15.2,0.507664766999985));
#260847=CARTESIAN_POINT('Ctrl Pts',(-11.4138372610001,11.6,0.507664766999984));
#260848=CARTESIAN_POINT('Ctrl Pts',(-11.4105420820001,15.2,0.505931953999985));
#260849=CARTESIAN_POINT('Ctrl Pts',(-11.4105420820001,11.6,0.505931953999985));
#260850=CARTESIAN_POINT('Ctrl Pts',(-11.4072495570001,15.2,0.504203755999986));
#260851=CARTESIAN_POINT('Ctrl Pts',(-11.4072495570001,11.6,0.504203755999985));
#260852=CARTESIAN_POINT('Ctrl Pts',(-11.4039596970001,15.2,0.502480167999986));
#260853=CARTESIAN_POINT('Ctrl Pts',(-11.4039596970001,11.6,0.502480167999985));
#260854=CARTESIAN_POINT('Ctrl Pts',(-11.4006725110001,15.2,0.500761190999985));
#260855=CARTESIAN_POINT('Ctrl Pts',(-11.4006725110001,11.6,0.500761190999985));
#260856=CARTESIAN_POINT('Ctrl Pts',(-11.3973880080001,15.2,0.499046821999984));
#260857=CARTESIAN_POINT('Ctrl Pts',(-11.3973880080001,11.6,0.499046821999984));
#260858=CARTESIAN_POINT('Ctrl Pts',(-11.3941061970001,15.2,0.497337060999987));
#260859=CARTESIAN_POINT('Ctrl Pts',(-11.3941061970001,11.6,0.497337060999987));
#260860=CARTESIAN_POINT('Ctrl Pts',(-11.3908270860001,15.2,0.495631902999989));
#260861=CARTESIAN_POINT('Ctrl Pts',(-11.3908270860001,11.6,0.495631902999988));
#260862=CARTESIAN_POINT('Ctrl Pts',(-11.3875506850001,15.2,0.493931348999985));
#260863=CARTESIAN_POINT('Ctrl Pts',(-11.3875506850001,11.6,0.493931348999985));
#260864=CARTESIAN_POINT('Ctrl Pts',(-11.3842770020001,15.2,0.492235395999985));
#260865=CARTESIAN_POINT('Ctrl Pts',(-11.3842770020001,11.6,0.492235395999984));
#260866=CARTESIAN_POINT('Ctrl Pts',(-11.3810060480001,15.2,0.490544042999983));
#260867=CARTESIAN_POINT('Ctrl Pts',(-11.3810060480001,11.6,0.490544042999983));
#260868=CARTESIAN_POINT('Ctrl Pts',(-11.3777378300001,15.2,0.488857287999984));
#260869=CARTESIAN_POINT('Ctrl Pts',(-11.3777378300001,11.6,0.488857287999984));
#260870=CARTESIAN_POINT('Ctrl Pts',(-11.3744723580001,15.2,0.487175127999984));
#260871=CARTESIAN_POINT('Ctrl Pts',(-11.3744723580001,11.6,0.487175127999983));
#260872=CARTESIAN_POINT('Ctrl Pts',(-11.3712096420001,15.2,0.485497562999986));
#260873=CARTESIAN_POINT('Ctrl Pts',(-11.3712096420001,11.6,0.485497562999985));
#260874=CARTESIAN_POINT('Ctrl Pts',(-11.3679496900001,15.2,0.483824590999986));
#260875=CARTESIAN_POINT('Ctrl Pts',(-11.3679496900001,11.6,0.483824590999986));
#260876=CARTESIAN_POINT('Ctrl Pts',(-11.3646925130001,15.2,0.482156208999989));
#260877=CARTESIAN_POINT('Ctrl Pts',(-11.3646925130001,11.6,0.482156208999988));
#260878=CARTESIAN_POINT('Ctrl Pts',(-11.3614381180001,15.2,0.480492415999985));
#260879=CARTESIAN_POINT('Ctrl Pts',(-11.3614381180001,11.6,0.480492415999984));
#260880=CARTESIAN_POINT('Ctrl Pts',(-11.3581865150001,15.2,0.478833208999987));
#260881=CARTESIAN_POINT('Ctrl Pts',(-11.3581865150001,11.6,0.478833208999986));
#260882=CARTESIAN_POINT('Ctrl Pts',(-11.3549377140001,15.2,0.477178588999987));
#260883=CARTESIAN_POINT('Ctrl Pts',(-11.3549377140001,11.6,0.477178588999986));
#260884=CARTESIAN_POINT('Ctrl Pts',(-11.3516917240001,15.2,0.475528550999984));
#260885=CARTESIAN_POINT('Ctrl Pts',(-11.3516917240001,11.6,0.475528550999984));
#260886=CARTESIAN_POINT('Ctrl Pts',(-11.3484485530001,15.2,0.473883093999987));
#260887=CARTESIAN_POINT('Ctrl Pts',(-11.3484485530001,11.6,0.473883093999987));
#260888=CARTESIAN_POINT('Ctrl Pts',(-11.3452082120001,15.2,0.472242216999987));
#260889=CARTESIAN_POINT('Ctrl Pts',(-11.3452082120001,11.6,0.472242216999987));
#260890=CARTESIAN_POINT('Ctrl Pts',(-11.3419707090001,15.2,0.470605916999984));
#260891=CARTESIAN_POINT('Ctrl Pts',(-11.3419707090001,11.6,0.470605916999984));
#260892=CARTESIAN_POINT('Ctrl Pts',(-11.3387360540001,15.2,0.468974193999987));
#260893=CARTESIAN_POINT('Ctrl Pts',(-11.3387360540001,11.6,0.468974193999987));
#260894=CARTESIAN_POINT('Ctrl Pts',(-11.3355042560001,15.2,0.467347044999986));
#260895=CARTESIAN_POINT('Ctrl Pts',(-11.3355042560001,11.6,0.467347044999986));
#260896=CARTESIAN_POINT('Ctrl Pts',(-11.3322753250001,15.2,0.465724465999986));
#260897=CARTESIAN_POINT('Ctrl Pts',(-11.3322753250001,11.6,0.465724465999986));
#260898=CARTESIAN_POINT('Ctrl Pts',(-11.3290492700001,15.2,0.464106457999982));
#260899=CARTESIAN_POINT('Ctrl Pts',(-11.3290492700001,11.6,0.464106457999982));
#260900=CARTESIAN_POINT('Ctrl Pts',(-11.3258260990001,15.2,0.462493017999983));
#260901=CARTESIAN_POINT('Ctrl Pts',(-11.3258260990001,11.6,0.462493017999983));
#260902=CARTESIAN_POINT('Ctrl Pts',(-11.3226058230001,15.2,0.460884142999984));
#260903=CARTESIAN_POINT('Ctrl Pts',(-11.3226058230001,11.6,0.460884142999984));
#260904=CARTESIAN_POINT('Ctrl Pts',(-11.3193884510001,15.2,0.459279831999986));
#260905=CARTESIAN_POINT('Ctrl Pts',(-11.3193884510001,11.6,0.459279831999985));
#260906=CARTESIAN_POINT('Ctrl Pts',(-11.3161739920001,15.2,0.457680083999983));
#260907=CARTESIAN_POINT('Ctrl Pts',(-11.3161739920001,11.6,0.457680083999982));
#260908=CARTESIAN_POINT('Ctrl Pts',(-11.3129624580001,15.2,0.456084895999984));
#260909=CARTESIAN_POINT('Ctrl Pts',(-11.3129624580001,11.6,0.456084895999984));
#260910=CARTESIAN_POINT('Ctrl Pts',(-11.3097538530001,15.2,0.454494265999985));
#260911=CARTESIAN_POINT('Ctrl Pts',(-11.3097538530001,11.6,0.454494265999985));
#260912=CARTESIAN_POINT('Ctrl Pts',(-11.3065481920001,15.2,0.452908190999985));
#260913=CARTESIAN_POINT('Ctrl Pts',(-11.3065481920001,11.6,0.452908190999985));
#260914=CARTESIAN_POINT('Ctrl Pts',(-11.3033454810001,15.2,0.451326670999985));
#260915=CARTESIAN_POINT('Ctrl Pts',(-11.3033454810001,11.6,0.451326670999985));
#260916=CARTESIAN_POINT('Ctrl Pts',(-11.3001457320001,15.2,0.449749702999984));
#260917=CARTESIAN_POINT('Ctrl Pts',(-11.3001457320001,11.6,0.449749702999984));
#260918=CARTESIAN_POINT('Ctrl Pts',(-11.2969489510001,15.2,0.448177283999982));
#260919=CARTESIAN_POINT('Ctrl Pts',(-11.2969489510001,11.6,0.448177283999982));
#260920=CARTESIAN_POINT('Ctrl Pts',(-11.2937551520001,15.2,0.446609412999983));
#260921=CARTESIAN_POINT('Ctrl Pts',(-11.2937551520001,11.6,0.446609412999983));
#260922=CARTESIAN_POINT('Ctrl Pts',(-11.2905643410001,15.2,0.445046087999987));
#260923=CARTESIAN_POINT('Ctrl Pts',(-11.2905643410001,11.6,0.445046087999987));
#260924=CARTESIAN_POINT('Ctrl Pts',(-11.2873765290001,15.2,0.443487306999986));
#260925=CARTESIAN_POINT('Ctrl Pts',(-11.2873765290001,11.6,0.443487306999985));
#260926=CARTESIAN_POINT('Ctrl Pts',(-11.2841917260001,15.2,0.441933066999987));
#260927=CARTESIAN_POINT('Ctrl Pts',(-11.2841917260001,11.6,0.441933066999986));
#260928=CARTESIAN_POINT('Ctrl Pts',(-11.2810099400001,15.2,0.440383366999986));
#260929=CARTESIAN_POINT('Ctrl Pts',(-11.2810099400001,11.6,0.440383366999985));
#260930=CARTESIAN_POINT('Ctrl Pts',(-11.2778311820001,15.2,0.438838203999987));
#260931=CARTESIAN_POINT('Ctrl Pts',(-11.2778311820001,11.6,0.438838203999987));
#260932=CARTESIAN_POINT('Ctrl Pts',(-11.2746554610001,15.2,0.437297575999986));
#260933=CARTESIAN_POINT('Ctrl Pts',(-11.2746554610001,11.6,0.437297575999986));
#260934=CARTESIAN_POINT('Ctrl Pts',(-11.2714827870001,15.2,0.435761481999983));
#260935=CARTESIAN_POINT('Ctrl Pts',(-11.2714827870001,11.6,0.435761481999983));
#260936=CARTESIAN_POINT('Ctrl Pts',(-11.2683131690001,15.2,0.434229917999982));
#260937=CARTESIAN_POINT('Ctrl Pts',(-11.2683131690001,11.6,0.434229917999982));
#260938=CARTESIAN_POINT('Ctrl Pts',(-11.2651466170001,15.2,0.432702882999987));
#260939=CARTESIAN_POINT('Ctrl Pts',(-11.2651466170001,11.6,0.432702882999986));
#260940=CARTESIAN_POINT('Ctrl Pts',(-11.2619831420001,15.2,0.431180374999984));
#260941=CARTESIAN_POINT('Ctrl Pts',(-11.2619831420001,11.6,0.431180374999984));
#260942=CARTESIAN_POINT('Ctrl Pts',(-11.2588227510001,15.2,0.429662389999983));
#260943=CARTESIAN_POINT('Ctrl Pts',(-11.2588227510001,11.6,0.429662389999983));
#260944=CARTESIAN_POINT('Ctrl Pts',(-11.2556654560001,15.2,0.428148927999987));
#260945=CARTESIAN_POINT('Ctrl Pts',(-11.2556654560001,11.6,0.428148927999987));
#260946=CARTESIAN_POINT('Ctrl Pts',(-11.2525112650001,15.2,0.426639985999984));
#260947=CARTESIAN_POINT('Ctrl Pts',(-11.2525112650001,11.6,0.426639985999983));
#260948=CARTESIAN_POINT('Ctrl Pts',(-11.2493601900001,15.2,0.425135561999985));
#260949=CARTESIAN_POINT('Ctrl Pts',(-11.2493601900001,11.6,0.425135561999985));
#260950=CARTESIAN_POINT('Ctrl Pts',(-11.2462122380001,15.2,0.423635652999987));
#260951=CARTESIAN_POINT('Ctrl Pts',(-11.2462122380001,11.6,0.423635652999987));
#260952=CARTESIAN_POINT('Ctrl Pts',(-11.2430674210001,15.2,0.422140256999985));
#260953=CARTESIAN_POINT('Ctrl Pts',(-11.2430674210001,11.6,0.422140256999985));
#260954=CARTESIAN_POINT('Ctrl Pts',(-11.2399257470001,15.2,0.420649372999984));
#260955=CARTESIAN_POINT('Ctrl Pts',(-11.2399257470001,11.6,0.420649372999983));
#260956=CARTESIAN_POINT('Ctrl Pts',(-11.2367872280001,15.2,0.419162996999987));
#260957=CARTESIAN_POINT('Ctrl Pts',(-11.2367872280001,11.6,0.419162996999986));
#260958=CARTESIAN_POINT('Ctrl Pts',(-11.2336518720001,15.2,0.417681126999985));
#260959=CARTESIAN_POINT('Ctrl Pts',(-11.2336518720001,11.6,0.417681126999984));
#260960=CARTESIAN_POINT('Ctrl Pts',(-11.2305196890001,15.2,0.416203761999987));
#260961=CARTESIAN_POINT('Ctrl Pts',(-11.2305196890001,11.6,0.416203761999987));
#260962=CARTESIAN_POINT('Ctrl Pts',(-11.2273906900001,15.2,0.414730897999984));
#260963=CARTESIAN_POINT('Ctrl Pts',(-11.2273906900001,11.6,0.414730897999984));
#260964=CARTESIAN_POINT('Ctrl Pts',(-11.2242648840001,15.2,0.413262533999985));
#260965=CARTESIAN_POINT('Ctrl Pts',(-11.2242648840001,11.6,0.413262533999985));
#260966=CARTESIAN_POINT('Ctrl Pts',(-11.2211422810001,15.2,0.411798666999985));
#260967=CARTESIAN_POINT('Ctrl Pts',(-11.2211422810001,11.6,0.411798666999985));
#260968=CARTESIAN_POINT('Ctrl Pts',(-11.2180228910001,15.2,0.410339293999984));
#260969=CARTESIAN_POINT('Ctrl Pts',(-11.2180228910001,11.6,0.410339293999983));
#260970=CARTESIAN_POINT('Ctrl Pts',(-11.2149067230001,15.2,0.408884414999986));
#260971=CARTESIAN_POINT('Ctrl Pts',(-11.2149067230001,11.6,0.408884414999986));
#260972=CARTESIAN_POINT('Ctrl Pts',(-11.2117937880001,15.2,0.407434024999986));
#260973=CARTESIAN_POINT('Ctrl Pts',(-11.2117937880001,11.6,0.407434024999986));
#260974=CARTESIAN_POINT('Ctrl Pts',(-11.2086840970001,15.2,0.405988122999985));
#260975=CARTESIAN_POINT('Ctrl Pts',(-11.2086840970001,11.6,0.405988122999985));
#260976=CARTESIAN_POINT('Ctrl Pts',(-11.2055776580001,15.2,0.404546704999986));
#260977=CARTESIAN_POINT('Ctrl Pts',(-11.2055776580001,11.6,0.404546704999986));
#260978=CARTESIAN_POINT('Ctrl Pts',(-11.2024744820001,15.2,0.403109771999985));
#260979=CARTESIAN_POINT('Ctrl Pts',(-11.2024744820001,11.6,0.403109771999985));
#260980=CARTESIAN_POINT('Ctrl Pts',(-11.1993745780001,15.2,0.401677316999987));
#260981=CARTESIAN_POINT('Ctrl Pts',(-11.1993745780001,11.6,0.401677316999986));
#260982=CARTESIAN_POINT('Ctrl Pts',(-11.1962779570001,15.2,0.400249341999985));
#260983=CARTESIAN_POINT('Ctrl Pts',(-11.1962779570001,11.6,0.400249341999985));
#260984=CARTESIAN_POINT('Ctrl Pts',(-11.1931846300001,15.2,0.398825840999986));
#260985=CARTESIAN_POINT('Ctrl Pts',(-11.1931846300001,11.6,0.398825840999985));
#260986=CARTESIAN_POINT('Ctrl Pts',(-11.1900946040001,15.2,0.397406813999983));
#260987=CARTESIAN_POINT('Ctrl Pts',(-11.1900946040001,11.6,0.397406813999983));
#260988=CARTESIAN_POINT('Ctrl Pts',(-11.1870078920001,15.2,0.395992257999982));
#260989=CARTESIAN_POINT('Ctrl Pts',(-11.1870078920001,11.6,0.395992257999982));
#260990=CARTESIAN_POINT('Ctrl Pts',(-11.1839245020001,15.2,0.394582169999986));
#260991=CARTESIAN_POINT('Ctrl Pts',(-11.1839245020001,11.6,0.394582169999986));
#260992=CARTESIAN_POINT('Ctrl Pts',(-11.1808444470001,15.2,0.393176545999987));
#260993=CARTESIAN_POINT('Ctrl Pts',(-11.1808444470001,11.6,0.393176545999987));
#260994=CARTESIAN_POINT('Ctrl Pts',(-11.1777677340001,15.2,0.391775386999988));
#260995=CARTESIAN_POINT('Ctrl Pts',(-11.1777677340001,11.6,0.391775386999988));
#260996=CARTESIAN_POINT('Ctrl Pts',(-11.1746943740001,15.2,0.390378687999986));
#260997=CARTESIAN_POINT('Ctrl Pts',(-11.1746943740001,11.6,0.390378687999986));
#260998=CARTESIAN_POINT('Ctrl Pts',(-11.1716243780001,15.2,0.388986446999984));
#260999=CARTESIAN_POINT('Ctrl Pts',(-11.1716243780001,11.6,0.388986446999983));
#261000=CARTESIAN_POINT('Ctrl Pts',(-11.1685577570001,15.2,0.387598660999986));
#261001=CARTESIAN_POINT('Ctrl Pts',(-11.1685577570001,11.6,0.387598660999986));
#261002=CARTESIAN_POINT('Ctrl Pts',(-11.1654945190001,15.2,0.386215327999988));
#261003=CARTESIAN_POINT('Ctrl Pts',(-11.1654945190001,11.6,0.386215327999988));
#261004=CARTESIAN_POINT('Ctrl Pts',(-11.1624346740001,15.2,0.384836445999985));
#261005=CARTESIAN_POINT('Ctrl Pts',(-11.1624346740001,11.6,0.384836445999985));
#261006=CARTESIAN_POINT('Ctrl Pts',(-11.1593782350001,15.2,0.383462010999986));
#261007=CARTESIAN_POINT('Ctrl Pts',(-11.1593782350001,11.6,0.383462010999986));
#261008=CARTESIAN_POINT('Ctrl Pts',(-11.1563252100001,15.2,0.382092021999987));
#261009=CARTESIAN_POINT('Ctrl Pts',(-11.1563252100001,11.6,0.382092021999986));
#261010=CARTESIAN_POINT('Ctrl Pts',(-11.1532756110001,15.2,0.380726473999986));
#261011=CARTESIAN_POINT('Ctrl Pts',(-11.1532756110001,11.6,0.380726473999986));
#261012=CARTESIAN_POINT('Ctrl Pts',(-11.1502294460001,15.2,0.379365366999984));
#261013=CARTESIAN_POINT('Ctrl Pts',(-11.1502294460001,11.6,0.379365366999984));
#261014=CARTESIAN_POINT('Ctrl Pts',(-11.1471867270001,15.2,0.378008696999985));
#261015=CARTESIAN_POINT('Ctrl Pts',(-11.1471867270001,11.6,0.378008696999985));
#261016=CARTESIAN_POINT('Ctrl Pts',(-11.1441474640001,15.2,0.376656461999989));
#261017=CARTESIAN_POINT('Ctrl Pts',(-11.1441474640001,11.6,0.376656461999989));
#261018=CARTESIAN_POINT('Ctrl Pts',(-11.1411116670001,15.2,0.375308657999986));
#261019=CARTESIAN_POINT('Ctrl Pts',(-11.1411116670001,11.6,0.375308657999986));
#261020=CARTESIAN_POINT('Ctrl Pts',(-11.1380793470001,15.2,0.373965283999986));
#261021=CARTESIAN_POINT('Ctrl Pts',(-11.1380793470001,11.6,0.373965283999986));
#261022=CARTESIAN_POINT('Ctrl Pts',(-11.1350505130001,15.2,0.372626335999984));
#261023=CARTESIAN_POINT('Ctrl Pts',(-11.1350505130001,11.6,0.372626335999983));
#261024=CARTESIAN_POINT('Ctrl Pts',(-11.1320251780001,15.2,0.371291811999988));
#261025=CARTESIAN_POINT('Ctrl Pts',(-11.1320251780001,11.6,0.371291811999987));
#261026=CARTESIAN_POINT('Ctrl Pts',(-11.1290033490001,15.2,0.369961708999984));
#261027=CARTESIAN_POINT('Ctrl Pts',(-11.1290033490001,11.6,0.369961708999984));
#261028=CARTESIAN_POINT('Ctrl Pts',(-11.1259850390001,15.2,0.368636023999986));
#261029=CARTESIAN_POINT('Ctrl Pts',(-11.1259850390001,11.6,0.368636023999986));
#261030=CARTESIAN_POINT('Ctrl Pts',(-11.1229702580001,15.2,0.367314754999986));
#261031=CARTESIAN_POINT('Ctrl Pts',(-11.1229702580001,11.6,0.367314754999985));
#261032=CARTESIAN_POINT('Ctrl Pts',(-11.1199590150001,15.2,0.365997898999986));
#261033=CARTESIAN_POINT('Ctrl Pts',(-11.1199590150001,11.6,0.365997898999985));
#261034=CARTESIAN_POINT('Ctrl Pts',(-11.1169513230001,15.2,0.364685452999982));
#261035=CARTESIAN_POINT('Ctrl Pts',(-11.1169513230001,11.6,0.364685452999982));
#261036=CARTESIAN_POINT('Ctrl Pts',(-11.1139471900001,15.2,0.363377413999988));
#261037=CARTESIAN_POINT('Ctrl Pts',(-11.1139471900001,11.6,0.363377413999987));
#261038=CARTESIAN_POINT('Ctrl Pts',(-11.1109466290001,15.2,0.362073778999985));
#261039=CARTESIAN_POINT('Ctrl Pts',(-11.1109466290001,11.6,0.362073778999985));
#261040=CARTESIAN_POINT('Ctrl Pts',(-11.1079496490001,15.2,0.360774545999987));
#261041=CARTESIAN_POINT('Ctrl Pts',(-11.1079496490001,11.6,0.360774545999986));
#261042=CARTESIAN_POINT('Ctrl Pts',(-11.1049562600001,15.2,0.359479711999988));
#261043=CARTESIAN_POINT('Ctrl Pts',(-11.1049562600001,11.6,0.359479711999988));
#261044=CARTESIAN_POINT('Ctrl Pts',(-11.1019664740001,15.2,0.358189272999985));
#261045=CARTESIAN_POINT('Ctrl Pts',(-11.1019664740001,11.6,0.358189272999984));
#261046=CARTESIAN_POINT('Ctrl Pts',(-11.0989803000001,15.2,0.356903227999985));
#261047=CARTESIAN_POINT('Ctrl Pts',(-11.0989803000001,11.6,0.356903227999985));
#261048=CARTESIAN_POINT('Ctrl Pts',(-11.0959977500001,15.2,0.355621572999985));
#261049=CARTESIAN_POINT('Ctrl Pts',(-11.0959977500001,11.6,0.355621572999984));
#261050=CARTESIAN_POINT('Ctrl Pts',(-11.0930188360001,15.2,0.354344304999987));
#261051=CARTESIAN_POINT('Ctrl Pts',(-11.0930188360001,11.6,0.354344304999987));
#261052=CARTESIAN_POINT('Ctrl Pts',(-11.0900435650001,15.2,0.353071420999989));
#261053=CARTESIAN_POINT('Ctrl Pts',(-11.0900435650001,11.6,0.353071420999988));
#261054=CARTESIAN_POINT('Ctrl Pts',(-11.0870719500001,15.2,0.351802918999984));
#261055=CARTESIAN_POINT('Ctrl Pts',(-11.0870719500001,11.6,0.351802918999983));
#261056=CARTESIAN_POINT('Ctrl Pts',(-11.0841040020001,15.2,0.350538794999986));
#261057=CARTESIAN_POINT('Ctrl Pts',(-11.0841040020001,11.6,0.350538794999986));
#261058=CARTESIAN_POINT('Ctrl Pts',(-11.0811397300001,15.2,0.349279046999986));
#261059=CARTESIAN_POINT('Ctrl Pts',(-11.0811397300001,11.6,0.349279046999986));
#261060=CARTESIAN_POINT('Ctrl Pts',(-11.0781791480001,15.2,0.348023670999984));
#261061=CARTESIAN_POINT('Ctrl Pts',(-11.0781791480001,11.6,0.348023670999984));
#261062=CARTESIAN_POINT('Ctrl Pts',(-11.0752222620001,15.2,0.346772664999988));
#261063=CARTESIAN_POINT('Ctrl Pts',(-11.0752222620001,11.6,0.346772664999988));
#261064=CARTESIAN_POINT('Ctrl Pts',(-11.0722690870001,15.2,0.345526024999985));
#261065=CARTESIAN_POINT('Ctrl Pts',(-11.0722690870001,11.6,0.345526024999984));
#261066=CARTESIAN_POINT('Ctrl Pts',(-11.0693196320001,15.2,0.344283748999987));
#261067=CARTESIAN_POINT('Ctrl Pts',(-11.0693196320001,11.6,0.344283748999987));
#261068=CARTESIAN_POINT('Ctrl Pts',(-11.0663739070001,15.2,0.343045833999986));
#261069=CARTESIAN_POINT('Ctrl Pts',(-11.0663739070001,11.6,0.343045833999986));
#261070=CARTESIAN_POINT('Ctrl Pts',(-11.0634319250001,15.2,0.341812274999986));
#261071=CARTESIAN_POINT('Ctrl Pts',(-11.0634319250001,11.6,0.341812274999986));
#261072=CARTESIAN_POINT('Ctrl Pts',(-11.0604936960001,15.2,0.340583071999987));
#261073=CARTESIAN_POINT('Ctrl Pts',(-11.0604936960001,11.6,0.340583071999986));
#261074=CARTESIAN_POINT('Ctrl Pts',(-11.0575592300001,15.2,0.339358219999983));
#261075=CARTESIAN_POINT('Ctrl Pts',(-11.0575592300001,11.6,0.339358219999983));
#261076=CARTESIAN_POINT('Ctrl Pts',(-11.0546285370001,15.2,0.338137715999984));
#261077=CARTESIAN_POINT('Ctrl Pts',(-11.0546285370001,11.6,0.338137715999984));
#261078=CARTESIAN_POINT('Ctrl Pts',(-11.0517016320001,15.2,0.336921557999985));
#261079=CARTESIAN_POINT('Ctrl Pts',(-11.0517016320001,11.6,0.336921557999985));
#261080=CARTESIAN_POINT('Ctrl Pts',(-11.0487785220001,15.2,0.335709739999985));
#261081=CARTESIAN_POINT('Ctrl Pts',(-11.0487785220001,11.6,0.335709739999985));
#261082=CARTESIAN_POINT('Ctrl Pts',(-11.0458592200001,15.2,0.334502262999985));
#261083=CARTESIAN_POINT('Ctrl Pts',(-11.0458592200001,11.6,0.334502262999985));
#261084=CARTESIAN_POINT('Ctrl Pts',(-11.0429437360001,15.2,0.333299120999988));
#261085=CARTESIAN_POINT('Ctrl Pts',(-11.0429437360001,11.6,0.333299120999988));
#261086=CARTESIAN_POINT('Ctrl Pts',(-11.0400320810001,15.2,0.332100310999985));
#261087=CARTESIAN_POINT('Ctrl Pts',(-11.0400320810001,11.6,0.332100310999985));
#261088=CARTESIAN_POINT('Ctrl Pts',(-11.0371242670001,15.2,0.330905830999986));
#261089=CARTESIAN_POINT('Ctrl Pts',(-11.0371242670001,11.6,0.330905830999985));
#261090=CARTESIAN_POINT('Ctrl Pts',(-11.0342203030001,15.2,0.329715676999989));
#261091=CARTESIAN_POINT('Ctrl Pts',(-11.0342203030001,11.6,0.329715676999988));
#261092=CARTESIAN_POINT('Ctrl Pts',(-11.0313202040001,15.2,0.328529845999985));
#261093=CARTESIAN_POINT('Ctrl Pts',(-11.0313202040001,11.6,0.328529845999985));
#261094=CARTESIAN_POINT('Ctrl Pts',(-11.0284239770001,15.2,0.327348335999984));
#261095=CARTESIAN_POINT('Ctrl Pts',(-11.0284239770001,11.6,0.327348335999984));
#261096=CARTESIAN_POINT('Ctrl Pts',(-11.0255316350001,15.2,0.326171140999989));
#261097=CARTESIAN_POINT('Ctrl Pts',(-11.0255316350001,11.6,0.326171140999989));
#261098=CARTESIAN_POINT('Ctrl Pts',(-11.0226431890001,15.2,0.324998259999987));
#261099=CARTESIAN_POINT('Ctrl Pts',(-11.0226431890001,11.6,0.324998259999986));
#261100=CARTESIAN_POINT('Ctrl Pts',(-11.0197586510001,15.2,0.323829688999986));
#261101=CARTESIAN_POINT('Ctrl Pts',(-11.0197586510001,11.6,0.323829688999985));
#261102=CARTESIAN_POINT('Ctrl Pts',(-11.0168780300001,15.2,0.322665424999986));
#261103=CARTESIAN_POINT('Ctrl Pts',(-11.0168780300001,11.6,0.322665424999986));
#261104=CARTESIAN_POINT('Ctrl Pts',(-11.0140013380001,15.2,0.321505463999987));
#261105=CARTESIAN_POINT('Ctrl Pts',(-11.0140013380001,11.6,0.321505463999987));
#261106=CARTESIAN_POINT('Ctrl Pts',(-11.0111285880001,15.2,0.320349803999989));
#261107=CARTESIAN_POINT('Ctrl Pts',(-11.0111285880001,11.6,0.320349803999988));
#261108=CARTESIAN_POINT('Ctrl Pts',(-11.0082597890001,15.2,0.319198439999986));
#261109=CARTESIAN_POINT('Ctrl Pts',(-11.0082597890001,11.6,0.319198439999985));
#261110=CARTESIAN_POINT('Ctrl Pts',(-11.0053949540001,15.2,0.318051369999988));
#261111=CARTESIAN_POINT('Ctrl Pts',(-11.0053949540001,11.6,0.318051369999987));
#261112=CARTESIAN_POINT('Ctrl Pts',(-11.0025340930001,15.2,0.316908588999985));
#261113=CARTESIAN_POINT('Ctrl Pts',(-11.0025340930001,11.6,0.316908588999984));
#261114=CARTESIAN_POINT('Ctrl Pts',(-10.9996772170001,15.2,0.315770094999985));
#261115=CARTESIAN_POINT('Ctrl Pts',(-10.9996772170001,11.6,0.315770094999985));
#261116=CARTESIAN_POINT('Ctrl Pts',(-10.9968243390001,15.2,0.314635884999985));
#261117=CARTESIAN_POINT('Ctrl Pts',(-10.9968243390001,11.6,0.314635884999985));
#261118=CARTESIAN_POINT('Ctrl Pts',(-10.9939754690001,15.2,0.313505953999984));
#261119=CARTESIAN_POINT('Ctrl Pts',(-10.9939754690001,11.6,0.313505953999984));
#261120=CARTESIAN_POINT('Ctrl Pts',(-10.9911306190001,15.2,0.312380299999986));
#261121=CARTESIAN_POINT('Ctrl Pts',(-10.9911306190001,11.6,0.312380299999985));
#261122=CARTESIAN_POINT('Ctrl Pts',(-10.9882898000001,15.2,0.311258919999986));
#261123=CARTESIAN_POINT('Ctrl Pts',(-10.9882898000001,11.6,0.311258919999986));
#261124=CARTESIAN_POINT('Ctrl Pts',(-10.9854530250001,15.2,0.310141807999984));
#261125=CARTESIAN_POINT('Ctrl Pts',(-10.9854530250001,11.6,0.310141807999984));
#261126=CARTESIAN_POINT('Ctrl Pts',(-10.9826203020001,15.2,0.309028961999989));
#261127=CARTESIAN_POINT('Ctrl Pts',(-10.9826203020001,11.6,0.309028961999988));
#261128=CARTESIAN_POINT('Ctrl Pts',(-10.9797916470001,15.2,0.307920378999986));
#261129=CARTESIAN_POINT('Ctrl Pts',(-10.9797916470001,11.6,0.307920378999986));
#261130=CARTESIAN_POINT('Ctrl Pts',(-10.9769670670001,15.2,0.306816054999985));
#261131=CARTESIAN_POINT('Ctrl Pts',(-10.9769670670001,11.6,0.306816054999985));
#261132=CARTESIAN_POINT('Ctrl Pts',(-10.9741465770001,15.2,0.305715986999986));
#261133=CARTESIAN_POINT('Ctrl Pts',(-10.9741465770001,11.6,0.305715986999985));
#261134=CARTESIAN_POINT('Ctrl Pts',(-10.9713301870001,15.2,0.304620170999983));
#261135=CARTESIAN_POINT('Ctrl Pts',(-10.9713301870001,11.6,0.304620170999983));
#261136=CARTESIAN_POINT('Ctrl Pts',(-10.9685179070001,15.2,0.303528602999985));
#261137=CARTESIAN_POINT('Ctrl Pts',(-10.9685179070001,11.6,0.303528602999985));
#261138=CARTESIAN_POINT('Ctrl Pts',(-10.9657097520001,15.2,0.302441278999983));
#261139=CARTESIAN_POINT('Ctrl Pts',(-10.9657097520001,11.6,0.302441278999983));
#261140=CARTESIAN_POINT('Ctrl Pts',(-10.9629057310001,15.2,0.301358197999986));
#261141=CARTESIAN_POINT('Ctrl Pts',(-10.9629057310001,11.6,0.301358197999985));
#261142=CARTESIAN_POINT('Ctrl Pts',(-10.9601058580001,15.2,0.300279352999984));
#261143=CARTESIAN_POINT('Ctrl Pts',(-10.9601058580001,11.6,0.300279352999983));
#261144=CARTESIAN_POINT('Ctrl Pts',(-10.9573101410001,15.2,0.299204742999986));
#261145=CARTESIAN_POINT('Ctrl Pts',(-10.9573101410001,11.6,0.299204742999985));
#261146=CARTESIAN_POINT('Ctrl Pts',(-10.9545185950001,15.2,0.298134361999987));
#261147=CARTESIAN_POINT('Ctrl Pts',(-10.9545185950001,11.6,0.298134361999986));
#261148=CARTESIAN_POINT('Ctrl Pts',(-10.9517312310001,15.2,0.297068208999987));
#261149=CARTESIAN_POINT('Ctrl Pts',(-10.9517312310001,11.6,0.297068208999986));
#261150=CARTESIAN_POINT('Ctrl Pts',(-10.9489480600001,15.2,0.296006278999985));
#261151=CARTESIAN_POINT('Ctrl Pts',(-10.9489480600001,11.6,0.296006278999985));
#261152=CARTESIAN_POINT('Ctrl Pts',(-10.9461690940001,15.2,0.294948567999986));
#261153=CARTESIAN_POINT('Ctrl Pts',(-10.9461690940001,11.6,0.294948567999986));
#261154=CARTESIAN_POINT('Ctrl Pts',(-10.9433943440001,15.2,0.293895071999986));
#261155=CARTESIAN_POINT('Ctrl Pts',(-10.9433943440001,11.6,0.293895071999985));
#261156=CARTESIAN_POINT('Ctrl Pts',(-10.9406238230001,15.2,0.292845787999987));
#261157=CARTESIAN_POINT('Ctrl Pts',(-10.9406238230001,11.6,0.292845787999986));
#261158=CARTESIAN_POINT('Ctrl Pts',(-10.9378575430001,15.2,0.291800712999986));
#261159=CARTESIAN_POINT('Ctrl Pts',(-10.9378575430001,11.6,0.291800712999985));
#261160=CARTESIAN_POINT('Ctrl Pts',(-10.9350955160001,15.2,0.290759840999986));
#261161=CARTESIAN_POINT('Ctrl Pts',(-10.9350955160001,11.6,0.290759840999985));
#261162=CARTESIAN_POINT('Ctrl Pts',(-10.9323377520001,15.2,0.289723170999987));
#261163=CARTESIAN_POINT('Ctrl Pts',(-10.9323377520001,11.6,0.289723170999987));
#261164=CARTESIAN_POINT('Ctrl Pts',(-10.9295842640001,15.2,0.288690695999985));
#261165=CARTESIAN_POINT('Ctrl Pts',(-10.9295842640001,11.6,0.288690695999984));
#261166=CARTESIAN_POINT('Ctrl Pts',(-10.9268350640001,15.2,0.287662414999983));
#261167=CARTESIAN_POINT('Ctrl Pts',(-10.9268350640001,11.6,0.287662414999982));
#261168=CARTESIAN_POINT('Ctrl Pts',(-10.9240901640001,15.2,0.286638322999986));
#261169=CARTESIAN_POINT('Ctrl Pts',(-10.9240901640001,11.6,0.286638322999985));
#261170=CARTESIAN_POINT('Ctrl Pts',(-10.9213495760001,15.2,0.285618414999984));
#261171=CARTESIAN_POINT('Ctrl Pts',(-10.9213495760001,11.6,0.285618414999984));
#261172=CARTESIAN_POINT('Ctrl Pts',(-10.9186133120001,15.2,0.284602688999982));
#261173=CARTESIAN_POINT('Ctrl Pts',(-10.9186133120001,11.6,0.284602688999982));
#261174=CARTESIAN_POINT('Ctrl Pts',(-10.9158813840001,15.2,0.283591140999988));
#261175=CARTESIAN_POINT('Ctrl Pts',(-10.9158813840001,11.6,0.283591140999988));
#261176=CARTESIAN_POINT('Ctrl Pts',(-10.9131538030001,15.2,0.282583765999984));
#261177=CARTESIAN_POINT('Ctrl Pts',(-10.9131538030001,11.6,0.282583765999984));
#261178=CARTESIAN_POINT('Ctrl Pts',(-10.9104305830001,15.2,0.281580559999988));
#261179=CARTESIAN_POINT('Ctrl Pts',(-10.9104305830001,11.6,0.281580559999987));
#261180=CARTESIAN_POINT('Ctrl Pts',(-10.9077117350001,15.2,0.280581520999985));
#261181=CARTESIAN_POINT('Ctrl Pts',(-10.9077117350001,11.6,0.280581520999985));
#261182=CARTESIAN_POINT('Ctrl Pts',(-10.9049972710001,15.2,0.279586640999985));
#261183=CARTESIAN_POINT('Ctrl Pts',(-10.9049972710001,11.6,0.279586640999984));
#261184=CARTESIAN_POINT('Ctrl Pts',(-10.9022872040001,15.2,0.278595920999987));
#261185=CARTESIAN_POINT('Ctrl Pts',(-10.9022872040001,11.6,0.278595920999986));
#261186=CARTESIAN_POINT('Ctrl Pts',(-10.8995815450001,15.2,0.277609353999986));
#261187=CARTESIAN_POINT('Ctrl Pts',(-10.8995815450001,11.6,0.277609353999985));
#261188=CARTESIAN_POINT('Ctrl Pts',(-10.8968803070001,15.2,0.276626936999986));
#261189=CARTESIAN_POINT('Ctrl Pts',(-10.8968803070001,11.6,0.276626936999986));
#261190=CARTESIAN_POINT('Ctrl Pts',(-10.8941835000001,15.2,0.275648664999988));
#261191=CARTESIAN_POINT('Ctrl Pts',(-10.8941835000001,11.6,0.275648664999987));
#261192=CARTESIAN_POINT('Ctrl Pts',(-10.8914911410001,15.2,0.274674534999986));
#261193=CARTESIAN_POINT('Ctrl Pts',(-10.8914911410001,11.6,0.274674534999985));
#261194=CARTESIAN_POINT('Ctrl Pts',(-10.8888032380001,15.2,0.273704540999984));
#261195=CARTESIAN_POINT('Ctrl Pts',(-10.8888032380001,11.6,0.273704540999983));
#261196=CARTESIAN_POINT('Ctrl Pts',(-10.8861198050001,15.2,0.272738680999982));
#261197=CARTESIAN_POINT('Ctrl Pts',(-10.8861198050001,11.6,0.272738680999982));
#261198=CARTESIAN_POINT('Ctrl Pts',(-10.8834408550001,15.2,0.271776950999989));
#261199=CARTESIAN_POINT('Ctrl Pts',(-10.8834408550001,11.6,0.271776950999989));
#261200=CARTESIAN_POINT('Ctrl Pts',(-10.8807663990001,15.2,0.270819344999986));
#261201=CARTESIAN_POINT('Ctrl Pts',(-10.8807663990001,11.6,0.270819344999986));
#261202=CARTESIAN_POINT('Ctrl Pts',(-10.8780964490001,15.2,0.269865860999987));
#261203=CARTESIAN_POINT('Ctrl Pts',(-10.8780964490001,11.6,0.269865860999987));
#261204=CARTESIAN_POINT('Ctrl Pts',(-10.8754310200001,15.2,0.268916491999986));
#261205=CARTESIAN_POINT('Ctrl Pts',(-10.8754310200001,11.6,0.268916491999986));
#261206=CARTESIAN_POINT('Ctrl Pts',(-10.8727701220001,15.2,0.267971236999984));
#261207=CARTESIAN_POINT('Ctrl Pts',(-10.8727701220001,11.6,0.267971236999984));
#261208=CARTESIAN_POINT('Ctrl Pts',(-10.8701137680001,15.2,0.267030089999984));
#261209=CARTESIAN_POINT('Ctrl Pts',(-10.8701137680001,11.6,0.267030089999984));
#261210=CARTESIAN_POINT('Ctrl Pts',(-10.8674619700001,15.2,0.266093045999987));
#261211=CARTESIAN_POINT('Ctrl Pts',(-10.8674619700001,11.6,0.266093045999986));
#261212=CARTESIAN_POINT('Ctrl Pts',(-10.8648147410001,15.2,0.265160102999986));
#261213=CARTESIAN_POINT('Ctrl Pts',(-10.8648147410001,11.6,0.265160102999986));
#261214=CARTESIAN_POINT('Ctrl Pts',(-10.8621720950001,15.2,0.264231254999987));
#261215=CARTESIAN_POINT('Ctrl Pts',(-10.8621720950001,11.6,0.264231254999987));
#261216=CARTESIAN_POINT('Ctrl Pts',(-10.8595340430001,15.2,0.263306497999984));
#261217=CARTESIAN_POINT('Ctrl Pts',(-10.8595340430001,11.6,0.263306497999984));
#261218=CARTESIAN_POINT('Ctrl Pts',(-10.8569005980001,15.2,0.262385827999987));
#261219=CARTESIAN_POINT('Ctrl Pts',(-10.8569005980001,11.6,0.262385827999986));
#261220=CARTESIAN_POINT('Ctrl Pts',(-10.8542717720001,15.2,0.261469240999985));
#261221=CARTESIAN_POINT('Ctrl Pts',(-10.8542717720001,11.6,0.261469240999985));
#261222=CARTESIAN_POINT('Ctrl Pts',(-10.8516475780001,15.2,0.260556731999984));
#261223=CARTESIAN_POINT('Ctrl Pts',(-10.8516475780001,11.6,0.260556731999983));
#261224=CARTESIAN_POINT('Ctrl Pts',(-10.8490280300001,15.2,0.259648296999986));
#261225=CARTESIAN_POINT('Ctrl Pts',(-10.8490280300001,11.6,0.259648296999985));
#261226=CARTESIAN_POINT('Ctrl Pts',(-10.8464131390001,15.2,0.258743930999987));
#261227=CARTESIAN_POINT('Ctrl Pts',(-10.8464131390001,11.6,0.258743930999987));
#261228=CARTESIAN_POINT('Ctrl Pts',(-10.8438029180001,15.2,0.257843629999983));
#261229=CARTESIAN_POINT('Ctrl Pts',(-10.8438029180001,11.6,0.257843629999983));
#261230=CARTESIAN_POINT('Ctrl Pts',(-10.8411973810001,15.2,0.256947389999986));
#261231=CARTESIAN_POINT('Ctrl Pts',(-10.8411973810001,11.6,0.256947389999986));
#261232=CARTESIAN_POINT('Ctrl Pts',(-10.8385965390001,15.2,0.256055205999988));
#261233=CARTESIAN_POINT('Ctrl Pts',(-10.8385965390001,11.6,0.256055205999987));
#261234=CARTESIAN_POINT('Ctrl Pts',(-10.8360004070001,15.2,0.255167072999987));
#261235=CARTESIAN_POINT('Ctrl Pts',(-10.8360004070001,11.6,0.255167072999986));
#261236=CARTESIAN_POINT('Ctrl Pts',(-10.8334089940001,15.2,0.254282987999983));
#261237=CARTESIAN_POINT('Ctrl Pts',(-10.8334089940001,11.6,0.254282987999983));
#261238=CARTESIAN_POINT('Ctrl Pts',(-10.8308223180001,15.2,0.253402943999985));
#261239=CARTESIAN_POINT('Ctrl Pts',(-10.8308223180001,11.6,0.253402943999985));
#261240=CARTESIAN_POINT('Ctrl Pts',(-10.8282403890001,15.2,0.252526939999989));
#261241=CARTESIAN_POINT('Ctrl Pts',(-10.8282403890001,11.6,0.252526939999988));
#261242=CARTESIAN_POINT('Ctrl Pts',(-10.8256632200001,15.2,0.251654968999984));
#261243=CARTESIAN_POINT('Ctrl Pts',(-10.8256632200001,11.6,0.251654968999983));
#261244=CARTESIAN_POINT('Ctrl Pts',(-10.8230908230001,15.2,0.250787025999983));
#261245=CARTESIAN_POINT('Ctrl Pts',(-10.8230908230001,11.6,0.250787025999983));
#261246=CARTESIAN_POINT('Ctrl Pts',(-10.8205232130001,15.2,0.249923108999983));
#261247=CARTESIAN_POINT('Ctrl Pts',(-10.8205232130001,11.6,0.249923108999983));
#261248=CARTESIAN_POINT('Ctrl Pts',(-10.8179604030001,15.2,0.249063209999987));
#261249=CARTESIAN_POINT('Ctrl Pts',(-10.8179604030001,11.6,0.249063209999986));
#261250=CARTESIAN_POINT('Ctrl Pts',(-10.8154024050001,15.2,0.248207326999985));
#261251=CARTESIAN_POINT('Ctrl Pts',(-10.8154024050001,11.6,0.248207326999985));
#261252=CARTESIAN_POINT('Ctrl Pts',(-10.8128492330001,15.2,0.247355453999987));
#261253=CARTESIAN_POINT('Ctrl Pts',(-10.8128492330001,11.6,0.247355453999986));
#261254=CARTESIAN_POINT('Ctrl Pts',(-10.8103008990001,15.2,0.246507586999982));
#261255=CARTESIAN_POINT('Ctrl Pts',(-10.8103008990001,11.6,0.246507586999982));
#261256=CARTESIAN_POINT('Ctrl Pts',(-10.8077574170001,15.2,0.245663720999989));
#261257=CARTESIAN_POINT('Ctrl Pts',(-10.8077574170001,11.6,0.245663720999989));
#261258=CARTESIAN_POINT('Ctrl Pts',(-10.8052187990001,15.2,0.244823850999989));
#261259=CARTESIAN_POINT('Ctrl Pts',(-10.8052187990001,11.6,0.244823850999988));
#261260=CARTESIAN_POINT('Ctrl Pts',(-10.8026850610001,15.2,0.243987971999986));
#261261=CARTESIAN_POINT('Ctrl Pts',(-10.8026850610001,11.6,0.243987971999986));
#261262=CARTESIAN_POINT('Ctrl Pts',(-10.8001562130001,15.2,0.243156080999984));
#261263=CARTESIAN_POINT('Ctrl Pts',(-10.8001562130001,11.6,0.243156080999984));
#261264=CARTESIAN_POINT('Ctrl Pts',(-10.7976322700001,15.2,0.242328170999984));
#261265=CARTESIAN_POINT('Ctrl Pts',(-10.7976322700001,11.6,0.242328170999983));
#261266=CARTESIAN_POINT('Ctrl Pts',(-10.7951132440001,15.2,0.241504237999983));
#261267=CARTESIAN_POINT('Ctrl Pts',(-10.7951132440001,11.6,0.241504237999983));
#261268=CARTESIAN_POINT('Ctrl Pts',(-10.7925991510001,15.2,0.240684276999983));
#261269=CARTESIAN_POINT('Ctrl Pts',(-10.7925991510001,11.6,0.240684276999982));
#261270=CARTESIAN_POINT('Ctrl Pts',(-10.7900900010001,15.2,0.239868283999982));
#261271=CARTESIAN_POINT('Ctrl Pts',(-10.7900900010001,11.6,0.239868283999982));
#261272=CARTESIAN_POINT('Ctrl Pts',(-10.7875858100001,15.2,0.239056253999985));
#261273=CARTESIAN_POINT('Ctrl Pts',(-10.7875858100001,11.6,0.239056253999985));
#261274=CARTESIAN_POINT('Ctrl Pts',(-10.7850865910001,15.2,0.238248179999987));
#261275=CARTESIAN_POINT('Ctrl Pts',(-10.7850865910001,11.6,0.238248179999986));
#261276=CARTESIAN_POINT('Ctrl Pts',(-10.7825923560001,15.2,0.237444060999987));
#261277=CARTESIAN_POINT('Ctrl Pts',(-10.7825923560001,11.6,0.237444060999987));
#261278=CARTESIAN_POINT('Ctrl Pts',(-10.7801031190001,15.2,0.236643886999985));
#261279=CARTESIAN_POINT('Ctrl Pts',(-10.7801031190001,11.6,0.236643886999985));
#261280=CARTESIAN_POINT('Ctrl Pts',(-10.7776188950001,15.2,0.235847656999986));
#261281=CARTESIAN_POINT('Ctrl Pts',(-10.7776188950001,11.6,0.235847656999985));
#261282=CARTESIAN_POINT('Ctrl Pts',(-10.7751396960001,15.2,0.235055364999983));
#261283=CARTESIAN_POINT('Ctrl Pts',(-10.7751396960001,11.6,0.235055364999983));
#261284=CARTESIAN_POINT('Ctrl Pts',(-10.7726655360001,15.2,0.234267004999986));
#261285=CARTESIAN_POINT('Ctrl Pts',(-10.7726655360001,11.6,0.234267004999986));
#261286=CARTESIAN_POINT('Ctrl Pts',(-10.7701964290001,15.2,0.233482572999986));
#261287=CARTESIAN_POINT('Ctrl Pts',(-10.7701964290001,11.6,0.233482572999985));
#261288=CARTESIAN_POINT('Ctrl Pts',(-10.7677323890001,15.2,0.232702063999985));
#261289=CARTESIAN_POINT('Ctrl Pts',(-10.7677323890001,11.6,0.232702063999985));
#261290=CARTESIAN_POINT('Ctrl Pts',(-10.7652734280001,15.2,0.231925471999985));
#261291=CARTESIAN_POINT('Ctrl Pts',(-10.7652734280001,11.6,0.231925471999985));
#261292=CARTESIAN_POINT('Ctrl Pts',(-10.7628195610001,15.2,0.231152792999989));
#261293=CARTESIAN_POINT('Ctrl Pts',(-10.7628195610001,11.6,0.231152792999989));
#261294=CARTESIAN_POINT('Ctrl Pts',(-10.7603708020001,15.2,0.230384019999987));
#261295=CARTESIAN_POINT('Ctrl Pts',(-10.7603708020001,11.6,0.230384019999987));
#261296=CARTESIAN_POINT('Ctrl Pts',(-10.7579271630001,15.2,0.229619148999984));
#261297=CARTESIAN_POINT('Ctrl Pts',(-10.7579271630001,11.6,0.229619148999984));
#261298=CARTESIAN_POINT('Ctrl Pts',(-10.7554886610001,15.2,0.228858175999989));
#261299=CARTESIAN_POINT('Ctrl Pts',(-10.7554886610001,11.6,0.228858175999988));
#261300=CARTESIAN_POINT('Ctrl Pts',(-10.7530553070001,15.2,0.228101093999986));
#261301=CARTESIAN_POINT('Ctrl Pts',(-10.7530553070001,11.6,0.228101093999986));
#261302=CARTESIAN_POINT('Ctrl Pts',(-10.7506271160001,15.2,0.227347897999985));
#261303=CARTESIAN_POINT('Ctrl Pts',(-10.7506271160001,11.6,0.227347897999985));
#261304=CARTESIAN_POINT('Ctrl Pts',(-10.7482041010001,15.2,0.226598583999986));
#261305=CARTESIAN_POINT('Ctrl Pts',(-10.7482041010001,11.6,0.226598583999986));
#261306=CARTESIAN_POINT('Ctrl Pts',(-10.7457862770001,15.2,0.225853145999988));
#261307=CARTESIAN_POINT('Ctrl Pts',(-10.7457862770001,11.6,0.225853145999988));
#261308=CARTESIAN_POINT('Ctrl Pts',(-10.7433736600001,15.2,0.225111577999986));
#261309=CARTESIAN_POINT('Ctrl Pts',(-10.7433736600001,11.6,0.225111577999985));
#261310=CARTESIAN_POINT('Ctrl Pts',(-10.7409662590001,15.2,0.224373874999984));
#261311=CARTESIAN_POINT('Ctrl Pts',(-10.7409662590001,11.6,0.224373874999983));
#261312=CARTESIAN_POINT('Ctrl Pts',(-10.7385640920001,15.2,0.223640032999985));
#261313=CARTESIAN_POINT('Ctrl Pts',(-10.7385640920001,11.6,0.223640032999985));
#261314=CARTESIAN_POINT('Ctrl Pts',(-10.7361671710001,15.2,0.222910043999986));
#261315=CARTESIAN_POINT('Ctrl Pts',(-10.7361671710001,11.6,0.222910043999986));
#261316=CARTESIAN_POINT('Ctrl Pts',(-10.7337755120001,15.2,0.222183903999986));
#261317=CARTESIAN_POINT('Ctrl Pts',(-10.7337755120001,11.6,0.222183903999986));
#261318=CARTESIAN_POINT('Ctrl Pts',(-10.7313891280001,15.2,0.221461608999984));
#261319=CARTESIAN_POINT('Ctrl Pts',(-10.7313891280001,11.6,0.221461608999984));
#261320=CARTESIAN_POINT('Ctrl Pts',(-10.7290080330001,15.2,0.220743150999985));
#261321=CARTESIAN_POINT('Ctrl Pts',(-10.7290080330001,11.6,0.220743150999984));
#261322=CARTESIAN_POINT('Ctrl Pts',(-10.7266322420001,15.2,0.220028526999982));
#261323=CARTESIAN_POINT('Ctrl Pts',(-10.7266322420001,11.6,0.220028526999982));
#261324=CARTESIAN_POINT('Ctrl Pts',(-10.7242617690001,15.2,0.219317729999986));
#261325=CARTESIAN_POINT('Ctrl Pts',(-10.7242617690001,11.6,0.219317729999986));
#261326=CARTESIAN_POINT('Ctrl Pts',(-10.7218966280001,15.2,0.218610753999986));
#261327=CARTESIAN_POINT('Ctrl Pts',(-10.7218966280001,11.6,0.218610753999986));
#261328=CARTESIAN_POINT('Ctrl Pts',(-10.7195368330001,15.2,0.217907592999986));
#261329=CARTESIAN_POINT('Ctrl Pts',(-10.7195368330001,11.6,0.217907592999986));
#261330=CARTESIAN_POINT('Ctrl Pts',(-10.7171823990001,15.2,0.217208243999987));
#261331=CARTESIAN_POINT('Ctrl Pts',(-10.7171823990001,11.6,0.217208243999986));
#261332=CARTESIAN_POINT('Ctrl Pts',(-10.7148333410001,15.2,0.216512699999987));
#261333=CARTESIAN_POINT('Ctrl Pts',(-10.7148333410001,11.6,0.216512699999986));
#261334=CARTESIAN_POINT('Ctrl Pts',(-10.7124896730001,15.2,0.215820953999986));
#261335=CARTESIAN_POINT('Ctrl Pts',(-10.7124896730001,11.6,0.215820953999985));
#261336=CARTESIAN_POINT('Ctrl Pts',(-10.7101514080001,15.2,0.215133002999988));
#261337=CARTESIAN_POINT('Ctrl Pts',(-10.7101514080001,11.6,0.215133002999987));
#261338=CARTESIAN_POINT('Ctrl Pts',(-10.7078185620001,15.2,0.214448838999988));
#261339=CARTESIAN_POINT('Ctrl Pts',(-10.7078185620001,11.6,0.214448838999987));
#261340=CARTESIAN_POINT('Ctrl Pts',(-10.7054911500001,15.2,0.213768457999985));
#261341=CARTESIAN_POINT('Ctrl Pts',(-10.7054911500001,11.6,0.213768457999985));
#261342=CARTESIAN_POINT('Ctrl Pts',(-10.7031691860001,15.2,0.213091852999985));
#261343=CARTESIAN_POINT('Ctrl Pts',(-10.7031691860001,11.6,0.213091852999984));
#261344=CARTESIAN_POINT('Ctrl Pts',(-10.7008526850001,15.2,0.212419018999985));
#261345=CARTESIAN_POINT('Ctrl Pts',(-10.7008526850001,11.6,0.212419018999985));
#261346=CARTESIAN_POINT('Ctrl Pts',(-10.6985416600001,15.2,0.211749948999986));
#261347=CARTESIAN_POINT('Ctrl Pts',(-10.6985416600001,11.6,0.211749948999986));
#261348=CARTESIAN_POINT('Ctrl Pts',(-10.6962361280001,15.2,0.211084637999988));
#261349=CARTESIAN_POINT('Ctrl Pts',(-10.6962361280001,11.6,0.211084637999987));
#261350=CARTESIAN_POINT('Ctrl Pts',(-10.6939361020001,15.2,0.210423081999984));
#261351=CARTESIAN_POINT('Ctrl Pts',(-10.6939361020001,11.6,0.210423081999984));
#261352=CARTESIAN_POINT('Ctrl Pts',(-10.6916415980001,15.2,0.209765271999984));
#261353=CARTESIAN_POINT('Ctrl Pts',(-10.6916415980001,11.6,0.209765271999984));
#261354=CARTESIAN_POINT('Ctrl Pts',(-10.6893526300001,15.2,0.209111201999987));
#261355=CARTESIAN_POINT('Ctrl Pts',(-10.6893526300001,11.6,0.209111201999987));
#261356=CARTESIAN_POINT('Ctrl Pts',(-10.6870692130001,15.2,0.208460869999989));
#261357=CARTESIAN_POINT('Ctrl Pts',(-10.6870692130001,11.6,0.208460869999989));
#261358=CARTESIAN_POINT('Ctrl Pts',(-10.6847913630001,15.2,0.207814266999984));
#261359=CARTESIAN_POINT('Ctrl Pts',(-10.6847913630001,11.6,0.207814266999983));
#261360=CARTESIAN_POINT('Ctrl Pts',(-10.6825190920001,15.2,0.207171386999985));
#261361=CARTESIAN_POINT('Ctrl Pts',(-10.6825190920001,11.6,0.207171386999984));
#261362=CARTESIAN_POINT('Ctrl Pts',(-10.6802524190001,15.2,0.206532224999982));
#261363=CARTESIAN_POINT('Ctrl Pts',(-10.6802524190001,11.6,0.206532224999982));
#261364=CARTESIAN_POINT('Ctrl Pts',(-10.6779913570001,15.2,0.205896773999985));
#261365=CARTESIAN_POINT('Ctrl Pts',(-10.6779913570001,11.6,0.205896773999985));
#261366=CARTESIAN_POINT('Ctrl Pts',(-10.6757359200001,15.2,0.205265028999988));
#261367=CARTESIAN_POINT('Ctrl Pts',(-10.6757359200001,11.6,0.205265028999988));
#261368=CARTESIAN_POINT('Ctrl Pts',(-10.6734861240001,15.2,0.204636982999986));
#261369=CARTESIAN_POINT('Ctrl Pts',(-10.6734861240001,11.6,0.204636982999986));
#261370=CARTESIAN_POINT('Ctrl Pts',(-10.6712419860001,15.2,0.204012629999983));
#261371=CARTESIAN_POINT('Ctrl Pts',(-10.6712419860001,11.6,0.204012629999983));
#261372=CARTESIAN_POINT('Ctrl Pts',(-10.6690035190001,15.2,0.203391963999984));
#261373=CARTESIAN_POINT('Ctrl Pts',(-10.6690035190001,11.6,0.203391963999983));
#261374=CARTESIAN_POINT('Ctrl Pts',(-10.6667707370001,15.2,0.202774979999987));
#261375=CARTESIAN_POINT('Ctrl Pts',(-10.6667707370001,11.6,0.202774979999986));
#261376=CARTESIAN_POINT('Ctrl Pts',(-10.6645436590001,15.2,0.202161669999987));
#261377=CARTESIAN_POINT('Ctrl Pts',(-10.6645436590001,11.6,0.202161669999987));
#261378=CARTESIAN_POINT('Ctrl Pts',(-10.6623222980001,15.2,0.201552028999985));
#261379=CARTESIAN_POINT('Ctrl Pts',(-10.6623222980001,11.6,0.201552028999985));
#261380=CARTESIAN_POINT('Ctrl Pts',(-10.6601066700001,15.2,0.200946048999988));
#261381=CARTESIAN_POINT('Ctrl Pts',(-10.6601066700001,11.6,0.200946048999988));
#261382=CARTESIAN_POINT('Ctrl Pts',(-10.6578967890001,15.2,0.200343724999983));
#261383=CARTESIAN_POINT('Ctrl Pts',(-10.6578967890001,11.6,0.200343724999982));
#261384=CARTESIAN_POINT('Ctrl Pts',(-10.6556926720001,15.2,0.199745050999987));
#261385=CARTESIAN_POINT('Ctrl Pts',(-10.6556926720001,11.6,0.199745050999986));
#261386=CARTESIAN_POINT('Ctrl Pts',(-10.6534943330001,15.2,0.199150019999985));
#261387=CARTESIAN_POINT('Ctrl Pts',(-10.6534943330001,11.6,0.199150019999985));
#261388=CARTESIAN_POINT('Ctrl Pts',(-10.6513017900001,15.2,0.198558625999983));
#261389=CARTESIAN_POINT('Ctrl Pts',(-10.6513017900001,11.6,0.198558625999982));
#261390=CARTESIAN_POINT('Ctrl Pts',(-10.6491150560001,15.2,0.197970862999988));
#261391=CARTESIAN_POINT('Ctrl Pts',(-10.6491150560001,11.6,0.197970862999987));
#261392=CARTESIAN_POINT('Ctrl Pts',(-10.6469341480001,15.2,0.197386722999986));
#261393=CARTESIAN_POINT('Ctrl Pts',(-10.6469341480001,11.6,0.197386722999985));
#261394=CARTESIAN_POINT('Ctrl Pts',(-10.6447590820001,15.2,0.196806200999986));
#261395=CARTESIAN_POINT('Ctrl Pts',(-10.6447590820001,11.6,0.196806200999986));
#261396=CARTESIAN_POINT('Ctrl Pts',(-10.6425898720001,15.2,0.196229288999987));
#261397=CARTESIAN_POINT('Ctrl Pts',(-10.6425898720001,11.6,0.196229288999987));
#261398=CARTESIAN_POINT('Ctrl Pts',(-10.6404265340001,15.2,0.195655982999985));
#261399=CARTESIAN_POINT('Ctrl Pts',(-10.6404265340001,11.6,0.195655982999984));
#261400=CARTESIAN_POINT('Ctrl Pts',(-10.6382690860001,15.2,0.195086272999987));
#261401=CARTESIAN_POINT('Ctrl Pts',(-10.6382690860001,11.6,0.195086272999986));
#261402=CARTESIAN_POINT('Ctrl Pts',(-10.6361175410001,15.2,0.194520154999989));
#261403=CARTESIAN_POINT('Ctrl Pts',(-10.6361175410001,11.6,0.194520154999988));
#261404=CARTESIAN_POINT('Ctrl Pts',(-10.6339719170001,15.2,0.193957621999985));
#261405=CARTESIAN_POINT('Ctrl Pts',(-10.6339719170001,11.6,0.193957621999985));
#261406=CARTESIAN_POINT('Ctrl Pts',(-10.6318322290001,15.2,0.193398666999984));
#261407=CARTESIAN_POINT('Ctrl Pts',(-10.6318322290001,11.6,0.193398666999984));
#261408=CARTESIAN_POINT('Ctrl Pts',(-10.6296984920001,15.2,0.192843283999986));
#261409=CARTESIAN_POINT('Ctrl Pts',(-10.6296984920001,11.6,0.192843283999986));
#261410=CARTESIAN_POINT('Ctrl Pts',(-10.6275707240001,15.2,0.192291463999985));
#261411=CARTESIAN_POINT('Ctrl Pts',(-10.6275707240001,11.6,0.192291463999985));
#261412=CARTESIAN_POINT('Ctrl Pts',(-10.6254489400001,15.2,0.191743201999985));
#261413=CARTESIAN_POINT('Ctrl Pts',(-10.6254489400001,11.6,0.191743201999985));
#261414=CARTESIAN_POINT('Ctrl Pts',(-10.6233331560001,15.2,0.191198491999987));
#261415=CARTESIAN_POINT('Ctrl Pts',(-10.6233331560001,11.6,0.191198491999986));
#261416=CARTESIAN_POINT('Ctrl Pts',(-10.6212233880001,15.2,0.190657325999983));
#261417=CARTESIAN_POINT('Ctrl Pts',(-10.6212233880001,11.6,0.190657325999983));
#261418=CARTESIAN_POINT('Ctrl Pts',(-10.6191196530001,15.2,0.190119695999984));
#261419=CARTESIAN_POINT('Ctrl Pts',(-10.6191196530001,11.6,0.190119695999984));
#261420=CARTESIAN_POINT('Ctrl Pts',(-10.6170219660001,15.2,0.189585598999984));
#261421=CARTESIAN_POINT('Ctrl Pts',(-10.6170219660001,11.6,0.189585598999984));
#261422=CARTESIAN_POINT('Ctrl Pts',(-10.6149303440001,15.2,0.189055023999987));
#261423=CARTESIAN_POINT('Ctrl Pts',(-10.6149303440001,11.6,0.189055023999986));
#261424=CARTESIAN_POINT('Ctrl Pts',(-10.6128448030001,15.2,0.188527964999987));
#261425=CARTESIAN_POINT('Ctrl Pts',(-10.6128448030001,11.6,0.188527964999987));
#261426=CARTESIAN_POINT('Ctrl Pts',(-10.6107653600001,15.2,0.188004416999985));
#261427=CARTESIAN_POINT('Ctrl Pts',(-10.6107653600001,11.6,0.188004416999985));
#261428=CARTESIAN_POINT('Ctrl Pts',(-10.6086920310001,15.2,0.187484370999984));
#261429=CARTESIAN_POINT('Ctrl Pts',(-10.6086920310001,11.6,0.187484370999984));
#261430=CARTESIAN_POINT('Ctrl Pts',(-10.6066248330001,15.2,0.186967819999988));
#261431=CARTESIAN_POINT('Ctrl Pts',(-10.6066248330001,11.6,0.186967819999988));
#261432=CARTESIAN_POINT('Ctrl Pts',(-10.6045637800001,15.2,0.186454757999983));
#261433=CARTESIAN_POINT('Ctrl Pts',(-10.6045637800001,11.6,0.186454757999983));
#261434=CARTESIAN_POINT('Ctrl Pts',(-10.6025088930001,15.2,0.185945177999987));
#261435=CARTESIAN_POINT('Ctrl Pts',(-10.6025088930001,11.6,0.185945177999986));
#261436=CARTESIAN_POINT('Ctrl Pts',(-10.6004601840001,15.2,0.185439070999984));
#261437=CARTESIAN_POINT('Ctrl Pts',(-10.6004601840001,11.6,0.185439070999984));
#261438=CARTESIAN_POINT('Ctrl Pts',(-10.5984176730001,15.2,0.184936432999985));
#261439=CARTESIAN_POINT('Ctrl Pts',(-10.5984176730001,11.6,0.184936432999984));
#261440=CARTESIAN_POINT('Ctrl Pts',(-10.5963813760001,15.2,0.184437252999987));
#261441=CARTESIAN_POINT('Ctrl Pts',(-10.5963813760001,11.6,0.184437252999987));
#261442=CARTESIAN_POINT('Ctrl Pts',(-10.5943513080001,15.2,0.183941525999987));
#261443=CARTESIAN_POINT('Ctrl Pts',(-10.5943513080001,11.6,0.183941525999986));
#261444=CARTESIAN_POINT('Ctrl Pts',(-10.5923274870001,15.2,0.183449243999987));
#261445=CARTESIAN_POINT('Ctrl Pts',(-10.5923274870001,11.6,0.183449243999986));
#261446=CARTESIAN_POINT('Ctrl Pts',(-10.5903099300001,15.2,0.182960399999987));
#261447=CARTESIAN_POINT('Ctrl Pts',(-10.5903099300001,11.6,0.182960399999987));
#261448=CARTESIAN_POINT('Ctrl Pts',(-10.5882986550001,15.2,0.182474987999988));
#261449=CARTESIAN_POINT('Ctrl Pts',(-10.5882986550001,11.6,0.182474987999987));
#261450=CARTESIAN_POINT('Ctrl Pts',(-10.5862936760001,15.2,0.181992998999987));
#261451=CARTESIAN_POINT('Ctrl Pts',(-10.5862936760001,11.6,0.181992998999986));
#261452=CARTESIAN_POINT('Ctrl Pts',(-10.5842950130001,15.2,0.181514424999989));
#261453=CARTESIAN_POINT('Ctrl Pts',(-10.5842950130001,11.6,0.181514424999988));
#261454=CARTESIAN_POINT('Ctrl Pts',(-10.5823026810001,15.2,0.181039259999984));
#261455=CARTESIAN_POINT('Ctrl Pts',(-10.5823026810001,11.6,0.181039259999984));
#261456=CARTESIAN_POINT('Ctrl Pts',(-10.5803166980001,15.2,0.180567494999986));
#261457=CARTESIAN_POINT('Ctrl Pts',(-10.5803166980001,11.6,0.180567494999985));
#261458=CARTESIAN_POINT('Ctrl Pts',(-10.5783370810001,15.2,0.180099124999984));
#261459=CARTESIAN_POINT('Ctrl Pts',(-10.5783370810001,11.6,0.180099124999983));
#261460=CARTESIAN_POINT('Ctrl Pts',(-10.5763638480001,15.2,0.179634139999987));
#261461=CARTESIAN_POINT('Ctrl Pts',(-10.5763638480001,11.6,0.179634139999986));
#261462=CARTESIAN_POINT('Ctrl Pts',(-10.5743970150001,15.2,0.179172532999985));
#261463=CARTESIAN_POINT('Ctrl Pts',(-10.5743970150001,11.6,0.179172532999984));
#261464=CARTESIAN_POINT('Ctrl Pts',(-10.5724365990001,15.2,0.178714295999987));
#261465=CARTESIAN_POINT('Ctrl Pts',(-10.5724365990001,11.6,0.178714295999986));
#261466=CARTESIAN_POINT('Ctrl Pts',(-10.5704826190001,15.2,0.178259422999982));
#261467=CARTESIAN_POINT('Ctrl Pts',(-10.5704826190001,11.6,0.178259422999982));
#261468=CARTESIAN_POINT('Ctrl Pts',(-10.5685350920001,15.2,0.177807903999985));
#261469=CARTESIAN_POINT('Ctrl Pts',(-10.5685350920001,11.6,0.177807903999984));
#261470=CARTESIAN_POINT('Ctrl Pts',(-10.5665940340001,15.2,0.177359733999989));
#261471=CARTESIAN_POINT('Ctrl Pts',(-10.5665940340001,11.6,0.177359733999988));
#261472=CARTESIAN_POINT('Ctrl Pts',(-10.5646594650001,15.2,0.176914901999985));
#261473=CARTESIAN_POINT('Ctrl Pts',(-10.5646594650001,11.6,0.176914901999984));
#261474=CARTESIAN_POINT('Ctrl Pts',(-10.5627314000001,15.2,0.176473403999986));
#261475=CARTESIAN_POINT('Ctrl Pts',(-10.5627314000001,11.6,0.176473403999986));
#261476=CARTESIAN_POINT('Ctrl Pts',(-10.5608098580001,15.2,0.176035227999982));
#261477=CARTESIAN_POINT('Ctrl Pts',(-10.5608098580001,11.6,0.176035227999982));
#261478=CARTESIAN_POINT('Ctrl Pts',(-10.5588948570001,15.2,0.175600368999986));
#261479=CARTESIAN_POINT('Ctrl Pts',(-10.5588948570001,11.6,0.175600368999986));
#261480=CARTESIAN_POINT('Ctrl Pts',(-10.5569864130001,15.2,0.175168818999989));
#261481=CARTESIAN_POINT('Ctrl Pts',(-10.5569864130001,11.6,0.175168818999988));
#261482=CARTESIAN_POINT('Ctrl Pts',(-10.5550845460001,15.2,0.174740567999985));
#261483=CARTESIAN_POINT('Ctrl Pts',(-10.5550845460001,11.6,0.174740567999984));
#261484=CARTESIAN_POINT('Ctrl Pts',(-10.5531892730001,15.2,0.174315608999986));
#261485=CARTESIAN_POINT('Ctrl Pts',(-10.5531892730001,11.6,0.174315608999986));
#261486=CARTESIAN_POINT('Ctrl Pts',(-10.5513006120001,15.2,0.173893933999985));
#261487=CARTESIAN_POINT('Ctrl Pts',(-10.5513006120001,11.6,0.173893933999984));
#261488=CARTESIAN_POINT('Ctrl Pts',(-10.5494185790001,15.2,0.173475535999987));
#261489=CARTESIAN_POINT('Ctrl Pts',(-10.5494185790001,11.6,0.173475535999987));
#261490=CARTESIAN_POINT('Ctrl Pts',(-10.5475431950001,15.2,0.173060405999985));
#261491=CARTESIAN_POINT('Ctrl Pts',(-10.5475431950001,11.6,0.173060405999985));
#261492=CARTESIAN_POINT('Ctrl Pts',(-10.5456744770001,15.2,0.172648534999986));
#261493=CARTESIAN_POINT('Ctrl Pts',(-10.5456744770001,11.6,0.172648534999986));
#261494=CARTESIAN_POINT('Ctrl Pts',(-10.5438124430001,15.2,0.172239915999985));
#261495=CARTESIAN_POINT('Ctrl Pts',(-10.5438124430001,11.6,0.172239915999985));
#261496=CARTESIAN_POINT('Ctrl Pts',(-10.5419571120001,15.2,0.171834540999987));
#261497=CARTESIAN_POINT('Ctrl Pts',(-10.5419571120001,11.6,0.171834540999986));
#261498=CARTESIAN_POINT('Ctrl Pts',(-10.5401085000001,15.2,0.171432399999984));
#261499=CARTESIAN_POINT('Ctrl Pts',(-10.5401085000001,11.6,0.171432399999984));
#261500=CARTESIAN_POINT('Ctrl Pts',(-10.5382666270001,15.2,0.171033485999987));
#261501=CARTESIAN_POINT('Ctrl Pts',(-10.5382666270001,11.6,0.171033485999987));
#261502=CARTESIAN_POINT('Ctrl Pts',(-10.5364315110001,15.2,0.170637790999986));
#261503=CARTESIAN_POINT('Ctrl Pts',(-10.5364315110001,11.6,0.170637790999985));
#261504=CARTESIAN_POINT('Ctrl Pts',(-10.5346031720001,15.2,0.170245304999987));
#261505=CARTESIAN_POINT('Ctrl Pts',(-10.5346031720001,11.6,0.170245304999987));
#261506=CARTESIAN_POINT('Ctrl Pts',(-10.5327816250001,15.2,0.169856020999983));
#261507=CARTESIAN_POINT('Ctrl Pts',(-10.5327816250001,11.6,0.169856020999983));
#261508=CARTESIAN_POINT('Ctrl Pts',(-10.5309668930001,15.2,0.169469929999986));
#261509=CARTESIAN_POINT('Ctrl Pts',(-10.5309668930001,11.6,0.169469929999985));
#261510=CARTESIAN_POINT('Ctrl Pts',(-10.5291589900001,15.2,0.169087022999985));
#261511=CARTESIAN_POINT('Ctrl Pts',(-10.5291589900001,11.6,0.169087022999985));
#261512=CARTESIAN_POINT('Ctrl Pts',(-10.5273579390001,15.2,0.168707291999985));
#261513=CARTESIAN_POINT('Ctrl Pts',(-10.5273579390001,11.6,0.168707291999985));
#261514=CARTESIAN_POINT('Ctrl Pts',(-10.5255637550001,15.2,0.168330728999986));
#261515=CARTESIAN_POINT('Ctrl Pts',(-10.5255637550001,11.6,0.168330728999985));
#261516=CARTESIAN_POINT('Ctrl Pts',(-10.5237764590001,15.2,0.167957323999985));
#261517=CARTESIAN_POINT('Ctrl Pts',(-10.5237764590001,11.6,0.167957323999985));
#261518=CARTESIAN_POINT('Ctrl Pts',(-10.5219960680001,15.2,0.167587068999988));
#261519=CARTESIAN_POINT('Ctrl Pts',(-10.5219960680001,11.6,0.167587068999988));
#261520=CARTESIAN_POINT('Ctrl Pts',(-10.5202226040001,15.2,0.167219955999984));
#261521=CARTESIAN_POINT('Ctrl Pts',(-10.5202226040001,11.6,0.167219955999984));
#261522=CARTESIAN_POINT('Ctrl Pts',(-10.5184560840001,15.2,0.166855974999987));
#261523=CARTESIAN_POINT('Ctrl Pts',(-10.5184560840001,11.6,0.166855974999986));
#261524=CARTESIAN_POINT('Ctrl Pts',(-10.5166965270001,15.2,0.166495116999985));
#261525=CARTESIAN_POINT('Ctrl Pts',(-10.5166965270001,11.6,0.166495116999985));
#261526=CARTESIAN_POINT('Ctrl Pts',(-10.5149439520001,15.2,0.166137374999984));
#261527=CARTESIAN_POINT('Ctrl Pts',(-10.5149439520001,11.6,0.166137374999983));
#261528=CARTESIAN_POINT('Ctrl Pts',(-10.5131983790001,15.2,0.165782736999986));
#261529=CARTESIAN_POINT('Ctrl Pts',(-10.5131983790001,11.6,0.165782736999986));
#261530=CARTESIAN_POINT('Ctrl Pts',(-10.5114598270001,15.2,0.165431196999983));
#261531=CARTESIAN_POINT('Ctrl Pts',(-10.5114598270001,11.6,0.165431196999983));
#261532=CARTESIAN_POINT('Ctrl Pts',(-10.5097283150001,15.2,0.165082744999987));
#261533=CARTESIAN_POINT('Ctrl Pts',(-10.5097283150001,11.6,0.165082744999987));
#261534=CARTESIAN_POINT('Ctrl Pts',(-10.5080038620001,15.2,0.164737371999983));
#261535=CARTESIAN_POINT('Ctrl Pts',(-10.5080038620001,11.6,0.164737371999983));
#261536=CARTESIAN_POINT('Ctrl Pts',(-10.5062864880001,15.2,0.164395067999985));
#261537=CARTESIAN_POINT('Ctrl Pts',(-10.5062864880001,11.6,0.164395067999985));
#261538=CARTESIAN_POINT('Ctrl Pts',(-10.5045762130001,15.2,0.164055823999987));
#261539=CARTESIAN_POINT('Ctrl Pts',(-10.5045762130001,11.6,0.164055823999986));
#261540=CARTESIAN_POINT('Ctrl Pts',(-10.5028730550001,15.2,0.163719632999988));
#261541=CARTESIAN_POINT('Ctrl Pts',(-10.5028730550001,11.6,0.163719632999987));
#261542=CARTESIAN_POINT('Ctrl Pts',(-10.5011770350001,15.2,0.163386482999983));
#261543=CARTESIAN_POINT('Ctrl Pts',(-10.5011770350001,11.6,0.163386482999983));
#261544=CARTESIAN_POINT('Ctrl Pts',(-10.4994881720001,15.2,0.163056365999985));
#261545=CARTESIAN_POINT('Ctrl Pts',(-10.4994881720001,11.6,0.163056365999985));
#261546=CARTESIAN_POINT('Ctrl Pts',(-10.4978064870001,15.2,0.162729272999984));
#261547=CARTESIAN_POINT('Ctrl Pts',(-10.4978064870001,11.6,0.162729272999984));
#261548=CARTESIAN_POINT('Ctrl Pts',(-10.4961320000001,15.2,0.162405193999984));
#261549=CARTESIAN_POINT('Ctrl Pts',(-10.4961320000001,11.6,0.162405193999983));
#261550=CARTESIAN_POINT('Ctrl Pts',(-10.4944647280001,15.2,0.162084120999988));
#261551=CARTESIAN_POINT('Ctrl Pts',(-10.4944647280001,11.6,0.162084120999987));
#261552=CARTESIAN_POINT('Ctrl Pts',(-10.4928046930001,15.2,0.161766040999982));
#261553=CARTESIAN_POINT('Ctrl Pts',(-10.4928046930001,11.6,0.161766040999982));
#261554=CARTESIAN_POINT('Ctrl Pts',(-10.4911519150001,15.2,0.161450947999988));
#261555=CARTESIAN_POINT('Ctrl Pts',(-10.4911519150001,11.6,0.161450947999988));
#261556=CARTESIAN_POINT('Ctrl Pts',(-10.4895064150001,15.2,0.161138831999987));
#261557=CARTESIAN_POINT('Ctrl Pts',(-10.4895064150001,11.6,0.161138831999987));
#261558=CARTESIAN_POINT('Ctrl Pts',(-10.4878682100001,15.2,0.160829682999988));
#261559=CARTESIAN_POINT('Ctrl Pts',(-10.4878682100001,11.6,0.160829682999987));
#261560=CARTESIAN_POINT('Ctrl Pts',(-10.4862373250001,15.2,0.160523489999989));
#261561=CARTESIAN_POINT('Ctrl Pts',(-10.4862373250001,11.6,0.160523489999988));
#261562=CARTESIAN_POINT('Ctrl Pts',(-10.4846137770001,15.2,0.160220243999984));
#261563=CARTESIAN_POINT('Ctrl Pts',(-10.4846137770001,11.6,0.160220243999984));
#261564=CARTESIAN_POINT('Ctrl Pts',(-10.4829975860001,15.2,0.159919936999984));
#261565=CARTESIAN_POINT('Ctrl Pts',(-10.4829975860001,11.6,0.159919936999983));
#261566=CARTESIAN_POINT('Ctrl Pts',(-10.4813887750001,15.2,0.159622555999985));
#261567=CARTESIAN_POINT('Ctrl Pts',(-10.4813887750001,11.6,0.159622555999985));
#261568=CARTESIAN_POINT('Ctrl Pts',(-10.4797873630001,15.2,0.159328093999989));
#261569=CARTESIAN_POINT('Ctrl Pts',(-10.4797873630001,11.6,0.159328093999988));
#261570=CARTESIAN_POINT('Ctrl Pts',(-10.4781933710001,15.2,0.159036539999988));
#261571=CARTESIAN_POINT('Ctrl Pts',(-10.4781933710001,11.6,0.159036539999988));
#261572=CARTESIAN_POINT('Ctrl Pts',(-10.4766068200001,15.2,0.158747883999983));
#261573=CARTESIAN_POINT('Ctrl Pts',(-10.4766068200001,11.6,0.158747883999983));
#261574=CARTESIAN_POINT('Ctrl Pts',(-10.4750277290001,15.2,0.158462115999987));
#261575=CARTESIAN_POINT('Ctrl Pts',(-10.4750277290001,11.6,0.158462115999986));
#261576=CARTESIAN_POINT('Ctrl Pts',(-10.4734561210001,15.2,0.158179226999984));
#261577=CARTESIAN_POINT('Ctrl Pts',(-10.4734561210001,11.6,0.158179226999983));
#261578=CARTESIAN_POINT('Ctrl Pts',(-10.4718920160001,15.2,0.157899203999987));
#261579=CARTESIAN_POINT('Ctrl Pts',(-10.4718920160001,11.6,0.157899203999987));
#261580=CARTESIAN_POINT('Ctrl Pts',(-10.4703354350001,15.2,0.157622039999987));
#261581=CARTESIAN_POINT('Ctrl Pts',(-10.4703354350001,11.6,0.157622039999987));
#261582=CARTESIAN_POINT('Ctrl Pts',(-10.4687864010001,15.2,0.157347723999983));
#261583=CARTESIAN_POINT('Ctrl Pts',(-10.4687864010001,11.6,0.157347723999983));
#261584=CARTESIAN_POINT('Ctrl Pts',(-10.4672449310001,15.2,0.157076244999987));
#261585=CARTESIAN_POINT('Ctrl Pts',(-10.4672449310001,11.6,0.157076244999987));
#261586=CARTESIAN_POINT('Ctrl Pts',(-10.4657110500001,15.2,0.156807592999986));
#261587=CARTESIAN_POINT('Ctrl Pts',(-10.4657110500001,11.6,0.156807592999985));
#261588=CARTESIAN_POINT('Ctrl Pts',(-10.4641847780001,15.2,0.156541757999986));
#261589=CARTESIAN_POINT('Ctrl Pts',(-10.4641847780001,11.6,0.156541757999986));
#261590=CARTESIAN_POINT('Ctrl Pts',(-10.4626661360001,15.2,0.156278728999983));
#261591=CARTESIAN_POINT('Ctrl Pts',(-10.4626661360001,11.6,0.156278728999983));
#261592=CARTESIAN_POINT('Ctrl Pts',(-10.4611551460001,15.2,0.156018495999986));
#261593=CARTESIAN_POINT('Ctrl Pts',(-10.4611551460001,11.6,0.156018495999985));
#261594=CARTESIAN_POINT('Ctrl Pts',(-10.4596518290001,15.2,0.155761047999987));
#261595=CARTESIAN_POINT('Ctrl Pts',(-10.4596518290001,11.6,0.155761047999987));
#261596=CARTESIAN_POINT('Ctrl Pts',(-10.4581562070001,15.2,0.155506375999988));
#261597=CARTESIAN_POINT('Ctrl Pts',(-10.4581562070001,11.6,0.155506375999987));
#261598=CARTESIAN_POINT('Ctrl Pts',(-10.4566683020001,15.2,0.155254465999985));
#261599=CARTESIAN_POINT('Ctrl Pts',(-10.4566683020001,11.6,0.155254465999985));
#261600=CARTESIAN_POINT('Ctrl Pts',(-10.4551881360001,15.2,0.155005310999985));
#261601=CARTESIAN_POINT('Ctrl Pts',(-10.4551881360001,11.6,0.155005310999984));
#261602=CARTESIAN_POINT('Ctrl Pts',(-10.4537157300001,15.2,0.154758897999985));
#261603=CARTESIAN_POINT('Ctrl Pts',(-10.4537157300001,11.6,0.154758897999984));
#261604=CARTESIAN_POINT('Ctrl Pts',(-10.4522511070001,15.2,0.154515216999984));
#261605=CARTESIAN_POINT('Ctrl Pts',(-10.4522511070001,11.6,0.154515216999984));
#261606=CARTESIAN_POINT('Ctrl Pts',(-10.4507942880001,15.2,0.154274255999987));
#261607=CARTESIAN_POINT('Ctrl Pts',(-10.4507942880001,11.6,0.154274255999986));
#261608=CARTESIAN_POINT('Ctrl Pts',(-10.4493452950001,15.2,0.154036006999987));
#261609=CARTESIAN_POINT('Ctrl Pts',(-10.4493452950001,11.6,0.154036006999986));
#261610=CARTESIAN_POINT('Ctrl Pts',(-10.4479041520001,15.2,0.153800454999988));
#261611=CARTESIAN_POINT('Ctrl Pts',(-10.4479041520001,11.6,0.153800454999988));
#261612=CARTESIAN_POINT('Ctrl Pts',(-10.4464708800001,15.2,0.153567592999986));
#261613=CARTESIAN_POINT('Ctrl Pts',(-10.4464708800001,11.6,0.153567592999985));
#261614=CARTESIAN_POINT('Ctrl Pts',(-10.4450455010001,15.2,0.153337406999987));
#261615=CARTESIAN_POINT('Ctrl Pts',(-10.4450455010001,11.6,0.153337406999987));
#261616=CARTESIAN_POINT('Ctrl Pts',(-10.4436280380001,15.2,0.153109886999987));
#261617=CARTESIAN_POINT('Ctrl Pts',(-10.4436280380001,11.6,0.153109886999987));
#261618=CARTESIAN_POINT('Ctrl Pts',(-10.4422185140001,15.2,0.152885022999989));
#261619=CARTESIAN_POINT('Ctrl Pts',(-10.4422185140001,11.6,0.152885022999989));
#261620=CARTESIAN_POINT('Ctrl Pts',(-10.4408169510001,15.2,0.152662800999988));
#261621=CARTESIAN_POINT('Ctrl Pts',(-10.4408169510001,11.6,0.152662800999987));
#261622=CARTESIAN_POINT('Ctrl Pts',(-10.4394233720001,15.2,0.152443211999986));
#261623=CARTESIAN_POINT('Ctrl Pts',(-10.4394233720001,11.6,0.152443211999986));
#261624=CARTESIAN_POINT('Ctrl Pts',(-10.4380378000001,15.2,0.152226242999984));
#261625=CARTESIAN_POINT('Ctrl Pts',(-10.4380378000001,11.6,0.152226242999984));
#261626=CARTESIAN_POINT('Ctrl Pts',(-10.4366602580001,15.2,0.152011882999985));
#261627=CARTESIAN_POINT('Ctrl Pts',(-10.4366602580001,11.6,0.152011882999985));
#261628=CARTESIAN_POINT('Ctrl Pts',(-10.4352907680001,15.2,0.151800122999983));
#261629=CARTESIAN_POINT('Ctrl Pts',(-10.4352907680001,11.6,0.151800122999983));
#261630=CARTESIAN_POINT('Ctrl Pts',(-10.4339293550001,15.2,0.151590946999987));
#261631=CARTESIAN_POINT('Ctrl Pts',(-10.4339293550001,11.6,0.151590946999986));
#261632=CARTESIAN_POINT('Ctrl Pts',(-10.4325760410001,15.2,0.151384346999985));
#261633=CARTESIAN_POINT('Ctrl Pts',(-10.4325760410001,11.6,0.151384346999985));
#261634=CARTESIAN_POINT('Ctrl Pts',(-10.4312308480001,15.2,0.151180308999983));
#261635=CARTESIAN_POINT('Ctrl Pts',(-10.4312308480001,11.6,0.151180308999983));
#261636=CARTESIAN_POINT('Ctrl Pts',(-10.4298938030001,15.2,0.150978822999988));
#261637=CARTESIAN_POINT('Ctrl Pts',(-10.4298938030001,11.6,0.150978822999987));
#261638=CARTESIAN_POINT('Ctrl Pts',(-10.4285649260001,15.2,0.150779875999985));
#261639=CARTESIAN_POINT('Ctrl Pts',(-10.4285649260001,11.6,0.150779875999984));
#261640=CARTESIAN_POINT('Ctrl Pts',(-10.4272442410001,15.2,0.150583456999982));
#261641=CARTESIAN_POINT('Ctrl Pts',(-10.4272442410001,11.6,0.150583456999982));
#261642=CARTESIAN_POINT('Ctrl Pts',(-10.4259317730001,15.2,0.150389553999983));
#261643=CARTESIAN_POINT('Ctrl Pts',(-10.4259317730001,11.6,0.150389553999983));
#261644=CARTESIAN_POINT('Ctrl Pts',(-10.4246275460001,15.2,0.150198153999987));
#261645=CARTESIAN_POINT('Ctrl Pts',(-10.4246275460001,11.6,0.150198153999987));
#261646=CARTESIAN_POINT('Ctrl Pts',(-10.4233315830001,15.2,0.150009245999985));
#261647=CARTESIAN_POINT('Ctrl Pts',(-10.4233315830001,11.6,0.150009245999984));
#261648=CARTESIAN_POINT('Ctrl Pts',(-10.4220439070001,15.2,0.149822816999983));
#261649=CARTESIAN_POINT('Ctrl Pts',(-10.4220439070001,11.6,0.149822816999982));
#261650=CARTESIAN_POINT('Ctrl Pts',(-10.4207645450001,15.2,0.149638854999985));
#261651=CARTESIAN_POINT('Ctrl Pts',(-10.4207645450001,11.6,0.149638854999985));
#261652=CARTESIAN_POINT('Ctrl Pts',(-10.4194935180001,15.2,0.149457348999986));
#261653=CARTESIAN_POINT('Ctrl Pts',(-10.4194935180001,11.6,0.149457348999986));
#261654=CARTESIAN_POINT('Ctrl Pts',(-10.4182308520001,15.2,0.149278284999985));
#261655=CARTESIAN_POINT('Ctrl Pts',(-10.4182308520001,11.6,0.149278284999985));
#261656=CARTESIAN_POINT('Ctrl Pts',(-10.4169765720001,15.2,0.149101651999985));
#261657=CARTESIAN_POINT('Ctrl Pts',(-10.4169765720001,11.6,0.149101651999985));
#261658=CARTESIAN_POINT('Ctrl Pts',(-10.4157307010001,15.2,0.148927436999986));
#261659=CARTESIAN_POINT('Ctrl Pts',(-10.4157307010001,11.6,0.148927436999986));
#261660=CARTESIAN_POINT('Ctrl Pts',(-10.4144932620001,15.2,0.148755626999986));
#261661=CARTESIAN_POINT('Ctrl Pts',(-10.4144932620001,11.6,0.148755626999985));
#261662=CARTESIAN_POINT('Ctrl Pts',(-10.4132642840001,15.2,0.148586209999984));
#261663=CARTESIAN_POINT('Ctrl Pts',(-10.4132642840001,11.6,0.148586209999983));
#261664=CARTESIAN_POINT('Ctrl Pts',(-10.4120437890001,15.2,0.148419172999983));
#261665=CARTESIAN_POINT('Ctrl Pts',(-10.4120437890001,11.6,0.148419172999982));
#261666=CARTESIAN_POINT('Ctrl Pts',(-10.4108318020001,15.2,0.148254502999983));
#261667=CARTESIAN_POINT('Ctrl Pts',(-10.4108318020001,11.6,0.148254502999982));
#261668=CARTESIAN_POINT('Ctrl Pts',(-10.4096283490001,15.2,0.148092186999986));
#261669=CARTESIAN_POINT('Ctrl Pts',(-10.4096283490001,11.6,0.148092186999986));
#261670=CARTESIAN_POINT('Ctrl Pts',(-10.4084334530001,15.2,0.147932213999984));
#261671=CARTESIAN_POINT('Ctrl Pts',(-10.4084334530001,11.6,0.147932213999983));
#261672=CARTESIAN_POINT('Ctrl Pts',(-10.4072471420001,15.2,0.147774568999988));
#261673=CARTESIAN_POINT('Ctrl Pts',(-10.4072471420001,11.6,0.147774568999987));
#261674=CARTESIAN_POINT('Ctrl Pts',(-10.4060694410001,15.2,0.147619239999983));
#261675=CARTESIAN_POINT('Ctrl Pts',(-10.4060694410001,11.6,0.147619239999983));
#261676=CARTESIAN_POINT('Ctrl Pts',(-10.4049003720001,15.2,0.147466213999987));
#261677=CARTESIAN_POINT('Ctrl Pts',(-10.4049003720001,11.6,0.147466213999987));
#261678=CARTESIAN_POINT('Ctrl Pts',(-10.4037399650001,15.2,0.147315476999985));
#261679=CARTESIAN_POINT('Ctrl Pts',(-10.4037399650001,11.6,0.147315476999985));
#261680=CARTESIAN_POINT('Ctrl Pts',(-10.4025882420001,15.2,0.147167016999985));
#261681=CARTESIAN_POINT('Ctrl Pts',(-10.4025882420001,11.6,0.147167016999985));
#261682=CARTESIAN_POINT('Ctrl Pts',(-10.4014452320001,15.2,0.147020818999986));
#261683=CARTESIAN_POINT('Ctrl Pts',(-10.4014452320001,11.6,0.147020818999985));
#261684=CARTESIAN_POINT('Ctrl Pts',(-10.4003109570001,15.2,0.146876870999986));
#261685=CARTESIAN_POINT('Ctrl Pts',(-10.4003109570001,11.6,0.146876870999985));
#261686=CARTESIAN_POINT('Ctrl Pts',(-10.3991854470001,15.2,0.146735159999984));
#261687=CARTESIAN_POINT('Ctrl Pts',(-10.3991854470001,11.6,0.146735159999984));
#261688=CARTESIAN_POINT('Ctrl Pts',(-10.3980687260001,15.2,0.146595670999985));
#261689=CARTESIAN_POINT('Ctrl Pts',(-10.3980687260001,11.6,0.146595670999984));
#261690=CARTESIAN_POINT('Ctrl Pts',(-10.3969608200001,15.2,0.146458390999986));
#261691=CARTESIAN_POINT('Ctrl Pts',(-10.3969608200001,11.6,0.146458390999986));
#261692=CARTESIAN_POINT('Ctrl Pts',(-10.3958617570001,15.2,0.146323306999987));
#261693=CARTESIAN_POINT('Ctrl Pts',(-10.3958617570001,11.6,0.146323306999987));
#261694=CARTESIAN_POINT('Ctrl Pts',(-10.3947715610001,15.2,0.146190402999986));
#261695=CARTESIAN_POINT('Ctrl Pts',(-10.3947715610001,11.6,0.146190402999986));
#261696=CARTESIAN_POINT('Ctrl Pts',(-10.3936902610001,15.2,0.146059668999987));
#261697=CARTESIAN_POINT('Ctrl Pts',(-10.3936902610001,11.6,0.146059668999987));
#261698=CARTESIAN_POINT('Ctrl Pts',(-10.3926178820001,15.2,0.145931086999984));
#261699=CARTESIAN_POINT('Ctrl Pts',(-10.3926178820001,11.6,0.145931086999984));
#261700=CARTESIAN_POINT('Ctrl Pts',(-10.3915544510001,15.2,0.145804645999985));
#261701=CARTESIAN_POINT('Ctrl Pts',(-10.3915544510001,11.6,0.145804645999985));
#261702=CARTESIAN_POINT('Ctrl Pts',(-10.3904999960001,15.2,0.145680330999984));
#261703=CARTESIAN_POINT('Ctrl Pts',(-10.3904999960001,11.6,0.145680330999984));
#261704=CARTESIAN_POINT('Ctrl Pts',(-10.3894545430001,15.2,0.145558126999985));
#261705=CARTESIAN_POINT('Ctrl Pts',(-10.3894545430001,11.6,0.145558126999985));
#261706=CARTESIAN_POINT('Ctrl Pts',(-10.3884181200001,15.2,0.145438019999986));
#261707=CARTESIAN_POINT('Ctrl Pts',(-10.3884181200001,11.6,0.145438019999986));
#261708=CARTESIAN_POINT('Ctrl Pts',(-10.3873907530001,15.2,0.145319995999986));
#261709=CARTESIAN_POINT('Ctrl Pts',(-10.3873907530001,11.6,0.145319995999986));
#261710=CARTESIAN_POINT('Ctrl Pts',(-10.3863724700001,15.2,0.145204041999989));
#261711=CARTESIAN_POINT('Ctrl Pts',(-10.3863724700001,11.6,0.145204041999988));
#261712=CARTESIAN_POINT('Ctrl Pts',(-10.3853633010001,15.2,0.145090140999984));
#261713=CARTESIAN_POINT('Ctrl Pts',(-10.3853633010001,11.6,0.145090140999983));
#261714=CARTESIAN_POINT('Ctrl Pts',(-10.3843632700001,15.2,0.144978280999983));
#261715=CARTESIAN_POINT('Ctrl Pts',(-10.3843632700001,11.6,0.144978280999983));
#261716=CARTESIAN_POINT('Ctrl Pts',(-10.3833724070001,15.2,0.144868444999986));
#261717=CARTESIAN_POINT('Ctrl Pts',(-10.3833724070001,11.6,0.144868444999986));
#261718=CARTESIAN_POINT('Ctrl Pts',(-10.3823907380001,15.2,0.144760619999986));
#261719=CARTESIAN_POINT('Ctrl Pts',(-10.3823907380001,11.6,0.144760619999986));
#261720=CARTESIAN_POINT('Ctrl Pts',(-10.3814182930001,15.2,0.144654789999983));
#261721=CARTESIAN_POINT('Ctrl Pts',(-10.3814182930001,11.6,0.144654789999982));
#261722=CARTESIAN_POINT('Ctrl Pts',(-10.3804551000001,15.2,0.144550940999988));
#261723=CARTESIAN_POINT('Ctrl Pts',(-10.3804551000001,11.6,0.144550940999987));
#261724=CARTESIAN_POINT('Ctrl Pts',(-10.3795011870001,15.2,0.144449057999987));
#261725=CARTESIAN_POINT('Ctrl Pts',(-10.3795011870001,11.6,0.144449057999986));
#261726=CARTESIAN_POINT('Ctrl Pts',(-10.3785565820001,15.2,0.144349124999987));
#261727=CARTESIAN_POINT('Ctrl Pts',(-10.3785565820001,11.6,0.144349124999987));
#261728=CARTESIAN_POINT('Ctrl Pts',(-10.3776213140001,15.2,0.144251127999984));
#261729=CARTESIAN_POINT('Ctrl Pts',(-10.3776213140001,11.6,0.144251127999983));
#261730=CARTESIAN_POINT('Ctrl Pts',(-10.3766954110001,15.2,0.144155049999988));
#261731=CARTESIAN_POINT('Ctrl Pts',(-10.3766954110001,11.6,0.144155049999987));
#261732=CARTESIAN_POINT('Ctrl Pts',(-10.3757841830001,15.2,0.144061419999986));
#261733=CARTESIAN_POINT('Ctrl Pts',(-10.3757841830001,11.6,0.144061419999985));
#261734=CARTESIAN_POINT('Ctrl Pts',(-10.3750636860001,15.2,0.143988113999987));
#261735=CARTESIAN_POINT('Ctrl Pts',(-10.3750636860001,11.6,0.143988113999986));
#261736=CARTESIAN_POINT('Ctrl Pts',(-10.3745287910001,15.2,0.143934095999985));
#261737=CARTESIAN_POINT('Ctrl Pts',(-10.3745287910001,11.6,0.143934095999984));
#261738=CARTESIAN_POINT('Ctrl Pts',(-10.3741757630001,15.2,0.143898618999985));
#261739=CARTESIAN_POINT('Ctrl Pts',(-10.3741757630001,11.6,0.143898618999984));
#261740=CARTESIAN_POINT('Ctrl Pts',(-10.3740022750001,15.2,0.143881226999985));
#261741=CARTESIAN_POINT('Ctrl Pts',(-10.3740022750001,11.6,0.143881226999984));
#261742=CARTESIAN_POINT('',(-10.3740022750001,12.2,0.143881226999985));
#261743=CARTESIAN_POINT('',(-10.3740022750001,15.2,0.143881226999985));
#261744=CARTESIAN_POINT('',(-10.3740022750001,12.2,0.143881226999985));
#261745=CARTESIAN_POINT('Ctrl Pts',(-11.4869855320001,12.2,0.546958305999983));
#261746=CARTESIAN_POINT('Ctrl Pts',(-11.4863150090001,12.2,0.546590898999986));
#261747=CARTESIAN_POINT('Ctrl Pts',(-11.4849742100001,12.2,0.545856550999986));
#261748=CARTESIAN_POINT('Ctrl Pts',(-11.4829637560001,12.2,0.544756421999986));
#261749=CARTESIAN_POINT('Ctrl Pts',(-11.4802846430001,12.2,0.543292367999988));
#261750=CARTESIAN_POINT('Ctrl Pts',(-11.4769382380001,12.2,0.541466945999982));
#261751=CARTESIAN_POINT('Ctrl Pts',(-11.4735943180001,12.2,0.539646165999983));
#261752=CARTESIAN_POINT('Ctrl Pts',(-11.4702528880001,12.2,0.537830029999986));
#261753=CARTESIAN_POINT('Ctrl Pts',(-11.4669139500001,12.2,0.536018536999983));
#261754=CARTESIAN_POINT('Ctrl Pts',(-11.4635775100001,12.2,0.534211684999986));
#261755=CARTESIAN_POINT('Ctrl Pts',(-11.4602435780001,12.2,0.532409473999986));
#261756=CARTESIAN_POINT('Ctrl Pts',(-11.4569121620001,12.2,0.530611900999984));
#261757=CARTESIAN_POINT('Ctrl Pts',(-11.4535832720001,12.2,0.528818965999989));
#261758=CARTESIAN_POINT('Ctrl Pts',(-11.4502569220001,12.2,0.527030663999986));
#261759=CARTESIAN_POINT('Ctrl Pts',(-11.4469331180001,12.2,0.525246995999984));
#261760=CARTESIAN_POINT('Ctrl Pts',(-11.4436118760001,12.2,0.523467958999984));
#261761=CARTESIAN_POINT('Ctrl Pts',(-11.4402932010001,12.2,0.521693550999984));
#261762=CARTESIAN_POINT('Ctrl Pts',(-11.4369771030001,12.2,0.519923770999986));
#261763=CARTESIAN_POINT('Ctrl Pts',(-11.4336635900001,12.2,0.518158617999984));
#261764=CARTESIAN_POINT('Ctrl Pts',(-11.4303526710001,12.2,0.516398088999988));
#261765=CARTESIAN_POINT('Ctrl Pts',(-11.4270443520001,12.2,0.514642183999987));
#261766=CARTESIAN_POINT('Ctrl Pts',(-11.4237386430001,12.2,0.512890900999987));
#261767=CARTESIAN_POINT('Ctrl Pts',(-11.4204355510001,12.2,0.511144238999983));
#261768=CARTESIAN_POINT('Ctrl Pts',(-11.4171350880001,12.2,0.509402193999984));
#261769=CARTESIAN_POINT('Ctrl Pts',(-11.4138372610001,12.2,0.507664766999985));
#261770=CARTESIAN_POINT('Ctrl Pts',(-11.4105420820001,12.2,0.505931953999985));
#261771=CARTESIAN_POINT('Ctrl Pts',(-11.4072495570001,12.2,0.504203755999986));
#261772=CARTESIAN_POINT('Ctrl Pts',(-11.4039596970001,12.2,0.502480167999986));
#261773=CARTESIAN_POINT('Ctrl Pts',(-11.4006725110001,12.2,0.500761190999985));
#261774=CARTESIAN_POINT('Ctrl Pts',(-11.3973880080001,12.2,0.499046821999984));
#261775=CARTESIAN_POINT('Ctrl Pts',(-11.3941061970001,12.2,0.497337060999987));
#261776=CARTESIAN_POINT('Ctrl Pts',(-11.3908270860001,12.2,0.495631902999989));
#261777=CARTESIAN_POINT('Ctrl Pts',(-11.3875506850001,12.2,0.493931348999985));
#261778=CARTESIAN_POINT('Ctrl Pts',(-11.3842770020001,12.2,0.492235395999985));
#261779=CARTESIAN_POINT('Ctrl Pts',(-11.3810060480001,12.2,0.490544042999983));
#261780=CARTESIAN_POINT('Ctrl Pts',(-11.3777378300001,12.2,0.488857287999984));
#261781=CARTESIAN_POINT('Ctrl Pts',(-11.3744723580001,12.2,0.487175127999984));
#261782=CARTESIAN_POINT('Ctrl Pts',(-11.3712096420001,12.2,0.485497562999986));
#261783=CARTESIAN_POINT('Ctrl Pts',(-11.3679496900001,12.2,0.483824590999986));
#261784=CARTESIAN_POINT('Ctrl Pts',(-11.3646925130001,12.2,0.482156208999989));
#261785=CARTESIAN_POINT('Ctrl Pts',(-11.3614381180001,12.2,0.480492415999985));
#261786=CARTESIAN_POINT('Ctrl Pts',(-11.3581865150001,12.2,0.478833208999987));
#261787=CARTESIAN_POINT('Ctrl Pts',(-11.3549377140001,12.2,0.477178588999987));
#261788=CARTESIAN_POINT('Ctrl Pts',(-11.3516917240001,12.2,0.475528550999984));
#261789=CARTESIAN_POINT('Ctrl Pts',(-11.3484485530001,12.2,0.473883093999987));
#261790=CARTESIAN_POINT('Ctrl Pts',(-11.3452082120001,12.2,0.472242216999987));
#261791=CARTESIAN_POINT('Ctrl Pts',(-11.3419707090001,12.2,0.470605916999984));
#261792=CARTESIAN_POINT('Ctrl Pts',(-11.3387360540001,12.2,0.468974193999987));
#261793=CARTESIAN_POINT('Ctrl Pts',(-11.3355042560001,12.2,0.467347044999986));
#261794=CARTESIAN_POINT('Ctrl Pts',(-11.3322753250001,12.2,0.465724465999986));
#261795=CARTESIAN_POINT('Ctrl Pts',(-11.3290492700001,12.2,0.464106457999982));
#261796=CARTESIAN_POINT('Ctrl Pts',(-11.3258260990001,12.2,0.462493017999983));
#261797=CARTESIAN_POINT('Ctrl Pts',(-11.3226058230001,12.2,0.460884142999984));
#261798=CARTESIAN_POINT('Ctrl Pts',(-11.3193884510001,12.2,0.459279831999986));
#261799=CARTESIAN_POINT('Ctrl Pts',(-11.3161739920001,12.2,0.457680083999983));
#261800=CARTESIAN_POINT('Ctrl Pts',(-11.3129624580001,12.2,0.456084895999984));
#261801=CARTESIAN_POINT('Ctrl Pts',(-11.3097538530001,12.2,0.454494265999985));
#261802=CARTESIAN_POINT('Ctrl Pts',(-11.3065481920001,12.2,0.452908190999985));
#261803=CARTESIAN_POINT('Ctrl Pts',(-11.3033454810001,12.2,0.451326670999985));
#261804=CARTESIAN_POINT('Ctrl Pts',(-11.3001457320001,12.2,0.449749702999984));
#261805=CARTESIAN_POINT('Ctrl Pts',(-11.2969489510001,12.2,0.448177283999982));
#261806=CARTESIAN_POINT('Ctrl Pts',(-11.2937551520001,12.2,0.446609412999983));
#261807=CARTESIAN_POINT('Ctrl Pts',(-11.2905643410001,12.2,0.445046087999987));
#261808=CARTESIAN_POINT('Ctrl Pts',(-11.2873765290001,12.2,0.443487306999986));
#261809=CARTESIAN_POINT('Ctrl Pts',(-11.2841917260001,12.2,0.441933066999987));
#261810=CARTESIAN_POINT('Ctrl Pts',(-11.2810099400001,12.2,0.440383366999986));
#261811=CARTESIAN_POINT('Ctrl Pts',(-11.2778311820001,12.2,0.438838203999987));
#261812=CARTESIAN_POINT('Ctrl Pts',(-11.2746554610001,12.2,0.437297575999986));
#261813=CARTESIAN_POINT('Ctrl Pts',(-11.2714827870001,12.2,0.435761481999983));
#261814=CARTESIAN_POINT('Ctrl Pts',(-11.2683131690001,12.2,0.434229917999982));
#261815=CARTESIAN_POINT('Ctrl Pts',(-11.2651466170001,12.2,0.432702882999987));
#261816=CARTESIAN_POINT('Ctrl Pts',(-11.2619831420001,12.2,0.431180374999984));
#261817=CARTESIAN_POINT('Ctrl Pts',(-11.2588227510001,12.2,0.429662389999983));
#261818=CARTESIAN_POINT('Ctrl Pts',(-11.2556654560001,12.2,0.428148927999987));
#261819=CARTESIAN_POINT('Ctrl Pts',(-11.2525112650001,12.2,0.426639985999984));
#261820=CARTESIAN_POINT('Ctrl Pts',(-11.2493601900001,12.2,0.425135561999985));
#261821=CARTESIAN_POINT('Ctrl Pts',(-11.2462122380001,12.2,0.423635652999987));
#261822=CARTESIAN_POINT('Ctrl Pts',(-11.2430674210001,12.2,0.422140256999985));
#261823=CARTESIAN_POINT('Ctrl Pts',(-11.2399257470001,12.2,0.420649372999984));
#261824=CARTESIAN_POINT('Ctrl Pts',(-11.2367872280001,12.2,0.419162996999987));
#261825=CARTESIAN_POINT('Ctrl Pts',(-11.2336518720001,12.2,0.417681126999985));
#261826=CARTESIAN_POINT('Ctrl Pts',(-11.2305196890001,12.2,0.416203761999987));
#261827=CARTESIAN_POINT('Ctrl Pts',(-11.2273906900001,12.2,0.414730897999984));
#261828=CARTESIAN_POINT('Ctrl Pts',(-11.2242648840001,12.2,0.413262533999985));
#261829=CARTESIAN_POINT('Ctrl Pts',(-11.2211422810001,12.2,0.411798666999985));
#261830=CARTESIAN_POINT('Ctrl Pts',(-11.2180228910001,12.2,0.410339293999984));
#261831=CARTESIAN_POINT('Ctrl Pts',(-11.2149067230001,12.2,0.408884414999986));
#261832=CARTESIAN_POINT('Ctrl Pts',(-11.2117937880001,12.2,0.407434024999986));
#261833=CARTESIAN_POINT('Ctrl Pts',(-11.2086840970001,12.2,0.405988122999985));
#261834=CARTESIAN_POINT('Ctrl Pts',(-11.2055776580001,12.2,0.404546704999986));
#261835=CARTESIAN_POINT('Ctrl Pts',(-11.2024744820001,12.2,0.403109771999985));
#261836=CARTESIAN_POINT('Ctrl Pts',(-11.1993745780001,12.2,0.401677316999987));
#261837=CARTESIAN_POINT('Ctrl Pts',(-11.1962779570001,12.2,0.400249341999985));
#261838=CARTESIAN_POINT('Ctrl Pts',(-11.1931846300001,12.2,0.398825840999986));
#261839=CARTESIAN_POINT('Ctrl Pts',(-11.1900946040001,12.2,0.397406813999983));
#261840=CARTESIAN_POINT('Ctrl Pts',(-11.1870078920001,12.2,0.395992257999982));
#261841=CARTESIAN_POINT('Ctrl Pts',(-11.1839245020001,12.2,0.394582169999986));
#261842=CARTESIAN_POINT('Ctrl Pts',(-11.1808444470001,12.2,0.393176545999987));
#261843=CARTESIAN_POINT('Ctrl Pts',(-11.1777677340001,12.2,0.391775386999988));
#261844=CARTESIAN_POINT('Ctrl Pts',(-11.1746943740001,12.2,0.390378687999986));
#261845=CARTESIAN_POINT('Ctrl Pts',(-11.1716243780001,12.2,0.388986446999984));
#261846=CARTESIAN_POINT('Ctrl Pts',(-11.1685577570001,12.2,0.387598660999986));
#261847=CARTESIAN_POINT('Ctrl Pts',(-11.1654945190001,12.2,0.386215327999988));
#261848=CARTESIAN_POINT('Ctrl Pts',(-11.1624346740001,12.2,0.384836445999985));
#261849=CARTESIAN_POINT('Ctrl Pts',(-11.1593782350001,12.2,0.383462010999986));
#261850=CARTESIAN_POINT('Ctrl Pts',(-11.1563252100001,12.2,0.382092021999987));
#261851=CARTESIAN_POINT('Ctrl Pts',(-11.1532756110001,12.2,0.380726473999986));
#261852=CARTESIAN_POINT('Ctrl Pts',(-11.1502294460001,12.2,0.379365366999984));
#261853=CARTESIAN_POINT('Ctrl Pts',(-11.1471867270001,12.2,0.378008696999985));
#261854=CARTESIAN_POINT('Ctrl Pts',(-11.1441474640001,12.2,0.376656461999989));
#261855=CARTESIAN_POINT('Ctrl Pts',(-11.1411116670001,12.2,0.375308657999986));
#261856=CARTESIAN_POINT('Ctrl Pts',(-11.1380793470001,12.2,0.373965283999986));
#261857=CARTESIAN_POINT('Ctrl Pts',(-11.1350505130001,12.2,0.372626335999984));
#261858=CARTESIAN_POINT('Ctrl Pts',(-11.1320251780001,12.2,0.371291811999988));
#261859=CARTESIAN_POINT('Ctrl Pts',(-11.1290033490001,12.2,0.369961708999984));
#261860=CARTESIAN_POINT('Ctrl Pts',(-11.1259850390001,12.2,0.368636023999986));
#261861=CARTESIAN_POINT('Ctrl Pts',(-11.1229702580001,12.2,0.367314754999986));
#261862=CARTESIAN_POINT('Ctrl Pts',(-11.1199590150001,12.2,0.365997898999986));
#261863=CARTESIAN_POINT('Ctrl Pts',(-11.1169513230001,12.2,0.364685452999982));
#261864=CARTESIAN_POINT('Ctrl Pts',(-11.1139471900001,12.2,0.363377413999988));
#261865=CARTESIAN_POINT('Ctrl Pts',(-11.1109466290001,12.2,0.362073778999985));
#261866=CARTESIAN_POINT('Ctrl Pts',(-11.1079496490001,12.2,0.360774545999987));
#261867=CARTESIAN_POINT('Ctrl Pts',(-11.1049562600001,12.2,0.359479711999988));
#261868=CARTESIAN_POINT('Ctrl Pts',(-11.1019664740001,12.2,0.358189272999985));
#261869=CARTESIAN_POINT('Ctrl Pts',(-11.0989803000001,12.2,0.356903227999985));
#261870=CARTESIAN_POINT('Ctrl Pts',(-11.0959977500001,12.2,0.355621572999985));
#261871=CARTESIAN_POINT('Ctrl Pts',(-11.0930188360001,12.2,0.354344304999987));
#261872=CARTESIAN_POINT('Ctrl Pts',(-11.0900435650001,12.2,0.353071420999989));
#261873=CARTESIAN_POINT('Ctrl Pts',(-11.0870719500001,12.2,0.351802918999984));
#261874=CARTESIAN_POINT('Ctrl Pts',(-11.0841040020001,12.2,0.350538794999986));
#261875=CARTESIAN_POINT('Ctrl Pts',(-11.0811397300001,12.2,0.349279046999986));
#261876=CARTESIAN_POINT('Ctrl Pts',(-11.0781791480001,12.2,0.348023670999984));
#261877=CARTESIAN_POINT('Ctrl Pts',(-11.0752222620001,12.2,0.346772664999988));
#261878=CARTESIAN_POINT('Ctrl Pts',(-11.0722690870001,12.2,0.345526024999985));
#261879=CARTESIAN_POINT('Ctrl Pts',(-11.0693196320001,12.2,0.344283748999987));
#261880=CARTESIAN_POINT('Ctrl Pts',(-11.0663739070001,12.2,0.343045833999986));
#261881=CARTESIAN_POINT('Ctrl Pts',(-11.0634319250001,12.2,0.341812274999986));
#261882=CARTESIAN_POINT('Ctrl Pts',(-11.0604936960001,12.2,0.340583071999987));
#261883=CARTESIAN_POINT('Ctrl Pts',(-11.0575592300001,12.2,0.339358219999983));
#261884=CARTESIAN_POINT('Ctrl Pts',(-11.0546285370001,12.2,0.338137715999984));
#261885=CARTESIAN_POINT('Ctrl Pts',(-11.0517016320001,12.2,0.336921557999985));
#261886=CARTESIAN_POINT('Ctrl Pts',(-11.0487785220001,12.2,0.335709739999985));
#261887=CARTESIAN_POINT('Ctrl Pts',(-11.0458592200001,12.2,0.334502262999985));
#261888=CARTESIAN_POINT('Ctrl Pts',(-11.0429437360001,12.2,0.333299120999988));
#261889=CARTESIAN_POINT('Ctrl Pts',(-11.0400320810001,12.2,0.332100310999985));
#261890=CARTESIAN_POINT('Ctrl Pts',(-11.0371242670001,12.2,0.330905830999986));
#261891=CARTESIAN_POINT('Ctrl Pts',(-11.0342203030001,12.2,0.329715676999989));
#261892=CARTESIAN_POINT('Ctrl Pts',(-11.0313202040001,12.2,0.328529845999985));
#261893=CARTESIAN_POINT('Ctrl Pts',(-11.0284239770001,12.2,0.327348335999984));
#261894=CARTESIAN_POINT('Ctrl Pts',(-11.0255316350001,12.2,0.326171140999989));
#261895=CARTESIAN_POINT('Ctrl Pts',(-11.0226431890001,12.2,0.324998259999987));
#261896=CARTESIAN_POINT('Ctrl Pts',(-11.0197586510001,12.2,0.323829688999986));
#261897=CARTESIAN_POINT('Ctrl Pts',(-11.0168780300001,12.2,0.322665424999986));
#261898=CARTESIAN_POINT('Ctrl Pts',(-11.0140013380001,12.2,0.321505463999987));
#261899=CARTESIAN_POINT('Ctrl Pts',(-11.0111285880001,12.2,0.320349803999989));
#261900=CARTESIAN_POINT('Ctrl Pts',(-11.0082597890001,12.2,0.319198439999986));
#261901=CARTESIAN_POINT('Ctrl Pts',(-11.0053949540001,12.2,0.318051369999988));
#261902=CARTESIAN_POINT('Ctrl Pts',(-11.0025340930001,12.2,0.316908588999985));
#261903=CARTESIAN_POINT('Ctrl Pts',(-10.9996772170001,12.2,0.315770094999985));
#261904=CARTESIAN_POINT('Ctrl Pts',(-10.9968243390001,12.2,0.314635884999985));
#261905=CARTESIAN_POINT('Ctrl Pts',(-10.9939754690001,12.2,0.313505953999984));
#261906=CARTESIAN_POINT('Ctrl Pts',(-10.9911306190001,12.2,0.312380299999986));
#261907=CARTESIAN_POINT('Ctrl Pts',(-10.9882898000001,12.2,0.311258919999986));
#261908=CARTESIAN_POINT('Ctrl Pts',(-10.9854530250001,12.2,0.310141807999984));
#261909=CARTESIAN_POINT('Ctrl Pts',(-10.9826203020001,12.2,0.309028961999989));
#261910=CARTESIAN_POINT('Ctrl Pts',(-10.9797916470001,12.2,0.307920378999986));
#261911=CARTESIAN_POINT('Ctrl Pts',(-10.9769670670001,12.2,0.306816054999985));
#261912=CARTESIAN_POINT('Ctrl Pts',(-10.9741465770001,12.2,0.305715986999986));
#261913=CARTESIAN_POINT('Ctrl Pts',(-10.9713301870001,12.2,0.304620170999983));
#261914=CARTESIAN_POINT('Ctrl Pts',(-10.9685179070001,12.2,0.303528602999985));
#261915=CARTESIAN_POINT('Ctrl Pts',(-10.9657097520001,12.2,0.302441278999983));
#261916=CARTESIAN_POINT('Ctrl Pts',(-10.9629057310001,12.2,0.301358197999986));
#261917=CARTESIAN_POINT('Ctrl Pts',(-10.9601058580001,12.2,0.300279352999984));
#261918=CARTESIAN_POINT('Ctrl Pts',(-10.9573101410001,12.2,0.299204742999986));
#261919=CARTESIAN_POINT('Ctrl Pts',(-10.9545185950001,12.2,0.298134361999987));
#261920=CARTESIAN_POINT('Ctrl Pts',(-10.9517312310001,12.2,0.297068208999987));
#261921=CARTESIAN_POINT('Ctrl Pts',(-10.9489480600001,12.2,0.296006278999985));
#261922=CARTESIAN_POINT('Ctrl Pts',(-10.9461690940001,12.2,0.294948567999986));
#261923=CARTESIAN_POINT('Ctrl Pts',(-10.9433943440001,12.2,0.293895071999986));
#261924=CARTESIAN_POINT('Ctrl Pts',(-10.9406238230001,12.2,0.292845787999987));
#261925=CARTESIAN_POINT('Ctrl Pts',(-10.9378575430001,12.2,0.291800712999986));
#261926=CARTESIAN_POINT('Ctrl Pts',(-10.9350955160001,12.2,0.290759840999986));
#261927=CARTESIAN_POINT('Ctrl Pts',(-10.9323377520001,12.2,0.289723170999987));
#261928=CARTESIAN_POINT('Ctrl Pts',(-10.9295842640001,12.2,0.288690695999985));
#261929=CARTESIAN_POINT('Ctrl Pts',(-10.9268350640001,12.2,0.287662414999983));
#261930=CARTESIAN_POINT('Ctrl Pts',(-10.9240901640001,12.2,0.286638322999986));
#261931=CARTESIAN_POINT('Ctrl Pts',(-10.9213495760001,12.2,0.285618414999984));
#261932=CARTESIAN_POINT('Ctrl Pts',(-10.9186133120001,12.2,0.284602688999982));
#261933=CARTESIAN_POINT('Ctrl Pts',(-10.9158813840001,12.2,0.283591140999988));
#261934=CARTESIAN_POINT('Ctrl Pts',(-10.9131538030001,12.2,0.282583765999984));
#261935=CARTESIAN_POINT('Ctrl Pts',(-10.9104305830001,12.2,0.281580559999988));
#261936=CARTESIAN_POINT('Ctrl Pts',(-10.9077117350001,12.2,0.280581520999985));
#261937=CARTESIAN_POINT('Ctrl Pts',(-10.9049972710001,12.2,0.279586640999985));
#261938=CARTESIAN_POINT('Ctrl Pts',(-10.9022872040001,12.2,0.278595920999987));
#261939=CARTESIAN_POINT('Ctrl Pts',(-10.8995815450001,12.2,0.277609353999986));
#261940=CARTESIAN_POINT('Ctrl Pts',(-10.8968803070001,12.2,0.276626936999986));
#261941=CARTESIAN_POINT('Ctrl Pts',(-10.8941835000001,12.2,0.275648664999988));
#261942=CARTESIAN_POINT('Ctrl Pts',(-10.8914911410001,12.2,0.274674534999986));
#261943=CARTESIAN_POINT('Ctrl Pts',(-10.8888032380001,12.2,0.273704540999984));
#261944=CARTESIAN_POINT('Ctrl Pts',(-10.8861198050001,12.2,0.272738680999982));
#261945=CARTESIAN_POINT('Ctrl Pts',(-10.8834408550001,12.2,0.271776950999989));
#261946=CARTESIAN_POINT('Ctrl Pts',(-10.8807663990001,12.2,0.270819344999986));
#261947=CARTESIAN_POINT('Ctrl Pts',(-10.8780964490001,12.2,0.269865860999987));
#261948=CARTESIAN_POINT('Ctrl Pts',(-10.8754310200001,12.2,0.268916491999986));
#261949=CARTESIAN_POINT('Ctrl Pts',(-10.8727701220001,12.2,0.267971236999984));
#261950=CARTESIAN_POINT('Ctrl Pts',(-10.8701137680001,12.2,0.267030089999984));
#261951=CARTESIAN_POINT('Ctrl Pts',(-10.8674619700001,12.2,0.266093045999987));
#261952=CARTESIAN_POINT('Ctrl Pts',(-10.8648147410001,12.2,0.265160102999986));
#261953=CARTESIAN_POINT('Ctrl Pts',(-10.8621720950001,12.2,0.264231254999987));
#261954=CARTESIAN_POINT('Ctrl Pts',(-10.8595340430001,12.2,0.263306497999984));
#261955=CARTESIAN_POINT('Ctrl Pts',(-10.8569005980001,12.2,0.262385827999987));
#261956=CARTESIAN_POINT('Ctrl Pts',(-10.8542717720001,12.2,0.261469240999985));
#261957=CARTESIAN_POINT('Ctrl Pts',(-10.8516475780001,12.2,0.260556731999984));
#261958=CARTESIAN_POINT('Ctrl Pts',(-10.8490280300001,12.2,0.259648296999986));
#261959=CARTESIAN_POINT('Ctrl Pts',(-10.8464131390001,12.2,0.258743930999987));
#261960=CARTESIAN_POINT('Ctrl Pts',(-10.8438029180001,12.2,0.257843629999983));
#261961=CARTESIAN_POINT('Ctrl Pts',(-10.8411973810001,12.2,0.256947389999986));
#261962=CARTESIAN_POINT('Ctrl Pts',(-10.8385965390001,12.2,0.256055205999988));
#261963=CARTESIAN_POINT('Ctrl Pts',(-10.8360004070001,12.2,0.255167072999987));
#261964=CARTESIAN_POINT('Ctrl Pts',(-10.8334089940001,12.2,0.254282987999983));
#261965=CARTESIAN_POINT('Ctrl Pts',(-10.8308223180001,12.2,0.253402943999985));
#261966=CARTESIAN_POINT('Ctrl Pts',(-10.8282403890001,12.2,0.252526939999989));
#261967=CARTESIAN_POINT('Ctrl Pts',(-10.8256632200001,12.2,0.251654968999984));
#261968=CARTESIAN_POINT('Ctrl Pts',(-10.8230908230001,12.2,0.250787025999983));
#261969=CARTESIAN_POINT('Ctrl Pts',(-10.8205232130001,12.2,0.249923108999983));
#261970=CARTESIAN_POINT('Ctrl Pts',(-10.8179604030001,12.2,0.249063209999987));
#261971=CARTESIAN_POINT('Ctrl Pts',(-10.8154024050001,12.2,0.248207326999985));
#261972=CARTESIAN_POINT('Ctrl Pts',(-10.8128492330001,12.2,0.247355453999987));
#261973=CARTESIAN_POINT('Ctrl Pts',(-10.8103008990001,12.2,0.246507586999982));
#261974=CARTESIAN_POINT('Ctrl Pts',(-10.8077574170001,12.2,0.245663720999989));
#261975=CARTESIAN_POINT('Ctrl Pts',(-10.8052187990001,12.2,0.244823850999989));
#261976=CARTESIAN_POINT('Ctrl Pts',(-10.8026850610001,12.2,0.243987971999986));
#261977=CARTESIAN_POINT('Ctrl Pts',(-10.8001562130001,12.2,0.243156080999984));
#261978=CARTESIAN_POINT('Ctrl Pts',(-10.7976322700001,12.2,0.242328170999984));
#261979=CARTESIAN_POINT('Ctrl Pts',(-10.7951132440001,12.2,0.241504237999983));
#261980=CARTESIAN_POINT('Ctrl Pts',(-10.7925991510001,12.2,0.240684276999983));
#261981=CARTESIAN_POINT('Ctrl Pts',(-10.7900900010001,12.2,0.239868283999982));
#261982=CARTESIAN_POINT('Ctrl Pts',(-10.7875858100001,12.2,0.239056253999985));
#261983=CARTESIAN_POINT('Ctrl Pts',(-10.7850865910001,12.2,0.238248179999987));
#261984=CARTESIAN_POINT('Ctrl Pts',(-10.7825923560001,12.2,0.237444060999987));
#261985=CARTESIAN_POINT('Ctrl Pts',(-10.7801031190001,12.2,0.236643886999985));
#261986=CARTESIAN_POINT('Ctrl Pts',(-10.7776188950001,12.2,0.235847656999986));
#261987=CARTESIAN_POINT('Ctrl Pts',(-10.7751396960001,12.2,0.235055364999983));
#261988=CARTESIAN_POINT('Ctrl Pts',(-10.7726655360001,12.2,0.234267004999986));
#261989=CARTESIAN_POINT('Ctrl Pts',(-10.7701964290001,12.2,0.233482572999986));
#261990=CARTESIAN_POINT('Ctrl Pts',(-10.7677323890001,12.2,0.232702063999985));
#261991=CARTESIAN_POINT('Ctrl Pts',(-10.7652734280001,12.2,0.231925471999985));
#261992=CARTESIAN_POINT('Ctrl Pts',(-10.7628195610001,12.2,0.231152792999989));
#261993=CARTESIAN_POINT('Ctrl Pts',(-10.7603708020001,12.2,0.230384019999987));
#261994=CARTESIAN_POINT('Ctrl Pts',(-10.7579271630001,12.2,0.229619148999984));
#261995=CARTESIAN_POINT('Ctrl Pts',(-10.7554886610001,12.2,0.228858175999989));
#261996=CARTESIAN_POINT('Ctrl Pts',(-10.7530553070001,12.2,0.228101093999986));
#261997=CARTESIAN_POINT('Ctrl Pts',(-10.7506271160001,12.2,0.227347897999985));
#261998=CARTESIAN_POINT('Ctrl Pts',(-10.7482041010001,12.2,0.226598583999986));
#261999=CARTESIAN_POINT('Ctrl Pts',(-10.7457862770001,12.2,0.225853145999988));
#262000=CARTESIAN_POINT('Ctrl Pts',(-10.7433736600001,12.2,0.225111577999986));
#262001=CARTESIAN_POINT('Ctrl Pts',(-10.7409662590001,12.2,0.224373874999984));
#262002=CARTESIAN_POINT('Ctrl Pts',(-10.7385640920001,12.2,0.223640032999985));
#262003=CARTESIAN_POINT('Ctrl Pts',(-10.7361671710001,12.2,0.222910043999986));
#262004=CARTESIAN_POINT('Ctrl Pts',(-10.7337755120001,12.2,0.222183903999986));
#262005=CARTESIAN_POINT('Ctrl Pts',(-10.7313891280001,12.2,0.221461608999984));
#262006=CARTESIAN_POINT('Ctrl Pts',(-10.7290080330001,12.2,0.220743150999985));
#262007=CARTESIAN_POINT('Ctrl Pts',(-10.7266322420001,12.2,0.220028526999982));
#262008=CARTESIAN_POINT('Ctrl Pts',(-10.7242617690001,12.2,0.219317729999986));
#262009=CARTESIAN_POINT('Ctrl Pts',(-10.7218966280001,12.2,0.218610753999986));
#262010=CARTESIAN_POINT('Ctrl Pts',(-10.7195368330001,12.2,0.217907592999986));
#262011=CARTESIAN_POINT('Ctrl Pts',(-10.7171823990001,12.2,0.217208243999987));
#262012=CARTESIAN_POINT('Ctrl Pts',(-10.7148333410001,12.2,0.216512699999987));
#262013=CARTESIAN_POINT('Ctrl Pts',(-10.7124896730001,12.2,0.215820953999986));
#262014=CARTESIAN_POINT('Ctrl Pts',(-10.7101514080001,12.2,0.215133002999988));
#262015=CARTESIAN_POINT('Ctrl Pts',(-10.7078185620001,12.2,0.214448838999988));
#262016=CARTESIAN_POINT('Ctrl Pts',(-10.7054911500001,12.2,0.213768457999985));
#262017=CARTESIAN_POINT('Ctrl Pts',(-10.7031691860001,12.2,0.213091852999985));
#262018=CARTESIAN_POINT('Ctrl Pts',(-10.7008526850001,12.2,0.212419018999985));
#262019=CARTESIAN_POINT('Ctrl Pts',(-10.6985416600001,12.2,0.211749948999986));
#262020=CARTESIAN_POINT('Ctrl Pts',(-10.6962361280001,12.2,0.211084637999988));
#262021=CARTESIAN_POINT('Ctrl Pts',(-10.6939361020001,12.2,0.210423081999984));
#262022=CARTESIAN_POINT('Ctrl Pts',(-10.6916415980001,12.2,0.209765271999984));
#262023=CARTESIAN_POINT('Ctrl Pts',(-10.6893526300001,12.2,0.209111201999987));
#262024=CARTESIAN_POINT('Ctrl Pts',(-10.6870692130001,12.2,0.208460869999989));
#262025=CARTESIAN_POINT('Ctrl Pts',(-10.6847913630001,12.2,0.207814266999984));
#262026=CARTESIAN_POINT('Ctrl Pts',(-10.6825190920001,12.2,0.207171386999985));
#262027=CARTESIAN_POINT('Ctrl Pts',(-10.6802524190001,12.2,0.206532224999982));
#262028=CARTESIAN_POINT('Ctrl Pts',(-10.6779913570001,12.2,0.205896773999985));
#262029=CARTESIAN_POINT('Ctrl Pts',(-10.6757359200001,12.2,0.205265028999988));
#262030=CARTESIAN_POINT('Ctrl Pts',(-10.6734861240001,12.2,0.204636982999986));
#262031=CARTESIAN_POINT('Ctrl Pts',(-10.6712419860001,12.2,0.204012629999983));
#262032=CARTESIAN_POINT('Ctrl Pts',(-10.6690035190001,12.2,0.203391963999984));
#262033=CARTESIAN_POINT('Ctrl Pts',(-10.6667707370001,12.2,0.202774979999987));
#262034=CARTESIAN_POINT('Ctrl Pts',(-10.6645436590001,12.2,0.202161669999987));
#262035=CARTESIAN_POINT('Ctrl Pts',(-10.6623222980001,12.2,0.201552028999985));
#262036=CARTESIAN_POINT('Ctrl Pts',(-10.6601066700001,12.2,0.200946048999988));
#262037=CARTESIAN_POINT('Ctrl Pts',(-10.6578967890001,12.2,0.200343724999983));
#262038=CARTESIAN_POINT('Ctrl Pts',(-10.6556926720001,12.2,0.199745050999987));
#262039=CARTESIAN_POINT('Ctrl Pts',(-10.6534943330001,12.2,0.199150019999985));
#262040=CARTESIAN_POINT('Ctrl Pts',(-10.6513017900001,12.2,0.198558625999983));
#262041=CARTESIAN_POINT('Ctrl Pts',(-10.6491150560001,12.2,0.197970862999988));
#262042=CARTESIAN_POINT('Ctrl Pts',(-10.6469341480001,12.2,0.197386722999986));
#262043=CARTESIAN_POINT('Ctrl Pts',(-10.6447590820001,12.2,0.196806200999986));
#262044=CARTESIAN_POINT('Ctrl Pts',(-10.6425898720001,12.2,0.196229288999987));
#262045=CARTESIAN_POINT('Ctrl Pts',(-10.6404265340001,12.2,0.195655982999985));
#262046=CARTESIAN_POINT('Ctrl Pts',(-10.6382690860001,12.2,0.195086272999987));
#262047=CARTESIAN_POINT('Ctrl Pts',(-10.6361175410001,12.2,0.194520154999989));
#262048=CARTESIAN_POINT('Ctrl Pts',(-10.6339719170001,12.2,0.193957621999985));
#262049=CARTESIAN_POINT('Ctrl Pts',(-10.6318322290001,12.2,0.193398666999984));
#262050=CARTESIAN_POINT('Ctrl Pts',(-10.6296984920001,12.2,0.192843283999986));
#262051=CARTESIAN_POINT('Ctrl Pts',(-10.6275707240001,12.2,0.192291463999985));
#262052=CARTESIAN_POINT('Ctrl Pts',(-10.6254489400001,12.2,0.191743201999985));
#262053=CARTESIAN_POINT('Ctrl Pts',(-10.6233331560001,12.2,0.191198491999987));
#262054=CARTESIAN_POINT('Ctrl Pts',(-10.6212233880001,12.2,0.190657325999983));
#262055=CARTESIAN_POINT('Ctrl Pts',(-10.6191196530001,12.2,0.190119695999984));
#262056=CARTESIAN_POINT('Ctrl Pts',(-10.6170219660001,12.2,0.189585598999984));
#262057=CARTESIAN_POINT('Ctrl Pts',(-10.6149303440001,12.2,0.189055023999987));
#262058=CARTESIAN_POINT('Ctrl Pts',(-10.6128448030001,12.2,0.188527964999987));
#262059=CARTESIAN_POINT('Ctrl Pts',(-10.6107653600001,12.2,0.188004416999985));
#262060=CARTESIAN_POINT('Ctrl Pts',(-10.6086920310001,12.2,0.187484370999984));
#262061=CARTESIAN_POINT('Ctrl Pts',(-10.6066248330001,12.2,0.186967819999988));
#262062=CARTESIAN_POINT('Ctrl Pts',(-10.6045637800001,12.2,0.186454757999983));
#262063=CARTESIAN_POINT('Ctrl Pts',(-10.6025088930001,12.2,0.185945177999987));
#262064=CARTESIAN_POINT('Ctrl Pts',(-10.6004601840001,12.2,0.185439070999984));
#262065=CARTESIAN_POINT('Ctrl Pts',(-10.5984176730001,12.2,0.184936432999985));
#262066=CARTESIAN_POINT('Ctrl Pts',(-10.5963813760001,12.2,0.184437252999987));
#262067=CARTESIAN_POINT('Ctrl Pts',(-10.5943513080001,12.2,0.183941525999987));
#262068=CARTESIAN_POINT('Ctrl Pts',(-10.5923274870001,12.2,0.183449243999987));
#262069=CARTESIAN_POINT('Ctrl Pts',(-10.5903099300001,12.2,0.182960399999987));
#262070=CARTESIAN_POINT('Ctrl Pts',(-10.5882986550001,12.2,0.182474987999988));
#262071=CARTESIAN_POINT('Ctrl Pts',(-10.5862936760001,12.2,0.181992998999987));
#262072=CARTESIAN_POINT('Ctrl Pts',(-10.5842950130001,12.2,0.181514424999989));
#262073=CARTESIAN_POINT('Ctrl Pts',(-10.5823026810001,12.2,0.181039259999984));
#262074=CARTESIAN_POINT('Ctrl Pts',(-10.5803166980001,12.2,0.180567494999986));
#262075=CARTESIAN_POINT('Ctrl Pts',(-10.5783370810001,12.2,0.180099124999984));
#262076=CARTESIAN_POINT('Ctrl Pts',(-10.5763638480001,12.2,0.179634139999987));
#262077=CARTESIAN_POINT('Ctrl Pts',(-10.5743970150001,12.2,0.179172532999985));
#262078=CARTESIAN_POINT('Ctrl Pts',(-10.5724365990001,12.2,0.178714295999987));
#262079=CARTESIAN_POINT('Ctrl Pts',(-10.5704826190001,12.2,0.178259422999982));
#262080=CARTESIAN_POINT('Ctrl Pts',(-10.5685350920001,12.2,0.177807903999985));
#262081=CARTESIAN_POINT('Ctrl Pts',(-10.5665940340001,12.2,0.177359733999989));
#262082=CARTESIAN_POINT('Ctrl Pts',(-10.5646594650001,12.2,0.176914901999985));
#262083=CARTESIAN_POINT('Ctrl Pts',(-10.5627314000001,12.2,0.176473403999986));
#262084=CARTESIAN_POINT('Ctrl Pts',(-10.5608098580001,12.2,0.176035227999982));
#262085=CARTESIAN_POINT('Ctrl Pts',(-10.5588948570001,12.2,0.175600368999986));
#262086=CARTESIAN_POINT('Ctrl Pts',(-10.5569864130001,12.2,0.175168818999989));
#262087=CARTESIAN_POINT('Ctrl Pts',(-10.5550845460001,12.2,0.174740567999985));
#262088=CARTESIAN_POINT('Ctrl Pts',(-10.5531892730001,12.2,0.174315608999986));
#262089=CARTESIAN_POINT('Ctrl Pts',(-10.5513006120001,12.2,0.173893933999985));
#262090=CARTESIAN_POINT('Ctrl Pts',(-10.5494185790001,12.2,0.173475535999987));
#262091=CARTESIAN_POINT('Ctrl Pts',(-10.5475431950001,12.2,0.173060405999985));
#262092=CARTESIAN_POINT('Ctrl Pts',(-10.5456744770001,12.2,0.172648534999986));
#262093=CARTESIAN_POINT('Ctrl Pts',(-10.5438124430001,12.2,0.172239915999985));
#262094=CARTESIAN_POINT('Ctrl Pts',(-10.5419571120001,12.2,0.171834540999987));
#262095=CARTESIAN_POINT('Ctrl Pts',(-10.5401085000001,12.2,0.171432399999984));
#262096=CARTESIAN_POINT('Ctrl Pts',(-10.5382666270001,12.2,0.171033485999987));
#262097=CARTESIAN_POINT('Ctrl Pts',(-10.5364315110001,12.2,0.170637790999986));
#262098=CARTESIAN_POINT('Ctrl Pts',(-10.5346031720001,12.2,0.170245304999987));
#262099=CARTESIAN_POINT('Ctrl Pts',(-10.5327816250001,12.2,0.169856020999983));
#262100=CARTESIAN_POINT('Ctrl Pts',(-10.5309668930001,12.2,0.169469929999986));
#262101=CARTESIAN_POINT('Ctrl Pts',(-10.5291589900001,12.2,0.169087022999985));
#262102=CARTESIAN_POINT('Ctrl Pts',(-10.5273579390001,12.2,0.168707291999985));
#262103=CARTESIAN_POINT('Ctrl Pts',(-10.5255637550001,12.2,0.168330728999986));
#262104=CARTESIAN_POINT('Ctrl Pts',(-10.5237764590001,12.2,0.167957323999985));
#262105=CARTESIAN_POINT('Ctrl Pts',(-10.5219960680001,12.2,0.167587068999988));
#262106=CARTESIAN_POINT('Ctrl Pts',(-10.5202226040001,12.2,0.167219955999984));
#262107=CARTESIAN_POINT('Ctrl Pts',(-10.5184560840001,12.2,0.166855974999987));
#262108=CARTESIAN_POINT('Ctrl Pts',(-10.5166965270001,12.2,0.166495116999985));
#262109=CARTESIAN_POINT('Ctrl Pts',(-10.5149439520001,12.2,0.166137374999984));
#262110=CARTESIAN_POINT('Ctrl Pts',(-10.5131983790001,12.2,0.165782736999986));
#262111=CARTESIAN_POINT('Ctrl Pts',(-10.5114598270001,12.2,0.165431196999983));
#262112=CARTESIAN_POINT('Ctrl Pts',(-10.5097283150001,12.2,0.165082744999987));
#262113=CARTESIAN_POINT('Ctrl Pts',(-10.5080038620001,12.2,0.164737371999983));
#262114=CARTESIAN_POINT('Ctrl Pts',(-10.5062864880001,12.2,0.164395067999985));
#262115=CARTESIAN_POINT('Ctrl Pts',(-10.5045762130001,12.2,0.164055823999987));
#262116=CARTESIAN_POINT('Ctrl Pts',(-10.5028730550001,12.2,0.163719632999988));
#262117=CARTESIAN_POINT('Ctrl Pts',(-10.5011770350001,12.2,0.163386482999983));
#262118=CARTESIAN_POINT('Ctrl Pts',(-10.4994881720001,12.2,0.163056365999985));
#262119=CARTESIAN_POINT('Ctrl Pts',(-10.4978064870001,12.2,0.162729272999984));
#262120=CARTESIAN_POINT('Ctrl Pts',(-10.4961320000001,12.2,0.162405193999984));
#262121=CARTESIAN_POINT('Ctrl Pts',(-10.4944647280001,12.2,0.162084120999988));
#262122=CARTESIAN_POINT('Ctrl Pts',(-10.4928046930001,12.2,0.161766040999982));
#262123=CARTESIAN_POINT('Ctrl Pts',(-10.4911519150001,12.2,0.161450947999988));
#262124=CARTESIAN_POINT('Ctrl Pts',(-10.4895064150001,12.2,0.161138831999987));
#262125=CARTESIAN_POINT('Ctrl Pts',(-10.4878682100001,12.2,0.160829682999988));
#262126=CARTESIAN_POINT('Ctrl Pts',(-10.4862373250001,12.2,0.160523489999989));
#262127=CARTESIAN_POINT('Ctrl Pts',(-10.4846137770001,12.2,0.160220243999984));
#262128=CARTESIAN_POINT('Ctrl Pts',(-10.4829975860001,12.2,0.159919936999984));
#262129=CARTESIAN_POINT('Ctrl Pts',(-10.4813887750001,12.2,0.159622555999985));
#262130=CARTESIAN_POINT('Ctrl Pts',(-10.4797873630001,12.2,0.159328093999989));
#262131=CARTESIAN_POINT('Ctrl Pts',(-10.4781933710001,12.2,0.159036539999988));
#262132=CARTESIAN_POINT('Ctrl Pts',(-10.4766068200001,12.2,0.158747883999983));
#262133=CARTESIAN_POINT('Ctrl Pts',(-10.4750277290001,12.2,0.158462115999987));
#262134=CARTESIAN_POINT('Ctrl Pts',(-10.4734561210001,12.2,0.158179226999984));
#262135=CARTESIAN_POINT('Ctrl Pts',(-10.4718920160001,12.2,0.157899203999987));
#262136=CARTESIAN_POINT('Ctrl Pts',(-10.4703354350001,12.2,0.157622039999987));
#262137=CARTESIAN_POINT('Ctrl Pts',(-10.4687864010001,12.2,0.157347723999983));
#262138=CARTESIAN_POINT('Ctrl Pts',(-10.4672449310001,12.2,0.157076244999987));
#262139=CARTESIAN_POINT('Ctrl Pts',(-10.4657110500001,12.2,0.156807592999986));
#262140=CARTESIAN_POINT('Ctrl Pts',(-10.4641847780001,12.2,0.156541757999986));
#262141=CARTESIAN_POINT('Ctrl Pts',(-10.4626661360001,12.2,0.156278728999983));
#262142=CARTESIAN_POINT('Ctrl Pts',(-10.4611551460001,12.2,0.156018495999986));
#262143=CARTESIAN_POINT('Ctrl Pts',(-10.4596518290001,12.2,0.155761047999987));
#262144=CARTESIAN_POINT('Ctrl Pts',(-10.4581562070001,12.2,0.155506375999988));
#262145=CARTESIAN_POINT('Ctrl Pts',(-10.4566683020001,12.2,0.155254465999985));
#262146=CARTESIAN_POINT('Ctrl Pts',(-10.4551881360001,12.2,0.155005310999985));
#262147=CARTESIAN_POINT('Ctrl Pts',(-10.4537157300001,12.2,0.154758897999985));
#262148=CARTESIAN_POINT('Ctrl Pts',(-10.4522511070001,12.2,0.154515216999984));
#262149=CARTESIAN_POINT('Ctrl Pts',(-10.4507942880001,12.2,0.154274255999987));
#262150=CARTESIAN_POINT('Ctrl Pts',(-10.4493452950001,12.2,0.154036006999987));
#262151=CARTESIAN_POINT('Ctrl Pts',(-10.4479041520001,12.2,0.153800454999988));
#262152=CARTESIAN_POINT('Ctrl Pts',(-10.4464708800001,12.2,0.153567592999986));
#262153=CARTESIAN_POINT('Ctrl Pts',(-10.4450455010001,12.2,0.153337406999987));
#262154=CARTESIAN_POINT('Ctrl Pts',(-10.4436280380001,12.2,0.153109886999987));
#262155=CARTESIAN_POINT('Ctrl Pts',(-10.4422185140001,12.2,0.152885022999989));
#262156=CARTESIAN_POINT('Ctrl Pts',(-10.4408169510001,12.2,0.152662800999988));
#262157=CARTESIAN_POINT('Ctrl Pts',(-10.4394233720001,12.2,0.152443211999986));
#262158=CARTESIAN_POINT('Ctrl Pts',(-10.4380378000001,12.2,0.152226242999984));
#262159=CARTESIAN_POINT('Ctrl Pts',(-10.4366602580001,12.2,0.152011882999985));
#262160=CARTESIAN_POINT('Ctrl Pts',(-10.4352907680001,12.2,0.151800122999983));
#262161=CARTESIAN_POINT('Ctrl Pts',(-10.4339293550001,12.2,0.151590946999987));
#262162=CARTESIAN_POINT('Ctrl Pts',(-10.4325760410001,12.2,0.151384346999985));
#262163=CARTESIAN_POINT('Ctrl Pts',(-10.4312308480001,12.2,0.151180308999983));
#262164=CARTESIAN_POINT('Ctrl Pts',(-10.4298938030001,12.2,0.150978822999988));
#262165=CARTESIAN_POINT('Ctrl Pts',(-10.4285649260001,12.2,0.150779875999985));
#262166=CARTESIAN_POINT('Ctrl Pts',(-10.4272442410001,12.2,0.150583456999982));
#262167=CARTESIAN_POINT('Ctrl Pts',(-10.4259317730001,12.2,0.150389553999983));
#262168=CARTESIAN_POINT('Ctrl Pts',(-10.4246275460001,12.2,0.150198153999987));
#262169=CARTESIAN_POINT('Ctrl Pts',(-10.4233315830001,12.2,0.150009245999985));
#262170=CARTESIAN_POINT('Ctrl Pts',(-10.4220439070001,12.2,0.149822816999983));
#262171=CARTESIAN_POINT('Ctrl Pts',(-10.4207645450001,12.2,0.149638854999985));
#262172=CARTESIAN_POINT('Ctrl Pts',(-10.4194935180001,12.2,0.149457348999986));
#262173=CARTESIAN_POINT('Ctrl Pts',(-10.4182308520001,12.2,0.149278284999985));
#262174=CARTESIAN_POINT('Ctrl Pts',(-10.4169765720001,12.2,0.149101651999985));
#262175=CARTESIAN_POINT('Ctrl Pts',(-10.4157307010001,12.2,0.148927436999986));
#262176=CARTESIAN_POINT('Ctrl Pts',(-10.4144932620001,12.2,0.148755626999986));
#262177=CARTESIAN_POINT('Ctrl Pts',(-10.4132642840001,12.2,0.148586209999984));
#262178=CARTESIAN_POINT('Ctrl Pts',(-10.4120437890001,12.2,0.148419172999983));
#262179=CARTESIAN_POINT('Ctrl Pts',(-10.4108318020001,12.2,0.148254502999983));
#262180=CARTESIAN_POINT('Ctrl Pts',(-10.4096283490001,12.2,0.148092186999986));
#262181=CARTESIAN_POINT('Ctrl Pts',(-10.4084334530001,12.2,0.147932213999984));
#262182=CARTESIAN_POINT('Ctrl Pts',(-10.4072471420001,12.2,0.147774568999988));
#262183=CARTESIAN_POINT('Ctrl Pts',(-10.4060694410001,12.2,0.147619239999983));
#262184=CARTESIAN_POINT('Ctrl Pts',(-10.4049003720001,12.2,0.147466213999987));
#262185=CARTESIAN_POINT('Ctrl Pts',(-10.4037399650001,12.2,0.147315476999985));
#262186=CARTESIAN_POINT('Ctrl Pts',(-10.4025882420001,12.2,0.147167016999985));
#262187=CARTESIAN_POINT('Ctrl Pts',(-10.4014452320001,12.2,0.147020818999986));
#262188=CARTESIAN_POINT('Ctrl Pts',(-10.4003109570001,12.2,0.146876870999986));
#262189=CARTESIAN_POINT('Ctrl Pts',(-10.3991854470001,12.2,0.146735159999984));
#262190=CARTESIAN_POINT('Ctrl Pts',(-10.3980687260001,12.2,0.146595670999985));
#262191=CARTESIAN_POINT('Ctrl Pts',(-10.3969608200001,12.2,0.146458390999986));
#262192=CARTESIAN_POINT('Ctrl Pts',(-10.3958617570001,12.2,0.146323306999987));
#262193=CARTESIAN_POINT('Ctrl Pts',(-10.3947715610001,12.2,0.146190402999986));
#262194=CARTESIAN_POINT('Ctrl Pts',(-10.3936902610001,12.2,0.146059668999987));
#262195=CARTESIAN_POINT('Ctrl Pts',(-10.3926178820001,12.2,0.145931086999984));
#262196=CARTESIAN_POINT('Ctrl Pts',(-10.3915544510001,12.2,0.145804645999985));
#262197=CARTESIAN_POINT('Ctrl Pts',(-10.3904999960001,12.2,0.145680330999984));
#262198=CARTESIAN_POINT('Ctrl Pts',(-10.3894545430001,12.2,0.145558126999985));
#262199=CARTESIAN_POINT('Ctrl Pts',(-10.3884181200001,12.2,0.145438019999986));
#262200=CARTESIAN_POINT('Ctrl Pts',(-10.3873907530001,12.2,0.145319995999986));
#262201=CARTESIAN_POINT('Ctrl Pts',(-10.3863724700001,12.2,0.145204041999989));
#262202=CARTESIAN_POINT('Ctrl Pts',(-10.3853633010001,12.2,0.145090140999984));
#262203=CARTESIAN_POINT('Ctrl Pts',(-10.3843632700001,12.2,0.144978280999983));
#262204=CARTESIAN_POINT('Ctrl Pts',(-10.3833724070001,12.2,0.144868444999986));
#262205=CARTESIAN_POINT('Ctrl Pts',(-10.3823907380001,12.2,0.144760619999986));
#262206=CARTESIAN_POINT('Ctrl Pts',(-10.3814182930001,12.2,0.144654789999983));
#262207=CARTESIAN_POINT('Ctrl Pts',(-10.3804551000001,12.2,0.144550940999988));
#262208=CARTESIAN_POINT('Ctrl Pts',(-10.3795011870001,12.2,0.144449057999987));
#262209=CARTESIAN_POINT('Ctrl Pts',(-10.3785565820001,12.2,0.144349124999987));
#262210=CARTESIAN_POINT('Ctrl Pts',(-10.3776213140001,12.2,0.144251127999984));
#262211=CARTESIAN_POINT('Ctrl Pts',(-10.3766954110001,12.2,0.144155049999988));
#262212=CARTESIAN_POINT('Ctrl Pts',(-10.3757841820001,12.2,0.144061419999986));
#262213=CARTESIAN_POINT('Ctrl Pts',(-10.3750636860001,12.2,0.143988113999987));
#262214=CARTESIAN_POINT('Ctrl Pts',(-10.3745287910001,12.2,0.143934095999985));
#262215=CARTESIAN_POINT('Ctrl Pts',(-10.3741757630001,12.2,0.143898618999985));
#262216=CARTESIAN_POINT('Ctrl Pts',(-10.3740022750001,12.2,0.143881226999985));
#262217=CARTESIAN_POINT('Ctrl Pts',(-10.3740022750001,15.2,0.143881226999985));
#262218=CARTESIAN_POINT('Ctrl Pts',(-10.3741757630001,15.2,0.143898618999985));
#262219=CARTESIAN_POINT('Ctrl Pts',(-10.3745287910001,15.2,0.143934095999985));
#262220=CARTESIAN_POINT('Ctrl Pts',(-10.3750636860001,15.2,0.143988113999987));
#262221=CARTESIAN_POINT('Ctrl Pts',(-10.3757841820001,15.2,0.144061419999986));
#262222=CARTESIAN_POINT('Ctrl Pts',(-10.3766954110001,15.2,0.144155049999988));
#262223=CARTESIAN_POINT('Ctrl Pts',(-10.3776213140001,15.2,0.144251127999984));
#262224=CARTESIAN_POINT('Ctrl Pts',(-10.3785565820001,15.2,0.144349124999987));
#262225=CARTESIAN_POINT('Ctrl Pts',(-10.3795011870001,15.2,0.144449057999987));
#262226=CARTESIAN_POINT('Ctrl Pts',(-10.3804551000001,15.2,0.144550940999988));
#262227=CARTESIAN_POINT('Ctrl Pts',(-10.3814182930001,15.2,0.144654789999983));
#262228=CARTESIAN_POINT('Ctrl Pts',(-10.3823907380001,15.2,0.144760619999986));
#262229=CARTESIAN_POINT('Ctrl Pts',(-10.3833724070001,15.2,0.144868444999986));
#262230=CARTESIAN_POINT('Ctrl Pts',(-10.3843632700001,15.2,0.144978280999983));
#262231=CARTESIAN_POINT('Ctrl Pts',(-10.3853633010001,15.2,0.145090140999984));
#262232=CARTESIAN_POINT('Ctrl Pts',(-10.3863724700001,15.2,0.145204041999989));
#262233=CARTESIAN_POINT('Ctrl Pts',(-10.3873907530001,15.2,0.145319995999986));
#262234=CARTESIAN_POINT('Ctrl Pts',(-10.3884181200001,15.2,0.145438019999986));
#262235=CARTESIAN_POINT('Ctrl Pts',(-10.3894545430001,15.2,0.145558126999985));
#262236=CARTESIAN_POINT('Ctrl Pts',(-10.3904999960001,15.2,0.145680330999984));
#262237=CARTESIAN_POINT('Ctrl Pts',(-10.3915544510001,15.2,0.145804645999985));
#262238=CARTESIAN_POINT('Ctrl Pts',(-10.3926178820001,15.2,0.145931086999984));
#262239=CARTESIAN_POINT('Ctrl Pts',(-10.3936902610001,15.2,0.146059668999987));
#262240=CARTESIAN_POINT('Ctrl Pts',(-10.3947715610001,15.2,0.146190402999986));
#262241=CARTESIAN_POINT('Ctrl Pts',(-10.3958617570001,15.2,0.146323306999987));
#262242=CARTESIAN_POINT('Ctrl Pts',(-10.3969608200001,15.2,0.146458390999986));
#262243=CARTESIAN_POINT('Ctrl Pts',(-10.3980687260001,15.2,0.146595670999985));
#262244=CARTESIAN_POINT('Ctrl Pts',(-10.3991854470001,15.2,0.146735159999984));
#262245=CARTESIAN_POINT('Ctrl Pts',(-10.4003109570001,15.2,0.146876870999986));
#262246=CARTESIAN_POINT('Ctrl Pts',(-10.4014452320001,15.2,0.147020818999986));
#262247=CARTESIAN_POINT('Ctrl Pts',(-10.4025882420001,15.2,0.147167016999985));
#262248=CARTESIAN_POINT('Ctrl Pts',(-10.4037399650001,15.2,0.147315476999985));
#262249=CARTESIAN_POINT('Ctrl Pts',(-10.4049003720001,15.2,0.147466213999987));
#262250=CARTESIAN_POINT('Ctrl Pts',(-10.4060694410001,15.2,0.147619239999983));
#262251=CARTESIAN_POINT('Ctrl Pts',(-10.4072471420001,15.2,0.147774568999988));
#262252=CARTESIAN_POINT('Ctrl Pts',(-10.4084334530001,15.2,0.147932213999984));
#262253=CARTESIAN_POINT('Ctrl Pts',(-10.4096283490001,15.2,0.148092186999986));
#262254=CARTESIAN_POINT('Ctrl Pts',(-10.4108318020001,15.2,0.148254502999983));
#262255=CARTESIAN_POINT('Ctrl Pts',(-10.4120437890001,15.2,0.148419172999983));
#262256=CARTESIAN_POINT('Ctrl Pts',(-10.4132642840001,15.2,0.148586209999984));
#262257=CARTESIAN_POINT('Ctrl Pts',(-10.4144932620001,15.2,0.148755626999986));
#262258=CARTESIAN_POINT('Ctrl Pts',(-10.4157307010001,15.2,0.148927436999986));
#262259=CARTESIAN_POINT('Ctrl Pts',(-10.4169765720001,15.2,0.149101651999985));
#262260=CARTESIAN_POINT('Ctrl Pts',(-10.4182308520001,15.2,0.149278284999985));
#262261=CARTESIAN_POINT('Ctrl Pts',(-10.4194935180001,15.2,0.149457348999986));
#262262=CARTESIAN_POINT('Ctrl Pts',(-10.4207645450001,15.2,0.149638854999985));
#262263=CARTESIAN_POINT('Ctrl Pts',(-10.4220439070001,15.2,0.149822816999983));
#262264=CARTESIAN_POINT('Ctrl Pts',(-10.4233315830001,15.2,0.150009245999985));
#262265=CARTESIAN_POINT('Ctrl Pts',(-10.4246275460001,15.2,0.150198153999987));
#262266=CARTESIAN_POINT('Ctrl Pts',(-10.4259317730001,15.2,0.150389553999983));
#262267=CARTESIAN_POINT('Ctrl Pts',(-10.4272442410001,15.2,0.150583456999982));
#262268=CARTESIAN_POINT('Ctrl Pts',(-10.4285649260001,15.2,0.150779875999985));
#262269=CARTESIAN_POINT('Ctrl Pts',(-10.4298938030001,15.2,0.150978822999988));
#262270=CARTESIAN_POINT('Ctrl Pts',(-10.4312308480001,15.2,0.151180308999983));
#262271=CARTESIAN_POINT('Ctrl Pts',(-10.4325760410001,15.2,0.151384346999985));
#262272=CARTESIAN_POINT('Ctrl Pts',(-10.4339293550001,15.2,0.151590946999987));
#262273=CARTESIAN_POINT('Ctrl Pts',(-10.4352907680001,15.2,0.151800122999983));
#262274=CARTESIAN_POINT('Ctrl Pts',(-10.4366602580001,15.2,0.152011882999985));
#262275=CARTESIAN_POINT('Ctrl Pts',(-10.4380378000001,15.2,0.152226242999984));
#262276=CARTESIAN_POINT('Ctrl Pts',(-10.4394233720001,15.2,0.152443211999986));
#262277=CARTESIAN_POINT('Ctrl Pts',(-10.4408169510001,15.2,0.152662800999988));
#262278=CARTESIAN_POINT('Ctrl Pts',(-10.4422185140001,15.2,0.152885022999989));
#262279=CARTESIAN_POINT('Ctrl Pts',(-10.4436280380001,15.2,0.153109886999987));
#262280=CARTESIAN_POINT('Ctrl Pts',(-10.4450455010001,15.2,0.153337406999987));
#262281=CARTESIAN_POINT('Ctrl Pts',(-10.4464708800001,15.2,0.153567592999986));
#262282=CARTESIAN_POINT('Ctrl Pts',(-10.4479041520001,15.2,0.153800454999988));
#262283=CARTESIAN_POINT('Ctrl Pts',(-10.4493452950001,15.2,0.154036006999987));
#262284=CARTESIAN_POINT('Ctrl Pts',(-10.4507942880001,15.2,0.154274255999987));
#262285=CARTESIAN_POINT('Ctrl Pts',(-10.4522511070001,15.2,0.154515216999984));
#262286=CARTESIAN_POINT('Ctrl Pts',(-10.4537157300001,15.2,0.154758897999985));
#262287=CARTESIAN_POINT('Ctrl Pts',(-10.4551881360001,15.2,0.155005310999985));
#262288=CARTESIAN_POINT('Ctrl Pts',(-10.4566683020001,15.2,0.155254465999985));
#262289=CARTESIAN_POINT('Ctrl Pts',(-10.4581562070001,15.2,0.155506375999988));
#262290=CARTESIAN_POINT('Ctrl Pts',(-10.4596518290001,15.2,0.155761047999987));
#262291=CARTESIAN_POINT('Ctrl Pts',(-10.4611551460001,15.2,0.156018495999986));
#262292=CARTESIAN_POINT('Ctrl Pts',(-10.4626661360001,15.2,0.156278728999983));
#262293=CARTESIAN_POINT('Ctrl Pts',(-10.4641847780001,15.2,0.156541757999986));
#262294=CARTESIAN_POINT('Ctrl Pts',(-10.4657110500001,15.2,0.156807592999986));
#262295=CARTESIAN_POINT('Ctrl Pts',(-10.4672449310001,15.2,0.157076244999987));
#262296=CARTESIAN_POINT('Ctrl Pts',(-10.4687864010001,15.2,0.157347723999983));
#262297=CARTESIAN_POINT('Ctrl Pts',(-10.4703354350001,15.2,0.157622039999987));
#262298=CARTESIAN_POINT('Ctrl Pts',(-10.4718920160001,15.2,0.157899203999987));
#262299=CARTESIAN_POINT('Ctrl Pts',(-10.4734561210001,15.2,0.158179226999984));
#262300=CARTESIAN_POINT('Ctrl Pts',(-10.4750277290001,15.2,0.158462115999987));
#262301=CARTESIAN_POINT('Ctrl Pts',(-10.4766068200001,15.2,0.158747883999983));
#262302=CARTESIAN_POINT('Ctrl Pts',(-10.4781933710001,15.2,0.159036539999988));
#262303=CARTESIAN_POINT('Ctrl Pts',(-10.4797873630001,15.2,0.159328093999989));
#262304=CARTESIAN_POINT('Ctrl Pts',(-10.4813887750001,15.2,0.159622555999985));
#262305=CARTESIAN_POINT('Ctrl Pts',(-10.4829975860001,15.2,0.159919936999984));
#262306=CARTESIAN_POINT('Ctrl Pts',(-10.4846137770001,15.2,0.160220243999984));
#262307=CARTESIAN_POINT('Ctrl Pts',(-10.4862373250001,15.2,0.160523489999989));
#262308=CARTESIAN_POINT('Ctrl Pts',(-10.4878682100001,15.2,0.160829682999988));
#262309=CARTESIAN_POINT('Ctrl Pts',(-10.4895064150001,15.2,0.161138831999987));
#262310=CARTESIAN_POINT('Ctrl Pts',(-10.4911519150001,15.2,0.161450947999988));
#262311=CARTESIAN_POINT('Ctrl Pts',(-10.4928046930001,15.2,0.161766040999982));
#262312=CARTESIAN_POINT('Ctrl Pts',(-10.4944647280001,15.2,0.162084120999988));
#262313=CARTESIAN_POINT('Ctrl Pts',(-10.4961320000001,15.2,0.162405193999984));
#262314=CARTESIAN_POINT('Ctrl Pts',(-10.4978064870001,15.2,0.162729272999984));
#262315=CARTESIAN_POINT('Ctrl Pts',(-10.4994881720001,15.2,0.163056365999985));
#262316=CARTESIAN_POINT('Ctrl Pts',(-10.5011770350001,15.2,0.163386482999983));
#262317=CARTESIAN_POINT('Ctrl Pts',(-10.5028730550001,15.2,0.163719632999988));
#262318=CARTESIAN_POINT('Ctrl Pts',(-10.5045762130001,15.2,0.164055823999987));
#262319=CARTESIAN_POINT('Ctrl Pts',(-10.5062864880001,15.2,0.164395067999985));
#262320=CARTESIAN_POINT('Ctrl Pts',(-10.5080038620001,15.2,0.164737371999983));
#262321=CARTESIAN_POINT('Ctrl Pts',(-10.5097283150001,15.2,0.165082744999987));
#262322=CARTESIAN_POINT('Ctrl Pts',(-10.5114598270001,15.2,0.165431196999983));
#262323=CARTESIAN_POINT('Ctrl Pts',(-10.5131983790001,15.2,0.165782736999986));
#262324=CARTESIAN_POINT('Ctrl Pts',(-10.5149439520001,15.2,0.166137374999984));
#262325=CARTESIAN_POINT('Ctrl Pts',(-10.5166965270001,15.2,0.166495116999985));
#262326=CARTESIAN_POINT('Ctrl Pts',(-10.5184560840001,15.2,0.166855974999987));
#262327=CARTESIAN_POINT('Ctrl Pts',(-10.5202226040001,15.2,0.167219955999984));
#262328=CARTESIAN_POINT('Ctrl Pts',(-10.5219960680001,15.2,0.167587068999988));
#262329=CARTESIAN_POINT('Ctrl Pts',(-10.5237764590001,15.2,0.167957323999985));
#262330=CARTESIAN_POINT('Ctrl Pts',(-10.5255637550001,15.2,0.168330728999986));
#262331=CARTESIAN_POINT('Ctrl Pts',(-10.5273579390001,15.2,0.168707291999985));
#262332=CARTESIAN_POINT('Ctrl Pts',(-10.5291589900001,15.2,0.169087022999985));
#262333=CARTESIAN_POINT('Ctrl Pts',(-10.5309668930001,15.2,0.169469929999986));
#262334=CARTESIAN_POINT('Ctrl Pts',(-10.5327816250001,15.2,0.169856020999983));
#262335=CARTESIAN_POINT('Ctrl Pts',(-10.5346031720001,15.2,0.170245304999987));
#262336=CARTESIAN_POINT('Ctrl Pts',(-10.5364315110001,15.2,0.170637790999986));
#262337=CARTESIAN_POINT('Ctrl Pts',(-10.5382666270001,15.2,0.171033485999987));
#262338=CARTESIAN_POINT('Ctrl Pts',(-10.5401085000001,15.2,0.171432399999984));
#262339=CARTESIAN_POINT('Ctrl Pts',(-10.5419571120001,15.2,0.171834540999987));
#262340=CARTESIAN_POINT('Ctrl Pts',(-10.5438124430001,15.2,0.172239915999985));
#262341=CARTESIAN_POINT('Ctrl Pts',(-10.5456744770001,15.2,0.172648534999986));
#262342=CARTESIAN_POINT('Ctrl Pts',(-10.5475431950001,15.2,0.173060405999985));
#262343=CARTESIAN_POINT('Ctrl Pts',(-10.5494185790001,15.2,0.173475535999987));
#262344=CARTESIAN_POINT('Ctrl Pts',(-10.5513006120001,15.2,0.173893933999985));
#262345=CARTESIAN_POINT('Ctrl Pts',(-10.5531892730001,15.2,0.174315608999986));
#262346=CARTESIAN_POINT('Ctrl Pts',(-10.5550845460001,15.2,0.174740567999985));
#262347=CARTESIAN_POINT('Ctrl Pts',(-10.5569864130001,15.2,0.175168818999989));
#262348=CARTESIAN_POINT('Ctrl Pts',(-10.5588948570001,15.2,0.175600368999986));
#262349=CARTESIAN_POINT('Ctrl Pts',(-10.5608098580001,15.2,0.176035227999982));
#262350=CARTESIAN_POINT('Ctrl Pts',(-10.5627314000001,15.2,0.176473403999986));
#262351=CARTESIAN_POINT('Ctrl Pts',(-10.5646594650001,15.2,0.176914901999985));
#262352=CARTESIAN_POINT('Ctrl Pts',(-10.5665940340001,15.2,0.177359733999989));
#262353=CARTESIAN_POINT('Ctrl Pts',(-10.5685350920001,15.2,0.177807903999985));
#262354=CARTESIAN_POINT('Ctrl Pts',(-10.5704826190001,15.2,0.178259422999982));
#262355=CARTESIAN_POINT('Ctrl Pts',(-10.5724365990001,15.2,0.178714295999987));
#262356=CARTESIAN_POINT('Ctrl Pts',(-10.5743970150001,15.2,0.179172532999985));
#262357=CARTESIAN_POINT('Ctrl Pts',(-10.5763638480001,15.2,0.179634139999987));
#262358=CARTESIAN_POINT('Ctrl Pts',(-10.5783370810001,15.2,0.180099124999984));
#262359=CARTESIAN_POINT('Ctrl Pts',(-10.5803166980001,15.2,0.180567494999986));
#262360=CARTESIAN_POINT('Ctrl Pts',(-10.5823026810001,15.2,0.181039259999984));
#262361=CARTESIAN_POINT('Ctrl Pts',(-10.5842950130001,15.2,0.181514424999989));
#262362=CARTESIAN_POINT('Ctrl Pts',(-10.5862936760001,15.2,0.181992998999987));
#262363=CARTESIAN_POINT('Ctrl Pts',(-10.5882986550001,15.2,0.182474987999988));
#262364=CARTESIAN_POINT('Ctrl Pts',(-10.5903099300001,15.2,0.182960399999987));
#262365=CARTESIAN_POINT('Ctrl Pts',(-10.5923274870001,15.2,0.183449243999987));
#262366=CARTESIAN_POINT('Ctrl Pts',(-10.5943513080001,15.2,0.183941525999987));
#262367=CARTESIAN_POINT('Ctrl Pts',(-10.5963813760001,15.2,0.184437252999987));
#262368=CARTESIAN_POINT('Ctrl Pts',(-10.5984176730001,15.2,0.184936432999985));
#262369=CARTESIAN_POINT('Ctrl Pts',(-10.6004601840001,15.2,0.185439070999984));
#262370=CARTESIAN_POINT('Ctrl Pts',(-10.6025088930001,15.2,0.185945177999987));
#262371=CARTESIAN_POINT('Ctrl Pts',(-10.6045637800001,15.2,0.186454757999983));
#262372=CARTESIAN_POINT('Ctrl Pts',(-10.6066248330001,15.2,0.186967819999988));
#262373=CARTESIAN_POINT('Ctrl Pts',(-10.6086920310001,15.2,0.187484370999984));
#262374=CARTESIAN_POINT('Ctrl Pts',(-10.6107653600001,15.2,0.188004416999985));
#262375=CARTESIAN_POINT('Ctrl Pts',(-10.6128448030001,15.2,0.188527964999987));
#262376=CARTESIAN_POINT('Ctrl Pts',(-10.6149303440001,15.2,0.189055023999987));
#262377=CARTESIAN_POINT('Ctrl Pts',(-10.6170219660001,15.2,0.189585598999984));
#262378=CARTESIAN_POINT('Ctrl Pts',(-10.6191196530001,15.2,0.190119695999984));
#262379=CARTESIAN_POINT('Ctrl Pts',(-10.6212233880001,15.2,0.190657325999983));
#262380=CARTESIAN_POINT('Ctrl Pts',(-10.6233331560001,15.2,0.191198491999987));
#262381=CARTESIAN_POINT('Ctrl Pts',(-10.6254489400001,15.2,0.191743201999985));
#262382=CARTESIAN_POINT('Ctrl Pts',(-10.6275707240001,15.2,0.192291463999985));
#262383=CARTESIAN_POINT('Ctrl Pts',(-10.6296984920001,15.2,0.192843283999986));
#262384=CARTESIAN_POINT('Ctrl Pts',(-10.6318322290001,15.2,0.193398666999984));
#262385=CARTESIAN_POINT('Ctrl Pts',(-10.6339719170001,15.2,0.193957621999985));
#262386=CARTESIAN_POINT('Ctrl Pts',(-10.6361175410001,15.2,0.194520154999989));
#262387=CARTESIAN_POINT('Ctrl Pts',(-10.6382690860001,15.2,0.195086272999987));
#262388=CARTESIAN_POINT('Ctrl Pts',(-10.6404265340001,15.2,0.195655982999985));
#262389=CARTESIAN_POINT('Ctrl Pts',(-10.6425898720001,15.2,0.196229288999987));
#262390=CARTESIAN_POINT('Ctrl Pts',(-10.6447590820001,15.2,0.196806200999986));
#262391=CARTESIAN_POINT('Ctrl Pts',(-10.6469341480001,15.2,0.197386722999986));
#262392=CARTESIAN_POINT('Ctrl Pts',(-10.6491150560001,15.2,0.197970862999988));
#262393=CARTESIAN_POINT('Ctrl Pts',(-10.6513017900001,15.2,0.198558625999983));
#262394=CARTESIAN_POINT('Ctrl Pts',(-10.6534943330001,15.2,0.199150019999985));
#262395=CARTESIAN_POINT('Ctrl Pts',(-10.6556926720001,15.2,0.199745050999987));
#262396=CARTESIAN_POINT('Ctrl Pts',(-10.6578967890001,15.2,0.200343724999983));
#262397=CARTESIAN_POINT('Ctrl Pts',(-10.6601066700001,15.2,0.200946048999988));
#262398=CARTESIAN_POINT('Ctrl Pts',(-10.6623222980001,15.2,0.201552028999985));
#262399=CARTESIAN_POINT('Ctrl Pts',(-10.6645436590001,15.2,0.202161669999987));
#262400=CARTESIAN_POINT('Ctrl Pts',(-10.6667707370001,15.2,0.202774979999987));
#262401=CARTESIAN_POINT('Ctrl Pts',(-10.6690035190001,15.2,0.203391963999984));
#262402=CARTESIAN_POINT('Ctrl Pts',(-10.6712419860001,15.2,0.204012629999983));
#262403=CARTESIAN_POINT('Ctrl Pts',(-10.6734861240001,15.2,0.204636982999986));
#262404=CARTESIAN_POINT('Ctrl Pts',(-10.6757359200001,15.2,0.205265028999988));
#262405=CARTESIAN_POINT('Ctrl Pts',(-10.6779913570001,15.2,0.205896773999985));
#262406=CARTESIAN_POINT('Ctrl Pts',(-10.6802524190001,15.2,0.206532224999982));
#262407=CARTESIAN_POINT('Ctrl Pts',(-10.6825190920001,15.2,0.207171386999985));
#262408=CARTESIAN_POINT('Ctrl Pts',(-10.6847913630001,15.2,0.207814266999984));
#262409=CARTESIAN_POINT('Ctrl Pts',(-10.6870692130001,15.2,0.208460869999989));
#262410=CARTESIAN_POINT('Ctrl Pts',(-10.6893526300001,15.2,0.209111201999987));
#262411=CARTESIAN_POINT('Ctrl Pts',(-10.6916415980001,15.2,0.209765271999984));
#262412=CARTESIAN_POINT('Ctrl Pts',(-10.6939361020001,15.2,0.210423081999984));
#262413=CARTESIAN_POINT('Ctrl Pts',(-10.6962361280001,15.2,0.211084637999988));
#262414=CARTESIAN_POINT('Ctrl Pts',(-10.6985416600001,15.2,0.211749948999986));
#262415=CARTESIAN_POINT('Ctrl Pts',(-10.7008526850001,15.2,0.212419018999985));
#262416=CARTESIAN_POINT('Ctrl Pts',(-10.7031691860001,15.2,0.213091852999985));
#262417=CARTESIAN_POINT('Ctrl Pts',(-10.7054911500001,15.2,0.213768457999985));
#262418=CARTESIAN_POINT('Ctrl Pts',(-10.7078185620001,15.2,0.214448838999988));
#262419=CARTESIAN_POINT('Ctrl Pts',(-10.7101514080001,15.2,0.215133002999988));
#262420=CARTESIAN_POINT('Ctrl Pts',(-10.7124896730001,15.2,0.215820953999986));
#262421=CARTESIAN_POINT('Ctrl Pts',(-10.7148333410001,15.2,0.216512699999987));
#262422=CARTESIAN_POINT('Ctrl Pts',(-10.7171823990001,15.2,0.217208243999987));
#262423=CARTESIAN_POINT('Ctrl Pts',(-10.7195368330001,15.2,0.217907592999986));
#262424=CARTESIAN_POINT('Ctrl Pts',(-10.7218966280001,15.2,0.218610753999986));
#262425=CARTESIAN_POINT('Ctrl Pts',(-10.7242617690001,15.2,0.219317729999986));
#262426=CARTESIAN_POINT('Ctrl Pts',(-10.7266322420001,15.2,0.220028526999982));
#262427=CARTESIAN_POINT('Ctrl Pts',(-10.7290080330001,15.2,0.220743150999985));
#262428=CARTESIAN_POINT('Ctrl Pts',(-10.7313891280001,15.2,0.221461608999984));
#262429=CARTESIAN_POINT('Ctrl Pts',(-10.7337755120001,15.2,0.222183903999986));
#262430=CARTESIAN_POINT('Ctrl Pts',(-10.7361671710001,15.2,0.222910043999986));
#262431=CARTESIAN_POINT('Ctrl Pts',(-10.7385640920001,15.2,0.223640032999985));
#262432=CARTESIAN_POINT('Ctrl Pts',(-10.7409662590001,15.2,0.224373874999984));
#262433=CARTESIAN_POINT('Ctrl Pts',(-10.7433736600001,15.2,0.225111577999986));
#262434=CARTESIAN_POINT('Ctrl Pts',(-10.7457862770001,15.2,0.225853145999988));
#262435=CARTESIAN_POINT('Ctrl Pts',(-10.7482041010001,15.2,0.226598583999986));
#262436=CARTESIAN_POINT('Ctrl Pts',(-10.7506271160001,15.2,0.227347897999985));
#262437=CARTESIAN_POINT('Ctrl Pts',(-10.7530553070001,15.2,0.228101093999986));
#262438=CARTESIAN_POINT('Ctrl Pts',(-10.7554886610001,15.2,0.228858175999989));
#262439=CARTESIAN_POINT('Ctrl Pts',(-10.7579271630001,15.2,0.229619148999984));
#262440=CARTESIAN_POINT('Ctrl Pts',(-10.7603708020001,15.2,0.230384019999987));
#262441=CARTESIAN_POINT('Ctrl Pts',(-10.7628195610001,15.2,0.231152792999989));
#262442=CARTESIAN_POINT('Ctrl Pts',(-10.7652734280001,15.2,0.231925471999985));
#262443=CARTESIAN_POINT('Ctrl Pts',(-10.7677323890001,15.2,0.232702063999985));
#262444=CARTESIAN_POINT('Ctrl Pts',(-10.7701964290001,15.2,0.233482572999986));
#262445=CARTESIAN_POINT('Ctrl Pts',(-10.7726655360001,15.2,0.234267004999986));
#262446=CARTESIAN_POINT('Ctrl Pts',(-10.7751396960001,15.2,0.235055364999983));
#262447=CARTESIAN_POINT('Ctrl Pts',(-10.7776188950001,15.2,0.235847656999986));
#262448=CARTESIAN_POINT('Ctrl Pts',(-10.7801031190001,15.2,0.236643886999985));
#262449=CARTESIAN_POINT('Ctrl Pts',(-10.7825923560001,15.2,0.237444060999987));
#262450=CARTESIAN_POINT('Ctrl Pts',(-10.7850865910001,15.2,0.238248179999987));
#262451=CARTESIAN_POINT('Ctrl Pts',(-10.7875858100001,15.2,0.239056253999985));
#262452=CARTESIAN_POINT('Ctrl Pts',(-10.7900900010001,15.2,0.239868283999982));
#262453=CARTESIAN_POINT('Ctrl Pts',(-10.7925991510001,15.2,0.240684276999983));
#262454=CARTESIAN_POINT('Ctrl Pts',(-10.7951132440001,15.2,0.241504237999983));
#262455=CARTESIAN_POINT('Ctrl Pts',(-10.7976322700001,15.2,0.242328170999984));
#262456=CARTESIAN_POINT('Ctrl Pts',(-10.8001562130001,15.2,0.243156080999984));
#262457=CARTESIAN_POINT('Ctrl Pts',(-10.8026850610001,15.2,0.243987971999986));
#262458=CARTESIAN_POINT('Ctrl Pts',(-10.8052187990001,15.2,0.244823850999989));
#262459=CARTESIAN_POINT('Ctrl Pts',(-10.8077574170001,15.2,0.245663720999989));
#262460=CARTESIAN_POINT('Ctrl Pts',(-10.8103008990001,15.2,0.246507586999982));
#262461=CARTESIAN_POINT('Ctrl Pts',(-10.8128492330001,15.2,0.247355453999987));
#262462=CARTESIAN_POINT('Ctrl Pts',(-10.8154024050001,15.2,0.248207326999985));
#262463=CARTESIAN_POINT('Ctrl Pts',(-10.8179604030001,15.2,0.249063209999987));
#262464=CARTESIAN_POINT('Ctrl Pts',(-10.8205232130001,15.2,0.249923108999983));
#262465=CARTESIAN_POINT('Ctrl Pts',(-10.8230908230001,15.2,0.250787025999983));
#262466=CARTESIAN_POINT('Ctrl Pts',(-10.8256632200001,15.2,0.251654968999984));
#262467=CARTESIAN_POINT('Ctrl Pts',(-10.8282403890001,15.2,0.252526939999989));
#262468=CARTESIAN_POINT('Ctrl Pts',(-10.8308223180001,15.2,0.253402943999985));
#262469=CARTESIAN_POINT('Ctrl Pts',(-10.8334089940001,15.2,0.254282987999983));
#262470=CARTESIAN_POINT('Ctrl Pts',(-10.8360004070001,15.2,0.255167072999987));
#262471=CARTESIAN_POINT('Ctrl Pts',(-10.8385965390001,15.2,0.256055205999988));
#262472=CARTESIAN_POINT('Ctrl Pts',(-10.8411973810001,15.2,0.256947389999986));
#262473=CARTESIAN_POINT('Ctrl Pts',(-10.8438029180001,15.2,0.257843629999983));
#262474=CARTESIAN_POINT('Ctrl Pts',(-10.8464131390001,15.2,0.258743930999987));
#262475=CARTESIAN_POINT('Ctrl Pts',(-10.8490280300001,15.2,0.259648296999986));
#262476=CARTESIAN_POINT('Ctrl Pts',(-10.8516475780001,15.2,0.260556731999984));
#262477=CARTESIAN_POINT('Ctrl Pts',(-10.8542717720001,15.2,0.261469240999985));
#262478=CARTESIAN_POINT('Ctrl Pts',(-10.8569005980001,15.2,0.262385827999987));
#262479=CARTESIAN_POINT('Ctrl Pts',(-10.8595340430001,15.2,0.263306497999984));
#262480=CARTESIAN_POINT('Ctrl Pts',(-10.8621720950001,15.2,0.264231254999987));
#262481=CARTESIAN_POINT('Ctrl Pts',(-10.8648147410001,15.2,0.265160102999986));
#262482=CARTESIAN_POINT('Ctrl Pts',(-10.8674619700001,15.2,0.266093045999987));
#262483=CARTESIAN_POINT('Ctrl Pts',(-10.8701137680001,15.2,0.267030089999984));
#262484=CARTESIAN_POINT('Ctrl Pts',(-10.8727701220001,15.2,0.267971236999984));
#262485=CARTESIAN_POINT('Ctrl Pts',(-10.8754310200001,15.2,0.268916491999986));
#262486=CARTESIAN_POINT('Ctrl Pts',(-10.8780964490001,15.2,0.269865860999987));
#262487=CARTESIAN_POINT('Ctrl Pts',(-10.8807663990001,15.2,0.270819344999986));
#262488=CARTESIAN_POINT('Ctrl Pts',(-10.8834408550001,15.2,0.271776950999989));
#262489=CARTESIAN_POINT('Ctrl Pts',(-10.8861198050001,15.2,0.272738680999982));
#262490=CARTESIAN_POINT('Ctrl Pts',(-10.8888032380001,15.2,0.273704540999984));
#262491=CARTESIAN_POINT('Ctrl Pts',(-10.8914911410001,15.2,0.274674534999986));
#262492=CARTESIAN_POINT('Ctrl Pts',(-10.8941835000001,15.2,0.275648664999988));
#262493=CARTESIAN_POINT('Ctrl Pts',(-10.8968803070001,15.2,0.276626936999986));
#262494=CARTESIAN_POINT('Ctrl Pts',(-10.8995815450001,15.2,0.277609353999986));
#262495=CARTESIAN_POINT('Ctrl Pts',(-10.9022872040001,15.2,0.278595920999987));
#262496=CARTESIAN_POINT('Ctrl Pts',(-10.9049972710001,15.2,0.279586640999985));
#262497=CARTESIAN_POINT('Ctrl Pts',(-10.9077117350001,15.2,0.280581520999985));
#262498=CARTESIAN_POINT('Ctrl Pts',(-10.9104305830001,15.2,0.281580559999988));
#262499=CARTESIAN_POINT('Ctrl Pts',(-10.9131538030001,15.2,0.282583765999984));
#262500=CARTESIAN_POINT('Ctrl Pts',(-10.9158813840001,15.2,0.283591140999988));
#262501=CARTESIAN_POINT('Ctrl Pts',(-10.9186133120001,15.2,0.284602688999982));
#262502=CARTESIAN_POINT('Ctrl Pts',(-10.9213495760001,15.2,0.285618414999984));
#262503=CARTESIAN_POINT('Ctrl Pts',(-10.9240901640001,15.2,0.286638322999986));
#262504=CARTESIAN_POINT('Ctrl Pts',(-10.9268350640001,15.2,0.287662414999983));
#262505=CARTESIAN_POINT('Ctrl Pts',(-10.9295842640001,15.2,0.288690695999985));
#262506=CARTESIAN_POINT('Ctrl Pts',(-10.9323377520001,15.2,0.289723170999987));
#262507=CARTESIAN_POINT('Ctrl Pts',(-10.9350955160001,15.2,0.290759840999986));
#262508=CARTESIAN_POINT('Ctrl Pts',(-10.9378575430001,15.2,0.291800712999986));
#262509=CARTESIAN_POINT('Ctrl Pts',(-10.9406238230001,15.2,0.292845787999987));
#262510=CARTESIAN_POINT('Ctrl Pts',(-10.9433943440001,15.2,0.293895071999986));
#262511=CARTESIAN_POINT('Ctrl Pts',(-10.9461690940001,15.2,0.294948567999986));
#262512=CARTESIAN_POINT('Ctrl Pts',(-10.9489480600001,15.2,0.296006278999985));
#262513=CARTESIAN_POINT('Ctrl Pts',(-10.9517312310001,15.2,0.297068208999987));
#262514=CARTESIAN_POINT('Ctrl Pts',(-10.9545185950001,15.2,0.298134361999987));
#262515=CARTESIAN_POINT('Ctrl Pts',(-10.9573101410001,15.2,0.299204742999986));
#262516=CARTESIAN_POINT('Ctrl Pts',(-10.9601058580001,15.2,0.300279352999984));
#262517=CARTESIAN_POINT('Ctrl Pts',(-10.9629057310001,15.2,0.301358197999986));
#262518=CARTESIAN_POINT('Ctrl Pts',(-10.9657097520001,15.2,0.302441278999983));
#262519=CARTESIAN_POINT('Ctrl Pts',(-10.9685179070001,15.2,0.303528602999985));
#262520=CARTESIAN_POINT('Ctrl Pts',(-10.9713301870001,15.2,0.304620170999983));
#262521=CARTESIAN_POINT('Ctrl Pts',(-10.9741465770001,15.2,0.305715986999986));
#262522=CARTESIAN_POINT('Ctrl Pts',(-10.9769670670001,15.2,0.306816054999985));
#262523=CARTESIAN_POINT('Ctrl Pts',(-10.9797916470001,15.2,0.307920378999986));
#262524=CARTESIAN_POINT('Ctrl Pts',(-10.9826203020001,15.2,0.309028961999989));
#262525=CARTESIAN_POINT('Ctrl Pts',(-10.9854530250001,15.2,0.310141807999984));
#262526=CARTESIAN_POINT('Ctrl Pts',(-10.9882898000001,15.2,0.311258919999986));
#262527=CARTESIAN_POINT('Ctrl Pts',(-10.9911306190001,15.2,0.312380299999986));
#262528=CARTESIAN_POINT('Ctrl Pts',(-10.9939754690001,15.2,0.313505953999984));
#262529=CARTESIAN_POINT('Ctrl Pts',(-10.9968243390001,15.2,0.314635884999985));
#262530=CARTESIAN_POINT('Ctrl Pts',(-10.9996772170001,15.2,0.315770094999985));
#262531=CARTESIAN_POINT('Ctrl Pts',(-11.0025340930001,15.2,0.316908588999985));
#262532=CARTESIAN_POINT('Ctrl Pts',(-11.0053949540001,15.2,0.318051369999988));
#262533=CARTESIAN_POINT('Ctrl Pts',(-11.0082597890001,15.2,0.319198439999986));
#262534=CARTESIAN_POINT('Ctrl Pts',(-11.0111285880001,15.2,0.320349803999989));
#262535=CARTESIAN_POINT('Ctrl Pts',(-11.0140013380001,15.2,0.321505463999987));
#262536=CARTESIAN_POINT('Ctrl Pts',(-11.0168780300001,15.2,0.322665424999986));
#262537=CARTESIAN_POINT('Ctrl Pts',(-11.0197586510001,15.2,0.323829688999986));
#262538=CARTESIAN_POINT('Ctrl Pts',(-11.0226431890001,15.2,0.324998259999987));
#262539=CARTESIAN_POINT('Ctrl Pts',(-11.0255316350001,15.2,0.326171140999989));
#262540=CARTESIAN_POINT('Ctrl Pts',(-11.0284239770001,15.2,0.327348335999984));
#262541=CARTESIAN_POINT('Ctrl Pts',(-11.0313202040001,15.2,0.328529845999985));
#262542=CARTESIAN_POINT('Ctrl Pts',(-11.0342203030001,15.2,0.329715676999989));
#262543=CARTESIAN_POINT('Ctrl Pts',(-11.0371242670001,15.2,0.330905830999986));
#262544=CARTESIAN_POINT('Ctrl Pts',(-11.0400320810001,15.2,0.332100310999985));
#262545=CARTESIAN_POINT('Ctrl Pts',(-11.0429437360001,15.2,0.333299120999988));
#262546=CARTESIAN_POINT('Ctrl Pts',(-11.0458592200001,15.2,0.334502262999985));
#262547=CARTESIAN_POINT('Ctrl Pts',(-11.0487785220001,15.2,0.335709739999985));
#262548=CARTESIAN_POINT('Ctrl Pts',(-11.0517016320001,15.2,0.336921557999985));
#262549=CARTESIAN_POINT('Ctrl Pts',(-11.0546285370001,15.2,0.338137715999984));
#262550=CARTESIAN_POINT('Ctrl Pts',(-11.0575592300001,15.2,0.339358219999983));
#262551=CARTESIAN_POINT('Ctrl Pts',(-11.0604936960001,15.2,0.340583071999987));
#262552=CARTESIAN_POINT('Ctrl Pts',(-11.0634319250001,15.2,0.341812274999986));
#262553=CARTESIAN_POINT('Ctrl Pts',(-11.0663739070001,15.2,0.343045833999986));
#262554=CARTESIAN_POINT('Ctrl Pts',(-11.0693196320001,15.2,0.344283748999987));
#262555=CARTESIAN_POINT('Ctrl Pts',(-11.0722690870001,15.2,0.345526024999985));
#262556=CARTESIAN_POINT('Ctrl Pts',(-11.0752222620001,15.2,0.346772664999988));
#262557=CARTESIAN_POINT('Ctrl Pts',(-11.0781791480001,15.2,0.348023670999984));
#262558=CARTESIAN_POINT('Ctrl Pts',(-11.0811397300001,15.2,0.349279046999986));
#262559=CARTESIAN_POINT('Ctrl Pts',(-11.0841040020001,15.2,0.350538794999986));
#262560=CARTESIAN_POINT('Ctrl Pts',(-11.0870719500001,15.2,0.351802918999984));
#262561=CARTESIAN_POINT('Ctrl Pts',(-11.0900435650001,15.2,0.353071420999989));
#262562=CARTESIAN_POINT('Ctrl Pts',(-11.0930188360001,15.2,0.354344304999987));
#262563=CARTESIAN_POINT('Ctrl Pts',(-11.0959977500001,15.2,0.355621572999985));
#262564=CARTESIAN_POINT('Ctrl Pts',(-11.0989803000001,15.2,0.356903227999985));
#262565=CARTESIAN_POINT('Ctrl Pts',(-11.1019664740001,15.2,0.358189272999985));
#262566=CARTESIAN_POINT('Ctrl Pts',(-11.1049562600001,15.2,0.359479711999988));
#262567=CARTESIAN_POINT('Ctrl Pts',(-11.1079496490001,15.2,0.360774545999987));
#262568=CARTESIAN_POINT('Ctrl Pts',(-11.1109466290001,15.2,0.362073778999985));
#262569=CARTESIAN_POINT('Ctrl Pts',(-11.1139471900001,15.2,0.363377413999988));
#262570=CARTESIAN_POINT('Ctrl Pts',(-11.1169513230001,15.2,0.364685452999982));
#262571=CARTESIAN_POINT('Ctrl Pts',(-11.1199590150001,15.2,0.365997898999986));
#262572=CARTESIAN_POINT('Ctrl Pts',(-11.1229702580001,15.2,0.367314754999986));
#262573=CARTESIAN_POINT('Ctrl Pts',(-11.1259850390001,15.2,0.368636023999986));
#262574=CARTESIAN_POINT('Ctrl Pts',(-11.1290033490001,15.2,0.369961708999984));
#262575=CARTESIAN_POINT('Ctrl Pts',(-11.1320251780001,15.2,0.371291811999988));
#262576=CARTESIAN_POINT('Ctrl Pts',(-11.1350505130001,15.2,0.372626335999984));
#262577=CARTESIAN_POINT('Ctrl Pts',(-11.1380793470001,15.2,0.373965283999986));
#262578=CARTESIAN_POINT('Ctrl Pts',(-11.1411116670001,15.2,0.375308657999986));
#262579=CARTESIAN_POINT('Ctrl Pts',(-11.1441474640001,15.2,0.376656461999989));
#262580=CARTESIAN_POINT('Ctrl Pts',(-11.1471867270001,15.2,0.378008696999985));
#262581=CARTESIAN_POINT('Ctrl Pts',(-11.1502294460001,15.2,0.379365366999984));
#262582=CARTESIAN_POINT('Ctrl Pts',(-11.1532756110001,15.2,0.380726473999986));
#262583=CARTESIAN_POINT('Ctrl Pts',(-11.1563252100001,15.2,0.382092021999987));
#262584=CARTESIAN_POINT('Ctrl Pts',(-11.1593782350001,15.2,0.383462010999986));
#262585=CARTESIAN_POINT('Ctrl Pts',(-11.1624346740001,15.2,0.384836445999985));
#262586=CARTESIAN_POINT('Ctrl Pts',(-11.1654945190001,15.2,0.386215327999988));
#262587=CARTESIAN_POINT('Ctrl Pts',(-11.1685577570001,15.2,0.387598660999986));
#262588=CARTESIAN_POINT('Ctrl Pts',(-11.1716243780001,15.2,0.388986446999984));
#262589=CARTESIAN_POINT('Ctrl Pts',(-11.1746943740001,15.2,0.390378687999986));
#262590=CARTESIAN_POINT('Ctrl Pts',(-11.1777677340001,15.2,0.391775386999988));
#262591=CARTESIAN_POINT('Ctrl Pts',(-11.1808444470001,15.2,0.393176545999987));
#262592=CARTESIAN_POINT('Ctrl Pts',(-11.1839245020001,15.2,0.394582169999986));
#262593=CARTESIAN_POINT('Ctrl Pts',(-11.1870078920001,15.2,0.395992257999982));
#262594=CARTESIAN_POINT('Ctrl Pts',(-11.1900946040001,15.2,0.397406813999983));
#262595=CARTESIAN_POINT('Ctrl Pts',(-11.1931846300001,15.2,0.398825840999986));
#262596=CARTESIAN_POINT('Ctrl Pts',(-11.1962779570001,15.2,0.400249341999985));
#262597=CARTESIAN_POINT('Ctrl Pts',(-11.1993745780001,15.2,0.401677316999987));
#262598=CARTESIAN_POINT('Ctrl Pts',(-11.2024744820001,15.2,0.403109771999985));
#262599=CARTESIAN_POINT('Ctrl Pts',(-11.2055776580001,15.2,0.404546704999986));
#262600=CARTESIAN_POINT('Ctrl Pts',(-11.2086840970001,15.2,0.405988122999985));
#262601=CARTESIAN_POINT('Ctrl Pts',(-11.2117937880001,15.2,0.407434024999986));
#262602=CARTESIAN_POINT('Ctrl Pts',(-11.2149067230001,15.2,0.408884414999986));
#262603=CARTESIAN_POINT('Ctrl Pts',(-11.2180228910001,15.2,0.410339293999984));
#262604=CARTESIAN_POINT('Ctrl Pts',(-11.2211422810001,15.2,0.411798666999985));
#262605=CARTESIAN_POINT('Ctrl Pts',(-11.2242648840001,15.2,0.413262533999985));
#262606=CARTESIAN_POINT('Ctrl Pts',(-11.2273906900001,15.2,0.414730897999984));
#262607=CARTESIAN_POINT('Ctrl Pts',(-11.2305196890001,15.2,0.416203761999987));
#262608=CARTESIAN_POINT('Ctrl Pts',(-11.2336518720001,15.2,0.417681126999985));
#262609=CARTESIAN_POINT('Ctrl Pts',(-11.2367872280001,15.2,0.419162996999987));
#262610=CARTESIAN_POINT('Ctrl Pts',(-11.2399257470001,15.2,0.420649372999984));
#262611=CARTESIAN_POINT('Ctrl Pts',(-11.2430674210001,15.2,0.422140256999985));
#262612=CARTESIAN_POINT('Ctrl Pts',(-11.2462122380001,15.2,0.423635652999987));
#262613=CARTESIAN_POINT('Ctrl Pts',(-11.2493601900001,15.2,0.425135561999985));
#262614=CARTESIAN_POINT('Ctrl Pts',(-11.2525112650001,15.2,0.426639985999984));
#262615=CARTESIAN_POINT('Ctrl Pts',(-11.2556654560001,15.2,0.428148927999987));
#262616=CARTESIAN_POINT('Ctrl Pts',(-11.2588227510001,15.2,0.429662389999983));
#262617=CARTESIAN_POINT('Ctrl Pts',(-11.2619831420001,15.2,0.431180374999984));
#262618=CARTESIAN_POINT('Ctrl Pts',(-11.2651466170001,15.2,0.432702882999987));
#262619=CARTESIAN_POINT('Ctrl Pts',(-11.2683131690001,15.2,0.434229917999982));
#262620=CARTESIAN_POINT('Ctrl Pts',(-11.2714827870001,15.2,0.435761481999983));
#262621=CARTESIAN_POINT('Ctrl Pts',(-11.2746554610001,15.2,0.437297575999986));
#262622=CARTESIAN_POINT('Ctrl Pts',(-11.2778311820001,15.2,0.438838203999987));
#262623=CARTESIAN_POINT('Ctrl Pts',(-11.2810099400001,15.2,0.440383366999986));
#262624=CARTESIAN_POINT('Ctrl Pts',(-11.2841917260001,15.2,0.441933066999987));
#262625=CARTESIAN_POINT('Ctrl Pts',(-11.2873765290001,15.2,0.443487306999986));
#262626=CARTESIAN_POINT('Ctrl Pts',(-11.2905643410001,15.2,0.445046087999987));
#262627=CARTESIAN_POINT('Ctrl Pts',(-11.2937551520001,15.2,0.446609412999983));
#262628=CARTESIAN_POINT('Ctrl Pts',(-11.2969489510001,15.2,0.448177283999982));
#262629=CARTESIAN_POINT('Ctrl Pts',(-11.3001457320001,15.2,0.449749702999984));
#262630=CARTESIAN_POINT('Ctrl Pts',(-11.3033454810001,15.2,0.451326670999985));
#262631=CARTESIAN_POINT('Ctrl Pts',(-11.3065481920001,15.2,0.452908190999985));
#262632=CARTESIAN_POINT('Ctrl Pts',(-11.3097538530001,15.2,0.454494265999985));
#262633=CARTESIAN_POINT('Ctrl Pts',(-11.3129624580001,15.2,0.456084895999984));
#262634=CARTESIAN_POINT('Ctrl Pts',(-11.3161739920001,15.2,0.457680083999983));
#262635=CARTESIAN_POINT('Ctrl Pts',(-11.3193884510001,15.2,0.459279831999986));
#262636=CARTESIAN_POINT('Ctrl Pts',(-11.3226058230001,15.2,0.460884142999984));
#262637=CARTESIAN_POINT('Ctrl Pts',(-11.3258260990001,15.2,0.462493017999983));
#262638=CARTESIAN_POINT('Ctrl Pts',(-11.3290492700001,15.2,0.464106457999982));
#262639=CARTESIAN_POINT('Ctrl Pts',(-11.3322753250001,15.2,0.465724465999986));
#262640=CARTESIAN_POINT('Ctrl Pts',(-11.3355042560001,15.2,0.467347044999986));
#262641=CARTESIAN_POINT('Ctrl Pts',(-11.3387360540001,15.2,0.468974193999987));
#262642=CARTESIAN_POINT('Ctrl Pts',(-11.3419707090001,15.2,0.470605916999984));
#262643=CARTESIAN_POINT('Ctrl Pts',(-11.3452082120001,15.2,0.472242216999987));
#262644=CARTESIAN_POINT('Ctrl Pts',(-11.3484485530001,15.2,0.473883093999987));
#262645=CARTESIAN_POINT('Ctrl Pts',(-11.3516917240001,15.2,0.475528550999984));
#262646=CARTESIAN_POINT('Ctrl Pts',(-11.3549377140001,15.2,0.477178588999987));
#262647=CARTESIAN_POINT('Ctrl Pts',(-11.3581865150001,15.2,0.478833208999987));
#262648=CARTESIAN_POINT('Ctrl Pts',(-11.3614381180001,15.2,0.480492415999985));
#262649=CARTESIAN_POINT('Ctrl Pts',(-11.3646925130001,15.2,0.482156208999989));
#262650=CARTESIAN_POINT('Ctrl Pts',(-11.3679496900001,15.2,0.483824590999986));
#262651=CARTESIAN_POINT('Ctrl Pts',(-11.3712096420001,15.2,0.485497562999986));
#262652=CARTESIAN_POINT('Ctrl Pts',(-11.3744723580001,15.2,0.487175127999984));
#262653=CARTESIAN_POINT('Ctrl Pts',(-11.3777378300001,15.2,0.488857287999984));
#262654=CARTESIAN_POINT('Ctrl Pts',(-11.3810060480001,15.2,0.490544042999983));
#262655=CARTESIAN_POINT('Ctrl Pts',(-11.3842770020001,15.2,0.492235395999985));
#262656=CARTESIAN_POINT('Ctrl Pts',(-11.3875506850001,15.2,0.493931348999985));
#262657=CARTESIAN_POINT('Ctrl Pts',(-11.3908270860001,15.2,0.495631902999989));
#262658=CARTESIAN_POINT('Ctrl Pts',(-11.3941061970001,15.2,0.497337060999987));
#262659=CARTESIAN_POINT('Ctrl Pts',(-11.3973880080001,15.2,0.499046821999984));
#262660=CARTESIAN_POINT('Ctrl Pts',(-11.4006725110001,15.2,0.500761190999985));
#262661=CARTESIAN_POINT('Ctrl Pts',(-11.4039596970001,15.2,0.502480167999986));
#262662=CARTESIAN_POINT('Ctrl Pts',(-11.4072495570001,15.2,0.504203755999986));
#262663=CARTESIAN_POINT('Ctrl Pts',(-11.4105420820001,15.2,0.505931953999985));
#262664=CARTESIAN_POINT('Ctrl Pts',(-11.4138372610001,15.2,0.507664766999985));
#262665=CARTESIAN_POINT('Ctrl Pts',(-11.4171350880001,15.2,0.509402193999984));
#262666=CARTESIAN_POINT('Ctrl Pts',(-11.4204355510001,15.2,0.511144238999983));
#262667=CARTESIAN_POINT('Ctrl Pts',(-11.4237386430001,15.2,0.512890900999987));
#262668=CARTESIAN_POINT('Ctrl Pts',(-11.4270443520001,15.2,0.514642183999987));
#262669=CARTESIAN_POINT('Ctrl Pts',(-11.4303526710001,15.2,0.516398088999988));
#262670=CARTESIAN_POINT('Ctrl Pts',(-11.4336635900001,15.2,0.518158617999984));
#262671=CARTESIAN_POINT('Ctrl Pts',(-11.4369771030001,15.2,0.519923770999986));
#262672=CARTESIAN_POINT('Ctrl Pts',(-11.4402932010001,15.2,0.521693550999984));
#262673=CARTESIAN_POINT('Ctrl Pts',(-11.4436118760001,15.2,0.523467958999984));
#262674=CARTESIAN_POINT('Ctrl Pts',(-11.4469331180001,15.2,0.525246995999984));
#262675=CARTESIAN_POINT('Ctrl Pts',(-11.4502569220001,15.2,0.527030663999986));
#262676=CARTESIAN_POINT('Ctrl Pts',(-11.4535832720001,15.2,0.528818965999989));
#262677=CARTESIAN_POINT('Ctrl Pts',(-11.4569121620001,15.2,0.530611900999984));
#262678=CARTESIAN_POINT('Ctrl Pts',(-11.4602435780001,15.2,0.532409473999986));
#262679=CARTESIAN_POINT('Ctrl Pts',(-11.4635775100001,15.2,0.534211684999986));
#262680=CARTESIAN_POINT('Ctrl Pts',(-11.4669139500001,15.2,0.536018536999983));
#262681=CARTESIAN_POINT('Ctrl Pts',(-11.4702528880001,15.2,0.537830029999986));
#262682=CARTESIAN_POINT('Ctrl Pts',(-11.4735943180001,15.2,0.539646165999983));
#262683=CARTESIAN_POINT('Ctrl Pts',(-11.4769382380001,15.2,0.541466945999982));
#262684=CARTESIAN_POINT('Ctrl Pts',(-11.4802846430001,15.2,0.543292367999988));
#262685=CARTESIAN_POINT('Ctrl Pts',(-11.4829637560001,15.2,0.544756421999986));
#262686=CARTESIAN_POINT('Ctrl Pts',(-11.4849742100001,15.2,0.545856550999986));
#262687=CARTESIAN_POINT('Ctrl Pts',(-11.4863150090001,15.2,0.546590898999986));
#262688=CARTESIAN_POINT('Ctrl Pts',(-11.4869855320001,15.2,0.546958305999983));
#262689=CARTESIAN_POINT('Origin',(-5.66257110645729E-14,15.2,-1.77635683940025E-14));
#262690=CARTESIAN_POINT('',(-10.3708900234024,15.2,-0.292001929001953));
#262691=CARTESIAN_POINT('',(-10.3708900234024,12.2,-0.292001929001953));
#262692=CARTESIAN_POINT('',(-10.3708900230001,15.2,-0.292001929000012));
#262693=CARTESIAN_POINT('Origin',(-5.66257110645729E-14,12.2,-1.77635683940025E-14));
#262694=CARTESIAN_POINT('Origin',(-5.66257110645729E-14,15.2,-1.77635683940025E-14));
#262695=CARTESIAN_POINT('Origin',(-5.66257110645729E-14,15.2,-1.77635683940025E-14));
#262696=CARTESIAN_POINT('',(-11.4780040730001,15.2,-0.710930734000015));
#262697=CARTESIAN_POINT('',(-11.4479048650001,15.2,-1.09337742900002));
#262698=CARTESIAN_POINT('Origin',(-5.66257110645729E-14,15.2,-1.77635683940025E-14));
#262699=CARTESIAN_POINT('',(-11.4479048650001,12.2,-1.09337742900002));
#262700=CARTESIAN_POINT('',(-11.4479048650001,15.2,-1.09337742900002));
#262701=CARTESIAN_POINT('',(-11.4780040730001,12.2,-0.710930734000015));
#262702=CARTESIAN_POINT('Origin',(-5.66257110645729E-14,12.2,-1.77635683940025E-14));
#262703=CARTESIAN_POINT('',(-11.4780040730001,15.2,-0.710930734000015));
#262704=CARTESIAN_POINT('Ctrl Pts',(-11.4479048650001,15.2,-1.09337742900002));
#262705=CARTESIAN_POINT('Ctrl Pts',(-11.4479048650001,11.6,-1.09337742900002));
#262706=CARTESIAN_POINT('Ctrl Pts',(-11.4471888790001,15.2,-1.09364567100001));
#262707=CARTESIAN_POINT('Ctrl Pts',(-11.4471888790001,11.6,-1.09364567100001));
#262708=CARTESIAN_POINT('Ctrl Pts',(-11.4457572180001,15.2,-1.09418172800002));
#262709=CARTESIAN_POINT('Ctrl Pts',(-11.4457572180001,11.6,-1.09418172800002));
#262710=CARTESIAN_POINT('Ctrl Pts',(-11.4436106650001,15.2,-1.09498454300001));
#262711=CARTESIAN_POINT('Ctrl Pts',(-11.4436106650001,11.6,-1.09498454300002));
#262712=CARTESIAN_POINT('Ctrl Pts',(-11.4407504650001,15.2,-1.09605241700002));
#262713=CARTESIAN_POINT('Ctrl Pts',(-11.4407504650001,11.6,-1.09605241700002));
#262714=CARTESIAN_POINT('Ctrl Pts',(-11.4371783360001,15.2,-1.09738301600002));
#262715=CARTESIAN_POINT('Ctrl Pts',(-11.4371783360001,11.6,-1.09738301600002));
#262716=CARTESIAN_POINT('Ctrl Pts',(-11.4336093280001,15.2,-1.09870937400002));
#262717=CARTESIAN_POINT('Ctrl Pts',(-11.4336093280001,11.6,-1.09870937400002));
#262718=CARTESIAN_POINT('Ctrl Pts',(-11.4300434450001,15.2,-1.10003148800002));
#262719=CARTESIAN_POINT('Ctrl Pts',(-11.4300434450001,11.6,-1.10003148800002));
#262720=CARTESIAN_POINT('Ctrl Pts',(-11.4264806910001,15.2,-1.10134936300001));
#262721=CARTESIAN_POINT('Ctrl Pts',(-11.4264806910001,11.6,-1.10134936300002));
#262722=CARTESIAN_POINT('Ctrl Pts',(-11.4229210700001,15.2,-1.10266299900001));
#262723=CARTESIAN_POINT('Ctrl Pts',(-11.4229210700001,11.6,-1.10266299900002));
#262724=CARTESIAN_POINT('Ctrl Pts',(-11.4193645910001,15.2,-1.10397239900001));
#262725=CARTESIAN_POINT('Ctrl Pts',(-11.4193645910001,11.6,-1.10397239900002));
#262726=CARTESIAN_POINT('Ctrl Pts',(-11.4158112620001,15.2,-1.10527756400002));
#262727=CARTESIAN_POINT('Ctrl Pts',(-11.4158112620001,11.6,-1.10527756400002));
#262728=CARTESIAN_POINT('Ctrl Pts',(-11.4122610950001,15.2,-1.10657850000001));
#262729=CARTESIAN_POINT('Ctrl Pts',(-11.4122610950001,11.6,-1.10657850000001));
#262730=CARTESIAN_POINT('Ctrl Pts',(-11.4087141000001,15.2,-1.10787520900002));
#262731=CARTESIAN_POINT('Ctrl Pts',(-11.4087141000001,11.6,-1.10787520900002));
#262732=CARTESIAN_POINT('Ctrl Pts',(-11.4051702860001,15.2,-1.10916769600002));
#262733=CARTESIAN_POINT('Ctrl Pts',(-11.4051702860001,11.6,-1.10916769600002));
#262734=CARTESIAN_POINT('Ctrl Pts',(-11.4016296650001,15.2,-1.11045596300002));
#262735=CARTESIAN_POINT('Ctrl Pts',(-11.4016296650001,11.6,-1.11045596300002));
#262736=CARTESIAN_POINT('Ctrl Pts',(-11.3980922450001,15.2,-1.11174001300002));
#262737=CARTESIAN_POINT('Ctrl Pts',(-11.3980922450001,11.6,-1.11174001300002));
#262738=CARTESIAN_POINT('Ctrl Pts',(-11.3945580340001,15.2,-1.11301985000001));
#262739=CARTESIAN_POINT('Ctrl Pts',(-11.3945580340001,11.6,-1.11301985000001));
#262740=CARTESIAN_POINT('Ctrl Pts',(-11.3910270410001,15.2,-1.11429547400002));
#262741=CARTESIAN_POINT('Ctrl Pts',(-11.3910270410001,11.6,-1.11429547400002));
#262742=CARTESIAN_POINT('Ctrl Pts',(-11.3874992720001,15.2,-1.11556689000002));
#262743=CARTESIAN_POINT('Ctrl Pts',(-11.3874992720001,11.6,-1.11556689000002));
#262744=CARTESIAN_POINT('Ctrl Pts',(-11.3839747360001,15.2,-1.11683410000001));
#262745=CARTESIAN_POINT('Ctrl Pts',(-11.3839747360001,11.6,-1.11683410000001));
#262746=CARTESIAN_POINT('Ctrl Pts',(-11.3804534400001,15.2,-1.11809710600001));
#262747=CARTESIAN_POINT('Ctrl Pts',(-11.3804534400001,11.6,-1.11809710600001));
#262748=CARTESIAN_POINT('Ctrl Pts',(-11.3769353940001,15.2,-1.11935591200002));
#262749=CARTESIAN_POINT('Ctrl Pts',(-11.3769353940001,11.6,-1.11935591200002));
#262750=CARTESIAN_POINT('Ctrl Pts',(-11.3734206060001,15.2,-1.12061052000001));
#262751=CARTESIAN_POINT('Ctrl Pts',(-11.3734206060001,11.6,-1.12061052000001));
#262752=CARTESIAN_POINT('Ctrl Pts',(-11.3699090850001,15.2,-1.12186093300001));
#262753=CARTESIAN_POINT('Ctrl Pts',(-11.3699090850001,11.6,-1.12186093300001));
#262754=CARTESIAN_POINT('Ctrl Pts',(-11.3664008400001,15.2,-1.12310715400001));
#262755=CARTESIAN_POINT('Ctrl Pts',(-11.3664008400001,11.6,-1.12310715400001));
#262756=CARTESIAN_POINT('Ctrl Pts',(-11.3628958810001,15.2,-1.12434918700002));
#262757=CARTESIAN_POINT('Ctrl Pts',(-11.3628958810001,11.6,-1.12434918700002));
#262758=CARTESIAN_POINT('Ctrl Pts',(-11.3593942150001,15.2,-1.12558703500001));
#262759=CARTESIAN_POINT('Ctrl Pts',(-11.3593942150001,11.6,-1.12558703500001));
#262760=CARTESIAN_POINT('Ctrl Pts',(-11.3558958510001,15.2,-1.12682069900002));
#262761=CARTESIAN_POINT('Ctrl Pts',(-11.3558958510001,11.6,-1.12682069900002));
#262762=CARTESIAN_POINT('Ctrl Pts',(-11.3524008000001,15.2,-1.12805018600001));
#262763=CARTESIAN_POINT('Ctrl Pts',(-11.3524008000001,11.6,-1.12805018600001));
#262764=CARTESIAN_POINT('Ctrl Pts',(-11.3489090690001,15.2,-1.12927549400001));
#262765=CARTESIAN_POINT('Ctrl Pts',(-11.3489090690001,11.6,-1.12927549400002));
#262766=CARTESIAN_POINT('Ctrl Pts',(-11.3454206650001,15.2,-1.13049662900002));
#262767=CARTESIAN_POINT('Ctrl Pts',(-11.3454206650001,11.6,-1.13049662900002));
#262768=CARTESIAN_POINT('Ctrl Pts',(-11.3419355990001,15.2,-1.13171359300001));
#262769=CARTESIAN_POINT('Ctrl Pts',(-11.3419355990001,11.6,-1.13171359300001));
#262770=CARTESIAN_POINT('Ctrl Pts',(-11.3384538780001,15.2,-1.13292639100001));
#262771=CARTESIAN_POINT('Ctrl Pts',(-11.3384538780001,11.6,-1.13292639100001));
#262772=CARTESIAN_POINT('Ctrl Pts',(-11.3349755130001,15.2,-1.13413502300002));
#262773=CARTESIAN_POINT('Ctrl Pts',(-11.3349755130001,11.6,-1.13413502300002));
#262774=CARTESIAN_POINT('Ctrl Pts',(-11.3315005100001,15.2,-1.13533949300002));
#262775=CARTESIAN_POINT('Ctrl Pts',(-11.3315005100001,11.6,-1.13533949300002));
#262776=CARTESIAN_POINT('Ctrl Pts',(-11.3280288800001,15.2,-1.13653980600001));
#262777=CARTESIAN_POINT('Ctrl Pts',(-11.3280288800001,11.6,-1.13653980600001));
#262778=CARTESIAN_POINT('Ctrl Pts',(-11.3245606310001,15.2,-1.13773596300002));
#262779=CARTESIAN_POINT('Ctrl Pts',(-11.3245606310001,11.6,-1.13773596300002));
#262780=CARTESIAN_POINT('Ctrl Pts',(-11.3210957720001,15.2,-1.13892796700001));
#262781=CARTESIAN_POINT('Ctrl Pts',(-11.3210957720001,11.6,-1.13892796700001));
#262782=CARTESIAN_POINT('Ctrl Pts',(-11.3176343120001,15.2,-1.14011582200002));
#262783=CARTESIAN_POINT('Ctrl Pts',(-11.3176343120001,11.6,-1.14011582200002));
#262784=CARTESIAN_POINT('Ctrl Pts',(-11.3141762600001,15.2,-1.14129953200001));
#262785=CARTESIAN_POINT('Ctrl Pts',(-11.3141762600001,11.6,-1.14129953200001));
#262786=CARTESIAN_POINT('Ctrl Pts',(-11.3107216250001,15.2,-1.14247909900001));
#262787=CARTESIAN_POINT('Ctrl Pts',(-11.3107216250001,11.6,-1.14247909900001));
#262788=CARTESIAN_POINT('Ctrl Pts',(-11.3072704150001,15.2,-1.14365452600001));
#262789=CARTESIAN_POINT('Ctrl Pts',(-11.3072704150001,11.6,-1.14365452600001));
#262790=CARTESIAN_POINT('Ctrl Pts',(-11.3038226390001,15.2,-1.14482581600001));
#262791=CARTESIAN_POINT('Ctrl Pts',(-11.3038226390001,11.6,-1.14482581600001));
#262792=CARTESIAN_POINT('Ctrl Pts',(-11.3003783060001,15.2,-1.14599297300002));
#262793=CARTESIAN_POINT('Ctrl Pts',(-11.3003783060001,11.6,-1.14599297300002));
#262794=CARTESIAN_POINT('Ctrl Pts',(-11.2969374260001,15.2,-1.14715599900002));
#262795=CARTESIAN_POINT('Ctrl Pts',(-11.2969374260001,11.6,-1.14715599900002));
#262796=CARTESIAN_POINT('Ctrl Pts',(-11.2935000060001,15.2,-1.14831489900002));
#262797=CARTESIAN_POINT('Ctrl Pts',(-11.2935000060001,11.6,-1.14831489900002));
#262798=CARTESIAN_POINT('Ctrl Pts',(-11.2900660570001,15.2,-1.14946967500002));
#262799=CARTESIAN_POINT('Ctrl Pts',(-11.2900660570001,11.6,-1.14946967500002));
#262800=CARTESIAN_POINT('Ctrl Pts',(-11.2866355860001,15.2,-1.15062033000001));
#262801=CARTESIAN_POINT('Ctrl Pts',(-11.2866355860001,11.6,-1.15062033000001));
#262802=CARTESIAN_POINT('Ctrl Pts',(-11.2832086040001,15.2,-1.15176686800002));
#262803=CARTESIAN_POINT('Ctrl Pts',(-11.2832086040001,11.6,-1.15176686800002));
#262804=CARTESIAN_POINT('Ctrl Pts',(-11.2797851190001,15.2,-1.15290929100002));
#262805=CARTESIAN_POINT('Ctrl Pts',(-11.2797851190001,11.6,-1.15290929100002));
#262806=CARTESIAN_POINT('Ctrl Pts',(-11.2763651390001,15.2,-1.15404760400001));
#262807=CARTESIAN_POINT('Ctrl Pts',(-11.2763651390001,11.6,-1.15404760400002));
#262808=CARTESIAN_POINT('Ctrl Pts',(-11.2729486730001,15.2,-1.15518181000001));
#262809=CARTESIAN_POINT('Ctrl Pts',(-11.2729486730001,11.6,-1.15518181000001));
#262810=CARTESIAN_POINT('Ctrl Pts',(-11.2695357330001,15.2,-1.15631191100002));
#262811=CARTESIAN_POINT('Ctrl Pts',(-11.2695357330001,11.6,-1.15631191100002));
#262812=CARTESIAN_POINT('Ctrl Pts',(-11.2661263250001,15.2,-1.15743791100002));
#262813=CARTESIAN_POINT('Ctrl Pts',(-11.2661263250001,11.6,-1.15743791100002));
#262814=CARTESIAN_POINT('Ctrl Pts',(-11.2627204590001,15.2,-1.15855981300002));
#262815=CARTESIAN_POINT('Ctrl Pts',(-11.2627204590001,11.6,-1.15855981300002));
#262816=CARTESIAN_POINT('Ctrl Pts',(-11.2593181450001,15.2,-1.15967762100002));
#262817=CARTESIAN_POINT('Ctrl Pts',(-11.2593181450001,11.6,-1.15967762100002));
#262818=CARTESIAN_POINT('Ctrl Pts',(-11.2559193900001,15.2,-1.16079133800001));
#262819=CARTESIAN_POINT('Ctrl Pts',(-11.2559193900001,11.6,-1.16079133800001));
#262820=CARTESIAN_POINT('Ctrl Pts',(-11.2525242050001,15.2,-1.16190096800001));
#262821=CARTESIAN_POINT('Ctrl Pts',(-11.2525242050001,11.6,-1.16190096800001));
#262822=CARTESIAN_POINT('Ctrl Pts',(-11.2491325970001,15.2,-1.16300651300001));
#262823=CARTESIAN_POINT('Ctrl Pts',(-11.2491325970001,11.6,-1.16300651300001));
#262824=CARTESIAN_POINT('Ctrl Pts',(-11.2457445790001,15.2,-1.16410797700001));
#262825=CARTESIAN_POINT('Ctrl Pts',(-11.2457445790001,11.6,-1.16410797700001));
#262826=CARTESIAN_POINT('Ctrl Pts',(-11.2423601550001,15.2,-1.16520536500001));
#262827=CARTESIAN_POINT('Ctrl Pts',(-11.2423601550001,11.6,-1.16520536500001));
#262828=CARTESIAN_POINT('Ctrl Pts',(-11.2389793380001,15.2,-1.16629867700001));
#262829=CARTESIAN_POINT('Ctrl Pts',(-11.2389793380001,11.6,-1.16629867700001));
#262830=CARTESIAN_POINT('Ctrl Pts',(-11.2356021350001,15.2,-1.16738791900001));
#262831=CARTESIAN_POINT('Ctrl Pts',(-11.2356021350001,11.6,-1.16738791900001));
#262832=CARTESIAN_POINT('Ctrl Pts',(-11.2322285580001,15.2,-1.16847309500002));
#262833=CARTESIAN_POINT('Ctrl Pts',(-11.2322285580001,11.6,-1.16847309500002));
#262834=CARTESIAN_POINT('Ctrl Pts',(-11.2288586130001,15.2,-1.16955420600001));
#262835=CARTESIAN_POINT('Ctrl Pts',(-11.2288586130001,11.6,-1.16955420600001));
#262836=CARTESIAN_POINT('Ctrl Pts',(-11.2254923100001,15.2,-1.17063125600001));
#262837=CARTESIAN_POINT('Ctrl Pts',(-11.2254923100001,11.6,-1.17063125600001));
#262838=CARTESIAN_POINT('Ctrl Pts',(-11.2221296590001,15.2,-1.17170425100001));
#262839=CARTESIAN_POINT('Ctrl Pts',(-11.2221296590001,11.6,-1.17170425100001));
#262840=CARTESIAN_POINT('Ctrl Pts',(-11.2187706690001,15.2,-1.17277319100001));
#262841=CARTESIAN_POINT('Ctrl Pts',(-11.2187706690001,11.6,-1.17277319100001));
#262842=CARTESIAN_POINT('Ctrl Pts',(-11.2154153490001,15.2,-1.17383808300001));
#262843=CARTESIAN_POINT('Ctrl Pts',(-11.2154153490001,11.6,-1.17383808300001));
#262844=CARTESIAN_POINT('Ctrl Pts',(-11.2120637080001,15.2,-1.17489892700001));
#262845=CARTESIAN_POINT('Ctrl Pts',(-11.2120637080001,11.6,-1.17489892700001));
#262846=CARTESIAN_POINT('Ctrl Pts',(-11.2087157570001,15.2,-1.17595572900001));
#262847=CARTESIAN_POINT('Ctrl Pts',(-11.2087157570001,11.6,-1.17595572900001));
#262848=CARTESIAN_POINT('Ctrl Pts',(-11.2053715030001,15.2,-1.17700849300002));
#262849=CARTESIAN_POINT('Ctrl Pts',(-11.2053715030001,11.6,-1.17700849300002));
#262850=CARTESIAN_POINT('Ctrl Pts',(-11.2020309560001,15.2,-1.17805721900002));
#262851=CARTESIAN_POINT('Ctrl Pts',(-11.2020309560001,11.6,-1.17805721900002));
#262852=CARTESIAN_POINT('Ctrl Pts',(-11.1986941260001,15.2,-1.17910191500001));
#262853=CARTESIAN_POINT('Ctrl Pts',(-11.1986941260001,11.6,-1.17910191500001));
#262854=CARTESIAN_POINT('Ctrl Pts',(-11.1953610220001,15.2,-1.18014258100001));
#262855=CARTESIAN_POINT('Ctrl Pts',(-11.1953610220001,11.6,-1.18014258100001));
#262856=CARTESIAN_POINT('Ctrl Pts',(-11.1920316530001,15.2,-1.18117922300002));
#262857=CARTESIAN_POINT('Ctrl Pts',(-11.1920316530001,11.6,-1.18117922300002));
#262858=CARTESIAN_POINT('Ctrl Pts',(-11.1887060280001,15.2,-1.18221184300001));
#262859=CARTESIAN_POINT('Ctrl Pts',(-11.1887060280001,11.6,-1.18221184300001));
#262860=CARTESIAN_POINT('Ctrl Pts',(-11.1853841570001,15.2,-1.18324044600001));
#262861=CARTESIAN_POINT('Ctrl Pts',(-11.1853841570001,11.6,-1.18324044600001));
#262862=CARTESIAN_POINT('Ctrl Pts',(-11.1820660500001,15.2,-1.18426503500002));
#262863=CARTESIAN_POINT('Ctrl Pts',(-11.1820660500001,11.6,-1.18426503500002));
#262864=CARTESIAN_POINT('Ctrl Pts',(-11.1787517160001,15.2,-1.18528561300002));
#262865=CARTESIAN_POINT('Ctrl Pts',(-11.1787517160001,11.6,-1.18528561300002));
#262866=CARTESIAN_POINT('Ctrl Pts',(-11.1754411630001,15.2,-1.18630218500002));
#262867=CARTESIAN_POINT('Ctrl Pts',(-11.1754411630001,11.6,-1.18630218500002));
#262868=CARTESIAN_POINT('Ctrl Pts',(-11.1721344020001,15.2,-1.18731475500002));
#262869=CARTESIAN_POINT('Ctrl Pts',(-11.1721344020001,11.6,-1.18731475500002));
#262870=CARTESIAN_POINT('Ctrl Pts',(-11.1688314420001,15.2,-1.18832332500002));
#262871=CARTESIAN_POINT('Ctrl Pts',(-11.1688314420001,11.6,-1.18832332500002));
#262872=CARTESIAN_POINT('Ctrl Pts',(-11.1655322930001,15.2,-1.18932789900001));
#262873=CARTESIAN_POINT('Ctrl Pts',(-11.1655322930001,11.6,-1.18932789900001));
#262874=CARTESIAN_POINT('Ctrl Pts',(-11.1622369630001,15.2,-1.19032848100002));
#262875=CARTESIAN_POINT('Ctrl Pts',(-11.1622369630001,11.6,-1.19032848100002));
#262876=CARTESIAN_POINT('Ctrl Pts',(-11.1589454620001,15.2,-1.19132507600002));
#262877=CARTESIAN_POINT('Ctrl Pts',(-11.1589454620001,11.6,-1.19132507600002));
#262878=CARTESIAN_POINT('Ctrl Pts',(-11.1556578010001,15.2,-1.19231768700002));
#262879=CARTESIAN_POINT('Ctrl Pts',(-11.1556578010001,11.6,-1.19231768700002));
#262880=CARTESIAN_POINT('Ctrl Pts',(-11.1523739880001,15.2,-1.19330631600001));
#262881=CARTESIAN_POINT('Ctrl Pts',(-11.1523739880001,11.6,-1.19330631600001));
#262882=CARTESIAN_POINT('Ctrl Pts',(-11.1490940330001,15.2,-1.19429096900001));
#262883=CARTESIAN_POINT('Ctrl Pts',(-11.1490940330001,11.6,-1.19429096900001));
#262884=CARTESIAN_POINT('Ctrl Pts',(-11.1458179460001,15.2,-1.19527164900001));
#262885=CARTESIAN_POINT('Ctrl Pts',(-11.1458179460001,11.6,-1.19527164900001));
#262886=CARTESIAN_POINT('Ctrl Pts',(-11.1425457350001,15.2,-1.19624836000002));
#262887=CARTESIAN_POINT('Ctrl Pts',(-11.1425457350001,11.6,-1.19624836000002));
#262888=CARTESIAN_POINT('Ctrl Pts',(-11.1392774120001,15.2,-1.19722110600001));
#262889=CARTESIAN_POINT('Ctrl Pts',(-11.1392774120001,11.6,-1.19722110600002));
#262890=CARTESIAN_POINT('Ctrl Pts',(-11.1360129840001,15.2,-1.19818989000001));
#262891=CARTESIAN_POINT('Ctrl Pts',(-11.1360129840001,11.6,-1.19818989000001));
#262892=CARTESIAN_POINT('Ctrl Pts',(-11.1327524620001,15.2,-1.19915471800002));
#262893=CARTESIAN_POINT('Ctrl Pts',(-11.1327524620001,11.6,-1.19915471800002));
#262894=CARTESIAN_POINT('Ctrl Pts',(-11.1294958560001,15.2,-1.20011559100002));
#262895=CARTESIAN_POINT('Ctrl Pts',(-11.1294958560001,11.6,-1.20011559100002));
#262896=CARTESIAN_POINT('Ctrl Pts',(-11.1262431750001,15.2,-1.20107251400002));
#262897=CARTESIAN_POINT('Ctrl Pts',(-11.1262431750001,11.6,-1.20107251400002));
#262898=CARTESIAN_POINT('Ctrl Pts',(-11.1229944280001,15.2,-1.20202549200001));
#262899=CARTESIAN_POINT('Ctrl Pts',(-11.1229944280001,11.6,-1.20202549200001));
#262900=CARTESIAN_POINT('Ctrl Pts',(-11.1197496260001,15.2,-1.20297452800001));
#262901=CARTESIAN_POINT('Ctrl Pts',(-11.1197496260001,11.6,-1.20297452800001));
#262902=CARTESIAN_POINT('Ctrl Pts',(-11.1165087780001,15.2,-1.20391962700001));
#262903=CARTESIAN_POINT('Ctrl Pts',(-11.1165087780001,11.6,-1.20391962700001));
#262904=CARTESIAN_POINT('Ctrl Pts',(-11.1132718940001,15.2,-1.20486079100001));
#262905=CARTESIAN_POINT('Ctrl Pts',(-11.1132718940001,11.6,-1.20486079100001));
#262906=CARTESIAN_POINT('Ctrl Pts',(-11.1100389830001,15.2,-1.20579802500002));
#262907=CARTESIAN_POINT('Ctrl Pts',(-11.1100389830001,11.6,-1.20579802500002));
#262908=CARTESIAN_POINT('Ctrl Pts',(-11.1068100550001,15.2,-1.20673133400001));
#262909=CARTESIAN_POINT('Ctrl Pts',(-11.1068100550001,11.6,-1.20673133400001));
#262910=CARTESIAN_POINT('Ctrl Pts',(-11.1035851210001,15.2,-1.20766072000002));
#262911=CARTESIAN_POINT('Ctrl Pts',(-11.1035851210001,11.6,-1.20766072000002));
#262912=CARTESIAN_POINT('Ctrl Pts',(-11.1003641890001,15.2,-1.20858618800002));
#262913=CARTESIAN_POINT('Ctrl Pts',(-11.1003641890001,11.6,-1.20858618800002));
#262914=CARTESIAN_POINT('Ctrl Pts',(-11.0971472700001,15.2,-1.20950774300002));
#262915=CARTESIAN_POINT('Ctrl Pts',(-11.0971472700001,11.6,-1.20950774300002));
#262916=CARTESIAN_POINT('Ctrl Pts',(-11.0939343730001,15.2,-1.21042538700001));
#262917=CARTESIAN_POINT('Ctrl Pts',(-11.0939343730001,11.6,-1.21042538700001));
#262918=CARTESIAN_POINT('Ctrl Pts',(-11.0907255090001,15.2,-1.21133912600001));
#262919=CARTESIAN_POINT('Ctrl Pts',(-11.0907255090001,11.6,-1.21133912600001));
#262920=CARTESIAN_POINT('Ctrl Pts',(-11.0875206860001,15.2,-1.21224896200001));
#262921=CARTESIAN_POINT('Ctrl Pts',(-11.0875206860001,11.6,-1.21224896200001));
#262922=CARTESIAN_POINT('Ctrl Pts',(-11.0843199150001,15.2,-1.21315490200002));
#262923=CARTESIAN_POINT('Ctrl Pts',(-11.0843199150001,11.6,-1.21315490200002));
#262924=CARTESIAN_POINT('Ctrl Pts',(-11.0811232050001,15.2,-1.21405694800002));
#262925=CARTESIAN_POINT('Ctrl Pts',(-11.0811232050001,11.6,-1.21405694800002));
#262926=CARTESIAN_POINT('Ctrl Pts',(-11.0779305680001,15.2,-1.21495510400001));
#262927=CARTESIAN_POINT('Ctrl Pts',(-11.0779305680001,11.6,-1.21495510400001));
#262928=CARTESIAN_POINT('Ctrl Pts',(-11.0747420110001,15.2,-1.21584937600002));
#262929=CARTESIAN_POINT('Ctrl Pts',(-11.0747420110001,11.6,-1.21584937600002));
#262930=CARTESIAN_POINT('Ctrl Pts',(-11.0715575460001,15.2,-1.21673976600002));
#262931=CARTESIAN_POINT('Ctrl Pts',(-11.0715575460001,11.6,-1.21673976600002));
#262932=CARTESIAN_POINT('Ctrl Pts',(-11.0683771820001,15.2,-1.21762628000001));
#262933=CARTESIAN_POINT('Ctrl Pts',(-11.0683771820001,11.6,-1.21762628000001));
#262934=CARTESIAN_POINT('Ctrl Pts',(-11.0652009300001,15.2,-1.21850892000001));
#262935=CARTESIAN_POINT('Ctrl Pts',(-11.0652009300001,11.6,-1.21850892000001));
#262936=CARTESIAN_POINT('Ctrl Pts',(-11.0620287980001,15.2,-1.21938769300002));
#262937=CARTESIAN_POINT('Ctrl Pts',(-11.0620287980001,11.6,-1.21938769300002));
#262938=CARTESIAN_POINT('Ctrl Pts',(-11.0588607980001,15.2,-1.22026260000001));
#262939=CARTESIAN_POINT('Ctrl Pts',(-11.0588607980001,11.6,-1.22026260000002));
#262940=CARTESIAN_POINT('Ctrl Pts',(-11.0556969390001,15.2,-1.22113364900001));
#262941=CARTESIAN_POINT('Ctrl Pts',(-11.0556969390001,11.6,-1.22113364900002));
#262942=CARTESIAN_POINT('Ctrl Pts',(-11.0525372310001,15.2,-1.22200084200002));
#262943=CARTESIAN_POINT('Ctrl Pts',(-11.0525372310001,11.6,-1.22200084200002));
#262944=CARTESIAN_POINT('Ctrl Pts',(-11.0493816840001,15.2,-1.22286418300002));
#262945=CARTESIAN_POINT('Ctrl Pts',(-11.0493816840001,11.6,-1.22286418300002));
#262946=CARTESIAN_POINT('Ctrl Pts',(-11.0462303080001,15.2,-1.22372367600001));
#262947=CARTESIAN_POINT('Ctrl Pts',(-11.0462303080001,11.6,-1.22372367600002));
#262948=CARTESIAN_POINT('Ctrl Pts',(-11.0430831140001,15.2,-1.22457932800002));
#262949=CARTESIAN_POINT('Ctrl Pts',(-11.0430831140001,11.6,-1.22457932800002));
#262950=CARTESIAN_POINT('Ctrl Pts',(-11.0399401110001,15.2,-1.22543114000001));
#262951=CARTESIAN_POINT('Ctrl Pts',(-11.0399401110001,11.6,-1.22543114000001));
#262952=CARTESIAN_POINT('Ctrl Pts',(-11.0368013090001,15.2,-1.22627911900001));
#262953=CARTESIAN_POINT('Ctrl Pts',(-11.0368013090001,11.6,-1.22627911900001));
#262954=CARTESIAN_POINT('Ctrl Pts',(-11.0336667190001,15.2,-1.22712326700002));
#262955=CARTESIAN_POINT('Ctrl Pts',(-11.0336667190001,11.6,-1.22712326700002));
#262956=CARTESIAN_POINT('Ctrl Pts',(-11.0305363500001,15.2,-1.22796359100001));
#262957=CARTESIAN_POINT('Ctrl Pts',(-11.0305363500001,11.6,-1.22796359100001));
#262958=CARTESIAN_POINT('Ctrl Pts',(-11.0274102140001,15.2,-1.22880009400001));
#262959=CARTESIAN_POINT('Ctrl Pts',(-11.0274102140001,11.6,-1.22880009400001));
#262960=CARTESIAN_POINT('Ctrl Pts',(-11.0242883200001,15.2,-1.22963277900002));
#262961=CARTESIAN_POINT('Ctrl Pts',(-11.0242883200001,11.6,-1.22963277900002));
#262962=CARTESIAN_POINT('Ctrl Pts',(-11.0211706780001,15.2,-1.23046165300002));
#262963=CARTESIAN_POINT('Ctrl Pts',(-11.0211706780001,11.6,-1.23046165300002));
#262964=CARTESIAN_POINT('Ctrl Pts',(-11.0180572970001,15.2,-1.23128671800002));
#262965=CARTESIAN_POINT('Ctrl Pts',(-11.0180572970001,11.6,-1.23128671800002));
#262966=CARTESIAN_POINT('Ctrl Pts',(-11.0149481890001,15.2,-1.23210798200001));
#262967=CARTESIAN_POINT('Ctrl Pts',(-11.0149481890001,11.6,-1.23210798200002));
#262968=CARTESIAN_POINT('Ctrl Pts',(-11.0118433650001,15.2,-1.23292544600002));
#262969=CARTESIAN_POINT('Ctrl Pts',(-11.0118433650001,11.6,-1.23292544600002));
#262970=CARTESIAN_POINT('Ctrl Pts',(-11.0087428330001,15.2,-1.23373911600002));
#262971=CARTESIAN_POINT('Ctrl Pts',(-11.0087428330001,11.6,-1.23373911600002));
#262972=CARTESIAN_POINT('Ctrl Pts',(-11.0056466050001,15.2,-1.23454899600001));
#262973=CARTESIAN_POINT('Ctrl Pts',(-11.0056466050001,11.6,-1.23454899600001));
#262974=CARTESIAN_POINT('Ctrl Pts',(-11.0025546900001,15.2,-1.23535509100002));
#262975=CARTESIAN_POINT('Ctrl Pts',(-11.0025546900001,11.6,-1.23535509100002));
#262976=CARTESIAN_POINT('Ctrl Pts',(-10.9994670990001,15.2,-1.23615740600002));
#262977=CARTESIAN_POINT('Ctrl Pts',(-10.9994670990001,11.6,-1.23615740600002));
#262978=CARTESIAN_POINT('Ctrl Pts',(-10.9963838420001,15.2,-1.23695594400001));
#262979=CARTESIAN_POINT('Ctrl Pts',(-10.9963838420001,11.6,-1.23695594400001));
#262980=CARTESIAN_POINT('Ctrl Pts',(-10.9933049300001,15.2,-1.23775071100001));
#262981=CARTESIAN_POINT('Ctrl Pts',(-10.9933049300001,11.6,-1.23775071100001));
#262982=CARTESIAN_POINT('Ctrl Pts',(-10.9902303730001,15.2,-1.23854171100001));
#262983=CARTESIAN_POINT('Ctrl Pts',(-10.9902303730001,11.6,-1.23854171100001));
#262984=CARTESIAN_POINT('Ctrl Pts',(-10.9871601810001,15.2,-1.23932894900001));
#262985=CARTESIAN_POINT('Ctrl Pts',(-10.9871601810001,11.6,-1.23932894900001));
#262986=CARTESIAN_POINT('Ctrl Pts',(-10.9840943650001,15.2,-1.24011242900002));
#262987=CARTESIAN_POINT('Ctrl Pts',(-10.9840943650001,11.6,-1.24011242900002));
#262988=CARTESIAN_POINT('Ctrl Pts',(-10.9810329350001,15.2,-1.24089215700002));
#262989=CARTESIAN_POINT('Ctrl Pts',(-10.9810329350001,11.6,-1.24089215700002));
#262990=CARTESIAN_POINT('Ctrl Pts',(-10.9779759010001,15.2,-1.24166813600001));
#262991=CARTESIAN_POINT('Ctrl Pts',(-10.9779759010001,11.6,-1.24166813600001));
#262992=CARTESIAN_POINT('Ctrl Pts',(-10.9749232750001,15.2,-1.24244037200001));
#262993=CARTESIAN_POINT('Ctrl Pts',(-10.9749232750001,11.6,-1.24244037200001));
#262994=CARTESIAN_POINT('Ctrl Pts',(-10.9718750660001,15.2,-1.24320886800001));
#262995=CARTESIAN_POINT('Ctrl Pts',(-10.9718750660001,11.6,-1.24320886800001));
#262996=CARTESIAN_POINT('Ctrl Pts',(-10.9688312840001,15.2,-1.24397363100002));
#262997=CARTESIAN_POINT('Ctrl Pts',(-10.9688312840001,11.6,-1.24397363100002));
#262998=CARTESIAN_POINT('Ctrl Pts',(-10.9657919420001,15.2,-1.24473466500001));
#262999=CARTESIAN_POINT('Ctrl Pts',(-10.9657919420001,11.6,-1.24473466500001));
#263000=CARTESIAN_POINT('Ctrl Pts',(-10.9627570480001,15.2,-1.24549197300002));
#263001=CARTESIAN_POINT('Ctrl Pts',(-10.9627570480001,11.6,-1.24549197300002));
#263002=CARTESIAN_POINT('Ctrl Pts',(-10.9597266140001,15.2,-1.24624556300001));
#263003=CARTESIAN_POINT('Ctrl Pts',(-10.9597266140001,11.6,-1.24624556300002));
#263004=CARTESIAN_POINT('Ctrl Pts',(-10.9567006500001,15.2,-1.24699543600002));
#263005=CARTESIAN_POINT('Ctrl Pts',(-10.9567006500001,11.6,-1.24699543600002));
#263006=CARTESIAN_POINT('Ctrl Pts',(-10.9536791670001,15.2,-1.24774160000001));
#263007=CARTESIAN_POINT('Ctrl Pts',(-10.9536791670001,11.6,-1.24774160000001));
#263008=CARTESIAN_POINT('Ctrl Pts',(-10.9506621740001,15.2,-1.24848405800002));
#263009=CARTESIAN_POINT('Ctrl Pts',(-10.9506621740001,11.6,-1.24848405800002));
#263010=CARTESIAN_POINT('Ctrl Pts',(-10.9476496840001,15.2,-1.24922281700002));
#263011=CARTESIAN_POINT('Ctrl Pts',(-10.9476496840001,11.6,-1.24922281700002));
#263012=CARTESIAN_POINT('Ctrl Pts',(-10.9446417060001,15.2,-1.24995787900001));
#263013=CARTESIAN_POINT('Ctrl Pts',(-10.9446417060001,11.6,-1.24995787900001));
#263014=CARTESIAN_POINT('Ctrl Pts',(-10.9416382510001,15.2,-1.25068925100001));
#263015=CARTESIAN_POINT('Ctrl Pts',(-10.9416382510001,11.6,-1.25068925100001));
#263016=CARTESIAN_POINT('Ctrl Pts',(-10.9386393310001,15.2,-1.25141693800002));
#263017=CARTESIAN_POINT('Ctrl Pts',(-10.9386393310001,11.6,-1.25141693800002));
#263018=CARTESIAN_POINT('Ctrl Pts',(-10.9356449540001,15.2,-1.25214094400001));
#263019=CARTESIAN_POINT('Ctrl Pts',(-10.9356449540001,11.6,-1.25214094400001));
#263020=CARTESIAN_POINT('Ctrl Pts',(-10.9326551340001,15.2,-1.25286127300001));
#263021=CARTESIAN_POINT('Ctrl Pts',(-10.9326551340001,11.6,-1.25286127300001));
#263022=CARTESIAN_POINT('Ctrl Pts',(-10.9296698780001,15.2,-1.25357793200001));
#263023=CARTESIAN_POINT('Ctrl Pts',(-10.9296698780001,11.6,-1.25357793200001));
#263024=CARTESIAN_POINT('Ctrl Pts',(-10.9266892000001,15.2,-1.25429092500001));
#263025=CARTESIAN_POINT('Ctrl Pts',(-10.9266892000001,11.6,-1.25429092500001));
#263026=CARTESIAN_POINT('Ctrl Pts',(-10.9237131090001,15.2,-1.25500025700001));
#263027=CARTESIAN_POINT('Ctrl Pts',(-10.9237131090001,11.6,-1.25500025700001));
#263028=CARTESIAN_POINT('Ctrl Pts',(-10.9207416170001,15.2,-1.25570593300001));
#263029=CARTESIAN_POINT('Ctrl Pts',(-10.9207416170001,11.6,-1.25570593300001));
#263030=CARTESIAN_POINT('Ctrl Pts',(-10.9177747340001,15.2,-1.25640795900001));
#263031=CARTESIAN_POINT('Ctrl Pts',(-10.9177747340001,11.6,-1.25640795900001));
#263032=CARTESIAN_POINT('Ctrl Pts',(-10.9148124710001,15.2,-1.25710633900002));
#263033=CARTESIAN_POINT('Ctrl Pts',(-10.9148124710001,11.6,-1.25710633900002));
#263034=CARTESIAN_POINT('Ctrl Pts',(-10.9118548380001,15.2,-1.25780107900002));
#263035=CARTESIAN_POINT('Ctrl Pts',(-10.9118548380001,11.6,-1.25780107900002));
#263036=CARTESIAN_POINT('Ctrl Pts',(-10.9089018470001,15.2,-1.25849218200001));
#263037=CARTESIAN_POINT('Ctrl Pts',(-10.9089018470001,11.6,-1.25849218200001));
#263038=CARTESIAN_POINT('Ctrl Pts',(-10.9059535100001,15.2,-1.25917965600001));
#263039=CARTESIAN_POINT('Ctrl Pts',(-10.9059535100001,11.6,-1.25917965600001));
#263040=CARTESIAN_POINT('Ctrl Pts',(-10.9030098350001,15.2,-1.25986350400002));
#263041=CARTESIAN_POINT('Ctrl Pts',(-10.9030098350001,11.6,-1.25986350400002));
#263042=CARTESIAN_POINT('Ctrl Pts',(-10.9000708340001,15.2,-1.26054373200001));
#263043=CARTESIAN_POINT('Ctrl Pts',(-10.9000708340001,11.6,-1.26054373200002));
#263044=CARTESIAN_POINT('Ctrl Pts',(-10.8971365200001,15.2,-1.26122034700002));
#263045=CARTESIAN_POINT('Ctrl Pts',(-10.8971365200001,11.6,-1.26122034700002));
#263046=CARTESIAN_POINT('Ctrl Pts',(-10.8942069010001,15.2,-1.26189335000001));
#263047=CARTESIAN_POINT('Ctrl Pts',(-10.8942069010001,11.6,-1.26189335000001));
#263048=CARTESIAN_POINT('Ctrl Pts',(-10.8912819900001,15.2,-1.26256275000001));
#263049=CARTESIAN_POINT('Ctrl Pts',(-10.8912819900001,11.6,-1.26256275000001));
#263050=CARTESIAN_POINT('Ctrl Pts',(-10.8883617980001,15.2,-1.26322855100002));
#263051=CARTESIAN_POINT('Ctrl Pts',(-10.8883617980001,11.6,-1.26322855100002));
#263052=CARTESIAN_POINT('Ctrl Pts',(-10.8854463350001,15.2,-1.26389075700001));
#263053=CARTESIAN_POINT('Ctrl Pts',(-10.8854463350001,11.6,-1.26389075700002));
#263054=CARTESIAN_POINT('Ctrl Pts',(-10.8825356130001,15.2,-1.26454937500001));
#263055=CARTESIAN_POINT('Ctrl Pts',(-10.8825356130001,11.6,-1.26454937500002));
#263056=CARTESIAN_POINT('Ctrl Pts',(-10.8796296420001,15.2,-1.26520441000002));
#263057=CARTESIAN_POINT('Ctrl Pts',(-10.8796296420001,11.6,-1.26520441000002));
#263058=CARTESIAN_POINT('Ctrl Pts',(-10.8767284330001,15.2,-1.26585586700001));
#263059=CARTESIAN_POINT('Ctrl Pts',(-10.8767284330001,11.6,-1.26585586700001));
#263060=CARTESIAN_POINT('Ctrl Pts',(-10.8738319990001,15.2,-1.26650375200001));
#263061=CARTESIAN_POINT('Ctrl Pts',(-10.8738319990001,11.6,-1.26650375200001));
#263062=CARTESIAN_POINT('Ctrl Pts',(-10.8709403490001,15.2,-1.26714806900001));
#263063=CARTESIAN_POINT('Ctrl Pts',(-10.8709403490001,11.6,-1.26714806900001));
#263064=CARTESIAN_POINT('Ctrl Pts',(-10.8680534960001,15.2,-1.26778882500002));
#263065=CARTESIAN_POINT('Ctrl Pts',(-10.8680534960001,11.6,-1.26778882500002));
#263066=CARTESIAN_POINT('Ctrl Pts',(-10.8651714500001,15.2,-1.26842602400002));
#263067=CARTESIAN_POINT('Ctrl Pts',(-10.8651714500001,11.6,-1.26842602400002));
#263068=CARTESIAN_POINT('Ctrl Pts',(-10.8622942230001,15.2,-1.26905967200001));
#263069=CARTESIAN_POINT('Ctrl Pts',(-10.8622942230001,11.6,-1.26905967200001));
#263070=CARTESIAN_POINT('Ctrl Pts',(-10.8594218250001,15.2,-1.26968977500002));
#263071=CARTESIAN_POINT('Ctrl Pts',(-10.8594218250001,11.6,-1.26968977500002));
#263072=CARTESIAN_POINT('Ctrl Pts',(-10.8565542680001,15.2,-1.27031633800001));
#263073=CARTESIAN_POINT('Ctrl Pts',(-10.8565542680001,11.6,-1.27031633800002));
#263074=CARTESIAN_POINT('Ctrl Pts',(-10.8536915640001,15.2,-1.27093936700001));
#263075=CARTESIAN_POINT('Ctrl Pts',(-10.8536915640001,11.6,-1.27093936700002));
#263076=CARTESIAN_POINT('Ctrl Pts',(-10.8508337230001,15.2,-1.27155886700002));
#263077=CARTESIAN_POINT('Ctrl Pts',(-10.8508337230001,11.6,-1.27155886700002));
#263078=CARTESIAN_POINT('Ctrl Pts',(-10.8479807570001,15.2,-1.27217484400001));
#263079=CARTESIAN_POINT('Ctrl Pts',(-10.8479807570001,11.6,-1.27217484400001));
#263080=CARTESIAN_POINT('Ctrl Pts',(-10.8451326780001,15.2,-1.27278730200001));
#263081=CARTESIAN_POINT('Ctrl Pts',(-10.8451326780001,11.6,-1.27278730200001));
#263082=CARTESIAN_POINT('Ctrl Pts',(-10.8422894960001,15.2,-1.27339624800001));
#263083=CARTESIAN_POINT('Ctrl Pts',(-10.8422894960001,11.6,-1.27339624800001));
#263084=CARTESIAN_POINT('Ctrl Pts',(-10.8394512230001,15.2,-1.27400168700001));
#263085=CARTESIAN_POINT('Ctrl Pts',(-10.8394512230001,11.6,-1.27400168700001));
#263086=CARTESIAN_POINT('Ctrl Pts',(-10.8366178710001,15.2,-1.27460362600001));
#263087=CARTESIAN_POINT('Ctrl Pts',(-10.8366178710001,11.6,-1.27460362600001));
#263088=CARTESIAN_POINT('Ctrl Pts',(-10.8337894500001,15.2,-1.27520207000002));
#263089=CARTESIAN_POINT('Ctrl Pts',(-10.8337894500001,11.6,-1.27520207000002));
#263090=CARTESIAN_POINT('Ctrl Pts',(-10.8309659720001,15.2,-1.27579702400002));
#263091=CARTESIAN_POINT('Ctrl Pts',(-10.8309659720001,11.6,-1.27579702400002));
#263092=CARTESIAN_POINT('Ctrl Pts',(-10.8281474500001,15.2,-1.27638849300002));
#263093=CARTESIAN_POINT('Ctrl Pts',(-10.8281474500001,11.6,-1.27638849300002));
#263094=CARTESIAN_POINT('Ctrl Pts',(-10.8253338940001,15.2,-1.27697648500002));
#263095=CARTESIAN_POINT('Ctrl Pts',(-10.8253338940001,11.6,-1.27697648500002));
#263096=CARTESIAN_POINT('Ctrl Pts',(-10.8225253160001,15.2,-1.27756100400001));
#263097=CARTESIAN_POINT('Ctrl Pts',(-10.8225253160001,11.6,-1.27756100400001));
#263098=CARTESIAN_POINT('Ctrl Pts',(-10.8197217270001,15.2,-1.27814205700002));
#263099=CARTESIAN_POINT('Ctrl Pts',(-10.8197217270001,11.6,-1.27814205700002));
#263100=CARTESIAN_POINT('Ctrl Pts',(-10.8169231390001,15.2,-1.27871964900002));
#263101=CARTESIAN_POINT('Ctrl Pts',(-10.8169231390001,11.6,-1.27871964900002));
#263102=CARTESIAN_POINT('Ctrl Pts',(-10.8141295640001,15.2,-1.27929378400002));
#263103=CARTESIAN_POINT('Ctrl Pts',(-10.8141295640001,11.6,-1.27929378400002));
#263104=CARTESIAN_POINT('Ctrl Pts',(-10.8113410120001,15.2,-1.27986447200001));
#263105=CARTESIAN_POINT('Ctrl Pts',(-10.8113410120001,11.6,-1.27986447200001));
#263106=CARTESIAN_POINT('Ctrl Pts',(-10.8085574970001,15.2,-1.28043171600002));
#263107=CARTESIAN_POINT('Ctrl Pts',(-10.8085574970001,11.6,-1.28043171600002));
#263108=CARTESIAN_POINT('Ctrl Pts',(-10.8057790290001,15.2,-1.28099552100001));
#263109=CARTESIAN_POINT('Ctrl Pts',(-10.8057790290001,11.6,-1.28099552100002));
#263110=CARTESIAN_POINT('Ctrl Pts',(-10.8030056200001,15.2,-1.28155589700001));
#263111=CARTESIAN_POINT('Ctrl Pts',(-10.8030056200001,11.6,-1.28155589700001));
#263112=CARTESIAN_POINT('Ctrl Pts',(-10.8002372820001,15.2,-1.28211284500001));
#263113=CARTESIAN_POINT('Ctrl Pts',(-10.8002372820001,11.6,-1.28211284500001));
#263114=CARTESIAN_POINT('Ctrl Pts',(-10.7974740270001,15.2,-1.28266637400001));
#263115=CARTESIAN_POINT('Ctrl Pts',(-10.7974740270001,11.6,-1.28266637400001));
#263116=CARTESIAN_POINT('Ctrl Pts',(-10.7947158660001,15.2,-1.28321649000001));
#263117=CARTESIAN_POINT('Ctrl Pts',(-10.7947158660001,11.6,-1.28321649000001));
#263118=CARTESIAN_POINT('Ctrl Pts',(-10.7919628110001,15.2,-1.28376319800001));
#263119=CARTESIAN_POINT('Ctrl Pts',(-10.7919628110001,11.6,-1.28376319800001));
#263120=CARTESIAN_POINT('Ctrl Pts',(-10.7892148740001,15.2,-1.28430650300002));
#263121=CARTESIAN_POINT('Ctrl Pts',(-10.7892148740001,11.6,-1.28430650300002));
#263122=CARTESIAN_POINT('Ctrl Pts',(-10.7864720660001,15.2,-1.28484641300001));
#263123=CARTESIAN_POINT('Ctrl Pts',(-10.7864720660001,11.6,-1.28484641300001));
#263124=CARTESIAN_POINT('Ctrl Pts',(-10.7837344010001,15.2,-1.28538293400001));
#263125=CARTESIAN_POINT('Ctrl Pts',(-10.7837344010001,11.6,-1.28538293400001));
#263126=CARTESIAN_POINT('Ctrl Pts',(-10.7810018880001,15.2,-1.28591607100002));
#263127=CARTESIAN_POINT('Ctrl Pts',(-10.7810018880001,11.6,-1.28591607100002));
#263128=CARTESIAN_POINT('Ctrl Pts',(-10.7782745420001,15.2,-1.28644583000002));
#263129=CARTESIAN_POINT('Ctrl Pts',(-10.7782745420001,11.6,-1.28644583000002));
#263130=CARTESIAN_POINT('Ctrl Pts',(-10.7755523730001,15.2,-1.28697221800001));
#263131=CARTESIAN_POINT('Ctrl Pts',(-10.7755523730001,11.6,-1.28697221800001));
#263132=CARTESIAN_POINT('Ctrl Pts',(-10.7728353940001,15.2,-1.28749524100002));
#263133=CARTESIAN_POINT('Ctrl Pts',(-10.7728353940001,11.6,-1.28749524100002));
#263134=CARTESIAN_POINT('Ctrl Pts',(-10.7701236150001,15.2,-1.28801490500001));
#263135=CARTESIAN_POINT('Ctrl Pts',(-10.7701236150001,11.6,-1.28801490500001));
#263136=CARTESIAN_POINT('Ctrl Pts',(-10.7674170490001,15.2,-1.28853121600002));
#263137=CARTESIAN_POINT('Ctrl Pts',(-10.7674170490001,11.6,-1.28853121600002));
#263138=CARTESIAN_POINT('Ctrl Pts',(-10.7647157090001,15.2,-1.28904418000001));
#263139=CARTESIAN_POINT('Ctrl Pts',(-10.7647157090001,11.6,-1.28904418000001));
#263140=CARTESIAN_POINT('Ctrl Pts',(-10.7620196070001,15.2,-1.28955380500001));
#263141=CARTESIAN_POINT('Ctrl Pts',(-10.7620196070001,11.6,-1.28955380500001));
#263142=CARTESIAN_POINT('Ctrl Pts',(-10.7593287540001,15.2,-1.29006009500001));
#263143=CARTESIAN_POINT('Ctrl Pts',(-10.7593287540001,11.6,-1.29006009500001));
#263144=CARTESIAN_POINT('Ctrl Pts',(-10.7566431620001,15.2,-1.29056305800002));
#263145=CARTESIAN_POINT('Ctrl Pts',(-10.7566431620001,11.6,-1.29056305800002));
#263146=CARTESIAN_POINT('Ctrl Pts',(-10.7539628450001,15.2,-1.29106270000001));
#263147=CARTESIAN_POINT('Ctrl Pts',(-10.7539628450001,11.6,-1.29106270000001));
#263148=CARTESIAN_POINT('Ctrl Pts',(-10.7512878130001,15.2,-1.29155902600001));
#263149=CARTESIAN_POINT('Ctrl Pts',(-10.7512878130001,11.6,-1.29155902600001));
#263150=CARTESIAN_POINT('Ctrl Pts',(-10.7486180790001,15.2,-1.29205204400002));
#263151=CARTESIAN_POINT('Ctrl Pts',(-10.7486180790001,11.6,-1.29205204400002));
#263152=CARTESIAN_POINT('Ctrl Pts',(-10.7459536560001,15.2,-1.29254175900002));
#263153=CARTESIAN_POINT('Ctrl Pts',(-10.7459536560001,11.6,-1.29254175900002));
#263154=CARTESIAN_POINT('Ctrl Pts',(-10.7432945550001,15.2,-1.29302817900002));
#263155=CARTESIAN_POINT('Ctrl Pts',(-10.7432945550001,11.6,-1.29302817900002));
#263156=CARTESIAN_POINT('Ctrl Pts',(-10.7406407890001,15.2,-1.29351131000002));
#263157=CARTESIAN_POINT('Ctrl Pts',(-10.7406407890001,11.6,-1.29351131000002));
#263158=CARTESIAN_POINT('Ctrl Pts',(-10.7379923700001,15.2,-1.29399115700001));
#263159=CARTESIAN_POINT('Ctrl Pts',(-10.7379923700001,11.6,-1.29399115700001));
#263160=CARTESIAN_POINT('Ctrl Pts',(-10.7353493100001,15.2,-1.29446772800001));
#263161=CARTESIAN_POINT('Ctrl Pts',(-10.7353493100001,11.6,-1.29446772800002));
#263162=CARTESIAN_POINT('Ctrl Pts',(-10.7327116220001,15.2,-1.29494103100001));
#263163=CARTESIAN_POINT('Ctrl Pts',(-10.7327116220001,11.6,-1.29494103100001));
#263164=CARTESIAN_POINT('Ctrl Pts',(-10.7300793190001,15.2,-1.29541106900001));
#263165=CARTESIAN_POINT('Ctrl Pts',(-10.7300793190001,11.6,-1.29541106900001));
#263166=CARTESIAN_POINT('Ctrl Pts',(-10.7274524110001,15.2,-1.29587785100002));
#263167=CARTESIAN_POINT('Ctrl Pts',(-10.7274524110001,11.6,-1.29587785100002));
#263168=CARTESIAN_POINT('Ctrl Pts',(-10.7248309140001,15.2,-1.29634138200001));
#263169=CARTESIAN_POINT('Ctrl Pts',(-10.7248309140001,11.6,-1.29634138200002));
#263170=CARTESIAN_POINT('Ctrl Pts',(-10.7222148360001,15.2,-1.29680167100001));
#263171=CARTESIAN_POINT('Ctrl Pts',(-10.7222148360001,11.6,-1.29680167100001));
#263172=CARTESIAN_POINT('Ctrl Pts',(-10.7196041930001,15.2,-1.29725872300002));
#263173=CARTESIAN_POINT('Ctrl Pts',(-10.7196041930001,11.6,-1.29725872300002));
#263174=CARTESIAN_POINT('Ctrl Pts',(-10.7169989970001,15.2,-1.29771254400001));
#263175=CARTESIAN_POINT('Ctrl Pts',(-10.7169989970001,11.6,-1.29771254400001));
#263176=CARTESIAN_POINT('Ctrl Pts',(-10.7143992590001,15.2,-1.29816314300002));
#263177=CARTESIAN_POINT('Ctrl Pts',(-10.7143992590001,11.6,-1.29816314300002));
#263178=CARTESIAN_POINT('Ctrl Pts',(-10.7118049930001,15.2,-1.29861052400001));
#263179=CARTESIAN_POINT('Ctrl Pts',(-10.7118049930001,11.6,-1.29861052400001));
#263180=CARTESIAN_POINT('Ctrl Pts',(-10.7092162110001,15.2,-1.29905469600001));
#263181=CARTESIAN_POINT('Ctrl Pts',(-10.7092162110001,11.6,-1.29905469600002));
#263182=CARTESIAN_POINT('Ctrl Pts',(-10.7066329250001,15.2,-1.29949566500001));
#263183=CARTESIAN_POINT('Ctrl Pts',(-10.7066329250001,11.6,-1.29949566500001));
#263184=CARTESIAN_POINT('Ctrl Pts',(-10.7040551500001,15.2,-1.29993343800002));
#263185=CARTESIAN_POINT('Ctrl Pts',(-10.7040551500001,11.6,-1.29993343800002));
#263186=CARTESIAN_POINT('Ctrl Pts',(-10.7014828960001,15.2,-1.30036802200001));
#263187=CARTESIAN_POINT('Ctrl Pts',(-10.7014828960001,11.6,-1.30036802200001));
#263188=CARTESIAN_POINT('Ctrl Pts',(-10.6989161770001,15.2,-1.30079942300001));
#263189=CARTESIAN_POINT('Ctrl Pts',(-10.6989161770001,11.6,-1.30079942300001));
#263190=CARTESIAN_POINT('Ctrl Pts',(-10.6963550050001,15.2,-1.30122764900001));
#263191=CARTESIAN_POINT('Ctrl Pts',(-10.6963550050001,11.6,-1.30122764900001));
#263192=CARTESIAN_POINT('Ctrl Pts',(-10.6937993940001,15.2,-1.30165270500001));
#263193=CARTESIAN_POINT('Ctrl Pts',(-10.6937993940001,11.6,-1.30165270500001));
#263194=CARTESIAN_POINT('Ctrl Pts',(-10.6912493550001,15.2,-1.30207460100001));
#263195=CARTESIAN_POINT('Ctrl Pts',(-10.6912493550001,11.6,-1.30207460100001));
#263196=CARTESIAN_POINT('Ctrl Pts',(-10.6887049020001,15.2,-1.30249334200002));
#263197=CARTESIAN_POINT('Ctrl Pts',(-10.6887049020001,11.6,-1.30249334200002));
#263198=CARTESIAN_POINT('Ctrl Pts',(-10.6861660490001,15.2,-1.30290893500002));
#263199=CARTESIAN_POINT('Ctrl Pts',(-10.6861660490001,11.6,-1.30290893500002));
#263200=CARTESIAN_POINT('Ctrl Pts',(-10.6836328060001,15.2,-1.30332138700001));
#263201=CARTESIAN_POINT('Ctrl Pts',(-10.6836328060001,11.6,-1.30332138700001));
#263202=CARTESIAN_POINT('Ctrl Pts',(-10.6811051890001,15.2,-1.30373070700001));
#263203=CARTESIAN_POINT('Ctrl Pts',(-10.6811051890001,11.6,-1.30373070700002));
#263204=CARTESIAN_POINT('Ctrl Pts',(-10.6785832090001,15.2,-1.30413690000001));
#263205=CARTESIAN_POINT('Ctrl Pts',(-10.6785832090001,11.6,-1.30413690000002));
#263206=CARTESIAN_POINT('Ctrl Pts',(-10.6760668780001,15.2,-1.30453997300001));
#263207=CARTESIAN_POINT('Ctrl Pts',(-10.6760668780001,11.6,-1.30453997300001));
#263208=CARTESIAN_POINT('Ctrl Pts',(-10.6735562130001,15.2,-1.30493993500002));
#263209=CARTESIAN_POINT('Ctrl Pts',(-10.6735562130001,11.6,-1.30493993500002));
#263210=CARTESIAN_POINT('Ctrl Pts',(-10.6710512220001,15.2,-1.30533679100001));
#263211=CARTESIAN_POINT('Ctrl Pts',(-10.6710512220001,11.6,-1.30533679100001));
#263212=CARTESIAN_POINT('Ctrl Pts',(-10.6685519220001,15.2,-1.30573054900001));
#263213=CARTESIAN_POINT('Ctrl Pts',(-10.6685519220001,11.6,-1.30573054900002));
#263214=CARTESIAN_POINT('Ctrl Pts',(-10.6660583240001,15.2,-1.30612121800001));
#263215=CARTESIAN_POINT('Ctrl Pts',(-10.6660583240001,11.6,-1.30612121800001));
#263216=CARTESIAN_POINT('Ctrl Pts',(-10.6635704410001,15.2,-1.30650880300001));
#263217=CARTESIAN_POINT('Ctrl Pts',(-10.6635704410001,11.6,-1.30650880300002));
#263218=CARTESIAN_POINT('Ctrl Pts',(-10.6610882880001,15.2,-1.30689331200001));
#263219=CARTESIAN_POINT('Ctrl Pts',(-10.6610882880001,11.6,-1.30689331200002));
#263220=CARTESIAN_POINT('Ctrl Pts',(-10.6586118770001,15.2,-1.30727475400001));
#263221=CARTESIAN_POINT('Ctrl Pts',(-10.6586118770001,11.6,-1.30727475400001));
#263222=CARTESIAN_POINT('Ctrl Pts',(-10.6561412200001,15.2,-1.30765313300001));
#263223=CARTESIAN_POINT('Ctrl Pts',(-10.6561412200001,11.6,-1.30765313300001));
#263224=CARTESIAN_POINT('Ctrl Pts',(-10.6536763330001,15.2,-1.30802845900002));
#263225=CARTESIAN_POINT('Ctrl Pts',(-10.6536763330001,11.6,-1.30802845900002));
#263226=CARTESIAN_POINT('Ctrl Pts',(-10.6512172270001,15.2,-1.30840073900002));
#263227=CARTESIAN_POINT('Ctrl Pts',(-10.6512172270001,11.6,-1.30840073900002));
#263228=CARTESIAN_POINT('Ctrl Pts',(-10.6487639160001,15.2,-1.30876997900002));
#263229=CARTESIAN_POINT('Ctrl Pts',(-10.6487639160001,11.6,-1.30876997900002));
#263230=CARTESIAN_POINT('Ctrl Pts',(-10.6463164150001,15.2,-1.30913618800002));
#263231=CARTESIAN_POINT('Ctrl Pts',(-10.6463164150001,11.6,-1.30913618800002));
#263232=CARTESIAN_POINT('Ctrl Pts',(-10.6438747330001,15.2,-1.30949937400001));
#263233=CARTESIAN_POINT('Ctrl Pts',(-10.6438747330001,11.6,-1.30949937400001));
#263234=CARTESIAN_POINT('Ctrl Pts',(-10.6414388880001,15.2,-1.30985954200002));
#263235=CARTESIAN_POINT('Ctrl Pts',(-10.6414388880001,11.6,-1.30985954200002));
#263236=CARTESIAN_POINT('Ctrl Pts',(-10.6390088920001,15.2,-1.31021670200001));
#263237=CARTESIAN_POINT('Ctrl Pts',(-10.6390088920001,11.6,-1.31021670200001));
#263238=CARTESIAN_POINT('Ctrl Pts',(-10.6365847570001,15.2,-1.31057086100002));
#263239=CARTESIAN_POINT('Ctrl Pts',(-10.6365847570001,11.6,-1.31057086100002));
#263240=CARTESIAN_POINT('Ctrl Pts',(-10.6341664980001,15.2,-1.31092202700001));
#263241=CARTESIAN_POINT('Ctrl Pts',(-10.6341664980001,11.6,-1.31092202700001));
#263242=CARTESIAN_POINT('Ctrl Pts',(-10.6317541280001,15.2,-1.31127020600001));
#263243=CARTESIAN_POINT('Ctrl Pts',(-10.6317541280001,11.6,-1.31127020600002));
#263244=CARTESIAN_POINT('Ctrl Pts',(-10.6293476610001,15.2,-1.31161540800001));
#263245=CARTESIAN_POINT('Ctrl Pts',(-10.6293476610001,11.6,-1.31161540800001));
#263246=CARTESIAN_POINT('Ctrl Pts',(-10.6269471100001,15.2,-1.31195763900001));
#263247=CARTESIAN_POINT('Ctrl Pts',(-10.6269471100001,11.6,-1.31195763900001));
#263248=CARTESIAN_POINT('Ctrl Pts',(-10.6245524890001,15.2,-1.31229690700001));
#263249=CARTESIAN_POINT('Ctrl Pts',(-10.6245524890001,11.6,-1.31229690700002));
#263250=CARTESIAN_POINT('Ctrl Pts',(-10.6221638120001,15.2,-1.31263322000001));
#263251=CARTESIAN_POINT('Ctrl Pts',(-10.6221638120001,11.6,-1.31263322000002));
#263252=CARTESIAN_POINT('Ctrl Pts',(-10.6197810910001,15.2,-1.31296658600002));
#263253=CARTESIAN_POINT('Ctrl Pts',(-10.6197810910001,11.6,-1.31296658600002));
#263254=CARTESIAN_POINT('Ctrl Pts',(-10.6174043430001,15.2,-1.31329701400002));
#263255=CARTESIAN_POINT('Ctrl Pts',(-10.6174043430001,11.6,-1.31329701400002));
#263256=CARTESIAN_POINT('Ctrl Pts',(-10.6150335790001,15.2,-1.31362450900002));
#263257=CARTESIAN_POINT('Ctrl Pts',(-10.6150335790001,11.6,-1.31362450900002));
#263258=CARTESIAN_POINT('Ctrl Pts',(-10.6126688130001,15.2,-1.31394908200001));
#263259=CARTESIAN_POINT('Ctrl Pts',(-10.6126688130001,11.6,-1.31394908200001));
#263260=CARTESIAN_POINT('Ctrl Pts',(-10.6103100600001,15.2,-1.31427073900001));
#263261=CARTESIAN_POINT('Ctrl Pts',(-10.6103100600001,11.6,-1.31427073900001));
#263262=CARTESIAN_POINT('Ctrl Pts',(-10.6079573330001,15.2,-1.31458948800002));
#263263=CARTESIAN_POINT('Ctrl Pts',(-10.6079573330001,11.6,-1.31458948800002));
#263264=CARTESIAN_POINT('Ctrl Pts',(-10.6056106460001,15.2,-1.31490533800001));
#263265=CARTESIAN_POINT('Ctrl Pts',(-10.6056106460001,11.6,-1.31490533800001));
#263266=CARTESIAN_POINT('Ctrl Pts',(-10.6032700140001,15.2,-1.31521829600001));
#263267=CARTESIAN_POINT('Ctrl Pts',(-10.6032700140001,11.6,-1.31521829600001));
#263268=CARTESIAN_POINT('Ctrl Pts',(-10.6009354490001,15.2,-1.31552837200001));
#263269=CARTESIAN_POINT('Ctrl Pts',(-10.6009354490001,11.6,-1.31552837200001));
#263270=CARTESIAN_POINT('Ctrl Pts',(-10.5986069670001,15.2,-1.31583557100001));
#263271=CARTESIAN_POINT('Ctrl Pts',(-10.5986069670001,11.6,-1.31583557100001));
#263272=CARTESIAN_POINT('Ctrl Pts',(-10.5962845810001,15.2,-1.31613990400002));
#263273=CARTESIAN_POINT('Ctrl Pts',(-10.5962845810001,11.6,-1.31613990400002));
#263274=CARTESIAN_POINT('Ctrl Pts',(-10.5939683050001,15.2,-1.31644137800001));
#263275=CARTESIAN_POINT('Ctrl Pts',(-10.5939683050001,11.6,-1.31644137800001));
#263276=CARTESIAN_POINT('Ctrl Pts',(-10.5916581540001,15.2,-1.31674000200002));
#263277=CARTESIAN_POINT('Ctrl Pts',(-10.5916581540001,11.6,-1.31674000200002));
#263278=CARTESIAN_POINT('Ctrl Pts',(-10.5893541410001,15.2,-1.31703578300002));
#263279=CARTESIAN_POINT('Ctrl Pts',(-10.5893541410001,11.6,-1.31703578300002));
#263280=CARTESIAN_POINT('Ctrl Pts',(-10.5870562810001,15.2,-1.31732872900002));
#263281=CARTESIAN_POINT('Ctrl Pts',(-10.5870562810001,11.6,-1.31732872900002));
#263282=CARTESIAN_POINT('Ctrl Pts',(-10.5847645880001,15.2,-1.31761885100001));
#263283=CARTESIAN_POINT('Ctrl Pts',(-10.5847645880001,11.6,-1.31761885100001));
#263284=CARTESIAN_POINT('Ctrl Pts',(-10.5824790750001,15.2,-1.31790615500002));
#263285=CARTESIAN_POINT('Ctrl Pts',(-10.5824790750001,11.6,-1.31790615500002));
#263286=CARTESIAN_POINT('Ctrl Pts',(-10.5801997580001,15.2,-1.31819064900002));
#263287=CARTESIAN_POINT('Ctrl Pts',(-10.5801997580001,11.6,-1.31819064900002));
#263288=CARTESIAN_POINT('Ctrl Pts',(-10.5779266520001,15.2,-1.31847234300002));
#263289=CARTESIAN_POINT('Ctrl Pts',(-10.5779266520001,11.6,-1.31847234300002));
#263290=CARTESIAN_POINT('Ctrl Pts',(-10.5756597690001,15.2,-1.31875124500001));
#263291=CARTESIAN_POINT('Ctrl Pts',(-10.5756597690001,11.6,-1.31875124500001));
#263292=CARTESIAN_POINT('Ctrl Pts',(-10.5733991250001,15.2,-1.31902736300002));
#263293=CARTESIAN_POINT('Ctrl Pts',(-10.5733991250001,11.6,-1.31902736300002));
#263294=CARTESIAN_POINT('Ctrl Pts',(-10.5711447350001,15.2,-1.31930070600002));
#263295=CARTESIAN_POINT('Ctrl Pts',(-10.5711447350001,11.6,-1.31930070600002));
#263296=CARTESIAN_POINT('Ctrl Pts',(-10.5688966110001,15.2,-1.31957128200002));
#263297=CARTESIAN_POINT('Ctrl Pts',(-10.5688966110001,11.6,-1.31957128200002));
#263298=CARTESIAN_POINT('Ctrl Pts',(-10.5666547700001,15.2,-1.31983910100002));
#263299=CARTESIAN_POINT('Ctrl Pts',(-10.5666547700001,11.6,-1.31983910100002));
#263300=CARTESIAN_POINT('Ctrl Pts',(-10.5644192250001,15.2,-1.32010417000001));
#263301=CARTESIAN_POINT('Ctrl Pts',(-10.5644192250001,11.6,-1.32010417000001));
#263302=CARTESIAN_POINT('Ctrl Pts',(-10.5621899910001,15.2,-1.32036649800002));
#263303=CARTESIAN_POINT('Ctrl Pts',(-10.5621899910001,11.6,-1.32036649800002));
#263304=CARTESIAN_POINT('Ctrl Pts',(-10.5599670840001,15.2,-1.32062609500001));
#263305=CARTESIAN_POINT('Ctrl Pts',(-10.5599670840001,11.6,-1.32062609500002));
#263306=CARTESIAN_POINT('Ctrl Pts',(-10.5577505170001,15.2,-1.32088296800001));
#263307=CARTESIAN_POINT('Ctrl Pts',(-10.5577505170001,11.6,-1.32088296800001));
#263308=CARTESIAN_POINT('Ctrl Pts',(-10.5555403050001,15.2,-1.32113712700002));
#263309=CARTESIAN_POINT('Ctrl Pts',(-10.5555403050001,11.6,-1.32113712700002));
#263310=CARTESIAN_POINT('Ctrl Pts',(-10.5533364630001,15.2,-1.32138858100001));
#263311=CARTESIAN_POINT('Ctrl Pts',(-10.5533364630001,11.6,-1.32138858100001));
#263312=CARTESIAN_POINT('Ctrl Pts',(-10.5511390070001,15.2,-1.32163733700001));
#263313=CARTESIAN_POINT('Ctrl Pts',(-10.5511390070001,11.6,-1.32163733700001));
#263314=CARTESIAN_POINT('Ctrl Pts',(-10.5489479500001,15.2,-1.32188340500001));
#263315=CARTESIAN_POINT('Ctrl Pts',(-10.5489479500001,11.6,-1.32188340500001));
#263316=CARTESIAN_POINT('Ctrl Pts',(-10.5467633070001,15.2,-1.32212679400002));
#263317=CARTESIAN_POINT('Ctrl Pts',(-10.5467633070001,11.6,-1.32212679400002));
#263318=CARTESIAN_POINT('Ctrl Pts',(-10.5445850930001,15.2,-1.32236751500002));
#263319=CARTESIAN_POINT('Ctrl Pts',(-10.5445850930001,11.6,-1.32236751500002));
#263320=CARTESIAN_POINT('Ctrl Pts',(-10.5424133250001,15.2,-1.32260557300001));
#263321=CARTESIAN_POINT('Ctrl Pts',(-10.5424133250001,11.6,-1.32260557300001));
#263322=CARTESIAN_POINT('Ctrl Pts',(-10.5402480150001,15.2,-1.32284098000001));
#263323=CARTESIAN_POINT('Ctrl Pts',(-10.5402480150001,11.6,-1.32284098000001));
#263324=CARTESIAN_POINT('Ctrl Pts',(-10.5380891800001,15.2,-1.32307374300002));
#263325=CARTESIAN_POINT('Ctrl Pts',(-10.5380891800001,11.6,-1.32307374300002));
#263326=CARTESIAN_POINT('Ctrl Pts',(-10.5359368350001,15.2,-1.32330387300001));
#263327=CARTESIAN_POINT('Ctrl Pts',(-10.5359368350001,11.6,-1.32330387300002));
#263328=CARTESIAN_POINT('Ctrl Pts',(-10.5337909930001,15.2,-1.32353137900001));
#263329=CARTESIAN_POINT('Ctrl Pts',(-10.5337909930001,11.6,-1.32353137900001));
#263330=CARTESIAN_POINT('Ctrl Pts',(-10.5316516720001,15.2,-1.32375626900001));
#263331=CARTESIAN_POINT('Ctrl Pts',(-10.5316516720001,11.6,-1.32375626900001));
#263332=CARTESIAN_POINT('Ctrl Pts',(-10.5295188860001,15.2,-1.32397855400002));
#263333=CARTESIAN_POINT('Ctrl Pts',(-10.5295188860001,11.6,-1.32397855400002));
#263334=CARTESIAN_POINT('Ctrl Pts',(-10.5273926510001,15.2,-1.32419824100001));
#263335=CARTESIAN_POINT('Ctrl Pts',(-10.5273926510001,11.6,-1.32419824100001));
#263336=CARTESIAN_POINT('Ctrl Pts',(-10.5252729800001,15.2,-1.32441534000002));
#263337=CARTESIAN_POINT('Ctrl Pts',(-10.5252729800001,11.6,-1.32441534000002));
#263338=CARTESIAN_POINT('Ctrl Pts',(-10.5231598910001,15.2,-1.32462986200002));
#263339=CARTESIAN_POINT('Ctrl Pts',(-10.5231598910001,11.6,-1.32462986200002));
#263340=CARTESIAN_POINT('Ctrl Pts',(-10.5210533970001,15.2,-1.32484181400002));
#263341=CARTESIAN_POINT('Ctrl Pts',(-10.5210533970001,11.6,-1.32484181400002));
#263342=CARTESIAN_POINT('Ctrl Pts',(-10.5189535150001,15.2,-1.32505120800001));
#263343=CARTESIAN_POINT('Ctrl Pts',(-10.5189535150001,11.6,-1.32505120800001));
#263344=CARTESIAN_POINT('Ctrl Pts',(-10.5168602610001,15.2,-1.32525805100002));
#263345=CARTESIAN_POINT('Ctrl Pts',(-10.5168602610001,11.6,-1.32525805100002));
#263346=CARTESIAN_POINT('Ctrl Pts',(-10.5147736500001,15.2,-1.32546235400001));
#263347=CARTESIAN_POINT('Ctrl Pts',(-10.5147736500001,11.6,-1.32546235400001));
#263348=CARTESIAN_POINT('Ctrl Pts',(-10.5126936960001,15.2,-1.32566412600001));
#263349=CARTESIAN_POINT('Ctrl Pts',(-10.5126936960001,11.6,-1.32566412600002));
#263350=CARTESIAN_POINT('Ctrl Pts',(-10.5106204160001,15.2,-1.32586337800001));
#263351=CARTESIAN_POINT('Ctrl Pts',(-10.5106204160001,11.6,-1.32586337800001));
#263352=CARTESIAN_POINT('Ctrl Pts',(-10.5085538250001,15.2,-1.32606011700001));
#263353=CARTESIAN_POINT('Ctrl Pts',(-10.5085538250001,11.6,-1.32606011700001));
#263354=CARTESIAN_POINT('Ctrl Pts',(-10.5064939400001,15.2,-1.32625435500001));
#263355=CARTESIAN_POINT('Ctrl Pts',(-10.5064939400001,11.6,-1.32625435500001));
#263356=CARTESIAN_POINT('Ctrl Pts',(-10.5044407750001,15.2,-1.32644610000002));
#263357=CARTESIAN_POINT('Ctrl Pts',(-10.5044407750001,11.6,-1.32644610000002));
#263358=CARTESIAN_POINT('Ctrl Pts',(-10.5023943470001,15.2,-1.32663536300001));
#263359=CARTESIAN_POINT('Ctrl Pts',(-10.5023943470001,11.6,-1.32663536300001));
#263360=CARTESIAN_POINT('Ctrl Pts',(-10.5003546710001,15.2,-1.32682215400001));
#263361=CARTESIAN_POINT('Ctrl Pts',(-10.5003546710001,11.6,-1.32682215400001));
#263362=CARTESIAN_POINT('Ctrl Pts',(-10.4983217640001,15.2,-1.32700648100001));
#263363=CARTESIAN_POINT('Ctrl Pts',(-10.4983217640001,11.6,-1.32700648100002));
#263364=CARTESIAN_POINT('Ctrl Pts',(-10.4962956400001,15.2,-1.32718835600001));
#263365=CARTESIAN_POINT('Ctrl Pts',(-10.4962956400001,11.6,-1.32718835600001));
#263366=CARTESIAN_POINT('Ctrl Pts',(-10.4942763170001,15.2,-1.32736778800002));
#263367=CARTESIAN_POINT('Ctrl Pts',(-10.4942763170001,11.6,-1.32736778800002));
#263368=CARTESIAN_POINT('Ctrl Pts',(-10.4922638100001,15.2,-1.32754478700001));
#263369=CARTESIAN_POINT('Ctrl Pts',(-10.4922638100001,11.6,-1.32754478700001));
#263370=CARTESIAN_POINT('Ctrl Pts',(-10.4902581350001,15.2,-1.32771936200001));
#263371=CARTESIAN_POINT('Ctrl Pts',(-10.4902581350001,11.6,-1.32771936200002));
#263372=CARTESIAN_POINT('Ctrl Pts',(-10.4882593090001,15.2,-1.32789152500001));
#263373=CARTESIAN_POINT('Ctrl Pts',(-10.4882593090001,11.6,-1.32789152500001));
#263374=CARTESIAN_POINT('Ctrl Pts',(-10.4862673460001,15.2,-1.32806128600001));
#263375=CARTESIAN_POINT('Ctrl Pts',(-10.4862673460001,11.6,-1.32806128600001));
#263376=CARTESIAN_POINT('Ctrl Pts',(-10.4842822650001,15.2,-1.32822865400001));
#263377=CARTESIAN_POINT('Ctrl Pts',(-10.4842822650001,11.6,-1.32822865400001));
#263378=CARTESIAN_POINT('Ctrl Pts',(-10.4823040800001,15.2,-1.32839363900001));
#263379=CARTESIAN_POINT('Ctrl Pts',(-10.4823040800001,11.6,-1.32839363900001));
#263380=CARTESIAN_POINT('Ctrl Pts',(-10.4803328080001,15.2,-1.32855625200001));
#263381=CARTESIAN_POINT('Ctrl Pts',(-10.4803328080001,11.6,-1.32855625200001));
#263382=CARTESIAN_POINT('Ctrl Pts',(-10.4783684660001,15.2,-1.32871650300002));
#263383=CARTESIAN_POINT('Ctrl Pts',(-10.4783684660001,11.6,-1.32871650300002));
#263384=CARTESIAN_POINT('Ctrl Pts',(-10.4764110690001,15.2,-1.32887440400001));
#263385=CARTESIAN_POINT('Ctrl Pts',(-10.4764110690001,11.6,-1.32887440400001));
#263386=CARTESIAN_POINT('Ctrl Pts',(-10.4744606350001,15.2,-1.32902996200002));
#263387=CARTESIAN_POINT('Ctrl Pts',(-10.4744606350001,11.6,-1.32902996200002));
#263388=CARTESIAN_POINT('Ctrl Pts',(-10.4725171800001,15.2,-1.32918319000002));
#263389=CARTESIAN_POINT('Ctrl Pts',(-10.4725171800001,11.6,-1.32918319000002));
#263390=CARTESIAN_POINT('Ctrl Pts',(-10.4705807200001,15.2,-1.32933409700001));
#263391=CARTESIAN_POINT('Ctrl Pts',(-10.4705807200001,11.6,-1.32933409700001));
#263392=CARTESIAN_POINT('Ctrl Pts',(-10.4686512720001,15.2,-1.32948269500002));
#263393=CARTESIAN_POINT('Ctrl Pts',(-10.4686512720001,11.6,-1.32948269500002));
#263394=CARTESIAN_POINT('Ctrl Pts',(-10.4667288520001,15.2,-1.32962899400002));
#263395=CARTESIAN_POINT('Ctrl Pts',(-10.4667288520001,11.6,-1.32962899400002));
#263396=CARTESIAN_POINT('Ctrl Pts',(-10.4648134780001,15.2,-1.32977300400002));
#263397=CARTESIAN_POINT('Ctrl Pts',(-10.4648134780001,11.6,-1.32977300400002));
#263398=CARTESIAN_POINT('Ctrl Pts',(-10.4629051650001,15.2,-1.32991473500002));
#263399=CARTESIAN_POINT('Ctrl Pts',(-10.4629051650001,11.6,-1.32991473500002));
#263400=CARTESIAN_POINT('Ctrl Pts',(-10.4610039310001,15.2,-1.33005420000002));
#263401=CARTESIAN_POINT('Ctrl Pts',(-10.4610039310001,11.6,-1.33005420000002));
#263402=CARTESIAN_POINT('Ctrl Pts',(-10.4591097930001,15.2,-1.33019140900001));
#263403=CARTESIAN_POINT('Ctrl Pts',(-10.4591097930001,11.6,-1.33019140900001));
#263404=CARTESIAN_POINT('Ctrl Pts',(-10.4572227670001,15.2,-1.33032637100001));
#263405=CARTESIAN_POINT('Ctrl Pts',(-10.4572227670001,11.6,-1.33032637100001));
#263406=CARTESIAN_POINT('Ctrl Pts',(-10.4553428710001,15.2,-1.33045909900002));
#263407=CARTESIAN_POINT('Ctrl Pts',(-10.4553428710001,11.6,-1.33045909900002));
#263408=CARTESIAN_POINT('Ctrl Pts',(-10.4534701210001,15.2,-1.33058960200001));
#263409=CARTESIAN_POINT('Ctrl Pts',(-10.4534701210001,11.6,-1.33058960200001));
#263410=CARTESIAN_POINT('Ctrl Pts',(-10.4516045340001,15.2,-1.33071789400002));
#263411=CARTESIAN_POINT('Ctrl Pts',(-10.4516045340001,11.6,-1.33071789400002));
#263412=CARTESIAN_POINT('Ctrl Pts',(-10.4497461280001,15.2,-1.33084398300001));
#263413=CARTESIAN_POINT('Ctrl Pts',(-10.4497461280001,11.6,-1.33084398300001));
#263414=CARTESIAN_POINT('Ctrl Pts',(-10.4478949200001,15.2,-1.33096788000001));
#263415=CARTESIAN_POINT('Ctrl Pts',(-10.4478949200001,11.6,-1.33096788000001));
#263416=CARTESIAN_POINT('Ctrl Pts',(-10.4460509260001,15.2,-1.33108959700001));
#263417=CARTESIAN_POINT('Ctrl Pts',(-10.4460509260001,11.6,-1.33108959700001));
#263418=CARTESIAN_POINT('Ctrl Pts',(-10.4442141650001,15.2,-1.33120914700001));
#263419=CARTESIAN_POINT('Ctrl Pts',(-10.4442141650001,11.6,-1.33120914700001));
#263420=CARTESIAN_POINT('Ctrl Pts',(-10.4423846530001,15.2,-1.33132653900002));
#263421=CARTESIAN_POINT('Ctrl Pts',(-10.4423846530001,11.6,-1.33132653900002));
#263422=CARTESIAN_POINT('Ctrl Pts',(-10.4405624080001,15.2,-1.33144178400002));
#263423=CARTESIAN_POINT('Ctrl Pts',(-10.4405624080001,11.6,-1.33144178400002));
#263424=CARTESIAN_POINT('Ctrl Pts',(-10.4387474470001,15.2,-1.33155489400002));
#263425=CARTESIAN_POINT('Ctrl Pts',(-10.4387474470001,11.6,-1.33155489400002));
#263426=CARTESIAN_POINT('Ctrl Pts',(-10.4369397880001,15.2,-1.33166588100002));
#263427=CARTESIAN_POINT('Ctrl Pts',(-10.4369397880001,11.6,-1.33166588100002));
#263428=CARTESIAN_POINT('Ctrl Pts',(-10.4351394480001,15.2,-1.33177475500001));
#263429=CARTESIAN_POINT('Ctrl Pts',(-10.4351394480001,11.6,-1.33177475500002));
#263430=CARTESIAN_POINT('Ctrl Pts',(-10.4333464460001,15.2,-1.33188152900001));
#263431=CARTESIAN_POINT('Ctrl Pts',(-10.4333464460001,11.6,-1.33188152900001));
#263432=CARTESIAN_POINT('Ctrl Pts',(-10.4315607980001,15.2,-1.33198621200001));
#263433=CARTESIAN_POINT('Ctrl Pts',(-10.4315607980001,11.6,-1.33198621200001));
#263434=CARTESIAN_POINT('Ctrl Pts',(-10.4297825220001,15.2,-1.33208881900002));
#263435=CARTESIAN_POINT('Ctrl Pts',(-10.4297825220001,11.6,-1.33208881900002));
#263436=CARTESIAN_POINT('Ctrl Pts',(-10.4280116360001,15.2,-1.33218936000001));
#263437=CARTESIAN_POINT('Ctrl Pts',(-10.4280116360001,11.6,-1.33218936000001));
#263438=CARTESIAN_POINT('Ctrl Pts',(-10.4262481590001,15.2,-1.33228784500002));
#263439=CARTESIAN_POINT('Ctrl Pts',(-10.4262481590001,11.6,-1.33228784500002));
#263440=CARTESIAN_POINT('Ctrl Pts',(-10.4244921060001,15.2,-1.33238428800002));
#263441=CARTESIAN_POINT('Ctrl Pts',(-10.4244921060001,11.6,-1.33238428800002));
#263442=CARTESIAN_POINT('Ctrl Pts',(-10.4227434980001,15.2,-1.33247870000002));
#263443=CARTESIAN_POINT('Ctrl Pts',(-10.4227434980001,11.6,-1.33247870000002));
#263444=CARTESIAN_POINT('Ctrl Pts',(-10.4210023520001,15.2,-1.33257109300001));
#263445=CARTESIAN_POINT('Ctrl Pts',(-10.4210023520001,11.6,-1.33257109300001));
#263446=CARTESIAN_POINT('Ctrl Pts',(-10.4192686840001,15.2,-1.33266147700001));
#263447=CARTESIAN_POINT('Ctrl Pts',(-10.4192686840001,11.6,-1.33266147700001));
#263448=CARTESIAN_POINT('Ctrl Pts',(-10.4175425150001,15.2,-1.33274986700001));
#263449=CARTESIAN_POINT('Ctrl Pts',(-10.4175425150001,11.6,-1.33274986700001));
#263450=CARTESIAN_POINT('Ctrl Pts',(-10.4158238630001,15.2,-1.33283627400001));
#263451=CARTESIAN_POINT('Ctrl Pts',(-10.4158238630001,11.6,-1.33283627400001));
#263452=CARTESIAN_POINT('Ctrl Pts',(-10.4141127450001,15.2,-1.33292070900001));
#263453=CARTESIAN_POINT('Ctrl Pts',(-10.4141127450001,11.6,-1.33292070900001));
#263454=CARTESIAN_POINT('Ctrl Pts',(-10.4124091790001,15.2,-1.33300318500002));
#263455=CARTESIAN_POINT('Ctrl Pts',(-10.4124091790001,11.6,-1.33300318500002));
#263456=CARTESIAN_POINT('Ctrl Pts',(-10.4107131830001,15.2,-1.33308371300001));
#263457=CARTESIAN_POINT('Ctrl Pts',(-10.4107131830001,11.6,-1.33308371300001));
#263458=CARTESIAN_POINT('Ctrl Pts',(-10.4090247790001,15.2,-1.33316230600002));
#263459=CARTESIAN_POINT('Ctrl Pts',(-10.4090247790001,11.6,-1.33316230600002));
#263460=CARTESIAN_POINT('Ctrl Pts',(-10.4073439810001,15.2,-1.33323897700001));
#263461=CARTESIAN_POINT('Ctrl Pts',(-10.4073439810001,11.6,-1.33323897700001));
#263462=CARTESIAN_POINT('Ctrl Pts',(-10.4056708110001,15.2,-1.33331373800001));
#263463=CARTESIAN_POINT('Ctrl Pts',(-10.4056708110001,11.6,-1.33331373800001));
#263464=CARTESIAN_POINT('Ctrl Pts',(-10.4040052850001,15.2,-1.33338660100002));
#263465=CARTESIAN_POINT('Ctrl Pts',(-10.4040052850001,11.6,-1.33338660100002));
#263466=CARTESIAN_POINT('Ctrl Pts',(-10.4023474230001,15.2,-1.33345757700001));
#263467=CARTESIAN_POINT('Ctrl Pts',(-10.4023474230001,11.6,-1.33345757700001));
#263468=CARTESIAN_POINT('Ctrl Pts',(-10.4006972440001,15.2,-1.33352668100001));
#263469=CARTESIAN_POINT('Ctrl Pts',(-10.4006972440001,11.6,-1.33352668100002));
#263470=CARTESIAN_POINT('Ctrl Pts',(-10.3990547660001,15.2,-1.33359392500001));
#263471=CARTESIAN_POINT('Ctrl Pts',(-10.3990547660001,11.6,-1.33359392500001));
#263472=CARTESIAN_POINT('Ctrl Pts',(-10.3974200090001,15.2,-1.33365931900002));
#263473=CARTESIAN_POINT('Ctrl Pts',(-10.3974200090001,11.6,-1.33365931900002));
#263474=CARTESIAN_POINT('Ctrl Pts',(-10.3957929910001,15.2,-1.33372288000002));
#263475=CARTESIAN_POINT('Ctrl Pts',(-10.3957929910001,11.6,-1.33372288000002));
#263476=CARTESIAN_POINT('Ctrl Pts',(-10.3941737300001,15.2,-1.33378461700001));
#263477=CARTESIAN_POINT('Ctrl Pts',(-10.3941737300001,11.6,-1.33378461700001));
#263478=CARTESIAN_POINT('Ctrl Pts',(-10.3925622480001,15.2,-1.33384454600002));
#263479=CARTESIAN_POINT('Ctrl Pts',(-10.3925622480001,11.6,-1.33384454600002));
#263480=CARTESIAN_POINT('Ctrl Pts',(-10.3909585610001,15.2,-1.33390267600001));
#263481=CARTESIAN_POINT('Ctrl Pts',(-10.3909585610001,11.6,-1.33390267600001));
#263482=CARTESIAN_POINT('Ctrl Pts',(-10.3893626900001,15.2,-1.33395902400002));
#263483=CARTESIAN_POINT('Ctrl Pts',(-10.3893626900001,11.6,-1.33395902400002));
#263484=CARTESIAN_POINT('Ctrl Pts',(-10.3877746550001,15.2,-1.33401360000001));
#263485=CARTESIAN_POINT('Ctrl Pts',(-10.3877746550001,11.6,-1.33401360000002));
#263486=CARTESIAN_POINT('Ctrl Pts',(-10.3861944730001,15.2,-1.33406641800002));
#263487=CARTESIAN_POINT('Ctrl Pts',(-10.3861944730001,11.6,-1.33406641800002));
#263488=CARTESIAN_POINT('Ctrl Pts',(-10.3846221650001,15.2,-1.33411749200001));
#263489=CARTESIAN_POINT('Ctrl Pts',(-10.3846221650001,11.6,-1.33411749200001));
#263490=CARTESIAN_POINT('Ctrl Pts',(-10.3830577510001,15.2,-1.33416683400001));
#263491=CARTESIAN_POINT('Ctrl Pts',(-10.3830577510001,11.6,-1.33416683400002));
#263492=CARTESIAN_POINT('Ctrl Pts',(-10.3815012490001,15.2,-1.33421445700002));
#263493=CARTESIAN_POINT('Ctrl Pts',(-10.3815012490001,11.6,-1.33421445700002));
#263494=CARTESIAN_POINT('Ctrl Pts',(-10.3799526800001,15.2,-1.33426037500001));
#263495=CARTESIAN_POINT('Ctrl Pts',(-10.3799526800001,11.6,-1.33426037500001));
#263496=CARTESIAN_POINT('Ctrl Pts',(-10.3784120630001,15.2,-1.33430460200001));
#263497=CARTESIAN_POINT('Ctrl Pts',(-10.3784120630001,11.6,-1.33430460200001));
#263498=CARTESIAN_POINT('Ctrl Pts',(-10.3768794170001,15.2,-1.33434714900002));
#263499=CARTESIAN_POINT('Ctrl Pts',(-10.3768794170001,11.6,-1.33434714900002));
#263500=CARTESIAN_POINT('Ctrl Pts',(-10.3753547630001,15.2,-1.33438803300002));
#263501=CARTESIAN_POINT('Ctrl Pts',(-10.3753547630001,11.6,-1.33438803300002));
#263502=CARTESIAN_POINT('Ctrl Pts',(-10.3738381210001,15.2,-1.33442726500002));
#263503=CARTESIAN_POINT('Ctrl Pts',(-10.3738381210001,11.6,-1.33442726500002));
#263504=CARTESIAN_POINT('Ctrl Pts',(-10.3723295110001,15.2,-1.33446485900001));
#263505=CARTESIAN_POINT('Ctrl Pts',(-10.3723295110001,11.6,-1.33446485900001));
#263506=CARTESIAN_POINT('Ctrl Pts',(-10.3708289520001,15.2,-1.33450082900001));
#263507=CARTESIAN_POINT('Ctrl Pts',(-10.3708289520001,11.6,-1.33450082900001));
#263508=CARTESIAN_POINT('Ctrl Pts',(-10.3693364650001,15.2,-1.33453518900001));
#263509=CARTESIAN_POINT('Ctrl Pts',(-10.3693364650001,11.6,-1.33453518900001));
#263510=CARTESIAN_POINT('Ctrl Pts',(-10.3678520690001,15.2,-1.33456795200001));
#263511=CARTESIAN_POINT('Ctrl Pts',(-10.3678520690001,11.6,-1.33456795200001));
#263512=CARTESIAN_POINT('Ctrl Pts',(-10.3663757870001,15.2,-1.33459913200001));
#263513=CARTESIAN_POINT('Ctrl Pts',(-10.3663757870001,11.6,-1.33459913200001));
#263514=CARTESIAN_POINT('Ctrl Pts',(-10.3649076360001,15.2,-1.33462874400001));
#263515=CARTESIAN_POINT('Ctrl Pts',(-10.3649076360001,11.6,-1.33462874400002));
#263516=CARTESIAN_POINT('Ctrl Pts',(-10.3634476390001,15.2,-1.33465680100001));
#263517=CARTESIAN_POINT('Ctrl Pts',(-10.3634476390001,11.6,-1.33465680100001));
#263518=CARTESIAN_POINT('Ctrl Pts',(-10.3619958160001,15.2,-1.33468331700001));
#263519=CARTESIAN_POINT('Ctrl Pts',(-10.3619958160001,11.6,-1.33468331700001));
#263520=CARTESIAN_POINT('Ctrl Pts',(-10.3605521870001,15.2,-1.33470830800002));
#263521=CARTESIAN_POINT('Ctrl Pts',(-10.3605521870001,11.6,-1.33470830800002));
#263522=CARTESIAN_POINT('Ctrl Pts',(-10.3591167720001,15.2,-1.33473178600001));
#263523=CARTESIAN_POINT('Ctrl Pts',(-10.3591167720001,11.6,-1.33473178600001));
#263524=CARTESIAN_POINT('Ctrl Pts',(-10.3576895940001,15.2,-1.33475376600002));
#263525=CARTESIAN_POINT('Ctrl Pts',(-10.3576895940001,11.6,-1.33475376600002));
#263526=CARTESIAN_POINT('Ctrl Pts',(-10.3562706710001,15.2,-1.33477426200002));
#263527=CARTESIAN_POINT('Ctrl Pts',(-10.3562706710001,11.6,-1.33477426200002));
#263528=CARTESIAN_POINT('Ctrl Pts',(-10.3548600260001,15.2,-1.33479329000001));
#263529=CARTESIAN_POINT('Ctrl Pts',(-10.3548600260001,11.6,-1.33479329000001));
#263530=CARTESIAN_POINT('Ctrl Pts',(-10.3534576790001,15.2,-1.33481086200002));
#263531=CARTESIAN_POINT('Ctrl Pts',(-10.3534576790001,11.6,-1.33481086200002));
#263532=CARTESIAN_POINT('Ctrl Pts',(-10.3520636520001,15.2,-1.33482699500002));
#263533=CARTESIAN_POINT('Ctrl Pts',(-10.3520636520001,11.6,-1.33482699500002));
#263534=CARTESIAN_POINT('Ctrl Pts',(-10.3506779650001,15.2,-1.33484170200001));
#263535=CARTESIAN_POINT('Ctrl Pts',(-10.3506779650001,11.6,-1.33484170200001));
#263536=CARTESIAN_POINT('Ctrl Pts',(-10.3493006400001,15.2,-1.33485499900001));
#263537=CARTESIAN_POINT('Ctrl Pts',(-10.3493006400001,11.6,-1.33485499900001));
#263538=CARTESIAN_POINT('Ctrl Pts',(-10.3479316980001,15.2,-1.33486689900002));
#263539=CARTESIAN_POINT('Ctrl Pts',(-10.3479316980001,11.6,-1.33486689900002));
#263540=CARTESIAN_POINT('Ctrl Pts',(-10.3465711600001,15.2,-1.33487741900002));
#263541=CARTESIAN_POINT('Ctrl Pts',(-10.3465711600001,11.6,-1.33487741900002));
#263542=CARTESIAN_POINT('Ctrl Pts',(-10.3452190490001,15.2,-1.33488657300001));
#263543=CARTESIAN_POINT('Ctrl Pts',(-10.3452190490001,11.6,-1.33488657300001));
#263544=CARTESIAN_POINT('Ctrl Pts',(-10.3438753840001,15.2,-1.33489437600002));
#263545=CARTESIAN_POINT('Ctrl Pts',(-10.3438753840001,11.6,-1.33489437600002));
#263546=CARTESIAN_POINT('Ctrl Pts',(-10.3425401900001,15.2,-1.33490084300002));
#263547=CARTESIAN_POINT('Ctrl Pts',(-10.3425401900001,11.6,-1.33490084300002));
#263548=CARTESIAN_POINT('Ctrl Pts',(-10.3412134860001,15.2,-1.33490598900002));
#263549=CARTESIAN_POINT('Ctrl Pts',(-10.3412134860001,11.6,-1.33490598900002));
#263550=CARTESIAN_POINT('Ctrl Pts',(-10.3398952940001,15.2,-1.33490982900001));
#263551=CARTESIAN_POINT('Ctrl Pts',(-10.3398952940001,11.6,-1.33490982900002));
#263552=CARTESIAN_POINT('Ctrl Pts',(-10.3385856380001,15.2,-1.33491238000001));
#263553=CARTESIAN_POINT('Ctrl Pts',(-10.3385856380001,11.6,-1.33491238000001));
#263554=CARTESIAN_POINT('Ctrl Pts',(-10.3372845370001,15.2,-1.33491365700001));
#263555=CARTESIAN_POINT('Ctrl Pts',(-10.3372845370001,11.6,-1.33491365700001));
#263556=CARTESIAN_POINT('Ctrl Pts',(-10.3359920170001,15.2,-1.33491367300001));
#263557=CARTESIAN_POINT('Ctrl Pts',(-10.3359920170001,11.6,-1.33491367300001));
#263558=CARTESIAN_POINT('Ctrl Pts',(-10.3347080960001,15.2,-1.33491244600001));
#263559=CARTESIAN_POINT('Ctrl Pts',(-10.3347080960001,11.6,-1.33491244600001));
#263560=CARTESIAN_POINT('Ctrl Pts',(-10.3334327990001,15.2,-1.33490999100002));
#263561=CARTESIAN_POINT('Ctrl Pts',(-10.3334327990001,11.6,-1.33490999100002));
#263562=CARTESIAN_POINT('Ctrl Pts',(-10.3321661480001,15.2,-1.33490632400001));
#263563=CARTESIAN_POINT('Ctrl Pts',(-10.3321661480001,11.6,-1.33490632400001));
#263564=CARTESIAN_POINT('Ctrl Pts',(-10.3309081640001,15.2,-1.33490146000002));
#263565=CARTESIAN_POINT('Ctrl Pts',(-10.3309081640001,11.6,-1.33490146000002));
#263566=CARTESIAN_POINT('Ctrl Pts',(-10.3296588710001,15.2,-1.33489541500001));
#263567=CARTESIAN_POINT('Ctrl Pts',(-10.3296588710001,11.6,-1.33489541500001));
#263568=CARTESIAN_POINT('Ctrl Pts',(-10.3284182910001,15.2,-1.33488820600002));
#263569=CARTESIAN_POINT('Ctrl Pts',(-10.3284182910001,11.6,-1.33488820600002));
#263570=CARTESIAN_POINT('Ctrl Pts',(-10.3271864460001,15.2,-1.33487984800002));
#263571=CARTESIAN_POINT('Ctrl Pts',(-10.3271864460001,11.6,-1.33487984800002));
#263572=CARTESIAN_POINT('Ctrl Pts',(-10.3259633610001,15.2,-1.33487035800002));
#263573=CARTESIAN_POINT('Ctrl Pts',(-10.3259633610001,11.6,-1.33487035800002));
#263574=CARTESIAN_POINT('Ctrl Pts',(-10.3247490570001,15.2,-1.33485975200001));
#263575=CARTESIAN_POINT('Ctrl Pts',(-10.3247490570001,11.6,-1.33485975200002));
#263576=CARTESIAN_POINT('Ctrl Pts',(-10.3235435580001,15.2,-1.33484804600001));
#263577=CARTESIAN_POINT('Ctrl Pts',(-10.3235435580001,11.6,-1.33484804600001));
#263578=CARTESIAN_POINT('Ctrl Pts',(-10.3223468860001,15.2,-1.33483525700001));
#263579=CARTESIAN_POINT('Ctrl Pts',(-10.3223468860001,11.6,-1.33483525700001));
#263580=CARTESIAN_POINT('Ctrl Pts',(-10.3211590660001,15.2,-1.33482140000002));
#263581=CARTESIAN_POINT('Ctrl Pts',(-10.3211590660001,11.6,-1.33482140000002));
#263582=CARTESIAN_POINT('Ctrl Pts',(-10.3199801190001,15.2,-1.33480649300001));
#263583=CARTESIAN_POINT('Ctrl Pts',(-10.3199801190001,11.6,-1.33480649300001));
#263584=CARTESIAN_POINT('Ctrl Pts',(-10.3188100710001,15.2,-1.33479055200001));
#263585=CARTESIAN_POINT('Ctrl Pts',(-10.3188100710001,11.6,-1.33479055200001));
#263586=CARTESIAN_POINT('Ctrl Pts',(-10.3176489430001,15.2,-1.33477359400001));
#263587=CARTESIAN_POINT('Ctrl Pts',(-10.3176489430001,11.6,-1.33477359400001));
#263588=CARTESIAN_POINT('Ctrl Pts',(-10.3164967600001,15.2,-1.33475563600001));
#263589=CARTESIAN_POINT('Ctrl Pts',(-10.3164967600001,11.6,-1.33475563600001));
#263590=CARTESIAN_POINT('Ctrl Pts',(-10.3153535460001,15.2,-1.33473669500002));
#263591=CARTESIAN_POINT('Ctrl Pts',(-10.3153535460001,11.6,-1.33473669500002));
#263592=CARTESIAN_POINT('Ctrl Pts',(-10.3142193240001,15.2,-1.33471678800001));
#263593=CARTESIAN_POINT('Ctrl Pts',(-10.3142193240001,11.6,-1.33471678800001));
#263594=CARTESIAN_POINT('Ctrl Pts',(-10.3130941180001,15.2,-1.33469593100001));
#263595=CARTESIAN_POINT('Ctrl Pts',(-10.3130941180001,11.6,-1.33469593100001));
#263596=CARTESIAN_POINT('Ctrl Pts',(-10.3119779530001,15.2,-1.33467414100001));
#263597=CARTESIAN_POINT('Ctrl Pts',(-10.3119779530001,11.6,-1.33467414100001));
#263598=CARTESIAN_POINT('Ctrl Pts',(-10.3108708510001,15.2,-1.33465143800001));
#263599=CARTESIAN_POINT('Ctrl Pts',(-10.3108708510001,11.6,-1.33465143800001));
#263600=CARTESIAN_POINT('Ctrl Pts',(-10.3097728380001,15.2,-1.33462783700002));
#263601=CARTESIAN_POINT('Ctrl Pts',(-10.3097728380001,11.6,-1.33462783700002));
#263602=CARTESIAN_POINT('Ctrl Pts',(-10.3086839380001,15.2,-1.33460335600001));
#263603=CARTESIAN_POINT('Ctrl Pts',(-10.3086839380001,11.6,-1.33460335600002));
#263604=CARTESIAN_POINT('Ctrl Pts',(-10.3076041750001,15.2,-1.33457801300001));
#263605=CARTESIAN_POINT('Ctrl Pts',(-10.3076041750001,11.6,-1.33457801300001));
#263606=CARTESIAN_POINT('Ctrl Pts',(-10.3065335750001,15.2,-1.33455182600001));
#263607=CARTESIAN_POINT('Ctrl Pts',(-10.3065335750001,11.6,-1.33455182600001));
#263608=CARTESIAN_POINT('Ctrl Pts',(-10.3054721600001,15.2,-1.33452481200001));
#263609=CARTESIAN_POINT('Ctrl Pts',(-10.3054721600001,11.6,-1.33452481200001));
#263610=CARTESIAN_POINT('Ctrl Pts',(-10.3044199570001,15.2,-1.33449698800002));
#263611=CARTESIAN_POINT('Ctrl Pts',(-10.3044199570001,11.6,-1.33449698800002));
#263612=CARTESIAN_POINT('Ctrl Pts',(-10.3033769900001,15.2,-1.33446837400002));
#263613=CARTESIAN_POINT('Ctrl Pts',(-10.3033769900001,11.6,-1.33446837400002));
#263614=CARTESIAN_POINT('Ctrl Pts',(-10.3023432850001,15.2,-1.33443898600001));
#263615=CARTESIAN_POINT('Ctrl Pts',(-10.3023432850001,11.6,-1.33443898600001));
#263616=CARTESIAN_POINT('Ctrl Pts',(-10.3013188650001,15.2,-1.33440884400001));
#263617=CARTESIAN_POINT('Ctrl Pts',(-10.3013188650001,11.6,-1.33440884400002));
#263618=CARTESIAN_POINT('Ctrl Pts',(-10.3003037570001,15.2,-1.33437796600001));
#263619=CARTESIAN_POINT('Ctrl Pts',(-10.3003037570001,11.6,-1.33437796600001));
#263620=CARTESIAN_POINT('Ctrl Pts',(-10.2992979850001,15.2,-1.33434636800001));
#263621=CARTESIAN_POINT('Ctrl Pts',(-10.2992979850001,11.6,-1.33434636800001));
#263622=CARTESIAN_POINT('Ctrl Pts',(-10.2983015770001,15.2,-1.33431407100002));
#263623=CARTESIAN_POINT('Ctrl Pts',(-10.2983015770001,11.6,-1.33431407100002));
#263624=CARTESIAN_POINT('Ctrl Pts',(-10.2973145550001,15.2,-1.33428109300001));
#263625=CARTESIAN_POINT('Ctrl Pts',(-10.2973145550001,11.6,-1.33428109300001));
#263626=CARTESIAN_POINT('Ctrl Pts',(-10.2963369470001,15.2,-1.33424745200001));
#263627=CARTESIAN_POINT('Ctrl Pts',(-10.2963369470001,11.6,-1.33424745200002));
#263628=CARTESIAN_POINT('Ctrl Pts',(-10.2953687780001,15.2,-1.33421316700002));
#263629=CARTESIAN_POINT('Ctrl Pts',(-10.2953687780001,11.6,-1.33421316700002));
#263630=CARTESIAN_POINT('Ctrl Pts',(-10.2944100750001,15.2,-1.33417825800001));
#263631=CARTESIAN_POINT('Ctrl Pts',(-10.2944100750001,11.6,-1.33417825800001));
#263632=CARTESIAN_POINT('Ctrl Pts',(-10.2934608630001,15.2,-1.33414274200002));
#263633=CARTESIAN_POINT('Ctrl Pts',(-10.2934608630001,11.6,-1.33414274200002));
#263634=CARTESIAN_POINT('Ctrl Pts',(-10.2925211680001,15.2,-1.33410664000001));
#263635=CARTESIAN_POINT('Ctrl Pts',(-10.2925211680001,11.6,-1.33410664000001));
#263636=CARTESIAN_POINT('Ctrl Pts',(-10.2915910170001,15.2,-1.33406997000002));
#263637=CARTESIAN_POINT('Ctrl Pts',(-10.2915910170001,11.6,-1.33406997000002));
#263638=CARTESIAN_POINT('Ctrl Pts',(-10.2906757380001,15.2,-1.33403296500001));
#263639=CARTESIAN_POINT('Ctrl Pts',(-10.2906757380001,11.6,-1.33403296500001));
#263640=CARTESIAN_POINT('Ctrl Pts',(-10.2899521420001,15.2,-1.33400298800002));
#263641=CARTESIAN_POINT('Ctrl Pts',(-10.2899521420001,11.6,-1.33400298800002));
#263642=CARTESIAN_POINT('Ctrl Pts',(-10.2894150050001,15.2,-1.33398033400002));
#263643=CARTESIAN_POINT('Ctrl Pts',(-10.2894150050001,11.6,-1.33398033400002));
#263644=CARTESIAN_POINT('Ctrl Pts',(-10.2890605210001,15.2,-1.33396520700002));
#263645=CARTESIAN_POINT('Ctrl Pts',(-10.2890605210001,11.6,-1.33396520700002));
#263646=CARTESIAN_POINT('Ctrl Pts',(-10.2888863240001,15.2,-1.33395773200002));
#263647=CARTESIAN_POINT('Ctrl Pts',(-10.2888863240001,11.6,-1.33395773200002));
#263648=CARTESIAN_POINT('',(-10.2888863233592,12.2,-1.33395773200336));
#263649=CARTESIAN_POINT('',(-10.2888863233592,15.2,-1.33395773200336));
#263650=CARTESIAN_POINT('',(-10.2888863230001,12.2,-1.33395773200002));
#263651=CARTESIAN_POINT('Ctrl Pts',(-11.4479048650001,12.2,-1.09337742900002));
#263652=CARTESIAN_POINT('Ctrl Pts',(-11.4443249343497,12.2,-1.09471863924366));
#263653=CARTESIAN_POINT('Ctrl Pts',(-11.4407496848669,12.2,-1.0960534771315));
#263654=CARTESIAN_POINT('Ctrl Pts',(-11.437179116671,12.2,-1.09738195555992));
#263655=CARTESIAN_POINT('Ctrl Pts',(-11.4336085484751,12.2,-1.09871043398834));
#263656=CARTESIAN_POINT('Ctrl Pts',(-11.4300426619881,12.2,-1.10003254737677));
#263657=CARTESIAN_POINT('Ctrl Pts',(-11.4264814749807,12.2,-1.10134830302043));
#263658=CARTESIAN_POINT('Ctrl Pts',(-11.4217332252062,12.2,-1.103102644038));
#263659=CARTESIAN_POINT('Ctrl Pts',(-11.4169933281401,12.2,-1.10484567960066));
#263660=CARTESIAN_POINT('Ctrl Pts',(-11.412261887605,12.2,-1.10657744341652));
#263661=CARTESIAN_POINT('Ctrl Pts',(-11.408713307526,12.2,-1.10787626616044));
#263662=CARTESIAN_POINT('Ctrl Pts',(-11.4051694849548,12.2,-1.10916875001346));
#263663=CARTESIAN_POINT('Ctrl Pts',(-11.40163046525,12.2,-1.1104549087584));
#263664=CARTESIAN_POINT('Ctrl Pts',(-11.3980914455453,12.2,-1.11174106750334));
#263665=CARTESIAN_POINT('Ctrl Pts',(-11.394557227657,12.2,-1.1130209015902));
#263666=CARTESIAN_POINT('Ctrl Pts',(-11.3910278474098,12.2,-1.11429442183614));
#263667=CARTESIAN_POINT('Ctrl Pts',(-11.3874984671626,12.2,-1.11556794208209));
#263668=CARTESIAN_POINT('Ctrl Pts',(-11.3839739234629,12.2,-1.11683514947146));
#263669=CARTESIAN_POINT('Ctrl Pts',(-11.3804542531644,12.2,-1.11809605573938));
#263670=CARTESIAN_POINT('Ctrl Pts',(-11.3769345828659,12.2,-1.11935696200729));
#263671=CARTESIAN_POINT('Ctrl Pts',(-11.373419786855,12.2,-1.12061156748908));
#263672=CARTESIAN_POINT('Ctrl Pts',(-11.3699099047735,12.2,-1.12185988473625));
#263673=CARTESIAN_POINT('Ctrl Pts',(-11.3664000220544,12.2,-1.1231082022102));
#263674=CARTESIAN_POINT('Ctrl Pts',(-11.3628950544283,12.2,-1.12435023280738));
#263675=CARTESIAN_POINT('Ctrl Pts',(-11.3593950397537,12.2,-1.12558598931945));
#263676=CARTESIAN_POINT('Ctrl Pts',(-11.3558950257149,12.2,-1.12682174560702));
#263677=CARTESIAN_POINT('Ctrl Pts',(-11.3523999670258,12.2,-1.12805122906161));
#263678=CARTESIAN_POINT('Ctrl Pts',(-11.348909900403,12.2,-1.12927445084995));
#263679=CARTESIAN_POINT('Ctrl Pts',(-11.3454198337803,12.2,-1.13049767263829));
#263680=CARTESIAN_POINT('Ctrl Pts',(-11.3419347591362,12.2,-1.13171463440634));
#263681=CARTESIAN_POINT('Ctrl Pts',(-11.3384547169552,12.2,-1.13292534953449));
#263682=CARTESIAN_POINT('Ctrl Pts',(-11.3349746747742,12.2,-1.13413606466264));
#263683=CARTESIAN_POINT('Ctrl Pts',(-11.3314996639429,12.2,-1.13534053188703));
#263684=CARTESIAN_POINT('Ctrl Pts',(-11.3280297252615,12.2,-1.13653876701564));
#263685=CARTESIAN_POINT('Ctrl Pts',(-11.3245597865801,12.2,-1.13773700214424));
#263686=CARTESIAN_POINT('Ctrl Pts',(-11.321094919502,12.2,-1.13892900289658));
#263687=CARTESIAN_POINT('Ctrl Pts',(-11.3176351643772,12.2,-1.14011478560404));
#263688=CARTESIAN_POINT('Ctrl Pts',(-11.3141754092525,12.2,-1.1413005683115));
#263689=CARTESIAN_POINT('Ctrl Pts',(-11.3107207663774,12.2,-1.14248013275271));
#263690=CARTESIAN_POINT('Ctrl Pts',(-11.307271274252,12.2,-1.14365349150259));
#263691=CARTESIAN_POINT('Ctrl Pts',(-11.3038217815,12.2,-1.14482685046563));
#263692=CARTESIAN_POINT('Ctrl Pts',(-11.3003774400327,12.2,-1.14599400426859));
#263693=CARTESIAN_POINT('Ctrl Pts',(-11.2969382902836,12.2,-1.14715496772814));
#263694=CARTESIAN_POINT('Ctrl Pts',(-11.2923527583261,12.2,-1.14870291865603));
#263695=CARTESIAN_POINT('Ctrl Pts',(-11.2877764550117,12.2,-1.15023986500291));
#263696=CARTESIAN_POINT('Ctrl Pts',(-11.2832094782531,12.2,-1.15176583927402));
#263697=CARTESIAN_POINT('Ctrl Pts',(-11.2797842455287,12.2,-1.15291032002932));
#263698=CARTESIAN_POINT('Ctrl Pts',(-11.2763642569487,12.2,-1.15404862993381));
#263699=CARTESIAN_POINT('Ctrl Pts',(-11.2729495548223,12.2,-1.15518078364322));
#263700=CARTESIAN_POINT('Ctrl Pts',(-11.2683966182402,12.2,-1.15669032205955));
#263701=CARTESIAN_POINT('Ctrl Pts',(-11.2638530796593,12.2,-1.15818891457732));
#263702=CARTESIAN_POINT('Ctrl Pts',(-11.2593190344128,12.2,-1.15967659837991));
#263703=CARTESIAN_POINT('Ctrl Pts',(-11.2559185007868,12.2,-1.1607923611305));
#263704=CARTESIAN_POINT('Ctrl Pts',(-11.2525233065935,12.2,-1.16190198792349));
#263705=CARTESIAN_POINT('Ctrl Pts',(-11.249133494425,12.2,-1.16300549275839));
#263706=CARTESIAN_POINT('Ctrl Pts',(-11.2457436822565,12.2,-1.1641089975933));
#263707=CARTESIAN_POINT('Ctrl Pts',(-11.2423592509961,12.2,-1.16520638198679));
#263708=CARTESIAN_POINT('Ctrl Pts',(-11.2389802419101,12.2,-1.16629765936434));
#263709=CARTESIAN_POINT('Ctrl Pts',(-11.235601232824,12.2,-1.16738893674189));
#263710=CARTESIAN_POINT('Ctrl Pts',(-11.2322276473649,12.2,-1.16847410962581));
#263711=CARTESIAN_POINT('Ctrl Pts',(-11.2288595241517,12.2,-1.16955319055789));
#263712=CARTESIAN_POINT('Ctrl Pts',(-11.2254914009385,12.2,-1.17063227148996));
#263713=CARTESIAN_POINT('Ctrl Pts',(-11.2221287413606,12.2,-1.1717052624554));
#263714=CARTESIAN_POINT('Ctrl Pts',(-11.2187715872319,12.2,-1.17277217870913));
#263715=CARTESIAN_POINT('Ctrl Pts',(-11.2154144324932,12.2,-1.17383909515668));
#263716=CARTESIAN_POINT('Ctrl Pts',(-11.2120627828228,12.2,-1.17489993637752));
#263717=CARTESIAN_POINT('Ctrl Pts',(-11.2087166805456,12.2,-1.17595471969666));
#263718=CARTESIAN_POINT('Ctrl Pts',(-11.2053705788762,12.2,-1.17700950282418));
#263719=CARTESIAN_POINT('Ctrl Pts',(-11.2020300232649,12.2,-1.17805822645202));
#263720=CARTESIAN_POINT('Ctrl Pts',(-11.1986950571366,12.2,-1.17910090766361));
#263721=CARTESIAN_POINT('Ctrl Pts',(-11.1942484358341,12.2,-1.18049114921591));
#263722=CARTESIAN_POINT('Ctrl Pts',(-11.1898117494387,12.2,-1.18187064734396));
#263723=CARTESIAN_POINT('Ctrl Pts',(-11.1853850986341,12.2,-1.18323944230138));
#263724=CARTESIAN_POINT('Ctrl Pts',(-11.1820651103798,12.2,-1.18426603856607));
#263725=CARTESIAN_POINT('Ctrl Pts',(-11.1787507677519,12.2,-1.18528661304825));
#263726=CARTESIAN_POINT('Ctrl Pts',(-11.1754421117046,12.2,-1.18630118426221));
#263727=CARTESIAN_POINT('Ctrl Pts',(-11.1721334550563,12.2,-1.18731575566048));
#263728=CARTESIAN_POINT('Ctrl Pts',(-11.1688304862763,12.2,-1.18832432270706));
#263729=CARTESIAN_POINT('Ctrl Pts',(-11.1655332470479,12.2,-1.18932690122695));
#263730=CARTESIAN_POINT('Ctrl Pts',(-11.1622360084185,12.2,-1.1903294795647));
#263731=CARTESIAN_POINT('Ctrl Pts',(-11.1589444987887,12.2,-1.19132607134445));
#263732=CARTESIAN_POINT('Ctrl Pts',(-11.1556587626586,12.2,-1.19231669164127));
#263733=CARTESIAN_POINT('Ctrl Pts',(-11.1523730265285,12.2,-1.19330731193808));
#263734=CARTESIAN_POINT('Ctrl Pts',(-11.1490930630929,12.2,-1.19429196094875));
#263735=CARTESIAN_POINT('Ctrl Pts',(-11.1458189150304,12.2,-1.19527065675094));
#263736=CARTESIAN_POINT('Ctrl Pts',(-11.1425447669678,12.2,-1.19624935255314));
#263737=CARTESIAN_POINT('Ctrl Pts',(-11.1392764345159,12.2,-1.19722209469656));
#263738=CARTESIAN_POINT('Ctrl Pts',(-11.1360139604947,12.2,-1.19818890095751));
#263739=CARTESIAN_POINT('Ctrl Pts',(-11.1327514864734,12.2,-1.19915570721846));
#263740=CARTESIAN_POINT('Ctrl Pts',(-11.1294948719202,12.2,-1.20011657683005));
#263741=CARTESIAN_POINT('Ctrl Pts',(-11.1262441588711,12.2,-1.2010715276292));
#263742=CARTESIAN_POINT('Ctrl Pts',(-11.122993445822,12.2,-1.20202647842836));
#263743=CARTESIAN_POINT('Ctrl Pts',(-11.1197486347892,12.2,-1.20297551131124));
#263744=CARTESIAN_POINT('Ctrl Pts',(-11.1165097696978,12.2,-1.20391864306945));
#263745=CARTESIAN_POINT('Ctrl Pts',(-11.1132709040179,12.2,-1.20486177499899));
#263746=CARTESIAN_POINT('Ctrl Pts',(-11.1100379834481,12.2,-1.20579900555186));
#263747=CARTESIAN_POINT('Ctrl Pts',(-11.1068110527716,12.2,-1.20673035347808));
#263748=CARTESIAN_POINT('Ctrl Pts',(-11.1025084795132,12.2,-1.20797215043106));
#263749=CARTESIAN_POINT('Ctrl Pts',(-11.0982165538419,12.2,-1.20920348836568));
#263750=CARTESIAN_POINT('Ctrl Pts',(-11.0939353812279,12.2,-1.21042441071589));
#263751=CARTESIAN_POINT('Ctrl Pts',(-11.088583915023,12.2,-1.21195056377841));
#263752=CARTESIAN_POINT('Ctrl Pts',(-11.0832492483889,12.2,-1.21346044241117));
#263753=CARTESIAN_POINT('Ctrl Pts',(-11.0779315880417,12.2,-1.21495413296672));
#263754=CARTESIAN_POINT('Ctrl Pts',(-11.0736774595321,12.2,-1.21614908547629));
#263755=CARTESIAN_POINT('Ctrl Pts',(-11.0694342144598,12.2,-1.21733367755132));
#263756=CARTESIAN_POINT('Ctrl Pts',(-11.0652019593414,12.2,-1.21850795339204));
#263757=CARTESIAN_POINT('Ctrl Pts',(-11.0599116413083,12.2,-1.21997579795295));
#263758=CARTESIAN_POINT('Ctrl Pts',(-11.0546384945827,12.2,-1.22142752522855));
#263759=CARTESIAN_POINT('Ctrl Pts',(-11.0493827274458,12.2,-1.22286322083726));
#263760=CARTESIAN_POINT('Ctrl Pts',(-11.0441269597361,12.2,-1.22429891660247));
#263761=CARTESIAN_POINT('Ctrl Pts',(-11.0388885726677,12.2,-1.2257185834207));
#263762=CARTESIAN_POINT('Ctrl Pts',(-11.0336677749579,12.2,-1.22712231078311));
#263763=CARTESIAN_POINT('Ctrl Pts',(-11.0294911365625,12.2,-1.22824529273425));
#263764=CARTESIAN_POINT('Ctrl Pts',(-11.0253257576841,12.2,-1.22935807418019));
#263765=CARTESIAN_POINT('Ctrl Pts',(-11.0211717432722,12.2,-1.2304607008008));
#263766=CARTESIAN_POINT('Ctrl Pts',(-11.0170177294263,12.2,-1.23156332727119));
#263767=CARTESIAN_POINT('Ctrl Pts',(-11.0128750814806,12.2,-1.2326558012522));
#263768=CARTESIAN_POINT('Ctrl Pts',(-11.0087439096505,12.2,-1.23373816833142));
#263769=CARTESIAN_POINT('Ctrl Pts',(-11.0046127372575,12.2,-1.23482053555811));
#263770=CARTESIAN_POINT('Ctrl Pts',(-11.0004930399656,12.2,-1.23589279728661));
#263771=CARTESIAN_POINT('Ctrl Pts',(-10.9963849282417,12.2,-1.23695500123339));
#263772=CARTESIAN_POINT('Ctrl Pts',(-10.9922768165178,12.2,-1.23801720518017));
#263773=CARTESIAN_POINT('Ctrl Pts',(-10.9881802906091,12.2,-1.239069351923));
#263774=CARTESIAN_POINT('Ctrl Pts',(-10.9840954608322,12.2,-1.24011149114544));
#263775=CARTESIAN_POINT('Ctrl Pts',(-10.9800106316117,12.2,-1.24115363022589));
#263776=CARTESIAN_POINT('Ctrl Pts',(-10.9759374985198,12.2,-1.24218576152546));
#263777=CARTESIAN_POINT('Ctrl Pts',(-10.9718761727778,12.2,-1.24320793472435));
#263778=CARTESIAN_POINT('Ctrl Pts',(-10.9667995151852,12.2,-1.24448565132742));
#263779=CARTESIAN_POINT('Ctrl Pts',(-10.9617413080111,12.2,-1.24574781044451));
#263780=CARTESIAN_POINT('Ctrl Pts',(-10.9567017702333,12.2,-1.24699450870839));
#263781=CARTESIAN_POINT('Ctrl Pts',(-10.9526701397914,12.2,-1.24799186737385));
#263782=CARTESIAN_POINT('Ctrl Pts',(-10.9486504570425,12.2,-1.24897933325762));
#263783=CARTESIAN_POINT('Ctrl Pts',(-10.9446428361031,12.2,-1.24995695664322));
#263784=CARTESIAN_POINT('Ctrl Pts',(-10.9396333107479,12.2,-1.25117898567543));
#263785=CARTESIAN_POINT('Ctrl Pts',(-10.9346426326377,12.2,-1.25238563818949));
#263786=CARTESIAN_POINT('Ctrl Pts',(-10.9296710231086,12.2,-1.25357701535255));
#263787=CARTESIAN_POINT('Ctrl Pts',(-10.925693734835,12.2,-1.25453011723883));
#263788=CARTESIAN_POINT('Ctrl Pts',(-10.9217286520404,12.2,-1.25547344291028));
#263789=CARTESIAN_POINT('Ctrl Pts',(-10.9177758889917,12.2,-1.25640704751672));
#263790=CARTESIAN_POINT('Ctrl Pts',(-10.9138231259429,12.2,-1.25734065212316));
#263791=CARTESIAN_POINT('Ctrl Pts',(-10.9098826819928,12.2,-1.25826453445901));
#263792=CARTESIAN_POINT('Ctrl Pts',(-10.9059546748911,12.2,-1.25917874967452));
#263793=CARTESIAN_POINT('Ctrl Pts',(-10.9020266683246,12.2,-1.26009296476547));
#263794=CARTESIAN_POINT('Ctrl Pts',(-10.898111096651,12.2,-1.26099751315211));
#263795=CARTESIAN_POINT('Ctrl Pts',(-10.8942080783025,12.2,-1.26189244913513));
#263796=CARTESIAN_POINT('Ctrl Pts',(-10.8903050594223,12.2,-1.26278738524009));
#263797=CARTESIAN_POINT('Ctrl Pts',(-10.8864145947664,12.2,-1.26367271006421));
#263798=CARTESIAN_POINT('Ctrl Pts',(-10.8825368001957,12.2,-1.26454847937708));
#263799=CARTESIAN_POINT('Ctrl Pts',(-10.8786590061534,12.2,-1.26542424857063));
#263800=CARTESIAN_POINT('Ctrl Pts',(-10.8747938822815,12.2,-1.2662904627799));
#263801=CARTESIAN_POINT('Ctrl Pts',(-10.8709415485401,12.2,-1.26714717865493));
#263802=CARTESIAN_POINT('Ctrl Pts',(-10.8670892142737,12.2,-1.26800389464668));
#263803=CARTESIAN_POINT('Ctrl Pts',(-10.8632496704783,12.2,-1.2688511120873));
#263804=CARTESIAN_POINT('Ctrl Pts',(-10.8594230349373,12.2,-1.26968889007678));
#263805=CARTESIAN_POINT('Ctrl Pts',(-10.8555963999176,12.2,-1.27052666795213));
#263806=CARTESIAN_POINT('Ctrl Pts',(-10.8517826746097,12.2,-1.27135500690361));
#263807=CARTESIAN_POINT('Ctrl Pts',(-10.8479819792849,12.2,-1.27217396415616));
#263808=CARTESIAN_POINT('Ctrl Pts',(-10.8441812834423,12.2,-1.2729929215203));
#263809=CARTESIAN_POINT('Ctrl Pts',(-10.8403936177742,12.2,-1.27380249638349));
#263810=CARTESIAN_POINT('Ctrl Pts',(-10.8366191034582,12.2,-1.27460275231538));
#263811=CARTESIAN_POINT('Ctrl Pts',(-10.8319009608204,12.2,-1.27560307217574));
#263812=CARTESIAN_POINT('Ctrl Pts',(-10.8272033671876,12.2,-1.27658882671425));
#263813=CARTESIAN_POINT('Ctrl Pts',(-10.8225265629526,12.2,-1.27756013754682));
#263814=CARTESIAN_POINT('Ctrl Pts',(-10.8187851198705,12.2,-1.27833718614936));
#263815=CARTESIAN_POINT('Ctrl Pts',(-10.8150569816388,12.2,-1.27910498915213));
#263816=CARTESIAN_POINT('Ctrl Pts',(-10.8113422717558,12.2,-1.27986361090659));
#263817=CARTESIAN_POINT('Ctrl Pts',(-10.8066988840224,12.2,-1.28081188817718));
#263818=CARTESIAN_POINT('Ctrl Pts',(-10.8020764792133,12.2,-1.28174581575018));
#263819=CARTESIAN_POINT('Ctrl Pts',(-10.7974753008094,12.2,-1.28266552068148));
#263820=CARTESIAN_POINT('Ctrl Pts',(-10.7937943578857,12.2,-1.28340128466662));
#263821=CARTESIAN_POINT('Ctrl Pts',(-10.7901269989969,12.2,-1.284127944484));
#263822=CARTESIAN_POINT('Ctrl Pts',(-10.7864733514098,12.2,-1.2848455658003));
#263823=CARTESIAN_POINT('Ctrl Pts',(-10.7828197043205,12.2,-1.28556318701882));
#263824=CARTESIAN_POINT('Ctrl Pts',(-10.7791797682761,12.2,-1.28627176866994));
#263825=CARTESIAN_POINT('Ctrl Pts',(-10.7755536710012,12.2,-1.28697137664848));
#263826=CARTESIAN_POINT('Ctrl Pts',(-10.7719275732324,12.2,-1.28767098472235));
#263827=CARTESIAN_POINT('Ctrl Pts',(-10.7683153117817,12.2,-1.28836161856912));
#263828=CARTESIAN_POINT('Ctrl Pts',(-10.7647170181976,12.2,-1.28904334527236));
#263829=CARTESIAN_POINT('Ctrl Pts',(-10.7611187251038,12.2,-1.28972507188272));
#263830=CARTESIAN_POINT('Ctrl Pts',(-10.7575343979572,12.2,-1.29039789158097));
#263831=CARTESIAN_POINT('Ctrl Pts',(-10.7539641668588,12.2,-1.29106187091648));
#263832=CARTESIAN_POINT('Ctrl Pts',(-10.7503939352738,12.2,-1.29172585034246));
#263833=CARTESIAN_POINT('Ctrl Pts',(-10.7468377988928,12.2,-1.29238098875958));
#263834=CARTESIAN_POINT('Ctrl Pts',(-10.7432958887393,12.2,-1.29302735674216));
#263835=CARTESIAN_POINT('Ctrl Pts',(-10.7397539790683,12.2,-1.29367372463666));
#263836=CARTESIAN_POINT('Ctrl Pts',(-10.7362262945692,12.2,-1.29431132008108));
#263837=CARTESIAN_POINT('Ctrl Pts',(-10.7327129687994,12.2,-1.29494021469722));
#263838=CARTESIAN_POINT('Ctrl Pts',(-10.7291996425509,12.2,-1.29556910939905));
#263839=CARTESIAN_POINT('Ctrl Pts',(-10.7257006740177,12.2,-1.29618930044728));
#263840=CARTESIAN_POINT('Ctrl Pts',(-10.7222161947167,12.2,-1.29680086175838));
#263841=CARTESIAN_POINT('Ctrl Pts',(-10.7187317154157,12.2,-1.29741242306949));
#263842=CARTESIAN_POINT('Ctrl Pts',(-10.7152617276219,12.2,-1.2980153522907));
#263843=CARTESIAN_POINT('Ctrl Pts',(-10.7118063634351,12.2,-1.29860972182222));
#263844=CARTESIAN_POINT('Ctrl Pts',(-10.708350999719,12.2,-1.29920409127276));
#263845=CARTESIAN_POINT('Ctrl Pts',(-10.7049102600267,12.2,-1.29978990219976));
#263846=CARTESIAN_POINT('Ctrl Pts',(-10.7014842797357,12.2,-1.30036722626632));
#263847=CARTESIAN_POINT('Ctrl Pts',(-10.6980582989778,12.2,-1.30094455041154));
#263848=CARTESIAN_POINT('Ctrl Pts',(-10.6946470775727,12.2,-1.30151338699532));
#263849=CARTESIAN_POINT('Ctrl Pts',(-10.6912507509447,12.2,-1.30207381235834));
#263850=CARTESIAN_POINT('Ctrl Pts',(-10.6878544247794,12.2,-1.302634237645));
#263851=CARTESIAN_POINT('Ctrl Pts',(-10.6844729949817,12.2,-1.30318624926609));
#263852=CARTESIAN_POINT('Ctrl Pts',(-10.6811065985337,12.2,-1.30372992522219));
#263853=CARTESIAN_POINT('Ctrl Pts',(-10.677740201627,12.2,-1.30427360125237));
#263854=CARTESIAN_POINT('Ctrl Pts',(-10.6743888370076,12.2,-1.30480893958603));
#263855=CARTESIAN_POINT('Ctrl Pts',(-10.671052644216,12.2,-1.30533601658482));
#263856=CARTESIAN_POINT('Ctrl Pts',(-10.6677164518789,12.2,-1.30586309351179));
#263857=CARTESIAN_POINT('Ctrl Pts',(-10.6643954315011,12.2,-1.30638191048555));
#263858=CARTESIAN_POINT('Ctrl Pts',(-10.6610897237704,12.2,-1.30689254516656));
#263859=CARTESIAN_POINT('Ctrl Pts',(-10.6569575887691,12.2,-1.30753083857));
#263860=CARTESIAN_POINT('Ctrl Pts',(-10.6528493770518,12.2,-1.30815634585368));
#263861=CARTESIAN_POINT('Ctrl Pts',(-10.6487653687172,12.2,-1.30876922120156));
#263862=CARTESIAN_POINT('Ctrl Pts',(-10.6446813603826,12.2,-1.30938209654944));
#263863=CARTESIAN_POINT('Ctrl Pts',(-10.6406215523928,12.2,-1.3099823409248));
#263864=CARTESIAN_POINT('Ctrl Pts',(-10.6365862259855,12.2,-1.31057011273306));
#263865=CARTESIAN_POINT('Ctrl Pts',(-10.6325508995783,12.2,-1.31115788454132));
#263866=CARTESIAN_POINT('Ctrl Pts',(-10.6285400548445,12.2,-1.31173318297227));
#263867=CARTESIAN_POINT('Ctrl Pts',(-10.6245539749833,12.2,-1.31229616825005));
#263868=CARTESIAN_POINT('Ctrl Pts',(-10.6205678951222,12.2,-1.31285915352783));
#263869=CARTESIAN_POINT('Ctrl Pts',(-10.6166065801222,12.2,-1.31340982704449));
#263870=CARTESIAN_POINT('Ctrl Pts',(-10.6126703162333,12.2,-1.31394835301671));
#263871=CARTESIAN_POINT('Ctrl Pts',(-10.6087340523445,12.2,-1.31448687898893));
#263872=CARTESIAN_POINT('Ctrl Pts',(-10.6048228402266,12.2,-1.31501325585358));
#263873=CARTESIAN_POINT('Ctrl Pts',(-10.6009369697229,12.2,-1.31552765280032));
#263874=CARTESIAN_POINT('Ctrl Pts',(-10.5970510992192,12.2,-1.31604204974707));
#263875=CARTESIAN_POINT('Ctrl Pts',(-10.5931905711424,12.2,-1.3165444671549));
#263876=CARTESIAN_POINT('Ctrl Pts',(-10.589355678991,12.2,-1.31703507430706));
#263877=CARTESIAN_POINT('Ctrl Pts',(-10.5847538085765,12.2,-1.31762380286826));
#263878=CARTESIAN_POINT('Ctrl Pts',(-10.5801888532424,12.2,-1.31819552758083));
#263879=CARTESIAN_POINT('Ctrl Pts',(-10.5756613289886,12.2,-1.31875054897806));
#263880=CARTESIAN_POINT('Ctrl Pts',(-10.5711338047347,12.2,-1.31930557037529));
#263881=CARTESIAN_POINT('Ctrl Pts',(-10.5666437116344,12.2,-1.31984388876933));
#263882=CARTESIAN_POINT('Ctrl Pts',(-10.5621915732103,12.2,-1.32036581516815));
#263883=CARTESIAN_POINT('Ctrl Pts',(-10.5569974114458,12.2,-1.32097472933171));
#263884=CARTESIAN_POINT('Ctrl Pts',(-10.551854911308,12.2,-1.32156133035842));
#263885=CARTESIAN_POINT('Ctrl Pts',(-10.5467649145046,12.2,-1.32212612692359));
#263886=CARTESIAN_POINT('Ctrl Pts',(-10.5431292025587,12.2,-1.32252955303529));
#263887=CARTESIAN_POINT('Ctrl Pts',(-10.5395202811572,12.2,-1.32292185247585));
#263888=CARTESIAN_POINT('Ctrl Pts',(-10.5359384607936,12.2,-1.3233032169915));
#263889=CARTESIAN_POINT('Ctrl Pts',(-10.5309239122065,12.2,-1.32383712732172));
#263890=CARTESIAN_POINT('Ctrl Pts',(-10.5259624852953,12.2,-1.32434960229385));
#263891=CARTESIAN_POINT('Ctrl Pts',(-10.5210550497626,12.2,-1.32484117448127));
#263892=CARTESIAN_POINT('Ctrl Pts',(-10.5175497387223,12.2,-1.32519229746683));
#263893=CARTESIAN_POINT('Ctrl Pts',(-10.5140719783145,12.2,-1.32553275599477));
#263894=CARTESIAN_POINT('Ctrl Pts',(-10.5106220878663,12.2,-1.32586274982998));
#263895=CARTESIAN_POINT('Ctrl Pts',(-10.5071721974181,12.2,-1.32619274366518));
#263896=CARTESIAN_POINT('Ctrl Pts',(-10.5037501797926,12.2,-1.32651227168577));
#263897=CARTESIAN_POINT('Ctrl Pts',(-10.5003563627811,12.2,-1.32682153807382));
#263898=CARTESIAN_POINT('Ctrl Pts',(-10.4969625457695,12.2,-1.32713080446187));
#263899=CARTESIAN_POINT('Ctrl Pts',(-10.4935969288001,12.2,-1.32742980916087));
#263900=CARTESIAN_POINT('Ctrl Pts',(-10.4902598467885,12.2,-1.32771875902116));
#263901=CARTESIAN_POINT('Ctrl Pts',(-10.4862553485201,12.2,-1.32806549884092));
#263902=CARTESIAN_POINT('Ctrl Pts',(-10.4822919381671,12.2,-1.32839776190449));
#263903=CARTESIAN_POINT('Ctrl Pts',(-10.4783702020614,12.2,-1.32871591547565));
#263904=CARTESIAN_POINT('Ctrl Pts',(-10.4744484659558,12.2,-1.32903406904681));
#263905=CARTESIAN_POINT('Ctrl Pts',(-10.4705684047967,12.2,-1.32933811107744));
#263906=CARTESIAN_POINT('Ctrl Pts',(-10.4667306136843,12.2,-1.32962842173416));
#263907=CARTESIAN_POINT('Ctrl Pts',(-10.4628928225719,12.2,-1.32991873239088));
#263908=CARTESIAN_POINT('Ctrl Pts',(-10.4590973010339,12.2,-1.330195309855));
#263909=CARTESIAN_POINT('Ctrl Pts',(-10.4553446579174,12.2,-1.33045854276301));
#263910=CARTESIAN_POINT('Ctrl Pts',(-10.4515920144599,12.2,-1.33072177569494));
#263911=CARTESIAN_POINT('Ctrl Pts',(-10.4478822474316,12.2,-1.33097166385054));
#263912=CARTESIAN_POINT('Ctrl Pts',(-10.444215977067,12.2,-1.33120860752956));
#263913=CARTESIAN_POINT('Ctrl Pts',(-10.4405497070355,12.2,-1.33144555118706));
#263914=CARTESIAN_POINT('Ctrl Pts',(-10.4369269315713,12.2,-1.33166954730663));
#263915=CARTESIAN_POINT('Ctrl Pts',(-10.4333482845183,12.2,-1.33188100629994));
#263916=CARTESIAN_POINT('Ctrl Pts',(-10.429173196073,12.2,-1.3321277084716));
#263917=CARTESIAN_POINT('Ctrl Pts',(-10.4250581674828,12.2,-1.33235734853502));
#263918=CARTESIAN_POINT('Ctrl Pts',(-10.4210042213525,12.2,-1.33257059080161));
#263919=CARTESIAN_POINT('Ctrl Pts',(-10.417529410564,12.2,-1.33275336987778));
#263920=CARTESIAN_POINT('Ctrl Pts',(-10.4140994778273,12.2,-1.33292410608833));
#263921=CARTESIAN_POINT('Ctrl Pts',(-10.4107150809348,12.2,-1.33308322924996));
#263922=CARTESIAN_POINT('Ctrl Pts',(-10.4073306840424,12.2,-1.33324235241159));
#263923=CARTESIAN_POINT('Ctrl Pts',(-10.4039918233424,12.2,-1.33338986613936));
#263924=CARTESIAN_POINT('Ctrl Pts',(-10.4006991696256,12.2,-1.3335262159685));
#263925=CARTESIAN_POINT('Ctrl Pts',(-10.3974065156096,12.2,-1.33366256581003));
#263926=CARTESIAN_POINT('Ctrl Pts',(-10.3941600695731,12.2,-1.33378775019212));
#263927=CARTESIAN_POINT('Ctrl Pts',(-10.3909605148175,12.2,-1.33390223044789));
#263928=CARTESIAN_POINT('Ctrl Pts',(-10.3877609603524,12.2,-1.33401671069327));
#263929=CARTESIAN_POINT('Ctrl Pts',(-10.3846082998028,12.2,-1.33412048741961));
#263930=CARTESIAN_POINT('Ctrl Pts',(-10.3815032322347,12.2,-1.33421403074999));
#263931=CARTESIAN_POINT('Ctrl Pts',(-10.3783981646667,12.2,-1.33430757408037));
#263932=CARTESIAN_POINT('Ctrl Pts',(-10.3753406896553,12.2,-1.33439088666069));
#263933=CARTESIAN_POINT('Ctrl Pts',(-10.3723315240947,12.2,-1.33446445299201));
#263934=CARTESIAN_POINT('Ctrl Pts',(-10.3688208307584,12.2,-1.33455028038301));
#263935=CARTESIAN_POINT('Ctrl Pts',(-10.3653758880138,12.2,-1.33462284149322));
#263936=CARTESIAN_POINT('Ctrl Pts',(-10.3619978645013,12.2,-1.33468293571667));
#263937=CARTESIAN_POINT('Ctrl Pts',(-10.358137266314,12.2,-1.33475161482719));
#263938=CARTESIAN_POINT('Ctrl Pts',(-10.3543640668174,12.2,-1.3348040075846));
#263939=CARTESIAN_POINT('Ctrl Pts',(-10.3506800556424,12.2,-1.33484134947347));
#263940=CARTESIAN_POINT('Ctrl Pts',(-10.347917047324,12.2,-1.33486935588948));
#263941=CARTESIAN_POINT('Ctrl Pts',(-10.3452042073052,12.2,-1.33488889724864));
#263942=CARTESIAN_POINT('Ctrl Pts',(-10.3425423128151,12.2,-1.33490051274876));
#263943=CARTESIAN_POINT('Ctrl Pts',(-10.3398804180833,12.2,-1.33491212824994));
#263944=CARTESIAN_POINT('Ctrl Pts',(-10.3372694660563,12.2,-1.33491581842531));
#263945=CARTESIAN_POINT('Ctrl Pts',(-10.3347102518357,12.2,-1.33491213900813));
#263946=CARTESIAN_POINT('Ctrl Pts',(-10.3321510378476,12.2,-1.33490845959128));
#263947=CARTESIAN_POINT('Ctrl Pts',(-10.3296435620565,12.2,-1.33489741024112));
#263948=CARTESIAN_POINT('Ctrl Pts',(-10.3271886359678,12.2,-1.3348795649917));
#263949=CARTESIAN_POINT('Ctrl Pts',(-10.3243245553822,12.2,-1.33485874553297));
#263950=CARTESIAN_POINT('Ctrl Pts',(-10.3215320018072,12.2,-1.33482867661023));
#263951=CARTESIAN_POINT('Ctrl Pts',(-10.3188123009065,12.2,-1.33479029774821));
#263952=CARTESIAN_POINT('Ctrl Pts',(-10.3160926002175,12.2,-1.33475191888917));
#263953=CARTESIAN_POINT('Ctrl Pts',(-10.3134457526233,12.2,-1.33470523165128));
#263954=CARTESIAN_POINT('Ctrl Pts',(-10.3108731234737,12.2,-1.33465121353007));
#263955=CARTESIAN_POINT('Ctrl Pts',(-10.3086680125165,12.2,-1.33460491227792));
#263956=CARTESIAN_POINT('Ctrl Pts',(-10.3065174318478,12.2,-1.33455322546687));
#263957=CARTESIAN_POINT('Ctrl Pts',(-10.3044222659027,12.2,-1.3344967904636));
#263958=CARTESIAN_POINT('Ctrl Pts',(-10.3023271001479,12.2,-1.33444035546544));
#263959=CARTESIAN_POINT('Ctrl Pts',(-10.3002873493213,12.2,-1.33437917274797));
#263960=CARTESIAN_POINT('Ctrl Pts',(-10.2983039235509,12.2,-1.33431390075005));
#263961=CARTESIAN_POINT('Ctrl Pts',(-10.2950077328095,12.2,-1.33420542734085));
#263962=CARTESIAN_POINT('Ctrl Pts',(-10.2918670873981,12.2,-1.33408564009489));
#263963=CARTESIAN_POINT('Ctrl Pts',(-10.2888863240001,12.2,-1.33395773200002));
#263964=CARTESIAN_POINT('Ctrl Pts',(-10.2888863240001,15.2,-1.33395773200002));
#263965=CARTESIAN_POINT('Ctrl Pts',(-10.2906713387415,15.2,-1.33403432910097));
#263966=CARTESIAN_POINT('Ctrl Pts',(-10.2925136934523,15.2,-1.33410802241805));
#263967=CARTESIAN_POINT('Ctrl Pts',(-10.2944124475503,15.2,-1.33417810627568));
#263968=CARTESIAN_POINT('Ctrl Pts',(-10.2963203584004,15.2,-1.3342485281131));
#263969=CARTESIAN_POINT('Ctrl Pts',(-10.2982852153479,15.2,-1.33431531312478));
#263970=CARTESIAN_POINT('Ctrl Pts',(-10.3003060912289,15.2,-1.33437778604772));
#263971=CARTESIAN_POINT('Ctrl Pts',(-10.3026637794814,15.2,-1.33445067111597));
#263972=CARTESIAN_POINT('Ctrl Pts',(-10.3050977134762,15.2,-1.33451768705885));
#263973=CARTESIAN_POINT('Ctrl Pts',(-10.3076064654823,15.2,-1.33457780198607));
#263974=CARTESIAN_POINT('Ctrl Pts',(-10.3097568245957,15.2,-1.33462932907256));
#263975=CARTESIAN_POINT('Ctrl Pts',(-10.3119621540712,15.2,-1.33467578925836));
#263976=CARTESIAN_POINT('Ctrl Pts',(-10.314221578227,15.2,-1.33471655051229));
#263977=CARTESIAN_POINT('Ctrl Pts',(-10.3168575727676,15.2,-1.33476410530298));
#263978=CARTESIAN_POINT('Ctrl Pts',(-10.319567196023,15.2,-1.33480390623188));
#263979=CARTESIAN_POINT('Ctrl Pts',(-10.3223490987067,15.2,-1.33483499002212));
#263980=CARTESIAN_POINT('Ctrl Pts',(-10.3247335869998,15.2,-1.334861633274));
#263981=CARTESIAN_POINT('Ctrl Pts',(-10.3271711798945,15.2,-1.33488187265031));
#263982=CARTESIAN_POINT('Ctrl Pts',(-10.329661049491,15.2,-1.33489512398462));
#263983=CARTESIAN_POINT('Ctrl Pts',(-10.3321509188613,15.2,-1.33490837531773));
#263984=CARTESIAN_POINT('Ctrl Pts',(-10.3346930649442,15.2,-1.33491463737498));
#263985=CARTESIAN_POINT('Ctrl Pts',(-10.3372866821833,15.2,-1.33491334179169));
#263986=CARTESIAN_POINT('Ctrl Pts',(-10.3398802994224,15.2,-1.33491204620841));
#263987=CARTESIAN_POINT('Ctrl Pts',(-10.3425253879222,15.2,-1.33490319475141));
#263988=CARTESIAN_POINT('Ctrl Pts',(-10.3452211602893,15.2,-1.33488623525165));
#263989=CARTESIAN_POINT('Ctrl Pts',(-10.3479169329013,15.2,-1.33486927575035));
#263990=CARTESIAN_POINT('Ctrl Pts',(-10.3506633886323,15.2,-1.33484420971545));
#263991=CARTESIAN_POINT('Ctrl Pts',(-10.3534597592881,15.2,-1.33481050221302));
#263992=CARTESIAN_POINT('Ctrl Pts',(-10.3562561296899,15.2,-1.33477679471366));
#263993=CARTESIAN_POINT('Ctrl Pts',(-10.3591024159266,15.2,-1.33473444504839));
#263994=CARTESIAN_POINT('Ctrl Pts',(-10.3619978645013,15.2,-1.33468293571667));
#263995=CARTESIAN_POINT('Ctrl Pts',(-10.364893313076,15.2,-1.33463142638496));
#263996=CARTESIAN_POINT('Ctrl Pts',(-10.3678379272646,15.2,-1.33457075874251));
#263997=CARTESIAN_POINT('Ctrl Pts',(-10.3708309698204,15.2,-1.33450042649549));
#263998=CARTESIAN_POINT('Ctrl Pts',(-10.3738240126481,15.2,-1.33443009424208));
#263999=CARTESIAN_POINT('Ctrl Pts',(-10.3768654853318,15.2,-1.33435009930414));
#264000=CARTESIAN_POINT('Ctrl Pts',(-10.3799546683367,15.2,-1.3342599522152));
#264001=CARTESIAN_POINT('Ctrl Pts',(-10.383043851061,15.2,-1.33416980513445));
#264002=CARTESIAN_POINT('Ctrl Pts',(-10.3861807463457,15.2,-1.33406950702371));
#264003=CARTESIAN_POINT('Ctrl Pts',(-10.3893646491487,15.2,-1.33395858102728));
#264004=CARTESIAN_POINT('Ctrl Pts',(-10.3925485519517,15.2,-1.33384765503084));
#264005=CARTESIAN_POINT('Ctrl Pts',(-10.3957794643427,15.2,-1.33372610281025));
#264006=CARTESIAN_POINT('Ctrl Pts',(-10.3990566960549,15.2,-1.33359346256555));
#264007=CARTESIAN_POINT('Ctrl Pts',(-10.4023339280648,15.2,-1.3334608223088));
#264008=CARTESIAN_POINT('Ctrl Pts',(-10.4056574817472,15.2,-1.33331709156735));
#264009=CARTESIAN_POINT('Ctrl Pts',(-10.4090266809339,15.2,-1.33316182547477));
#264010=CARTESIAN_POINT('Ctrl Pts',(-10.4123958798146,15.2,-1.3330065593963));
#264011=CARTESIAN_POINT('Ctrl Pts',(-10.4158107252875,15.2,-1.3328397546176));
#264012=CARTESIAN_POINT('Ctrl Pts',(-10.4192705589137,15.2,-1.33266097845691));
#264013=CARTESIAN_POINT('Ctrl Pts',(-10.4233070316872,15.2,-1.33245240625861));
#264014=CARTESIAN_POINT('Ctrl Pts',(-10.4274047334869,15.2,-1.33222753370442));
#264015=CARTESIAN_POINT('Ctrl Pts',(-10.4315626413885,15.2,-1.33198569293577));
#264016=CARTESIAN_POINT('Ctrl Pts',(-10.435126562262,15.2,-1.33177840085911));
#264017=CARTESIAN_POINT('Ctrl Pts',(-10.4387347159883,15.2,-1.33155864115441));
#264018=CARTESIAN_POINT('Ctrl Pts',(-10.4423864699409,15.2,-1.33132600224564));
#264019=CARTESIAN_POINT('Ctrl Pts',(-10.4478641008697,15.2,-1.33097704388247));
#264020=CARTESIAN_POINT('Ctrl Pts',(-10.4534398288274,15.2,-1.33059910656405));
#264021=CARTESIAN_POINT('Ctrl Pts',(-10.459111570651,15.2,-1.33019084730967));
#264022=CARTESIAN_POINT('Ctrl Pts',(-10.4628927322101,15.2,-1.32991867444869));
#264023=CARTESIAN_POINT('Ctrl Pts',(-10.4667165679495,15.2,-1.32963302655132));
#264024=CARTESIAN_POINT('Ctrl Pts',(-10.470582473413,15.2,-1.32933351970072));
#264025=CARTESIAN_POINT('Ctrl Pts',(-10.4757370136799,15.2,-1.32893417726047));
#264026=CARTESIAN_POINT('Ctrl Pts',(-10.4809663449806,15.2,-1.32851019518761));
#264027=CARTESIAN_POINT('Ctrl Pts',(-10.4862690668431,15.2,-1.32806068772572));
#264028=CARTESIAN_POINT('Ctrl Pts',(-10.4902461081497,15.2,-1.32772355713696));
#264029=CARTESIAN_POINT('Ctrl Pts',(-10.4942644315975,15.2,-1.32737207171173));
#264030=CARTESIAN_POINT('Ctrl Pts',(-10.4983234597833,15.2,-1.32700586797504));
#264031=CARTESIAN_POINT('Ctrl Pts',(-10.5017059833944,15.2,-1.32670069818338));
#264032=CARTESIAN_POINT('Ctrl Pts',(-10.505116773614,15.2,-1.32638530727359));
#264033=CARTESIAN_POINT('Ctrl Pts',(-10.5085555014769,15.2,-1.32605949171653));
#264034=CARTESIAN_POINT('Ctrl Pts',(-10.5119942293398,15.2,-1.32573367615947));
#264035=CARTESIAN_POINT('Ctrl Pts',(-10.5154608943717,15.2,-1.32539743567784));
#264036=CARTESIAN_POINT('Ctrl Pts',(-10.5189551722203,15.2,-1.32505057026062));
#264037=CARTESIAN_POINT('Ctrl Pts',(-10.522449450069,15.2,-1.3247037048434));
#264038=CARTESIAN_POINT('Ctrl Pts',(-10.525971341803,15.2,-1.32434621568201));
#264039=CARTESIAN_POINT('Ctrl Pts',(-10.5295205239573,15.2,-1.32397790450089));
#264040=CARTESIAN_POINT('Ctrl Pts',(-10.5330697061115,15.2,-1.32360959331977));
#264041=CARTESIAN_POINT('Ctrl Pts',(-10.5366461820254,15.2,-1.32323046192497));
#264042=CARTESIAN_POINT('Ctrl Pts',(-10.5402496341517,15.2,-1.32284031898805));
#264043=CARTESIAN_POINT('Ctrl Pts',(-10.543853086278,15.2,-1.32245017605112));
#264044=CARTESIAN_POINT('Ctrl Pts',(-10.5474835150206,15.2,-1.32204901959146));
#264045=CARTESIAN_POINT('Ctrl Pts',(-10.551140607245,15.2,-1.32163666493777));
#264046=CARTESIAN_POINT('Ctrl Pts',(-10.5547976994694,15.2,-1.32122431028407));
#264047=CARTESIAN_POINT('Ctrl Pts',(-10.558481457722,15.2,-1.32080075384964));
#264048=CARTESIAN_POINT('Ctrl Pts',(-10.5621915732103,15.2,-1.32036581516815));
#264049=CARTESIAN_POINT('Ctrl Pts',(-10.5659016882941,15.2,-1.31993087653407));
#264050=CARTESIAN_POINT('Ctrl Pts',(-10.5696381619368,15.2,-1.31948455459797));
#264051=CARTESIAN_POINT('Ctrl Pts',(-10.5734006879829,15.2,-1.3190266693016));
#264052=CARTESIAN_POINT('Ctrl Pts',(-10.5771632144391,15.2,-1.31856878395532));
#264053=CARTESIAN_POINT('Ctrl Pts',(-10.5809517962087,15.2,-1.31809933588424));
#264054=CARTESIAN_POINT('Ctrl Pts',(-10.5847661325261,15.2,-1.31761814657965));
#264055=CARTESIAN_POINT('Ctrl Pts',(-10.5893433363564,15.2,-1.31704071938266));
#264056=CARTESIAN_POINT('Ctrl Pts',(-10.5939576252204,15.2,-1.31644638797239));
#264057=CARTESIAN_POINT('Ctrl Pts',(-10.5986084914583,15.2,-1.31583485440751));
#264058=CARTESIAN_POINT('Ctrl Pts',(-10.6024842131121,15.2,-1.31532524313121));
#264059=CARTESIAN_POINT('Ctrl Pts',(-10.6063853355615,15.2,-1.31480368478678));
#264060=CARTESIAN_POINT('Ctrl Pts',(-10.6103115670219,15.2,-1.31427001193857));
#264061=CARTESIAN_POINT('Ctrl Pts',(-10.6158082907241,15.2,-1.31352286999761));
#264062=CARTESIAN_POINT('Ctrl Pts',(-10.6213542277175,15.2,-1.31275198199561));
#264063=CARTESIAN_POINT('Ctrl Pts',(-10.6269485919773,15.2,-1.31195689832433));
#264064=CARTESIAN_POINT('Ctrl Pts',(-10.6309445666975,15.2,-1.31138898138089));
#264065=CARTESIAN_POINT('Ctrl Pts',(-10.6349652493134,15.2,-1.31080871873089));
#264066=CARTESIAN_POINT('Ctrl Pts',(-10.6390103568055,15.2,-1.31021595182715));
#264067=CARTESIAN_POINT('Ctrl Pts',(-10.6430554642976,15.2,-1.3096231849234));
#264068=CARTESIAN_POINT('Ctrl Pts',(-10.6471249966725,15.2,-1.30901791343972));
#264069=CARTESIAN_POINT('Ctrl Pts',(-10.6512186754907,15.2,-1.30839997906539));
#264070=CARTESIAN_POINT('Ctrl Pts',(-10.6553123543089,15.2,-1.30778204469104));
#264071=CARTESIAN_POINT('Ctrl Pts',(-10.6594301784139,15.2,-1.30715144689694));
#264072=CARTESIAN_POINT('Ctrl Pts',(-10.6635718732043,15.2,-1.30650803405038));
#264073=CARTESIAN_POINT('Ctrl Pts',(-10.6677135679947,15.2,-1.30586462120383));
#264074=CARTESIAN_POINT('Ctrl Pts',(-10.6718791328065,15.2,-1.30520839202564));
#264075=CARTESIAN_POINT('Ctrl Pts',(-10.6760682944227,15.2,-1.30453919521708));
#264076=CARTESIAN_POINT('Ctrl Pts',(-10.6802574560389,15.2,-1.30386999840852));
#264077=CARTESIAN_POINT('Ctrl Pts',(-10.6844702153,15.2,-1.30318783430561));
#264078=CARTESIAN_POINT('Ctrl Pts',(-10.6887063019667,15.2,-1.30249255500005));
#264079=CARTESIAN_POINT('Ctrl Pts',(-10.6920951714847,15.2,-1.30193633152529));
#264080=CARTESIAN_POINT('Ctrl Pts',(-10.6954989715822,15.2,-1.30137171455233));
#264081=CARTESIAN_POINT('Ctrl Pts',(-10.6989175643256,15.2,-1.30079862913134));
#264082=CARTESIAN_POINT('Ctrl Pts',(-10.7023361566032,15.2,-1.30022554378844));
#264083=CARTESIAN_POINT('Ctrl Pts',(-10.7057695414556,15.2,-1.29964398993542));
#264084=CARTESIAN_POINT('Ctrl Pts',(-10.7092175850227,15.2,-1.29905389525878));
#264085=CARTESIAN_POINT('Ctrl Pts',(-10.7143896506082,15.2,-1.29816875320362));
#264086=CARTESIAN_POINT('Ctrl Pts',(-10.7195946954383,15.2,-1.29726439269918));
#264087=CARTESIAN_POINT('Ctrl Pts',(-10.7248322682458,15.2,-1.29634057156741));
#264088=CARTESIAN_POINT('Ctrl Pts',(-10.7291969124106,15.2,-1.2955707205963));
#264089=CARTESIAN_POINT('Ctrl Pts',(-10.7335841449306,15.2,-1.2947873542425));
#264090=CARTESIAN_POINT('Ctrl Pts',(-10.7379937092465,15.2,-1.29399033809252));
#264091=CARTESIAN_POINT('Ctrl Pts',(-10.7415213608915,15.2,-1.29335272513779));
#264092=CARTESIAN_POINT('Ctrl Pts',(-10.7450633034961,15.2,-1.29270637431324));
#264093=CARTESIAN_POINT('Ctrl Pts',(-10.7486194070242,15.2,-1.29205121822141));
#264094=CARTESIAN_POINT('Ctrl Pts',(-10.7521755100677,15.2,-1.29139606221884));
#264095=CARTESIAN_POINT('Ctrl Pts',(-10.7557457737529,15.2,-1.29073209939859));
#264096=CARTESIAN_POINT('Ctrl Pts',(-10.7593300686806,15.2,-1.29005926334339));
#264097=CARTESIAN_POINT('Ctrl Pts',(-10.7629143640968,15.2,-1.28938642719651));
#264098=CARTESIAN_POINT('Ctrl Pts',(-10.7665126894836,15.2,-1.28870471745705));
#264099=CARTESIAN_POINT('Ctrl Pts',(-10.7701249182525,15.2,-1.28801406674958));
#264100=CARTESIAN_POINT('Ctrl Pts',(-10.7737371465292,15.2,-1.28732341613621));
#264101=CARTESIAN_POINT('Ctrl Pts',(-10.7773632748011,15.2,-1.28662382462094));
#264102=CARTESIAN_POINT('Ctrl Pts',(-10.7810031791132,15.2,-1.28591522662424));
#264103=CARTESIAN_POINT('Ctrl Pts',(-10.7855530598753,15.2,-1.28502947905594));
#264104=CARTESIAN_POINT('Ctrl Pts',(-10.7901244635677,15.2,-1.28412965881288));
#264105=CARTESIAN_POINT('Ctrl Pts',(-10.7947171418993,15.2,-1.2832156381196));
#264106=CARTESIAN_POINT('Ctrl Pts',(-10.7983912847648,15.2,-1.28248442152512));
#264107=CARTESIAN_POINT('Ctrl Pts',(-10.802079043534,15.2,-1.28174411832992));
#264108=CARTESIAN_POINT('Ctrl Pts',(-10.8057802937525,15.2,-1.28099466367454));
#264109=CARTESIAN_POINT('Ctrl Pts',(-10.8094815434668,15.2,-1.28024520912126));
#264110=CARTESIAN_POINT('Ctrl Pts',(-10.8131962844855,15.2,-1.27948660363966));
#264111=CARTESIAN_POINT('Ctrl Pts',(-10.8169243916238,15.2,-1.27871878492559));
#264112=CARTESIAN_POINT('Ctrl Pts',(-10.8215845259277,15.2,-1.27775901145454));
#264113=CARTESIAN_POINT('Ctrl Pts',(-10.8262655452923,15.2,-1.27678483963929));
#264114=CARTESIAN_POINT('Ctrl Pts',(-10.83096721036,15.2,-1.27579615290437));
#264115=CARTESIAN_POINT('Ctrl Pts',(-10.8347285426192,15.2,-1.27500520347332));
#264116=CARTESIAN_POINT('Ctrl Pts',(-10.8385030876956,15.2,-1.27420496198066));
#264117=CARTESIAN_POINT('Ctrl Pts',(-10.8422907232526,15.2,-1.27339537126616));
#264118=CARTESIAN_POINT('Ctrl Pts',(-10.8489190852193,15.2,-1.27197858757095));
#264119=CARTESIAN_POINT('Ctrl Pts',(-10.8555875370922,15.2,-1.27053316286473));
#264120=CARTESIAN_POINT('Ctrl Pts',(-10.8622954308934,15.2,-1.26905878560396));
#264121=CARTESIAN_POINT('Ctrl Pts',(-10.8661285126925,15.2,-1.26821628439409));
#264122=CARTESIAN_POINT('Ctrl Pts',(-10.8699744735899,15.2,-1.26736432863545));
#264123=CARTESIAN_POINT('Ctrl Pts',(-10.873833194718,15.2,-1.26650286009539));
#264124=CARTESIAN_POINT('Ctrl Pts',(-10.8786565965225,15.2,-1.26542602433228));
#264125=CARTESIAN_POINT('Ctrl Pts',(-10.8834999359364,15.2,-1.26433432554453));
#264126=CARTESIAN_POINT('Ctrl Pts',(-10.888362980264,15.2,-1.26322765227565));
#264127=CARTESIAN_POINT('Ctrl Pts',(-10.8922534159381,15.2,-1.2623423136123));
#264128=CARTESIAN_POINT('Ctrl Pts',(-10.8961564639672,15.2,-1.26144739104688));
#264129=CARTESIAN_POINT('Ctrl Pts',(-10.9000720063485,15.2,-1.26054282855215));
#264130=CARTESIAN_POINT('Ctrl Pts',(-10.9039875481964,15.2,-1.25963826618067));
#264131=CARTESIAN_POINT('Ctrl Pts',(-10.9079155838343,15.2,-1.25872406573544));
#264132=CARTESIAN_POINT('Ctrl Pts',(-10.911855998178,15.2,-1.25780016986716));
#264133=CARTESIAN_POINT('Ctrl Pts',(-10.9157964130586,15.2,-1.25687627387299));
#264134=CARTESIAN_POINT('Ctrl Pts',(-10.9197492047296,15.2,-1.255942682261));
#264135=CARTESIAN_POINT('Ctrl Pts',(-10.9237142590576,15.2,-1.25499934293117));
#264136=CARTESIAN_POINT('Ctrl Pts',(-10.9286705766975,15.2,-1.25382016883316));
#264137=CARTESIAN_POINT('Ctrl Pts',(-10.9336460544901,15.2,-1.2526257623933));
#264138=CARTESIAN_POINT('Ctrl Pts',(-10.9386404673799,15.2,-1.25141601760956));
#264139=CARTESIAN_POINT('Ctrl Pts',(-10.942635997365,15.2,-1.25044822186169));
#264140=CARTESIAN_POINT('Ctrl Pts',(-10.9466436456065,15.2,-1.24947061170765));
#264141=CARTESIAN_POINT('Ctrl Pts',(-10.9506632993882,15.2,-1.24848313328902));
#264142=CARTESIAN_POINT('Ctrl Pts',(-10.9556878670261,15.2,-1.24724878516483));
#264143=CARTESIAN_POINT('Ctrl Pts',(-10.9607311917589,15.2,-1.24599901938746));
#264144=CARTESIAN_POINT('Ctrl Pts',(-10.9657930537024,15.2,-1.24473373362438));
#264145=CARTESIAN_POINT('Ctrl Pts',(-10.9708549156459,15.2,-1.2434684478613));
#264146=CARTESIAN_POINT('Ctrl Pts',(-10.9759353155186,15.2,-1.2421876429066));
#264147=CARTESIAN_POINT('Ctrl Pts',(-10.9810340340139,15.2,-1.24089121977576));
#264148=CARTESIAN_POINT('Ctrl Pts',(-10.9851130090325,15.2,-1.23985408121456));
#264149=CARTESIAN_POINT('Ctrl Pts',(-10.9892037076405,15.2,-1.23880694764417));
#264150=CARTESIAN_POINT('Ctrl Pts',(-10.9933060194207,15.2,-1.23774976908553));
#264151=CARTESIAN_POINT('Ctrl Pts',(-10.9984339088666,15.2,-1.23642829595925));
#264152=CARTESIAN_POINT('Ctrl Pts',(-11.0035799444407,15.2,-1.23509112729103));
#264153=CARTESIAN_POINT('Ctrl Pts',(-11.0087439096505,15.2,-1.23373816833142));
#264154=CARTESIAN_POINT('Ctrl Pts',(-11.0128750814806,15.2,-1.23265580125221));
#264155=CARTESIAN_POINT('Ctrl Pts',(-11.0170177294263,15.2,-1.23156332727119));
#264156=CARTESIAN_POINT('Ctrl Pts',(-11.0211717432722,15.2,-1.23046070080081));
#264157=CARTESIAN_POINT('Ctrl Pts',(-11.027402764324,15.2,-1.22880676102011));
#264158=CARTESIAN_POINT('Ctrl Pts',(-11.0336593575536,15.2,-1.22712997358033));
#264159=CARTESIAN_POINT('Ctrl Pts',(-11.0399411605736,15.2,-1.22543018189366));
#264160=CARTESIAN_POINT('Ctrl Pts',(-11.044129029634,15.2,-1.22429698733295));
#264161=CARTESIAN_POINT('Ctrl Pts',(-11.0483281021154,15.2,-1.2231535688452));
#264162=CARTESIAN_POINT('Ctrl Pts',(-11.0525382712529,15.2,-1.22199987899927));
#264163=CARTESIAN_POINT('Ctrl Pts',(-11.0567484398168,15.2,-1.22084618931053));
#264164=CARTESIAN_POINT('Ctrl Pts',(-11.0609697047996,15.2,-1.21968222907277));
#264165=CARTESIAN_POINT('Ctrl Pts',(-11.0652019593414,15.2,-1.21850795339204));
#264166=CARTESIAN_POINT('Ctrl Pts',(-11.0694342144598,15.2,-1.21733367755132));
#264167=CARTESIAN_POINT('Ctrl Pts',(-11.073677459532,15.2,-1.21614908547629));
#264168=CARTESIAN_POINT('Ctrl Pts',(-11.0779315880417,15.2,-1.21495413296673));
#264169=CARTESIAN_POINT('Ctrl Pts',(-11.0821857165513,15.2,-1.21375918045716));
#264170=CARTESIAN_POINT('Ctrl Pts',(-11.0864507294622,15.2,-1.21255386732693));
#264171=CARTESIAN_POINT('Ctrl Pts',(-11.0907265199741,15.2,-1.21133815009294));
#264172=CARTESIAN_POINT('Ctrl Pts',(-11.0939333625668,15.2,-1.21042636225027));
#264173=CARTESIAN_POINT('Ctrl Pts',(-11.097146268145,15.2,-1.20950872135125));
#264174=CARTESIAN_POINT('Ctrl Pts',(-11.1003651928562,15.2,-1.20858520954632));
#264175=CARTESIAN_POINT('Ctrl Pts',(-11.1057300675698,15.2,-1.20704602314885));
#264176=CARTESIAN_POINT('Ctrl Pts',(-11.1111116610158,15.2,-1.20549052939023));
#264177=CARTESIAN_POINT('Ctrl Pts',(-11.1165097696978,15.2,-1.20391864306944));
#264178=CARTESIAN_POINT('Ctrl Pts',(-11.1197486347892,15.2,-1.20297551131124));
#264179=CARTESIAN_POINT('Ctrl Pts',(-11.122993445822,15.2,-1.20202647842835));
#264180=CARTESIAN_POINT('Ctrl Pts',(-11.1262441588711,15.2,-1.2010715276292));
#264181=CARTESIAN_POINT('Ctrl Pts',(-11.1305784427397,15.2,-1.19979825995483));
#264182=CARTESIAN_POINT('Ctrl Pts',(-11.1349232189575,15.2,-1.19851446950407));
#264183=CARTESIAN_POINT('Ctrl Pts',(-11.1392783851514,15.2,-1.19722011571282));
#264184=CARTESIAN_POINT('Ctrl Pts',(-11.1425447599452,15.2,-1.19624935032529));
#264185=CARTESIAN_POINT('Ctrl Pts',(-11.1458169791386,15.2,-1.19527264272776));
#264186=CARTESIAN_POINT('Ctrl Pts',(-11.1490949992687,15.2,-1.1942899759726));
#264187=CARTESIAN_POINT('Ctrl Pts',(-11.1523730199944,15.2,-1.19330730903893));
#264188=CARTESIAN_POINT('Ctrl Pts',(-11.155656842005,15.2,-1.19231868312859));
#264189=CARTESIAN_POINT('Ctrl Pts',(-11.1589464226921,15.2,-1.1913240797749));
#264190=CARTESIAN_POINT('Ctrl Pts',(-11.1622360027817,15.2,-1.19032947660189));
#264191=CARTESIAN_POINT('Ctrl Pts',(-11.1655313414627,15.2,-1.18932889818752));
#264192=CARTESIAN_POINT('Ctrl Pts',(-11.1688323950933,15.2,-1.18832232589024));
#264193=CARTESIAN_POINT('Ctrl Pts',(-11.1732337997341,15.2,-1.18698022955482));
#264194=CARTESIAN_POINT('Ctrl Pts',(-11.1776453663527,15.2,-1.18562747753135));
#264195=CARTESIAN_POINT('Ctrl Pts',(-11.1820669926001,15.2,-1.18426403246451));
#264196=CARTESIAN_POINT('Ctrl Pts',(-11.1853832124363,15.2,-1.18324144861794));
#264197=CARTESIAN_POINT('Ctrl Pts',(-11.1887050921963,15.2,-1.18221284900386));
#264198=CARTESIAN_POINT('Ctrl Pts',(-11.192032588283,15.2,-1.1811782177506));
#264199=CARTESIAN_POINT('Ctrl Pts',(-11.1953600849741,15.2,-1.18014358630939));
#264200=CARTESIAN_POINT('Ctrl Pts',(-11.1986931977752,15.2,-1.17910292269149));
#264201=CARTESIAN_POINT('Ctrl Pts',(-11.2020318859695,15.2,-1.1780562112052));
#264202=CARTESIAN_POINT('Ctrl Pts',(-11.2053705735573,15.2,-1.17700949990907));
#264203=CARTESIAN_POINT('Ctrl Pts',(-11.2087148357031,15.2,-1.1759567397466));
#264204=CARTESIAN_POINT('Ctrl Pts',(-11.2120646308319,15.2,-1.17489791636787));
#264205=CARTESIAN_POINT('Ctrl Pts',(-11.2176476229161,15.2,-1.17313321067255));
#264206=CARTESIAN_POINT('Ctrl Pts',(-11.2232459852591,15.2,-1.17135165884336));
#264207=CARTESIAN_POINT('Ctrl Pts',(-11.2288595241517,15.2,-1.16955319055789));
#264208=CARTESIAN_POINT('Ctrl Pts',(-11.2322276473649,15.2,-1.16847410962581));
#264209=CARTESIAN_POINT('Ctrl Pts',(-11.2356012328241,15.2,-1.16738893674188));
#264210=CARTESIAN_POINT('Ctrl Pts',(-11.2389802419101,15.2,-1.16629765936434));
#264211=CARTESIAN_POINT('Ctrl Pts',(-11.2423592509961,15.2,-1.16520638198679));
#264212=CARTESIAN_POINT('Ctrl Pts',(-11.2457436822565,15.2,-1.16410899759329));
#264213=CARTESIAN_POINT('Ctrl Pts',(-11.249133494425,15.2,-1.16300549275839));
#264214=CARTESIAN_POINT('Ctrl Pts',(-11.2547831815778,15.2,-1.16116631796673));
#264215=CARTESIAN_POINT('Ctrl Pts',(-11.2604478168889,15.2,-1.15931013866118));
#264216=CARTESIAN_POINT('Ctrl Pts',(-11.2661272105,15.2,-1.1574368865084));
#264217=CARTESIAN_POINT('Ctrl Pts',(-11.2718066041111,15.2,-1.15556363435561));
#264218=CARTESIAN_POINT('Ctrl Pts',(-11.2775007568383,15.2,-1.15367330726883));
#264219=CARTESIAN_POINT('Ctrl Pts',(-11.2832094782531,15.2,-1.15176583927402));
#264220=CARTESIAN_POINT('Ctrl Pts',(-11.2877764550117,15.2,-1.15023986500291));
#264221=CARTESIAN_POINT('Ctrl Pts',(-11.2923527583261,15.2,-1.14870291865603));
#264222=CARTESIAN_POINT('Ctrl Pts',(-11.2969382902836,15.2,-1.14715496772814));
#264223=CARTESIAN_POINT('Ctrl Pts',(-11.3026702056991,15.2,-1.1452200289101));
#264224=CARTESIAN_POINT('Ctrl Pts',(-11.3084165421699,15.2,-1.14326789436179));
#264225=CARTESIAN_POINT('Ctrl Pts',(-11.3141771134882,15.2,-1.14129849651598));
#264226=CARTESIAN_POINT('Ctrl Pts',(-11.3176334567815,15.2,-1.14011685763677));
#264227=CARTESIAN_POINT('Ctrl Pts',(-11.3210949255012,15.2,-1.13892900546413));
#264228=CARTESIAN_POINT('Ctrl Pts',(-11.3245614792557,15.2,-1.13773492449808));
#264229=CARTESIAN_POINT('Ctrl Pts',(-11.3291835498788,15.2,-1.13614281690487));
#264230=CARTESIAN_POINT('Ctrl Pts',(-11.3338146609246,15.2,-1.13453963629871));
#264231=CARTESIAN_POINT('Ctrl Pts',(-11.3384547169552,15.2,-1.13292534953449));
#264232=CARTESIAN_POINT('Ctrl Pts',(-11.3419347591362,15.2,-1.13171463440633));
#264233=CARTESIAN_POINT('Ctrl Pts',(-11.3454198337803,15.2,-1.13049767263829));
#264234=CARTESIAN_POINT('Ctrl Pts',(-11.348909900403,15.2,-1.12927445084995));
#264235=CARTESIAN_POINT('Ctrl Pts',(-11.3523999670258,15.2,-1.12805122906162));
#264236=CARTESIAN_POINT('Ctrl Pts',(-11.3558950257149,15.2,-1.12682174560703));
#264237=CARTESIAN_POINT('Ctrl Pts',(-11.3593950397537,15.2,-1.12558598931945));
#264238=CARTESIAN_POINT('Ctrl Pts',(-11.3628950544283,15.2,-1.12435023280738));
#264239=CARTESIAN_POINT('Ctrl Pts',(-11.3664000220544,15.2,-1.1231082022102));
#264240=CARTESIAN_POINT('Ctrl Pts',(-11.3699099047735,15.2,-1.12185988473625));
#264241=CARTESIAN_POINT('Ctrl Pts',(-11.373419786855,15.2,-1.12061156748908));
#264242=CARTESIAN_POINT('Ctrl Pts',(-11.3769345828659,15.2,-1.11935696200728));
#264243=CARTESIAN_POINT('Ctrl Pts',(-11.3804542531644,15.2,-1.11809605573937));
#264244=CARTESIAN_POINT('Ctrl Pts',(-11.3839739234629,15.2,-1.11683514947147));
#264245=CARTESIAN_POINT('Ctrl Pts',(-11.3874984671626,15.2,-1.11556794208208));
#264246=CARTESIAN_POINT('Ctrl Pts',(-11.3910278474098,15.2,-1.11429442183614));
#264247=CARTESIAN_POINT('Ctrl Pts',(-11.3957336875257,15.2,-1.11259639491866));
#264248=CARTESIAN_POINT('Ctrl Pts',(-11.4004481282759,15.2,-1.11088714409233));
#264249=CARTESIAN_POINT('Ctrl Pts',(-11.4051710834445,15.2,-1.10916664128969));
#264250=CARTESIAN_POINT('Ctrl Pts',(-11.4110747778878,15.2,-1.10701601261058));
#264251=CARTESIAN_POINT('Ctrl Pts',(-11.4169917723552,15.2,-1.10484780395616));
#264252=CARTESIAN_POINT('Ctrl Pts',(-11.4229218548033,15.2,-1.10266194023708));
#264253=CARTESIAN_POINT('Ctrl Pts',(-11.4264799041429,15.2,-1.10135042205328));
#264254=CARTESIAN_POINT('Ctrl Pts',(-11.4300426634359,15.2,-1.10003254938976));
#264255=CARTESIAN_POINT('Ctrl Pts',(-11.4336101084723,15.2,-1.09870831335541));
#264256=CARTESIAN_POINT('Ctrl Pts',(-11.4383667022862,15.2,-1.09694266514923));
#264257=CARTESIAN_POINT('Ctrl Pts',(-11.4431316236994,15.2,-1.09516570948731));
#264258=CARTESIAN_POINT('Ctrl Pts',(-11.4479048650001,15.2,-1.09337742900002));
#264259=CARTESIAN_POINT('Ctrl Pts',(-10.3708900240001,15.2,-0.292001929000012));
#264260=CARTESIAN_POINT('Ctrl Pts',(-10.3708900240001,11.6,-0.292001929000012));
#264261=CARTESIAN_POINT('Ctrl Pts',(-10.3710632460001,15.2,-0.292021795000017));
#264262=CARTESIAN_POINT('Ctrl Pts',(-10.3710632460001,11.6,-0.292021795000017));
#264263=CARTESIAN_POINT('Ctrl Pts',(-10.3714157310001,15.2,-0.292062310000016));
#264264=CARTESIAN_POINT('Ctrl Pts',(-10.3714157310001,11.6,-0.292062310000017));
#264265=CARTESIAN_POINT('Ctrl Pts',(-10.3719498000001,15.2,-0.292123961000015));
#264266=CARTESIAN_POINT('Ctrl Pts',(-10.3719498000001,11.6,-0.292123961000015));
#264267=CARTESIAN_POINT('Ctrl Pts',(-10.3726691760001,15.2,-0.292207548000012));
#264268=CARTESIAN_POINT('Ctrl Pts',(-10.3726691760001,11.6,-0.292207548000012));
#264269=CARTESIAN_POINT('Ctrl Pts',(-10.3735789750001,15.2,-0.292314181000015));
#264270=CARTESIAN_POINT('Ctrl Pts',(-10.3735789750001,11.6,-0.292314181000016));
#264271=CARTESIAN_POINT('Ctrl Pts',(-10.3745034120001,15.2,-0.292423469000016));
#264272=CARTESIAN_POINT('Ctrl Pts',(-10.3745034120001,11.6,-0.292423469000016));
#264273=CARTESIAN_POINT('Ctrl Pts',(-10.3754371840001,15.2,-0.292534812000014));
#264274=CARTESIAN_POINT('Ctrl Pts',(-10.3754371840001,11.6,-0.292534812000014));
#264275=CARTESIAN_POINT('Ctrl Pts',(-10.3763802670001,15.2,-0.292648223000014));
#264276=CARTESIAN_POINT('Ctrl Pts',(-10.3763802670001,11.6,-0.292648223000014));
#264277=CARTESIAN_POINT('Ctrl Pts',(-10.3773326270001,15.2,-0.292763718000018));
#264278=CARTESIAN_POINT('Ctrl Pts',(-10.3773326270001,11.6,-0.292763718000018));
#264279=CARTESIAN_POINT('Ctrl Pts',(-10.3782942400001,15.2,-0.292881310000013));
#264280=CARTESIAN_POINT('Ctrl Pts',(-10.3782942400001,11.6,-0.292881310000013));
#264281=CARTESIAN_POINT('Ctrl Pts',(-10.3792650740001,15.2,-0.293001015000014));
#264282=CARTESIAN_POINT('Ctrl Pts',(-10.3792650740001,11.6,-0.293001015000014));
#264283=CARTESIAN_POINT('Ctrl Pts',(-10.3802451030001,15.2,-0.293122847000014));
#264284=CARTESIAN_POINT('Ctrl Pts',(-10.3802451030001,11.6,-0.293122847000014));
#264285=CARTESIAN_POINT('Ctrl Pts',(-10.3812342970001,15.2,-0.293246820000017));
#264286=CARTESIAN_POINT('Ctrl Pts',(-10.3812342970001,11.6,-0.293246820000018));
#264287=CARTESIAN_POINT('Ctrl Pts',(-10.3822326280001,15.2,-0.293372950000013));
#264288=CARTESIAN_POINT('Ctrl Pts',(-10.3822326280001,11.6,-0.293372950000013));
#264289=CARTESIAN_POINT('Ctrl Pts',(-10.3832400690001,15.2,-0.293501248000014));
#264290=CARTESIAN_POINT('Ctrl Pts',(-10.3832400690001,11.6,-0.293501248000015));
#264291=CARTESIAN_POINT('Ctrl Pts',(-10.3842565920001,15.2,-0.293631732000015));
#264292=CARTESIAN_POINT('Ctrl Pts',(-10.3842565920001,11.6,-0.293631732000015));
#264293=CARTESIAN_POINT('Ctrl Pts',(-10.3852821680001,15.2,-0.293764413000015));
#264294=CARTESIAN_POINT('Ctrl Pts',(-10.3852821680001,11.6,-0.293764413000015));
#264295=CARTESIAN_POINT('Ctrl Pts',(-10.3863167710001,15.2,-0.293899307000016));
#264296=CARTESIAN_POINT('Ctrl Pts',(-10.3863167710001,11.6,-0.293899307000017));
#264297=CARTESIAN_POINT('Ctrl Pts',(-10.3873603720001,15.2,-0.294036427000015));
#264298=CARTESIAN_POINT('Ctrl Pts',(-10.3873603720001,11.6,-0.294036427000016));
#264299=CARTESIAN_POINT('Ctrl Pts',(-10.3884129450001,15.2,-0.294175788000013));
#264300=CARTESIAN_POINT('Ctrl Pts',(-10.3884129450001,11.6,-0.294175788000013));
#264301=CARTESIAN_POINT('Ctrl Pts',(-10.3894744620001,15.2,-0.294317401000015));
#264302=CARTESIAN_POINT('Ctrl Pts',(-10.3894744620001,11.6,-0.294317401000015));
#264303=CARTESIAN_POINT('Ctrl Pts',(-10.3905448950001,15.2,-0.294461282000014));
#264304=CARTESIAN_POINT('Ctrl Pts',(-10.3905448950001,11.6,-0.294461282000014));
#264305=CARTESIAN_POINT('Ctrl Pts',(-10.3916242180001,15.2,-0.294607444000015));
#264306=CARTESIAN_POINT('Ctrl Pts',(-10.3916242180001,11.6,-0.294607444000015));
#264307=CARTESIAN_POINT('Ctrl Pts',(-10.3927124050001,15.2,-0.294755901000014));
#264308=CARTESIAN_POINT('Ctrl Pts',(-10.3927124050001,11.6,-0.294755901000015));
#264309=CARTESIAN_POINT('Ctrl Pts',(-10.3938094280001,15.2,-0.294906666000014));
#264310=CARTESIAN_POINT('Ctrl Pts',(-10.3938094280001,11.6,-0.294906666000015));
#264311=CARTESIAN_POINT('Ctrl Pts',(-10.3949152600001,15.2,-0.295059752000015));
#264312=CARTESIAN_POINT('Ctrl Pts',(-10.3949152600001,11.6,-0.295059752000016));
#264313=CARTESIAN_POINT('Ctrl Pts',(-10.3960298750001,15.2,-0.295215173000014));
#264314=CARTESIAN_POINT('Ctrl Pts',(-10.3960298750001,11.6,-0.295215173000015));
#264315=CARTESIAN_POINT('Ctrl Pts',(-10.3971532480001,15.2,-0.295372943000016));
#264316=CARTESIAN_POINT('Ctrl Pts',(-10.3971532480001,11.6,-0.295372943000017));
#264317=CARTESIAN_POINT('Ctrl Pts',(-10.3982853500001,15.2,-0.295533072000014));
#264318=CARTESIAN_POINT('Ctrl Pts',(-10.3982853500001,11.6,-0.295533072000014));
#264319=CARTESIAN_POINT('Ctrl Pts',(-10.3994261560001,15.2,-0.295695576000017));
#264320=CARTESIAN_POINT('Ctrl Pts',(-10.3994261560001,11.6,-0.295695576000017));
#264321=CARTESIAN_POINT('Ctrl Pts',(-10.4005756420001,15.2,-0.295860468000013));
#264322=CARTESIAN_POINT('Ctrl Pts',(-10.4005756420001,11.6,-0.295860468000014));
#264323=CARTESIAN_POINT('Ctrl Pts',(-10.4017337790001,15.2,-0.296027759000013));
#264324=CARTESIAN_POINT('Ctrl Pts',(-10.4017337790001,11.6,-0.296027759000013));
#264325=CARTESIAN_POINT('Ctrl Pts',(-10.4029005420001,15.2,-0.296197463000016));
#264326=CARTESIAN_POINT('Ctrl Pts',(-10.4029005420001,11.6,-0.296197463000017));
#264327=CARTESIAN_POINT('Ctrl Pts',(-10.4040759070001,15.2,-0.296369593000012));
#264328=CARTESIAN_POINT('Ctrl Pts',(-10.4040759070001,11.6,-0.296369593000013));
#264329=CARTESIAN_POINT('Ctrl Pts',(-10.4052598460001,15.2,-0.296544162000014));
#264330=CARTESIAN_POINT('Ctrl Pts',(-10.4052598460001,11.6,-0.296544162000015));
#264331=CARTESIAN_POINT('Ctrl Pts',(-10.4064523340001,15.2,-0.296721181000015));
#264332=CARTESIAN_POINT('Ctrl Pts',(-10.4064523340001,11.6,-0.296721181000015));
#264333=CARTESIAN_POINT('Ctrl Pts',(-10.4076533470001,15.2,-0.296900665000015));
#264334=CARTESIAN_POINT('Ctrl Pts',(-10.4076533470001,11.6,-0.296900665000015));
#264335=CARTESIAN_POINT('Ctrl Pts',(-10.4088628590001,15.2,-0.297082624000016));
#264336=CARTESIAN_POINT('Ctrl Pts',(-10.4088628590001,11.6,-0.297082624000016));
#264337=CARTESIAN_POINT('Ctrl Pts',(-10.4100808450001,15.2,-0.297267072000014));
#264338=CARTESIAN_POINT('Ctrl Pts',(-10.4100808450001,11.6,-0.297267072000014));
#264339=CARTESIAN_POINT('Ctrl Pts',(-10.4113072790001,15.2,-0.297454022000014));
#264340=CARTESIAN_POINT('Ctrl Pts',(-10.4113072790001,11.6,-0.297454022000015));
#264341=CARTESIAN_POINT('Ctrl Pts',(-10.4125421370001,15.2,-0.297643484000014));
#264342=CARTESIAN_POINT('Ctrl Pts',(-10.4125421370001,11.6,-0.297643484000015));
#264343=CARTESIAN_POINT('Ctrl Pts',(-10.4137853940001,15.2,-0.297835472000014));
#264344=CARTESIAN_POINT('Ctrl Pts',(-10.4137853940001,11.6,-0.297835472000015));
#264345=CARTESIAN_POINT('Ctrl Pts',(-10.4150370250001,15.2,-0.298029998000011));
#264346=CARTESIAN_POINT('Ctrl Pts',(-10.4150370250001,11.6,-0.298029998000012));
#264347=CARTESIAN_POINT('Ctrl Pts',(-10.4162970050001,15.2,-0.298227073000015));
#264348=CARTESIAN_POINT('Ctrl Pts',(-10.4162970050001,11.6,-0.298227073000015));
#264349=CARTESIAN_POINT('Ctrl Pts',(-10.4175653100001,15.2,-0.298426711000013));
#264350=CARTESIAN_POINT('Ctrl Pts',(-10.4175653100001,11.6,-0.298426711000013));
#264351=CARTESIAN_POINT('Ctrl Pts',(-10.4188419160001,15.2,-0.298628922000015));
#264352=CARTESIAN_POINT('Ctrl Pts',(-10.4188419160001,11.6,-0.298628922000015));
#264353=CARTESIAN_POINT('Ctrl Pts',(-10.4201267970001,15.2,-0.298833719000013));
#264354=CARTESIAN_POINT('Ctrl Pts',(-10.4201267970001,11.6,-0.298833719000014));
#264355=CARTESIAN_POINT('Ctrl Pts',(-10.4214199300001,15.2,-0.299041114000014));
#264356=CARTESIAN_POINT('Ctrl Pts',(-10.4214199300001,11.6,-0.299041114000014));
#264357=CARTESIAN_POINT('Ctrl Pts',(-10.4227212920001,15.2,-0.299251118000012));
#264358=CARTESIAN_POINT('Ctrl Pts',(-10.4227212920001,11.6,-0.299251118000013));
#264359=CARTESIAN_POINT('Ctrl Pts',(-10.4240308570001,15.2,-0.299463743000015));
#264360=CARTESIAN_POINT('Ctrl Pts',(-10.4240308570001,11.6,-0.299463743000015));
#264361=CARTESIAN_POINT('Ctrl Pts',(-10.4253486020001,15.2,-0.299679001000013));
#264362=CARTESIAN_POINT('Ctrl Pts',(-10.4253486020001,11.6,-0.299679001000013));
#264363=CARTESIAN_POINT('Ctrl Pts',(-10.4266745030001,15.2,-0.299896903000012));
#264364=CARTESIAN_POINT('Ctrl Pts',(-10.4266745030001,11.6,-0.299896903000012));
#264365=CARTESIAN_POINT('Ctrl Pts',(-10.4280085350001,15.2,-0.300117461000013));
#264366=CARTESIAN_POINT('Ctrl Pts',(-10.4280085350001,11.6,-0.300117461000014));
#264367=CARTESIAN_POINT('Ctrl Pts',(-10.4293506770001,15.2,-0.300340686000014));
#264368=CARTESIAN_POINT('Ctrl Pts',(-10.4293506770001,11.6,-0.300340686000014));
#264369=CARTESIAN_POINT('Ctrl Pts',(-10.4307009030001,15.2,-0.300566590000013));
#264370=CARTESIAN_POINT('Ctrl Pts',(-10.4307009030001,11.6,-0.300566590000014));
#264371=CARTESIAN_POINT('Ctrl Pts',(-10.4320591910001,15.2,-0.300795184000013));
#264372=CARTESIAN_POINT('Ctrl Pts',(-10.4320591910001,11.6,-0.300795184000014));
#264373=CARTESIAN_POINT('Ctrl Pts',(-10.4334255170001,15.2,-0.301026479000015));
#264374=CARTESIAN_POINT('Ctrl Pts',(-10.4334255170001,11.6,-0.301026479000015));
#264375=CARTESIAN_POINT('Ctrl Pts',(-10.4347998580001,15.2,-0.301260488000015));
#264376=CARTESIAN_POINT('Ctrl Pts',(-10.4347998580001,11.6,-0.301260488000015));
#264377=CARTESIAN_POINT('Ctrl Pts',(-10.4361821910001,15.2,-0.301497219000013));
#264378=CARTESIAN_POINT('Ctrl Pts',(-10.4361821910001,11.6,-0.301497219000014));
#264379=CARTESIAN_POINT('Ctrl Pts',(-10.4375724920001,15.2,-0.301736686000016));
#264380=CARTESIAN_POINT('Ctrl Pts',(-10.4375724920001,11.6,-0.301736686000016));
#264381=CARTESIAN_POINT('Ctrl Pts',(-10.4389707380001,15.2,-0.301978898000015));
#264382=CARTESIAN_POINT('Ctrl Pts',(-10.4389707380001,11.6,-0.301978898000015));
#264383=CARTESIAN_POINT('Ctrl Pts',(-10.4403769080001,15.2,-0.302223867000015));
#264384=CARTESIAN_POINT('Ctrl Pts',(-10.4403769080001,11.6,-0.302223867000016));
#264385=CARTESIAN_POINT('Ctrl Pts',(-10.4417909780001,15.2,-0.302471605000014));
#264386=CARTESIAN_POINT('Ctrl Pts',(-10.4417909780001,11.6,-0.302471605000015));
#264387=CARTESIAN_POINT('Ctrl Pts',(-10.4432129240001,15.2,-0.302722121000016));
#264388=CARTESIAN_POINT('Ctrl Pts',(-10.4432129240001,11.6,-0.302722121000017));
#264389=CARTESIAN_POINT('Ctrl Pts',(-10.4446427250001,15.2,-0.302975426000014));
#264390=CARTESIAN_POINT('Ctrl Pts',(-10.4446427250001,11.6,-0.302975426000014));
#264391=CARTESIAN_POINT('Ctrl Pts',(-10.4460803580001,15.2,-0.303231532000012));
#264392=CARTESIAN_POINT('Ctrl Pts',(-10.4460803580001,11.6,-0.303231532000013));
#264393=CARTESIAN_POINT('Ctrl Pts',(-10.4475258000001,15.2,-0.303490448000012));
#264394=CARTESIAN_POINT('Ctrl Pts',(-10.4475258000001,11.6,-0.303490448000013));
#264395=CARTESIAN_POINT('Ctrl Pts',(-10.4489790300001,15.2,-0.303752186000015));
#264396=CARTESIAN_POINT('Ctrl Pts',(-10.4489790300001,11.6,-0.303752186000015));
#264397=CARTESIAN_POINT('Ctrl Pts',(-10.4504400240001,15.2,-0.304016756000016));
#264398=CARTESIAN_POINT('Ctrl Pts',(-10.4504400240001,11.6,-0.304016756000017));
#264399=CARTESIAN_POINT('Ctrl Pts',(-10.4519087610001,15.2,-0.304284170000013));
#264400=CARTESIAN_POINT('Ctrl Pts',(-10.4519087610001,11.6,-0.304284170000014));
#264401=CARTESIAN_POINT('Ctrl Pts',(-10.4533852190001,15.2,-0.304554436000015));
#264402=CARTESIAN_POINT('Ctrl Pts',(-10.4533852190001,11.6,-0.304554436000016));
#264403=CARTESIAN_POINT('Ctrl Pts',(-10.4548693740001,15.2,-0.304827566000014));
#264404=CARTESIAN_POINT('Ctrl Pts',(-10.4548693740001,11.6,-0.304827566000015));
#264405=CARTESIAN_POINT('Ctrl Pts',(-10.4563612070001,15.2,-0.305103570000016));
#264406=CARTESIAN_POINT('Ctrl Pts',(-10.4563612070001,11.6,-0.305103570000016));
#264407=CARTESIAN_POINT('Ctrl Pts',(-10.4578606950001,15.2,-0.305382458000012));
#264408=CARTESIAN_POINT('Ctrl Pts',(-10.4578606950001,11.6,-0.305382458000012));
#264409=CARTESIAN_POINT('Ctrl Pts',(-10.4593678150001,15.2,-0.305664241000017));
#264410=CARTESIAN_POINT('Ctrl Pts',(-10.4593678150001,11.6,-0.305664241000017));
#264411=CARTESIAN_POINT('Ctrl Pts',(-10.4608825450001,15.2,-0.305948928000017));
#264412=CARTESIAN_POINT('Ctrl Pts',(-10.4608825450001,11.6,-0.305948928000018));
#264413=CARTESIAN_POINT('Ctrl Pts',(-10.4624048670001,15.2,-0.306236531000015));
#264414=CARTESIAN_POINT('Ctrl Pts',(-10.4624048670001,11.6,-0.306236531000015));
#264415=CARTESIAN_POINT('Ctrl Pts',(-10.4639347550001,15.2,-0.306527058000015));
#264416=CARTESIAN_POINT('Ctrl Pts',(-10.4639347550001,11.6,-0.306527058000015));
#264417=CARTESIAN_POINT('Ctrl Pts',(-10.4654721910001,15.2,-0.306820521000013));
#264418=CARTESIAN_POINT('Ctrl Pts',(-10.4654721910001,11.6,-0.306820521000013));
#264419=CARTESIAN_POINT('Ctrl Pts',(-10.4670171510001,15.2,-0.307116929000015));
#264420=CARTESIAN_POINT('Ctrl Pts',(-10.4670171510001,11.6,-0.307116929000016));
#264421=CARTESIAN_POINT('Ctrl Pts',(-10.4685696160001,15.2,-0.307416292000013));
#264422=CARTESIAN_POINT('Ctrl Pts',(-10.4685696160001,11.6,-0.307416292000014));
#264423=CARTESIAN_POINT('Ctrl Pts',(-10.4701295620001,15.2,-0.307718619000017));
#264424=CARTESIAN_POINT('Ctrl Pts',(-10.4701295620001,11.6,-0.307718619000017));
#264425=CARTESIAN_POINT('Ctrl Pts',(-10.4716969700001,15.2,-0.308023923000014));
#264426=CARTESIAN_POINT('Ctrl Pts',(-10.4716969700001,11.6,-0.308023923000014));
#264427=CARTESIAN_POINT('Ctrl Pts',(-10.4732718190001,15.2,-0.308332210000017));
#264428=CARTESIAN_POINT('Ctrl Pts',(-10.4732718190001,11.6,-0.308332210000018));
#264429=CARTESIAN_POINT('Ctrl Pts',(-10.4748540860001,15.2,-0.308643492000016));
#264430=CARTESIAN_POINT('Ctrl Pts',(-10.4748540860001,11.6,-0.308643492000016));
#264431=CARTESIAN_POINT('Ctrl Pts',(-10.4764437530001,15.2,-0.308957777000014));
#264432=CARTESIAN_POINT('Ctrl Pts',(-10.4764437530001,11.6,-0.308957777000014));
#264433=CARTESIAN_POINT('Ctrl Pts',(-10.4780407970001,15.2,-0.309275076000013));
#264434=CARTESIAN_POINT('Ctrl Pts',(-10.4780407970001,11.6,-0.309275076000013));
#264435=CARTESIAN_POINT('Ctrl Pts',(-10.4796451980001,15.2,-0.309595399000013));
#264436=CARTESIAN_POINT('Ctrl Pts',(-10.4796451980001,11.6,-0.309595399000014));
#264437=CARTESIAN_POINT('Ctrl Pts',(-10.4812569350001,15.2,-0.309918754000016));
#264438=CARTESIAN_POINT('Ctrl Pts',(-10.4812569350001,11.6,-0.309918754000016));
#264439=CARTESIAN_POINT('Ctrl Pts',(-10.4828759870001,15.2,-0.310245152000017));
#264440=CARTESIAN_POINT('Ctrl Pts',(-10.4828759870001,11.6,-0.310245152000018));
#264441=CARTESIAN_POINT('Ctrl Pts',(-10.4845023350001,15.2,-0.310574602000013));
#264442=CARTESIAN_POINT('Ctrl Pts',(-10.4845023350001,11.6,-0.310574602000014));
#264443=CARTESIAN_POINT('Ctrl Pts',(-10.4861359570001,15.2,-0.310907114000014));
#264444=CARTESIAN_POINT('Ctrl Pts',(-10.4861359570001,11.6,-0.310907114000015));
#264445=CARTESIAN_POINT('Ctrl Pts',(-10.4877768330001,15.2,-0.311242696000011));
#264446=CARTESIAN_POINT('Ctrl Pts',(-10.4877768330001,11.6,-0.311242696000012));
#264447=CARTESIAN_POINT('Ctrl Pts',(-10.4894249420001,15.2,-0.311581357000015));
#264448=CARTESIAN_POINT('Ctrl Pts',(-10.4894249420001,11.6,-0.311581357000015));
#264449=CARTESIAN_POINT('Ctrl Pts',(-10.4910802660001,15.2,-0.311923107000016));
#264450=CARTESIAN_POINT('Ctrl Pts',(-10.4910802660001,11.6,-0.311923107000017));
#264451=CARTESIAN_POINT('Ctrl Pts',(-10.4927427830001,15.2,-0.312267956000016));
#264452=CARTESIAN_POINT('Ctrl Pts',(-10.4927427830001,11.6,-0.312267956000017));
#264453=CARTESIAN_POINT('Ctrl Pts',(-10.4944124730001,15.2,-0.312615913000016));
#264454=CARTESIAN_POINT('Ctrl Pts',(-10.4944124730001,11.6,-0.312615913000017));
#264455=CARTESIAN_POINT('Ctrl Pts',(-10.4960893160001,15.2,-0.312966987000016));
#264456=CARTESIAN_POINT('Ctrl Pts',(-10.4960893160001,11.6,-0.312966987000017));
#264457=CARTESIAN_POINT('Ctrl Pts',(-10.4977732930001,15.2,-0.313321185000017));
#264458=CARTESIAN_POINT('Ctrl Pts',(-10.4977732930001,11.6,-0.313321185000018));
#264459=CARTESIAN_POINT('Ctrl Pts',(-10.4994643820001,15.2,-0.313678519000016));
#264460=CARTESIAN_POINT('Ctrl Pts',(-10.4994643820001,11.6,-0.313678519000016));
#264461=CARTESIAN_POINT('Ctrl Pts',(-10.5011625650001,15.2,-0.314038997000012));
#264462=CARTESIAN_POINT('Ctrl Pts',(-10.5011625650001,11.6,-0.314038997000013));
#264463=CARTESIAN_POINT('Ctrl Pts',(-10.5028678220001,15.2,-0.314402627000017));
#264464=CARTESIAN_POINT('Ctrl Pts',(-10.5028678220001,11.6,-0.314402627000017));
#264465=CARTESIAN_POINT('Ctrl Pts',(-10.5045801340001,15.2,-0.314769419000012));
#264466=CARTESIAN_POINT('Ctrl Pts',(-10.5045801340001,11.6,-0.314769419000012));
#264467=CARTESIAN_POINT('Ctrl Pts',(-10.5062994780001,15.2,-0.315139382000016));
#264468=CARTESIAN_POINT('Ctrl Pts',(-10.5062994780001,11.6,-0.315139382000016));
#264469=CARTESIAN_POINT('Ctrl Pts',(-10.5080258380001,15.2,-0.315512524000017));
#264470=CARTESIAN_POINT('Ctrl Pts',(-10.5080258380001,11.6,-0.315512524000017));
#264471=CARTESIAN_POINT('Ctrl Pts',(-10.5097591940001,15.2,-0.315888854000015));
#264472=CARTESIAN_POINT('Ctrl Pts',(-10.5097591940001,11.6,-0.315888854000015));
#264473=CARTESIAN_POINT('Ctrl Pts',(-10.5114995250001,15.2,-0.316268381000011));
#264474=CARTESIAN_POINT('Ctrl Pts',(-10.5114995250001,11.6,-0.316268381000012));
#264475=CARTESIAN_POINT('Ctrl Pts',(-10.5132468120001,15.2,-0.316651113000015));
#264476=CARTESIAN_POINT('Ctrl Pts',(-10.5132468120001,11.6,-0.316651113000015));
#264477=CARTESIAN_POINT('Ctrl Pts',(-10.5150010370001,15.2,-0.317037060000014));
#264478=CARTESIAN_POINT('Ctrl Pts',(-10.5150010370001,11.6,-0.317037060000014));
#264479=CARTESIAN_POINT('Ctrl Pts',(-10.5167621800001,15.2,-0.317426229000013));
#264480=CARTESIAN_POINT('Ctrl Pts',(-10.5167621800001,11.6,-0.317426229000013));
#264481=CARTESIAN_POINT('Ctrl Pts',(-10.5185302210001,15.2,-0.317818628000013));
#264482=CARTESIAN_POINT('Ctrl Pts',(-10.5185302210001,11.6,-0.317818628000013));
#264483=CARTESIAN_POINT('Ctrl Pts',(-10.5203051430001,15.2,-0.318214269000014));
#264484=CARTESIAN_POINT('Ctrl Pts',(-10.5203051430001,11.6,-0.318214269000015));
#264485=CARTESIAN_POINT('Ctrl Pts',(-10.5220869250001,15.2,-0.318613157000014));
#264486=CARTESIAN_POINT('Ctrl Pts',(-10.5220869250001,11.6,-0.318613157000014));
#264487=CARTESIAN_POINT('Ctrl Pts',(-10.5238755480001,15.2,-0.319015302000012));
#264488=CARTESIAN_POINT('Ctrl Pts',(-10.5238755480001,11.6,-0.319015302000012));
#264489=CARTESIAN_POINT('Ctrl Pts',(-10.5256709940001,15.2,-0.319420713000014));
#264490=CARTESIAN_POINT('Ctrl Pts',(-10.5256709940001,11.6,-0.319420713000014));
#264491=CARTESIAN_POINT('Ctrl Pts',(-10.5274732440001,15.2,-0.319829396000015));
#264492=CARTESIAN_POINT('Ctrl Pts',(-10.5274732440001,11.6,-0.319829396000016));
#264493=CARTESIAN_POINT('Ctrl Pts',(-10.5292822790001,15.2,-0.320241361000013));
#264494=CARTESIAN_POINT('Ctrl Pts',(-10.5292822790001,11.6,-0.320241361000014));
#264495=CARTESIAN_POINT('Ctrl Pts',(-10.5310980810001,15.2,-0.320656616000012));
#264496=CARTESIAN_POINT('Ctrl Pts',(-10.5310980810001,11.6,-0.320656616000013));
#264497=CARTESIAN_POINT('Ctrl Pts',(-10.5329206290001,15.2,-0.321075169000018));
#264498=CARTESIAN_POINT('Ctrl Pts',(-10.5329206290001,11.6,-0.321075169000018));
#264499=CARTESIAN_POINT('Ctrl Pts',(-10.5347499080001,15.2,-0.321497029000017));
#264500=CARTESIAN_POINT('Ctrl Pts',(-10.5347499080001,11.6,-0.321497029000018));
#264501=CARTESIAN_POINT('Ctrl Pts',(-10.5365858960001,15.2,-0.321922203000016));
#264502=CARTESIAN_POINT('Ctrl Pts',(-10.5365858960001,11.6,-0.321922203000016));
#264503=CARTESIAN_POINT('Ctrl Pts',(-10.5384285770001,15.2,-0.322350700000014));
#264504=CARTESIAN_POINT('Ctrl Pts',(-10.5384285770001,11.6,-0.322350700000014));
#264505=CARTESIAN_POINT('Ctrl Pts',(-10.5402779310001,15.2,-0.322782527000012));
#264506=CARTESIAN_POINT('Ctrl Pts',(-10.5402779310001,11.6,-0.322782527000012));
#264507=CARTESIAN_POINT('Ctrl Pts',(-10.5421339400001,15.2,-0.323217694000015));
#264508=CARTESIAN_POINT('Ctrl Pts',(-10.5421339400001,11.6,-0.323217694000016));
#264509=CARTESIAN_POINT('Ctrl Pts',(-10.5439965860001,15.2,-0.323656207000016));
#264510=CARTESIAN_POINT('Ctrl Pts',(-10.5439965860001,11.6,-0.323656207000016));
#264511=CARTESIAN_POINT('Ctrl Pts',(-10.5458658520001,15.2,-0.324098074000014));
#264512=CARTESIAN_POINT('Ctrl Pts',(-10.5458658520001,11.6,-0.324098074000015));
#264513=CARTESIAN_POINT('Ctrl Pts',(-10.5477417170001,15.2,-0.324543305000016));
#264514=CARTESIAN_POINT('Ctrl Pts',(-10.5477417170001,11.6,-0.324543305000016));
#264515=CARTESIAN_POINT('Ctrl Pts',(-10.5496241650001,15.2,-0.324991905000012));
#264516=CARTESIAN_POINT('Ctrl Pts',(-10.5496241650001,11.6,-0.324991905000012));
#264517=CARTESIAN_POINT('Ctrl Pts',(-10.5515131770001,15.2,-0.325443883000016));
#264518=CARTESIAN_POINT('Ctrl Pts',(-10.5515131770001,11.6,-0.325443883000017));
#264519=CARTESIAN_POINT('Ctrl Pts',(-10.5534087350001,15.2,-0.325899248000017));
#264520=CARTESIAN_POINT('Ctrl Pts',(-10.5534087350001,11.6,-0.325899248000017));
#264521=CARTESIAN_POINT('Ctrl Pts',(-10.5553108210001,15.2,-0.326358007000014));
#264522=CARTESIAN_POINT('Ctrl Pts',(-10.5553108210001,11.6,-0.326358007000014));
#264523=CARTESIAN_POINT('Ctrl Pts',(-10.5572194180001,15.2,-0.326820167000013));
#264524=CARTESIAN_POINT('Ctrl Pts',(-10.5572194180001,11.6,-0.326820167000013));
#264525=CARTESIAN_POINT('Ctrl Pts',(-10.5591345070001,15.2,-0.327285736000014));
#264526=CARTESIAN_POINT('Ctrl Pts',(-10.5591345070001,11.6,-0.327285736000014));
#264527=CARTESIAN_POINT('Ctrl Pts',(-10.5610560710001,15.2,-0.327754722000013));
#264528=CARTESIAN_POINT('Ctrl Pts',(-10.5610560710001,11.6,-0.327754722000014));
#264529=CARTESIAN_POINT('Ctrl Pts',(-10.5629840910001,15.2,-0.328227133000016));
#264530=CARTESIAN_POINT('Ctrl Pts',(-10.5629840910001,11.6,-0.328227133000017));
#264531=CARTESIAN_POINT('Ctrl Pts',(-10.5649185510001,15.2,-0.328702975000015));
#264532=CARTESIAN_POINT('Ctrl Pts',(-10.5649185510001,11.6,-0.328702975000015));
#264533=CARTESIAN_POINT('Ctrl Pts',(-10.5668594320001,15.2,-0.329182256000013));
#264534=CARTESIAN_POINT('Ctrl Pts',(-10.5668594320001,11.6,-0.329182256000014));
#264535=CARTESIAN_POINT('Ctrl Pts',(-10.5688067180001,15.2,-0.329664985000013));
#264536=CARTESIAN_POINT('Ctrl Pts',(-10.5688067180001,11.6,-0.329664985000014));
#264537=CARTESIAN_POINT('Ctrl Pts',(-10.5707603900001,15.2,-0.330151169000015));
#264538=CARTESIAN_POINT('Ctrl Pts',(-10.5707603900001,11.6,-0.330151169000015));
#264539=CARTESIAN_POINT('Ctrl Pts',(-10.5727204310001,15.2,-0.330640814000014));
#264540=CARTESIAN_POINT('Ctrl Pts',(-10.5727204310001,11.6,-0.330640814000014));
#264541=CARTESIAN_POINT('Ctrl Pts',(-10.5746868240001,15.2,-0.331133928000016));
#264542=CARTESIAN_POINT('Ctrl Pts',(-10.5746868240001,11.6,-0.331133928000016));
#264543=CARTESIAN_POINT('Ctrl Pts',(-10.5766595510001,15.2,-0.331630519000012));
#264544=CARTESIAN_POINT('Ctrl Pts',(-10.5766595510001,11.6,-0.331630519000013));
#264545=CARTESIAN_POINT('Ctrl Pts',(-10.5786385950001,15.2,-0.332130595000013));
#264546=CARTESIAN_POINT('Ctrl Pts',(-10.5786385950001,11.6,-0.332130595000014));
#264547=CARTESIAN_POINT('Ctrl Pts',(-10.5806239380001,15.2,-0.332634161000014));
#264548=CARTESIAN_POINT('Ctrl Pts',(-10.5806239380001,11.6,-0.332634161000014));
#264549=CARTESIAN_POINT('Ctrl Pts',(-10.5826155640001,15.2,-0.333141226000016));
#264550=CARTESIAN_POINT('Ctrl Pts',(-10.5826155640001,11.6,-0.333141226000016));
#264551=CARTESIAN_POINT('Ctrl Pts',(-10.5846134550001,15.2,-0.333651796000014));
#264552=CARTESIAN_POINT('Ctrl Pts',(-10.5846134550001,11.6,-0.333651796000014));
#264553=CARTESIAN_POINT('Ctrl Pts',(-10.5866175950001,15.2,-0.334165879000015));
#264554=CARTESIAN_POINT('Ctrl Pts',(-10.5866175950001,11.6,-0.334165879000015));
#264555=CARTESIAN_POINT('Ctrl Pts',(-10.5886279650001,15.2,-0.334683483000013));
#264556=CARTESIAN_POINT('Ctrl Pts',(-10.5886279650001,11.6,-0.334683483000014));
#264557=CARTESIAN_POINT('Ctrl Pts',(-10.5906445490001,15.2,-0.335204613000015));
#264558=CARTESIAN_POINT('Ctrl Pts',(-10.5906445490001,11.6,-0.335204613000016));
#264559=CARTESIAN_POINT('Ctrl Pts',(-10.5926673320001,15.2,-0.335729278000017));
#264560=CARTESIAN_POINT('Ctrl Pts',(-10.5926673320001,11.6,-0.335729278000017));
#264561=CARTESIAN_POINT('Ctrl Pts',(-10.5946962940001,15.2,-0.336257483000013));
#264562=CARTESIAN_POINT('Ctrl Pts',(-10.5946962940001,11.6,-0.336257483000014));
#264563=CARTESIAN_POINT('Ctrl Pts',(-10.5967314190001,15.2,-0.336789237000015));
#264564=CARTESIAN_POINT('Ctrl Pts',(-10.5967314190001,11.6,-0.336789237000015));
#264565=CARTESIAN_POINT('Ctrl Pts',(-10.5987726910001,15.2,-0.337324546000013));
#264566=CARTESIAN_POINT('Ctrl Pts',(-10.5987726910001,11.6,-0.337324546000013));
#264567=CARTESIAN_POINT('Ctrl Pts',(-10.6008200940001,15.2,-0.337863418000013));
#264568=CARTESIAN_POINT('Ctrl Pts',(-10.6008200940001,11.6,-0.337863418000013));
#264569=CARTESIAN_POINT('Ctrl Pts',(-10.6028736090001,15.2,-0.338405859000015));
#264570=CARTESIAN_POINT('Ctrl Pts',(-10.6028736090001,11.6,-0.338405859000015));
#264571=CARTESIAN_POINT('Ctrl Pts',(-10.6049332210001,15.2,-0.338951874000015));
#264572=CARTESIAN_POINT('Ctrl Pts',(-10.6049332210001,11.6,-0.338951874000016));
#264573=CARTESIAN_POINT('Ctrl Pts',(-10.6069989120001,15.2,-0.339501473000015));
#264574=CARTESIAN_POINT('Ctrl Pts',(-10.6069989120001,11.6,-0.339501473000015));
#264575=CARTESIAN_POINT('Ctrl Pts',(-10.6090706680001,15.2,-0.340054662000018));
#264576=CARTESIAN_POINT('Ctrl Pts',(-10.6090706680001,11.6,-0.340054662000018));
#264577=CARTESIAN_POINT('Ctrl Pts',(-10.6111484700001,15.2,-0.340611447000012));
#264578=CARTESIAN_POINT('Ctrl Pts',(-10.6111484700001,11.6,-0.340611447000013));
#264579=CARTESIAN_POINT('Ctrl Pts',(-10.6132323020001,15.2,-0.341171835000011));
#264580=CARTESIAN_POINT('Ctrl Pts',(-10.6132323020001,11.6,-0.341171835000012));
#264581=CARTESIAN_POINT('Ctrl Pts',(-10.6153221490001,15.2,-0.341735833000012));
#264582=CARTESIAN_POINT('Ctrl Pts',(-10.6153221490001,11.6,-0.341735833000012));
#264583=CARTESIAN_POINT('Ctrl Pts',(-10.6174179920001,15.2,-0.342303448000014));
#264584=CARTESIAN_POINT('Ctrl Pts',(-10.6174179920001,11.6,-0.342303448000015));
#264585=CARTESIAN_POINT('Ctrl Pts',(-10.6195198180001,15.2,-0.342874685000014));
#264586=CARTESIAN_POINT('Ctrl Pts',(-10.6195198180001,11.6,-0.342874685000015));
#264587=CARTESIAN_POINT('Ctrl Pts',(-10.6216276080001,15.2,-0.343449552000017));
#264588=CARTESIAN_POINT('Ctrl Pts',(-10.6216276080001,11.6,-0.343449552000017));
#264589=CARTESIAN_POINT('Ctrl Pts',(-10.6237413470001,15.2,-0.344028056000014));
#264590=CARTESIAN_POINT('Ctrl Pts',(-10.6237413470001,11.6,-0.344028056000015));
#264591=CARTESIAN_POINT('Ctrl Pts',(-10.6258610180001,15.2,-0.344610202000015));
#264592=CARTESIAN_POINT('Ctrl Pts',(-10.6258610180001,11.6,-0.344610202000016));
#264593=CARTESIAN_POINT('Ctrl Pts',(-10.6279866070001,15.2,-0.345195998000012));
#264594=CARTESIAN_POINT('Ctrl Pts',(-10.6279866070001,11.6,-0.345195998000012));
#264595=CARTESIAN_POINT('Ctrl Pts',(-10.6301180950001,15.2,-0.345785450000013));
#264596=CARTESIAN_POINT('Ctrl Pts',(-10.6301180950001,11.6,-0.345785450000014));
#264597=CARTESIAN_POINT('Ctrl Pts',(-10.6322554680001,15.2,-0.346378564000016));
#264598=CARTESIAN_POINT('Ctrl Pts',(-10.6322554680001,11.6,-0.346378564000017));
#264599=CARTESIAN_POINT('Ctrl Pts',(-10.6343987090001,15.2,-0.346975347000011));
#264600=CARTESIAN_POINT('Ctrl Pts',(-10.6343987090001,11.6,-0.346975347000012));
#264601=CARTESIAN_POINT('Ctrl Pts',(-10.6365478020001,15.2,-0.347575805000013));
#264602=CARTESIAN_POINT('Ctrl Pts',(-10.6365478020001,11.6,-0.347575805000014));
#264603=CARTESIAN_POINT('Ctrl Pts',(-10.6387027320001,15.2,-0.348179945000013));
#264604=CARTESIAN_POINT('Ctrl Pts',(-10.6387027320001,11.6,-0.348179945000014));
#264605=CARTESIAN_POINT('Ctrl Pts',(-10.6408634830001,15.2,-0.348787773000012));
#264606=CARTESIAN_POINT('Ctrl Pts',(-10.6408634830001,11.6,-0.348787773000013));
#264607=CARTESIAN_POINT('Ctrl Pts',(-10.6430300390001,15.2,-0.349399295000015));
#264608=CARTESIAN_POINT('Ctrl Pts',(-10.6430300390001,11.6,-0.349399295000015));
#264609=CARTESIAN_POINT('Ctrl Pts',(-10.6452023830001,15.2,-0.350014516000012));
#264610=CARTESIAN_POINT('Ctrl Pts',(-10.6452023830001,11.6,-0.350014516000013));
#264611=CARTESIAN_POINT('Ctrl Pts',(-10.6473805010001,15.2,-0.350633446000015));
#264612=CARTESIAN_POINT('Ctrl Pts',(-10.6473805010001,11.6,-0.350633446000015));
#264613=CARTESIAN_POINT('Ctrl Pts',(-10.6495643770001,15.2,-0.351256088000014));
#264614=CARTESIAN_POINT('Ctrl Pts',(-10.6495643770001,11.6,-0.351256088000014));
#264615=CARTESIAN_POINT('Ctrl Pts',(-10.6517539940001,15.2,-0.351882449000014));
#264616=CARTESIAN_POINT('Ctrl Pts',(-10.6517539940001,11.6,-0.351882449000014));
#264617=CARTESIAN_POINT('Ctrl Pts',(-10.6539493380001,15.2,-0.352512536000016));
#264618=CARTESIAN_POINT('Ctrl Pts',(-10.6539493380001,11.6,-0.352512536000016));
#264619=CARTESIAN_POINT('Ctrl Pts',(-10.6561503920001,15.2,-0.353146354000016));
#264620=CARTESIAN_POINT('Ctrl Pts',(-10.6561503920001,11.6,-0.353146354000016));
#264621=CARTESIAN_POINT('Ctrl Pts',(-10.6583571410001,15.2,-0.353783910000014));
#264622=CARTESIAN_POINT('Ctrl Pts',(-10.6583571410001,11.6,-0.353783910000014));
#264623=CARTESIAN_POINT('Ctrl Pts',(-10.6605695710001,15.2,-0.354425210000016));
#264624=CARTESIAN_POINT('Ctrl Pts',(-10.6605695710001,11.6,-0.354425210000016));
#264625=CARTESIAN_POINT('Ctrl Pts',(-10.6627876650001,15.2,-0.355070259000012));
#264626=CARTESIAN_POINT('Ctrl Pts',(-10.6627876650001,11.6,-0.355070259000013));
#264627=CARTESIAN_POINT('Ctrl Pts',(-10.6650114070001,15.2,-0.355719063000013));
#264628=CARTESIAN_POINT('Ctrl Pts',(-10.6650114070001,11.6,-0.355719063000013));
#264629=CARTESIAN_POINT('Ctrl Pts',(-10.6672407830001,15.2,-0.356371629000014));
#264630=CARTESIAN_POINT('Ctrl Pts',(-10.6672407830001,11.6,-0.356371629000015));
#264631=CARTESIAN_POINT('Ctrl Pts',(-10.6694757780001,15.2,-0.357027964000016));
#264632=CARTESIAN_POINT('Ctrl Pts',(-10.6694757780001,11.6,-0.357027964000017));
#264633=CARTESIAN_POINT('Ctrl Pts',(-10.6717163760001,15.2,-0.357688071000015));
#264634=CARTESIAN_POINT('Ctrl Pts',(-10.6717163760001,11.6,-0.357688071000016));
#264635=CARTESIAN_POINT('Ctrl Pts',(-10.6739625620001,15.2,-0.358351959000016));
#264636=CARTESIAN_POINT('Ctrl Pts',(-10.6739625620001,11.6,-0.358351959000017));
#264637=CARTESIAN_POINT('Ctrl Pts',(-10.6762143200001,15.2,-0.359019631000015));
#264638=CARTESIAN_POINT('Ctrl Pts',(-10.6762143200001,11.6,-0.359019631000015));
#264639=CARTESIAN_POINT('Ctrl Pts',(-10.6784716350001,15.2,-0.359691096000017));
#264640=CARTESIAN_POINT('Ctrl Pts',(-10.6784716350001,11.6,-0.359691096000017));
#264641=CARTESIAN_POINT('Ctrl Pts',(-10.6807344940001,15.2,-0.360366356000017));
#264642=CARTESIAN_POINT('Ctrl Pts',(-10.6807344940001,11.6,-0.360366356000017));
#264643=CARTESIAN_POINT('Ctrl Pts',(-10.6830028780001,15.2,-0.361045420000017));
#264644=CARTESIAN_POINT('Ctrl Pts',(-10.6830028780001,11.6,-0.361045420000017));
#264645=CARTESIAN_POINT('Ctrl Pts',(-10.6852767760001,15.2,-0.361728293000017));
#264646=CARTESIAN_POINT('Ctrl Pts',(-10.6852767760001,11.6,-0.361728293000017));
#264647=CARTESIAN_POINT('Ctrl Pts',(-10.6875561710001,15.2,-0.362414981000012));
#264648=CARTESIAN_POINT('Ctrl Pts',(-10.6875561710001,11.6,-0.362414981000013));
#264649=CARTESIAN_POINT('Ctrl Pts',(-10.6898410480001,15.2,-0.363105487000013));
#264650=CARTESIAN_POINT('Ctrl Pts',(-10.6898410480001,11.6,-0.363105487000013));
#264651=CARTESIAN_POINT('Ctrl Pts',(-10.6921313930001,15.2,-0.363799821000015));
#264652=CARTESIAN_POINT('Ctrl Pts',(-10.6921313930001,11.6,-0.363799821000015));
#264653=CARTESIAN_POINT('Ctrl Pts',(-10.6944271900001,15.2,-0.364497985000014));
#264654=CARTESIAN_POINT('Ctrl Pts',(-10.6944271900001,11.6,-0.364497985000015));
#264655=CARTESIAN_POINT('Ctrl Pts',(-10.6967284250001,15.2,-0.365199987000011));
#264656=CARTESIAN_POINT('Ctrl Pts',(-10.6967284250001,11.6,-0.365199987000012));
#264657=CARTESIAN_POINT('Ctrl Pts',(-10.6990350820001,15.2,-0.365905831000015));
#264658=CARTESIAN_POINT('Ctrl Pts',(-10.6990350820001,11.6,-0.365905831000016));
#264659=CARTESIAN_POINT('Ctrl Pts',(-10.7013471480001,15.2,-0.366615523000018));
#264660=CARTESIAN_POINT('Ctrl Pts',(-10.7013471480001,11.6,-0.366615523000018));
#264661=CARTESIAN_POINT('Ctrl Pts',(-10.7036646080001,15.2,-0.367329069000015));
#264662=CARTESIAN_POINT('Ctrl Pts',(-10.7036646080001,11.6,-0.367329069000016));
#264663=CARTESIAN_POINT('Ctrl Pts',(-10.7059874460001,15.2,-0.368046475000017));
#264664=CARTESIAN_POINT('Ctrl Pts',(-10.7059874460001,11.6,-0.368046475000017));
#264665=CARTESIAN_POINT('Ctrl Pts',(-10.7083156480001,15.2,-0.368767746000014));
#264666=CARTESIAN_POINT('Ctrl Pts',(-10.7083156480001,11.6,-0.368767746000014));
#264667=CARTESIAN_POINT('Ctrl Pts',(-10.7106492000001,15.2,-0.369492887000016));
#264668=CARTESIAN_POINT('Ctrl Pts',(-10.7106492000001,11.6,-0.369492887000016));
#264669=CARTESIAN_POINT('Ctrl Pts',(-10.7129880860001,15.2,-0.370221904000014));
#264670=CARTESIAN_POINT('Ctrl Pts',(-10.7129880860001,11.6,-0.370221904000015));
#264671=CARTESIAN_POINT('Ctrl Pts',(-10.7153322940001,15.2,-0.370954801000014));
#264672=CARTESIAN_POINT('Ctrl Pts',(-10.7153322940001,11.6,-0.370954801000015));
#264673=CARTESIAN_POINT('Ctrl Pts',(-10.7176818070001,15.2,-0.371691587000011));
#264674=CARTESIAN_POINT('Ctrl Pts',(-10.7176818070001,11.6,-0.371691587000012));
#264675=CARTESIAN_POINT('Ctrl Pts',(-10.7200366120001,15.2,-0.372432264000011));
#264676=CARTESIAN_POINT('Ctrl Pts',(-10.7200366120001,11.6,-0.372432264000012));
#264677=CARTESIAN_POINT('Ctrl Pts',(-10.7223966940001,15.2,-0.373176838000013));
#264678=CARTESIAN_POINT('Ctrl Pts',(-10.7223966940001,11.6,-0.373176838000014));
#264679=CARTESIAN_POINT('Ctrl Pts',(-10.7247620380001,15.2,-0.373925315000014));
#264680=CARTESIAN_POINT('Ctrl Pts',(-10.7247620380001,11.6,-0.373925315000015));
#264681=CARTESIAN_POINT('Ctrl Pts',(-10.7271326310001,15.2,-0.374677700000015));
#264682=CARTESIAN_POINT('Ctrl Pts',(-10.7271326310001,11.6,-0.374677700000015));
#264683=CARTESIAN_POINT('Ctrl Pts',(-10.7295084580001,15.2,-0.375433998000014));
#264684=CARTESIAN_POINT('Ctrl Pts',(-10.7295084580001,11.6,-0.375433998000015));
#264685=CARTESIAN_POINT('Ctrl Pts',(-10.7318895040001,15.2,-0.376194215000014));
#264686=CARTESIAN_POINT('Ctrl Pts',(-10.7318895040001,11.6,-0.376194215000015));
#264687=CARTESIAN_POINT('Ctrl Pts',(-10.7342757570001,15.2,-0.376958356000014));
#264688=CARTESIAN_POINT('Ctrl Pts',(-10.7342757570001,11.6,-0.376958356000015));
#264689=CARTESIAN_POINT('Ctrl Pts',(-10.7366672000001,15.2,-0.377726425000016));
#264690=CARTESIAN_POINT('Ctrl Pts',(-10.7366672000001,11.6,-0.377726425000016));
#264691=CARTESIAN_POINT('Ctrl Pts',(-10.7390638200001,15.2,-0.378498429000014));
#264692=CARTESIAN_POINT('Ctrl Pts',(-10.7390638200001,11.6,-0.378498429000014));
#264693=CARTESIAN_POINT('Ctrl Pts',(-10.7414656040001,15.2,-0.379274372000014));
#264694=CARTESIAN_POINT('Ctrl Pts',(-10.7414656040001,11.6,-0.379274372000014));
#264695=CARTESIAN_POINT('Ctrl Pts',(-10.7438725370001,15.2,-0.380054260000016));
#264696=CARTESIAN_POINT('Ctrl Pts',(-10.7438725370001,11.6,-0.380054260000016));
#264697=CARTESIAN_POINT('Ctrl Pts',(-10.7462846040001,15.2,-0.380838098000016));
#264698=CARTESIAN_POINT('Ctrl Pts',(-10.7462846040001,11.6,-0.380838098000016));
#264699=CARTESIAN_POINT('Ctrl Pts',(-10.7487017930001,15.2,-0.381625889000015));
#264700=CARTESIAN_POINT('Ctrl Pts',(-10.7487017930001,11.6,-0.381625889000015));
#264701=CARTESIAN_POINT('Ctrl Pts',(-10.7511240870001,15.2,-0.382417641000017));
#264702=CARTESIAN_POINT('Ctrl Pts',(-10.7511240870001,11.6,-0.382417641000017));
#264703=CARTESIAN_POINT('Ctrl Pts',(-10.7535514750001,15.2,-0.383213358000014));
#264704=CARTESIAN_POINT('Ctrl Pts',(-10.7535514750001,11.6,-0.383213358000015));
#264705=CARTESIAN_POINT('Ctrl Pts',(-10.7559839420001,15.2,-0.384013044000016));
#264706=CARTESIAN_POINT('Ctrl Pts',(-10.7559839420001,11.6,-0.384013044000016));
#264707=CARTESIAN_POINT('Ctrl Pts',(-10.7584214740001,15.2,-0.384816705000013));
#264708=CARTESIAN_POINT('Ctrl Pts',(-10.7584214740001,11.6,-0.384816705000013));
#264709=CARTESIAN_POINT('Ctrl Pts',(-10.7608640580001,15.2,-0.385624345000015));
#264710=CARTESIAN_POINT('Ctrl Pts',(-10.7608640580001,11.6,-0.385624345000016));
#264711=CARTESIAN_POINT('Ctrl Pts',(-10.7633116780001,15.2,-0.386435971000014));
#264712=CARTESIAN_POINT('Ctrl Pts',(-10.7633116780001,11.6,-0.386435971000015));
#264713=CARTESIAN_POINT('Ctrl Pts',(-10.7657643230001,15.2,-0.387251586000015));
#264714=CARTESIAN_POINT('Ctrl Pts',(-10.7657643230001,11.6,-0.387251586000015));
#264715=CARTESIAN_POINT('Ctrl Pts',(-10.7682219760001,15.2,-0.388071196000013));
#264716=CARTESIAN_POINT('Ctrl Pts',(-10.7682219760001,11.6,-0.388071196000013));
#264717=CARTESIAN_POINT('Ctrl Pts',(-10.7706846260001,15.2,-0.388894805000017));
#264718=CARTESIAN_POINT('Ctrl Pts',(-10.7706846260001,11.6,-0.388894805000018));
#264719=CARTESIAN_POINT('Ctrl Pts',(-10.7731522590001,15.2,-0.389722418000016));
#264720=CARTESIAN_POINT('Ctrl Pts',(-10.7731522590001,11.6,-0.389722418000016));
#264721=CARTESIAN_POINT('Ctrl Pts',(-10.7756248610001,15.2,-0.390554041000013));
#264722=CARTESIAN_POINT('Ctrl Pts',(-10.7756248610001,11.6,-0.390554041000013));
#264723=CARTESIAN_POINT('Ctrl Pts',(-10.7781024170001,15.2,-0.391389677000014));
#264724=CARTESIAN_POINT('Ctrl Pts',(-10.7781024170001,11.6,-0.391389677000014));
#264725=CARTESIAN_POINT('Ctrl Pts',(-10.7805849160001,15.2,-0.392229332000014));
#264726=CARTESIAN_POINT('Ctrl Pts',(-10.7805849160001,11.6,-0.392229332000014));
#264727=CARTESIAN_POINT('Ctrl Pts',(-10.7830723410001,15.2,-0.393073009000013));
#264728=CARTESIAN_POINT('Ctrl Pts',(-10.7830723410001,11.6,-0.393073009000014));
#264729=CARTESIAN_POINT('Ctrl Pts',(-10.7855646820001,15.2,-0.393920716000018));
#264730=CARTESIAN_POINT('Ctrl Pts',(-10.7855646820001,11.6,-0.393920716000018));
#264731=CARTESIAN_POINT('Ctrl Pts',(-10.7880619230001,15.2,-0.394772456000014));
#264732=CARTESIAN_POINT('Ctrl Pts',(-10.7880619230001,11.6,-0.394772456000015));
#264733=CARTESIAN_POINT('Ctrl Pts',(-10.7905640520001,15.2,-0.395628232000016));
#264734=CARTESIAN_POINT('Ctrl Pts',(-10.7905640520001,11.6,-0.395628232000016));
#264735=CARTESIAN_POINT('Ctrl Pts',(-10.7930710550001,15.2,-0.396488052000015));
#264736=CARTESIAN_POINT('Ctrl Pts',(-10.7930710550001,11.6,-0.396488052000015));
#264737=CARTESIAN_POINT('Ctrl Pts',(-10.7955829180001,15.2,-0.397351917000015));
#264738=CARTESIAN_POINT('Ctrl Pts',(-10.7955829180001,11.6,-0.397351917000015));
#264739=CARTESIAN_POINT('Ctrl Pts',(-10.7980996290001,15.2,-0.398219835000013));
#264740=CARTESIAN_POINT('Ctrl Pts',(-10.7980996290001,11.6,-0.398219835000014));
#264741=CARTESIAN_POINT('Ctrl Pts',(-10.8006211740001,15.2,-0.399091809000014));
#264742=CARTESIAN_POINT('Ctrl Pts',(-10.8006211740001,11.6,-0.399091809000014));
#264743=CARTESIAN_POINT('Ctrl Pts',(-10.8031475400001,15.2,-0.399967843000013));
#264744=CARTESIAN_POINT('Ctrl Pts',(-10.8031475400001,11.6,-0.399967843000014));
#264745=CARTESIAN_POINT('Ctrl Pts',(-10.8056787130001,15.2,-0.400847944000016));
#264746=CARTESIAN_POINT('Ctrl Pts',(-10.8056787130001,11.6,-0.400847944000016));
#264747=CARTESIAN_POINT('Ctrl Pts',(-10.8082146790001,15.2,-0.401732113000013));
#264748=CARTESIAN_POINT('Ctrl Pts',(-10.8082146790001,11.6,-0.401732113000013));
#264749=CARTESIAN_POINT('Ctrl Pts',(-10.8107554270001,15.2,-0.402620357000014));
#264750=CARTESIAN_POINT('Ctrl Pts',(-10.8107554270001,11.6,-0.402620357000015));
#264751=CARTESIAN_POINT('Ctrl Pts',(-10.8133009430001,15.2,-0.403512679000015));
#264752=CARTESIAN_POINT('Ctrl Pts',(-10.8133009430001,11.6,-0.403512679000016));
#264753=CARTESIAN_POINT('Ctrl Pts',(-10.8158512130001,15.2,-0.404409086000013));
#264754=CARTESIAN_POINT('Ctrl Pts',(-10.8158512130001,11.6,-0.404409086000013));
#264755=CARTESIAN_POINT('Ctrl Pts',(-10.8184062250001,15.2,-0.405309580000015));
#264756=CARTESIAN_POINT('Ctrl Pts',(-10.8184062250001,11.6,-0.405309580000015));
#264757=CARTESIAN_POINT('Ctrl Pts',(-10.8209659650001,15.2,-0.406214166000014));
#264758=CARTESIAN_POINT('Ctrl Pts',(-10.8209659650001,11.6,-0.406214166000014));
#264759=CARTESIAN_POINT('Ctrl Pts',(-10.8235304190001,15.2,-0.407122849000014));
#264760=CARTESIAN_POINT('Ctrl Pts',(-10.8235304190001,11.6,-0.407122849000015));
#264761=CARTESIAN_POINT('Ctrl Pts',(-10.8260995770001,15.2,-0.408035633000012));
#264762=CARTESIAN_POINT('Ctrl Pts',(-10.8260995770001,11.6,-0.408035633000013));
#264763=CARTESIAN_POINT('Ctrl Pts',(-10.8286734240001,15.2,-0.408952523000017));
#264764=CARTESIAN_POINT('Ctrl Pts',(-10.8286734240001,11.6,-0.408952523000017));
#264765=CARTESIAN_POINT('Ctrl Pts',(-10.8312519470001,15.2,-0.409873522000015));
#264766=CARTESIAN_POINT('Ctrl Pts',(-10.8312519470001,11.6,-0.409873522000015));
#264767=CARTESIAN_POINT('Ctrl Pts',(-10.8338351330001,15.2,-0.410798635000016));
#264768=CARTESIAN_POINT('Ctrl Pts',(-10.8338351330001,11.6,-0.410798635000016));
#264769=CARTESIAN_POINT('Ctrl Pts',(-10.8364229690001,15.2,-0.411727867000016));
#264770=CARTESIAN_POINT('Ctrl Pts',(-10.8364229690001,11.6,-0.411727867000016));
#264771=CARTESIAN_POINT('Ctrl Pts',(-10.8390154430001,15.2,-0.412661222000015));
#264772=CARTESIAN_POINT('Ctrl Pts',(-10.8390154430001,11.6,-0.412661222000015));
#264773=CARTESIAN_POINT('Ctrl Pts',(-10.8416125420001,15.2,-0.413598703000013));
#264774=CARTESIAN_POINT('Ctrl Pts',(-10.8416125420001,11.6,-0.413598703000014));
#264775=CARTESIAN_POINT('Ctrl Pts',(-10.8442142530001,15.2,-0.414540317000016));
#264776=CARTESIAN_POINT('Ctrl Pts',(-10.8442142530001,11.6,-0.414540317000017));
#264777=CARTESIAN_POINT('Ctrl Pts',(-10.8468205630001,15.2,-0.415486065000015));
#264778=CARTESIAN_POINT('Ctrl Pts',(-10.8468205630001,11.6,-0.415486065000015));
#264779=CARTESIAN_POINT('Ctrl Pts',(-10.8494314580001,15.2,-0.416435953000014));
#264780=CARTESIAN_POINT('Ctrl Pts',(-10.8494314580001,11.6,-0.416435953000014));
#264781=CARTESIAN_POINT('Ctrl Pts',(-10.8520469280001,15.2,-0.417389985000014));
#264782=CARTESIAN_POINT('Ctrl Pts',(-10.8520469280001,11.6,-0.417389985000014));
#264783=CARTESIAN_POINT('Ctrl Pts',(-10.8546669570001,15.2,-0.418348165000015));
#264784=CARTESIAN_POINT('Ctrl Pts',(-10.8546669570001,11.6,-0.418348165000016));
#264785=CARTESIAN_POINT('Ctrl Pts',(-10.8572915350001,15.2,-0.419310498000014));
#264786=CARTESIAN_POINT('Ctrl Pts',(-10.8572915350001,11.6,-0.419310498000014));
#264787=CARTESIAN_POINT('Ctrl Pts',(-10.8599206490001,15.2,-0.420276987000014));
#264788=CARTESIAN_POINT('Ctrl Pts',(-10.8599206490001,11.6,-0.420276987000015));
#264789=CARTESIAN_POINT('Ctrl Pts',(-10.8625542860001,15.2,-0.421247636000013));
#264790=CARTESIAN_POINT('Ctrl Pts',(-10.8625542860001,11.6,-0.421247636000013));
#264791=CARTESIAN_POINT('Ctrl Pts',(-10.8651924320001,15.2,-0.422222450000014));
#264792=CARTESIAN_POINT('Ctrl Pts',(-10.8651924320001,11.6,-0.422222450000014));
#264793=CARTESIAN_POINT('Ctrl Pts',(-10.8678350770001,15.2,-0.423201432000013));
#264794=CARTESIAN_POINT('Ctrl Pts',(-10.8678350770001,11.6,-0.423201432000014));
#264795=CARTESIAN_POINT('Ctrl Pts',(-10.8704822050001,15.2,-0.424184588000016));
#264796=CARTESIAN_POINT('Ctrl Pts',(-10.8704822050001,11.6,-0.424184588000017));
#264797=CARTESIAN_POINT('Ctrl Pts',(-10.8731338070001,15.2,-0.425171920000014));
#264798=CARTESIAN_POINT('Ctrl Pts',(-10.8731338070001,11.6,-0.425171920000014));
#264799=CARTESIAN_POINT('Ctrl Pts',(-10.8757898690001,15.2,-0.426163433000015));
#264800=CARTESIAN_POINT('Ctrl Pts',(-10.8757898690001,11.6,-0.426163433000016));
#264801=CARTESIAN_POINT('Ctrl Pts',(-10.8784503780001,15.2,-0.427159131000017));
#264802=CARTESIAN_POINT('Ctrl Pts',(-10.8784503780001,11.6,-0.427159131000017));
#264803=CARTESIAN_POINT('Ctrl Pts',(-10.8811153220001,15.2,-0.428159018000014));
#264804=CARTESIAN_POINT('Ctrl Pts',(-10.8811153220001,11.6,-0.428159018000014));
#264805=CARTESIAN_POINT('Ctrl Pts',(-10.8837846900001,15.2,-0.429163097000016));
#264806=CARTESIAN_POINT('Ctrl Pts',(-10.8837846900001,11.6,-0.429163097000016));
#264807=CARTESIAN_POINT('Ctrl Pts',(-10.8864584680001,15.2,-0.430171373000015));
#264808=CARTESIAN_POINT('Ctrl Pts',(-10.8864584680001,11.6,-0.430171373000015));
#264809=CARTESIAN_POINT('Ctrl Pts',(-10.8891366430001,15.2,-0.431183850000014));
#264810=CARTESIAN_POINT('Ctrl Pts',(-10.8891366430001,11.6,-0.431183850000015));
#264811=CARTESIAN_POINT('Ctrl Pts',(-10.8918192040001,15.2,-0.432200531000015));
#264812=CARTESIAN_POINT('Ctrl Pts',(-10.8918192040001,11.6,-0.432200531000016));
#264813=CARTESIAN_POINT('Ctrl Pts',(-10.8945061380001,15.2,-0.433221421000014));
#264814=CARTESIAN_POINT('Ctrl Pts',(-10.8945061380001,11.6,-0.433221421000014));
#264815=CARTESIAN_POINT('Ctrl Pts',(-10.8971974330001,15.2,-0.434246522000015));
#264816=CARTESIAN_POINT('Ctrl Pts',(-10.8971974330001,11.6,-0.434246522000015));
#264817=CARTESIAN_POINT('Ctrl Pts',(-10.8998930780001,15.2,-0.435275840000013));
#264818=CARTESIAN_POINT('Ctrl Pts',(-10.8998930780001,11.6,-0.435275840000014));
#264819=CARTESIAN_POINT('Ctrl Pts',(-10.9025930590001,15.2,-0.436309378000015));
#264820=CARTESIAN_POINT('Ctrl Pts',(-10.9025930590001,11.6,-0.436309378000015));
#264821=CARTESIAN_POINT('Ctrl Pts',(-10.9052973640001,15.2,-0.437347141000015));
#264822=CARTESIAN_POINT('Ctrl Pts',(-10.9052973640001,11.6,-0.437347141000016));
#264823=CARTESIAN_POINT('Ctrl Pts',(-10.9080059810001,15.2,-0.438389130000014));
#264824=CARTESIAN_POINT('Ctrl Pts',(-10.9080059810001,11.6,-0.438389130000015));
#264825=CARTESIAN_POINT('Ctrl Pts',(-10.9107188990001,15.2,-0.439435350000017));
#264826=CARTESIAN_POINT('Ctrl Pts',(-10.9107188990001,11.6,-0.439435350000017));
#264827=CARTESIAN_POINT('Ctrl Pts',(-10.9134361040001,15.2,-0.440485807000015));
#264828=CARTESIAN_POINT('Ctrl Pts',(-10.9134361040001,11.6,-0.440485807000015));
#264829=CARTESIAN_POINT('Ctrl Pts',(-10.9161575860001,15.2,-0.441540501000013));
#264830=CARTESIAN_POINT('Ctrl Pts',(-10.9161575860001,11.6,-0.441540501000013));
#264831=CARTESIAN_POINT('Ctrl Pts',(-10.9188833300001,15.2,-0.442599438000015));
#264832=CARTESIAN_POINT('Ctrl Pts',(-10.9188833300001,11.6,-0.442599438000016));
#264833=CARTESIAN_POINT('Ctrl Pts',(-10.9216133270001,15.2,-0.443662622000014));
#264834=CARTESIAN_POINT('Ctrl Pts',(-10.9216133270001,11.6,-0.443662622000014));
#264835=CARTESIAN_POINT('Ctrl Pts',(-10.9243475630001,15.2,-0.444730056000013));
#264836=CARTESIAN_POINT('Ctrl Pts',(-10.9243475630001,11.6,-0.444730056000014));
#264837=CARTESIAN_POINT('Ctrl Pts',(-10.9270860270001,15.2,-0.445801743000014));
#264838=CARTESIAN_POINT('Ctrl Pts',(-10.9270860270001,11.6,-0.445801743000014));
#264839=CARTESIAN_POINT('Ctrl Pts',(-10.9298287070001,15.2,-0.446877689000011));
#264840=CARTESIAN_POINT('Ctrl Pts',(-10.9298287070001,11.6,-0.446877689000012));
#264841=CARTESIAN_POINT('Ctrl Pts',(-10.9325755900001,15.2,-0.447957894000015));
#264842=CARTESIAN_POINT('Ctrl Pts',(-10.9325755900001,11.6,-0.447957894000016));
#264843=CARTESIAN_POINT('Ctrl Pts',(-10.9353266640001,15.2,-0.449042364000016));
#264844=CARTESIAN_POINT('Ctrl Pts',(-10.9353266640001,11.6,-0.449042364000017));
#264845=CARTESIAN_POINT('Ctrl Pts',(-10.9380819200001,15.2,-0.450131103000011));
#264846=CARTESIAN_POINT('Ctrl Pts',(-10.9380819200001,11.6,-0.450131103000011));
#264847=CARTESIAN_POINT('Ctrl Pts',(-10.9408413420001,15.2,-0.451224112000013));
#264848=CARTESIAN_POINT('Ctrl Pts',(-10.9408413420001,11.6,-0.451224112000013));
#264849=CARTESIAN_POINT('Ctrl Pts',(-10.9436049220001,15.2,-0.452321397000013));
#264850=CARTESIAN_POINT('Ctrl Pts',(-10.9436049220001,11.6,-0.452321397000013));
#264851=CARTESIAN_POINT('Ctrl Pts',(-10.9463726460001,15.2,-0.453422962000012));
#264852=CARTESIAN_POINT('Ctrl Pts',(-10.9463726460001,11.6,-0.453422962000012));
#264853=CARTESIAN_POINT('Ctrl Pts',(-10.9491445020001,15.2,-0.454528810000014));
#264854=CARTESIAN_POINT('Ctrl Pts',(-10.9491445020001,11.6,-0.454528810000015));
#264855=CARTESIAN_POINT('Ctrl Pts',(-10.9519204780001,15.2,-0.455638942000016));
#264856=CARTESIAN_POINT('Ctrl Pts',(-10.9519204780001,11.6,-0.455638942000017));
#264857=CARTESIAN_POINT('Ctrl Pts',(-10.9547005640001,15.2,-0.456753364000013));
#264858=CARTESIAN_POINT('Ctrl Pts',(-10.9547005640001,11.6,-0.456753364000014));
#264859=CARTESIAN_POINT('Ctrl Pts',(-10.9574847480001,15.2,-0.457872080000015));
#264860=CARTESIAN_POINT('Ctrl Pts',(-10.9574847480001,11.6,-0.457872080000015));
#264861=CARTESIAN_POINT('Ctrl Pts',(-10.9602730170001,15.2,-0.458995091000016));
#264862=CARTESIAN_POINT('Ctrl Pts',(-10.9602730170001,11.6,-0.458995091000017));
#264863=CARTESIAN_POINT('Ctrl Pts',(-10.9630653590001,15.2,-0.460122402000014));
#264864=CARTESIAN_POINT('Ctrl Pts',(-10.9630653590001,11.6,-0.460122402000014));
#264865=CARTESIAN_POINT('Ctrl Pts',(-10.9658617640001,15.2,-0.461254017000012));
#264866=CARTESIAN_POINT('Ctrl Pts',(-10.9658617640001,11.6,-0.461254017000013));
#264867=CARTESIAN_POINT('Ctrl Pts',(-10.9686622200001,15.2,-0.462389938000012));
#264868=CARTESIAN_POINT('Ctrl Pts',(-10.9686622200001,11.6,-0.462389938000012));
#264869=CARTESIAN_POINT('Ctrl Pts',(-10.9714667150001,15.2,-0.463530170000013));
#264870=CARTESIAN_POINT('Ctrl Pts',(-10.9714667150001,11.6,-0.463530170000013));
#264871=CARTESIAN_POINT('Ctrl Pts',(-10.9742752370001,15.2,-0.464674714000015));
#264872=CARTESIAN_POINT('Ctrl Pts',(-10.9742752370001,11.6,-0.464674714000016));
#264873=CARTESIAN_POINT('Ctrl Pts',(-10.9770877740001,15.2,-0.465823575000015));
#264874=CARTESIAN_POINT('Ctrl Pts',(-10.9770877740001,11.6,-0.465823575000015));
#264875=CARTESIAN_POINT('Ctrl Pts',(-10.9799043170001,15.2,-0.466976757000013));
#264876=CARTESIAN_POINT('Ctrl Pts',(-10.9799043170001,11.6,-0.466976757000013));
#264877=CARTESIAN_POINT('Ctrl Pts',(-10.9827248520001,15.2,-0.468134263000017));
#264878=CARTESIAN_POINT('Ctrl Pts',(-10.9827248520001,11.6,-0.468134263000018));
#264879=CARTESIAN_POINT('Ctrl Pts',(-10.9855493680001,15.2,-0.469296094000011));
#264880=CARTESIAN_POINT('Ctrl Pts',(-10.9855493680001,11.6,-0.469296094000012));
#264881=CARTESIAN_POINT('Ctrl Pts',(-10.9883778540001,15.2,-0.470462257000013));
#264882=CARTESIAN_POINT('Ctrl Pts',(-10.9883778540001,11.6,-0.470462257000013));
#264883=CARTESIAN_POINT('Ctrl Pts',(-10.9912102990001,15.2,-0.471632753000013));
#264884=CARTESIAN_POINT('Ctrl Pts',(-10.9912102990001,11.6,-0.471632753000014));
#264885=CARTESIAN_POINT('Ctrl Pts',(-10.9940466900001,15.2,-0.472807585000012));
#264886=CARTESIAN_POINT('Ctrl Pts',(-10.9940466900001,11.6,-0.472807585000013));
#264887=CARTESIAN_POINT('Ctrl Pts',(-10.9968870170001,15.2,-0.473986757000016));
#264888=CARTESIAN_POINT('Ctrl Pts',(-10.9968870170001,11.6,-0.473986757000016));
#264889=CARTESIAN_POINT('Ctrl Pts',(-10.9997312680001,15.2,-0.475170273000014));
#264890=CARTESIAN_POINT('Ctrl Pts',(-10.9997312680001,11.6,-0.475170273000014));
#264891=CARTESIAN_POINT('Ctrl Pts',(-11.0025794320001,15.2,-0.476358134000012));
#264892=CARTESIAN_POINT('Ctrl Pts',(-11.0025794320001,11.6,-0.476358134000013));
#264893=CARTESIAN_POINT('Ctrl Pts',(-11.0054314970001,15.2,-0.477550346000015));
#264894=CARTESIAN_POINT('Ctrl Pts',(-11.0054314970001,11.6,-0.477550346000016));
#264895=CARTESIAN_POINT('Ctrl Pts',(-11.0082874530001,15.2,-0.478746910000014));
#264896=CARTESIAN_POINT('Ctrl Pts',(-11.0082874530001,11.6,-0.478746910000015));
#264897=CARTESIAN_POINT('Ctrl Pts',(-11.0111472870001,15.2,-0.479947831000014));
#264898=CARTESIAN_POINT('Ctrl Pts',(-11.0111472870001,11.6,-0.479947831000014));
#264899=CARTESIAN_POINT('Ctrl Pts',(-11.0140109890001,15.2,-0.481153110000014));
#264900=CARTESIAN_POINT('Ctrl Pts',(-11.0140109890001,11.6,-0.481153110000015));
#264901=CARTESIAN_POINT('Ctrl Pts',(-11.0168785470001,15.2,-0.482362752000016));
#264902=CARTESIAN_POINT('Ctrl Pts',(-11.0168785470001,11.6,-0.482362752000017));
#264903=CARTESIAN_POINT('Ctrl Pts',(-11.0197499510001,15.2,-0.483576758000015));
#264904=CARTESIAN_POINT('Ctrl Pts',(-11.0197499510001,11.6,-0.483576758000015));
#264905=CARTESIAN_POINT('Ctrl Pts',(-11.0226251880001,15.2,-0.484795134000016));
#264906=CARTESIAN_POINT('Ctrl Pts',(-11.0226251880001,11.6,-0.484795134000016));
#264907=CARTESIAN_POINT('Ctrl Pts',(-11.0255042470001,15.2,-0.486017881000014));
#264908=CARTESIAN_POINT('Ctrl Pts',(-11.0255042470001,11.6,-0.486017881000014));
#264909=CARTESIAN_POINT('Ctrl Pts',(-11.0283871190001,15.2,-0.487245003000014));
#264910=CARTESIAN_POINT('Ctrl Pts',(-11.0283871190001,11.6,-0.487245003000015));
#264911=CARTESIAN_POINT('Ctrl Pts',(-11.0312737910001,15.2,-0.488476502000013));
#264912=CARTESIAN_POINT('Ctrl Pts',(-11.0312737910001,11.6,-0.488476502000013));
#264913=CARTESIAN_POINT('Ctrl Pts',(-11.0341642530001,15.2,-0.489712383000014));
#264914=CARTESIAN_POINT('Ctrl Pts',(-11.0341642530001,11.6,-0.489712383000014));
#264915=CARTESIAN_POINT('Ctrl Pts',(-11.0370584920001,15.2,-0.490952646000018));
#264916=CARTESIAN_POINT('Ctrl Pts',(-11.0370584920001,11.6,-0.490952646000018));
#264917=CARTESIAN_POINT('Ctrl Pts',(-11.0399564980001,15.2,-0.492197297000012));
#264918=CARTESIAN_POINT('Ctrl Pts',(-11.0399564980001,11.6,-0.492197297000013));
#264919=CARTESIAN_POINT('Ctrl Pts',(-11.0428582610001,15.2,-0.493446338000014));
#264920=CARTESIAN_POINT('Ctrl Pts',(-11.0428582610001,11.6,-0.493446338000015));
#264921=CARTESIAN_POINT('Ctrl Pts',(-11.0457637680001,15.2,-0.494699772000011));
#264922=CARTESIAN_POINT('Ctrl Pts',(-11.0457637680001,11.6,-0.494699772000012));
#264923=CARTESIAN_POINT('Ctrl Pts',(-11.0486730100001,15.2,-0.495957601000012));
#264924=CARTESIAN_POINT('Ctrl Pts',(-11.0486730100001,11.6,-0.495957601000013));
#264925=CARTESIAN_POINT('Ctrl Pts',(-11.0515859750001,15.2,-0.497219830000013));
#264926=CARTESIAN_POINT('Ctrl Pts',(-11.0515859750001,11.6,-0.497219830000013));
#264927=CARTESIAN_POINT('Ctrl Pts',(-11.0545026510001,15.2,-0.498486460000014));
#264928=CARTESIAN_POINT('Ctrl Pts',(-11.0545026510001,11.6,-0.498486460000014));
#264929=CARTESIAN_POINT('Ctrl Pts',(-11.0574230290001,15.2,-0.499757494000015));
#264930=CARTESIAN_POINT('Ctrl Pts',(-11.0574230290001,11.6,-0.499757494000015));
#264931=CARTESIAN_POINT('Ctrl Pts',(-11.0603470970001,15.2,-0.501032937000012));
#264932=CARTESIAN_POINT('Ctrl Pts',(-11.0603470970001,11.6,-0.501032937000013));
#264933=CARTESIAN_POINT('Ctrl Pts',(-11.0632748440001,15.2,-0.502312789000015));
#264934=CARTESIAN_POINT('Ctrl Pts',(-11.0632748440001,11.6,-0.502312789000015));
#264935=CARTESIAN_POINT('Ctrl Pts',(-11.0662062590001,15.2,-0.503597056000018));
#264936=CARTESIAN_POINT('Ctrl Pts',(-11.0662062590001,11.6,-0.503597056000018));
#264937=CARTESIAN_POINT('Ctrl Pts',(-11.0691413320001,15.2,-0.504885738000014));
#264938=CARTESIAN_POINT('Ctrl Pts',(-11.0691413320001,11.6,-0.504885738000014));
#264939=CARTESIAN_POINT('Ctrl Pts',(-11.0720800520001,15.2,-0.506178839000011));
#264940=CARTESIAN_POINT('Ctrl Pts',(-11.0720800520001,11.6,-0.506178839000011));
#264941=CARTESIAN_POINT('Ctrl Pts',(-11.0750224080001,15.2,-0.507476362000014));
#264942=CARTESIAN_POINT('Ctrl Pts',(-11.0750224080001,11.6,-0.507476362000015));
#264943=CARTESIAN_POINT('Ctrl Pts',(-11.0779683880001,15.2,-0.508778311000011));
#264944=CARTESIAN_POINT('Ctrl Pts',(-11.0779683880001,11.6,-0.508778311000011));
#264945=CARTESIAN_POINT('Ctrl Pts',(-11.0809179820001,15.2,-0.510084687000014));
#264946=CARTESIAN_POINT('Ctrl Pts',(-11.0809179820001,11.6,-0.510084687000015));
#264947=CARTESIAN_POINT('Ctrl Pts',(-11.0838711810001,15.2,-0.511395492000015));
#264948=CARTESIAN_POINT('Ctrl Pts',(-11.0838711810001,11.6,-0.511395492000016));
#264949=CARTESIAN_POINT('Ctrl Pts',(-11.0868279720001,15.2,-0.512710732000015));
#264950=CARTESIAN_POINT('Ctrl Pts',(-11.0868279720001,11.6,-0.512710732000015));
#264951=CARTESIAN_POINT('Ctrl Pts',(-11.0897883450001,15.2,-0.514030406000017));
#264952=CARTESIAN_POINT('Ctrl Pts',(-11.0897883450001,11.6,-0.514030406000017));
#264953=CARTESIAN_POINT('Ctrl Pts',(-11.0927522890001,15.2,-0.515354521000013));
#264954=CARTESIAN_POINT('Ctrl Pts',(-11.0927522890001,11.6,-0.515354521000014));
#264955=CARTESIAN_POINT('Ctrl Pts',(-11.0957197940001,15.2,-0.516683076000017));
#264956=CARTESIAN_POINT('Ctrl Pts',(-11.0957197940001,11.6,-0.516683076000018));
#264957=CARTESIAN_POINT('Ctrl Pts',(-11.0986908480001,15.2,-0.518016075000016));
#264958=CARTESIAN_POINT('Ctrl Pts',(-11.0986908480001,11.6,-0.518016075000017));
#264959=CARTESIAN_POINT('Ctrl Pts',(-11.1016654420001,15.2,-0.519353522000015));
#264960=CARTESIAN_POINT('Ctrl Pts',(-11.1016654420001,11.6,-0.519353522000015));
#264961=CARTESIAN_POINT('Ctrl Pts',(-11.1046435640001,15.2,-0.520695418000017));
#264962=CARTESIAN_POINT('Ctrl Pts',(-11.1046435640001,11.6,-0.520695418000017));
#264963=CARTESIAN_POINT('Ctrl Pts',(-11.1076252050001,15.2,-0.522041766000014));
#264964=CARTESIAN_POINT('Ctrl Pts',(-11.1076252050001,11.6,-0.522041766000015));
#264965=CARTESIAN_POINT('Ctrl Pts',(-11.1106103520001,15.2,-0.523392569000016));
#264966=CARTESIAN_POINT('Ctrl Pts',(-11.1106103520001,11.6,-0.523392569000017));
#264967=CARTESIAN_POINT('Ctrl Pts',(-11.1135989970001,15.2,-0.524747830000014));
#264968=CARTESIAN_POINT('Ctrl Pts',(-11.1135989970001,11.6,-0.524747830000015));
#264969=CARTESIAN_POINT('Ctrl Pts',(-11.1165911290001,15.2,-0.526107550000017));
#264970=CARTESIAN_POINT('Ctrl Pts',(-11.1165911290001,11.6,-0.526107550000017));
#264971=CARTESIAN_POINT('Ctrl Pts',(-11.1195867360001,15.2,-0.527471735000016));
#264972=CARTESIAN_POINT('Ctrl Pts',(-11.1195867360001,11.6,-0.527471735000016));
#264973=CARTESIAN_POINT('Ctrl Pts',(-11.1225858080001,15.2,-0.528840384000016));
#264974=CARTESIAN_POINT('Ctrl Pts',(-11.1225858080001,11.6,-0.528840384000016));
#264975=CARTESIAN_POINT('Ctrl Pts',(-11.1255883350001,15.2,-0.530213501000016));
#264976=CARTESIAN_POINT('Ctrl Pts',(-11.1255883350001,11.6,-0.530213501000017));
#264977=CARTESIAN_POINT('Ctrl Pts',(-11.1285943060001,15.2,-0.531591090000014));
#264978=CARTESIAN_POINT('Ctrl Pts',(-11.1285943060001,11.6,-0.531591090000015));
#264979=CARTESIAN_POINT('Ctrl Pts',(-11.1316037120001,15.2,-0.532973151000018));
#264980=CARTESIAN_POINT('Ctrl Pts',(-11.1316037120001,11.6,-0.532973151000018));
#264981=CARTESIAN_POINT('Ctrl Pts',(-11.1346165400001,15.2,-0.534359689000015));
#264982=CARTESIAN_POINT('Ctrl Pts',(-11.1346165400001,11.6,-0.534359689000015));
#264983=CARTESIAN_POINT('Ctrl Pts',(-11.1376327810001,15.2,-0.535750705000013));
#264984=CARTESIAN_POINT('Ctrl Pts',(-11.1376327810001,11.6,-0.535750705000014));
#264985=CARTESIAN_POINT('Ctrl Pts',(-11.1406524250001,15.2,-0.537146200000014));
#264986=CARTESIAN_POINT('Ctrl Pts',(-11.1406524250001,11.6,-0.537146200000014));
#264987=CARTESIAN_POINT('Ctrl Pts',(-11.1436754620001,15.2,-0.538546181000013));
#264988=CARTESIAN_POINT('Ctrl Pts',(-11.1436754620001,11.6,-0.538546181000013));
#264989=CARTESIAN_POINT('Ctrl Pts',(-11.1467018790001,15.2,-0.539950647000014));
#264990=CARTESIAN_POINT('Ctrl Pts',(-11.1467018790001,11.6,-0.539950647000014));
#264991=CARTESIAN_POINT('Ctrl Pts',(-11.1497316690001,15.2,-0.541359602000018));
#264992=CARTESIAN_POINT('Ctrl Pts',(-11.1497316690001,11.6,-0.541359602000018));
#264993=CARTESIAN_POINT('Ctrl Pts',(-11.1527648200001,15.2,-0.542773047000011));
#264994=CARTESIAN_POINT('Ctrl Pts',(-11.1527648200001,11.6,-0.542773047000012));
#264995=CARTESIAN_POINT('Ctrl Pts',(-11.1558013220001,15.2,-0.544190986000017));
#264996=CARTESIAN_POINT('Ctrl Pts',(-11.1558013220001,11.6,-0.544190986000018));
#264997=CARTESIAN_POINT('Ctrl Pts',(-11.1588411640001,15.2,-0.545613421000013));
#264998=CARTESIAN_POINT('Ctrl Pts',(-11.1588411640001,11.6,-0.545613421000013));
#264999=CARTESIAN_POINT('Ctrl Pts',(-11.1618843360001,15.2,-0.547040354000017));
#265000=CARTESIAN_POINT('Ctrl Pts',(-11.1618843360001,11.6,-0.547040354000017));
#265001=CARTESIAN_POINT('Ctrl Pts',(-11.1649308290001,15.2,-0.548471788000011));
#265002=CARTESIAN_POINT('Ctrl Pts',(-11.1649308290001,11.6,-0.548471788000012));
#265003=CARTESIAN_POINT('Ctrl Pts',(-11.1679806310001,15.2,-0.549907725000014));
#265004=CARTESIAN_POINT('Ctrl Pts',(-11.1679806310001,11.6,-0.549907725000014));
#265005=CARTESIAN_POINT('Ctrl Pts',(-11.1710337330001,15.2,-0.551348168000012));
#265006=CARTESIAN_POINT('Ctrl Pts',(-11.1710337330001,11.6,-0.551348168000013));
#265007=CARTESIAN_POINT('Ctrl Pts',(-11.1740901240001,15.2,-0.552793118000015));
#265008=CARTESIAN_POINT('Ctrl Pts',(-11.1740901240001,11.6,-0.552793118000015));
#265009=CARTESIAN_POINT('Ctrl Pts',(-11.1771497950001,15.2,-0.554242580000013));
#265010=CARTESIAN_POINT('Ctrl Pts',(-11.1771497950001,11.6,-0.554242580000013));
#265011=CARTESIAN_POINT('Ctrl Pts',(-11.1802127340001,15.2,-0.555696554000011));
#265012=CARTESIAN_POINT('Ctrl Pts',(-11.1802127340001,11.6,-0.555696554000012));
#265013=CARTESIAN_POINT('Ctrl Pts',(-11.1832789320001,15.2,-0.557155042000015));
#265014=CARTESIAN_POINT('Ctrl Pts',(-11.1832789320001,11.6,-0.557155042000015));
#265015=CARTESIAN_POINT('Ctrl Pts',(-11.1863483800001,15.2,-0.558618049000015));
#265016=CARTESIAN_POINT('Ctrl Pts',(-11.1863483800001,11.6,-0.558618049000015));
#265017=CARTESIAN_POINT('Ctrl Pts',(-11.1894210660001,15.2,-0.560085575000016));
#265018=CARTESIAN_POINT('Ctrl Pts',(-11.1894210660001,11.6,-0.560085575000016));
#265019=CARTESIAN_POINT('Ctrl Pts',(-11.1924969800001,15.2,-0.561557623000013));
#265020=CARTESIAN_POINT('Ctrl Pts',(-11.1924969800001,11.6,-0.561557623000013));
#265021=CARTESIAN_POINT('Ctrl Pts',(-11.1955761130001,15.2,-0.563034196000016));
#265022=CARTESIAN_POINT('Ctrl Pts',(-11.1955761130001,11.6,-0.563034196000017));
#265023=CARTESIAN_POINT('Ctrl Pts',(-11.1986584540001,15.2,-0.564515295000017));
#265024=CARTESIAN_POINT('Ctrl Pts',(-11.1986584540001,11.6,-0.564515295000017));
#265025=CARTESIAN_POINT('Ctrl Pts',(-11.2017439940001,15.2,-0.566000924000014));
#265026=CARTESIAN_POINT('Ctrl Pts',(-11.2017439940001,11.6,-0.566000924000015));
#265027=CARTESIAN_POINT('Ctrl Pts',(-11.2048327210001,15.2,-0.567491084000018));
#265028=CARTESIAN_POINT('Ctrl Pts',(-11.2048327210001,11.6,-0.567491084000018));
#265029=CARTESIAN_POINT('Ctrl Pts',(-11.2079246280001,15.2,-0.568985776000015));
#265030=CARTESIAN_POINT('Ctrl Pts',(-11.2079246280001,11.6,-0.568985776000015));
#265031=CARTESIAN_POINT('Ctrl Pts',(-11.2110197020001,15.2,-0.570485006000014));
#265032=CARTESIAN_POINT('Ctrl Pts',(-11.2110197020001,11.6,-0.570485006000015));
#265033=CARTESIAN_POINT('Ctrl Pts',(-11.2141179350001,15.2,-0.571988772000012));
#265034=CARTESIAN_POINT('Ctrl Pts',(-11.2141179350001,11.6,-0.571988772000012));
#265035=CARTESIAN_POINT('Ctrl Pts',(-11.2172193170001,15.2,-0.573497079000016));
#265036=CARTESIAN_POINT('Ctrl Pts',(-11.2172193170001,11.6,-0.573497079000016));
#265037=CARTESIAN_POINT('Ctrl Pts',(-11.2203238380001,15.2,-0.575009928000014));
#265038=CARTESIAN_POINT('Ctrl Pts',(-11.2203238380001,11.6,-0.575009928000015));
#265039=CARTESIAN_POINT('Ctrl Pts',(-11.2234314850001,15.2,-0.576527323000011));
#265040=CARTESIAN_POINT('Ctrl Pts',(-11.2234314850001,11.6,-0.576527323000012));
#265041=CARTESIAN_POINT('Ctrl Pts',(-11.2265422530001,15.2,-0.578049263000011));
#265042=CARTESIAN_POINT('Ctrl Pts',(-11.2265422530001,11.6,-0.578049263000012));
#265043=CARTESIAN_POINT('Ctrl Pts',(-11.2296561290001,15.2,-0.579575753000015));
#265044=CARTESIAN_POINT('Ctrl Pts',(-11.2296561290001,11.6,-0.579575753000015));
#265045=CARTESIAN_POINT('Ctrl Pts',(-11.2327731030001,15.2,-0.581106794000017));
#265046=CARTESIAN_POINT('Ctrl Pts',(-11.2327731030001,11.6,-0.581106794000017));
#265047=CARTESIAN_POINT('Ctrl Pts',(-11.2358931670001,15.2,-0.582642387000014));
#265048=CARTESIAN_POINT('Ctrl Pts',(-11.2358931670001,11.6,-0.582642387000015));
#265049=CARTESIAN_POINT('Ctrl Pts',(-11.2390163100001,15.2,-0.584182538000011));
#265050=CARTESIAN_POINT('Ctrl Pts',(-11.2390163100001,11.6,-0.584182538000011));
#265051=CARTESIAN_POINT('Ctrl Pts',(-11.2421425230001,15.2,-0.585727245000012));
#265052=CARTESIAN_POINT('Ctrl Pts',(-11.2421425230001,11.6,-0.585727245000012));
#265053=CARTESIAN_POINT('Ctrl Pts',(-11.2452717950001,15.2,-0.587276511000017));
#265054=CARTESIAN_POINT('Ctrl Pts',(-11.2452717950001,11.6,-0.587276511000017));
#265055=CARTESIAN_POINT('Ctrl Pts',(-11.2484041180001,15.2,-0.588830340000013));
#265056=CARTESIAN_POINT('Ctrl Pts',(-11.2484041180001,11.6,-0.588830340000013));
#265057=CARTESIAN_POINT('Ctrl Pts',(-11.2515394790001,15.2,-0.590388732000013));
#265058=CARTESIAN_POINT('Ctrl Pts',(-11.2515394790001,11.6,-0.590388732000014));
#265059=CARTESIAN_POINT('Ctrl Pts',(-11.2546778710001,15.2,-0.591951690000014));
#265060=CARTESIAN_POINT('Ctrl Pts',(-11.2546778710001,11.6,-0.591951690000015));
#265061=CARTESIAN_POINT('Ctrl Pts',(-11.2578192840001,15.2,-0.593519216000011));
#265062=CARTESIAN_POINT('Ctrl Pts',(-11.2578192840001,11.6,-0.593519216000012));
#265063=CARTESIAN_POINT('Ctrl Pts',(-11.2609637080001,15.2,-0.595091312000013));
#265064=CARTESIAN_POINT('Ctrl Pts',(-11.2609637080001,11.6,-0.595091312000014));
#265065=CARTESIAN_POINT('Ctrl Pts',(-11.2641111320001,15.2,-0.596667981000016));
#265066=CARTESIAN_POINT('Ctrl Pts',(-11.2641111320001,11.6,-0.596667981000017));
#265067=CARTESIAN_POINT('Ctrl Pts',(-11.2672615480001,15.2,-0.598249222000016));
#265068=CARTESIAN_POINT('Ctrl Pts',(-11.2672615480001,11.6,-0.598249222000016));
#265069=CARTESIAN_POINT('Ctrl Pts',(-11.2704149460001,15.2,-0.599835041000016));
#265070=CARTESIAN_POINT('Ctrl Pts',(-11.2704149460001,11.6,-0.599835041000017));
#265071=CARTESIAN_POINT('Ctrl Pts',(-11.2735713160001,15.2,-0.601425437000014));
#265072=CARTESIAN_POINT('Ctrl Pts',(-11.2735713160001,11.6,-0.601425437000014));
#265073=CARTESIAN_POINT('Ctrl Pts',(-11.2767306480001,15.2,-0.603020414000017));
#265074=CARTESIAN_POINT('Ctrl Pts',(-11.2767306480001,11.6,-0.603020414000018));
#265075=CARTESIAN_POINT('Ctrl Pts',(-11.2798929340001,15.2,-0.604619973000013));
#265076=CARTESIAN_POINT('Ctrl Pts',(-11.2798929340001,11.6,-0.604619973000014));
#265077=CARTESIAN_POINT('Ctrl Pts',(-11.2830581620001,15.2,-0.606224115000016));
#265078=CARTESIAN_POINT('Ctrl Pts',(-11.2830581620001,11.6,-0.606224115000016));
#265079=CARTESIAN_POINT('Ctrl Pts',(-11.2862263240001,15.2,-0.607832843000011));
#265080=CARTESIAN_POINT('Ctrl Pts',(-11.2862263240001,11.6,-0.607832843000012));
#265081=CARTESIAN_POINT('Ctrl Pts',(-11.2893974100001,15.2,-0.609446160000013));
#265082=CARTESIAN_POINT('Ctrl Pts',(-11.2893974100001,11.6,-0.609446160000014));
#265083=CARTESIAN_POINT('Ctrl Pts',(-11.2925714100001,15.2,-0.611064067000013));
#265084=CARTESIAN_POINT('Ctrl Pts',(-11.2925714100001,11.6,-0.611064067000014));
#265085=CARTESIAN_POINT('Ctrl Pts',(-11.2957483150001,15.2,-0.612686565000011));
#265086=CARTESIAN_POINT('Ctrl Pts',(-11.2957483150001,11.6,-0.612686565000012));
#265087=CARTESIAN_POINT('Ctrl Pts',(-11.2989281170001,15.2,-0.614313657000016));
#265088=CARTESIAN_POINT('Ctrl Pts',(-11.2989281170001,11.6,-0.614313657000017));
#265089=CARTESIAN_POINT('Ctrl Pts',(-11.3021108030001,15.2,-0.615945345000015));
#265090=CARTESIAN_POINT('Ctrl Pts',(-11.3021108030001,11.6,-0.615945345000016));
#265091=CARTESIAN_POINT('Ctrl Pts',(-11.3052963650001,15.2,-0.617581630000017));
#265092=CARTESIAN_POINT('Ctrl Pts',(-11.3052963650001,11.6,-0.617581630000017));
#265093=CARTESIAN_POINT('Ctrl Pts',(-11.3084847960001,15.2,-0.619222515000013));
#265094=CARTESIAN_POINT('Ctrl Pts',(-11.3084847960001,11.6,-0.619222515000013));
#265095=CARTESIAN_POINT('Ctrl Pts',(-11.3116760820001,15.2,-0.620868001000012));
#265096=CARTESIAN_POINT('Ctrl Pts',(-11.3116760820001,11.6,-0.620868001000013));
#265097=CARTESIAN_POINT('Ctrl Pts',(-11.3148702170001,15.2,-0.622518091000015));
#265098=CARTESIAN_POINT('Ctrl Pts',(-11.3148702170001,11.6,-0.622518091000015));
#265099=CARTESIAN_POINT('Ctrl Pts',(-11.3180671910001,15.2,-0.624172784000017));
#265100=CARTESIAN_POINT('Ctrl Pts',(-11.3180671910001,11.6,-0.624172784000017));
#265101=CARTESIAN_POINT('Ctrl Pts',(-11.3212669940001,15.2,-0.625832085000013));
#265102=CARTESIAN_POINT('Ctrl Pts',(-11.3212669940001,11.6,-0.625832085000014));
#265103=CARTESIAN_POINT('Ctrl Pts',(-11.3244696160001,15.2,-0.627495996000014));
#265104=CARTESIAN_POINT('Ctrl Pts',(-11.3244696160001,11.6,-0.627495996000014));
#265105=CARTESIAN_POINT('Ctrl Pts',(-11.3276750490001,15.2,-0.629164515000014));
#265106=CARTESIAN_POINT('Ctrl Pts',(-11.3276750490001,11.6,-0.629164515000014));
#265107=CARTESIAN_POINT('Ctrl Pts',(-11.3308832820001,15.2,-0.630837648000018));
#265108=CARTESIAN_POINT('Ctrl Pts',(-11.3308832820001,11.6,-0.630837648000018));
#265109=CARTESIAN_POINT('Ctrl Pts',(-11.3340943080001,15.2,-0.632515395000013));
#265110=CARTESIAN_POINT('Ctrl Pts',(-11.3340943080001,11.6,-0.632515395000013));
#265111=CARTESIAN_POINT('Ctrl Pts',(-11.3373081150001,15.2,-0.634197758000017));
#265112=CARTESIAN_POINT('Ctrl Pts',(-11.3373081150001,11.6,-0.634197758000017));
#265113=CARTESIAN_POINT('Ctrl Pts',(-11.3405246950001,15.2,-0.635884737000012));
#265114=CARTESIAN_POINT('Ctrl Pts',(-11.3405246950001,11.6,-0.635884737000012));
#265115=CARTESIAN_POINT('Ctrl Pts',(-11.3437440390001,15.2,-0.637576336000016));
#265116=CARTESIAN_POINT('Ctrl Pts',(-11.3437440390001,11.6,-0.637576336000017));
#265117=CARTESIAN_POINT('Ctrl Pts',(-11.3469661360001,15.2,-0.639272557000012));
#265118=CARTESIAN_POINT('Ctrl Pts',(-11.3469661360001,11.6,-0.639272557000013));
#265119=CARTESIAN_POINT('Ctrl Pts',(-11.3501909790001,15.2,-0.640973401000018));
#265120=CARTESIAN_POINT('Ctrl Pts',(-11.3501909790001,11.6,-0.640973401000018));
#265121=CARTESIAN_POINT('Ctrl Pts',(-11.3534185570001,15.2,-0.642678869000015));
#265122=CARTESIAN_POINT('Ctrl Pts',(-11.3534185570001,11.6,-0.642678869000016));
#265123=CARTESIAN_POINT('Ctrl Pts',(-11.3566488620001,15.2,-0.644388964000013));
#265124=CARTESIAN_POINT('Ctrl Pts',(-11.3566488620001,11.6,-0.644388964000014));
#265125=CARTESIAN_POINT('Ctrl Pts',(-11.3598818840001,15.2,-0.646103687000017));
#265126=CARTESIAN_POINT('Ctrl Pts',(-11.3598818840001,11.6,-0.646103687000017));
#265127=CARTESIAN_POINT('Ctrl Pts',(-11.3631176140001,15.2,-0.647823039000013));
#265128=CARTESIAN_POINT('Ctrl Pts',(-11.3631176140001,11.6,-0.647823039000013));
#265129=CARTESIAN_POINT('Ctrl Pts',(-11.3663560430001,15.2,-0.649547023000014));
#265130=CARTESIAN_POINT('Ctrl Pts',(-11.3663560430001,11.6,-0.649547023000015));
#265131=CARTESIAN_POINT('Ctrl Pts',(-11.3695971620001,15.2,-0.651275639000013));
#265132=CARTESIAN_POINT('Ctrl Pts',(-11.3695971620001,11.6,-0.651275639000013));
#265133=CARTESIAN_POINT('Ctrl Pts',(-11.3728409600001,15.2,-0.653008892000013));
#265134=CARTESIAN_POINT('Ctrl Pts',(-11.3728409600001,11.6,-0.653008892000014));
#265135=CARTESIAN_POINT('Ctrl Pts',(-11.3760874300001,15.2,-0.654746780000015));
#265136=CARTESIAN_POINT('Ctrl Pts',(-11.3760874300001,11.6,-0.654746780000016));
#265137=CARTESIAN_POINT('Ctrl Pts',(-11.3793365610001,15.2,-0.656489306000014));
#265138=CARTESIAN_POINT('Ctrl Pts',(-11.3793365610001,11.6,-0.656489306000015));
#265139=CARTESIAN_POINT('Ctrl Pts',(-11.3825883450001,15.2,-0.658236472000016));
#265140=CARTESIAN_POINT('Ctrl Pts',(-11.3825883450001,11.6,-0.658236472000016));
#265141=CARTESIAN_POINT('Ctrl Pts',(-11.3858427730001,15.2,-0.659988280000015));
#265142=CARTESIAN_POINT('Ctrl Pts',(-11.3858427730001,11.6,-0.659988280000015));
#265143=CARTESIAN_POINT('Ctrl Pts',(-11.3890998350001,15.2,-0.661744730000016));
#265144=CARTESIAN_POINT('Ctrl Pts',(-11.3890998350001,11.6,-0.661744730000016));
#265145=CARTESIAN_POINT('Ctrl Pts',(-11.3923595230001,15.2,-0.663505825000015));
#265146=CARTESIAN_POINT('Ctrl Pts',(-11.3923595230001,11.6,-0.663505825000015));
#265147=CARTESIAN_POINT('Ctrl Pts',(-11.3956218280001,15.2,-0.665271566000012));
#265148=CARTESIAN_POINT('Ctrl Pts',(-11.3956218280001,11.6,-0.665271566000012));
#265149=CARTESIAN_POINT('Ctrl Pts',(-11.3988867400001,15.2,-0.667041955000016));
#265150=CARTESIAN_POINT('Ctrl Pts',(-11.3988867400001,11.6,-0.667041955000017));
#265151=CARTESIAN_POINT('Ctrl Pts',(-11.4021542520001,15.2,-0.668816993000014));
#265152=CARTESIAN_POINT('Ctrl Pts',(-11.4021542520001,11.6,-0.668816993000015));
#265153=CARTESIAN_POINT('Ctrl Pts',(-11.4054243520001,15.2,-0.670596683000015));
#265154=CARTESIAN_POINT('Ctrl Pts',(-11.4054243520001,11.6,-0.670596683000016));
#265155=CARTESIAN_POINT('Ctrl Pts',(-11.4086970320001,15.2,-0.672381023000015));
#265156=CARTESIAN_POINT('Ctrl Pts',(-11.4086970320001,11.6,-0.672381023000015));
#265157=CARTESIAN_POINT('Ctrl Pts',(-11.4119722840001,15.2,-0.674170019000013));
#265158=CARTESIAN_POINT('Ctrl Pts',(-11.4119722840001,11.6,-0.674170019000014));
#265159=CARTESIAN_POINT('Ctrl Pts',(-11.4152500960001,15.2,-0.675963670000015));
#265160=CARTESIAN_POINT('Ctrl Pts',(-11.4152500960001,11.6,-0.675963670000015));
#265161=CARTESIAN_POINT('Ctrl Pts',(-11.4185304610001,15.2,-0.677761979000016));
#265162=CARTESIAN_POINT('Ctrl Pts',(-11.4185304610001,11.6,-0.677761979000016));
#265163=CARTESIAN_POINT('Ctrl Pts',(-11.4218133690001,15.2,-0.679564946000015));
#265164=CARTESIAN_POINT('Ctrl Pts',(-11.4218133690001,11.6,-0.679564946000016));
#265165=CARTESIAN_POINT('Ctrl Pts',(-11.4250988120001,15.2,-0.681372573000014));
#265166=CARTESIAN_POINT('Ctrl Pts',(-11.4250988120001,11.6,-0.681372573000015));
#265167=CARTESIAN_POINT('Ctrl Pts',(-11.4283867810001,15.2,-0.683184862000012));
#265168=CARTESIAN_POINT('Ctrl Pts',(-11.4283867810001,11.6,-0.683184862000013));
#265169=CARTESIAN_POINT('Ctrl Pts',(-11.4316772700001,15.2,-0.685001814000015));
#265170=CARTESIAN_POINT('Ctrl Pts',(-11.4316772700001,11.6,-0.685001814000015));
#265171=CARTESIAN_POINT('Ctrl Pts',(-11.4349702680001,15.2,-0.686823430000012));
#265172=CARTESIAN_POINT('Ctrl Pts',(-11.4349702680001,11.6,-0.686823430000012));
#265173=CARTESIAN_POINT('Ctrl Pts',(-11.4382657700001,15.2,-0.688649711000018));
#265174=CARTESIAN_POINT('Ctrl Pts',(-11.4382657700001,11.6,-0.688649711000018));
#265175=CARTESIAN_POINT('Ctrl Pts',(-11.4415637630001,15.2,-0.690480659000015));
#265176=CARTESIAN_POINT('Ctrl Pts',(-11.4415637630001,11.6,-0.690480659000015));
#265177=CARTESIAN_POINT('Ctrl Pts',(-11.4448642400001,15.2,-0.692316276000016));
#265178=CARTESIAN_POINT('Ctrl Pts',(-11.4448642400001,11.6,-0.692316276000016));
#265179=CARTESIAN_POINT('Ctrl Pts',(-11.4481671870001,15.2,-0.694156565000017));
#265180=CARTESIAN_POINT('Ctrl Pts',(-11.4481671870001,11.6,-0.694156565000017));
#265181=CARTESIAN_POINT('Ctrl Pts',(-11.4514725950001,15.2,-0.696001525000014));
#265182=CARTESIAN_POINT('Ctrl Pts',(-11.4514725950001,11.6,-0.696001525000014));
#265183=CARTESIAN_POINT('Ctrl Pts',(-11.4547804530001,15.2,-0.697851159000016));
#265184=CARTESIAN_POINT('Ctrl Pts',(-11.4547804530001,11.6,-0.697851159000016));
#265185=CARTESIAN_POINT('Ctrl Pts',(-11.4580907510001,15.2,-0.699705470000014));
#265186=CARTESIAN_POINT('Ctrl Pts',(-11.4580907510001,11.6,-0.699705470000014));
#265187=CARTESIAN_POINT('Ctrl Pts',(-11.4614034810001,15.2,-0.701564457000017));
#265188=CARTESIAN_POINT('Ctrl Pts',(-11.4614034810001,11.6,-0.701564457000017));
#265189=CARTESIAN_POINT('Ctrl Pts',(-11.4647186380001,15.2,-0.703428121000016));
#265190=CARTESIAN_POINT('Ctrl Pts',(-11.4647186380001,11.6,-0.703428121000016));
#265191=CARTESIAN_POINT('Ctrl Pts',(-11.4680362160001,15.2,-0.705296464000016));
#265192=CARTESIAN_POINT('Ctrl Pts',(-11.4680362160001,11.6,-0.705296464000016));
#265193=CARTESIAN_POINT('Ctrl Pts',(-11.4713562160001,15.2,-0.707169486000012));
#265194=CARTESIAN_POINT('Ctrl Pts',(-11.4713562160001,11.6,-0.707169486000013));
#265195=CARTESIAN_POINT('Ctrl Pts',(-11.4740141490001,15.2,-0.708671646000014));
#265196=CARTESIAN_POINT('Ctrl Pts',(-11.4740141490001,11.6,-0.708671646000015));
#265197=CARTESIAN_POINT('Ctrl Pts',(-11.4760086880001,15.2,-0.709800372000018));
#265198=CARTESIAN_POINT('Ctrl Pts',(-11.4760086880001,11.6,-0.709800372000018));
#265199=CARTESIAN_POINT('Ctrl Pts',(-11.4773388640001,15.2,-0.710553791000015));
#265200=CARTESIAN_POINT('Ctrl Pts',(-11.4773388640001,11.6,-0.710553791000015));
#265201=CARTESIAN_POINT('Ctrl Pts',(-11.4780040730001,15.2,-0.710930734000015));
#265202=CARTESIAN_POINT('Ctrl Pts',(-11.4780040730001,11.6,-0.710930734000015));
#265203=CARTESIAN_POINT('Ctrl Pts',(-10.3708900240001,15.2,-0.292001929000012));
#265204=CARTESIAN_POINT('Ctrl Pts',(-10.3710632460001,15.2,-0.292021795000017));
#265205=CARTESIAN_POINT('Ctrl Pts',(-10.3714157310001,15.2,-0.292062310000016));
#265206=CARTESIAN_POINT('Ctrl Pts',(-10.3719498000001,15.2,-0.292123961000015));
#265207=CARTESIAN_POINT('Ctrl Pts',(-10.3726691760001,15.2,-0.292207548000012));
#265208=CARTESIAN_POINT('Ctrl Pts',(-10.3735789750001,15.2,-0.292314181000015));
#265209=CARTESIAN_POINT('Ctrl Pts',(-10.3745034120001,15.2,-0.292423469000016));
#265210=CARTESIAN_POINT('Ctrl Pts',(-10.3754371840001,15.2,-0.292534812000014));
#265211=CARTESIAN_POINT('Ctrl Pts',(-10.3763802670001,15.2,-0.292648223000014));
#265212=CARTESIAN_POINT('Ctrl Pts',(-10.3773326270001,15.2,-0.292763718000018));
#265213=CARTESIAN_POINT('Ctrl Pts',(-10.3782942400001,15.2,-0.292881310000013));
#265214=CARTESIAN_POINT('Ctrl Pts',(-10.3792650740001,15.2,-0.293001015000014));
#265215=CARTESIAN_POINT('Ctrl Pts',(-10.3802451030001,15.2,-0.293122847000014));
#265216=CARTESIAN_POINT('Ctrl Pts',(-10.3812342970001,15.2,-0.293246820000017));
#265217=CARTESIAN_POINT('Ctrl Pts',(-10.3822326280001,15.2,-0.293372950000013));
#265218=CARTESIAN_POINT('Ctrl Pts',(-10.3832400690001,15.2,-0.293501248000014));
#265219=CARTESIAN_POINT('Ctrl Pts',(-10.3842565920001,15.2,-0.293631732000015));
#265220=CARTESIAN_POINT('Ctrl Pts',(-10.3852821680001,15.2,-0.293764413000015));
#265221=CARTESIAN_POINT('Ctrl Pts',(-10.3863167710001,15.2,-0.293899307000016));
#265222=CARTESIAN_POINT('Ctrl Pts',(-10.3873603720001,15.2,-0.294036427000015));
#265223=CARTESIAN_POINT('Ctrl Pts',(-10.3884129450001,15.2,-0.294175788000013));
#265224=CARTESIAN_POINT('Ctrl Pts',(-10.3894744620001,15.2,-0.294317401000015));
#265225=CARTESIAN_POINT('Ctrl Pts',(-10.3905448950001,15.2,-0.294461282000014));
#265226=CARTESIAN_POINT('Ctrl Pts',(-10.3916242180001,15.2,-0.294607444000015));
#265227=CARTESIAN_POINT('Ctrl Pts',(-10.3927124050001,15.2,-0.294755901000014));
#265228=CARTESIAN_POINT('Ctrl Pts',(-10.3938094280001,15.2,-0.294906666000014));
#265229=CARTESIAN_POINT('Ctrl Pts',(-10.3949152600001,15.2,-0.295059752000015));
#265230=CARTESIAN_POINT('Ctrl Pts',(-10.3960298750001,15.2,-0.295215173000014));
#265231=CARTESIAN_POINT('Ctrl Pts',(-10.3971532480001,15.2,-0.295372943000016));
#265232=CARTESIAN_POINT('Ctrl Pts',(-10.3982853500001,15.2,-0.295533072000014));
#265233=CARTESIAN_POINT('Ctrl Pts',(-10.3994261560001,15.2,-0.295695576000017));
#265234=CARTESIAN_POINT('Ctrl Pts',(-10.4005756420001,15.2,-0.295860468000013));
#265235=CARTESIAN_POINT('Ctrl Pts',(-10.4017337790001,15.2,-0.296027759000013));
#265236=CARTESIAN_POINT('Ctrl Pts',(-10.4029005420001,15.2,-0.296197463000016));
#265237=CARTESIAN_POINT('Ctrl Pts',(-10.4040759070001,15.2,-0.296369593000012));
#265238=CARTESIAN_POINT('Ctrl Pts',(-10.4052598460001,15.2,-0.296544162000014));
#265239=CARTESIAN_POINT('Ctrl Pts',(-10.4064523340001,15.2,-0.296721181000015));
#265240=CARTESIAN_POINT('Ctrl Pts',(-10.4076533470001,15.2,-0.296900665000015));
#265241=CARTESIAN_POINT('Ctrl Pts',(-10.4088628590001,15.2,-0.297082624000016));
#265242=CARTESIAN_POINT('Ctrl Pts',(-10.4100808450001,15.2,-0.297267072000014));
#265243=CARTESIAN_POINT('Ctrl Pts',(-10.4113072790001,15.2,-0.297454022000014));
#265244=CARTESIAN_POINT('Ctrl Pts',(-10.4125421370001,15.2,-0.297643484000014));
#265245=CARTESIAN_POINT('Ctrl Pts',(-10.4137853940001,15.2,-0.297835472000014));
#265246=CARTESIAN_POINT('Ctrl Pts',(-10.4150370250001,15.2,-0.298029998000011));
#265247=CARTESIAN_POINT('Ctrl Pts',(-10.4162970050001,15.2,-0.298227073000015));
#265248=CARTESIAN_POINT('Ctrl Pts',(-10.4175653100001,15.2,-0.298426711000013));
#265249=CARTESIAN_POINT('Ctrl Pts',(-10.4188419160001,15.2,-0.298628922000015));
#265250=CARTESIAN_POINT('Ctrl Pts',(-10.4201267970001,15.2,-0.298833719000013));
#265251=CARTESIAN_POINT('Ctrl Pts',(-10.4214199300001,15.2,-0.299041114000014));
#265252=CARTESIAN_POINT('Ctrl Pts',(-10.4227212920001,15.2,-0.299251118000012));
#265253=CARTESIAN_POINT('Ctrl Pts',(-10.4240308570001,15.2,-0.299463743000015));
#265254=CARTESIAN_POINT('Ctrl Pts',(-10.4253486020001,15.2,-0.299679001000013));
#265255=CARTESIAN_POINT('Ctrl Pts',(-10.4266745030001,15.2,-0.299896903000012));
#265256=CARTESIAN_POINT('Ctrl Pts',(-10.4280085350001,15.2,-0.300117461000013));
#265257=CARTESIAN_POINT('Ctrl Pts',(-10.4293506770001,15.2,-0.300340686000014));
#265258=CARTESIAN_POINT('Ctrl Pts',(-10.4307009030001,15.2,-0.300566590000013));
#265259=CARTESIAN_POINT('Ctrl Pts',(-10.4320591910001,15.2,-0.300795184000013));
#265260=CARTESIAN_POINT('Ctrl Pts',(-10.4334255170001,15.2,-0.301026479000015));
#265261=CARTESIAN_POINT('Ctrl Pts',(-10.4347998580001,15.2,-0.301260488000015));
#265262=CARTESIAN_POINT('Ctrl Pts',(-10.4361821910001,15.2,-0.301497219000013));
#265263=CARTESIAN_POINT('Ctrl Pts',(-10.4375724920001,15.2,-0.301736686000016));
#265264=CARTESIAN_POINT('Ctrl Pts',(-10.4389707380001,15.2,-0.301978898000015));
#265265=CARTESIAN_POINT('Ctrl Pts',(-10.4403769080001,15.2,-0.302223867000015));
#265266=CARTESIAN_POINT('Ctrl Pts',(-10.4417909780001,15.2,-0.302471605000014));
#265267=CARTESIAN_POINT('Ctrl Pts',(-10.4432129240001,15.2,-0.302722121000016));
#265268=CARTESIAN_POINT('Ctrl Pts',(-10.4446427250001,15.2,-0.302975426000014));
#265269=CARTESIAN_POINT('Ctrl Pts',(-10.4460803580001,15.2,-0.303231532000012));
#265270=CARTESIAN_POINT('Ctrl Pts',(-10.4475258000001,15.2,-0.303490448000012));
#265271=CARTESIAN_POINT('Ctrl Pts',(-10.4489790300001,15.2,-0.303752186000015));
#265272=CARTESIAN_POINT('Ctrl Pts',(-10.4504400240001,15.2,-0.304016756000016));
#265273=CARTESIAN_POINT('Ctrl Pts',(-10.4519087610001,15.2,-0.304284170000013));
#265274=CARTESIAN_POINT('Ctrl Pts',(-10.4533852190001,15.2,-0.304554436000015));
#265275=CARTESIAN_POINT('Ctrl Pts',(-10.4548693740001,15.2,-0.304827566000014));
#265276=CARTESIAN_POINT('Ctrl Pts',(-10.4563612070001,15.2,-0.305103570000016));
#265277=CARTESIAN_POINT('Ctrl Pts',(-10.4578606950001,15.2,-0.305382458000012));
#265278=CARTESIAN_POINT('Ctrl Pts',(-10.4593678150001,15.2,-0.305664241000017));
#265279=CARTESIAN_POINT('Ctrl Pts',(-10.4608825450001,15.2,-0.305948928000017));
#265280=CARTESIAN_POINT('Ctrl Pts',(-10.4624048670001,15.2,-0.306236531000015));
#265281=CARTESIAN_POINT('Ctrl Pts',(-10.4639347550001,15.2,-0.306527058000015));
#265282=CARTESIAN_POINT('Ctrl Pts',(-10.4654721910001,15.2,-0.306820521000013));
#265283=CARTESIAN_POINT('Ctrl Pts',(-10.4670171510001,15.2,-0.307116929000015));
#265284=CARTESIAN_POINT('Ctrl Pts',(-10.4685696160001,15.2,-0.307416292000013));
#265285=CARTESIAN_POINT('Ctrl Pts',(-10.4701295620001,15.2,-0.307718619000017));
#265286=CARTESIAN_POINT('Ctrl Pts',(-10.4716969700001,15.2,-0.308023923000014));
#265287=CARTESIAN_POINT('Ctrl Pts',(-10.4732718190001,15.2,-0.308332210000017));
#265288=CARTESIAN_POINT('Ctrl Pts',(-10.4748540860001,15.2,-0.308643492000016));
#265289=CARTESIAN_POINT('Ctrl Pts',(-10.4764437530001,15.2,-0.308957777000014));
#265290=CARTESIAN_POINT('Ctrl Pts',(-10.4780407970001,15.2,-0.309275076000013));
#265291=CARTESIAN_POINT('Ctrl Pts',(-10.4796451980001,15.2,-0.309595399000013));
#265292=CARTESIAN_POINT('Ctrl Pts',(-10.4812569350001,15.2,-0.309918754000016));
#265293=CARTESIAN_POINT('Ctrl Pts',(-10.4828759870001,15.2,-0.310245152000017));
#265294=CARTESIAN_POINT('Ctrl Pts',(-10.4845023350001,15.2,-0.310574602000013));
#265295=CARTESIAN_POINT('Ctrl Pts',(-10.4861359570001,15.2,-0.310907114000014));
#265296=CARTESIAN_POINT('Ctrl Pts',(-10.4877768330001,15.2,-0.311242696000011));
#265297=CARTESIAN_POINT('Ctrl Pts',(-10.4894249420001,15.2,-0.311581357000015));
#265298=CARTESIAN_POINT('Ctrl Pts',(-10.4910802660001,15.2,-0.311923107000016));
#265299=CARTESIAN_POINT('Ctrl Pts',(-10.4927427830001,15.2,-0.312267956000016));
#265300=CARTESIAN_POINT('Ctrl Pts',(-10.4944124730001,15.2,-0.312615913000016));
#265301=CARTESIAN_POINT('Ctrl Pts',(-10.4960893160001,15.2,-0.312966987000016));
#265302=CARTESIAN_POINT('Ctrl Pts',(-10.4977732930001,15.2,-0.313321185000017));
#265303=CARTESIAN_POINT('Ctrl Pts',(-10.4994643820001,15.2,-0.313678519000016));
#265304=CARTESIAN_POINT('Ctrl Pts',(-10.5011625650001,15.2,-0.314038997000012));
#265305=CARTESIAN_POINT('Ctrl Pts',(-10.5028678220001,15.2,-0.314402627000017));
#265306=CARTESIAN_POINT('Ctrl Pts',(-10.5049225963254,15.2,-0.314842777384019));
#265307=CARTESIAN_POINT('Ctrl Pts',(-10.5069879188374,15.2,-0.315287684308014));
#265308=CARTESIAN_POINT('Ctrl Pts',(-10.5090637571627,15.2,-0.315737363692019));
#265309=CARTESIAN_POINT('Ctrl Pts',(-10.5111500674852,15.2,-0.316191834574724));
#265310=CARTESIAN_POINT('Ctrl Pts',(-10.5132468120001,15.2,-0.316651113000015));
#265311=CARTESIAN_POINT('Ctrl Pts',(-10.5150010370001,15.2,-0.317037060000014));
#265312=CARTESIAN_POINT('Ctrl Pts',(-10.5167621800001,15.2,-0.317426229000013));
#265313=CARTESIAN_POINT('Ctrl Pts',(-10.5185302210001,15.2,-0.317818628000013));
#265314=CARTESIAN_POINT('Ctrl Pts',(-10.5203051430001,15.2,-0.318214269000014));
#265315=CARTESIAN_POINT('Ctrl Pts',(-10.5220869250001,15.2,-0.318613157000014));
#265316=CARTESIAN_POINT('Ctrl Pts',(-10.5238755480001,15.2,-0.319015302000012));
#265317=CARTESIAN_POINT('Ctrl Pts',(-10.5256709940001,15.2,-0.319420713000014));
#265318=CARTESIAN_POINT('Ctrl Pts',(-10.5274732440001,15.2,-0.319829396000015));
#265319=CARTESIAN_POINT('Ctrl Pts',(-10.5292822790001,15.2,-0.320241361000013));
#265320=CARTESIAN_POINT('Ctrl Pts',(-10.5310980810001,15.2,-0.320656616000012));
#265321=CARTESIAN_POINT('Ctrl Pts',(-10.5329206290001,15.2,-0.321075169000018));
#265322=CARTESIAN_POINT('Ctrl Pts',(-10.5347499080001,15.2,-0.321497029000017));
#265323=CARTESIAN_POINT('Ctrl Pts',(-10.5365858960001,15.2,-0.321922203000016));
#265324=CARTESIAN_POINT('Ctrl Pts',(-10.5384285770001,15.2,-0.322350700000014));
#265325=CARTESIAN_POINT('Ctrl Pts',(-10.5402779310001,15.2,-0.322782527000012));
#265326=CARTESIAN_POINT('Ctrl Pts',(-10.5421339400001,15.2,-0.323217694000015));
#265327=CARTESIAN_POINT('Ctrl Pts',(-10.5439965860001,15.2,-0.323656207000016));
#265328=CARTESIAN_POINT('Ctrl Pts',(-10.5458658520001,15.2,-0.324098074000014));
#265329=CARTESIAN_POINT('Ctrl Pts',(-10.5477417170001,15.2,-0.324543305000016));
#265330=CARTESIAN_POINT('Ctrl Pts',(-10.5496241650001,15.2,-0.324991905000012));
#265331=CARTESIAN_POINT('Ctrl Pts',(-10.5515131770001,15.2,-0.325443883000016));
#265332=CARTESIAN_POINT('Ctrl Pts',(-10.5534087350001,15.2,-0.325899248000017));
#265333=CARTESIAN_POINT('Ctrl Pts',(-10.5553108210001,15.2,-0.326358007000014));
#265334=CARTESIAN_POINT('Ctrl Pts',(-10.5572194180001,15.2,-0.326820167000013));
#265335=CARTESIAN_POINT('Ctrl Pts',(-10.5591345070001,15.2,-0.327285736000014));
#265336=CARTESIAN_POINT('Ctrl Pts',(-10.5610560710001,15.2,-0.327754722000013));
#265337=CARTESIAN_POINT('Ctrl Pts',(-10.5629840910001,15.2,-0.328227133000016));
#265338=CARTESIAN_POINT('Ctrl Pts',(-10.5649185510001,15.2,-0.328702975000015));
#265339=CARTESIAN_POINT('Ctrl Pts',(-10.5668594320001,15.2,-0.329182256000013));
#265340=CARTESIAN_POINT('Ctrl Pts',(-10.5688067180001,15.2,-0.329664985000013));
#265341=CARTESIAN_POINT('Ctrl Pts',(-10.5707603900001,15.2,-0.330151169000015));
#265342=CARTESIAN_POINT('Ctrl Pts',(-10.5727204310001,15.2,-0.330640814000014));
#265343=CARTESIAN_POINT('Ctrl Pts',(-10.5746868240001,15.2,-0.331133928000016));
#265344=CARTESIAN_POINT('Ctrl Pts',(-10.5766595510001,15.2,-0.331630519000012));
#265345=CARTESIAN_POINT('Ctrl Pts',(-10.5786385950001,15.2,-0.332130595000013));
#265346=CARTESIAN_POINT('Ctrl Pts',(-10.5806239380001,15.2,-0.332634161000014));
#265347=CARTESIAN_POINT('Ctrl Pts',(-10.5826155640001,15.2,-0.333141226000016));
#265348=CARTESIAN_POINT('Ctrl Pts',(-10.5846134550001,15.2,-0.333651796000014));
#265349=CARTESIAN_POINT('Ctrl Pts',(-10.5866175950001,15.2,-0.334165879000015));
#265350=CARTESIAN_POINT('Ctrl Pts',(-10.5886279650001,15.2,-0.334683483000013));
#265351=CARTESIAN_POINT('Ctrl Pts',(-10.5906445490001,15.2,-0.335204613000015));
#265352=CARTESIAN_POINT('Ctrl Pts',(-10.5926673320001,15.2,-0.335729278000017));
#265353=CARTESIAN_POINT('Ctrl Pts',(-10.5946962940001,15.2,-0.336257483000013));
#265354=CARTESIAN_POINT('Ctrl Pts',(-10.5967314190001,15.2,-0.336789237000015));
#265355=CARTESIAN_POINT('Ctrl Pts',(-10.5987726910001,15.2,-0.337324546000013));
#265356=CARTESIAN_POINT('Ctrl Pts',(-10.6008200940001,15.2,-0.337863418000013));
#265357=CARTESIAN_POINT('Ctrl Pts',(-10.6028736090001,15.2,-0.338405859000015));
#265358=CARTESIAN_POINT('Ctrl Pts',(-10.6049332210001,15.2,-0.338951874000015));
#265359=CARTESIAN_POINT('Ctrl Pts',(-10.6069989120001,15.2,-0.339501473000015));
#265360=CARTESIAN_POINT('Ctrl Pts',(-10.6090706680001,15.2,-0.340054662000018));
#265361=CARTESIAN_POINT('Ctrl Pts',(-10.6111484700001,15.2,-0.340611447000012));
#265362=CARTESIAN_POINT('Ctrl Pts',(-10.6132323020001,15.2,-0.341171835000011));
#265363=CARTESIAN_POINT('Ctrl Pts',(-10.6153221490001,15.2,-0.341735833000012));
#265364=CARTESIAN_POINT('Ctrl Pts',(-10.6174179920001,15.2,-0.342303448000014));
#265365=CARTESIAN_POINT('Ctrl Pts',(-10.6195198180001,15.2,-0.342874685000014));
#265366=CARTESIAN_POINT('Ctrl Pts',(-10.6216276080001,15.2,-0.343449552000017));
#265367=CARTESIAN_POINT('Ctrl Pts',(-10.6237413470001,15.2,-0.344028056000014));
#265368=CARTESIAN_POINT('Ctrl Pts',(-10.6258610180001,15.2,-0.344610202000015));
#265369=CARTESIAN_POINT('Ctrl Pts',(-10.6279866070001,15.2,-0.345195998000012));
#265370=CARTESIAN_POINT('Ctrl Pts',(-10.6301180950001,15.2,-0.345785450000013));
#265371=CARTESIAN_POINT('Ctrl Pts',(-10.6322554680001,15.2,-0.346378564000016));
#265372=CARTESIAN_POINT('Ctrl Pts',(-10.6343987090001,15.2,-0.346975347000011));
#265373=CARTESIAN_POINT('Ctrl Pts',(-10.6365478020001,15.2,-0.347575805000013));
#265374=CARTESIAN_POINT('Ctrl Pts',(-10.6387027320001,15.2,-0.348179945000013));
#265375=CARTESIAN_POINT('Ctrl Pts',(-10.6408634830001,15.2,-0.348787773000012));
#265376=CARTESIAN_POINT('Ctrl Pts',(-10.6430300390001,15.2,-0.349399295000015));
#265377=CARTESIAN_POINT('Ctrl Pts',(-10.6452023830001,15.2,-0.350014516000012));
#265378=CARTESIAN_POINT('Ctrl Pts',(-10.6473805010001,15.2,-0.350633446000015));
#265379=CARTESIAN_POINT('Ctrl Pts',(-10.6495643770001,15.2,-0.351256088000014));
#265380=CARTESIAN_POINT('Ctrl Pts',(-10.6517539940001,15.2,-0.351882449000014));
#265381=CARTESIAN_POINT('Ctrl Pts',(-10.6539493380001,15.2,-0.352512536000016));
#265382=CARTESIAN_POINT('Ctrl Pts',(-10.6561503920001,15.2,-0.353146354000016));
#265383=CARTESIAN_POINT('Ctrl Pts',(-10.6583571410001,15.2,-0.353783910000014));
#265384=CARTESIAN_POINT('Ctrl Pts',(-10.6605695710001,15.2,-0.354425210000016));
#265385=CARTESIAN_POINT('Ctrl Pts',(-10.6627876650001,15.2,-0.355070259000012));
#265386=CARTESIAN_POINT('Ctrl Pts',(-10.6650114070001,15.2,-0.355719063000013));
#265387=CARTESIAN_POINT('Ctrl Pts',(-10.6672407830001,15.2,-0.356371629000014));
#265388=CARTESIAN_POINT('Ctrl Pts',(-10.6694757780001,15.2,-0.357027964000016));
#265389=CARTESIAN_POINT('Ctrl Pts',(-10.6717163760001,15.2,-0.357688071000015));
#265390=CARTESIAN_POINT('Ctrl Pts',(-10.6739625620001,15.2,-0.358351959000016));
#265391=CARTESIAN_POINT('Ctrl Pts',(-10.6762143200001,15.2,-0.359019631000015));
#265392=CARTESIAN_POINT('Ctrl Pts',(-10.6784716350001,15.2,-0.359691096000017));
#265393=CARTESIAN_POINT('Ctrl Pts',(-10.6807344940001,15.2,-0.360366356000017));
#265394=CARTESIAN_POINT('Ctrl Pts',(-10.6830028780001,15.2,-0.361045420000017));
#265395=CARTESIAN_POINT('Ctrl Pts',(-10.6852767760001,15.2,-0.361728293000017));
#265396=CARTESIAN_POINT('Ctrl Pts',(-10.6875561710001,15.2,-0.362414981000012));
#265397=CARTESIAN_POINT('Ctrl Pts',(-10.6898410480001,15.2,-0.363105487000013));
#265398=CARTESIAN_POINT('Ctrl Pts',(-10.6921313930001,15.2,-0.363799821000015));
#265399=CARTESIAN_POINT('Ctrl Pts',(-10.6944271900001,15.2,-0.364497985000014));
#265400=CARTESIAN_POINT('Ctrl Pts',(-10.6967284250001,15.2,-0.365199987000011));
#265401=CARTESIAN_POINT('Ctrl Pts',(-10.6990350820001,15.2,-0.365905831000015));
#265402=CARTESIAN_POINT('Ctrl Pts',(-10.7018095613513,15.2,-0.366757461446432));
#265403=CARTESIAN_POINT('Ctrl Pts',(-10.7045921314508,15.2,-0.367614872815749));
#265404=CARTESIAN_POINT('Ctrl Pts',(-10.7073827605493,15.2,-0.368478077184284));
#265405=CARTESIAN_POINT('Ctrl Pts',(-10.7101814229016,15.2,-0.369347083631473));
#265406=CARTESIAN_POINT('Ctrl Pts',(-10.7129880860001,15.2,-0.370221904000014));
#265407=CARTESIAN_POINT('Ctrl Pts',(-10.7153322940001,15.2,-0.370954801000014));
#265408=CARTESIAN_POINT('Ctrl Pts',(-10.7176818070001,15.2,-0.371691587000011));
#265409=CARTESIAN_POINT('Ctrl Pts',(-10.7200366120001,15.2,-0.372432264000011));
#265410=CARTESIAN_POINT('Ctrl Pts',(-10.7223966940001,15.2,-0.373176838000013));
#265411=CARTESIAN_POINT('Ctrl Pts',(-10.7247620380001,15.2,-0.373925315000014));
#265412=CARTESIAN_POINT('Ctrl Pts',(-10.7271326310001,15.2,-0.374677700000015));
#265413=CARTESIAN_POINT('Ctrl Pts',(-10.7295084580001,15.2,-0.375433998000014));
#265414=CARTESIAN_POINT('Ctrl Pts',(-10.7318895040001,15.2,-0.376194215000014));
#265415=CARTESIAN_POINT('Ctrl Pts',(-10.7342757570001,15.2,-0.376958356000014));
#265416=CARTESIAN_POINT('Ctrl Pts',(-10.7366672000001,15.2,-0.377726425000016));
#265417=CARTESIAN_POINT('Ctrl Pts',(-10.7390638200001,15.2,-0.378498429000014));
#265418=CARTESIAN_POINT('Ctrl Pts',(-10.7414656040001,15.2,-0.379274372000014));
#265419=CARTESIAN_POINT('Ctrl Pts',(-10.7438725370001,15.2,-0.380054260000016));
#265420=CARTESIAN_POINT('Ctrl Pts',(-10.7462846040001,15.2,-0.380838098000016));
#265421=CARTESIAN_POINT('Ctrl Pts',(-10.7487017930001,15.2,-0.381625889000015));
#265422=CARTESIAN_POINT('Ctrl Pts',(-10.7511240870001,15.2,-0.382417641000017));
#265423=CARTESIAN_POINT('Ctrl Pts',(-10.7535514750001,15.2,-0.383213358000014));
#265424=CARTESIAN_POINT('Ctrl Pts',(-10.7559839420001,15.2,-0.384013044000016));
#265425=CARTESIAN_POINT('Ctrl Pts',(-10.7584214740001,15.2,-0.384816705000013));
#265426=CARTESIAN_POINT('Ctrl Pts',(-10.7608640580001,15.2,-0.385624345000015));
#265427=CARTESIAN_POINT('Ctrl Pts',(-10.7633116780001,15.2,-0.386435971000014));
#265428=CARTESIAN_POINT('Ctrl Pts',(-10.7657643230001,15.2,-0.387251586000015));
#265429=CARTESIAN_POINT('Ctrl Pts',(-10.7682219760001,15.2,-0.388071196000013));
#265430=CARTESIAN_POINT('Ctrl Pts',(-10.7706846260001,15.2,-0.388894805000017));
#265431=CARTESIAN_POINT('Ctrl Pts',(-10.7731522590001,15.2,-0.389722418000016));
#265432=CARTESIAN_POINT('Ctrl Pts',(-10.7756248610001,15.2,-0.390554041000013));
#265433=CARTESIAN_POINT('Ctrl Pts',(-10.7781024170001,15.2,-0.391389677000014));
#265434=CARTESIAN_POINT('Ctrl Pts',(-10.7805849160001,15.2,-0.392229332000014));
#265435=CARTESIAN_POINT('Ctrl Pts',(-10.7830723410001,15.2,-0.393073009000013));
#265436=CARTESIAN_POINT('Ctrl Pts',(-10.7855646820001,15.2,-0.393920716000018));
#265437=CARTESIAN_POINT('Ctrl Pts',(-10.7880619230001,15.2,-0.394772456000014));
#265438=CARTESIAN_POINT('Ctrl Pts',(-10.7905640520001,15.2,-0.395628232000016));
#265439=CARTESIAN_POINT('Ctrl Pts',(-10.7930710550001,15.2,-0.396488052000015));
#265440=CARTESIAN_POINT('Ctrl Pts',(-10.7955829180001,15.2,-0.397351917000015));
#265441=CARTESIAN_POINT('Ctrl Pts',(-10.7980996290001,15.2,-0.398219835000013));
#265442=CARTESIAN_POINT('Ctrl Pts',(-10.8006211740001,15.2,-0.399091809000014));
#265443=CARTESIAN_POINT('Ctrl Pts',(-10.8031475400001,15.2,-0.399967843000013));
#265444=CARTESIAN_POINT('Ctrl Pts',(-10.8056787130001,15.2,-0.400847944000016));
#265445=CARTESIAN_POINT('Ctrl Pts',(-10.8082146790001,15.2,-0.401732113000013));
#265446=CARTESIAN_POINT('Ctrl Pts',(-10.8107554270001,15.2,-0.402620357000014));
#265447=CARTESIAN_POINT('Ctrl Pts',(-10.8133009430001,15.2,-0.403512679000015));
#265448=CARTESIAN_POINT('Ctrl Pts',(-10.8158512130001,15.2,-0.404409086000013));
#265449=CARTESIAN_POINT('Ctrl Pts',(-10.8184062250001,15.2,-0.405309580000015));
#265450=CARTESIAN_POINT('Ctrl Pts',(-10.8209659650001,15.2,-0.406214166000014));
#265451=CARTESIAN_POINT('Ctrl Pts',(-10.8235304190001,15.2,-0.407122849000014));
#265452=CARTESIAN_POINT('Ctrl Pts',(-10.8260995770001,15.2,-0.408035633000012));
#265453=CARTESIAN_POINT('Ctrl Pts',(-10.8286734240001,15.2,-0.408952523000017));
#265454=CARTESIAN_POINT('Ctrl Pts',(-10.8312519470001,15.2,-0.409873522000015));
#265455=CARTESIAN_POINT('Ctrl Pts',(-10.8338351330001,15.2,-0.410798635000016));
#265456=CARTESIAN_POINT('Ctrl Pts',(-10.8364229690001,15.2,-0.411727867000016));
#265457=CARTESIAN_POINT('Ctrl Pts',(-10.8390154430001,15.2,-0.412661222000015));
#265458=CARTESIAN_POINT('Ctrl Pts',(-10.8416125420001,15.2,-0.413598703000013));
#265459=CARTESIAN_POINT('Ctrl Pts',(-10.8442142530001,15.2,-0.414540317000016));
#265460=CARTESIAN_POINT('Ctrl Pts',(-10.8468205630001,15.2,-0.415486065000015));
#265461=CARTESIAN_POINT('Ctrl Pts',(-10.8494314580001,15.2,-0.416435953000014));
#265462=CARTESIAN_POINT('Ctrl Pts',(-10.8520469280001,15.2,-0.417389985000014));
#265463=CARTESIAN_POINT('Ctrl Pts',(-10.8546669570001,15.2,-0.418348165000015));
#265464=CARTESIAN_POINT('Ctrl Pts',(-10.8572915350001,15.2,-0.419310498000014));
#265465=CARTESIAN_POINT('Ctrl Pts',(-10.8599206490001,15.2,-0.420276987000014));
#265466=CARTESIAN_POINT('Ctrl Pts',(-10.8625542860001,15.2,-0.421247636000013));
#265467=CARTESIAN_POINT('Ctrl Pts',(-10.8651924320001,15.2,-0.422222450000014));
#265468=CARTESIAN_POINT('Ctrl Pts',(-10.8678350770001,15.2,-0.423201432000013));
#265469=CARTESIAN_POINT('Ctrl Pts',(-10.8704822050001,15.2,-0.424184588000016));
#265470=CARTESIAN_POINT('Ctrl Pts',(-10.8731338070001,15.2,-0.425171920000014));
#265471=CARTESIAN_POINT('Ctrl Pts',(-10.8757898690001,15.2,-0.426163433000015));
#265472=CARTESIAN_POINT('Ctrl Pts',(-10.8784503780001,15.2,-0.427159131000017));
#265473=CARTESIAN_POINT('Ctrl Pts',(-10.8811153220001,15.2,-0.428159018000014));
#265474=CARTESIAN_POINT('Ctrl Pts',(-10.8837846900001,15.2,-0.429163097000016));
#265475=CARTESIAN_POINT('Ctrl Pts',(-10.8864584680001,15.2,-0.430171373000015));
#265476=CARTESIAN_POINT('Ctrl Pts',(-10.8891366430001,15.2,-0.431183850000014));
#265477=CARTESIAN_POINT('Ctrl Pts',(-10.8918192040001,15.2,-0.432200531000015));
#265478=CARTESIAN_POINT('Ctrl Pts',(-10.8945061380001,15.2,-0.433221421000014));
#265479=CARTESIAN_POINT('Ctrl Pts',(-10.8971974330001,15.2,-0.434246522000015));
#265480=CARTESIAN_POINT('Ctrl Pts',(-10.8998930780001,15.2,-0.435275840000013));
#265481=CARTESIAN_POINT('Ctrl Pts',(-10.9025930590001,15.2,-0.436309378000015));
#265482=CARTESIAN_POINT('Ctrl Pts',(-10.9052973640001,15.2,-0.437347141000015));
#265483=CARTESIAN_POINT('Ctrl Pts',(-10.9080059810001,15.2,-0.438389130000014));
#265484=CARTESIAN_POINT('Ctrl Pts',(-10.9107188990001,15.2,-0.439435350000017));
#265485=CARTESIAN_POINT('Ctrl Pts',(-10.9134361040001,15.2,-0.440485807000015));
#265486=CARTESIAN_POINT('Ctrl Pts',(-10.9161575860001,15.2,-0.441540501000013));
#265487=CARTESIAN_POINT('Ctrl Pts',(-10.9188833300001,15.2,-0.442599438000015));
#265488=CARTESIAN_POINT('Ctrl Pts',(-10.9216133270001,15.2,-0.443662622000014));
#265489=CARTESIAN_POINT('Ctrl Pts',(-10.9243475630001,15.2,-0.444730056000013));
#265490=CARTESIAN_POINT('Ctrl Pts',(-10.9270860270001,15.2,-0.445801743000014));
#265491=CARTESIAN_POINT('Ctrl Pts',(-10.9298287070001,15.2,-0.446877689000011));
#265492=CARTESIAN_POINT('Ctrl Pts',(-10.9325755900001,15.2,-0.447957894000015));
#265493=CARTESIAN_POINT('Ctrl Pts',(-10.9353266640001,15.2,-0.449042364000016));
#265494=CARTESIAN_POINT('Ctrl Pts',(-10.9380819200001,15.2,-0.450131103000011));
#265495=CARTESIAN_POINT('Ctrl Pts',(-10.9408413420001,15.2,-0.451224112000013));
#265496=CARTESIAN_POINT('Ctrl Pts',(-10.9436049220001,15.2,-0.452321397000013));
#265497=CARTESIAN_POINT('Ctrl Pts',(-10.9463726460001,15.2,-0.453422962000012));
#265498=CARTESIAN_POINT('Ctrl Pts',(-10.9491445020001,15.2,-0.454528810000014));
#265499=CARTESIAN_POINT('Ctrl Pts',(-10.9519204780001,15.2,-0.455638942000016));
#265500=CARTESIAN_POINT('Ctrl Pts',(-10.9547005640001,15.2,-0.456753364000013));
#265501=CARTESIAN_POINT('Ctrl Pts',(-10.9574847480001,15.2,-0.457872080000015));
#265502=CARTESIAN_POINT('Ctrl Pts',(-10.9602730170001,15.2,-0.458995091000016));
#265503=CARTESIAN_POINT('Ctrl Pts',(-10.9630653590001,15.2,-0.460122402000014));
#265504=CARTESIAN_POINT('Ctrl Pts',(-10.9658617640001,15.2,-0.461254017000012));
#265505=CARTESIAN_POINT('Ctrl Pts',(-10.9686622200001,15.2,-0.462389938000012));
#265506=CARTESIAN_POINT('Ctrl Pts',(-10.9714667150001,15.2,-0.463530170000013));
#265507=CARTESIAN_POINT('Ctrl Pts',(-10.9742752370001,15.2,-0.464674714000015));
#265508=CARTESIAN_POINT('Ctrl Pts',(-10.9770877740001,15.2,-0.465823575000015));
#265509=CARTESIAN_POINT('Ctrl Pts',(-10.9799043170001,15.2,-0.466976757000013));
#265510=CARTESIAN_POINT('Ctrl Pts',(-10.9827248520001,15.2,-0.468134263000017));
#265511=CARTESIAN_POINT('Ctrl Pts',(-10.9855493680001,15.2,-0.469296094000011));
#265512=CARTESIAN_POINT('Ctrl Pts',(-10.9883778540001,15.2,-0.470462257000013));
#265513=CARTESIAN_POINT('Ctrl Pts',(-10.9912102990001,15.2,-0.471632753000013));
#265514=CARTESIAN_POINT('Ctrl Pts',(-10.9940466900001,15.2,-0.472807585000012));
#265515=CARTESIAN_POINT('Ctrl Pts',(-10.9968870170001,15.2,-0.473986757000016));
#265516=CARTESIAN_POINT('Ctrl Pts',(-10.9997312680001,15.2,-0.475170273000014));
#265517=CARTESIAN_POINT('Ctrl Pts',(-11.0025794320001,15.2,-0.476358134000012));
#265518=CARTESIAN_POINT('Ctrl Pts',(-11.0054314970001,15.2,-0.477550346000015));
#265519=CARTESIAN_POINT('Ctrl Pts',(-11.0082874530001,15.2,-0.478746910000014));
#265520=CARTESIAN_POINT('Ctrl Pts',(-11.0111472870001,15.2,-0.479947831000014));
#265521=CARTESIAN_POINT('Ctrl Pts',(-11.0140109890001,15.2,-0.481153110000014));
#265522=CARTESIAN_POINT('Ctrl Pts',(-11.0168785470001,15.2,-0.482362752000016));
#265523=CARTESIAN_POINT('Ctrl Pts',(-11.0197499510001,15.2,-0.483576758000015));
#265524=CARTESIAN_POINT('Ctrl Pts',(-11.0226251880001,15.2,-0.484795134000016));
#265525=CARTESIAN_POINT('Ctrl Pts',(-11.0255042470001,15.2,-0.486017881000014));
#265526=CARTESIAN_POINT('Ctrl Pts',(-11.0283871190001,15.2,-0.487245003000014));
#265527=CARTESIAN_POINT('Ctrl Pts',(-11.0312737910001,15.2,-0.488476502000013));
#265528=CARTESIAN_POINT('Ctrl Pts',(-11.0341642530001,15.2,-0.489712383000014));
#265529=CARTESIAN_POINT('Ctrl Pts',(-11.0370584920001,15.2,-0.490952646000018));
#265530=CARTESIAN_POINT('Ctrl Pts',(-11.0399564980001,15.2,-0.492197297000012));
#265531=CARTESIAN_POINT('Ctrl Pts',(-11.0428582610001,15.2,-0.493446338000014));
#265532=CARTESIAN_POINT('Ctrl Pts',(-11.0457637680001,15.2,-0.494699772000011));
#265533=CARTESIAN_POINT('Ctrl Pts',(-11.0486730100001,15.2,-0.495957601000012));
#265534=CARTESIAN_POINT('Ctrl Pts',(-11.0515859750001,15.2,-0.497219830000013));
#265535=CARTESIAN_POINT('Ctrl Pts',(-11.0545026510001,15.2,-0.498486460000014));
#265536=CARTESIAN_POINT('Ctrl Pts',(-11.0574230290001,15.2,-0.499757494000015));
#265537=CARTESIAN_POINT('Ctrl Pts',(-11.0603470970001,15.2,-0.501032937000012));
#265538=CARTESIAN_POINT('Ctrl Pts',(-11.0632748440001,15.2,-0.502312789000015));
#265539=CARTESIAN_POINT('Ctrl Pts',(-11.0662062590001,15.2,-0.503597056000018));
#265540=CARTESIAN_POINT('Ctrl Pts',(-11.0691413320001,15.2,-0.504885738000014));
#265541=CARTESIAN_POINT('Ctrl Pts',(-11.0720800520001,15.2,-0.506178839000011));
#265542=CARTESIAN_POINT('Ctrl Pts',(-11.0750224080001,15.2,-0.507476362000014));
#265543=CARTESIAN_POINT('Ctrl Pts',(-11.0779683880001,15.2,-0.508778311000011));
#265544=CARTESIAN_POINT('Ctrl Pts',(-11.0809179820001,15.2,-0.510084687000014));
#265545=CARTESIAN_POINT('Ctrl Pts',(-11.0838711810001,15.2,-0.511395492000015));
#265546=CARTESIAN_POINT('Ctrl Pts',(-11.0868279720001,15.2,-0.512710732000015));
#265547=CARTESIAN_POINT('Ctrl Pts',(-11.0897883450001,15.2,-0.514030406000017));
#265548=CARTESIAN_POINT('Ctrl Pts',(-11.0927522890001,15.2,-0.515354521000013));
#265549=CARTESIAN_POINT('Ctrl Pts',(-11.0957197940001,15.2,-0.516683076000017));
#265550=CARTESIAN_POINT('Ctrl Pts',(-11.0986908480001,15.2,-0.518016075000016));
#265551=CARTESIAN_POINT('Ctrl Pts',(-11.1016654420001,15.2,-0.519353522000015));
#265552=CARTESIAN_POINT('Ctrl Pts',(-11.1046435640001,15.2,-0.520695418000017));
#265553=CARTESIAN_POINT('Ctrl Pts',(-11.1076252050001,15.2,-0.522041766000014));
#265554=CARTESIAN_POINT('Ctrl Pts',(-11.1106103520001,15.2,-0.523392569000016));
#265555=CARTESIAN_POINT('Ctrl Pts',(-11.1135989970001,15.2,-0.524747830000014));
#265556=CARTESIAN_POINT('Ctrl Pts',(-11.1165911290001,15.2,-0.526107550000017));
#265557=CARTESIAN_POINT('Ctrl Pts',(-11.1195867360001,15.2,-0.527471735000016));
#265558=CARTESIAN_POINT('Ctrl Pts',(-11.1225858080001,15.2,-0.528840384000016));
#265559=CARTESIAN_POINT('Ctrl Pts',(-11.1255883350001,15.2,-0.530213501000016));
#265560=CARTESIAN_POINT('Ctrl Pts',(-11.1285943060001,15.2,-0.531591090000014));
#265561=CARTESIAN_POINT('Ctrl Pts',(-11.1316037120001,15.2,-0.532973151000018));
#265562=CARTESIAN_POINT('Ctrl Pts',(-11.1346165400001,15.2,-0.534359689000015));
#265563=CARTESIAN_POINT('Ctrl Pts',(-11.1376327810001,15.2,-0.535750705000013));
#265564=CARTESIAN_POINT('Ctrl Pts',(-11.1406524250001,15.2,-0.537146200000014));
#265565=CARTESIAN_POINT('Ctrl Pts',(-11.1436754620001,15.2,-0.538546181000013));
#265566=CARTESIAN_POINT('Ctrl Pts',(-11.1467018790001,15.2,-0.539950647000014));
#265567=CARTESIAN_POINT('Ctrl Pts',(-11.1497316690001,15.2,-0.541359602000018));
#265568=CARTESIAN_POINT('Ctrl Pts',(-11.1527648200001,15.2,-0.542773047000011));
#265569=CARTESIAN_POINT('Ctrl Pts',(-11.1558013220001,15.2,-0.544190986000017));
#265570=CARTESIAN_POINT('Ctrl Pts',(-11.1588411640001,15.2,-0.545613421000013));
#265571=CARTESIAN_POINT('Ctrl Pts',(-11.1618843360001,15.2,-0.547040354000017));
#265572=CARTESIAN_POINT('Ctrl Pts',(-11.1649308290001,15.2,-0.548471788000011));
#265573=CARTESIAN_POINT('Ctrl Pts',(-11.1679806310001,15.2,-0.549907725000014));
#265574=CARTESIAN_POINT('Ctrl Pts',(-11.1710337330001,15.2,-0.551348168000012));
#265575=CARTESIAN_POINT('Ctrl Pts',(-11.1740901240001,15.2,-0.552793118000015));
#265576=CARTESIAN_POINT('Ctrl Pts',(-11.1771497950001,15.2,-0.554242580000013));
#265577=CARTESIAN_POINT('Ctrl Pts',(-11.1802127340001,15.2,-0.555696554000011));
#265578=CARTESIAN_POINT('Ctrl Pts',(-11.1832789320001,15.2,-0.557155042000015));
#265579=CARTESIAN_POINT('Ctrl Pts',(-11.1863483800001,15.2,-0.558618049000015));
#265580=CARTESIAN_POINT('Ctrl Pts',(-11.1894210660001,15.2,-0.560085575000016));
#265581=CARTESIAN_POINT('Ctrl Pts',(-11.1924969800001,15.2,-0.561557623000013));
#265582=CARTESIAN_POINT('Ctrl Pts',(-11.1955761130001,15.2,-0.563034196000016));
#265583=CARTESIAN_POINT('Ctrl Pts',(-11.1986584540001,15.2,-0.564515295000017));
#265584=CARTESIAN_POINT('Ctrl Pts',(-11.2017439940001,15.2,-0.566000924000014));
#265585=CARTESIAN_POINT('Ctrl Pts',(-11.2048327210001,15.2,-0.567491084000018));
#265586=CARTESIAN_POINT('Ctrl Pts',(-11.2079246280001,15.2,-0.568985776000015));
#265587=CARTESIAN_POINT('Ctrl Pts',(-11.2110197020001,15.2,-0.570485006000014));
#265588=CARTESIAN_POINT('Ctrl Pts',(-11.2141179350001,15.2,-0.571988772000012));
#265589=CARTESIAN_POINT('Ctrl Pts',(-11.2172193170001,15.2,-0.573497079000016));
#265590=CARTESIAN_POINT('Ctrl Pts',(-11.2203238380001,15.2,-0.575009928000014));
#265591=CARTESIAN_POINT('Ctrl Pts',(-11.2234314850001,15.2,-0.576527323000011));
#265592=CARTESIAN_POINT('Ctrl Pts',(-11.2265422530001,15.2,-0.578049263000011));
#265593=CARTESIAN_POINT('Ctrl Pts',(-11.2296561290001,15.2,-0.579575753000015));
#265594=CARTESIAN_POINT('Ctrl Pts',(-11.2327731030001,15.2,-0.581106794000017));
#265595=CARTESIAN_POINT('Ctrl Pts',(-11.2358931670001,15.2,-0.582642387000014));
#265596=CARTESIAN_POINT('Ctrl Pts',(-11.2390163100001,15.2,-0.584182538000011));
#265597=CARTESIAN_POINT('Ctrl Pts',(-11.2421425230001,15.2,-0.585727245000012));
#265598=CARTESIAN_POINT('Ctrl Pts',(-11.2452717950001,15.2,-0.587276511000017));
#265599=CARTESIAN_POINT('Ctrl Pts',(-11.2484041180001,15.2,-0.588830340000013));
#265600=CARTESIAN_POINT('Ctrl Pts',(-11.2515394790001,15.2,-0.590388732000013));
#265601=CARTESIAN_POINT('Ctrl Pts',(-11.2546778710001,15.2,-0.591951690000014));
#265602=CARTESIAN_POINT('Ctrl Pts',(-11.2578192840001,15.2,-0.593519216000011));
#265603=CARTESIAN_POINT('Ctrl Pts',(-11.2609637080001,15.2,-0.595091312000013));
#265604=CARTESIAN_POINT('Ctrl Pts',(-11.2641111320001,15.2,-0.596667981000016));
#265605=CARTESIAN_POINT('Ctrl Pts',(-11.2672615480001,15.2,-0.598249222000016));
#265606=CARTESIAN_POINT('Ctrl Pts',(-11.2704149460001,15.2,-0.599835041000016));
#265607=CARTESIAN_POINT('Ctrl Pts',(-11.2735713160001,15.2,-0.601425437000014));
#265608=CARTESIAN_POINT('Ctrl Pts',(-11.2767306480001,15.2,-0.603020414000017));
#265609=CARTESIAN_POINT('Ctrl Pts',(-11.2798929340001,15.2,-0.604619973000013));
#265610=CARTESIAN_POINT('Ctrl Pts',(-11.2830581620001,15.2,-0.606224115000016));
#265611=CARTESIAN_POINT('Ctrl Pts',(-11.2862263240001,15.2,-0.607832843000011));
#265612=CARTESIAN_POINT('Ctrl Pts',(-11.2893974100001,15.2,-0.609446160000013));
#265613=CARTESIAN_POINT('Ctrl Pts',(-11.2925714100001,15.2,-0.611064067000013));
#265614=CARTESIAN_POINT('Ctrl Pts',(-11.2957483150001,15.2,-0.612686565000011));
#265615=CARTESIAN_POINT('Ctrl Pts',(-11.2989281170001,15.2,-0.614313657000016));
#265616=CARTESIAN_POINT('Ctrl Pts',(-11.3021108030001,15.2,-0.615945345000015));
#265617=CARTESIAN_POINT('Ctrl Pts',(-11.3052963650001,15.2,-0.617581630000017));
#265618=CARTESIAN_POINT('Ctrl Pts',(-11.3084847960001,15.2,-0.619222515000013));
#265619=CARTESIAN_POINT('Ctrl Pts',(-11.3116760820001,15.2,-0.620868001000012));
#265620=CARTESIAN_POINT('Ctrl Pts',(-11.3148702170001,15.2,-0.622518091000015));
#265621=CARTESIAN_POINT('Ctrl Pts',(-11.3180671910001,15.2,-0.624172784000017));
#265622=CARTESIAN_POINT('Ctrl Pts',(-11.3212669940001,15.2,-0.625832085000013));
#265623=CARTESIAN_POINT('Ctrl Pts',(-11.3244696160001,15.2,-0.627495996000014));
#265624=CARTESIAN_POINT('Ctrl Pts',(-11.3276750490001,15.2,-0.629164515000014));
#265625=CARTESIAN_POINT('Ctrl Pts',(-11.3308832820001,15.2,-0.630837648000018));
#265626=CARTESIAN_POINT('Ctrl Pts',(-11.3340943080001,15.2,-0.632515395000013));
#265627=CARTESIAN_POINT('Ctrl Pts',(-11.3373081150001,15.2,-0.634197758000017));
#265628=CARTESIAN_POINT('Ctrl Pts',(-11.3405246950001,15.2,-0.635884737000012));
#265629=CARTESIAN_POINT('Ctrl Pts',(-11.3437440390001,15.2,-0.637576336000016));
#265630=CARTESIAN_POINT('Ctrl Pts',(-11.3469661360001,15.2,-0.639272557000012));
#265631=CARTESIAN_POINT('Ctrl Pts',(-11.3501909790001,15.2,-0.640973401000018));
#265632=CARTESIAN_POINT('Ctrl Pts',(-11.3534185570001,15.2,-0.642678869000015));
#265633=CARTESIAN_POINT('Ctrl Pts',(-11.3566488620001,15.2,-0.644388964000013));
#265634=CARTESIAN_POINT('Ctrl Pts',(-11.3598818840001,15.2,-0.646103687000017));
#265635=CARTESIAN_POINT('Ctrl Pts',(-11.3631176140001,15.2,-0.647823039000013));
#265636=CARTESIAN_POINT('Ctrl Pts',(-11.3663560430001,15.2,-0.649547023000014));
#265637=CARTESIAN_POINT('Ctrl Pts',(-11.3695971620001,15.2,-0.651275639000013));
#265638=CARTESIAN_POINT('Ctrl Pts',(-11.3728409600001,15.2,-0.653008892000013));
#265639=CARTESIAN_POINT('Ctrl Pts',(-11.3760874300001,15.2,-0.654746780000015));
#265640=CARTESIAN_POINT('Ctrl Pts',(-11.3793365610001,15.2,-0.656489306000014));
#265641=CARTESIAN_POINT('Ctrl Pts',(-11.3825883450001,15.2,-0.658236472000016));
#265642=CARTESIAN_POINT('Ctrl Pts',(-11.3858427730001,15.2,-0.659988280000015));
#265643=CARTESIAN_POINT('Ctrl Pts',(-11.3890998350001,15.2,-0.661744730000016));
#265644=CARTESIAN_POINT('Ctrl Pts',(-11.3923595230001,15.2,-0.663505825000015));
#265645=CARTESIAN_POINT('Ctrl Pts',(-11.3956218280001,15.2,-0.665271566000012));
#265646=CARTESIAN_POINT('Ctrl Pts',(-11.3988867400001,15.2,-0.667041955000016));
#265647=CARTESIAN_POINT('Ctrl Pts',(-11.4021542520001,15.2,-0.668816993000014));
#265648=CARTESIAN_POINT('Ctrl Pts',(-11.4054243520001,15.2,-0.670596683000015));
#265649=CARTESIAN_POINT('Ctrl Pts',(-11.4086970320001,15.2,-0.672381023000015));
#265650=CARTESIAN_POINT('Ctrl Pts',(-11.4119722840001,15.2,-0.674170019000013));
#265651=CARTESIAN_POINT('Ctrl Pts',(-11.4152500960001,15.2,-0.675963670000015));
#265652=CARTESIAN_POINT('Ctrl Pts',(-11.4185304610001,15.2,-0.677761979000016));
#265653=CARTESIAN_POINT('Ctrl Pts',(-11.4218133690001,15.2,-0.679564946000015));
#265654=CARTESIAN_POINT('Ctrl Pts',(-11.4250988120001,15.2,-0.681372573000014));
#265655=CARTESIAN_POINT('Ctrl Pts',(-11.4283867810001,15.2,-0.683184862000012));
#265656=CARTESIAN_POINT('Ctrl Pts',(-11.4316772700001,15.2,-0.685001814000015));
#265657=CARTESIAN_POINT('Ctrl Pts',(-11.4349702680001,15.2,-0.686823430000012));
#265658=CARTESIAN_POINT('Ctrl Pts',(-11.4382657700001,15.2,-0.688649711000018));
#265659=CARTESIAN_POINT('Ctrl Pts',(-11.4415637630001,15.2,-0.690480659000015));
#265660=CARTESIAN_POINT('Ctrl Pts',(-11.4448642400001,15.2,-0.692316276000016));
#265661=CARTESIAN_POINT('Ctrl Pts',(-11.4481671870001,15.2,-0.694156565000017));
#265662=CARTESIAN_POINT('Ctrl Pts',(-11.4514725950001,15.2,-0.696001525000014));
#265663=CARTESIAN_POINT('Ctrl Pts',(-11.4547804530001,15.2,-0.697851159000016));
#265664=CARTESIAN_POINT('Ctrl Pts',(-11.4580907510001,15.2,-0.699705470000014));
#265665=CARTESIAN_POINT('Ctrl Pts',(-11.4614034810001,15.2,-0.701564457000017));
#265666=CARTESIAN_POINT('Ctrl Pts',(-11.4647186380001,15.2,-0.703428121000016));
#265667=CARTESIAN_POINT('Ctrl Pts',(-11.4680362160001,15.2,-0.705296464000016));
#265668=CARTESIAN_POINT('Ctrl Pts',(-11.4713562160001,15.2,-0.707169486000012));
#265669=CARTESIAN_POINT('Ctrl Pts',(-11.4740141490001,15.2,-0.708671646000014));
#265670=CARTESIAN_POINT('Ctrl Pts',(-11.4760086880001,15.2,-0.709800372000018));
#265671=CARTESIAN_POINT('Ctrl Pts',(-11.4773388640001,15.2,-0.710553791000015));
#265672=CARTESIAN_POINT('Ctrl Pts',(-11.4780040730001,15.2,-0.710930734000015));
#265673=CARTESIAN_POINT('Ctrl Pts',(-10.3708900240001,12.2,-0.292001929000012));
#265674=CARTESIAN_POINT('Ctrl Pts',(-10.3710632460001,12.2,-0.292021795000017));
#265675=CARTESIAN_POINT('Ctrl Pts',(-10.3714157310001,12.2,-0.292062310000016));
#265676=CARTESIAN_POINT('Ctrl Pts',(-10.3719498000001,12.2,-0.292123961000015));
#265677=CARTESIAN_POINT('Ctrl Pts',(-10.3726691760001,12.2,-0.292207548000012));
#265678=CARTESIAN_POINT('Ctrl Pts',(-10.3735789750001,12.2,-0.292314181000015));
#265679=CARTESIAN_POINT('Ctrl Pts',(-10.3745034120001,12.2,-0.292423469000016));
#265680=CARTESIAN_POINT('Ctrl Pts',(-10.3754371840001,12.2,-0.292534812000014));
#265681=CARTESIAN_POINT('Ctrl Pts',(-10.3763802670001,12.2,-0.292648223000014));
#265682=CARTESIAN_POINT('Ctrl Pts',(-10.3773326270001,12.2,-0.292763718000018));
#265683=CARTESIAN_POINT('Ctrl Pts',(-10.3782942400001,12.2,-0.292881310000013));
#265684=CARTESIAN_POINT('Ctrl Pts',(-10.3792650740001,12.2,-0.293001015000014));
#265685=CARTESIAN_POINT('Ctrl Pts',(-10.3802451030001,12.2,-0.293122847000014));
#265686=CARTESIAN_POINT('Ctrl Pts',(-10.3812342970001,12.2,-0.293246820000017));
#265687=CARTESIAN_POINT('Ctrl Pts',(-10.3822326280001,12.2,-0.293372950000013));
#265688=CARTESIAN_POINT('Ctrl Pts',(-10.3832400690001,12.2,-0.293501248000014));
#265689=CARTESIAN_POINT('Ctrl Pts',(-10.3842565920001,12.2,-0.293631732000015));
#265690=CARTESIAN_POINT('Ctrl Pts',(-10.3852821680001,12.2,-0.293764413000015));
#265691=CARTESIAN_POINT('Ctrl Pts',(-10.3863167710001,12.2,-0.293899307000016));
#265692=CARTESIAN_POINT('Ctrl Pts',(-10.3873603720001,12.2,-0.294036427000015));
#265693=CARTESIAN_POINT('Ctrl Pts',(-10.3884129450001,12.2,-0.294175788000013));
#265694=CARTESIAN_POINT('Ctrl Pts',(-10.3894744620001,12.2,-0.294317401000015));
#265695=CARTESIAN_POINT('Ctrl Pts',(-10.3905448950001,12.2,-0.294461282000014));
#265696=CARTESIAN_POINT('Ctrl Pts',(-10.3916242180001,12.2,-0.294607444000015));
#265697=CARTESIAN_POINT('Ctrl Pts',(-10.3927124050001,12.2,-0.294755901000014));
#265698=CARTESIAN_POINT('Ctrl Pts',(-10.3938094280001,12.2,-0.294906666000014));
#265699=CARTESIAN_POINT('Ctrl Pts',(-10.3949152600001,12.2,-0.295059752000015));
#265700=CARTESIAN_POINT('Ctrl Pts',(-10.3960298750001,12.2,-0.295215173000014));
#265701=CARTESIAN_POINT('Ctrl Pts',(-10.3971532480001,12.2,-0.295372943000016));
#265702=CARTESIAN_POINT('Ctrl Pts',(-10.3982853500001,12.2,-0.295533072000014));
#265703=CARTESIAN_POINT('Ctrl Pts',(-10.3994261560001,12.2,-0.295695576000017));
#265704=CARTESIAN_POINT('Ctrl Pts',(-10.4005756420001,12.2,-0.295860468000013));
#265705=CARTESIAN_POINT('Ctrl Pts',(-10.4017337790001,12.2,-0.296027759000013));
#265706=CARTESIAN_POINT('Ctrl Pts',(-10.4029005420001,12.2,-0.296197463000016));
#265707=CARTESIAN_POINT('Ctrl Pts',(-10.4040759070001,12.2,-0.296369593000012));
#265708=CARTESIAN_POINT('Ctrl Pts',(-10.4052598460001,12.2,-0.296544162000014));
#265709=CARTESIAN_POINT('Ctrl Pts',(-10.4064523340001,12.2,-0.296721181000015));
#265710=CARTESIAN_POINT('Ctrl Pts',(-10.4076533470001,12.2,-0.296900665000015));
#265711=CARTESIAN_POINT('Ctrl Pts',(-10.4088628590001,12.2,-0.297082624000016));
#265712=CARTESIAN_POINT('Ctrl Pts',(-10.4100808450001,12.2,-0.297267072000014));
#265713=CARTESIAN_POINT('Ctrl Pts',(-10.4113072790001,12.2,-0.297454022000014));
#265714=CARTESIAN_POINT('Ctrl Pts',(-10.4125421370001,12.2,-0.297643484000014));
#265715=CARTESIAN_POINT('Ctrl Pts',(-10.4137853940001,12.2,-0.297835472000014));
#265716=CARTESIAN_POINT('Ctrl Pts',(-10.4150370250001,12.2,-0.298029998000011));
#265717=CARTESIAN_POINT('Ctrl Pts',(-10.4162970050001,12.2,-0.298227073000015));
#265718=CARTESIAN_POINT('Ctrl Pts',(-10.4175653100001,12.2,-0.298426711000013));
#265719=CARTESIAN_POINT('Ctrl Pts',(-10.4188419160001,12.2,-0.298628922000015));
#265720=CARTESIAN_POINT('Ctrl Pts',(-10.4201267970001,12.2,-0.298833719000013));
#265721=CARTESIAN_POINT('Ctrl Pts',(-10.4214199300001,12.2,-0.299041114000014));
#265722=CARTESIAN_POINT('Ctrl Pts',(-10.4227212920001,12.2,-0.299251118000012));
#265723=CARTESIAN_POINT('Ctrl Pts',(-10.4240308570001,12.2,-0.299463743000015));
#265724=CARTESIAN_POINT('Ctrl Pts',(-10.4253486020001,12.2,-0.299679001000013));
#265725=CARTESIAN_POINT('Ctrl Pts',(-10.4266745030001,12.2,-0.299896903000012));
#265726=CARTESIAN_POINT('Ctrl Pts',(-10.4280085350001,12.2,-0.300117461000013));
#265727=CARTESIAN_POINT('Ctrl Pts',(-10.4293506770001,12.2,-0.300340686000014));
#265728=CARTESIAN_POINT('Ctrl Pts',(-10.4307009030001,12.2,-0.300566590000013));
#265729=CARTESIAN_POINT('Ctrl Pts',(-10.4320591910001,12.2,-0.300795184000013));
#265730=CARTESIAN_POINT('Ctrl Pts',(-10.4334255170001,12.2,-0.301026479000015));
#265731=CARTESIAN_POINT('Ctrl Pts',(-10.4347998580001,12.2,-0.301260488000015));
#265732=CARTESIAN_POINT('Ctrl Pts',(-10.4361821910001,12.2,-0.301497219000013));
#265733=CARTESIAN_POINT('Ctrl Pts',(-10.4375724920001,12.2,-0.301736686000016));
#265734=CARTESIAN_POINT('Ctrl Pts',(-10.4389707380001,12.2,-0.301978898000015));
#265735=CARTESIAN_POINT('Ctrl Pts',(-10.4403769080001,12.2,-0.302223867000015));
#265736=CARTESIAN_POINT('Ctrl Pts',(-10.4417909780001,12.2,-0.302471605000014));
#265737=CARTESIAN_POINT('Ctrl Pts',(-10.4432129240001,12.2,-0.302722121000016));
#265738=CARTESIAN_POINT('Ctrl Pts',(-10.4446427250001,12.2,-0.302975426000014));
#265739=CARTESIAN_POINT('Ctrl Pts',(-10.4460803580001,12.2,-0.303231532000012));
#265740=CARTESIAN_POINT('Ctrl Pts',(-10.4475258000001,12.2,-0.303490448000012));
#265741=CARTESIAN_POINT('Ctrl Pts',(-10.4489790300001,12.2,-0.303752186000015));
#265742=CARTESIAN_POINT('Ctrl Pts',(-10.4504400240001,12.2,-0.304016756000016));
#265743=CARTESIAN_POINT('Ctrl Pts',(-10.4519087610001,12.2,-0.304284170000013));
#265744=CARTESIAN_POINT('Ctrl Pts',(-10.4533852190001,12.2,-0.304554436000015));
#265745=CARTESIAN_POINT('Ctrl Pts',(-10.4548693740001,12.2,-0.304827566000014));
#265746=CARTESIAN_POINT('Ctrl Pts',(-10.4563612070001,12.2,-0.305103570000016));
#265747=CARTESIAN_POINT('Ctrl Pts',(-10.4578606950001,12.2,-0.305382458000012));
#265748=CARTESIAN_POINT('Ctrl Pts',(-10.4593678150001,12.2,-0.305664241000017));
#265749=CARTESIAN_POINT('Ctrl Pts',(-10.4608825450001,12.2,-0.305948928000017));
#265750=CARTESIAN_POINT('Ctrl Pts',(-10.4624048670001,12.2,-0.306236531000015));
#265751=CARTESIAN_POINT('Ctrl Pts',(-10.4639347550001,12.2,-0.306527058000015));
#265752=CARTESIAN_POINT('Ctrl Pts',(-10.4654721910001,12.2,-0.306820521000013));
#265753=CARTESIAN_POINT('Ctrl Pts',(-10.4670171510001,12.2,-0.307116929000015));
#265754=CARTESIAN_POINT('Ctrl Pts',(-10.4685696160001,12.2,-0.307416292000013));
#265755=CARTESIAN_POINT('Ctrl Pts',(-10.4701295620001,12.2,-0.307718619000017));
#265756=CARTESIAN_POINT('Ctrl Pts',(-10.4716969700001,12.2,-0.308023923000014));
#265757=CARTESIAN_POINT('Ctrl Pts',(-10.4732718190001,12.2,-0.308332210000017));
#265758=CARTESIAN_POINT('Ctrl Pts',(-10.4748540860001,12.2,-0.308643492000016));
#265759=CARTESIAN_POINT('Ctrl Pts',(-10.4764437530001,12.2,-0.308957777000014));
#265760=CARTESIAN_POINT('Ctrl Pts',(-10.4780407970001,12.2,-0.309275076000013));
#265761=CARTESIAN_POINT('Ctrl Pts',(-10.4796451980001,12.2,-0.309595399000013));
#265762=CARTESIAN_POINT('Ctrl Pts',(-10.4812569350001,12.2,-0.309918754000016));
#265763=CARTESIAN_POINT('Ctrl Pts',(-10.4828759870001,12.2,-0.310245152000017));
#265764=CARTESIAN_POINT('Ctrl Pts',(-10.4845023350001,12.2,-0.310574602000013));
#265765=CARTESIAN_POINT('Ctrl Pts',(-10.4861359570001,12.2,-0.310907114000014));
#265766=CARTESIAN_POINT('Ctrl Pts',(-10.4877768330001,12.2,-0.311242696000011));
#265767=CARTESIAN_POINT('Ctrl Pts',(-10.4894249420001,12.2,-0.311581357000015));
#265768=CARTESIAN_POINT('Ctrl Pts',(-10.4910802660001,12.2,-0.311923107000016));
#265769=CARTESIAN_POINT('Ctrl Pts',(-10.4927427830001,12.2,-0.312267956000016));
#265770=CARTESIAN_POINT('Ctrl Pts',(-10.4944124730001,12.2,-0.312615913000016));
#265771=CARTESIAN_POINT('Ctrl Pts',(-10.4960893160001,12.2,-0.312966987000016));
#265772=CARTESIAN_POINT('Ctrl Pts',(-10.4977732930001,12.2,-0.313321185000017));
#265773=CARTESIAN_POINT('Ctrl Pts',(-10.4994643820001,12.2,-0.313678519000016));
#265774=CARTESIAN_POINT('Ctrl Pts',(-10.5011625650001,12.2,-0.314038997000012));
#265775=CARTESIAN_POINT('Ctrl Pts',(-10.5028678220001,12.2,-0.314402627000017));
#265776=CARTESIAN_POINT('Ctrl Pts',(-10.5049225963254,12.2,-0.314842777384019));
#265777=CARTESIAN_POINT('Ctrl Pts',(-10.5069879188374,12.2,-0.315287684308014));
#265778=CARTESIAN_POINT('Ctrl Pts',(-10.5090637571627,12.2,-0.315737363692019));
#265779=CARTESIAN_POINT('Ctrl Pts',(-10.5111500674852,12.2,-0.316191834574724));
#265780=CARTESIAN_POINT('Ctrl Pts',(-10.5132468120001,12.2,-0.316651113000015));
#265781=CARTESIAN_POINT('Ctrl Pts',(-10.5150010370001,12.2,-0.317037060000014));
#265782=CARTESIAN_POINT('Ctrl Pts',(-10.5167621800001,12.2,-0.317426229000013));
#265783=CARTESIAN_POINT('Ctrl Pts',(-10.5185302210001,12.2,-0.317818628000013));
#265784=CARTESIAN_POINT('Ctrl Pts',(-10.5203051430001,12.2,-0.318214269000014));
#265785=CARTESIAN_POINT('Ctrl Pts',(-10.5220869250001,12.2,-0.318613157000014));
#265786=CARTESIAN_POINT('Ctrl Pts',(-10.5238755480001,12.2,-0.319015302000012));
#265787=CARTESIAN_POINT('Ctrl Pts',(-10.5256709940001,12.2,-0.319420713000014));
#265788=CARTESIAN_POINT('Ctrl Pts',(-10.5274732440001,12.2,-0.319829396000015));
#265789=CARTESIAN_POINT('Ctrl Pts',(-10.5292822790001,12.2,-0.320241361000013));
#265790=CARTESIAN_POINT('Ctrl Pts',(-10.5310980810001,12.2,-0.320656616000012));
#265791=CARTESIAN_POINT('Ctrl Pts',(-10.5329206290001,12.2,-0.321075169000018));
#265792=CARTESIAN_POINT('Ctrl Pts',(-10.5347499080001,12.2,-0.321497029000017));
#265793=CARTESIAN_POINT('Ctrl Pts',(-10.5365858960001,12.2,-0.321922203000016));
#265794=CARTESIAN_POINT('Ctrl Pts',(-10.5384285770001,12.2,-0.322350700000014));
#265795=CARTESIAN_POINT('Ctrl Pts',(-10.5402779310001,12.2,-0.322782527000012));
#265796=CARTESIAN_POINT('Ctrl Pts',(-10.5421339400001,12.2,-0.323217694000015));
#265797=CARTESIAN_POINT('Ctrl Pts',(-10.5439965860001,12.2,-0.323656207000016));
#265798=CARTESIAN_POINT('Ctrl Pts',(-10.5458658520001,12.2,-0.324098074000014));
#265799=CARTESIAN_POINT('Ctrl Pts',(-10.5477417170001,12.2,-0.324543305000016));
#265800=CARTESIAN_POINT('Ctrl Pts',(-10.5496241650001,12.2,-0.324991905000012));
#265801=CARTESIAN_POINT('Ctrl Pts',(-10.5515131770001,12.2,-0.325443883000016));
#265802=CARTESIAN_POINT('Ctrl Pts',(-10.5534087350001,12.2,-0.325899248000017));
#265803=CARTESIAN_POINT('Ctrl Pts',(-10.5553108210001,12.2,-0.326358007000014));
#265804=CARTESIAN_POINT('Ctrl Pts',(-10.5572194180001,12.2,-0.326820167000013));
#265805=CARTESIAN_POINT('Ctrl Pts',(-10.5591345070001,12.2,-0.327285736000014));
#265806=CARTESIAN_POINT('Ctrl Pts',(-10.5610560710001,12.2,-0.327754722000013));
#265807=CARTESIAN_POINT('Ctrl Pts',(-10.5629840910001,12.2,-0.328227133000016));
#265808=CARTESIAN_POINT('Ctrl Pts',(-10.5649185510001,12.2,-0.328702975000015));
#265809=CARTESIAN_POINT('Ctrl Pts',(-10.5668594320001,12.2,-0.329182256000013));
#265810=CARTESIAN_POINT('Ctrl Pts',(-10.5688067180001,12.2,-0.329664985000013));
#265811=CARTESIAN_POINT('Ctrl Pts',(-10.5707603900001,12.2,-0.330151169000015));
#265812=CARTESIAN_POINT('Ctrl Pts',(-10.5727204310001,12.2,-0.330640814000014));
#265813=CARTESIAN_POINT('Ctrl Pts',(-10.5746868240001,12.2,-0.331133928000016));
#265814=CARTESIAN_POINT('Ctrl Pts',(-10.5766595510001,12.2,-0.331630519000012));
#265815=CARTESIAN_POINT('Ctrl Pts',(-10.5786385950001,12.2,-0.332130595000013));
#265816=CARTESIAN_POINT('Ctrl Pts',(-10.5806239380001,12.2,-0.332634161000014));
#265817=CARTESIAN_POINT('Ctrl Pts',(-10.5826155640001,12.2,-0.333141226000016));
#265818=CARTESIAN_POINT('Ctrl Pts',(-10.5846134550001,12.2,-0.333651796000014));
#265819=CARTESIAN_POINT('Ctrl Pts',(-10.5866175950001,12.2,-0.334165879000015));
#265820=CARTESIAN_POINT('Ctrl Pts',(-10.5886279650001,12.2,-0.334683483000013));
#265821=CARTESIAN_POINT('Ctrl Pts',(-10.5906445490001,12.2,-0.335204613000015));
#265822=CARTESIAN_POINT('Ctrl Pts',(-10.5926673320001,12.2,-0.335729278000017));
#265823=CARTESIAN_POINT('Ctrl Pts',(-10.5946962940001,12.2,-0.336257483000013));
#265824=CARTESIAN_POINT('Ctrl Pts',(-10.5967314190001,12.2,-0.336789237000015));
#265825=CARTESIAN_POINT('Ctrl Pts',(-10.5987726910001,12.2,-0.337324546000013));
#265826=CARTESIAN_POINT('Ctrl Pts',(-10.6008200940001,12.2,-0.337863418000013));
#265827=CARTESIAN_POINT('Ctrl Pts',(-10.6028736090001,12.2,-0.338405859000015));
#265828=CARTESIAN_POINT('Ctrl Pts',(-10.6049332210001,12.2,-0.338951874000015));
#265829=CARTESIAN_POINT('Ctrl Pts',(-10.6069989120001,12.2,-0.339501473000015));
#265830=CARTESIAN_POINT('Ctrl Pts',(-10.6090706680001,12.2,-0.340054662000018));
#265831=CARTESIAN_POINT('Ctrl Pts',(-10.6111484700001,12.2,-0.340611447000012));
#265832=CARTESIAN_POINT('Ctrl Pts',(-10.6132323020001,12.2,-0.341171835000011));
#265833=CARTESIAN_POINT('Ctrl Pts',(-10.6153221490001,12.2,-0.341735833000012));
#265834=CARTESIAN_POINT('Ctrl Pts',(-10.6174179920001,12.2,-0.342303448000014));
#265835=CARTESIAN_POINT('Ctrl Pts',(-10.6195198180001,12.2,-0.342874685000014));
#265836=CARTESIAN_POINT('Ctrl Pts',(-10.6216276080001,12.2,-0.343449552000017));
#265837=CARTESIAN_POINT('Ctrl Pts',(-10.6237413470001,12.2,-0.344028056000014));
#265838=CARTESIAN_POINT('Ctrl Pts',(-10.6258610180001,12.2,-0.344610202000015));
#265839=CARTESIAN_POINT('Ctrl Pts',(-10.6279866070001,12.2,-0.345195998000012));
#265840=CARTESIAN_POINT('Ctrl Pts',(-10.6301180950001,12.2,-0.345785450000013));
#265841=CARTESIAN_POINT('Ctrl Pts',(-10.6322554680001,12.2,-0.346378564000016));
#265842=CARTESIAN_POINT('Ctrl Pts',(-10.6343987090001,12.2,-0.346975347000011));
#265843=CARTESIAN_POINT('Ctrl Pts',(-10.6365478020001,12.2,-0.347575805000013));
#265844=CARTESIAN_POINT('Ctrl Pts',(-10.6387027320001,12.2,-0.348179945000013));
#265845=CARTESIAN_POINT('Ctrl Pts',(-10.6408634830001,12.2,-0.348787773000012));
#265846=CARTESIAN_POINT('Ctrl Pts',(-10.6430300390001,12.2,-0.349399295000015));
#265847=CARTESIAN_POINT('Ctrl Pts',(-10.6452023830001,12.2,-0.350014516000012));
#265848=CARTESIAN_POINT('Ctrl Pts',(-10.6473805010001,12.2,-0.350633446000015));
#265849=CARTESIAN_POINT('Ctrl Pts',(-10.6495643770001,12.2,-0.351256088000014));
#265850=CARTESIAN_POINT('Ctrl Pts',(-10.6517539940001,12.2,-0.351882449000014));
#265851=CARTESIAN_POINT('Ctrl Pts',(-10.6539493380001,12.2,-0.352512536000016));
#265852=CARTESIAN_POINT('Ctrl Pts',(-10.6561503920001,12.2,-0.353146354000016));
#265853=CARTESIAN_POINT('Ctrl Pts',(-10.6583571410001,12.2,-0.353783910000014));
#265854=CARTESIAN_POINT('Ctrl Pts',(-10.6605695710001,12.2,-0.354425210000016));
#265855=CARTESIAN_POINT('Ctrl Pts',(-10.6627876650001,12.2,-0.355070259000012));
#265856=CARTESIAN_POINT('Ctrl Pts',(-10.6650114070001,12.2,-0.355719063000013));
#265857=CARTESIAN_POINT('Ctrl Pts',(-10.6672407830001,12.2,-0.356371629000014));
#265858=CARTESIAN_POINT('Ctrl Pts',(-10.6694757780001,12.2,-0.357027964000016));
#265859=CARTESIAN_POINT('Ctrl Pts',(-10.6717163760001,12.2,-0.357688071000015));
#265860=CARTESIAN_POINT('Ctrl Pts',(-10.6739625620001,12.2,-0.358351959000016));
#265861=CARTESIAN_POINT('Ctrl Pts',(-10.6762143200001,12.2,-0.359019631000015));
#265862=CARTESIAN_POINT('Ctrl Pts',(-10.6784716350001,12.2,-0.359691096000017));
#265863=CARTESIAN_POINT('Ctrl Pts',(-10.6807344940001,12.2,-0.360366356000017));
#265864=CARTESIAN_POINT('Ctrl Pts',(-10.6830028780001,12.2,-0.361045420000017));
#265865=CARTESIAN_POINT('Ctrl Pts',(-10.6852767760001,12.2,-0.361728293000017));
#265866=CARTESIAN_POINT('Ctrl Pts',(-10.6875561710001,12.2,-0.362414981000012));
#265867=CARTESIAN_POINT('Ctrl Pts',(-10.6898410480001,12.2,-0.363105487000013));
#265868=CARTESIAN_POINT('Ctrl Pts',(-10.6921313930001,12.2,-0.363799821000015));
#265869=CARTESIAN_POINT('Ctrl Pts',(-10.6944271900001,12.2,-0.364497985000014));
#265870=CARTESIAN_POINT('Ctrl Pts',(-10.6967284250001,12.2,-0.365199987000011));
#265871=CARTESIAN_POINT('Ctrl Pts',(-10.6990350820001,12.2,-0.365905831000015));
#265872=CARTESIAN_POINT('Ctrl Pts',(-10.7018095613513,12.2,-0.366757461446432));
#265873=CARTESIAN_POINT('Ctrl Pts',(-10.7045921314508,12.2,-0.367614872815749));
#265874=CARTESIAN_POINT('Ctrl Pts',(-10.7073827605493,12.2,-0.368478077184284));
#265875=CARTESIAN_POINT('Ctrl Pts',(-10.7101814229016,12.2,-0.369347083631473));
#265876=CARTESIAN_POINT('Ctrl Pts',(-10.7129880860001,12.2,-0.370221904000014));
#265877=CARTESIAN_POINT('Ctrl Pts',(-10.7153322940001,12.2,-0.370954801000014));
#265878=CARTESIAN_POINT('Ctrl Pts',(-10.7176818070001,12.2,-0.371691587000011));
#265879=CARTESIAN_POINT('Ctrl Pts',(-10.7200366120001,12.2,-0.372432264000011));
#265880=CARTESIAN_POINT('Ctrl Pts',(-10.7223966940001,12.2,-0.373176838000013));
#265881=CARTESIAN_POINT('Ctrl Pts',(-10.7247620380001,12.2,-0.373925315000014));
#265882=CARTESIAN_POINT('Ctrl Pts',(-10.7271326310001,12.2,-0.374677700000015));
#265883=CARTESIAN_POINT('Ctrl Pts',(-10.7295084580001,12.2,-0.375433998000014));
#265884=CARTESIAN_POINT('Ctrl Pts',(-10.7318895040001,12.2,-0.376194215000014));
#265885=CARTESIAN_POINT('Ctrl Pts',(-10.7342757570001,12.2,-0.376958356000014));
#265886=CARTESIAN_POINT('Ctrl Pts',(-10.7366672000001,12.2,-0.377726425000016));
#265887=CARTESIAN_POINT('Ctrl Pts',(-10.7390638200001,12.2,-0.378498429000014));
#265888=CARTESIAN_POINT('Ctrl Pts',(-10.7414656040001,12.2,-0.379274372000014));
#265889=CARTESIAN_POINT('Ctrl Pts',(-10.7438725370001,12.2,-0.380054260000016));
#265890=CARTESIAN_POINT('Ctrl Pts',(-10.7462846040001,12.2,-0.380838098000016));
#265891=CARTESIAN_POINT('Ctrl Pts',(-10.7487017930001,12.2,-0.381625889000015));
#265892=CARTESIAN_POINT('Ctrl Pts',(-10.7511240870001,12.2,-0.382417641000017));
#265893=CARTESIAN_POINT('Ctrl Pts',(-10.7535514750001,12.2,-0.383213358000014));
#265894=CARTESIAN_POINT('Ctrl Pts',(-10.7559839420001,12.2,-0.384013044000016));
#265895=CARTESIAN_POINT('Ctrl Pts',(-10.7584214740001,12.2,-0.384816705000013));
#265896=CARTESIAN_POINT('Ctrl Pts',(-10.7608640580001,12.2,-0.385624345000015));
#265897=CARTESIAN_POINT('Ctrl Pts',(-10.7633116780001,12.2,-0.386435971000014));
#265898=CARTESIAN_POINT('Ctrl Pts',(-10.7657643230001,12.2,-0.387251586000015));
#265899=CARTESIAN_POINT('Ctrl Pts',(-10.7682219760001,12.2,-0.388071196000013));
#265900=CARTESIAN_POINT('Ctrl Pts',(-10.7706846260001,12.2,-0.388894805000017));
#265901=CARTESIAN_POINT('Ctrl Pts',(-10.7731522590001,12.2,-0.389722418000016));
#265902=CARTESIAN_POINT('Ctrl Pts',(-10.7756248610001,12.2,-0.390554041000013));
#265903=CARTESIAN_POINT('Ctrl Pts',(-10.7781024170001,12.2,-0.391389677000014));
#265904=CARTESIAN_POINT('Ctrl Pts',(-10.7805849160001,12.2,-0.392229332000014));
#265905=CARTESIAN_POINT('Ctrl Pts',(-10.7830723410001,12.2,-0.393073009000013));
#265906=CARTESIAN_POINT('Ctrl Pts',(-10.7855646820001,12.2,-0.393920716000018));
#265907=CARTESIAN_POINT('Ctrl Pts',(-10.7880619230001,12.2,-0.394772456000014));
#265908=CARTESIAN_POINT('Ctrl Pts',(-10.7905640520001,12.2,-0.395628232000016));
#265909=CARTESIAN_POINT('Ctrl Pts',(-10.7930710550001,12.2,-0.396488052000015));
#265910=CARTESIAN_POINT('Ctrl Pts',(-10.7955829180001,12.2,-0.397351917000015));
#265911=CARTESIAN_POINT('Ctrl Pts',(-10.7980996290001,12.2,-0.398219835000013));
#265912=CARTESIAN_POINT('Ctrl Pts',(-10.8006211740001,12.2,-0.399091809000014));
#265913=CARTESIAN_POINT('Ctrl Pts',(-10.8031475400001,12.2,-0.399967843000013));
#265914=CARTESIAN_POINT('Ctrl Pts',(-10.8056787130001,12.2,-0.400847944000016));
#265915=CARTESIAN_POINT('Ctrl Pts',(-10.8082146790001,12.2,-0.401732113000013));
#265916=CARTESIAN_POINT('Ctrl Pts',(-10.8107554270001,12.2,-0.402620357000014));
#265917=CARTESIAN_POINT('Ctrl Pts',(-10.8133009430001,12.2,-0.403512679000015));
#265918=CARTESIAN_POINT('Ctrl Pts',(-10.8158512130001,12.2,-0.404409086000013));
#265919=CARTESIAN_POINT('Ctrl Pts',(-10.8184062250001,12.2,-0.405309580000015));
#265920=CARTESIAN_POINT('Ctrl Pts',(-10.8209659650001,12.2,-0.406214166000014));
#265921=CARTESIAN_POINT('Ctrl Pts',(-10.8235304190001,12.2,-0.407122849000014));
#265922=CARTESIAN_POINT('Ctrl Pts',(-10.8260995770001,12.2,-0.408035633000012));
#265923=CARTESIAN_POINT('Ctrl Pts',(-10.8286734240001,12.2,-0.408952523000017));
#265924=CARTESIAN_POINT('Ctrl Pts',(-10.8312519470001,12.2,-0.409873522000015));
#265925=CARTESIAN_POINT('Ctrl Pts',(-10.8338351330001,12.2,-0.410798635000016));
#265926=CARTESIAN_POINT('Ctrl Pts',(-10.8364229690001,12.2,-0.411727867000016));
#265927=CARTESIAN_POINT('Ctrl Pts',(-10.8390154430001,12.2,-0.412661222000015));
#265928=CARTESIAN_POINT('Ctrl Pts',(-10.8416125420001,12.2,-0.413598703000013));
#265929=CARTESIAN_POINT('Ctrl Pts',(-10.8442142530001,12.2,-0.414540317000016));
#265930=CARTESIAN_POINT('Ctrl Pts',(-10.8468205630001,12.2,-0.415486065000015));
#265931=CARTESIAN_POINT('Ctrl Pts',(-10.8494314580001,12.2,-0.416435953000014));
#265932=CARTESIAN_POINT('Ctrl Pts',(-10.8520469280001,12.2,-0.417389985000014));
#265933=CARTESIAN_POINT('Ctrl Pts',(-10.8546669570001,12.2,-0.418348165000015));
#265934=CARTESIAN_POINT('Ctrl Pts',(-10.8572915350001,12.2,-0.419310498000014));
#265935=CARTESIAN_POINT('Ctrl Pts',(-10.8599206490001,12.2,-0.420276987000014));
#265936=CARTESIAN_POINT('Ctrl Pts',(-10.8625542860001,12.2,-0.421247636000013));
#265937=CARTESIAN_POINT('Ctrl Pts',(-10.8651924320001,12.2,-0.422222450000014));
#265938=CARTESIAN_POINT('Ctrl Pts',(-10.8678350770001,12.2,-0.423201432000013));
#265939=CARTESIAN_POINT('Ctrl Pts',(-10.8704822050001,12.2,-0.424184588000016));
#265940=CARTESIAN_POINT('Ctrl Pts',(-10.8731338070001,12.2,-0.425171920000014));
#265941=CARTESIAN_POINT('Ctrl Pts',(-10.8757898690001,12.2,-0.426163433000015));
#265942=CARTESIAN_POINT('Ctrl Pts',(-10.8784503780001,12.2,-0.427159131000017));
#265943=CARTESIAN_POINT('Ctrl Pts',(-10.8811153220001,12.2,-0.428159018000014));
#265944=CARTESIAN_POINT('Ctrl Pts',(-10.8837846900001,12.2,-0.429163097000016));
#265945=CARTESIAN_POINT('Ctrl Pts',(-10.8864584680001,12.2,-0.430171373000015));
#265946=CARTESIAN_POINT('Ctrl Pts',(-10.8891366430001,12.2,-0.431183850000014));
#265947=CARTESIAN_POINT('Ctrl Pts',(-10.8918192040001,12.2,-0.432200531000015));
#265948=CARTESIAN_POINT('Ctrl Pts',(-10.8945061380001,12.2,-0.433221421000014));
#265949=CARTESIAN_POINT('Ctrl Pts',(-10.8971974330001,12.2,-0.434246522000015));
#265950=CARTESIAN_POINT('Ctrl Pts',(-10.8998930780001,12.2,-0.435275840000013));
#265951=CARTESIAN_POINT('Ctrl Pts',(-10.9025930590001,12.2,-0.436309378000015));
#265952=CARTESIAN_POINT('Ctrl Pts',(-10.9052973640001,12.2,-0.437347141000015));
#265953=CARTESIAN_POINT('Ctrl Pts',(-10.9080059810001,12.2,-0.438389130000014));
#265954=CARTESIAN_POINT('Ctrl Pts',(-10.9107188990001,12.2,-0.439435350000017));
#265955=CARTESIAN_POINT('Ctrl Pts',(-10.9134361040001,12.2,-0.440485807000015));
#265956=CARTESIAN_POINT('Ctrl Pts',(-10.9161575860001,12.2,-0.441540501000013));
#265957=CARTESIAN_POINT('Ctrl Pts',(-10.9188833300001,12.2,-0.442599438000015));
#265958=CARTESIAN_POINT('Ctrl Pts',(-10.9216133270001,12.2,-0.443662622000014));
#265959=CARTESIAN_POINT('Ctrl Pts',(-10.9243475630001,12.2,-0.444730056000013));
#265960=CARTESIAN_POINT('Ctrl Pts',(-10.9270860270001,12.2,-0.445801743000014));
#265961=CARTESIAN_POINT('Ctrl Pts',(-10.9298287070001,12.2,-0.446877689000011));
#265962=CARTESIAN_POINT('Ctrl Pts',(-10.9325755900001,12.2,-0.447957894000015));
#265963=CARTESIAN_POINT('Ctrl Pts',(-10.9353266640001,12.2,-0.449042364000016));
#265964=CARTESIAN_POINT('Ctrl Pts',(-10.9380819200001,12.2,-0.450131103000011));
#265965=CARTESIAN_POINT('Ctrl Pts',(-10.9408413420001,12.2,-0.451224112000013));
#265966=CARTESIAN_POINT('Ctrl Pts',(-10.9436049220001,12.2,-0.452321397000013));
#265967=CARTESIAN_POINT('Ctrl Pts',(-10.9463726460001,12.2,-0.453422962000012));
#265968=CARTESIAN_POINT('Ctrl Pts',(-10.9491445020001,12.2,-0.454528810000014));
#265969=CARTESIAN_POINT('Ctrl Pts',(-10.9519204780001,12.2,-0.455638942000016));
#265970=CARTESIAN_POINT('Ctrl Pts',(-10.9547005640001,12.2,-0.456753364000013));
#265971=CARTESIAN_POINT('Ctrl Pts',(-10.9574847480001,12.2,-0.457872080000015));
#265972=CARTESIAN_POINT('Ctrl Pts',(-10.9602730170001,12.2,-0.458995091000016));
#265973=CARTESIAN_POINT('Ctrl Pts',(-10.9630653590001,12.2,-0.460122402000014));
#265974=CARTESIAN_POINT('Ctrl Pts',(-10.9658617640001,12.2,-0.461254017000012));
#265975=CARTESIAN_POINT('Ctrl Pts',(-10.9686622200001,12.2,-0.462389938000012));
#265976=CARTESIAN_POINT('Ctrl Pts',(-10.9714667150001,12.2,-0.463530170000013));
#265977=CARTESIAN_POINT('Ctrl Pts',(-10.9742752370001,12.2,-0.464674714000015));
#265978=CARTESIAN_POINT('Ctrl Pts',(-10.9770877740001,12.2,-0.465823575000015));
#265979=CARTESIAN_POINT('Ctrl Pts',(-10.9799043170001,12.2,-0.466976757000013));
#265980=CARTESIAN_POINT('Ctrl Pts',(-10.9827248520001,12.2,-0.468134263000017));
#265981=CARTESIAN_POINT('Ctrl Pts',(-10.9855493680001,12.2,-0.469296094000011));
#265982=CARTESIAN_POINT('Ctrl Pts',(-10.9883778540001,12.2,-0.470462257000013));
#265983=CARTESIAN_POINT('Ctrl Pts',(-10.9912102990001,12.2,-0.471632753000013));
#265984=CARTESIAN_POINT('Ctrl Pts',(-10.9940466900001,12.2,-0.472807585000012));
#265985=CARTESIAN_POINT('Ctrl Pts',(-10.9968870170001,12.2,-0.473986757000016));
#265986=CARTESIAN_POINT('Ctrl Pts',(-10.9997312680001,12.2,-0.475170273000014));
#265987=CARTESIAN_POINT('Ctrl Pts',(-11.0025794320001,12.2,-0.476358134000012));
#265988=CARTESIAN_POINT('Ctrl Pts',(-11.0054314970001,12.2,-0.477550346000015));
#265989=CARTESIAN_POINT('Ctrl Pts',(-11.0082874530001,12.2,-0.478746910000014));
#265990=CARTESIAN_POINT('Ctrl Pts',(-11.0111472870001,12.2,-0.479947831000014));
#265991=CARTESIAN_POINT('Ctrl Pts',(-11.0140109890001,12.2,-0.481153110000014));
#265992=CARTESIAN_POINT('Ctrl Pts',(-11.0168785470001,12.2,-0.482362752000016));
#265993=CARTESIAN_POINT('Ctrl Pts',(-11.0197499510001,12.2,-0.483576758000015));
#265994=CARTESIAN_POINT('Ctrl Pts',(-11.0226251880001,12.2,-0.484795134000016));
#265995=CARTESIAN_POINT('Ctrl Pts',(-11.0255042470001,12.2,-0.486017881000014));
#265996=CARTESIAN_POINT('Ctrl Pts',(-11.0283871190001,12.2,-0.487245003000014));
#265997=CARTESIAN_POINT('Ctrl Pts',(-11.0312737910001,12.2,-0.488476502000013));
#265998=CARTESIAN_POINT('Ctrl Pts',(-11.0341642530001,12.2,-0.489712383000014));
#265999=CARTESIAN_POINT('Ctrl Pts',(-11.0370584920001,12.2,-0.490952646000018));
#266000=CARTESIAN_POINT('Ctrl Pts',(-11.0399564980001,12.2,-0.492197297000012));
#266001=CARTESIAN_POINT('Ctrl Pts',(-11.0428582610001,12.2,-0.493446338000014));
#266002=CARTESIAN_POINT('Ctrl Pts',(-11.0457637680001,12.2,-0.494699772000011));
#266003=CARTESIAN_POINT('Ctrl Pts',(-11.0486730100001,12.2,-0.495957601000012));
#266004=CARTESIAN_POINT('Ctrl Pts',(-11.0515859750001,12.2,-0.497219830000013));
#266005=CARTESIAN_POINT('Ctrl Pts',(-11.0545026510001,12.2,-0.498486460000014));
#266006=CARTESIAN_POINT('Ctrl Pts',(-11.0574230290001,12.2,-0.499757494000015));
#266007=CARTESIAN_POINT('Ctrl Pts',(-11.0603470970001,12.2,-0.501032937000012));
#266008=CARTESIAN_POINT('Ctrl Pts',(-11.0632748440001,12.2,-0.502312789000015));
#266009=CARTESIAN_POINT('Ctrl Pts',(-11.0662062590001,12.2,-0.503597056000018));
#266010=CARTESIAN_POINT('Ctrl Pts',(-11.0691413320001,12.2,-0.504885738000014));
#266011=CARTESIAN_POINT('Ctrl Pts',(-11.0720800520001,12.2,-0.506178839000011));
#266012=CARTESIAN_POINT('Ctrl Pts',(-11.0750224080001,12.2,-0.507476362000014));
#266013=CARTESIAN_POINT('Ctrl Pts',(-11.0779683880001,12.2,-0.508778311000011));
#266014=CARTESIAN_POINT('Ctrl Pts',(-11.0809179820001,12.2,-0.510084687000014));
#266015=CARTESIAN_POINT('Ctrl Pts',(-11.0838711810001,12.2,-0.511395492000015));
#266016=CARTESIAN_POINT('Ctrl Pts',(-11.0868279720001,12.2,-0.512710732000015));
#266017=CARTESIAN_POINT('Ctrl Pts',(-11.0897883450001,12.2,-0.514030406000017));
#266018=CARTESIAN_POINT('Ctrl Pts',(-11.0927522890001,12.2,-0.515354521000013));
#266019=CARTESIAN_POINT('Ctrl Pts',(-11.0957197940001,12.2,-0.516683076000017));
#266020=CARTESIAN_POINT('Ctrl Pts',(-11.0986908480001,12.2,-0.518016075000016));
#266021=CARTESIAN_POINT('Ctrl Pts',(-11.1016654420001,12.2,-0.519353522000015));
#266022=CARTESIAN_POINT('Ctrl Pts',(-11.1046435640001,12.2,-0.520695418000017));
#266023=CARTESIAN_POINT('Ctrl Pts',(-11.1076252050001,12.2,-0.522041766000014));
#266024=CARTESIAN_POINT('Ctrl Pts',(-11.1106103520001,12.2,-0.523392569000016));
#266025=CARTESIAN_POINT('Ctrl Pts',(-11.1135989970001,12.2,-0.524747830000014));
#266026=CARTESIAN_POINT('Ctrl Pts',(-11.1165911290001,12.2,-0.526107550000017));
#266027=CARTESIAN_POINT('Ctrl Pts',(-11.1195867360001,12.2,-0.527471735000016));
#266028=CARTESIAN_POINT('Ctrl Pts',(-11.1225858080001,12.2,-0.528840384000016));
#266029=CARTESIAN_POINT('Ctrl Pts',(-11.1255883350001,12.2,-0.530213501000016));
#266030=CARTESIAN_POINT('Ctrl Pts',(-11.1285943060001,12.2,-0.531591090000014));
#266031=CARTESIAN_POINT('Ctrl Pts',(-11.1316037120001,12.2,-0.532973151000018));
#266032=CARTESIAN_POINT('Ctrl Pts',(-11.1346165400001,12.2,-0.534359689000015));
#266033=CARTESIAN_POINT('Ctrl Pts',(-11.1376327810001,12.2,-0.535750705000013));
#266034=CARTESIAN_POINT('Ctrl Pts',(-11.1406524250001,12.2,-0.537146200000014));
#266035=CARTESIAN_POINT('Ctrl Pts',(-11.1436754620001,12.2,-0.538546181000013));
#266036=CARTESIAN_POINT('Ctrl Pts',(-11.1467018790001,12.2,-0.539950647000014));
#266037=CARTESIAN_POINT('Ctrl Pts',(-11.1497316690001,12.2,-0.541359602000018));
#266038=CARTESIAN_POINT('Ctrl Pts',(-11.1527648200001,12.2,-0.542773047000011));
#266039=CARTESIAN_POINT('Ctrl Pts',(-11.1558013220001,12.2,-0.544190986000017));
#266040=CARTESIAN_POINT('Ctrl Pts',(-11.1588411640001,12.2,-0.545613421000013));
#266041=CARTESIAN_POINT('Ctrl Pts',(-11.1618843360001,12.2,-0.547040354000017));
#266042=CARTESIAN_POINT('Ctrl Pts',(-11.1649308290001,12.2,-0.548471788000011));
#266043=CARTESIAN_POINT('Ctrl Pts',(-11.1679806310001,12.2,-0.549907725000014));
#266044=CARTESIAN_POINT('Ctrl Pts',(-11.1710337330001,12.2,-0.551348168000012));
#266045=CARTESIAN_POINT('Ctrl Pts',(-11.1740901240001,12.2,-0.552793118000015));
#266046=CARTESIAN_POINT('Ctrl Pts',(-11.1771497950001,12.2,-0.554242580000013));
#266047=CARTESIAN_POINT('Ctrl Pts',(-11.1802127340001,12.2,-0.555696554000011));
#266048=CARTESIAN_POINT('Ctrl Pts',(-11.1832789320001,12.2,-0.557155042000015));
#266049=CARTESIAN_POINT('Ctrl Pts',(-11.1863483800001,12.2,-0.558618049000015));
#266050=CARTESIAN_POINT('Ctrl Pts',(-11.1894210660001,12.2,-0.560085575000016));
#266051=CARTESIAN_POINT('Ctrl Pts',(-11.1924969800001,12.2,-0.561557623000013));
#266052=CARTESIAN_POINT('Ctrl Pts',(-11.1955761130001,12.2,-0.563034196000016));
#266053=CARTESIAN_POINT('Ctrl Pts',(-11.1986584540001,12.2,-0.564515295000017));
#266054=CARTESIAN_POINT('Ctrl Pts',(-11.2017439940001,12.2,-0.566000924000014));
#266055=CARTESIAN_POINT('Ctrl Pts',(-11.2048327210001,12.2,-0.567491084000018));
#266056=CARTESIAN_POINT('Ctrl Pts',(-11.2079246280001,12.2,-0.568985776000015));
#266057=CARTESIAN_POINT('Ctrl Pts',(-11.2110197020001,12.2,-0.570485006000014));
#266058=CARTESIAN_POINT('Ctrl Pts',(-11.2141179350001,12.2,-0.571988772000012));
#266059=CARTESIAN_POINT('Ctrl Pts',(-11.2172193170001,12.2,-0.573497079000016));
#266060=CARTESIAN_POINT('Ctrl Pts',(-11.2203238380001,12.2,-0.575009928000014));
#266061=CARTESIAN_POINT('Ctrl Pts',(-11.2234314850001,12.2,-0.576527323000011));
#266062=CARTESIAN_POINT('Ctrl Pts',(-11.2265422530001,12.2,-0.578049263000011));
#266063=CARTESIAN_POINT('Ctrl Pts',(-11.2296561290001,12.2,-0.579575753000015));
#266064=CARTESIAN_POINT('Ctrl Pts',(-11.2327731030001,12.2,-0.581106794000017));
#266065=CARTESIAN_POINT('Ctrl Pts',(-11.2358931670001,12.2,-0.582642387000014));
#266066=CARTESIAN_POINT('Ctrl Pts',(-11.2390163100001,12.2,-0.584182538000011));
#266067=CARTESIAN_POINT('Ctrl Pts',(-11.2421425230001,12.2,-0.585727245000012));
#266068=CARTESIAN_POINT('Ctrl Pts',(-11.2452717950001,12.2,-0.587276511000017));
#266069=CARTESIAN_POINT('Ctrl Pts',(-11.2484041180001,12.2,-0.588830340000013));
#266070=CARTESIAN_POINT('Ctrl Pts',(-11.2515394790001,12.2,-0.590388732000013));
#266071=CARTESIAN_POINT('Ctrl Pts',(-11.2546778710001,12.2,-0.591951690000014));
#266072=CARTESIAN_POINT('Ctrl Pts',(-11.2578192840001,12.2,-0.593519216000011));
#266073=CARTESIAN_POINT('Ctrl Pts',(-11.2609637080001,12.2,-0.595091312000013));
#266074=CARTESIAN_POINT('Ctrl Pts',(-11.2641111320001,12.2,-0.596667981000016));
#266075=CARTESIAN_POINT('Ctrl Pts',(-11.2672615480001,12.2,-0.598249222000016));
#266076=CARTESIAN_POINT('Ctrl Pts',(-11.2704149460001,12.2,-0.599835041000016));
#266077=CARTESIAN_POINT('Ctrl Pts',(-11.2735713160001,12.2,-0.601425437000014));
#266078=CARTESIAN_POINT('Ctrl Pts',(-11.2767306480001,12.2,-0.603020414000017));
#266079=CARTESIAN_POINT('Ctrl Pts',(-11.2798929340001,12.2,-0.604619973000013));
#266080=CARTESIAN_POINT('Ctrl Pts',(-11.2830581620001,12.2,-0.606224115000016));
#266081=CARTESIAN_POINT('Ctrl Pts',(-11.2862263240001,12.2,-0.607832843000011));
#266082=CARTESIAN_POINT('Ctrl Pts',(-11.2893974100001,12.2,-0.609446160000013));
#266083=CARTESIAN_POINT('Ctrl Pts',(-11.2925714100001,12.2,-0.611064067000013));
#266084=CARTESIAN_POINT('Ctrl Pts',(-11.2957483150001,12.2,-0.612686565000011));
#266085=CARTESIAN_POINT('Ctrl Pts',(-11.2989281170001,12.2,-0.614313657000016));
#266086=CARTESIAN_POINT('Ctrl Pts',(-11.3021108030001,12.2,-0.615945345000015));
#266087=CARTESIAN_POINT('Ctrl Pts',(-11.3052963650001,12.2,-0.617581630000017));
#266088=CARTESIAN_POINT('Ctrl Pts',(-11.3084847960001,12.2,-0.619222515000013));
#266089=CARTESIAN_POINT('Ctrl Pts',(-11.3116760820001,12.2,-0.620868001000012));
#266090=CARTESIAN_POINT('Ctrl Pts',(-11.3148702170001,12.2,-0.622518091000015));
#266091=CARTESIAN_POINT('Ctrl Pts',(-11.3180671910001,12.2,-0.624172784000017));
#266092=CARTESIAN_POINT('Ctrl Pts',(-11.3212669940001,12.2,-0.625832085000013));
#266093=CARTESIAN_POINT('Ctrl Pts',(-11.3244696160001,12.2,-0.627495996000014));
#266094=CARTESIAN_POINT('Ctrl Pts',(-11.3276750490001,12.2,-0.629164515000014));
#266095=CARTESIAN_POINT('Ctrl Pts',(-11.3308832820001,12.2,-0.630837648000018));
#266096=CARTESIAN_POINT('Ctrl Pts',(-11.3340943080001,12.2,-0.632515395000013));
#266097=CARTESIAN_POINT('Ctrl Pts',(-11.3373081150001,12.2,-0.634197758000017));
#266098=CARTESIAN_POINT('Ctrl Pts',(-11.3405246950001,12.2,-0.635884737000012));
#266099=CARTESIAN_POINT('Ctrl Pts',(-11.3437440390001,12.2,-0.637576336000016));
#266100=CARTESIAN_POINT('Ctrl Pts',(-11.3469661360001,12.2,-0.639272557000012));
#266101=CARTESIAN_POINT('Ctrl Pts',(-11.3501909790001,12.2,-0.640973401000018));
#266102=CARTESIAN_POINT('Ctrl Pts',(-11.3534185570001,12.2,-0.642678869000015));
#266103=CARTESIAN_POINT('Ctrl Pts',(-11.3566488620001,12.2,-0.644388964000013));
#266104=CARTESIAN_POINT('Ctrl Pts',(-11.3598818840001,12.2,-0.646103687000017));
#266105=CARTESIAN_POINT('Ctrl Pts',(-11.3631176140001,12.2,-0.647823039000013));
#266106=CARTESIAN_POINT('Ctrl Pts',(-11.3663560430001,12.2,-0.649547023000014));
#266107=CARTESIAN_POINT('Ctrl Pts',(-11.3695971620001,12.2,-0.651275639000013));
#266108=CARTESIAN_POINT('Ctrl Pts',(-11.3728409600001,12.2,-0.653008892000013));
#266109=CARTESIAN_POINT('Ctrl Pts',(-11.3760874300001,12.2,-0.654746780000015));
#266110=CARTESIAN_POINT('Ctrl Pts',(-11.3793365610001,12.2,-0.656489306000014));
#266111=CARTESIAN_POINT('Ctrl Pts',(-11.3825883450001,12.2,-0.658236472000016));
#266112=CARTESIAN_POINT('Ctrl Pts',(-11.3858427730001,12.2,-0.659988280000015));
#266113=CARTESIAN_POINT('Ctrl Pts',(-11.3890998350001,12.2,-0.661744730000016));
#266114=CARTESIAN_POINT('Ctrl Pts',(-11.3923595230001,12.2,-0.663505825000015));
#266115=CARTESIAN_POINT('Ctrl Pts',(-11.3956218280001,12.2,-0.665271566000012));
#266116=CARTESIAN_POINT('Ctrl Pts',(-11.3988867400001,12.2,-0.667041955000016));
#266117=CARTESIAN_POINT('Ctrl Pts',(-11.4021542520001,12.2,-0.668816993000014));
#266118=CARTESIAN_POINT('Ctrl Pts',(-11.4054243520001,12.2,-0.670596683000015));
#266119=CARTESIAN_POINT('Ctrl Pts',(-11.4086970320001,12.2,-0.672381023000015));
#266120=CARTESIAN_POINT('Ctrl Pts',(-11.4119722840001,12.2,-0.674170019000013));
#266121=CARTESIAN_POINT('Ctrl Pts',(-11.4152500960001,12.2,-0.675963670000015));
#266122=CARTESIAN_POINT('Ctrl Pts',(-11.4185304610001,12.2,-0.677761979000016));
#266123=CARTESIAN_POINT('Ctrl Pts',(-11.4218133690001,12.2,-0.679564946000015));
#266124=CARTESIAN_POINT('Ctrl Pts',(-11.4250988120001,12.2,-0.681372573000014));
#266125=CARTESIAN_POINT('Ctrl Pts',(-11.4283867810001,12.2,-0.683184862000012));
#266126=CARTESIAN_POINT('Ctrl Pts',(-11.4316772700001,12.2,-0.685001814000015));
#266127=CARTESIAN_POINT('Ctrl Pts',(-11.4349702680001,12.2,-0.686823430000012));
#266128=CARTESIAN_POINT('Ctrl Pts',(-11.4382657700001,12.2,-0.688649711000018));
#266129=CARTESIAN_POINT('Ctrl Pts',(-11.4415637630001,12.2,-0.690480659000015));
#266130=CARTESIAN_POINT('Ctrl Pts',(-11.4448642400001,12.2,-0.692316276000016));
#266131=CARTESIAN_POINT('Ctrl Pts',(-11.4481671870001,12.2,-0.694156565000017));
#266132=CARTESIAN_POINT('Ctrl Pts',(-11.4514725950001,12.2,-0.696001525000014));
#266133=CARTESIAN_POINT('Ctrl Pts',(-11.4547804530001,12.2,-0.697851159000016));
#266134=CARTESIAN_POINT('Ctrl Pts',(-11.4580907510001,12.2,-0.699705470000014));
#266135=CARTESIAN_POINT('Ctrl Pts',(-11.4614034810001,12.2,-0.701564457000017));
#266136=CARTESIAN_POINT('Ctrl Pts',(-11.4647186380001,12.2,-0.703428121000016));
#266137=CARTESIAN_POINT('Ctrl Pts',(-11.4680362160001,12.2,-0.705296464000016));
#266138=CARTESIAN_POINT('Ctrl Pts',(-11.4713562160001,12.2,-0.707169486000012));
#266139=CARTESIAN_POINT('Ctrl Pts',(-11.4740141490001,12.2,-0.708671646000014));
#266140=CARTESIAN_POINT('Ctrl Pts',(-11.4760086880001,12.2,-0.709800372000018));
#266141=CARTESIAN_POINT('Ctrl Pts',(-11.4773388640001,12.2,-0.710553791000015));
#266142=CARTESIAN_POINT('Ctrl Pts',(-11.4780040730001,12.2,-0.710930734000015));
#266143=CARTESIAN_POINT('Origin',(-5.66257110645729E-14,15.2,-1.77635683940025E-14));
#266144=CARTESIAN_POINT('',(-10.2237731093969,15.2,-1.76496130634431));
#266145=CARTESIAN_POINT('',(-10.2237731093969,12.2,-1.76496130634431));
#266146=CARTESIAN_POINT('',(-10.2237731090001,15.2,-1.76496130600002));
#266147=CARTESIAN_POINT('Origin',(-5.66257110645729E-14,12.2,-1.77635683940025E-14));
#266148=CARTESIAN_POINT('Origin',(-5.66257110645729E-14,15.2,-1.77635683940025E-14));
#266149=CARTESIAN_POINT('Origin',(-5.66257110645729E-14,15.2,-1.77635683940025E-14));
#266150=CARTESIAN_POINT('',(-11.2599985490001,15.2,-2.33718477800001));
#266151=CARTESIAN_POINT('',(-11.1757778680001,15.2,-2.71145515300002));
#266152=CARTESIAN_POINT('Origin',(-5.66257110645729E-14,15.2,-1.77635683940025E-14));
#266153=CARTESIAN_POINT('',(-11.1757778680001,12.2,-2.71145515300002));
#266154=CARTESIAN_POINT('',(-11.1757778680001,15.2,-2.71145515300002));
#266155=CARTESIAN_POINT('',(-11.2599985490001,12.2,-2.33718477800001));
#266156=CARTESIAN_POINT('Origin',(-5.66257110645729E-14,12.2,-1.77635683940025E-14));
#266157=CARTESIAN_POINT('',(-11.2599985490001,15.2,-2.33718477800001));
#266158=CARTESIAN_POINT('Ctrl Pts',(-10.2237731100001,15.2,-1.76496130700002));
#266159=CARTESIAN_POINT('Ctrl Pts',(-10.2237731100001,11.6,-1.76496130700002));
#266160=CARTESIAN_POINT('Ctrl Pts',(-10.2239417410001,15.2,-1.76500562400001));
#266161=CARTESIAN_POINT('Ctrl Pts',(-10.2239417410001,11.6,-1.76500562400001));
#266162=CARTESIAN_POINT('Ctrl Pts',(-10.2242848730001,15.2,-1.76509588800001));
#266163=CARTESIAN_POINT('Ctrl Pts',(-10.2242848730001,11.6,-1.76509588800001));
#266164=CARTESIAN_POINT('Ctrl Pts',(-10.2248047310001,15.2,-1.76523291900001));
#266165=CARTESIAN_POINT('Ctrl Pts',(-10.2248047310001,11.6,-1.76523291900002));
#266166=CARTESIAN_POINT('Ctrl Pts',(-10.2255048910001,15.2,-1.76541803300001));
#266167=CARTESIAN_POINT('Ctrl Pts',(-10.2255048910001,11.6,-1.76541803300002));
#266168=CARTESIAN_POINT('Ctrl Pts',(-10.2263902540001,15.2,-1.76565305800001));
#266169=CARTESIAN_POINT('Ctrl Pts',(-10.2263902540001,11.6,-1.76565305800001));
#266170=CARTESIAN_POINT('Ctrl Pts',(-10.2272897270001,15.2,-1.76589279500002));
#266171=CARTESIAN_POINT('Ctrl Pts',(-10.2272897270001,11.6,-1.76589279500002));
#266172=CARTESIAN_POINT('Ctrl Pts',(-10.2281981500001,15.2,-1.76613589400001));
#266173=CARTESIAN_POINT('Ctrl Pts',(-10.2281981500001,11.6,-1.76613589400001));
#266174=CARTESIAN_POINT('Ctrl Pts',(-10.2291154920001,15.2,-1.76638236500001));
#266175=CARTESIAN_POINT('Ctrl Pts',(-10.2291154920001,11.6,-1.76638236500001));
#266176=CARTESIAN_POINT('Ctrl Pts',(-10.2300417240001,15.2,-1.76663221900001));
#266177=CARTESIAN_POINT('Ctrl Pts',(-10.2300417240001,11.6,-1.76663221900002));
#266178=CARTESIAN_POINT('Ctrl Pts',(-10.2309768130001,15.2,-1.76688546700001));
#266179=CARTESIAN_POINT('Ctrl Pts',(-10.2309768130001,11.6,-1.76688546700001));
#266180=CARTESIAN_POINT('Ctrl Pts',(-10.2319207290001,15.2,-1.76714211800002));
#266181=CARTESIAN_POINT('Ctrl Pts',(-10.2319207290001,11.6,-1.76714211800002));
#266182=CARTESIAN_POINT('Ctrl Pts',(-10.2328734440001,15.2,-1.76740218200001));
#266183=CARTESIAN_POINT('Ctrl Pts',(-10.2328734440001,11.6,-1.76740218200001));
#266184=CARTESIAN_POINT('Ctrl Pts',(-10.2338349260001,15.2,-1.76766567100001));
#266185=CARTESIAN_POINT('Ctrl Pts',(-10.2338349260001,11.6,-1.76766567100001));
#266186=CARTESIAN_POINT('Ctrl Pts',(-10.2348051460001,15.2,-1.76793259300001));
#266187=CARTESIAN_POINT('Ctrl Pts',(-10.2348051460001,11.6,-1.76793259300001));
#266188=CARTESIAN_POINT('Ctrl Pts',(-10.2357840740001,15.2,-1.76820296000002));
#266189=CARTESIAN_POINT('Ctrl Pts',(-10.2357840740001,11.6,-1.76820296000002));
#266190=CARTESIAN_POINT('Ctrl Pts',(-10.2367716800001,15.2,-1.76847678200001));
#266191=CARTESIAN_POINT('Ctrl Pts',(-10.2367716800001,11.6,-1.76847678200002));
#266192=CARTESIAN_POINT('Ctrl Pts',(-10.2377679360001,15.2,-1.76875406700002));
#266193=CARTESIAN_POINT('Ctrl Pts',(-10.2377679360001,11.6,-1.76875406700002));
#266194=CARTESIAN_POINT('Ctrl Pts',(-10.2387728090001,15.2,-1.76903482700002));
#266195=CARTESIAN_POINT('Ctrl Pts',(-10.2387728090001,11.6,-1.76903482700002));
#266196=CARTESIAN_POINT('Ctrl Pts',(-10.2397862740001,15.2,-1.76931907200002));
#266197=CARTESIAN_POINT('Ctrl Pts',(-10.2397862740001,11.6,-1.76931907200002));
#266198=CARTESIAN_POINT('Ctrl Pts',(-10.2408083000001,15.2,-1.76960681000002));
#266199=CARTESIAN_POINT('Ctrl Pts',(-10.2408083000001,11.6,-1.76960681000002));
#266200=CARTESIAN_POINT('Ctrl Pts',(-10.2418388590001,15.2,-1.76989805200002));
#266201=CARTESIAN_POINT('Ctrl Pts',(-10.2418388590001,11.6,-1.76989805200002));
#266202=CARTESIAN_POINT('Ctrl Pts',(-10.2428779210001,15.2,-1.77019280700002));
#266203=CARTESIAN_POINT('Ctrl Pts',(-10.2428779210001,11.6,-1.77019280700002));
#266204=CARTESIAN_POINT('Ctrl Pts',(-10.2439254560001,15.2,-1.77049108600002));
#266205=CARTESIAN_POINT('Ctrl Pts',(-10.2439254560001,11.6,-1.77049108600002));
#266206=CARTESIAN_POINT('Ctrl Pts',(-10.2449814390001,15.2,-1.77079289700002));
#266207=CARTESIAN_POINT('Ctrl Pts',(-10.2449814390001,11.6,-1.77079289700002));
#266208=CARTESIAN_POINT('Ctrl Pts',(-10.2460458400001,15.2,-1.77109824900001));
#266209=CARTESIAN_POINT('Ctrl Pts',(-10.2460458400001,11.6,-1.77109824900001));
#266210=CARTESIAN_POINT('Ctrl Pts',(-10.2471186300001,15.2,-1.77140715300002));
#266211=CARTESIAN_POINT('Ctrl Pts',(-10.2471186300001,11.6,-1.77140715300002));
#266212=CARTESIAN_POINT('Ctrl Pts',(-10.2481997820001,15.2,-1.77171961900001));
#266213=CARTESIAN_POINT('Ctrl Pts',(-10.2481997820001,11.6,-1.77171961900001));
#266214=CARTESIAN_POINT('Ctrl Pts',(-10.2492892660001,15.2,-1.77203565400001));
#266215=CARTESIAN_POINT('Ctrl Pts',(-10.2492892660001,11.6,-1.77203565400002));
#266216=CARTESIAN_POINT('Ctrl Pts',(-10.2503870570001,15.2,-1.77235526900001));
#266217=CARTESIAN_POINT('Ctrl Pts',(-10.2503870570001,11.6,-1.77235526900001));
#266218=CARTESIAN_POINT('Ctrl Pts',(-10.2514931250001,15.2,-1.77267847300001));
#266219=CARTESIAN_POINT('Ctrl Pts',(-10.2514931250001,11.6,-1.77267847300001));
#266220=CARTESIAN_POINT('Ctrl Pts',(-10.2526074440001,15.2,-1.77300527500002));
#266221=CARTESIAN_POINT('Ctrl Pts',(-10.2526074440001,11.6,-1.77300527500002));
#266222=CARTESIAN_POINT('Ctrl Pts',(-10.2537299850001,15.2,-1.77333568400002));
#266223=CARTESIAN_POINT('Ctrl Pts',(-10.2537299850001,11.6,-1.77333568400002));
#266224=CARTESIAN_POINT('Ctrl Pts',(-10.2548607200001,15.2,-1.77366970900001));
#266225=CARTESIAN_POINT('Ctrl Pts',(-10.2548607200001,11.6,-1.77366970900001));
#266226=CARTESIAN_POINT('Ctrl Pts',(-10.2559996250001,15.2,-1.77400735800001));
#266227=CARTESIAN_POINT('Ctrl Pts',(-10.2559996250001,11.6,-1.77400735800001));
#266228=CARTESIAN_POINT('Ctrl Pts',(-10.2571466690001,15.2,-1.77434864200002));
#266229=CARTESIAN_POINT('Ctrl Pts',(-10.2571466690001,11.6,-1.77434864200002));
#266230=CARTESIAN_POINT('Ctrl Pts',(-10.2583018280001,15.2,-1.77469356900001));
#266231=CARTESIAN_POINT('Ctrl Pts',(-10.2583018280001,11.6,-1.77469356900001));
#266232=CARTESIAN_POINT('Ctrl Pts',(-10.2594650730001,15.2,-1.77504214700001));
#266233=CARTESIAN_POINT('Ctrl Pts',(-10.2594650730001,11.6,-1.77504214700001));
#266234=CARTESIAN_POINT('Ctrl Pts',(-10.2606363780001,15.2,-1.77539438600002));
#266235=CARTESIAN_POINT('Ctrl Pts',(-10.2606363780001,11.6,-1.77539438600002));
#266236=CARTESIAN_POINT('Ctrl Pts',(-10.2618157170001,15.2,-1.77575029400002));
#266237=CARTESIAN_POINT('Ctrl Pts',(-10.2618157170001,11.6,-1.77575029400002));
#266238=CARTESIAN_POINT('Ctrl Pts',(-10.2630030620001,15.2,-1.77610988000001));
#266239=CARTESIAN_POINT('Ctrl Pts',(-10.2630030620001,11.6,-1.77610988000001));
#266240=CARTESIAN_POINT('Ctrl Pts',(-10.2641983870001,15.2,-1.77647315300002));
#266241=CARTESIAN_POINT('Ctrl Pts',(-10.2641983870001,11.6,-1.77647315300002));
#266242=CARTESIAN_POINT('Ctrl Pts',(-10.2654016660001,15.2,-1.77684012100002));
#266243=CARTESIAN_POINT('Ctrl Pts',(-10.2654016660001,11.6,-1.77684012100002));
#266244=CARTESIAN_POINT('Ctrl Pts',(-10.2666128740001,15.2,-1.77721079200001));
#266245=CARTESIAN_POINT('Ctrl Pts',(-10.2666128740001,11.6,-1.77721079200001));
#266246=CARTESIAN_POINT('Ctrl Pts',(-10.2678319830001,15.2,-1.77758517500001));
#266247=CARTESIAN_POINT('Ctrl Pts',(-10.2678319830001,11.6,-1.77758517500001));
#266248=CARTESIAN_POINT('Ctrl Pts',(-10.2690589670001,15.2,-1.77796328000001));
#266249=CARTESIAN_POINT('Ctrl Pts',(-10.2690589670001,11.6,-1.77796328000001));
#266250=CARTESIAN_POINT('Ctrl Pts',(-10.2702938010001,15.2,-1.77834511200002));
#266251=CARTESIAN_POINT('Ctrl Pts',(-10.2702938010001,11.6,-1.77834511200002));
#266252=CARTESIAN_POINT('Ctrl Pts',(-10.2715364580001,15.2,-1.77873068300002));
#266253=CARTESIAN_POINT('Ctrl Pts',(-10.2715364580001,11.6,-1.77873068300002));
#266254=CARTESIAN_POINT('Ctrl Pts',(-10.2727869140001,15.2,-1.77911999900001));
#266255=CARTESIAN_POINT('Ctrl Pts',(-10.2727869140001,11.6,-1.77911999900001));
#266256=CARTESIAN_POINT('Ctrl Pts',(-10.2740451430001,15.2,-1.77951306800002));
#266257=CARTESIAN_POINT('Ctrl Pts',(-10.2740451430001,11.6,-1.77951306800002));
#266258=CARTESIAN_POINT('Ctrl Pts',(-10.2753111180001,15.2,-1.77990989900001));
#266259=CARTESIAN_POINT('Ctrl Pts',(-10.2753111180001,11.6,-1.77990989900001));
#266260=CARTESIAN_POINT('Ctrl Pts',(-10.2765848160001,15.2,-1.78031050100001));
#266261=CARTESIAN_POINT('Ctrl Pts',(-10.2765848160001,11.6,-1.78031050100001));
#266262=CARTESIAN_POINT('Ctrl Pts',(-10.2778662100001,15.2,-1.78071488100001));
#266263=CARTESIAN_POINT('Ctrl Pts',(-10.2778662100001,11.6,-1.78071488100001));
#266264=CARTESIAN_POINT('Ctrl Pts',(-10.2791552770001,15.2,-1.78112304700001));
#266265=CARTESIAN_POINT('Ctrl Pts',(-10.2791552770001,11.6,-1.78112304700001));
#266266=CARTESIAN_POINT('Ctrl Pts',(-10.2804519880001,15.2,-1.78153500600001));
#266267=CARTESIAN_POINT('Ctrl Pts',(-10.2804519880001,11.6,-1.78153500600002));
#266268=CARTESIAN_POINT('Ctrl Pts',(-10.2817563210001,15.2,-1.78195076800002));
#266269=CARTESIAN_POINT('Ctrl Pts',(-10.2817563210001,11.6,-1.78195076800002));
#266270=CARTESIAN_POINT('Ctrl Pts',(-10.2830682520001,15.2,-1.78237034000002));
#266271=CARTESIAN_POINT('Ctrl Pts',(-10.2830682520001,11.6,-1.78237034000002));
#266272=CARTESIAN_POINT('Ctrl Pts',(-10.2843877540001,15.2,-1.78279372900001));
#266273=CARTESIAN_POINT('Ctrl Pts',(-10.2843877540001,11.6,-1.78279372900001));
#266274=CARTESIAN_POINT('Ctrl Pts',(-10.2857148030001,15.2,-1.78322094400002));
#266275=CARTESIAN_POINT('Ctrl Pts',(-10.2857148030001,11.6,-1.78322094400002));
#266276=CARTESIAN_POINT('Ctrl Pts',(-10.2870493750001,15.2,-1.78365199300002));
#266277=CARTESIAN_POINT('Ctrl Pts',(-10.2870493750001,11.6,-1.78365199300002));
#266278=CARTESIAN_POINT('Ctrl Pts',(-10.2883914450001,15.2,-1.78408688200001));
#266279=CARTESIAN_POINT('Ctrl Pts',(-10.2883914450001,11.6,-1.78408688200001));
#266280=CARTESIAN_POINT('Ctrl Pts',(-10.2897409890001,15.2,-1.78452562100002));
#266281=CARTESIAN_POINT('Ctrl Pts',(-10.2897409890001,11.6,-1.78452562100002));
#266282=CARTESIAN_POINT('Ctrl Pts',(-10.2910979840001,15.2,-1.78496821600001));
#266283=CARTESIAN_POINT('Ctrl Pts',(-10.2910979840001,11.6,-1.78496821600001));
#266284=CARTESIAN_POINT('Ctrl Pts',(-10.2924624030001,15.2,-1.78541467500001));
#266285=CARTESIAN_POINT('Ctrl Pts',(-10.2924624030001,11.6,-1.78541467500001));
#266286=CARTESIAN_POINT('Ctrl Pts',(-10.2938342240001,15.2,-1.78586500400002));
#266287=CARTESIAN_POINT('Ctrl Pts',(-10.2938342240001,11.6,-1.78586500400002));
#266288=CARTESIAN_POINT('Ctrl Pts',(-10.2952134230001,15.2,-1.78631921300001));
#266289=CARTESIAN_POINT('Ctrl Pts',(-10.2952134230001,11.6,-1.78631921300001));
#266290=CARTESIAN_POINT('Ctrl Pts',(-10.2965999750001,15.2,-1.78677730900001));
#266291=CARTESIAN_POINT('Ctrl Pts',(-10.2965999750001,11.6,-1.78677730900001));
#266292=CARTESIAN_POINT('Ctrl Pts',(-10.2979938570001,15.2,-1.78723929800002));
#266293=CARTESIAN_POINT('Ctrl Pts',(-10.2979938570001,11.6,-1.78723929800002));
#266294=CARTESIAN_POINT('Ctrl Pts',(-10.2993950460001,15.2,-1.78770518800001));
#266295=CARTESIAN_POINT('Ctrl Pts',(-10.2993950460001,11.6,-1.78770518800001));
#266296=CARTESIAN_POINT('Ctrl Pts',(-10.3008035180001,15.2,-1.78817498600001));
#266297=CARTESIAN_POINT('Ctrl Pts',(-10.3008035180001,11.6,-1.78817498600001));
#266298=CARTESIAN_POINT('Ctrl Pts',(-10.3022192480001,15.2,-1.78864870100002));
#266299=CARTESIAN_POINT('Ctrl Pts',(-10.3022192480001,11.6,-1.78864870100002));
#266300=CARTESIAN_POINT('Ctrl Pts',(-10.3036422150001,15.2,-1.78912633800001));
#266301=CARTESIAN_POINT('Ctrl Pts',(-10.3036422150001,11.6,-1.78912633800001));
#266302=CARTESIAN_POINT('Ctrl Pts',(-10.3050723940001,15.2,-1.78960790500001));
#266303=CARTESIAN_POINT('Ctrl Pts',(-10.3050723940001,11.6,-1.78960790500002));
#266304=CARTESIAN_POINT('Ctrl Pts',(-10.3065097620001,15.2,-1.79009341000001));
#266305=CARTESIAN_POINT('Ctrl Pts',(-10.3065097620001,11.6,-1.79009341000001));
#266306=CARTESIAN_POINT('Ctrl Pts',(-10.3079542970001,15.2,-1.79058285800001));
#266307=CARTESIAN_POINT('Ctrl Pts',(-10.3079542970001,11.6,-1.79058285800001));
#266308=CARTESIAN_POINT('Ctrl Pts',(-10.3094059740001,15.2,-1.79107625800001));
#266309=CARTESIAN_POINT('Ctrl Pts',(-10.3094059740001,11.6,-1.79107625800001));
#266310=CARTESIAN_POINT('Ctrl Pts',(-10.3108647730001,15.2,-1.79157361600002));
#266311=CARTESIAN_POINT('Ctrl Pts',(-10.3108647730001,11.6,-1.79157361600002));
#266312=CARTESIAN_POINT('Ctrl Pts',(-10.3123306680001,15.2,-1.79207494100002));
#266313=CARTESIAN_POINT('Ctrl Pts',(-10.3123306680001,11.6,-1.79207494100002));
#266314=CARTESIAN_POINT('Ctrl Pts',(-10.3138036390001,15.2,-1.79258023700001));
#266315=CARTESIAN_POINT('Ctrl Pts',(-10.3138036390001,11.6,-1.79258023700001));
#266316=CARTESIAN_POINT('Ctrl Pts',(-10.3152836600001,15.2,-1.79308951300001));
#266317=CARTESIAN_POINT('Ctrl Pts',(-10.3152836600001,11.6,-1.79308951300001));
#266318=CARTESIAN_POINT('Ctrl Pts',(-10.3167707130001,15.2,-1.79360277400002));
#266319=CARTESIAN_POINT('Ctrl Pts',(-10.3167707130001,11.6,-1.79360277400002));
#266320=CARTESIAN_POINT('Ctrl Pts',(-10.3182647710001,15.2,-1.79412002800001));
#266321=CARTESIAN_POINT('Ctrl Pts',(-10.3182647710001,11.6,-1.79412002800001));
#266322=CARTESIAN_POINT('Ctrl Pts',(-10.3197658140001,15.2,-1.79464128300001));
#266323=CARTESIAN_POINT('Ctrl Pts',(-10.3197658140001,11.6,-1.79464128300001));
#266324=CARTESIAN_POINT('Ctrl Pts',(-10.3212738190001,15.2,-1.79516654400001));
#266325=CARTESIAN_POINT('Ctrl Pts',(-10.3212738190001,11.6,-1.79516654400001));
#266326=CARTESIAN_POINT('Ctrl Pts',(-10.3227887640001,15.2,-1.79569581700001));
#266327=CARTESIAN_POINT('Ctrl Pts',(-10.3227887640001,11.6,-1.79569581700001));
#266328=CARTESIAN_POINT('Ctrl Pts',(-10.3243106270001,15.2,-1.79622911100001));
#266329=CARTESIAN_POINT('Ctrl Pts',(-10.3243106270001,11.6,-1.79622911100001));
#266330=CARTESIAN_POINT('Ctrl Pts',(-10.3258393850001,15.2,-1.79676643100001));
#266331=CARTESIAN_POINT('Ctrl Pts',(-10.3258393850001,11.6,-1.79676643100001));
#266332=CARTESIAN_POINT('Ctrl Pts',(-10.3273750170001,15.2,-1.79730778300002));
#266333=CARTESIAN_POINT('Ctrl Pts',(-10.3273750170001,11.6,-1.79730778300002));
#266334=CARTESIAN_POINT('Ctrl Pts',(-10.3289175010001,15.2,-1.79785317600002));
#266335=CARTESIAN_POINT('Ctrl Pts',(-10.3289175010001,11.6,-1.79785317600002));
#266336=CARTESIAN_POINT('Ctrl Pts',(-10.3304668150001,15.2,-1.79840261500001));
#266337=CARTESIAN_POINT('Ctrl Pts',(-10.3304668150001,11.6,-1.79840261500001));
#266338=CARTESIAN_POINT('Ctrl Pts',(-10.3320229360001,15.2,-1.79895610500001));
#266339=CARTESIAN_POINT('Ctrl Pts',(-10.3320229360001,11.6,-1.79895610500001));
#266340=CARTESIAN_POINT('Ctrl Pts',(-10.3335858440001,15.2,-1.79951365400001));
#266341=CARTESIAN_POINT('Ctrl Pts',(-10.3335858440001,11.6,-1.79951365400001));
#266342=CARTESIAN_POINT('Ctrl Pts',(-10.3351555170001,15.2,-1.80007527000001));
#266343=CARTESIAN_POINT('Ctrl Pts',(-10.3351555170001,11.6,-1.80007527000001));
#266344=CARTESIAN_POINT('Ctrl Pts',(-10.3367319330001,15.2,-1.80064095700001));
#266345=CARTESIAN_POINT('Ctrl Pts',(-10.3367319330001,11.6,-1.80064095700002));
#266346=CARTESIAN_POINT('Ctrl Pts',(-10.3383150710001,15.2,-1.80121072200001));
#266347=CARTESIAN_POINT('Ctrl Pts',(-10.3383150710001,11.6,-1.80121072200001));
#266348=CARTESIAN_POINT('Ctrl Pts',(-10.3399049090001,15.2,-1.80178457100002));
#266349=CARTESIAN_POINT('Ctrl Pts',(-10.3399049090001,11.6,-1.80178457100002));
#266350=CARTESIAN_POINT('Ctrl Pts',(-10.3415014270001,15.2,-1.80236251100002));
#266351=CARTESIAN_POINT('Ctrl Pts',(-10.3415014270001,11.6,-1.80236251100002));
#266352=CARTESIAN_POINT('Ctrl Pts',(-10.3431046030001,15.2,-1.80294454800002));
#266353=CARTESIAN_POINT('Ctrl Pts',(-10.3431046030001,11.6,-1.80294454800002));
#266354=CARTESIAN_POINT('Ctrl Pts',(-10.3447144150001,15.2,-1.80353068700001));
#266355=CARTESIAN_POINT('Ctrl Pts',(-10.3447144150001,11.6,-1.80353068700001));
#266356=CARTESIAN_POINT('Ctrl Pts',(-10.3463308440001,15.2,-1.80412093600001));
#266357=CARTESIAN_POINT('Ctrl Pts',(-10.3463308440001,11.6,-1.80412093600001));
#266358=CARTESIAN_POINT('Ctrl Pts',(-10.3479538660001,15.2,-1.80471530000001));
#266359=CARTESIAN_POINT('Ctrl Pts',(-10.3479538660001,11.6,-1.80471530000002));
#266360=CARTESIAN_POINT('Ctrl Pts',(-10.3495834630001,15.2,-1.80531378500001));
#266361=CARTESIAN_POINT('Ctrl Pts',(-10.3495834630001,11.6,-1.80531378500001));
#266362=CARTESIAN_POINT('Ctrl Pts',(-10.3512196130001,15.2,-1.80591639700001));
#266363=CARTESIAN_POINT('Ctrl Pts',(-10.3512196130001,11.6,-1.80591639700001));
#266364=CARTESIAN_POINT('Ctrl Pts',(-10.3528622950001,15.2,-1.80652314400001));
#266365=CARTESIAN_POINT('Ctrl Pts',(-10.3528622950001,11.6,-1.80652314400001));
#266366=CARTESIAN_POINT('Ctrl Pts',(-10.3545114890001,15.2,-1.80713402800002));
#266367=CARTESIAN_POINT('Ctrl Pts',(-10.3545114890001,11.6,-1.80713402800002));
#266368=CARTESIAN_POINT('Ctrl Pts',(-10.3561671730001,15.2,-1.80774905900002));
#266369=CARTESIAN_POINT('Ctrl Pts',(-10.3561671730001,11.6,-1.80774905900002));
#266370=CARTESIAN_POINT('Ctrl Pts',(-10.3578293270001,15.2,-1.80836824100002));
#266371=CARTESIAN_POINT('Ctrl Pts',(-10.3578293270001,11.6,-1.80836824100002));
#266372=CARTESIAN_POINT('Ctrl Pts',(-10.3594979320001,15.2,-1.80899157900001));
#266373=CARTESIAN_POINT('Ctrl Pts',(-10.3594979320001,11.6,-1.80899157900001));
#266374=CARTESIAN_POINT('Ctrl Pts',(-10.3611729670001,15.2,-1.80961908100001));
#266375=CARTESIAN_POINT('Ctrl Pts',(-10.3611729670001,11.6,-1.80961908100001));
#266376=CARTESIAN_POINT('Ctrl Pts',(-10.3628544100001,15.2,-1.81025075100001));
#266377=CARTESIAN_POINT('Ctrl Pts',(-10.3628544100001,11.6,-1.81025075100001));
#266378=CARTESIAN_POINT('Ctrl Pts',(-10.3645422430001,15.2,-1.81088659500002));
#266379=CARTESIAN_POINT('Ctrl Pts',(-10.3645422430001,11.6,-1.81088659500002));
#266380=CARTESIAN_POINT('Ctrl Pts',(-10.3662364440001,15.2,-1.81152662100001));
#266381=CARTESIAN_POINT('Ctrl Pts',(-10.3662364440001,11.6,-1.81152662100002));
#266382=CARTESIAN_POINT('Ctrl Pts',(-10.3679369930001,15.2,-1.81217083200002));
#266383=CARTESIAN_POINT('Ctrl Pts',(-10.3679369930001,11.6,-1.81217083200002));
#266384=CARTESIAN_POINT('Ctrl Pts',(-10.3696438710001,15.2,-1.81281923400002));
#266385=CARTESIAN_POINT('Ctrl Pts',(-10.3696438710001,11.6,-1.81281923400002));
#266386=CARTESIAN_POINT('Ctrl Pts',(-10.3713570580001,15.2,-1.81347183300002));
#266387=CARTESIAN_POINT('Ctrl Pts',(-10.3713570580001,11.6,-1.81347183300002));
#266388=CARTESIAN_POINT('Ctrl Pts',(-10.3730765340001,15.2,-1.81412863500002));
#266389=CARTESIAN_POINT('Ctrl Pts',(-10.3730765340001,11.6,-1.81412863500002));
#266390=CARTESIAN_POINT('Ctrl Pts',(-10.3748022770001,15.2,-1.81478964500001));
#266391=CARTESIAN_POINT('Ctrl Pts',(-10.3748022770001,11.6,-1.81478964500001));
#266392=CARTESIAN_POINT('Ctrl Pts',(-10.3765342700001,15.2,-1.81545487000002));
#266393=CARTESIAN_POINT('Ctrl Pts',(-10.3765342700001,11.6,-1.81545487000002));
#266394=CARTESIAN_POINT('Ctrl Pts',(-10.3782724920001,15.2,-1.81612431500001));
#266395=CARTESIAN_POINT('Ctrl Pts',(-10.3782724920001,11.6,-1.81612431500001));
#266396=CARTESIAN_POINT('Ctrl Pts',(-10.3800169250001,15.2,-1.81679798300001));
#266397=CARTESIAN_POINT('Ctrl Pts',(-10.3800169250001,11.6,-1.81679798300001));
#266398=CARTESIAN_POINT('Ctrl Pts',(-10.3817675460001,15.2,-1.81747588200002));
#266399=CARTESIAN_POINT('Ctrl Pts',(-10.3817675460001,11.6,-1.81747588200002));
#266400=CARTESIAN_POINT('Ctrl Pts',(-10.3835243380001,15.2,-1.81815801700001));
#266401=CARTESIAN_POINT('Ctrl Pts',(-10.3835243380001,11.6,-1.81815801700001));
#266402=CARTESIAN_POINT('Ctrl Pts',(-10.3852872810001,15.2,-1.81884439400001));
#266403=CARTESIAN_POINT('Ctrl Pts',(-10.3852872810001,11.6,-1.81884439400001));
#266404=CARTESIAN_POINT('Ctrl Pts',(-10.3870563570001,15.2,-1.81953501600002));
#266405=CARTESIAN_POINT('Ctrl Pts',(-10.3870563570001,11.6,-1.81953501600002));
#266406=CARTESIAN_POINT('Ctrl Pts',(-10.3888315440001,15.2,-1.82022989000002));
#266407=CARTESIAN_POINT('Ctrl Pts',(-10.3888315440001,11.6,-1.82022989000002));
#266408=CARTESIAN_POINT('Ctrl Pts',(-10.3906128240001,15.2,-1.82092902200001));
#266409=CARTESIAN_POINT('Ctrl Pts',(-10.3906128240001,11.6,-1.82092902200001));
#266410=CARTESIAN_POINT('Ctrl Pts',(-10.3924001790001,15.2,-1.82163241600001));
#266411=CARTESIAN_POINT('Ctrl Pts',(-10.3924001790001,11.6,-1.82163241600001));
#266412=CARTESIAN_POINT('Ctrl Pts',(-10.3941935880001,15.2,-1.82234007800002));
#266413=CARTESIAN_POINT('Ctrl Pts',(-10.3941935880001,11.6,-1.82234007800002));
#266414=CARTESIAN_POINT('Ctrl Pts',(-10.3959930320001,15.2,-1.82305201200001));
#266415=CARTESIAN_POINT('Ctrl Pts',(-10.3959930320001,11.6,-1.82305201200002));
#266416=CARTESIAN_POINT('Ctrl Pts',(-10.3977984930001,15.2,-1.82376822500002));
#266417=CARTESIAN_POINT('Ctrl Pts',(-10.3977984930001,11.6,-1.82376822500002));
#266418=CARTESIAN_POINT('Ctrl Pts',(-10.3996099520001,15.2,-1.82448872100001));
#266419=CARTESIAN_POINT('Ctrl Pts',(-10.3996099520001,11.6,-1.82448872100002));
#266420=CARTESIAN_POINT('Ctrl Pts',(-10.4014273890001,15.2,-1.82521350500001));
#266421=CARTESIAN_POINT('Ctrl Pts',(-10.4014273890001,11.6,-1.82521350500001));
#266422=CARTESIAN_POINT('Ctrl Pts',(-10.4032507880001,15.2,-1.82594258300002));
#266423=CARTESIAN_POINT('Ctrl Pts',(-10.4032507880001,11.6,-1.82594258300002));
#266424=CARTESIAN_POINT('Ctrl Pts',(-10.4050801260001,15.2,-1.82667595800002));
#266425=CARTESIAN_POINT('Ctrl Pts',(-10.4050801260001,11.6,-1.82667595800002));
#266426=CARTESIAN_POINT('Ctrl Pts',(-10.4069153870001,15.2,-1.82741363800002));
#266427=CARTESIAN_POINT('Ctrl Pts',(-10.4069153870001,11.6,-1.82741363800002));
#266428=CARTESIAN_POINT('Ctrl Pts',(-10.4087565520001,15.2,-1.82815562600001));
#266429=CARTESIAN_POINT('Ctrl Pts',(-10.4087565520001,11.6,-1.82815562600001));
#266430=CARTESIAN_POINT('Ctrl Pts',(-10.4106036030001,15.2,-1.82890192700001));
#266431=CARTESIAN_POINT('Ctrl Pts',(-10.4106036030001,11.6,-1.82890192700001));
#266432=CARTESIAN_POINT('Ctrl Pts',(-10.4124565210001,15.2,-1.82965254700001));
#266433=CARTESIAN_POINT('Ctrl Pts',(-10.4124565210001,11.6,-1.82965254700001));
#266434=CARTESIAN_POINT('Ctrl Pts',(-10.4143152860001,15.2,-1.83040749000002));
#266435=CARTESIAN_POINT('Ctrl Pts',(-10.4143152860001,11.6,-1.83040749000002));
#266436=CARTESIAN_POINT('Ctrl Pts',(-10.4161798810001,15.2,-1.83116676100001));
#266437=CARTESIAN_POINT('Ctrl Pts',(-10.4161798810001,11.6,-1.83116676100001));
#266438=CARTESIAN_POINT('Ctrl Pts',(-10.4180502880001,15.2,-1.83193036600001));
#266439=CARTESIAN_POINT('Ctrl Pts',(-10.4180502880001,11.6,-1.83193036600001));
#266440=CARTESIAN_POINT('Ctrl Pts',(-10.4199264880001,15.2,-1.83269830700001));
#266441=CARTESIAN_POINT('Ctrl Pts',(-10.4199264880001,11.6,-1.83269830700001));
#266442=CARTESIAN_POINT('Ctrl Pts',(-10.4218084630001,15.2,-1.83347059200001));
#266443=CARTESIAN_POINT('Ctrl Pts',(-10.4218084630001,11.6,-1.83347059200001));
#266444=CARTESIAN_POINT('Ctrl Pts',(-10.4236961950001,15.2,-1.83424722500002));
#266445=CARTESIAN_POINT('Ctrl Pts',(-10.4236961950001,11.6,-1.83424722500002));
#266446=CARTESIAN_POINT('Ctrl Pts',(-10.4255896650001,15.2,-1.83502820900001));
#266447=CARTESIAN_POINT('Ctrl Pts',(-10.4255896650001,11.6,-1.83502820900001));
#266448=CARTESIAN_POINT('Ctrl Pts',(-10.4274888570001,15.2,-1.83581355100001));
#266449=CARTESIAN_POINT('Ctrl Pts',(-10.4274888570001,11.6,-1.83581355100001));
#266450=CARTESIAN_POINT('Ctrl Pts',(-10.4293937510001,15.2,-1.83660325400002));
#266451=CARTESIAN_POINT('Ctrl Pts',(-10.4293937510001,11.6,-1.83660325400002));
#266452=CARTESIAN_POINT('Ctrl Pts',(-10.4313043290001,15.2,-1.83739732300001));
#266453=CARTESIAN_POINT('Ctrl Pts',(-10.4313043290001,11.6,-1.83739732300001));
#266454=CARTESIAN_POINT('Ctrl Pts',(-10.4332205740001,15.2,-1.83819576400001));
#266455=CARTESIAN_POINT('Ctrl Pts',(-10.4332205740001,11.6,-1.83819576400001));
#266456=CARTESIAN_POINT('Ctrl Pts',(-10.4351424680001,15.2,-1.83899858000002));
#266457=CARTESIAN_POINT('Ctrl Pts',(-10.4351424680001,11.6,-1.83899858000002));
#266458=CARTESIAN_POINT('Ctrl Pts',(-10.4370699940001,15.2,-1.83980577500002));
#266459=CARTESIAN_POINT('Ctrl Pts',(-10.4370699940001,11.6,-1.83980577500002));
#266460=CARTESIAN_POINT('Ctrl Pts',(-10.4390031330001,15.2,-1.84061735600002));
#266461=CARTESIAN_POINT('Ctrl Pts',(-10.4390031330001,11.6,-1.84061735600002));
#266462=CARTESIAN_POINT('Ctrl Pts',(-10.4409418670001,15.2,-1.84143332600001));
#266463=CARTESIAN_POINT('Ctrl Pts',(-10.4409418670001,11.6,-1.84143332600002));
#266464=CARTESIAN_POINT('Ctrl Pts',(-10.4428861800001,15.2,-1.84225369000002));
#266465=CARTESIAN_POINT('Ctrl Pts',(-10.4428861800001,11.6,-1.84225369000002));
#266466=CARTESIAN_POINT('Ctrl Pts',(-10.4448360520001,15.2,-1.84307845200001));
#266467=CARTESIAN_POINT('Ctrl Pts',(-10.4448360520001,11.6,-1.84307845200001));
#266468=CARTESIAN_POINT('Ctrl Pts',(-10.4467914690001,15.2,-1.84390761700001));
#266469=CARTESIAN_POINT('Ctrl Pts',(-10.4467914690001,11.6,-1.84390761700001));
#266470=CARTESIAN_POINT('Ctrl Pts',(-10.4487524110001,15.2,-1.84474118900001));
#266471=CARTESIAN_POINT('Ctrl Pts',(-10.4487524110001,11.6,-1.84474118900001));
#266472=CARTESIAN_POINT('Ctrl Pts',(-10.4507188600001,15.2,-1.84557917300001));
#266473=CARTESIAN_POINT('Ctrl Pts',(-10.4507188600001,11.6,-1.84557917300001));
#266474=CARTESIAN_POINT('Ctrl Pts',(-10.4526908010001,15.2,-1.84642157200001));
#266475=CARTESIAN_POINT('Ctrl Pts',(-10.4526908010001,11.6,-1.84642157200001));
#266476=CARTESIAN_POINT('Ctrl Pts',(-10.4546682150001,15.2,-1.84726839200001));
#266477=CARTESIAN_POINT('Ctrl Pts',(-10.4546682150001,11.6,-1.84726839200001));
#266478=CARTESIAN_POINT('Ctrl Pts',(-10.4566510860001,15.2,-1.84811963600001));
#266479=CARTESIAN_POINT('Ctrl Pts',(-10.4566510860001,11.6,-1.84811963600001));
#266480=CARTESIAN_POINT('Ctrl Pts',(-10.4586393950001,15.2,-1.84897530900002));
#266481=CARTESIAN_POINT('Ctrl Pts',(-10.4586393950001,11.6,-1.84897530900002));
#266482=CARTESIAN_POINT('Ctrl Pts',(-10.4606331260001,15.2,-1.84983541700001));
#266483=CARTESIAN_POINT('Ctrl Pts',(-10.4606331260001,11.6,-1.84983541700001));
#266484=CARTESIAN_POINT('Ctrl Pts',(-10.4626322630001,15.2,-1.85069996000002));
#266485=CARTESIAN_POINT('Ctrl Pts',(-10.4626322630001,11.6,-1.85069996000002));
#266486=CARTESIAN_POINT('Ctrl Pts',(-10.4646367870001,15.2,-1.85156894600001));
#266487=CARTESIAN_POINT('Ctrl Pts',(-10.4646367870001,11.6,-1.85156894600001));
#266488=CARTESIAN_POINT('Ctrl Pts',(-10.4666466810001,15.2,-1.85244237700001));
#266489=CARTESIAN_POINT('Ctrl Pts',(-10.4666466810001,11.6,-1.85244237700001));
#266490=CARTESIAN_POINT('Ctrl Pts',(-10.4686619290001,15.2,-1.85332026000002));
#266491=CARTESIAN_POINT('Ctrl Pts',(-10.4686619290001,11.6,-1.85332026000002));
#266492=CARTESIAN_POINT('Ctrl Pts',(-10.4706825140001,15.2,-1.85420259600001));
#266493=CARTESIAN_POINT('Ctrl Pts',(-10.4706825140001,11.6,-1.85420259600001));
#266494=CARTESIAN_POINT('Ctrl Pts',(-10.4727084200001,15.2,-1.85508939100002));
#266495=CARTESIAN_POINT('Ctrl Pts',(-10.4727084200001,11.6,-1.85508939100002));
#266496=CARTESIAN_POINT('Ctrl Pts',(-10.4747396280001,15.2,-1.85598064700002));
#266497=CARTESIAN_POINT('Ctrl Pts',(-10.4747396280001,11.6,-1.85598064700002));
#266498=CARTESIAN_POINT('Ctrl Pts',(-10.4767761230001,15.2,-1.85687637000001));
#266499=CARTESIAN_POINT('Ctrl Pts',(-10.4767761230001,11.6,-1.85687637000001));
#266500=CARTESIAN_POINT('Ctrl Pts',(-10.4788178880001,15.2,-1.85777656500001));
#266501=CARTESIAN_POINT('Ctrl Pts',(-10.4788178880001,11.6,-1.85777656500001));
#266502=CARTESIAN_POINT('Ctrl Pts',(-10.4808649060001,15.2,-1.85868123400001));
#266503=CARTESIAN_POINT('Ctrl Pts',(-10.4808649060001,11.6,-1.85868123400002));
#266504=CARTESIAN_POINT('Ctrl Pts',(-10.4829171610001,15.2,-1.85959038200001));
#266505=CARTESIAN_POINT('Ctrl Pts',(-10.4829171610001,11.6,-1.85959038200001));
#266506=CARTESIAN_POINT('Ctrl Pts',(-10.4849746350001,15.2,-1.86050401200001));
#266507=CARTESIAN_POINT('Ctrl Pts',(-10.4849746350001,11.6,-1.86050401200002));
#266508=CARTESIAN_POINT('Ctrl Pts',(-10.4870373130001,15.2,-1.86142212900001));
#266509=CARTESIAN_POINT('Ctrl Pts',(-10.4870373130001,11.6,-1.86142212900001));
#266510=CARTESIAN_POINT('Ctrl Pts',(-10.4891051780001,15.2,-1.86234473700001));
#266511=CARTESIAN_POINT('Ctrl Pts',(-10.4891051780001,11.6,-1.86234473700001));
#266512=CARTESIAN_POINT('Ctrl Pts',(-10.4911782130001,15.2,-1.86327184000001));
#266513=CARTESIAN_POINT('Ctrl Pts',(-10.4911782130001,11.6,-1.86327184000001));
#266514=CARTESIAN_POINT('Ctrl Pts',(-10.4932564020001,15.2,-1.86420344000001));
#266515=CARTESIAN_POINT('Ctrl Pts',(-10.4932564020001,11.6,-1.86420344000001));
#266516=CARTESIAN_POINT('Ctrl Pts',(-10.4953397300001,15.2,-1.86513954400001));
#266517=CARTESIAN_POINT('Ctrl Pts',(-10.4953397300001,11.6,-1.86513954400001));
#266518=CARTESIAN_POINT('Ctrl Pts',(-10.4974281790001,15.2,-1.86608015400001));
#266519=CARTESIAN_POINT('Ctrl Pts',(-10.4974281790001,11.6,-1.86608015400001));
#266520=CARTESIAN_POINT('Ctrl Pts',(-10.4995217330001,15.2,-1.86702527300001));
#266521=CARTESIAN_POINT('Ctrl Pts',(-10.4995217330001,11.6,-1.86702527300001));
#266522=CARTESIAN_POINT('Ctrl Pts',(-10.5016203770001,15.2,-1.86797490600001));
#266523=CARTESIAN_POINT('Ctrl Pts',(-10.5016203770001,11.6,-1.86797490600001));
#266524=CARTESIAN_POINT('Ctrl Pts',(-10.5037240940001,15.2,-1.86892905700001));
#266525=CARTESIAN_POINT('Ctrl Pts',(-10.5037240940001,11.6,-1.86892905700002));
#266526=CARTESIAN_POINT('Ctrl Pts',(-10.5058328690001,15.2,-1.86988772900001));
#266527=CARTESIAN_POINT('Ctrl Pts',(-10.5058328690001,11.6,-1.86988772900001));
#266528=CARTESIAN_POINT('Ctrl Pts',(-10.5079466830001,15.2,-1.87085092700002));
#266529=CARTESIAN_POINT('Ctrl Pts',(-10.5079466830001,11.6,-1.87085092700002));
#266530=CARTESIAN_POINT('Ctrl Pts',(-10.5100655220001,15.2,-1.87181865400001));
#266531=CARTESIAN_POINT('Ctrl Pts',(-10.5100655220001,11.6,-1.87181865400001));
#266532=CARTESIAN_POINT('Ctrl Pts',(-10.5121893710001,15.2,-1.87279091200002));
#266533=CARTESIAN_POINT('Ctrl Pts',(-10.5121893710001,11.6,-1.87279091200002));
#266534=CARTESIAN_POINT('Ctrl Pts',(-10.5143182130001,15.2,-1.87376770800002));
#266535=CARTESIAN_POINT('Ctrl Pts',(-10.5143182130001,11.6,-1.87376770800002));
#266536=CARTESIAN_POINT('Ctrl Pts',(-10.5164520310001,15.2,-1.87474904400001));
#266537=CARTESIAN_POINT('Ctrl Pts',(-10.5164520310001,11.6,-1.87474904400002));
#266538=CARTESIAN_POINT('Ctrl Pts',(-10.5185908110001,15.2,-1.87573492300002));
#266539=CARTESIAN_POINT('Ctrl Pts',(-10.5185908110001,11.6,-1.87573492300002));
#266540=CARTESIAN_POINT('Ctrl Pts',(-10.5207345370001,15.2,-1.87672534900001));
#266541=CARTESIAN_POINT('Ctrl Pts',(-10.5207345370001,11.6,-1.87672534900001));
#266542=CARTESIAN_POINT('Ctrl Pts',(-10.5228831920001,15.2,-1.87772032600002));
#266543=CARTESIAN_POINT('Ctrl Pts',(-10.5228831920001,11.6,-1.87772032600002));
#266544=CARTESIAN_POINT('Ctrl Pts',(-10.5250367610001,15.2,-1.87871985700002));
#266545=CARTESIAN_POINT('Ctrl Pts',(-10.5250367610001,11.6,-1.87871985700002));
#266546=CARTESIAN_POINT('Ctrl Pts',(-10.5271952300001,15.2,-1.87972394700001));
#266547=CARTESIAN_POINT('Ctrl Pts',(-10.5271952300001,11.6,-1.87972394700001));
#266548=CARTESIAN_POINT('Ctrl Pts',(-10.5293585800001,15.2,-1.88073259700001));
#266549=CARTESIAN_POINT('Ctrl Pts',(-10.5293585800001,11.6,-1.88073259700001));
#266550=CARTESIAN_POINT('Ctrl Pts',(-10.5315267990001,15.2,-1.88174581200002));
#266551=CARTESIAN_POINT('Ctrl Pts',(-10.5315267990001,11.6,-1.88174581200002));
#266552=CARTESIAN_POINT('Ctrl Pts',(-10.5336998690001,15.2,-1.88276359700001));
#266553=CARTESIAN_POINT('Ctrl Pts',(-10.5336998690001,11.6,-1.88276359700001));
#266554=CARTESIAN_POINT('Ctrl Pts',(-10.5358777760001,15.2,-1.88378595200001));
#266555=CARTESIAN_POINT('Ctrl Pts',(-10.5358777760001,11.6,-1.88378595200001));
#266556=CARTESIAN_POINT('Ctrl Pts',(-10.5380605030001,15.2,-1.88481288500002));
#266557=CARTESIAN_POINT('Ctrl Pts',(-10.5380605030001,11.6,-1.88481288500002));
#266558=CARTESIAN_POINT('Ctrl Pts',(-10.5402480350001,15.2,-1.88584439400001));
#266559=CARTESIAN_POINT('Ctrl Pts',(-10.5402480350001,11.6,-1.88584439400001));
#266560=CARTESIAN_POINT('Ctrl Pts',(-10.5424403580001,15.2,-1.88688048700001));
#266561=CARTESIAN_POINT('Ctrl Pts',(-10.5424403580001,11.6,-1.88688048700001));
#266562=CARTESIAN_POINT('Ctrl Pts',(-10.5446374560001,15.2,-1.88792116400001));
#266563=CARTESIAN_POINT('Ctrl Pts',(-10.5446374560001,11.6,-1.88792116400002));
#266564=CARTESIAN_POINT('Ctrl Pts',(-10.5468393120001,15.2,-1.88896643200001));
#266565=CARTESIAN_POINT('Ctrl Pts',(-10.5468393120001,11.6,-1.88896643200001));
#266566=CARTESIAN_POINT('Ctrl Pts',(-10.5490459140001,15.2,-1.89001629000002));
#266567=CARTESIAN_POINT('Ctrl Pts',(-10.5490459140001,11.6,-1.89001629000002));
#266568=CARTESIAN_POINT('Ctrl Pts',(-10.5512572450001,15.2,-1.89107074500001));
#266569=CARTESIAN_POINT('Ctrl Pts',(-10.5512572450001,11.6,-1.89107074500001));
#266570=CARTESIAN_POINT('Ctrl Pts',(-10.5534732880001,15.2,-1.89212980000002));
#266571=CARTESIAN_POINT('Ctrl Pts',(-10.5534732880001,11.6,-1.89212980000002));
#266572=CARTESIAN_POINT('Ctrl Pts',(-10.5556940320001,15.2,-1.89319345500001));
#266573=CARTESIAN_POINT('Ctrl Pts',(-10.5556940320001,11.6,-1.89319345500001));
#266574=CARTESIAN_POINT('Ctrl Pts',(-10.5579194590001,15.2,-1.89426171700001));
#266575=CARTESIAN_POINT('Ctrl Pts',(-10.5579194590001,11.6,-1.89426171700001));
#266576=CARTESIAN_POINT('Ctrl Pts',(-10.5601495550001,15.2,-1.89533458700001));
#266577=CARTESIAN_POINT('Ctrl Pts',(-10.5601495550001,11.6,-1.89533458700002));
#266578=CARTESIAN_POINT('Ctrl Pts',(-10.5623843040001,15.2,-1.89641206900002));
#266579=CARTESIAN_POINT('Ctrl Pts',(-10.5623843040001,11.6,-1.89641206900002));
#266580=CARTESIAN_POINT('Ctrl Pts',(-10.5646236920001,15.2,-1.89749416600002));
#266581=CARTESIAN_POINT('Ctrl Pts',(-10.5646236920001,11.6,-1.89749416600002));
#266582=CARTESIAN_POINT('Ctrl Pts',(-10.5668677030001,15.2,-1.89858088200001));
#266583=CARTESIAN_POINT('Ctrl Pts',(-10.5668677030001,11.6,-1.89858088200001));
#266584=CARTESIAN_POINT('Ctrl Pts',(-10.5691163240001,15.2,-1.89967222000002));
#266585=CARTESIAN_POINT('Ctrl Pts',(-10.5691163240001,11.6,-1.89967222000002));
#266586=CARTESIAN_POINT('Ctrl Pts',(-10.5713695390001,15.2,-1.90076818100001));
#266587=CARTESIAN_POINT('Ctrl Pts',(-10.5713695390001,11.6,-1.90076818100001));
#266588=CARTESIAN_POINT('Ctrl Pts',(-10.5736273340001,15.2,-1.90186877100002));
#266589=CARTESIAN_POINT('Ctrl Pts',(-10.5736273340001,11.6,-1.90186877100002));
#266590=CARTESIAN_POINT('Ctrl Pts',(-10.5758896930001,15.2,-1.90297399200002));
#266591=CARTESIAN_POINT('Ctrl Pts',(-10.5758896930001,11.6,-1.90297399200002));
#266592=CARTESIAN_POINT('Ctrl Pts',(-10.5781566020001,15.2,-1.90408384600001));
#266593=CARTESIAN_POINT('Ctrl Pts',(-10.5781566020001,11.6,-1.90408384600001));
#266594=CARTESIAN_POINT('Ctrl Pts',(-10.5804280450001,15.2,-1.90519833800002));
#266595=CARTESIAN_POINT('Ctrl Pts',(-10.5804280450001,11.6,-1.90519833800002));
#266596=CARTESIAN_POINT('Ctrl Pts',(-10.5827040090001,15.2,-1.90631747000001));
#266597=CARTESIAN_POINT('Ctrl Pts',(-10.5827040090001,11.6,-1.90631747000001));
#266598=CARTESIAN_POINT('Ctrl Pts',(-10.5849844800001,15.2,-1.90744124500001));
#266599=CARTESIAN_POINT('Ctrl Pts',(-10.5849844800001,11.6,-1.90744124500001));
#266600=CARTESIAN_POINT('Ctrl Pts',(-10.5872694410001,15.2,-1.90856966700002));
#266601=CARTESIAN_POINT('Ctrl Pts',(-10.5872694410001,11.6,-1.90856966700002));
#266602=CARTESIAN_POINT('Ctrl Pts',(-10.5895588790001,15.2,-1.90970273700001));
#266603=CARTESIAN_POINT('Ctrl Pts',(-10.5895588790001,11.6,-1.90970273700001));
#266604=CARTESIAN_POINT('Ctrl Pts',(-10.5918527800001,15.2,-1.91084046000002));
#266605=CARTESIAN_POINT('Ctrl Pts',(-10.5918527800001,11.6,-1.91084046000002));
#266606=CARTESIAN_POINT('Ctrl Pts',(-10.5941511290001,15.2,-1.91198283800002));
#266607=CARTESIAN_POINT('Ctrl Pts',(-10.5941511290001,11.6,-1.91198283800002));
#266608=CARTESIAN_POINT('Ctrl Pts',(-10.5964539110001,15.2,-1.91312987400002));
#266609=CARTESIAN_POINT('Ctrl Pts',(-10.5964539110001,11.6,-1.91312987400002));
#266610=CARTESIAN_POINT('Ctrl Pts',(-10.5987611120001,15.2,-1.91428157100002));
#266611=CARTESIAN_POINT('Ctrl Pts',(-10.5987611120001,11.6,-1.91428157100002));
#266612=CARTESIAN_POINT('Ctrl Pts',(-10.6010727180001,15.2,-1.91543793200001));
#266613=CARTESIAN_POINT('Ctrl Pts',(-10.6010727180001,11.6,-1.91543793200002));
#266614=CARTESIAN_POINT('Ctrl Pts',(-10.6033887130001,15.2,-1.91659895900001));
#266615=CARTESIAN_POINT('Ctrl Pts',(-10.6033887130001,11.6,-1.91659895900001));
#266616=CARTESIAN_POINT('Ctrl Pts',(-10.6057090860001,15.2,-1.91776465800002));
#266617=CARTESIAN_POINT('Ctrl Pts',(-10.6057090860001,11.6,-1.91776465800002));
#266618=CARTESIAN_POINT('Ctrl Pts',(-10.6080338200001,15.2,-1.91893502800002));
#266619=CARTESIAN_POINT('Ctrl Pts',(-10.6080338200001,11.6,-1.91893502800002));
#266620=CARTESIAN_POINT('Ctrl Pts',(-10.6103629020001,15.2,-1.92011007300001));
#266621=CARTESIAN_POINT('Ctrl Pts',(-10.6103629020001,11.6,-1.92011007300001));
#266622=CARTESIAN_POINT('Ctrl Pts',(-10.6126963170001,15.2,-1.92128979600001));
#266623=CARTESIAN_POINT('Ctrl Pts',(-10.6126963170001,11.6,-1.92128979600001));
#266624=CARTESIAN_POINT('Ctrl Pts',(-10.6150340510001,15.2,-1.92247420100002));
#266625=CARTESIAN_POINT('Ctrl Pts',(-10.6150340510001,11.6,-1.92247420100002));
#266626=CARTESIAN_POINT('Ctrl Pts',(-10.6173760910001,15.2,-1.92366329000001));
#266627=CARTESIAN_POINT('Ctrl Pts',(-10.6173760910001,11.6,-1.92366329000001));
#266628=CARTESIAN_POINT('Ctrl Pts',(-10.6197224210001,15.2,-1.92485706400001));
#266629=CARTESIAN_POINT('Ctrl Pts',(-10.6197224210001,11.6,-1.92485706400001));
#266630=CARTESIAN_POINT('Ctrl Pts',(-10.6220730290001,15.2,-1.92605552900002));
#266631=CARTESIAN_POINT('Ctrl Pts',(-10.6220730290001,11.6,-1.92605552900002));
#266632=CARTESIAN_POINT('Ctrl Pts',(-10.6244279010001,15.2,-1.92725868500002));
#266633=CARTESIAN_POINT('Ctrl Pts',(-10.6244279010001,11.6,-1.92725868500002));
#266634=CARTESIAN_POINT('Ctrl Pts',(-10.6267870210001,15.2,-1.92846653600002));
#266635=CARTESIAN_POINT('Ctrl Pts',(-10.6267870210001,11.6,-1.92846653600002));
#266636=CARTESIAN_POINT('Ctrl Pts',(-10.6291503760001,15.2,-1.92967908500002));
#266637=CARTESIAN_POINT('Ctrl Pts',(-10.6291503760001,11.6,-1.92967908500002));
#266638=CARTESIAN_POINT('Ctrl Pts',(-10.6315179530001,15.2,-1.93089633400001));
#266639=CARTESIAN_POINT('Ctrl Pts',(-10.6315179530001,11.6,-1.93089633400001));
#266640=CARTESIAN_POINT('Ctrl Pts',(-10.6338897380001,15.2,-1.93211828500001));
#266641=CARTESIAN_POINT('Ctrl Pts',(-10.6338897380001,11.6,-1.93211828500001));
#266642=CARTESIAN_POINT('Ctrl Pts',(-10.6362657160001,15.2,-1.93334494300001));
#266643=CARTESIAN_POINT('Ctrl Pts',(-10.6362657160001,11.6,-1.93334494300002));
#266644=CARTESIAN_POINT('Ctrl Pts',(-10.6386458730001,15.2,-1.93457630700001));
#266645=CARTESIAN_POINT('Ctrl Pts',(-10.6386458730001,11.6,-1.93457630700001));
#266646=CARTESIAN_POINT('Ctrl Pts',(-10.6410301980001,15.2,-1.93581238300002));
#266647=CARTESIAN_POINT('Ctrl Pts',(-10.6410301980001,11.6,-1.93581238300002));
#266648=CARTESIAN_POINT('Ctrl Pts',(-10.6434186740001,15.2,-1.93705317200001));
#266649=CARTESIAN_POINT('Ctrl Pts',(-10.6434186740001,11.6,-1.93705317200001));
#266650=CARTESIAN_POINT('Ctrl Pts',(-10.6458112890001,15.2,-1.93829867700002));
#266651=CARTESIAN_POINT('Ctrl Pts',(-10.6458112890001,11.6,-1.93829867700002));
#266652=CARTESIAN_POINT('Ctrl Pts',(-10.6482080300001,15.2,-1.93954890100001));
#266653=CARTESIAN_POINT('Ctrl Pts',(-10.6482080300001,11.6,-1.93954890100001));
#266654=CARTESIAN_POINT('Ctrl Pts',(-10.6506088810001,15.2,-1.94080384500001));
#266655=CARTESIAN_POINT('Ctrl Pts',(-10.6506088810001,11.6,-1.94080384500001));
#266656=CARTESIAN_POINT('Ctrl Pts',(-10.6530138300001,15.2,-1.94206351200001));
#266657=CARTESIAN_POINT('Ctrl Pts',(-10.6530138300001,11.6,-1.94206351200001));
#266658=CARTESIAN_POINT('Ctrl Pts',(-10.6554228640001,15.2,-1.94332790700001));
#266659=CARTESIAN_POINT('Ctrl Pts',(-10.6554228640001,11.6,-1.94332790700001));
#266660=CARTESIAN_POINT('Ctrl Pts',(-10.6578359690001,15.2,-1.94459703000001));
#266661=CARTESIAN_POINT('Ctrl Pts',(-10.6578359690001,11.6,-1.94459703000002));
#266662=CARTESIAN_POINT('Ctrl Pts',(-10.6602531300001,15.2,-1.94587088200001));
#266663=CARTESIAN_POINT('Ctrl Pts',(-10.6602531300001,11.6,-1.94587088200001));
#266664=CARTESIAN_POINT('Ctrl Pts',(-10.6626743350001,15.2,-1.94714946900001));
#266665=CARTESIAN_POINT('Ctrl Pts',(-10.6626743350001,11.6,-1.94714946900001));
#266666=CARTESIAN_POINT('Ctrl Pts',(-10.6650995710001,15.2,-1.94843279300001));
#266667=CARTESIAN_POINT('Ctrl Pts',(-10.6650995710001,11.6,-1.94843279300001));
#266668=CARTESIAN_POINT('Ctrl Pts',(-10.6675288230001,15.2,-1.94972085400002));
#266669=CARTESIAN_POINT('Ctrl Pts',(-10.6675288230001,11.6,-1.94972085400002));
#266670=CARTESIAN_POINT('Ctrl Pts',(-10.6699620800001,15.2,-1.95101365600001));
#266671=CARTESIAN_POINT('Ctrl Pts',(-10.6699620800001,11.6,-1.95101365600001));
#266672=CARTESIAN_POINT('Ctrl Pts',(-10.6723993270001,15.2,-1.95231120100001));
#266673=CARTESIAN_POINT('Ctrl Pts',(-10.6723993270001,11.6,-1.95231120100001));
#266674=CARTESIAN_POINT('Ctrl Pts',(-10.6748405500001,15.2,-1.95361349100001));
#266675=CARTESIAN_POINT('Ctrl Pts',(-10.6748405500001,11.6,-1.95361349100002));
#266676=CARTESIAN_POINT('Ctrl Pts',(-10.6772857370001,15.2,-1.95492053000001));
#266677=CARTESIAN_POINT('Ctrl Pts',(-10.6772857370001,11.6,-1.95492053000002));
#266678=CARTESIAN_POINT('Ctrl Pts',(-10.6797348740001,15.2,-1.95623231900001));
#266679=CARTESIAN_POINT('Ctrl Pts',(-10.6797348740001,11.6,-1.95623231900001));
#266680=CARTESIAN_POINT('Ctrl Pts',(-10.6821879490001,15.2,-1.95754886000001));
#266681=CARTESIAN_POINT('Ctrl Pts',(-10.6821879490001,11.6,-1.95754886000001));
#266682=CARTESIAN_POINT('Ctrl Pts',(-10.6846449480001,15.2,-1.95887015700002));
#266683=CARTESIAN_POINT('Ctrl Pts',(-10.6846449480001,11.6,-1.95887015700002));
#266684=CARTESIAN_POINT('Ctrl Pts',(-10.6871058570001,15.2,-1.96019621100001));
#266685=CARTESIAN_POINT('Ctrl Pts',(-10.6871058570001,11.6,-1.96019621100001));
#266686=CARTESIAN_POINT('Ctrl Pts',(-10.6895706640001,15.2,-1.96152702300001));
#266687=CARTESIAN_POINT('Ctrl Pts',(-10.6895706640001,11.6,-1.96152702300001));
#266688=CARTESIAN_POINT('Ctrl Pts',(-10.6920393560001,15.2,-1.96286259900001));
#266689=CARTESIAN_POINT('Ctrl Pts',(-10.6920393560001,11.6,-1.96286259900001));
#266690=CARTESIAN_POINT('Ctrl Pts',(-10.6945119200001,15.2,-1.96420293800001));
#266691=CARTESIAN_POINT('Ctrl Pts',(-10.6945119200001,11.6,-1.96420293800002));
#266692=CARTESIAN_POINT('Ctrl Pts',(-10.6969883420001,15.2,-1.96554804400002));
#266693=CARTESIAN_POINT('Ctrl Pts',(-10.6969883420001,11.6,-1.96554804400002));
#266694=CARTESIAN_POINT('Ctrl Pts',(-10.6994686090001,15.2,-1.96689791700001));
#266695=CARTESIAN_POINT('Ctrl Pts',(-10.6994686090001,11.6,-1.96689791700001));
#266696=CARTESIAN_POINT('Ctrl Pts',(-10.7019527100001,15.2,-1.96825256300002));
#266697=CARTESIAN_POINT('Ctrl Pts',(-10.7019527100001,11.6,-1.96825256300002));
#266698=CARTESIAN_POINT('Ctrl Pts',(-10.7044406300001,15.2,-1.96961198000002));
#266699=CARTESIAN_POINT('Ctrl Pts',(-10.7044406300001,11.6,-1.96961198000002));
#266700=CARTESIAN_POINT('Ctrl Pts',(-10.7069323560001,15.2,-1.97097617300001));
#266701=CARTESIAN_POINT('Ctrl Pts',(-10.7069323560001,11.6,-1.97097617300001));
#266702=CARTESIAN_POINT('Ctrl Pts',(-10.7094278770001,15.2,-1.97234514300002));
#266703=CARTESIAN_POINT('Ctrl Pts',(-10.7094278770001,11.6,-1.97234514300002));
#266704=CARTESIAN_POINT('Ctrl Pts',(-10.7119271780001,15.2,-1.97371889300001));
#266705=CARTESIAN_POINT('Ctrl Pts',(-10.7119271780001,11.6,-1.97371889300001));
#266706=CARTESIAN_POINT('Ctrl Pts',(-10.7144302480001,15.2,-1.97509742500001));
#266707=CARTESIAN_POINT('Ctrl Pts',(-10.7144302480001,11.6,-1.97509742500001));
#266708=CARTESIAN_POINT('Ctrl Pts',(-10.7169370730001,15.2,-1.97648074000002));
#266709=CARTESIAN_POINT('Ctrl Pts',(-10.7169370730001,11.6,-1.97648074000002));
#266710=CARTESIAN_POINT('Ctrl Pts',(-10.7194476400001,15.2,-1.97786884100001));
#266711=CARTESIAN_POINT('Ctrl Pts',(-10.7194476400001,11.6,-1.97786884100001));
#266712=CARTESIAN_POINT('Ctrl Pts',(-10.7219619380001,15.2,-1.97926173000001));
#266713=CARTESIAN_POINT('Ctrl Pts',(-10.7219619380001,11.6,-1.97926173000001));
#266714=CARTESIAN_POINT('Ctrl Pts',(-10.7244799520001,15.2,-1.98065940900001));
#266715=CARTESIAN_POINT('Ctrl Pts',(-10.7244799520001,11.6,-1.98065940900001));
#266716=CARTESIAN_POINT('Ctrl Pts',(-10.7270016720001,15.2,-1.98206188000002));
#266717=CARTESIAN_POINT('Ctrl Pts',(-10.7270016720001,11.6,-1.98206188000002));
#266718=CARTESIAN_POINT('Ctrl Pts',(-10.7295270830001,15.2,-1.98346914600001));
#266719=CARTESIAN_POINT('Ctrl Pts',(-10.7295270830001,11.6,-1.98346914600001));
#266720=CARTESIAN_POINT('Ctrl Pts',(-10.7320561730001,15.2,-1.98488120800001));
#266721=CARTESIAN_POINT('Ctrl Pts',(-10.7320561730001,11.6,-1.98488120800001));
#266722=CARTESIAN_POINT('Ctrl Pts',(-10.7345889310001,15.2,-1.98629806800001));
#266723=CARTESIAN_POINT('Ctrl Pts',(-10.7345889310001,11.6,-1.98629806800001));
#266724=CARTESIAN_POINT('Ctrl Pts',(-10.7371253410001,15.2,-1.98771972800001));
#266725=CARTESIAN_POINT('Ctrl Pts',(-10.7371253410001,11.6,-1.98771972800001));
#266726=CARTESIAN_POINT('Ctrl Pts',(-10.7396653940001,15.2,-1.98914619100002));
#266727=CARTESIAN_POINT('Ctrl Pts',(-10.7396653940001,11.6,-1.98914619100002));
#266728=CARTESIAN_POINT('Ctrl Pts',(-10.7422090760001,15.2,-1.99057745700001));
#266729=CARTESIAN_POINT('Ctrl Pts',(-10.7422090760001,11.6,-1.99057745700001));
#266730=CARTESIAN_POINT('Ctrl Pts',(-10.7447563740001,15.2,-1.99201353000001));
#266731=CARTESIAN_POINT('Ctrl Pts',(-10.7447563740001,11.6,-1.99201353000001));
#266732=CARTESIAN_POINT('Ctrl Pts',(-10.7473072760001,15.2,-1.99345441100002));
#266733=CARTESIAN_POINT('Ctrl Pts',(-10.7473072760001,11.6,-1.99345441100002));
#266734=CARTESIAN_POINT('Ctrl Pts',(-10.7498617710001,15.2,-1.99490010200002));
#266735=CARTESIAN_POINT('Ctrl Pts',(-10.7498617710001,11.6,-1.99490010200002));
#266736=CARTESIAN_POINT('Ctrl Pts',(-10.7524198440001,15.2,-1.99635060600002));
#266737=CARTESIAN_POINT('Ctrl Pts',(-10.7524198440001,11.6,-1.99635060600002));
#266738=CARTESIAN_POINT('Ctrl Pts',(-10.7549814840001,15.2,-1.99780592200002));
#266739=CARTESIAN_POINT('Ctrl Pts',(-10.7549814840001,11.6,-1.99780592200002));
#266740=CARTESIAN_POINT('Ctrl Pts',(-10.7575466780001,15.2,-1.99926605500002));
#266741=CARTESIAN_POINT('Ctrl Pts',(-10.7575466780001,11.6,-1.99926605500002));
#266742=CARTESIAN_POINT('Ctrl Pts',(-10.7601154160001,15.2,-2.00073100600001));
#266743=CARTESIAN_POINT('Ctrl Pts',(-10.7601154160001,11.6,-2.00073100600001));
#266744=CARTESIAN_POINT('Ctrl Pts',(-10.7626876820001,15.2,-2.00220077700001));
#266745=CARTESIAN_POINT('Ctrl Pts',(-10.7626876820001,11.6,-2.00220077700001));
#266746=CARTESIAN_POINT('Ctrl Pts',(-10.7652634670001,15.2,-2.00367536800002));
#266747=CARTESIAN_POINT('Ctrl Pts',(-10.7652634670001,11.6,-2.00367536800002));
#266748=CARTESIAN_POINT('Ctrl Pts',(-10.7678427560001,15.2,-2.00515478300002));
#266749=CARTESIAN_POINT('Ctrl Pts',(-10.7678427560001,11.6,-2.00515478300002));
#266750=CARTESIAN_POINT('Ctrl Pts',(-10.7704255400001,15.2,-2.00663902300001));
#266751=CARTESIAN_POINT('Ctrl Pts',(-10.7704255400001,11.6,-2.00663902300001));
#266752=CARTESIAN_POINT('Ctrl Pts',(-10.7730118040001,15.2,-2.00812809000002));
#266753=CARTESIAN_POINT('Ctrl Pts',(-10.7730118040001,11.6,-2.00812809000002));
#266754=CARTESIAN_POINT('Ctrl Pts',(-10.7756015380001,15.2,-2.00962198600001));
#266755=CARTESIAN_POINT('Ctrl Pts',(-10.7756015380001,11.6,-2.00962198600001));
#266756=CARTESIAN_POINT('Ctrl Pts',(-10.7781947270001,15.2,-2.01112071200001));
#266757=CARTESIAN_POINT('Ctrl Pts',(-10.7781947270001,11.6,-2.01112071200001));
#266758=CARTESIAN_POINT('Ctrl Pts',(-10.7807913610001,15.2,-2.01262427100001));
#266759=CARTESIAN_POINT('Ctrl Pts',(-10.7807913610001,11.6,-2.01262427100001));
#266760=CARTESIAN_POINT('Ctrl Pts',(-10.7833914290001,15.2,-2.01413266400001));
#266761=CARTESIAN_POINT('Ctrl Pts',(-10.7833914290001,11.6,-2.01413266400001));
#266762=CARTESIAN_POINT('Ctrl Pts',(-10.7859949160001,15.2,-2.01564589300002));
#266763=CARTESIAN_POINT('Ctrl Pts',(-10.7859949160001,11.6,-2.01564589300002));
#266764=CARTESIAN_POINT('Ctrl Pts',(-10.7886018120001,15.2,-2.01716395900001));
#266765=CARTESIAN_POINT('Ctrl Pts',(-10.7886018120001,11.6,-2.01716395900001));
#266766=CARTESIAN_POINT('Ctrl Pts',(-10.7912121050001,15.2,-2.01868686500001));
#266767=CARTESIAN_POINT('Ctrl Pts',(-10.7912121050001,11.6,-2.01868686500001));
#266768=CARTESIAN_POINT('Ctrl Pts',(-10.7938257820001,15.2,-2.02021461100002));
#266769=CARTESIAN_POINT('Ctrl Pts',(-10.7938257820001,11.6,-2.02021461100002));
#266770=CARTESIAN_POINT('Ctrl Pts',(-10.7964428320001,15.2,-2.02174720000002));
#266771=CARTESIAN_POINT('Ctrl Pts',(-10.7964428320001,11.6,-2.02174720000002));
#266772=CARTESIAN_POINT('Ctrl Pts',(-10.7990632420001,15.2,-2.02328463400002));
#266773=CARTESIAN_POINT('Ctrl Pts',(-10.7990632420001,11.6,-2.02328463400002));
#266774=CARTESIAN_POINT('Ctrl Pts',(-10.8016870010001,15.2,-2.02482691400002));
#266775=CARTESIAN_POINT('Ctrl Pts',(-10.8016870010001,11.6,-2.02482691400002));
#266776=CARTESIAN_POINT('Ctrl Pts',(-10.8043140960001,15.2,-2.02637404200001));
#266777=CARTESIAN_POINT('Ctrl Pts',(-10.8043140960001,11.6,-2.02637404200001));
#266778=CARTESIAN_POINT('Ctrl Pts',(-10.8069445180001,15.2,-2.02792601900001));
#266779=CARTESIAN_POINT('Ctrl Pts',(-10.8069445180001,11.6,-2.02792601900002));
#266780=CARTESIAN_POINT('Ctrl Pts',(-10.8095782520001,15.2,-2.02948284700001));
#266781=CARTESIAN_POINT('Ctrl Pts',(-10.8095782520001,11.6,-2.02948284700002));
#266782=CARTESIAN_POINT('Ctrl Pts',(-10.8122152870001,15.2,-2.03104452700002));
#266783=CARTESIAN_POINT('Ctrl Pts',(-10.8122152870001,11.6,-2.03104452700002));
#266784=CARTESIAN_POINT('Ctrl Pts',(-10.8148556120001,15.2,-2.03261106200001));
#266785=CARTESIAN_POINT('Ctrl Pts',(-10.8148556120001,11.6,-2.03261106200001));
#266786=CARTESIAN_POINT('Ctrl Pts',(-10.8174992140001,15.2,-2.03418245300002));
#266787=CARTESIAN_POINT('Ctrl Pts',(-10.8174992140001,11.6,-2.03418245300002));
#266788=CARTESIAN_POINT('Ctrl Pts',(-10.8201460830001,15.2,-2.03575870100002));
#266789=CARTESIAN_POINT('Ctrl Pts',(-10.8201460830001,11.6,-2.03575870100002));
#266790=CARTESIAN_POINT('Ctrl Pts',(-10.8227962070001,15.2,-2.03733980800001));
#266791=CARTESIAN_POINT('Ctrl Pts',(-10.8227962070001,11.6,-2.03733980800001));
#266792=CARTESIAN_POINT('Ctrl Pts',(-10.8254495730001,15.2,-2.03892577600001));
#266793=CARTESIAN_POINT('Ctrl Pts',(-10.8254495730001,11.6,-2.03892577600001));
#266794=CARTESIAN_POINT('Ctrl Pts',(-10.8281061700001,15.2,-2.04051660600001));
#266795=CARTESIAN_POINT('Ctrl Pts',(-10.8281061700001,11.6,-2.04051660600001));
#266796=CARTESIAN_POINT('Ctrl Pts',(-10.8307659860001,15.2,-2.04211229900002));
#266797=CARTESIAN_POINT('Ctrl Pts',(-10.8307659860001,11.6,-2.04211229900002));
#266798=CARTESIAN_POINT('Ctrl Pts',(-10.8334290110001,15.2,-2.04371285800002));
#266799=CARTESIAN_POINT('Ctrl Pts',(-10.8334290110001,11.6,-2.04371285800002));
#266800=CARTESIAN_POINT('Ctrl Pts',(-10.8360952310001,15.2,-2.04531828300002));
#266801=CARTESIAN_POINT('Ctrl Pts',(-10.8360952310001,11.6,-2.04531828300002));
#266802=CARTESIAN_POINT('Ctrl Pts',(-10.8387646370001,15.2,-2.04692857600001));
#266803=CARTESIAN_POINT('Ctrl Pts',(-10.8387646370001,11.6,-2.04692857600001));
#266804=CARTESIAN_POINT('Ctrl Pts',(-10.8414372150001,15.2,-2.04854373900002));
#266805=CARTESIAN_POINT('Ctrl Pts',(-10.8414372150001,11.6,-2.04854373900002));
#266806=CARTESIAN_POINT('Ctrl Pts',(-10.8441129560001,15.2,-2.05016377300002));
#266807=CARTESIAN_POINT('Ctrl Pts',(-10.8441129560001,11.6,-2.05016377300002));
#266808=CARTESIAN_POINT('Ctrl Pts',(-10.8467918470001,15.2,-2.05178868100001));
#266809=CARTESIAN_POINT('Ctrl Pts',(-10.8467918470001,11.6,-2.05178868100001));
#266810=CARTESIAN_POINT('Ctrl Pts',(-10.8494738750001,15.2,-2.05341846100001));
#266811=CARTESIAN_POINT('Ctrl Pts',(-10.8494738750001,11.6,-2.05341846100001));
#266812=CARTESIAN_POINT('Ctrl Pts',(-10.8521590310001,15.2,-2.05505311700001));
#266813=CARTESIAN_POINT('Ctrl Pts',(-10.8521590310001,11.6,-2.05505311700001));
#266814=CARTESIAN_POINT('Ctrl Pts',(-10.8548473040001,15.2,-2.05669265100001));
#266815=CARTESIAN_POINT('Ctrl Pts',(-10.8548473040001,11.6,-2.05669265100001));
#266816=CARTESIAN_POINT('Ctrl Pts',(-10.8575386810001,15.2,-2.05833706200002));
#266817=CARTESIAN_POINT('Ctrl Pts',(-10.8575386810001,11.6,-2.05833706200002));
#266818=CARTESIAN_POINT('Ctrl Pts',(-10.8602331500001,15.2,-2.05998635300002));
#266819=CARTESIAN_POINT('Ctrl Pts',(-10.8602331500001,11.6,-2.05998635300002));
#266820=CARTESIAN_POINT('Ctrl Pts',(-10.8629307020001,15.2,-2.06164052600001));
#266821=CARTESIAN_POINT('Ctrl Pts',(-10.8629307020001,11.6,-2.06164052600002));
#266822=CARTESIAN_POINT('Ctrl Pts',(-10.8656313230001,15.2,-2.06329958000001));
#266823=CARTESIAN_POINT('Ctrl Pts',(-10.8656313230001,11.6,-2.06329958000001));
#266824=CARTESIAN_POINT('Ctrl Pts',(-10.8683350050001,15.2,-2.06496352000002));
#266825=CARTESIAN_POINT('Ctrl Pts',(-10.8683350050001,11.6,-2.06496352000002));
#266826=CARTESIAN_POINT('Ctrl Pts',(-10.8710417330001,15.2,-2.06663234400001));
#266827=CARTESIAN_POINT('Ctrl Pts',(-10.8710417330001,11.6,-2.06663234400001));
#266828=CARTESIAN_POINT('Ctrl Pts',(-10.8737514990001,15.2,-2.06830605400001));
#266829=CARTESIAN_POINT('Ctrl Pts',(-10.8737514990001,11.6,-2.06830605400001));
#266830=CARTESIAN_POINT('Ctrl Pts',(-10.8764642900001,15.2,-2.06998465200002));
#266831=CARTESIAN_POINT('Ctrl Pts',(-10.8764642900001,11.6,-2.06998465200002));
#266832=CARTESIAN_POINT('Ctrl Pts',(-10.8791800940001,15.2,-2.07166814000002));
#266833=CARTESIAN_POINT('Ctrl Pts',(-10.8791800940001,11.6,-2.07166814000002));
#266834=CARTESIAN_POINT('Ctrl Pts',(-10.8818989020001,15.2,-2.07335651800001));
#266835=CARTESIAN_POINT('Ctrl Pts',(-10.8818989020001,11.6,-2.07335651800001));
#266836=CARTESIAN_POINT('Ctrl Pts',(-10.8846207020001,15.2,-2.07504978700001));
#266837=CARTESIAN_POINT('Ctrl Pts',(-10.8846207020001,11.6,-2.07504978700001));
#266838=CARTESIAN_POINT('Ctrl Pts',(-10.8873454820001,15.2,-2.07674795000001));
#266839=CARTESIAN_POINT('Ctrl Pts',(-10.8873454820001,11.6,-2.07674795000001));
#266840=CARTESIAN_POINT('Ctrl Pts',(-10.8900732320001,15.2,-2.07845100700002));
#266841=CARTESIAN_POINT('Ctrl Pts',(-10.8900732320001,11.6,-2.07845100700002));
#266842=CARTESIAN_POINT('Ctrl Pts',(-10.8928039400001,15.2,-2.08015896100001));
#266843=CARTESIAN_POINT('Ctrl Pts',(-10.8928039400001,11.6,-2.08015896100001));
#266844=CARTESIAN_POINT('Ctrl Pts',(-10.8955375960001,15.2,-2.08187181000001));
#266845=CARTESIAN_POINT('Ctrl Pts',(-10.8955375960001,11.6,-2.08187181000001));
#266846=CARTESIAN_POINT('Ctrl Pts',(-10.8982741870001,15.2,-2.08358955900001));
#266847=CARTESIAN_POINT('Ctrl Pts',(-10.8982741870001,11.6,-2.08358955900001));
#266848=CARTESIAN_POINT('Ctrl Pts',(-10.9010137040001,15.2,-2.08531220500001));
#266849=CARTESIAN_POINT('Ctrl Pts',(-10.9010137040001,11.6,-2.08531220500001));
#266850=CARTESIAN_POINT('Ctrl Pts',(-10.9037561350001,15.2,-2.08703975300002));
#266851=CARTESIAN_POINT('Ctrl Pts',(-10.9037561350001,11.6,-2.08703975300002));
#266852=CARTESIAN_POINT('Ctrl Pts',(-10.9065014700001,15.2,-2.08877220300002));
#266853=CARTESIAN_POINT('Ctrl Pts',(-10.9065014700001,11.6,-2.08877220300002));
#266854=CARTESIAN_POINT('Ctrl Pts',(-10.9092496960001,15.2,-2.09050955500001));
#266855=CARTESIAN_POINT('Ctrl Pts',(-10.9092496960001,11.6,-2.09050955500001));
#266856=CARTESIAN_POINT('Ctrl Pts',(-10.9120008040001,15.2,-2.09225181200001));
#266857=CARTESIAN_POINT('Ctrl Pts',(-10.9120008040001,11.6,-2.09225181200001));
#266858=CARTESIAN_POINT('Ctrl Pts',(-10.9147547830001,15.2,-2.09399897400001));
#266859=CARTESIAN_POINT('Ctrl Pts',(-10.9147547830001,11.6,-2.09399897400001));
#266860=CARTESIAN_POINT('Ctrl Pts',(-10.9175116210001,15.2,-2.09575104200002));
#266861=CARTESIAN_POINT('Ctrl Pts',(-10.9175116210001,11.6,-2.09575104200002));
#266862=CARTESIAN_POINT('Ctrl Pts',(-10.9202713070001,15.2,-2.09750801800002));
#266863=CARTESIAN_POINT('Ctrl Pts',(-10.9202713070001,11.6,-2.09750801800002));
#266864=CARTESIAN_POINT('Ctrl Pts',(-10.9230338300001,15.2,-2.09926990300001));
#266865=CARTESIAN_POINT('Ctrl Pts',(-10.9230338300001,11.6,-2.09926990300001));
#266866=CARTESIAN_POINT('Ctrl Pts',(-10.9257991820001,15.2,-2.10103669800001));
#266867=CARTESIAN_POINT('Ctrl Pts',(-10.9257991820001,11.6,-2.10103669800001));
#266868=CARTESIAN_POINT('Ctrl Pts',(-10.9285673490001,15.2,-2.10280840300001));
#266869=CARTESIAN_POINT('Ctrl Pts',(-10.9285673490001,11.6,-2.10280840300001));
#266870=CARTESIAN_POINT('Ctrl Pts',(-10.9313383210001,15.2,-2.10458502100002));
#266871=CARTESIAN_POINT('Ctrl Pts',(-10.9313383210001,11.6,-2.10458502100002));
#266872=CARTESIAN_POINT('Ctrl Pts',(-10.9341120880001,15.2,-2.10636655200001));
#266873=CARTESIAN_POINT('Ctrl Pts',(-10.9341120880001,11.6,-2.10636655200001));
#266874=CARTESIAN_POINT('Ctrl Pts',(-10.9368886390001,15.2,-2.10815299600001));
#266875=CARTESIAN_POINT('Ctrl Pts',(-10.9368886390001,11.6,-2.10815299600001));
#266876=CARTESIAN_POINT('Ctrl Pts',(-10.9396679630001,15.2,-2.10994435800002));
#266877=CARTESIAN_POINT('Ctrl Pts',(-10.9396679630001,11.6,-2.10994435800002));
#266878=CARTESIAN_POINT('Ctrl Pts',(-10.9424500480001,15.2,-2.11174063500001));
#266879=CARTESIAN_POINT('Ctrl Pts',(-10.9424500480001,11.6,-2.11174063500001));
#266880=CARTESIAN_POINT('Ctrl Pts',(-10.9452348850001,15.2,-2.11354182900001));
#266881=CARTESIAN_POINT('Ctrl Pts',(-10.9452348850001,11.6,-2.11354182900001));
#266882=CARTESIAN_POINT('Ctrl Pts',(-10.9480224640001,15.2,-2.11534794200002));
#266883=CARTESIAN_POINT('Ctrl Pts',(-10.9480224640001,11.6,-2.11534794200002));
#266884=CARTESIAN_POINT('Ctrl Pts',(-10.9508127730001,15.2,-2.11715897500001));
#266885=CARTESIAN_POINT('Ctrl Pts',(-10.9508127730001,11.6,-2.11715897500001));
#266886=CARTESIAN_POINT('Ctrl Pts',(-10.9536058010001,15.2,-2.11897492800002));
#266887=CARTESIAN_POINT('Ctrl Pts',(-10.9536058010001,11.6,-2.11897492800002));
#266888=CARTESIAN_POINT('Ctrl Pts',(-10.9564015380001,15.2,-2.12079580400002));
#266889=CARTESIAN_POINT('Ctrl Pts',(-10.9564015380001,11.6,-2.12079580400002));
#266890=CARTESIAN_POINT('Ctrl Pts',(-10.9591999740001,15.2,-2.12262160100002));
#266891=CARTESIAN_POINT('Ctrl Pts',(-10.9591999740001,11.6,-2.12262160100002));
#266892=CARTESIAN_POINT('Ctrl Pts',(-10.9620010970001,15.2,-2.12445232200002));
#266893=CARTESIAN_POINT('Ctrl Pts',(-10.9620010970001,11.6,-2.12445232200002));
#266894=CARTESIAN_POINT('Ctrl Pts',(-10.9648048980001,15.2,-2.12628796700002));
#266895=CARTESIAN_POINT('Ctrl Pts',(-10.9648048980001,11.6,-2.12628796700002));
#266896=CARTESIAN_POINT('Ctrl Pts',(-10.9676113650001,15.2,-2.12812853800001));
#266897=CARTESIAN_POINT('Ctrl Pts',(-10.9676113650001,11.6,-2.12812853800001));
#266898=CARTESIAN_POINT('Ctrl Pts',(-10.9704204880001,15.2,-2.12997403600002));
#266899=CARTESIAN_POINT('Ctrl Pts',(-10.9704204880001,11.6,-2.12997403600002));
#266900=CARTESIAN_POINT('Ctrl Pts',(-10.9732322570001,15.2,-2.13182446100001));
#266901=CARTESIAN_POINT('Ctrl Pts',(-10.9732322570001,11.6,-2.13182446100001));
#266902=CARTESIAN_POINT('Ctrl Pts',(-10.9760466620001,15.2,-2.13367981500001));
#266903=CARTESIAN_POINT('Ctrl Pts',(-10.9760466620001,11.6,-2.13367981500001));
#266904=CARTESIAN_POINT('Ctrl Pts',(-10.9788636920001,15.2,-2.13554009700001));
#266905=CARTESIAN_POINT('Ctrl Pts',(-10.9788636920001,11.6,-2.13554009700002));
#266906=CARTESIAN_POINT('Ctrl Pts',(-10.9816833350001,15.2,-2.13740531000001));
#266907=CARTESIAN_POINT('Ctrl Pts',(-10.9816833350001,11.6,-2.13740531000001));
#266908=CARTESIAN_POINT('Ctrl Pts',(-10.9845055830001,15.2,-2.13927545500002));
#266909=CARTESIAN_POINT('Ctrl Pts',(-10.9845055830001,11.6,-2.13927545500002));
#266910=CARTESIAN_POINT('Ctrl Pts',(-10.9873304240001,15.2,-2.14115053100001));
#266911=CARTESIAN_POINT('Ctrl Pts',(-10.9873304240001,11.6,-2.14115053100001));
#266912=CARTESIAN_POINT('Ctrl Pts',(-10.9901578480001,15.2,-2.14303054100001));
#266913=CARTESIAN_POINT('Ctrl Pts',(-10.9901578480001,11.6,-2.14303054100002));
#266914=CARTESIAN_POINT('Ctrl Pts',(-10.9929878450001,15.2,-2.14491548300002));
#266915=CARTESIAN_POINT('Ctrl Pts',(-10.9929878450001,11.6,-2.14491548300002));
#266916=CARTESIAN_POINT('Ctrl Pts',(-10.9958204050001,15.2,-2.14680536000001));
#266917=CARTESIAN_POINT('Ctrl Pts',(-10.9958204050001,11.6,-2.14680536000001));
#266918=CARTESIAN_POINT('Ctrl Pts',(-10.9986555170001,15.2,-2.14870017400001));
#266919=CARTESIAN_POINT('Ctrl Pts',(-10.9986555170001,11.6,-2.14870017400001));
#266920=CARTESIAN_POINT('Ctrl Pts',(-11.0014931700001,15.2,-2.15059992300001));
#266921=CARTESIAN_POINT('Ctrl Pts',(-11.0014931700001,11.6,-2.15059992300001));
#266922=CARTESIAN_POINT('Ctrl Pts',(-11.0043333550001,15.2,-2.15250461100001));
#266923=CARTESIAN_POINT('Ctrl Pts',(-11.0043333550001,11.6,-2.15250461100002));
#266924=CARTESIAN_POINT('Ctrl Pts',(-11.0071760610001,15.2,-2.15441423500002));
#266925=CARTESIAN_POINT('Ctrl Pts',(-11.0071760610001,11.6,-2.15441423500002));
#266926=CARTESIAN_POINT('Ctrl Pts',(-11.0100212790001,15.2,-2.15632879900001));
#266927=CARTESIAN_POINT('Ctrl Pts',(-11.0100212790001,11.6,-2.15632879900001));
#266928=CARTESIAN_POINT('Ctrl Pts',(-11.0128689970001,15.2,-2.15824830200001));
#266929=CARTESIAN_POINT('Ctrl Pts',(-11.0128689970001,11.6,-2.15824830200001));
#266930=CARTESIAN_POINT('Ctrl Pts',(-11.0157192050001,15.2,-2.16017274600001));
#266931=CARTESIAN_POINT('Ctrl Pts',(-11.0157192050001,11.6,-2.16017274600001));
#266932=CARTESIAN_POINT('Ctrl Pts',(-11.0185718950001,15.2,-2.16210213100001));
#266933=CARTESIAN_POINT('Ctrl Pts',(-11.0185718950001,11.6,-2.16210213100001));
#266934=CARTESIAN_POINT('Ctrl Pts',(-11.0214270540001,15.2,-2.16403645900002));
#266935=CARTESIAN_POINT('Ctrl Pts',(-11.0214270540001,11.6,-2.16403645900002));
#266936=CARTESIAN_POINT('Ctrl Pts',(-11.0242846730001,15.2,-2.16597572800001));
#266937=CARTESIAN_POINT('Ctrl Pts',(-11.0242846730001,11.6,-2.16597572800001));
#266938=CARTESIAN_POINT('Ctrl Pts',(-11.0271447430001,15.2,-2.16791994200001));
#266939=CARTESIAN_POINT('Ctrl Pts',(-11.0271447430001,11.6,-2.16791994200001));
#266940=CARTESIAN_POINT('Ctrl Pts',(-11.0300072520001,15.2,-2.16986910100001));
#266941=CARTESIAN_POINT('Ctrl Pts',(-11.0300072520001,11.6,-2.16986910100002));
#266942=CARTESIAN_POINT('Ctrl Pts',(-11.0328721920001,15.2,-2.17182320300001));
#266943=CARTESIAN_POINT('Ctrl Pts',(-11.0328721920001,11.6,-2.17182320300001));
#266944=CARTESIAN_POINT('Ctrl Pts',(-11.0357395510001,15.2,-2.17378225200001));
#266945=CARTESIAN_POINT('Ctrl Pts',(-11.0357395510001,11.6,-2.17378225200001));
#266946=CARTESIAN_POINT('Ctrl Pts',(-11.0386093190001,15.2,-2.17574624800001));
#266947=CARTESIAN_POINT('Ctrl Pts',(-11.0386093190001,11.6,-2.17574624800001));
#266948=CARTESIAN_POINT('Ctrl Pts',(-11.0414814870001,15.2,-2.17771519000001));
#266949=CARTESIAN_POINT('Ctrl Pts',(-11.0414814870001,11.6,-2.17771519000001));
#266950=CARTESIAN_POINT('Ctrl Pts',(-11.0443560440001,15.2,-2.17968908100001));
#266951=CARTESIAN_POINT('Ctrl Pts',(-11.0443560440001,11.6,-2.17968908100001));
#266952=CARTESIAN_POINT('Ctrl Pts',(-11.0472329810001,15.2,-2.18166792000002));
#266953=CARTESIAN_POINT('Ctrl Pts',(-11.0472329810001,11.6,-2.18166792000002));
#266954=CARTESIAN_POINT('Ctrl Pts',(-11.0501122880001,15.2,-2.18365170900002));
#266955=CARTESIAN_POINT('Ctrl Pts',(-11.0501122880001,11.6,-2.18365170900002));
#266956=CARTESIAN_POINT('Ctrl Pts',(-11.0529939540001,15.2,-2.18564044700001));
#266957=CARTESIAN_POINT('Ctrl Pts',(-11.0529939540001,11.6,-2.18564044700001));
#266958=CARTESIAN_POINT('Ctrl Pts',(-11.0558779690001,15.2,-2.18763413700001));
#266959=CARTESIAN_POINT('Ctrl Pts',(-11.0558779690001,11.6,-2.18763413700001));
#266960=CARTESIAN_POINT('Ctrl Pts',(-11.0587643250001,15.2,-2.18963277700002));
#266961=CARTESIAN_POINT('Ctrl Pts',(-11.0587643250001,11.6,-2.18963277700002));
#266962=CARTESIAN_POINT('Ctrl Pts',(-11.0616530110001,15.2,-2.19163636900001));
#266963=CARTESIAN_POINT('Ctrl Pts',(-11.0616530110001,11.6,-2.19163636900001));
#266964=CARTESIAN_POINT('Ctrl Pts',(-11.0645440160001,15.2,-2.19364491400002));
#266965=CARTESIAN_POINT('Ctrl Pts',(-11.0645440160001,11.6,-2.19364491400002));
#266966=CARTESIAN_POINT('Ctrl Pts',(-11.0674373310001,15.2,-2.19565841300001));
#266967=CARTESIAN_POINT('Ctrl Pts',(-11.0674373310001,11.6,-2.19565841300001));
#266968=CARTESIAN_POINT('Ctrl Pts',(-11.0703329460001,15.2,-2.19767686500001));
#266969=CARTESIAN_POINT('Ctrl Pts',(-11.0703329460001,11.6,-2.19767686500001));
#266970=CARTESIAN_POINT('Ctrl Pts',(-11.0732308520001,15.2,-2.19970027200001));
#266971=CARTESIAN_POINT('Ctrl Pts',(-11.0732308520001,11.6,-2.19970027200001));
#266972=CARTESIAN_POINT('Ctrl Pts',(-11.0761310380001,15.2,-2.20172863400002));
#266973=CARTESIAN_POINT('Ctrl Pts',(-11.0761310380001,11.6,-2.20172863400002));
#266974=CARTESIAN_POINT('Ctrl Pts',(-11.0790334940001,15.2,-2.20376195100001));
#266975=CARTESIAN_POINT('Ctrl Pts',(-11.0790334940001,11.6,-2.20376195100001));
#266976=CARTESIAN_POINT('Ctrl Pts',(-11.0819382120001,15.2,-2.20580022500001));
#266977=CARTESIAN_POINT('Ctrl Pts',(-11.0819382120001,11.6,-2.20580022500001));
#266978=CARTESIAN_POINT('Ctrl Pts',(-11.0848451810001,15.2,-2.20784345600002));
#266979=CARTESIAN_POINT('Ctrl Pts',(-11.0848451810001,11.6,-2.20784345600002));
#266980=CARTESIAN_POINT('Ctrl Pts',(-11.0877543900001,15.2,-2.20989164400001));
#266981=CARTESIAN_POINT('Ctrl Pts',(-11.0877543900001,11.6,-2.20989164400002));
#266982=CARTESIAN_POINT('Ctrl Pts',(-11.0906658320001,15.2,-2.21194478900001));
#266983=CARTESIAN_POINT('Ctrl Pts',(-11.0906658320001,11.6,-2.21194478900001));
#266984=CARTESIAN_POINT('Ctrl Pts',(-11.0935794960001,15.2,-2.21400289400002));
#266985=CARTESIAN_POINT('Ctrl Pts',(-11.0935794960001,11.6,-2.21400289400002));
#266986=CARTESIAN_POINT('Ctrl Pts',(-11.0964953710001,15.2,-2.21606595800001));
#266987=CARTESIAN_POINT('Ctrl Pts',(-11.0964953710001,11.6,-2.21606595800001));
#266988=CARTESIAN_POINT('Ctrl Pts',(-11.0994134490001,15.2,-2.21813398000001));
#266989=CARTESIAN_POINT('Ctrl Pts',(-11.0994134490001,11.6,-2.21813398000001));
#266990=CARTESIAN_POINT('Ctrl Pts',(-11.1023337200001,15.2,-2.22020696400001));
#266991=CARTESIAN_POINT('Ctrl Pts',(-11.1023337200001,11.6,-2.22020696400001));
#266992=CARTESIAN_POINT('Ctrl Pts',(-11.1052561740001,15.2,-2.22228490700001));
#266993=CARTESIAN_POINT('Ctrl Pts',(-11.1052561740001,11.6,-2.22228490700001));
#266994=CARTESIAN_POINT('Ctrl Pts',(-11.1081808010001,15.2,-2.22436781200001));
#266995=CARTESIAN_POINT('Ctrl Pts',(-11.1081808010001,11.6,-2.22436781200001));
#266996=CARTESIAN_POINT('Ctrl Pts',(-11.1111075920001,15.2,-2.22645567900001));
#266997=CARTESIAN_POINT('Ctrl Pts',(-11.1111075920001,11.6,-2.22645567900001));
#266998=CARTESIAN_POINT('Ctrl Pts',(-11.1140365370001,15.2,-2.22854850700001));
#266999=CARTESIAN_POINT('Ctrl Pts',(-11.1140365370001,11.6,-2.22854850700001));
#267000=CARTESIAN_POINT('Ctrl Pts',(-11.1169676280001,15.2,-2.23064629800001));
#267001=CARTESIAN_POINT('Ctrl Pts',(-11.1169676280001,11.6,-2.23064629800001));
#267002=CARTESIAN_POINT('Ctrl Pts',(-11.1199008530001,15.2,-2.23274905300002));
#267003=CARTESIAN_POINT('Ctrl Pts',(-11.1199008530001,11.6,-2.23274905300002));
#267004=CARTESIAN_POINT('Ctrl Pts',(-11.1228362040001,15.2,-2.23485677100001));
#267005=CARTESIAN_POINT('Ctrl Pts',(-11.1228362040001,11.6,-2.23485677100001));
#267006=CARTESIAN_POINT('Ctrl Pts',(-11.1257736700001,15.2,-2.23696945200002));
#267007=CARTESIAN_POINT('Ctrl Pts',(-11.1257736700001,11.6,-2.23696945200002));
#267008=CARTESIAN_POINT('Ctrl Pts',(-11.1287132440001,15.2,-2.23908709800002));
#267009=CARTESIAN_POINT('Ctrl Pts',(-11.1287132440001,11.6,-2.23908709800002));
#267010=CARTESIAN_POINT('Ctrl Pts',(-11.1316549140001,15.2,-2.24120971000001));
#267011=CARTESIAN_POINT('Ctrl Pts',(-11.1316549140001,11.6,-2.24120971000001));
#267012=CARTESIAN_POINT('Ctrl Pts',(-11.1345986720001,15.2,-2.24333728500001));
#267013=CARTESIAN_POINT('Ctrl Pts',(-11.1345986720001,11.6,-2.24333728500001));
#267014=CARTESIAN_POINT('Ctrl Pts',(-11.1375445070001,15.2,-2.24546982700002));
#267015=CARTESIAN_POINT('Ctrl Pts',(-11.1375445070001,11.6,-2.24546982700002));
#267016=CARTESIAN_POINT('Ctrl Pts',(-11.1404924120001,15.2,-2.24760733500001));
#267017=CARTESIAN_POINT('Ctrl Pts',(-11.1404924120001,11.6,-2.24760733500002));
#267018=CARTESIAN_POINT('Ctrl Pts',(-11.1434423750001,15.2,-2.24974981000001));
#267019=CARTESIAN_POINT('Ctrl Pts',(-11.1434423750001,11.6,-2.24974981000001));
#267020=CARTESIAN_POINT('Ctrl Pts',(-11.1463943880001,15.2,-2.25189725100002));
#267021=CARTESIAN_POINT('Ctrl Pts',(-11.1463943880001,11.6,-2.25189725100002));
#267022=CARTESIAN_POINT('Ctrl Pts',(-11.1493484410001,15.2,-2.25404966000001));
#267023=CARTESIAN_POINT('Ctrl Pts',(-11.1493484410001,11.6,-2.25404966000002));
#267024=CARTESIAN_POINT('Ctrl Pts',(-11.1523045240001,15.2,-2.25620703600002));
#267025=CARTESIAN_POINT('Ctrl Pts',(-11.1523045240001,11.6,-2.25620703600002));
#267026=CARTESIAN_POINT('Ctrl Pts',(-11.1552626310001,15.2,-2.25836938000001));
#267027=CARTESIAN_POINT('Ctrl Pts',(-11.1552626310001,11.6,-2.25836938000001));
#267028=CARTESIAN_POINT('Ctrl Pts',(-11.1582227480001,15.2,-2.26053669300001));
#267029=CARTESIAN_POINT('Ctrl Pts',(-11.1582227480001,11.6,-2.26053669300002));
#267030=CARTESIAN_POINT('Ctrl Pts',(-11.1611848690001,15.2,-2.26270897400001));
#267031=CARTESIAN_POINT('Ctrl Pts',(-11.1611848690001,11.6,-2.26270897400001));
#267032=CARTESIAN_POINT('Ctrl Pts',(-11.1641489820001,15.2,-2.26488622400002));
#267033=CARTESIAN_POINT('Ctrl Pts',(-11.1641489820001,11.6,-2.26488622400002));
#267034=CARTESIAN_POINT('Ctrl Pts',(-11.1671150810001,15.2,-2.26706844400002));
#267035=CARTESIAN_POINT('Ctrl Pts',(-11.1671150810001,11.6,-2.26706844400002));
#267036=CARTESIAN_POINT('Ctrl Pts',(-11.1700831540001,15.2,-2.26925563400002));
#267037=CARTESIAN_POINT('Ctrl Pts',(-11.1700831540001,11.6,-2.26925563400002));
#267038=CARTESIAN_POINT('Ctrl Pts',(-11.1730531910001,15.2,-2.27144779400001));
#267039=CARTESIAN_POINT('Ctrl Pts',(-11.1730531910001,11.6,-2.27144779400001));
#267040=CARTESIAN_POINT('Ctrl Pts',(-11.1760251850001,15.2,-2.27364492400001));
#267041=CARTESIAN_POINT('Ctrl Pts',(-11.1760251850001,11.6,-2.27364492400001));
#267042=CARTESIAN_POINT('Ctrl Pts',(-11.1789991260001,15.2,-2.27584702400002));
#267043=CARTESIAN_POINT('Ctrl Pts',(-11.1789991260001,11.6,-2.27584702400002));
#267044=CARTESIAN_POINT('Ctrl Pts',(-11.1819750050001,15.2,-2.27805409600002));
#267045=CARTESIAN_POINT('Ctrl Pts',(-11.1819750050001,11.6,-2.27805409600002));
#267046=CARTESIAN_POINT('Ctrl Pts',(-11.1849528130001,15.2,-2.28026613900001));
#267047=CARTESIAN_POINT('Ctrl Pts',(-11.1849528130001,11.6,-2.28026613900001));
#267048=CARTESIAN_POINT('Ctrl Pts',(-11.1879325400001,15.2,-2.28248315300001));
#267049=CARTESIAN_POINT('Ctrl Pts',(-11.1879325400001,11.6,-2.28248315300001));
#267050=CARTESIAN_POINT('Ctrl Pts',(-11.1909141790001,15.2,-2.28470513900001));
#267051=CARTESIAN_POINT('Ctrl Pts',(-11.1909141790001,11.6,-2.28470513900001));
#267052=CARTESIAN_POINT('Ctrl Pts',(-11.1938977190001,15.2,-2.28693209700001));
#267053=CARTESIAN_POINT('Ctrl Pts',(-11.1938977190001,11.6,-2.28693209700001));
#267054=CARTESIAN_POINT('Ctrl Pts',(-11.1968831490001,15.2,-2.28916402700001));
#267055=CARTESIAN_POINT('Ctrl Pts',(-11.1968831490001,11.6,-2.28916402700001));
#267056=CARTESIAN_POINT('Ctrl Pts',(-11.1998704640001,15.2,-2.29140093100002));
#267057=CARTESIAN_POINT('Ctrl Pts',(-11.1998704640001,11.6,-2.29140093100002));
#267058=CARTESIAN_POINT('Ctrl Pts',(-11.2028596490001,15.2,-2.29364280600001));
#267059=CARTESIAN_POINT('Ctrl Pts',(-11.2028596490001,11.6,-2.29364280600001));
#267060=CARTESIAN_POINT('Ctrl Pts',(-11.2058506990001,15.2,-2.29588965500001));
#267061=CARTESIAN_POINT('Ctrl Pts',(-11.2058506990001,11.6,-2.29588965500001));
#267062=CARTESIAN_POINT('Ctrl Pts',(-11.2088436030001,15.2,-2.29814147700001));
#267063=CARTESIAN_POINT('Ctrl Pts',(-11.2088436030001,11.6,-2.29814147700001));
#267064=CARTESIAN_POINT('Ctrl Pts',(-11.2118383520001,15.2,-2.30039827300001));
#267065=CARTESIAN_POINT('Ctrl Pts',(-11.2118383520001,11.6,-2.30039827300002));
#267066=CARTESIAN_POINT('Ctrl Pts',(-11.2148349390001,15.2,-2.30266004200002));
#267067=CARTESIAN_POINT('Ctrl Pts',(-11.2148349390001,11.6,-2.30266004200002));
#267068=CARTESIAN_POINT('Ctrl Pts',(-11.2178333560001,15.2,-2.30492678400001));
#267069=CARTESIAN_POINT('Ctrl Pts',(-11.2178333560001,11.6,-2.30492678400001));
#267070=CARTESIAN_POINT('Ctrl Pts',(-11.2208335940001,15.2,-2.30719850100002));
#267071=CARTESIAN_POINT('Ctrl Pts',(-11.2208335940001,11.6,-2.30719850100002));
#267072=CARTESIAN_POINT('Ctrl Pts',(-11.2238356440001,15.2,-2.30947519200001));
#267073=CARTESIAN_POINT('Ctrl Pts',(-11.2238356440001,11.6,-2.30947519200001));
#267074=CARTESIAN_POINT('Ctrl Pts',(-11.2268394980001,15.2,-2.31175685800002));
#267075=CARTESIAN_POINT('Ctrl Pts',(-11.2268394980001,11.6,-2.31175685800002));
#267076=CARTESIAN_POINT('Ctrl Pts',(-11.2298451450001,15.2,-2.31404349800002));
#267077=CARTESIAN_POINT('Ctrl Pts',(-11.2298451450001,11.6,-2.31404349800002));
#267078=CARTESIAN_POINT('Ctrl Pts',(-11.2328525720001,15.2,-2.31633511300001));
#267079=CARTESIAN_POINT('Ctrl Pts',(-11.2328525720001,11.6,-2.31633511300001));
#267080=CARTESIAN_POINT('Ctrl Pts',(-11.2358617710001,15.2,-2.31863170300001));
#267081=CARTESIAN_POINT('Ctrl Pts',(-11.2358617710001,11.6,-2.31863170300001));
#267082=CARTESIAN_POINT('Ctrl Pts',(-11.2388727300001,15.2,-2.32093326800001));
#267083=CARTESIAN_POINT('Ctrl Pts',(-11.2388727300001,11.6,-2.32093326800001));
#267084=CARTESIAN_POINT('Ctrl Pts',(-11.2418854380001,15.2,-2.32323980800002));
#267085=CARTESIAN_POINT('Ctrl Pts',(-11.2418854380001,11.6,-2.32323980800002));
#267086=CARTESIAN_POINT('Ctrl Pts',(-11.2448998880001,15.2,-2.32555132400002));
#267087=CARTESIAN_POINT('Ctrl Pts',(-11.2448998880001,11.6,-2.32555132400002));
#267088=CARTESIAN_POINT('Ctrl Pts',(-11.2479160730001,15.2,-2.32786781500002));
#267089=CARTESIAN_POINT('Ctrl Pts',(-11.2479160730001,11.6,-2.32786781500002));
#267090=CARTESIAN_POINT('Ctrl Pts',(-11.2509339910001,15.2,-2.33018928300002));
#267091=CARTESIAN_POINT('Ctrl Pts',(-11.2509339910001,11.6,-2.33018928300002));
#267092=CARTESIAN_POINT('Ctrl Pts',(-11.2539536380001,15.2,-2.33251572400002));
#267093=CARTESIAN_POINT('Ctrl Pts',(-11.2539536380001,11.6,-2.33251572400002));
#267094=CARTESIAN_POINT('Ctrl Pts',(-11.2563707390001,15.2,-2.33438085900001));
#267095=CARTESIAN_POINT('Ctrl Pts',(-11.2563707390001,11.6,-2.33438085900001));
#267096=CARTESIAN_POINT('Ctrl Pts',(-11.2581843410001,15.2,-2.33578194700002));
#267097=CARTESIAN_POINT('Ctrl Pts',(-11.2581843410001,11.6,-2.33578194700002));
#267098=CARTESIAN_POINT('Ctrl Pts',(-11.2593937550001,15.2,-2.33671700200001));
#267099=CARTESIAN_POINT('Ctrl Pts',(-11.2593937550001,11.6,-2.33671700200001));
#267100=CARTESIAN_POINT('Ctrl Pts',(-11.2599985490001,15.2,-2.33718477800001));
#267101=CARTESIAN_POINT('Ctrl Pts',(-11.2599985490001,11.6,-2.33718477800001));
#267102=CARTESIAN_POINT('Ctrl Pts',(-10.2237731100001,15.2,-1.76496130700002));
#267103=CARTESIAN_POINT('Ctrl Pts',(-10.2255010902461,15.2,-1.76541542813168));
#267104=CARTESIAN_POINT('Ctrl Pts',(-10.2272829932875,15.2,-1.76588926588842));
#267105=CARTESIAN_POINT('Ctrl Pts',(-10.2291177142657,15.2,-1.76638321069588));
#267106=CARTESIAN_POINT('Ctrl Pts',(-10.2309612831959,15.2,-1.76687953755489));
#267107=CARTESIAN_POINT('Ctrl Pts',(-10.232858179982,15.2,-1.76739616339468));
#267108=CARTESIAN_POINT('Ctrl Pts',(-10.2348073231887,15.2,-1.76793345428534));
#267109=CARTESIAN_POINT('Ctrl Pts',(-10.2367564662182,15.2,-1.76847074512719));
#267110=CARTESIAN_POINT('Ctrl Pts',(-10.2387578531412,15.2,-1.76902870433768));
#267111=CARTESIAN_POINT('Ctrl Pts',(-10.2408104332333,15.2,-1.76960768598331));
#267112=CARTESIAN_POINT('Ctrl Pts',(-10.2428630133254,15.2,-1.77018666762894));
#267113=CARTESIAN_POINT('Ctrl Pts',(-10.2449667829903,15.2,-1.77078667199102));
#267114=CARTESIAN_POINT('Ctrl Pts',(-10.2471207202667,15.2,-1.77140804341492));
#267115=CARTESIAN_POINT('Ctrl Pts',(-10.2492746577388,15.2,-1.77202941489526));
#267116=CARTESIAN_POINT('Ctrl Pts',(-10.2514787619861,15.2,-1.77267215260972));
#267117=CARTESIAN_POINT('Ctrl Pts',(-10.2537320337789,15.2,-1.77333658806407));
#267118=CARTESIAN_POINT('Ctrl Pts',(-10.2559853053671,15.2,-1.77400102345808));
#267119=CARTESIAN_POINT('Ctrl Pts',(-10.258287747059,15.2,-1.77468715486442));
#267120=CARTESIAN_POINT('Ctrl Pts',(-10.2606383864844,15.2,-1.77539530325863));
#267121=CARTESIAN_POINT('Ctrl Pts',(-10.2633807992897,15.2,-1.77622147642809));
#267122=CARTESIAN_POINT('Ctrl Pts',(-10.2661888137587,15.2,-1.77707761705611));
#267123=CARTESIAN_POINT('Ctrl Pts',(-10.2690609297517,15.2,-1.77796421189115));
#267124=CARTESIAN_POINT('Ctrl Pts',(-10.2715227433321,15.2,-1.77872415028173));
#267125=CARTESIAN_POINT('Ctrl Pts',(-10.2740316522823,15.2,-1.77950646228422));
#267126=CARTESIAN_POINT('Ctrl Pts',(-10.2765867400345,15.2,-1.78031144550867));
#267127=CARTESIAN_POINT('Ctrl Pts',(-10.2791418277867,15.2,-1.78111642873313));
#267128=CARTESIAN_POINT('Ctrl Pts',(-10.2817430937041,15.2,-1.78194408006062));
#267129=CARTESIAN_POINT('Ctrl Pts',(-10.2843896406059,15.2,-1.78279468544538));
#267130=CARTESIAN_POINT('Ctrl Pts',(-10.2870361877482,15.2,-1.78364529090741));
#267131=CARTESIAN_POINT('Ctrl Pts',(-10.2897280174628,15.2,-1.78451885324728));
#267132=CARTESIAN_POINT('Ctrl Pts',(-10.2924642537816,15.2,-1.78541564263106));
#267133=CARTESIAN_POINT('Ctrl Pts',(-10.2952004898518,15.2,-1.78631243193339));
#267134=CARTESIAN_POINT('Ctrl Pts',(-10.2979811346214,15.2,-1.78723245113474));
#267135=CARTESIAN_POINT('Ctrl Pts',(-10.3008053326874,15.2,-1.78817596526816));
#267136=CARTESIAN_POINT('Ctrl Pts',(-10.3036295307534,15.2,-1.78911947940158));
#267137=CARTESIAN_POINT('Ctrl Pts',(-10.3064972822325,15.2,-1.79008648825811));
#267138=CARTESIAN_POINT('Ctrl Pts',(-10.3094077542915,15.2,-1.79107724747108));
#267139=CARTESIAN_POINT('Ctrl Pts',(-10.3123182263506,15.2,-1.79206800668404));
#267140=CARTESIAN_POINT('Ctrl Pts',(-10.3152714195936,15.2,-1.79308251806783));
#267141=CARTESIAN_POINT('Ctrl Pts',(-10.3182665168985,15.2,-1.79412102811178));
#267142=CARTESIAN_POINT('Ctrl Pts',(-10.3212616144756,15.2,-1.79515953825006));
#267143=CARTESIAN_POINT('Ctrl Pts',(-10.324298617665,15.2,-1.79622204704902));
#267144=CARTESIAN_POINT('Ctrl Pts',(-10.3273767301679,15.2,-1.79730879327597));
#267145=CARTESIAN_POINT('Ctrl Pts',(-10.3304548423912,15.2,-1.79839553940421));
#267146=CARTESIAN_POINT('Ctrl Pts',(-10.3335740630195,15.2,-1.79950652338884));
#267147=CARTESIAN_POINT('Ctrl Pts',(-10.3367336133196,15.2,-1.80064197642986));
#267148=CARTESIAN_POINT('Ctrl Pts',(-10.3404197555278,15.2,-1.80196667171315));
#267149=CARTESIAN_POINT('Ctrl Pts',(-10.3441607915552,15.2,-1.80332467195882));
#267150=CARTESIAN_POINT('Ctrl Pts',(-10.3479555098941,15.2,-1.80471633031509));
#267151=CARTESIAN_POINT('Ctrl Pts',(-10.3512081254443,15.2,-1.80590918027283));
#267152=CARTESIAN_POINT('Ctrl Pts',(-10.354500184008,15.2,-1.80712675892025));
#267153=CARTESIAN_POINT('Ctrl Pts',(-10.357830939552,15.2,-1.80836927995736));
#267154=CARTESIAN_POINT('Ctrl Pts',(-10.3611616950959,15.2,-1.80961180099447));
#267155=CARTESIAN_POINT('Ctrl Pts',(-10.3645311512467,15.2,-1.81087926565776));
#267156=CARTESIAN_POINT('Ctrl Pts',(-10.3679385748703,15.2,-1.81217187960908));
#267157=CARTESIAN_POINT('Ctrl Pts',(-10.3713459988033,15.2,-1.81346449367781));
#267158=CARTESIAN_POINT('Ctrl Pts',(-10.3747913931235,15.2,-1.81478225687398));
#267159=CARTESIAN_POINT('Ctrl Pts',(-10.3782740448983,15.2,-1.81612537086494));
#267160=CARTESIAN_POINT('Ctrl Pts',(-10.382337138161,15.2,-1.81769233700473));
#267161=CARTESIAN_POINT('Ctrl Pts',(-10.3864509388899,15.2,-1.81929380616216));
#267162=CARTESIAN_POINT('Ctrl Pts',(-10.390614342336,15.2,-1.82093008736377));
#267163=CARTESIAN_POINT('Ctrl Pts',(-10.394182974278,15.2,-1.8223326142718));
#267164=CARTESIAN_POINT('Ctrl Pts',(-10.3977880466902,15.2,-1.82376071572395));
#267165=CARTESIAN_POINT('Ctrl Pts',(-10.4014288796402,15.2,-1.82521457855431));
#267166=CARTESIAN_POINT('Ctrl Pts',(-10.4050697122595,15.2,-1.82666844125262));
#267167=CARTESIAN_POINT('Ctrl Pts',(-10.4087463029747,15.2,-1.82814806405555));
#267168=CARTESIAN_POINT('Ctrl Pts',(-10.4124579827733,15.2,-1.82965362775762));
#267169=CARTESIAN_POINT('Ctrl Pts',(-10.4155510493845,15.2,-1.8309082642216));
#267170=CARTESIAN_POINT('Ctrl Pts',(-10.4186684823111,15.2,-1.83218091350552));
#267171=CARTESIAN_POINT('Ctrl Pts',(-10.4218099022417,15.2,-1.83347167899163));
#267172=CARTESIAN_POINT('Ctrl Pts',(-10.4249513221722,15.2,-1.83476244447774));
#267173=CARTESIAN_POINT('Ctrl Pts',(-10.4281167289928,15.2,-1.83607132367796));
#267174=CARTESIAN_POINT('Ctrl Pts',(-10.4313057457434,15.2,-1.83739841597569));
#267175=CARTESIAN_POINT('Ctrl Pts',(-10.4344947624941,15.2,-1.83872550827343));
#267176=CARTESIAN_POINT('Ctrl Pts',(-10.4377073919272,15.2,-1.84007081228831));
#267177=CARTESIAN_POINT('Ctrl Pts',(-10.4409432619284,15.2,-1.84143442458093));
#267178=CARTESIAN_POINT('Ctrl Pts',(-10.4448263057888,15.2,-1.84307075927262));
#267179=CARTESIAN_POINT('Ctrl Pts',(-10.4487428171215,15.2,-1.84473345744554));
#267180=CARTESIAN_POINT('Ctrl Pts',(-10.4526921690599,15.2,-1.84642267713301));
#267181=CARTESIAN_POINT('Ctrl Pts',(-10.4559832957948,15.2,-1.84783036025705));
#267182=CARTESIAN_POINT('Ctrl Pts',(-10.4592972280831,15.2,-1.84925646249822));
#267183=CARTESIAN_POINT('Ctrl Pts',(-10.4626336097649,15.2,-1.85070107069918));
#267184=CARTESIAN_POINT('Ctrl Pts',(-10.4659699914466,15.2,-1.85214567890014));
#267185=CARTESIAN_POINT('Ctrl Pts',(-10.4693288195611,15.2,-1.85360879656108));
#267186=CARTESIAN_POINT('Ctrl Pts',(-10.4727097455333,15.2,-1.8550905062833));
#267187=CARTESIAN_POINT('Ctrl Pts',(-10.4767668565526,15.2,-1.85686855788536));
#267188=CARTESIAN_POINT('Ctrl Pts',(-10.4808557861972,15.2,-1.8586733857911));
#267189=CARTESIAN_POINT('Ctrl Pts',(-10.4849759355848,15.2,-1.8605051335645));
#267190=CARTESIAN_POINT('Ctrl Pts',(-10.4884093935326,15.2,-1.8620315900978));
#267191=CARTESIAN_POINT('Ctrl Pts',(-10.4918645315683,15.2,-1.86357674172655));
#267192=CARTESIAN_POINT('Ctrl Pts',(-10.4953410100394,15.2,-1.86514067040613));
#267193=CARTESIAN_POINT('Ctrl Pts',(-10.4995127844322,15.2,-1.86701738492392));
#267194=CARTESIAN_POINT('Ctrl Pts',(-10.503715288887,15.2,-1.86892113392835));
#267195=CARTESIAN_POINT('Ctrl Pts',(-10.507947939703,15.2,-1.87085205945211));
#267196=CARTESIAN_POINT('Ctrl Pts',(-10.5114751481398,15.2,-1.87246116379216));
#267197=CARTESIAN_POINT('Ctrl Pts',(-10.5150232947072,15.2,-1.87408913832673));
#267198=CARTESIAN_POINT('Ctrl Pts',(-10.5185920470249,15.2,-1.87573605953456));
#267199=CARTESIAN_POINT('Ctrl Pts',(-10.5221607997315,15.2,-1.87738298092189));
#267200=CARTESIAN_POINT('Ctrl Pts',(-10.5257501579795,15.2,-1.87904884983669));
#267201=CARTESIAN_POINT('Ctrl Pts',(-10.5293597967279,15.2,-1.88073373802959));
#267202=CARTESIAN_POINT('Ctrl Pts',(-10.5329694354762,15.2,-1.88241862622248));
#267203=CARTESIAN_POINT('Ctrl Pts',(-10.5365993551742,15.2,-1.88412253748728));
#267204=CARTESIAN_POINT('Ctrl Pts',(-10.5402492322559,15.2,-1.88584553970794));
#267205=CARTESIAN_POINT('Ctrl Pts',(-10.5446290849927,15.2,-1.8879131424854));
#267206=CARTESIAN_POINT('Ctrl Pts',(-10.5490376785725,15.2,-1.89000823945703));
#267207=CARTESIAN_POINT('Ctrl Pts',(-10.5534744636209,15.2,-1.89213095026371));
#267208=CARTESIAN_POINT('Ctrl Pts',(-10.5571717842932,15.2,-1.89389987583955));
#267209=CARTESIAN_POINT('Ctrl Pts',(-10.5608886844427,15.2,-1.89568797632368));
#267210=CARTESIAN_POINT('Ctrl Pts',(-10.5646248482637,15.2,-1.89749532097804));
#267211=CARTESIAN_POINT('Ctrl Pts',(-10.5683610120847,15.2,-1.8993026656324));
#267212=CARTESIAN_POINT('Ctrl Pts',(-10.5721164430588,15.2,-1.90112925419539));
#267213=CARTESIAN_POINT('Ctrl Pts',(-10.575890830977,15.2,-1.90297515051642));
#267214=CARTESIAN_POINT('Ctrl Pts',(-10.5796652184838,15.2,-1.90482104663624));
#267215=CARTESIAN_POINT('Ctrl Pts',(-10.5834585628684,15.2,-1.90668625191048));
#267216=CARTESIAN_POINT('Ctrl Pts',(-10.5872705597431,15.2,-1.9085708287868));
#267217=CARTESIAN_POINT('Ctrl Pts',(-10.5903201577414,15.2,-1.91007849053437));
#267218=CARTESIAN_POINT('Ctrl Pts',(-10.5933816951381,15.2,-1.91159855016644));
#267219=CARTESIAN_POINT('Ctrl Pts',(-10.59645501575,15.2,-1.91313103924996));
#267220=CARTESIAN_POINT('Ctrl Pts',(-10.5995283363619,15.2,-1.91466352833349));
#267221=CARTESIAN_POINT('Ctrl Pts',(-10.6026134402864,15.2,-1.91620844646012));
#267222=CARTESIAN_POINT('Ctrl Pts',(-10.6057101767897,15.2,-1.91776582604627));
#267223=CARTESIAN_POINT('Ctrl Pts',(-10.608806912871,15.2,-1.91932320542022));
#267224=CARTESIAN_POINT('Ctrl Pts',(-10.6119152799916,15.2,-1.92089304261277));
#267225=CARTESIAN_POINT('Ctrl Pts',(-10.6150351274729,15.2,-1.92247537199056));
#267226=CARTESIAN_POINT('Ctrl Pts',(-10.6181549753793,15.2,-1.92405770158394));
#267227=CARTESIAN_POINT('Ctrl Pts',(-10.6212863036442,15.2,-1.92565252052667));
#267228=CARTESIAN_POINT('Ctrl Pts',(-10.6244289635388,15.2,-1.92725985900444));
#267229=CARTESIAN_POINT('Ctrl Pts',(-10.6275716230053,15.2,-1.92886719726321));
#267230=CARTESIAN_POINT('Ctrl Pts',(-10.630725612537,15.2,-1.93048705547868));
#267231=CARTESIAN_POINT('Ctrl Pts',(-10.6338907859997,15.2,-1.93211946156664));
#267232=CARTESIAN_POINT('Ctrl Pts',(-10.6370559598937,15.2,-1.93375186787701));
#267233=CARTESIAN_POINT('Ctrl Pts',(-10.6402323162592,15.2,-1.93539682139965));
#267234=CARTESIAN_POINT('Ctrl Pts',(-10.6434197092043,15.2,-1.93705435124055));
#267235=CARTESIAN_POINT('Ctrl Pts',(-10.646607101715,15.2,-1.93871188085561));
#267236=CARTESIAN_POINT('Ctrl Pts',(-10.6498055307425,15.2,-1.94038198568146));
#267237=CARTESIAN_POINT('Ctrl Pts',(-10.6530148509794,15.2,-1.94206469382086));
#267238=CARTESIAN_POINT('Ctrl Pts',(-10.6562241716536,15.2,-1.94374740218952));
#267239=CARTESIAN_POINT('Ctrl Pts',(-10.6594443837097,15.2,-1.94544271250135));
#267240=CARTESIAN_POINT('Ctrl Pts',(-10.6626753429976,15.2,-1.94715065337304));
#267241=CARTESIAN_POINT('Ctrl Pts',(-10.6659063018453,15.2,-1.94885859401202));
#267242=CARTESIAN_POINT('Ctrl Pts',(-10.6691480087602,15.2,-1.95057916340473));
#267243=CARTESIAN_POINT('Ctrl Pts',(-10.6724003205448,15.2,-1.9523123870152));
#267244=CARTESIAN_POINT('Ctrl Pts',(-10.6756526327725,15.2,-1.95404561086182));
#267245=CARTESIAN_POINT('Ctrl Pts',(-10.6789155489775,15.2,-1.95579149007773));
#267246=CARTESIAN_POINT('Ctrl Pts',(-10.6821889302677,15.2,-1.95755004911885));
#267247=CARTESIAN_POINT('Ctrl Pts',(-10.6862806566575,15.2,-1.95974824780045));
#267248=CARTESIAN_POINT('Ctrl Pts',(-10.6903887316523,15.2,-1.96196625875095));
#267249=CARTESIAN_POINT('Ctrl Pts',(-10.6945128847782,15.2,-1.96420412986311));
#267250=CARTESIAN_POINT('Ctrl Pts',(-10.6978122070091,15.2,-1.96599442660647));
#267251=CARTESIAN_POINT('Ctrl Pts',(-10.7011218184748,15.2,-1.96779743342872));
#267252=CARTESIAN_POINT('Ctrl Pts',(-10.704441581035,15.2,-1.96961317370323));
#267253=CARTESIAN_POINT('Ctrl Pts',(-10.7077613440476,15.2,-1.97142891422513));
#267254=CARTESIAN_POINT('Ctrl Pts',(-10.7110912583488,15.2,-1.97325738926053));
#267255=CARTESIAN_POINT('Ctrl Pts',(-10.7144311870315,15.2,-1.97509862091727));
#267256=CARTESIAN_POINT('Ctrl Pts',(-10.7177711152591,15.2,-1.97693985232314));
#267257=CARTESIAN_POINT('Ctrl Pts',(-10.7211210569069,15.2,-1.97879383991255));
#267258=CARTESIAN_POINT('Ctrl Pts',(-10.724480877909,15.2,-1.98066060670309));
#267259=CARTESIAN_POINT('Ctrl Pts',(-10.728680654505,15.2,-1.98299406538202));
#267260=CARTESIAN_POINT('Ctrl Pts',(-10.7328958667709,15.2,-1.98534749229066));
#267261=CARTESIAN_POINT('Ctrl Pts',(-10.7371262512173,15.2,-1.98772092844951));
#267262=CARTESIAN_POINT('Ctrl Pts',(-10.7405105589589,15.2,-1.98961967748008));
#267263=CARTESIAN_POINT('Ctrl Pts',(-10.7439045777533,15.2,-1.99153123194891));
#267264=CARTESIAN_POINT('Ctrl Pts',(-10.747308174495,15.2,-1.99345561366574));
#267265=CARTESIAN_POINT('Ctrl Pts',(-10.7515626701902,15.2,-1.99586109068067));
#267266=CARTESIAN_POINT('Ctrl Pts',(-10.755832130074,15.2,-1.99828660933676));
#267267=CARTESIAN_POINT('Ctrl Pts',(-10.7601162983386,15.2,-2.00073221114336));
#267268=CARTESIAN_POINT('Ctrl Pts',(-10.7644004666033,15.2,-2.00317781294997));
#267269=CARTESIAN_POINT('Ctrl Pts',(-10.768699341812,15.2,-2.00564349469633));
#267270=CARTESIAN_POINT('Ctrl Pts',(-10.7730126719591,15.2,-2.00812929753027));
#267271=CARTESIAN_POINT('Ctrl Pts',(-10.7773260021062,15.2,-2.01061510036421));
#267272=CARTESIAN_POINT('Ctrl Pts',(-10.7816537844946,15.2,-2.01312102315096));
#267273=CARTESIAN_POINT('Ctrl Pts',(-10.7859957688013,15.2,-2.01564710259705));
#267274=CARTESIAN_POINT('Ctrl Pts',(-10.7894693559627,15.2,-2.01766796598872));
#267275=CARTESIAN_POINT('Ctrl Pts',(-10.7929520333507,15.2,-2.01970172907593));
#267276=CARTESIAN_POINT('Ctrl Pts',(-10.7964436717313,15.2,-2.02174841107444));
#267277=CARTESIAN_POINT('Ctrl Pts',(-10.8016811300159,15.2,-2.02481843449049));
#267278=CARTESIAN_POINT('Ctrl Pts',(-10.8069387517696,15.2,-2.02791752556847));
#267279=CARTESIAN_POINT('Ctrl Pts',(-10.8122161100586,15.2,-2.03104574107428));
#267280=CARTESIAN_POINT('Ctrl Pts',(-10.8157343484386,15.2,-2.03313121779401));
#267281=CARTESIAN_POINT('Ctrl Pts',(-10.8192613591206,15.2,-2.03522963990326));
#267282=CARTESIAN_POINT('Ctrl Pts',(-10.8227970175143,15.2,-2.0373410232402));
#267283=CARTESIAN_POINT('Ctrl Pts',(-10.8263326763897,15.2,-2.03945240686481));
#267284=CARTESIAN_POINT('Ctrl Pts',(-10.8298769814559,15.2,-2.0415767519705));
#267285=CARTESIAN_POINT('Ctrl Pts',(-10.8334298103726,15.2,-2.04371407486609));
#267286=CARTESIAN_POINT('Ctrl Pts',(-10.8378708462765,15.2,-2.04638572833997));
#267287=CARTESIAN_POINT('Ctrl Pts',(-10.8423252008944,15.2,-2.04907765926418));
#267288=CARTESIAN_POINT('Ctrl Pts',(-10.8467926318677,15.2,-2.05178989940473));
#267289=CARTESIAN_POINT('Ctrl Pts',(-10.8503665763542,15.2,-2.05395969133979));
#267290=CARTESIAN_POINT('Ctrl Pts',(-10.8539488914665,15.2,-2.0561424805486));
#267291=CARTESIAN_POINT('Ctrl Pts',(-10.8575394540226,15.2,-2.05833828199014));
#267292=CARTESIAN_POINT('Ctrl Pts',(-10.8611300170679,15.2,-2.06053408373086));
#267293=CARTESIAN_POINT('Ctrl Pts',(-10.8647288282285,15.2,-2.06274289860748));
#267294=CARTESIAN_POINT('Ctrl Pts',(-10.8683357671481,15.2,-2.06496474139658));
#267295=CARTESIAN_POINT('Ctrl Pts',(-10.8728444405519,15.2,-2.06774204473157));
#267296=CARTESIAN_POINT('Ctrl Pts',(-10.8773658122587,15.2,-2.07053970168913));
#267297=CARTESIAN_POINT('Ctrl Pts',(-10.8818996505931,15.2,-2.07335774113523));
#267298=CARTESIAN_POINT('Ctrl Pts',(-10.885526720964,15.2,-2.07561217250782));
#267299=CARTESIAN_POINT('Ctrl Pts',(-10.8891617691983,15.2,-2.07787964948287));
#267300=CARTESIAN_POINT('Ctrl Pts',(-10.8928046769725,15.2,-2.08016018480675));
#267301=CARTESIAN_POINT('Ctrl Pts',(-10.8964475852431,15.2,-2.08244072044135));
#267302=CARTESIAN_POINT('Ctrl Pts',(-10.9000983519841,15.2,-2.08473431341673));
#267303=CARTESIAN_POINT('Ctrl Pts',(-10.9037568615732,15.2,-2.08704097887711));
#267304=CARTESIAN_POINT('Ctrl Pts',(-10.9074153706638,15.2,-2.0893476440232));
#267305=CARTESIAN_POINT('Ctrl Pts',(-10.9110816210367,15.2,-2.0916673803426));
#267306=CARTESIAN_POINT('Ctrl Pts',(-10.9147554974581,15.2,-2.09400020031771));
#267307=CARTESIAN_POINT('Ctrl Pts',(-10.91842937438,15.2,-2.09633302061067));
#267308=CARTESIAN_POINT('Ctrl Pts',(-10.9221108745994,15.2,-2.09867892545313));
#267309=CARTESIAN_POINT('Ctrl Pts',(-10.9257998863187,15.2,-2.10103792586734));
#267310=CARTESIAN_POINT('Ctrl Pts',(-10.9304111507165,15.2,-2.1039866762244));
#267311=CARTESIAN_POINT('Ctrl Pts',(-10.9350341478386,15.2,-2.10695588808379));
#267312=CARTESIAN_POINT('Ctrl Pts',(-10.9396686538812,15.2,-2.10994558718269));
#267313=CARTESIAN_POINT('Ctrl Pts',(-10.9443031599238,15.2,-2.11293528628159));
#267314=CARTESIAN_POINT('Ctrl Pts',(-10.9489491760805,15.2,-2.11594546820026));
#267315=CARTESIAN_POINT('Ctrl Pts',(-10.9536064788592,15.2,-2.11897615910472));
#267316=CARTESIAN_POINT('Ctrl Pts',(-10.9564008604249,15.2,-2.12079457358132));
#267317=CARTESIAN_POINT('Ctrl Pts',(-10.9591993058536,15.2,-2.12262037026221));
#267318=CARTESIAN_POINT('Ctrl Pts',(-10.9620017670173,15.2,-2.12445355337138));
#267319=CARTESIAN_POINT('Ctrl Pts',(-10.9648042281809,15.2,-2.12628673648055));
#267320=CARTESIAN_POINT('Ctrl Pts',(-10.9676107047415,15.2,-2.12812730645135));
#267321=CARTESIAN_POINT('Ctrl Pts',(-10.9704211498064,15.2,-2.12997526796818));
#267322=CARTESIAN_POINT('Ctrl Pts',(-10.9732315948713,15.2,-2.13182322948502));
#267323=CARTESIAN_POINT('Ctrl Pts',(-10.9760460097191,15.2,-2.13367858213431));
#267324=CARTESIAN_POINT('Ctrl Pts',(-10.9788643452834,15.2,-2.13554132973329));
#267325=CARTESIAN_POINT('Ctrl Pts',(-10.9816826808476,15.2,-2.13740407733227));
#267326=CARTESIAN_POINT('Ctrl Pts',(-10.9845049378784,15.2,-2.13927422128096));
#267327=CARTESIAN_POINT('Ctrl Pts',(-10.987331069442,15.2,-2.14115176425377));
#267328=CARTESIAN_POINT('Ctrl Pts',(-10.9901572010057,15.2,-2.14302930722657));
#267329=CARTESIAN_POINT('Ctrl Pts',(-10.9929872073303,15.2,-2.14491424832566));
#267330=CARTESIAN_POINT('Ctrl Pts',(-10.9958210424518,15.2,-2.14680659385058));
#267331=CARTESIAN_POINT('Ctrl Pts',(-10.9986548775733,15.2,-2.1486989393755));
#267332=CARTESIAN_POINT('Ctrl Pts',(-11.0014925400843,15.2,-2.15059868867118));
#267333=CARTESIAN_POINT('Ctrl Pts',(-11.0043339846473,15.2,-2.15250584464254));
#267334=CARTESIAN_POINT('Ctrl Pts',(-11.0071754297264,15.2,-2.15441300096038));
#267335=CARTESIAN_POINT('Ctrl Pts',(-11.0100206574732,15.2,-2.15632756378862));
#267336=CARTESIAN_POINT('Ctrl Pts',(-11.0128696201378,15.2,-2.15824953765229));
#267337=CARTESIAN_POINT('Ctrl Pts',(-11.0157185822848,15.2,-2.1601715111668));
#267338=CARTESIAN_POINT('Ctrl Pts',(-11.0185712811649,15.2,-2.1621008959976));
#267339=CARTESIAN_POINT('Ctrl Pts',(-11.0214276693114,15.2,-2.1640376945112));
#267340=CARTESIAN_POINT('Ctrl Pts',(-11.0242840574579,15.2,-2.16597449302479));
#267341=CARTESIAN_POINT('Ctrl Pts',(-11.0271441361437,15.2,-2.16791870628042));
#267342=CARTESIAN_POINT('Ctrl Pts',(-11.0300078597193,15.2,-2.16987033680174));
#267343=CARTESIAN_POINT('Ctrl Pts',(-11.0328715832949,15.2,-2.17182196732306));
#267344=CARTESIAN_POINT('Ctrl Pts',(-11.0357389519054,15.2,-2.17378101551073));
#267345=CARTESIAN_POINT('Ctrl Pts',(-11.0386099189808,15.2,-2.17574748453151));
#267346=CARTESIAN_POINT('Ctrl Pts',(-11.042437875429,15.2,-2.17836944346405));
#267347=CARTESIAN_POINT('Ctrl Pts',(-11.0462722306763,15.2,-2.18100459512617));
#267348=CARTESIAN_POINT('Ctrl Pts',(-11.0501128783863,15.2,-2.18365294671631));
#267349=CARTESIAN_POINT('Ctrl Pts',(-11.0529933639072,15.2,-2.1856392102285));
#267350=CARTESIAN_POINT('Ctrl Pts',(-11.0558773878361,15.2,-2.18763289915694));
#267351=CARTESIAN_POINT('Ctrl Pts',(-11.0587649078148,15.2,-2.18963401520988));
#267352=CARTESIAN_POINT('Ctrl Pts',(-11.0616524277935,15.2,-2.19163513126281));
#267353=CARTESIAN_POINT('Ctrl Pts',(-11.0645434418947,15.2,-2.19364367579918));
#267354=CARTESIAN_POINT('Ctrl Pts',(-11.067437906011,15.2,-2.1956596512768));
#267355=CARTESIAN_POINT('Ctrl Pts',(-11.0703323701273,15.2,-2.19767562675442));
#267356=CARTESIAN_POINT('Ctrl Pts',(-11.0732302853563,15.2,-2.19969903324606));
#267357=CARTESIAN_POINT('Ctrl Pts',(-11.0761316055141,15.2,-2.20172987276479));
#267358=CARTESIAN_POINT('Ctrl Pts',(-11.0790329256718,15.2,-2.20376071228352));
#267359=CARTESIAN_POINT('Ctrl Pts',(-11.0819376525724,15.2,-2.20579898560209));
#267360=CARTESIAN_POINT('Ctrl Pts',(-11.0848457407164,15.2,-2.20784469502711));
#267361=CARTESIAN_POINT('Ctrl Pts',(-11.0877538288605,15.2,-2.20989040445212));
#267362=CARTESIAN_POINT('Ctrl Pts',(-11.0906652795376,15.2,-2.21194354895998));
#267363=CARTESIAN_POINT('Ctrl Pts',(-11.0935800481396,15.2,-2.21400413330076));
#267364=CARTESIAN_POINT('Ctrl Pts',(-11.0964948172711,15.2,-2.21606471801588));
#267365=CARTESIAN_POINT('Ctrl Pts',(-11.0994129042952,15.2,-2.21813274044978));
#267366=CARTESIAN_POINT('Ctrl Pts',(-11.1023342663869,15.2,-2.22020820425242));
#267367=CARTESIAN_POINT('Ctrl Pts',(-11.1052556279479,15.2,-2.22228366767801));
#267368=CARTESIAN_POINT('Ctrl Pts',(-11.108180263692,15.2,-2.22436657203656));
#267369=CARTESIAN_POINT('Ctrl Pts',(-11.1111081308359,15.2,-2.22645691950293));
#267370=CARTESIAN_POINT('Ctrl Pts',(-11.1140359979798,15.2,-2.22854726696931));
#267371=CARTESIAN_POINT('Ctrl Pts',(-11.1169670973626,15.2,-2.23064505736877));
#267372=CARTESIAN_POINT('Ctrl Pts',(-11.1199013844777,15.2,-2.23275029376021));
#267373=CARTESIAN_POINT('Ctrl Pts',(-11.1228356715928,15.2,-2.23485553015164));
#267374=CARTESIAN_POINT('Ctrl Pts',(-11.1257731469575,15.2,-2.23696821061548));
#267375=CARTESIAN_POINT('Ctrl Pts',(-11.1287137680307,15.2,-2.23908833946471));
#267376=CARTESIAN_POINT('Ctrl Pts',(-11.1326345964844,15.2,-2.24191517818711));
#267377=CARTESIAN_POINT('Ctrl Pts',(-11.1365610160725,15.2,-2.24475525504296));
#267378=CARTESIAN_POINT('Ctrl Pts',(-11.1404929271762,15.2,-2.24760857719982));
#267379=CARTESIAN_POINT('Ctrl Pts',(-11.1434418602362,15.2,-2.24974856862308));
#267380=CARTESIAN_POINT('Ctrl Pts',(-11.1463938816293,15.2,-2.25189600957929));
#267381=CARTESIAN_POINT('Ctrl Pts',(-11.1493489488555,15.2,-2.25405090200164));
#267382=CARTESIAN_POINT('Ctrl Pts',(-11.1523040160817,15.2,-2.25620579442399));
#267383=CARTESIAN_POINT('Ctrl Pts',(-11.1552621307969,15.2,-2.25836813808755));
#267384=CARTESIAN_POINT('Ctrl Pts',(-11.1582232489527,15.2,-2.2605379350186));
#267385=CARTESIAN_POINT('Ctrl Pts',(-11.1611843671086,15.2,-2.26270773194965));
#267386=CARTESIAN_POINT('Ctrl Pts',(-11.164148489525,15.2,-2.26488498156748));
#267387=CARTESIAN_POINT('Ctrl Pts',(-11.167115574514,15.2,-2.26706968649798));
#267388=CARTESIAN_POINT('Ctrl Pts',(-11.170082659503,15.2,-2.26925439142848));
#267389=CARTESIAN_POINT('Ctrl Pts',(-11.1730527048343,15.2,-2.27144655127422));
#267390=CARTESIAN_POINT('Ctrl Pts',(-11.1760256714344,15.2,-2.273646166277));
#267391=CARTESIAN_POINT('Ctrl Pts',(-11.1789986380344,15.2,-2.27584578127977));
#267392=CARTESIAN_POINT('Ctrl Pts',(-11.1819745254426,15.2,-2.27805285281535));
#267393=CARTESIAN_POINT('Ctrl Pts',(-11.1849532921257,15.2,-2.28026738127553));
#267394=CARTESIAN_POINT('Ctrl Pts',(-11.1899179034445,15.2,-2.28395826217661));
#267395=CARTESIAN_POINT('Ctrl Pts',(-11.1948905154792,15.2,-2.2876698573484));
#267396=CARTESIAN_POINT('Ctrl Pts',(-11.1998709310052,15.2,-2.29140217336677));
#267397=CARTESIAN_POINT('Ctrl Pts',(-11.2028591802123,15.2,-2.29364156289643));
#267398=CARTESIAN_POINT('Ctrl Pts',(-11.2058502378899,15.2,-2.29588841107478));
#267399=CARTESIAN_POINT('Ctrl Pts',(-11.2088440636141,15.2,-2.29814271999186));
#267400=CARTESIAN_POINT('Ctrl Pts',(-11.2128358316089,15.2,-2.30114846548766));
#267401=CARTESIAN_POINT('Ctrl Pts',(-11.2168325224014,15.2,-2.30416747235136));
#267402=CARTESIAN_POINT('Ctrl Pts',(-11.2208340470084,15.2,-2.30719974451662));
#267403=CARTESIAN_POINT('Ctrl Pts',(-11.2248355716153,15.2,-2.31023201668189));
#267404=CARTESIAN_POINT('Ctrl Pts',(-11.2288419325145,15.2,-2.31327755374869));
#267405=CARTESIAN_POINT('Ctrl Pts',(-11.2328530156225,15.2,-2.31633635725008));
#267406=CARTESIAN_POINT('Ctrl Pts',(-11.2358613276802,15.2,-2.31863045966774));
#267407=CARTESIAN_POINT('Ctrl Pts',(-11.2388722956251,15.2,-2.32093202439778));
#267408=CARTESIAN_POINT('Ctrl Pts',(-11.2418858740831,15.2,-2.32324105243011));
#267409=CARTESIAN_POINT('Ctrl Pts',(-11.2448994525412,15.2,-2.32555008046245));
#267410=CARTESIAN_POINT('Ctrl Pts',(-11.2479156413857,15.2,-2.32786657213309));
#267411=CARTESIAN_POINT('Ctrl Pts',(-11.2509344236132,15.2,-2.33019052657526));
#267412=CARTESIAN_POINT('Ctrl Pts',(-11.2539532058406,15.2,-2.33251448101743));
#267413=CARTESIAN_POINT('Ctrl Pts',(-11.2569745784507,15.2,-2.33484589757511));
#267414=CARTESIAN_POINT('Ctrl Pts',(-11.2599985490001,15.2,-2.33718477800001));
#267415=CARTESIAN_POINT('Ctrl Pts',(-10.2237731100001,12.2,-1.76496130700002));
#267416=CARTESIAN_POINT('Ctrl Pts',(-10.2255010902461,12.2,-1.76541542813168));
#267417=CARTESIAN_POINT('Ctrl Pts',(-10.2272829932875,12.2,-1.76588926588842));
#267418=CARTESIAN_POINT('Ctrl Pts',(-10.2291177142657,12.2,-1.76638321069588));
#267419=CARTESIAN_POINT('Ctrl Pts',(-10.2309612831959,12.2,-1.76687953755489));
#267420=CARTESIAN_POINT('Ctrl Pts',(-10.232858179982,12.2,-1.76739616339468));
#267421=CARTESIAN_POINT('Ctrl Pts',(-10.2348073231887,12.2,-1.76793345428534));
#267422=CARTESIAN_POINT('Ctrl Pts',(-10.2367564662182,12.2,-1.7684707451272));
#267423=CARTESIAN_POINT('Ctrl Pts',(-10.2387578531412,12.2,-1.76902870433768));
#267424=CARTESIAN_POINT('Ctrl Pts',(-10.2408104332333,12.2,-1.76960768598331));
#267425=CARTESIAN_POINT('Ctrl Pts',(-10.2428630133254,12.2,-1.77018666762894));
#267426=CARTESIAN_POINT('Ctrl Pts',(-10.2449667829903,12.2,-1.77078667199102));
#267427=CARTESIAN_POINT('Ctrl Pts',(-10.2471207202667,12.2,-1.77140804341492));
#267428=CARTESIAN_POINT('Ctrl Pts',(-10.2492746577388,12.2,-1.77202941489526));
#267429=CARTESIAN_POINT('Ctrl Pts',(-10.2514787619861,12.2,-1.77267215260972));
#267430=CARTESIAN_POINT('Ctrl Pts',(-10.2537320337789,12.2,-1.77333658806407));
#267431=CARTESIAN_POINT('Ctrl Pts',(-10.2559853053671,12.2,-1.77400102345808));
#267432=CARTESIAN_POINT('Ctrl Pts',(-10.258287747059,12.2,-1.77468715486442));
#267433=CARTESIAN_POINT('Ctrl Pts',(-10.2606383864844,12.2,-1.77539530325863));
#267434=CARTESIAN_POINT('Ctrl Pts',(-10.2629890259098,12.2,-1.77610345165284));
#267435=CARTESIAN_POINT('Ctrl Pts',(-10.2653878629661,12.2,-1.7768336161957));
#267436=CARTESIAN_POINT('Ctrl Pts',(-10.2678339516252,12.2,-1.77758610541739));
#267437=CARTESIAN_POINT('Ctrl Pts',(-10.2702800405064,12.2,-1.77833859470743));
#267438=CARTESIAN_POINT('Ctrl Pts',(-10.2727733800186,12.2,-1.77911340744191));
#267439=CARTESIAN_POINT('Ctrl Pts',(-10.2753130489935,12.2,-1.77991084182023));
#267440=CARTESIAN_POINT('Ctrl Pts',(-10.2778527177377,12.2,-1.78070827612613));
#267441=CARTESIAN_POINT('Ctrl Pts',(-10.2804387162622,12.2,-1.78152833200897));
#267442=CARTESIAN_POINT('Ctrl Pts',(-10.2830701449186,12.2,-1.78237129431268));
#267443=CARTESIAN_POINT('Ctrl Pts',(-10.285701573575,12.2,-1.78321425661639));
#267444=CARTESIAN_POINT('Ctrl Pts',(-10.2883784300777,12.2,-1.7840801268016));
#267445=CARTESIAN_POINT('Ctrl Pts',(-10.2910998398935,12.2,-1.78496918193495));
#267446=CARTESIAN_POINT('Ctrl Pts',(-10.2942748181768,12.2,-1.78600641297769));
#267447=CARTESIAN_POINT('Ctrl Pts',(-10.2975104347728,12.2,-1.78707519872204));
#267448=CARTESIAN_POINT('Ctrl Pts',(-10.3008053326874,12.2,-1.78817596526816));
#267449=CARTESIAN_POINT('Ctrl Pts',(-10.3036295307534,12.2,-1.78911947940158));
#267450=CARTESIAN_POINT('Ctrl Pts',(-10.3064972822325,12.2,-1.79008648825811));
#267451=CARTESIAN_POINT('Ctrl Pts',(-10.3094077542915,12.2,-1.79107724747108));
#267452=CARTESIAN_POINT('Ctrl Pts',(-10.3123182263506,12.2,-1.79206800668404));
#267453=CARTESIAN_POINT('Ctrl Pts',(-10.3152714195936,12.2,-1.79308251806783));
#267454=CARTESIAN_POINT('Ctrl Pts',(-10.3182665168985,12.2,-1.79412102811178));
#267455=CARTESIAN_POINT('Ctrl Pts',(-10.3212616144756,12.2,-1.79515953825006));
#267456=CARTESIAN_POINT('Ctrl Pts',(-10.324298617665,12.2,-1.79622204704902));
#267457=CARTESIAN_POINT('Ctrl Pts',(-10.3273767301679,12.2,-1.79730879327597));
#267458=CARTESIAN_POINT('Ctrl Pts',(-10.3304548423912,12.2,-1.79839553940421));
#267459=CARTESIAN_POINT('Ctrl Pts',(-10.3335740630195,12.2,-1.79950652338883));
#267460=CARTESIAN_POINT('Ctrl Pts',(-10.3367336133196,12.2,-1.80064197642986));
#267461=CARTESIAN_POINT('Ctrl Pts',(-10.3398931636198,12.2,-1.80177742947088));
#267462=CARTESIAN_POINT('Ctrl Pts',(-10.3430930445673,12.2,-1.80293735075724));
#267463=CARTESIAN_POINT('Ctrl Pts',(-10.3463324919469,12.2,-1.80412196462919));
#267464=CARTESIAN_POINT('Ctrl Pts',(-10.3495719396208,12.2,-1.80530657860875));
#267465=CARTESIAN_POINT('Ctrl Pts',(-10.3528509557568,12.2,-1.80651588300733));
#267466=CARTESIAN_POINT('Ctrl Pts',(-10.3561687906893,12.2,-1.80775009682568));
#267467=CARTESIAN_POINT('Ctrl Pts',(-10.3594866253204,12.2,-1.80898431053191));
#267468=CARTESIAN_POINT('Ctrl Pts',(-10.3628432843648,12.2,-1.81024342956528));
#267469=CARTESIAN_POINT('Ctrl Pts',(-10.3662380310068,12.2,-1.81152766727439));
#267470=CARTESIAN_POINT('Ctrl Pts',(-10.3701985689613,12.2,-1.81302594467945));
#267471=CARTESIAN_POINT('Ctrl Pts',(-10.3742109513193,12.2,-1.81455840460315));
#267472=CARTESIAN_POINT('Ctrl Pts',(-10.3782740448983,12.2,-1.81612537086494));
#267473=CARTESIAN_POINT('Ctrl Pts',(-10.3817566963567,12.2,-1.81746848473391));
#267474=CARTESIAN_POINT('Ctrl Pts',(-10.3852766033615,12.2,-1.81883694769372));
#267475=CARTESIAN_POINT('Ctrl Pts',(-10.3888330672484,12.2,-1.82023095448267));
#267476=CARTESIAN_POINT('Ctrl Pts',(-10.3923895311352,12.2,-1.82162496127163));
#267477=CARTESIAN_POINT('Ctrl Pts',(-10.3959825532721,12.2,-1.82304451198837));
#267478=CARTESIAN_POINT('Ctrl Pts',(-10.3996114461378,12.2,-1.82448979285078));
#267479=CARTESIAN_POINT('Ctrl Pts',(-10.4032403393331,12.2,-1.82593507384445));
#267480=CARTESIAN_POINT('Ctrl Pts',(-10.4069051039612,12.2,-1.82740608488698));
#267481=CARTESIAN_POINT('Ctrl Pts',(-10.4106050700997,12.2,-1.82890300687817));
#267482=CARTESIAN_POINT('Ctrl Pts',(-10.413688375047,12.2,-1.83015044180285));
#267483=CARTESIAN_POINT('Ctrl Pts',(-10.4167961221577,12.2,-1.83141587063305));
#267484=CARTESIAN_POINT('Ctrl Pts',(-10.4199279321596,12.2,-1.83269939313452));
#267485=CARTESIAN_POINT('Ctrl Pts',(-10.4230597421616,12.2,-1.833982915636));
#267486=CARTESIAN_POINT('Ctrl Pts',(-10.4262156148528,12.2,-1.83528453491556));
#267487=CARTESIAN_POINT('Ctrl Pts',(-10.4293951724242,12.2,-1.83660434568094));
#267488=CARTESIAN_POINT('Ctrl Pts',(-10.432574729649,12.2,-1.83792415630246));
#267489=CARTESIAN_POINT('Ctrl Pts',(-10.435777973226,12.2,-1.83926216018301));
#267490=CARTESIAN_POINT('Ctrl Pts',(-10.4390045313446,12.2,-1.84061845308924));
#267491=CARTESIAN_POINT('Ctrl Pts',(-10.442231089815,12.2,-1.8419747461433));
#267492=CARTESIAN_POINT('Ctrl Pts',(-10.4454809638072,12.2,-1.84334932791373));
#267493=CARTESIAN_POINT('Ctrl Pts',(-10.4487537873469,12.2,-1.84474229180111));
#267494=CARTESIAN_POINT('Ctrl Pts',(-10.4520266108867,12.2,-1.84613525568848));
#267495=CARTESIAN_POINT('Ctrl Pts',(-10.4553223855062,12.2,-1.84754659954724));
#267496=CARTESIAN_POINT('Ctrl Pts',(-10.4586407501149,12.2,-1.84897641753405));
#267497=CARTESIAN_POINT('Ctrl Pts',(-10.4619591147235,12.2,-1.85040623552086));
#267498=CARTESIAN_POINT('Ctrl Pts',(-10.4653000711647,12.2,-1.85185452354401));
#267499=CARTESIAN_POINT('Ctrl Pts',(-10.4686632630385,12.2,-1.85332137319582));
#267500=CARTESIAN_POINT('Ctrl Pts',(-10.4720264549123,12.2,-1.85478822284762));
#267501=CARTESIAN_POINT('Ctrl Pts',(-10.4754118841618,12.2,-1.85627362960824));
#267502=CARTESIAN_POINT('Ctrl Pts',(-10.4788192010356,12.2,-1.85777768342671));
#267503=CARTESIAN_POINT('Ctrl Pts',(-10.4822265179095,12.2,-1.85928173724519));
#267504=CARTESIAN_POINT('Ctrl Pts',(-10.4856557227825,12.2,-1.86080443447551));
#267505=CARTESIAN_POINT('Ctrl Pts',(-10.4891064705065,12.2,-1.86234586073246));
#267506=CARTESIAN_POINT('Ctrl Pts',(-10.4925572182304,12.2,-1.86388728698941));
#267507=CARTESIAN_POINT('Ctrl Pts',(-10.4960295093722,12.2,-1.86544744086663));
#267508=CARTESIAN_POINT('Ctrl Pts',(-10.4995230054833,12.2,-1.86702640149163));
#267509=CARTESIAN_POINT('Ctrl Pts',(-10.5030165015945,12.2,-1.86860536211663));
#267510=CARTESIAN_POINT('Ctrl Pts',(-10.506531203358,12.2,-1.87020313199346));
#267511=CARTESIAN_POINT('Ctrl Pts',(-10.5100667744853,12.2,-1.87181978679252));
#267512=CARTESIAN_POINT('Ctrl Pts',(-10.5136023456125,12.2,-1.87343644159158));
#267513=CARTESIAN_POINT('Ctrl Pts',(-10.5171587875552,12.2,-1.87507198386286));
#267514=CARTESIAN_POINT('Ctrl Pts',(-10.5207357695007,12.2,-1.87672648684995));
#267515=CARTESIAN_POINT('Ctrl Pts',(-10.5243127514462,12.2,-1.87838098983705));
#267516=CARTESIAN_POINT('Ctrl Pts',(-10.5279102734079,12.2,-1.8800544542209));
#267517=CARTESIAN_POINT('Ctrl Pts',(-10.5315280120201,12.2,-1.88174695456911));
#267518=CARTESIAN_POINT('Ctrl Pts',(-10.5351457506322,12.2,-1.88343945491733));
#267519=CARTESIAN_POINT('Ctrl Pts',(-10.5387837034383,12.2,-1.88515099101782));
#267520=CARTESIAN_POINT('Ctrl Pts',(-10.542441551981,12.2,-1.8868816331716));
#267521=CARTESIAN_POINT('Ctrl Pts',(-10.5460994005237,12.2,-1.88861227532538));
#267522=CARTESIAN_POINT('Ctrl Pts',(-10.5497771429487,12.2,-1.89036202468788));
#267523=CARTESIAN_POINT('Ctrl Pts',(-10.5534744636209,12.2,-1.89213095026371));
#267524=CARTESIAN_POINT('Ctrl Pts',(-10.5571717842932,12.2,-1.89389987583954));
#267525=CARTESIAN_POINT('Ctrl Pts',(-10.5608886844426,12.2,-1.89568797632368));
#267526=CARTESIAN_POINT('Ctrl Pts',(-10.5646248482637,12.2,-1.89749532097804));
#267527=CARTESIAN_POINT('Ctrl Pts',(-10.5676137790762,12.2,-1.89894119658332));
#267528=CARTESIAN_POINT('Ctrl Pts',(-10.5706150406843,12.2,-1.900399387862));
#267529=CARTESIAN_POINT('Ctrl Pts',(-10.5736284747704,12.2,-1.90186992862987));
#267530=CARTESIAN_POINT('Ctrl Pts',(-10.5766419092672,12.2,-1.9033404695981));
#267531=CARTESIAN_POINT('Ctrl Pts',(-10.5796675142364,12.2,-1.90482335909585));
#267532=CARTESIAN_POINT('Ctrl Pts',(-10.5827051361659,12.2,-1.90631863097534));
#267533=CARTESIAN_POINT('Ctrl Pts',(-10.5857427576814,12.2,-1.9078139026511));
#267534=CARTESIAN_POINT('Ctrl Pts',(-10.5887923936676,12.2,-1.90932155614812));
#267535=CARTESIAN_POINT('Ctrl Pts',(-10.5918538917498,12.2,-1.91084162363415));
#267536=CARTESIAN_POINT('Ctrl Pts',(-10.5949153902492,12.2,-1.9123616913273));
#267537=CARTESIAN_POINT('Ctrl Pts',(-10.5979887495418,12.2,-1.91389417279693));
#267538=CARTESIAN_POINT('Ctrl Pts',(-10.601073815544,12.2,-1.91543909865971));
#267539=CARTESIAN_POINT('Ctrl Pts',(-10.6041588811259,12.2,-1.916984024312));
#267540=CARTESIAN_POINT('Ctrl Pts',(-10.607255655185,12.2,-1.91854139660934));
#267541=CARTESIAN_POINT('Ctrl Pts',(-10.6103639848074,12.2,-1.92011124228058));
#267542=CARTESIAN_POINT('Ctrl Pts',(-10.6134723148533,12.2,-1.9216810881657));
#267543=CARTESIAN_POINT('Ctrl Pts',(-10.6165922000125,12.2,-1.92326341040938));
#267544=CARTESIAN_POINT('Ctrl Pts',(-10.6197234907394,12.2,-1.92485823683046));
#267545=CARTESIAN_POINT('Ctrl Pts',(-10.6236376039348,12.2,-1.92685176974816));
#267546=CARTESIAN_POINT('Ctrl Pts',(-10.6275695389298,12.2,-1.92886484250423));
#267547=CARTESIAN_POINT('Ctrl Pts',(-10.6315190052501,12.2,-1.93089750965803));
#267548=CARTESIAN_POINT('Ctrl Pts',(-10.6346785780481,12.2,-1.93252364324812));
#267549=CARTESIAN_POINT('Ctrl Pts',(-10.6378493697099,12.2,-1.93416231752513));
#267550=CARTESIAN_POINT('Ctrl Pts',(-10.64103123533,12.2,-1.9358135610271));
#267551=CARTESIAN_POINT('Ctrl Pts',(-10.6442131013837,12.2,-1.93746480475404));
#267552=CARTESIAN_POINT('Ctrl Pts',(-10.6474060403006,12.2,-1.93912861803384));
#267553=CARTESIAN_POINT('Ctrl Pts',(-10.6506099057537,12.2,-1.94080502590379));
#267554=CARTESIAN_POINT('Ctrl Pts',(-10.6538137707703,12.2,-1.94248143354534));
#267555=CARTESIAN_POINT('Ctrl Pts',(-10.6570285647847,12.2,-1.94417043913438));
#267556=CARTESIAN_POINT('Ctrl Pts',(-10.6602541404643,12.2,-1.94587206543842));
#267557=CARTESIAN_POINT('Ctrl Pts',(-10.6634797165834,12.2,-1.94757369197431));
#267558=CARTESIAN_POINT('Ctrl Pts',(-10.6667160762633,12.2,-1.94928794342693));
#267559=CARTESIAN_POINT('Ctrl Pts',(-10.6699630775106,12.2,-1.95101484175114));
#267560=CARTESIAN_POINT('Ctrl Pts',(-10.6732100783154,12.2,-1.95274173984006));
#267561=CARTESIAN_POINT('Ctrl Pts',(-10.6764677183284,12.2,-1.95448128654135));
#267562=CARTESIAN_POINT('Ctrl Pts',(-10.679735857949,12.2,-1.95623350673015));
#267563=CARTESIAN_POINT('Ctrl Pts',(-10.6830039980149,12.2,-1.95798572715768));
#267564=CARTESIAN_POINT('Ctrl Pts',(-10.6862826371819,12.2,-1.95975062156697));
#267565=CARTESIAN_POINT('Ctrl Pts',(-10.68957163525,12.2,-1.96152821394163));
#267566=CARTESIAN_POINT('Ctrl Pts',(-10.6928606333181,12.2,-1.96330580631628));
#267567=CARTESIAN_POINT('Ctrl Pts',(-10.6961599906042,12.2,-1.96509609748965));
#267568=CARTESIAN_POINT('Ctrl Pts',(-10.6994695680078,12.2,-1.9668991104781));
#267569=CARTESIAN_POINT('Ctrl Pts',(-10.7027791449605,12.2,-1.96870212322088));
#267570=CARTESIAN_POINT('Ctrl Pts',(-10.7060989423993,12.2,-1.97051785785383));
#267571=CARTESIAN_POINT('Ctrl Pts',(-10.7094288220311,12.2,-1.97234633799039));
#267572=CARTESIAN_POINT('Ctrl Pts',(-10.7127587021165,12.2,-1.97417481837608));
#267573=CARTESIAN_POINT('Ctrl Pts',(-10.7160986645253,12.2,-1.97601604464519));
#267574=CARTESIAN_POINT('Ctrl Pts',(-10.7194485732644,12.2,-1.9778700383031));
#267575=CARTESIAN_POINT('Ctrl Pts',(-10.7227984815471,12.2,-1.9797240317084));
#267576=CARTESIAN_POINT('Ctrl Pts',(-10.7261583367035,12.2,-1.98159079284259));
#267577=CARTESIAN_POINT('Ctrl Pts',(-10.729528002483,12.2,-1.98347034485477));
#267578=CARTESIAN_POINT('Ctrl Pts',(-10.7328976687215,12.2,-1.98534989712303));
#267579=CARTESIAN_POINT('Ctrl Pts',(-10.7362771462287,12.2,-1.98724223897082));
#267580=CARTESIAN_POINT('Ctrl Pts',(-10.7396663017502,12.2,-1.98914739205982));
#267581=CARTESIAN_POINT('Ctrl Pts',(-10.7430554568099,12.2,-1.99105254488924));
#267582=CARTESIAN_POINT('Ctrl Pts',(-10.7464542883118,12.2,-1.99297050843982));
#267583=CARTESIAN_POINT('Ctrl Pts',(-10.7498626652548,12.2,-1.99490130505891));
#267584=CARTESIAN_POINT('Ctrl Pts',(-10.7532710426621,12.2,-1.99683210194107));
#267585=CARTESIAN_POINT('Ctrl Pts',(-10.7566889635401,12.2,-1.99877572959145));
#267586=CARTESIAN_POINT('Ctrl Pts',(-10.7601162983386,12.2,-2.00073221114336));
#267587=CARTESIAN_POINT('Ctrl Pts',(-10.7635436326702,12.2,-2.0026886924287));
#267588=CARTESIAN_POINT('Ctrl Pts',(-10.7669803790409,12.2,-2.00465802463765));
#267589=CARTESIAN_POINT('Ctrl Pts',(-10.7704264095417,12.2,-2.00664022946241));
#267590=CARTESIAN_POINT('Ctrl Pts',(-10.773872440512,12.2,-2.00862243455724));
#267591=CARTESIAN_POINT('Ctrl Pts',(-10.777327753005,12.2,-2.01061751139563));
#267592=CARTESIAN_POINT('Ctrl Pts',(-10.78079221975,12.2,-2.01262547967257));
#267593=CARTESIAN_POINT('Ctrl Pts',(-10.7842566860229,12.2,-2.01463344767593));
#267594=CARTESIAN_POINT('Ctrl Pts',(-10.7877303053996,12.2,-2.01665430669337));
#267595=CARTESIAN_POINT('Ctrl Pts',(-10.7912129504473,12.2,-2.01868807469245));
#267596=CARTESIAN_POINT('Ctrl Pts',(-10.7946955959695,12.2,-2.02072184296864));
#267597=CARTESIAN_POINT('Ctrl Pts',(-10.7981872667314,12.2,-2.02276852037937));
#267598=CARTESIAN_POINT('Ctrl Pts',(-10.8016878350333,12.2,-2.02482812599162));
#267599=CARTESIAN_POINT('Ctrl Pts',(-10.8051884033352,12.2,-2.02688773160387));
#267600=CARTESIAN_POINT('Ctrl Pts',(-10.8086978711993,12.2,-2.02896026407041));
#267601=CARTESIAN_POINT('Ctrl Pts',(-10.8122161100586,12.2,-2.03104574107428));
#267602=CARTESIAN_POINT('Ctrl Pts',(-10.8157343484386,12.2,-2.03313121779401));
#267603=CARTESIAN_POINT('Ctrl Pts',(-10.8192613591206,12.2,-2.03522963990326));
#267604=CARTESIAN_POINT('Ctrl Pts',(-10.8227970175143,12.2,-2.03734102324019));
#267605=CARTESIAN_POINT('Ctrl Pts',(-10.8263326763897,12.2,-2.03945240686481));
#267606=CARTESIAN_POINT('Ctrl Pts',(-10.8298769814559,12.2,-2.0415767519705));
#267607=CARTESIAN_POINT('Ctrl Pts',(-10.8334298103726,12.2,-2.04371407486609));
#267608=CARTESIAN_POINT('Ctrl Pts',(-10.8369826388052,12.2,-2.04585139747047));
#267609=CARTESIAN_POINT('Ctrl Pts',(-10.8405439902784,12.2,-2.04800169673705));
#267610=CARTESIAN_POINT('Ctrl Pts',(-10.8441137432083,12.2,-2.05016499128157));
#267611=CARTESIAN_POINT('Ctrl Pts',(-10.8485759347354,12.2,-2.05286910968329));
#267612=CARTESIAN_POINT('Ctrl Pts',(-10.8530512504606,12.2,-2.05559352996384));
#267613=CARTESIAN_POINT('Ctrl Pts',(-10.8575394540226,12.2,-2.05833828199014));
#267614=CARTESIAN_POINT('Ctrl Pts',(-10.8611300170679,12.2,-2.06053408373086));
#267615=CARTESIAN_POINT('Ctrl Pts',(-10.8647288282285,12.2,-2.06274289860748));
#267616=CARTESIAN_POINT('Ctrl Pts',(-10.8683357671481,12.2,-2.06496474139658));
#267617=CARTESIAN_POINT('Ctrl Pts',(-10.8719427055763,12.2,-2.06718658388294));
#267618=CARTESIAN_POINT('Ctrl Pts',(-10.8755577714756,12.2,-2.06942145178704));
#267619=CARTESIAN_POINT('Ctrl Pts',(-10.8791808446789,12.2,-2.07166936232466));
#267620=CARTESIAN_POINT('Ctrl Pts',(-10.8828039183759,12.2,-2.07391727316855));
#267621=CARTESIAN_POINT('Ctrl Pts',(-10.8864350008862,12.2,-2.07617822391079));
#267622=CARTESIAN_POINT('Ctrl Pts',(-10.8900739720448,12.2,-2.07845223153834));
#267623=CARTESIAN_POINT('Ctrl Pts',(-10.8937129427075,12.2,-2.08072623885605));
#267624=CARTESIAN_POINT('Ctrl Pts',(-10.8973598017395,12.2,-2.08301330084816));
#267625=CARTESIAN_POINT('Ctrl Pts',(-10.901014432218,12.2,-2.08531343027038));
#267626=CARTESIAN_POINT('Ctrl Pts',(-10.9046690631944,12.2,-2.087613560006));
#267627=CARTESIAN_POINT('Ctrl Pts',(-10.9083314651191,12.2,-2.08992675893207));
#267628=CARTESIAN_POINT('Ctrl Pts',(-10.9120015220418,12.2,-2.09225303844859));
#267629=CARTESIAN_POINT('Ctrl Pts',(-10.9156715784645,12.2,-2.09457931764816));
#267630=CARTESIAN_POINT('Ctrl Pts',(-10.9193492880053,12.2,-2.09691867683739));
#267631=CARTESIAN_POINT('Ctrl Pts',(-10.9230345366653,12.2,-2.09927113015035));
#267632=CARTESIAN_POINT('Ctrl Pts',(-10.9267197858274,12.2,-2.10162358378383));
#267633=CARTESIAN_POINT('Ctrl Pts',(-10.9304125733227,12.2,-2.10398913007794));
#267634=CARTESIAN_POINT('Ctrl Pts',(-10.9341127843026,12.2,-2.10636778048621));
#267635=CARTESIAN_POINT('Ctrl Pts',(-10.9378129947784,12.2,-2.10874643057038));
#267636=CARTESIAN_POINT('Ctrl Pts',(-10.9415206274026,12.2,-2.11113818704638));
#267637=CARTESIAN_POINT('Ctrl Pts',(-10.945235569876,12.2,-2.11354305834844));
#267638=CARTESIAN_POINT('Ctrl Pts',(-10.9489505128555,12.2,-2.11594792997817));
#267639=CARTESIAN_POINT('Ctrl Pts',(-10.9526727650712,12.2,-2.11836591876081));
#267640=CARTESIAN_POINT('Ctrl Pts',(-10.9564022127359,12.2,-2.12079703429329));
#267641=CARTESIAN_POINT('Ctrl Pts',(-10.9591992982303,12.2,-2.12262037077703));
#267642=CARTESIAN_POINT('Ctrl Pts',(-10.96200043152,12.2,-2.12445109042344));
#267643=CARTESIAN_POINT('Ctrl Pts',(-10.9648055645141,12.2,-2.12628919848996));
#267644=CARTESIAN_POINT('Ctrl Pts',(-10.9676106975083,12.2,-2.12812730655649));
#267645=CARTESIAN_POINT('Ctrl Pts',(-10.9704198296627,12.2,-2.12997280354942));
#267646=CARTESIAN_POINT('Ctrl Pts',(-10.9732329156851,12.2,-2.13182569302312));
#267647=CARTESIAN_POINT('Ctrl Pts',(-10.9760460017076,12.2,-2.13367858249682));
#267648=CARTESIAN_POINT('Ctrl Pts',(-10.9788630410381,12.2,-2.13553886364502));
#267649=CARTESIAN_POINT('Ctrl Pts',(-10.9816839856017,12.2,-2.13740654257615));
#267650=CARTESIAN_POINT('Ctrl Pts',(-10.9845049306779,12.2,-2.13927422184658));
#267651=CARTESIAN_POINT('Ctrl Pts',(-10.9873297817884,12.2,-2.14114929813576));
#267652=CARTESIAN_POINT('Ctrl Pts',(-10.9901584918667,12.2,-2.14303177445202));
#267653=CARTESIAN_POINT('Ctrl Pts',(-10.9929872014311,12.2,-2.14491425042629));
#267654=CARTESIAN_POINT('Ctrl Pts',(-10.9958197711097,12.2,-2.14680412655707));
#267655=CARTESIAN_POINT('Ctrl Pts',(-10.9986561528155,12.2,-2.14870140816711));
#267656=CARTESIAN_POINT('Ctrl Pts',(-11.0014925345213,12.2,-2.15059868977715));
#267657=CARTESIAN_POINT('Ctrl Pts',(-11.0043327282631,12.2,-2.15250337611066));
#267658=CARTESIAN_POINT('Ctrl Pts',(-11.0071766892851,12.2,-2.15441547016684));
#267659=CARTESIAN_POINT('Ctrl Pts',(-11.0109686371422,12.2,-2.15696492879262));
#267660=CARTESIAN_POINT('Ctrl Pts',(-11.0147672805285,12.2,-2.15952755784075));
#267661=CARTESIAN_POINT('Ctrl Pts',(-11.0185725116612,12.2,-2.16210336629549));
#267662=CARTESIAN_POINT('Ctrl Pts',(-11.0214264356588,12.2,-2.16403522307523));
#267663=CARTESIAN_POINT('Ctrl Pts',(-11.0242840643241,12.2,-2.16597449195708));
#267664=CARTESIAN_POINT('Ctrl Pts',(-11.0271453534071,12.2,-2.16792117865768));
#267665=CARTESIAN_POINT('Ctrl Pts',(-11.0300066419703,12.2,-2.16986786500463));
#267666=CARTESIAN_POINT('Ctrl Pts',(-11.0328715910656,12.2,-2.17182196663529));
#267667=CARTESIAN_POINT('Ctrl Pts',(-11.0357401538134,12.2,-2.17378348912121));
#267668=CARTESIAN_POINT('Ctrl Pts',(-11.0386087165612,12.2,-2.17574501160713));
#267669=CARTESIAN_POINT('Ctrl Pts',(-11.041480893201,12.2,-2.17771395327));
#267670=CARTESIAN_POINT('Ctrl Pts',(-11.0443566393052,12.2,-2.17969031824051));
#267671=CARTESIAN_POINT('Ctrl Pts',(-11.0472323854094,12.2,-2.18166668321103));
#267672=CARTESIAN_POINT('Ctrl Pts',(-11.0501117016214,12.2,-2.18365047098897));
#267673=CARTESIAN_POINT('Ctrl Pts',(-11.0529945412667,12.2,-2.18564168495829));
#267674=CARTESIAN_POINT('Ctrl Pts',(-11.055877380912,12.2,-2.18763289892761));
#267675=CARTESIAN_POINT('Ctrl Pts',(-11.0587637458904,12.2,-2.18963153852162));
#267676=CARTESIAN_POINT('Ctrl Pts',(-11.0616535904518,12.2,-2.19163760703143));
#267677=CARTESIAN_POINT('Ctrl Pts',(-11.0645434350131,12.2,-2.19364367554123));
#267678=CARTESIAN_POINT('Ctrl Pts',(-11.0674367584672,12.2,-2.19565717373235));
#267679=CARTESIAN_POINT('Ctrl Pts',(-11.070333518173,12.2,-2.19767810334237));
#267680=CARTESIAN_POINT('Ctrl Pts',(-11.0732302778787,12.2,-2.19969903295239));
#267681=CARTESIAN_POINT('Ctrl Pts',(-11.0761304727397,12.2,-2.20172739428115));
#267682=CARTESIAN_POINT('Ctrl Pts',(-11.0790340588421,12.2,-2.2037631897895));
#267683=CARTESIAN_POINT('Ctrl Pts',(-11.0819376454719,12.2,-2.20579898566768));
#267684=CARTESIAN_POINT('Ctrl Pts',(-11.0848446236777,12.2,-2.20784221679796));
#267685=CARTESIAN_POINT('Ctrl Pts',(-11.0877549488512,12.2,-2.20989288372202));
#267686=CARTESIAN_POINT('Ctrl Pts',(-11.0906652734959,12.2,-2.21194355027354));
#267687=CARTESIAN_POINT('Ctrl Pts',(-11.0935789464071,12.2,-2.2140016547163));
#267688=CARTESIAN_POINT('Ctrl Pts',(-11.0964959220514,12.2,-2.2160671977669));
#267689=CARTESIAN_POINT('Ctrl Pts',(-11.0994128976957,12.2,-2.2181327408175));
#267690=CARTESIAN_POINT('Ctrl Pts',(-11.1023331776563,12.2,-2.22020572342555));
#267691=CARTESIAN_POINT('Ctrl Pts',(-11.1052567172584,12.2,-2.22228614747496));
#267692=CARTESIAN_POINT('Ctrl Pts',(-11.1081802568605,12.2,-2.22436657152438));
#267693=CARTESIAN_POINT('Ctrl Pts',(-11.1111070560874,12.2,-2.22645443796513));
#267694=CARTESIAN_POINT('Ctrl Pts',(-11.1140370731474,12.2,-2.22854974751337));
#267695=CARTESIAN_POINT('Ctrl Pts',(-11.1169670902073,12.2,-2.2306450570616));
#267696=CARTESIAN_POINT('Ctrl Pts',(-11.1199003244256,12.2,-2.23274781174721));
#267697=CARTESIAN_POINT('Ctrl Pts',(-11.1228367322153,12.2,-2.23485801135843));
#267698=CARTESIAN_POINT('Ctrl Pts',(-11.1257731400049,12.2,-2.23696821096966));
#267699=CARTESIAN_POINT('Ctrl Pts',(-11.1287127222325,12.2,-2.2390858568816));
#267700=CARTESIAN_POINT('Ctrl Pts',(-11.1316554353335,12.2,-2.24121095034504));
#267701=CARTESIAN_POINT('Ctrl Pts',(-11.1345981489691,12.2,-2.24333604419453));
#267702=CARTESIAN_POINT('Ctrl Pts',(-11.1375439935806,12.2,-2.24546858538778));
#267703=CARTESIAN_POINT('Ctrl Pts',(-11.1404929271762,12.2,-2.24760857719981));
#267704=CARTESIAN_POINT('Ctrl Pts',(-11.1434418602362,12.2,-2.24974856862307));
#267705=CARTESIAN_POINT('Ctrl Pts',(-11.1463938816293,12.2,-2.25189600957929));
#267706=CARTESIAN_POINT('Ctrl Pts',(-11.1493489488555,12.2,-2.25405090200164));
#267707=CARTESIAN_POINT('Ctrl Pts',(-11.1523040160817,12.2,-2.25620579442399));
#267708=CARTESIAN_POINT('Ctrl Pts',(-11.1552621307969,12.2,-2.25836813808755));
#267709=CARTESIAN_POINT('Ctrl Pts',(-11.1582232489527,12.2,-2.2605379350186));
#267710=CARTESIAN_POINT('Ctrl Pts',(-11.1611843671086,12.2,-2.26270773194965));
#267711=CARTESIAN_POINT('Ctrl Pts',(-11.164148489525,12.2,-2.26488498156748));
#267712=CARTESIAN_POINT('Ctrl Pts',(-11.167115574514,12.2,-2.26706968649798));
#267713=CARTESIAN_POINT('Ctrl Pts',(-11.170082659503,12.2,-2.26925439142848));
#267714=CARTESIAN_POINT('Ctrl Pts',(-11.1730527048343,12.2,-2.27144655127423));
#267715=CARTESIAN_POINT('Ctrl Pts',(-11.1760256714344,12.2,-2.273646166277));
#267716=CARTESIAN_POINT('Ctrl Pts',(-11.1789986380344,12.2,-2.27584578127977));
#267717=CARTESIAN_POINT('Ctrl Pts',(-11.1819745254426,12.2,-2.27805285281535));
#267718=CARTESIAN_POINT('Ctrl Pts',(-11.1849532921257,12.2,-2.28026738127554));
#267719=CARTESIAN_POINT('Ctrl Pts',(-11.1879320593499,12.2,-2.28248191013803));
#267720=CARTESIAN_POINT('Ctrl Pts',(-11.1909137074332,12.2,-2.28470389609429));
#267721=CARTESIAN_POINT('Ctrl Pts',(-11.1938981922006,12.2,-2.28693334050264));
#267722=CARTESIAN_POINT('Ctrl Pts',(-11.1968826764259,12.2,-2.28916278450598));
#267723=CARTESIAN_POINT('Ctrl Pts',(-11.1998699989042,12.2,-2.29139968778616));
#267724=CARTESIAN_POINT('Ctrl Pts',(-11.2028601157786,12.2,-2.29364404990093));
#267725=CARTESIAN_POINT('Ctrl Pts',(-11.2068469380967,12.2,-2.29663653258472));
#267726=CARTESIAN_POINT('Ctrl Pts',(-11.2108387281032,12.2,-2.29964227782317));
#267727=CARTESIAN_POINT('Ctrl Pts',(-11.214835396165,12.2,-2.30266128501995));
#267728=CARTESIAN_POINT('Ctrl Pts',(-11.2178328973476,12.2,-2.30492554052038));
#267729=CARTESIAN_POINT('Ctrl Pts',(-11.2208331432215,12.2,-2.30719725682027));
#267730=CARTESIAN_POINT('Ctrl Pts',(-11.2238360943204,12.2,-2.30947643523644));
#267731=CARTESIAN_POINT('Ctrl Pts',(-11.2268390459648,12.2,-2.31175561406666));
#267732=CARTESIAN_POINT('Ctrl Pts',(-11.2298447030183,12.2,-2.31404225441566));
#267733=CARTESIAN_POINT('Ctrl Pts',(-11.2328530156225,12.2,-2.31633635725008));
#267734=CARTESIAN_POINT('Ctrl Pts',(-11.2358613276802,12.2,-2.31863045966774));
#267735=CARTESIAN_POINT('Ctrl Pts',(-11.2388722956251,12.2,-2.32093202439778));
#267736=CARTESIAN_POINT('Ctrl Pts',(-11.2418858740831,12.2,-2.32324105243011));
#267737=CARTESIAN_POINT('Ctrl Pts',(-11.2448994525412,12.2,-2.32555008046245));
#267738=CARTESIAN_POINT('Ctrl Pts',(-11.2479156413857,12.2,-2.32786657213309));
#267739=CARTESIAN_POINT('Ctrl Pts',(-11.2509344236132,12.2,-2.33019052657526));
#267740=CARTESIAN_POINT('Ctrl Pts',(-11.2539532058406,12.2,-2.33251448101743));
#267741=CARTESIAN_POINT('Ctrl Pts',(-11.2569745784507,12.2,-2.33484589757511));
#267742=CARTESIAN_POINT('Ctrl Pts',(-11.2599985490001,12.2,-2.33718477800001));
#267743=CARTESIAN_POINT('Ctrl Pts',(-11.1757778680001,15.2,-2.71145515300002));
#267744=CARTESIAN_POINT('Ctrl Pts',(-11.1757778680001,11.6,-2.71145515300002));
#267745=CARTESIAN_POINT('Ctrl Pts',(-11.1750309950001,15.2,-2.71161876900001));
#267746=CARTESIAN_POINT('Ctrl Pts',(-11.1750309950001,11.6,-2.71161876900001));
#267747=CARTESIAN_POINT('Ctrl Pts',(-11.1735376180001,15.2,-2.71194562400002));
#267748=CARTESIAN_POINT('Ctrl Pts',(-11.1735376180001,11.6,-2.71194562400002));
#267749=CARTESIAN_POINT('Ctrl Pts',(-11.1712986600001,15.2,-2.71243478000001));
#267750=CARTESIAN_POINT('Ctrl Pts',(-11.1712986600001,11.6,-2.71243478000002));
#267751=CARTESIAN_POINT('Ctrl Pts',(-11.1683155990001,15.2,-2.71308473500001));
#267752=CARTESIAN_POINT('Ctrl Pts',(-11.1683155990001,11.6,-2.71308473500001));
#267753=CARTESIAN_POINT('Ctrl Pts',(-11.1645904650001,15.2,-2.71389342400001));
#267754=CARTESIAN_POINT('Ctrl Pts',(-11.1645904650001,11.6,-2.71389342400001));
#267755=CARTESIAN_POINT('Ctrl Pts',(-11.1608690250001,15.2,-2.71469835800001));
#267756=CARTESIAN_POINT('Ctrl Pts',(-11.1608690250001,11.6,-2.71469835800001));
#267757=CARTESIAN_POINT('Ctrl Pts',(-11.1571512810001,15.2,-2.71549953800001));
#267758=CARTESIAN_POINT('Ctrl Pts',(-11.1571512810001,11.6,-2.71549953800002));
#267759=CARTESIAN_POINT('Ctrl Pts',(-11.1534372360001,15.2,-2.71629696600002));
#267760=CARTESIAN_POINT('Ctrl Pts',(-11.1534372360001,11.6,-2.71629696600002));
#267761=CARTESIAN_POINT('Ctrl Pts',(-11.1497268980001,15.2,-2.71709064400001));
#267762=CARTESIAN_POINT('Ctrl Pts',(-11.1497268980001,11.6,-2.71709064400001));
#267763=CARTESIAN_POINT('Ctrl Pts',(-11.1460202710001,15.2,-2.71788057600002));
#267764=CARTESIAN_POINT('Ctrl Pts',(-11.1460202710001,11.6,-2.71788057600002));
#267765=CARTESIAN_POINT('Ctrl Pts',(-11.1423173660001,15.2,-2.71866676600002));
#267766=CARTESIAN_POINT('Ctrl Pts',(-11.1423173660001,11.6,-2.71866676600002));
#267767=CARTESIAN_POINT('Ctrl Pts',(-11.1386181920001,15.2,-2.71944921800001));
#267768=CARTESIAN_POINT('Ctrl Pts',(-11.1386181920001,11.6,-2.71944921800001));
#267769=CARTESIAN_POINT('Ctrl Pts',(-11.1349227590001,15.2,-2.72022793900002));
#267770=CARTESIAN_POINT('Ctrl Pts',(-11.1349227590001,11.6,-2.72022793900002));
#267771=CARTESIAN_POINT('Ctrl Pts',(-11.1312310760001,15.2,-2.72100293300001));
#267772=CARTESIAN_POINT('Ctrl Pts',(-11.1312310760001,11.6,-2.72100293300001));
#267773=CARTESIAN_POINT('Ctrl Pts',(-11.1275431540001,15.2,-2.72177420400002));
#267774=CARTESIAN_POINT('Ctrl Pts',(-11.1275431540001,11.6,-2.72177420400002));
#267775=CARTESIAN_POINT('Ctrl Pts',(-11.1238590000001,15.2,-2.72254175700001));
#267776=CARTESIAN_POINT('Ctrl Pts',(-11.1238590000001,11.6,-2.72254175700001));
#267777=CARTESIAN_POINT('Ctrl Pts',(-11.1201786230001,15.2,-2.72330559600002));
#267778=CARTESIAN_POINT('Ctrl Pts',(-11.1201786230001,11.6,-2.72330559600002));
#267779=CARTESIAN_POINT('Ctrl Pts',(-11.1165020290001,15.2,-2.72406572300001));
#267780=CARTESIAN_POINT('Ctrl Pts',(-11.1165020290001,11.6,-2.72406572300001));
#267781=CARTESIAN_POINT('Ctrl Pts',(-11.1128292270001,15.2,-2.72482214500001));
#267782=CARTESIAN_POINT('Ctrl Pts',(-11.1128292270001,11.6,-2.72482214500001));
#267783=CARTESIAN_POINT('Ctrl Pts',(-11.1091602230001,15.2,-2.72557486300002));
#267784=CARTESIAN_POINT('Ctrl Pts',(-11.1091602230001,11.6,-2.72557486300002));
#267785=CARTESIAN_POINT('Ctrl Pts',(-11.1054950240001,15.2,-2.72632388100002));
#267786=CARTESIAN_POINT('Ctrl Pts',(-11.1054950240001,11.6,-2.72632388100002));
#267787=CARTESIAN_POINT('Ctrl Pts',(-11.1018336410001,15.2,-2.72706920300001));
#267788=CARTESIAN_POINT('Ctrl Pts',(-11.1018336410001,11.6,-2.72706920300001));
#267789=CARTESIAN_POINT('Ctrl Pts',(-11.0981760790001,15.2,-2.72781083400002));
#267790=CARTESIAN_POINT('Ctrl Pts',(-11.0981760790001,11.6,-2.72781083400002));
#267791=CARTESIAN_POINT('Ctrl Pts',(-11.0945223470001,15.2,-2.72854877900001));
#267792=CARTESIAN_POINT('Ctrl Pts',(-11.0945223470001,11.6,-2.72854877900001));
#267793=CARTESIAN_POINT('Ctrl Pts',(-11.0908724560001,15.2,-2.72928304000001));
#267794=CARTESIAN_POINT('Ctrl Pts',(-11.0908724560001,11.6,-2.72928304000001));
#267795=CARTESIAN_POINT('Ctrl Pts',(-11.0872264110001,15.2,-2.73001362300001));
#267796=CARTESIAN_POINT('Ctrl Pts',(-11.0872264110001,11.6,-2.73001362300001));
#267797=CARTESIAN_POINT('Ctrl Pts',(-11.0835842240001,15.2,-2.73074053200002));
#267798=CARTESIAN_POINT('Ctrl Pts',(-11.0835842240001,11.6,-2.73074053200002));
#267799=CARTESIAN_POINT('Ctrl Pts',(-11.0799458990001,15.2,-2.73146377200002));
#267800=CARTESIAN_POINT('Ctrl Pts',(-11.0799458990001,11.6,-2.73146377200002));
#267801=CARTESIAN_POINT('Ctrl Pts',(-11.0763114490001,15.2,-2.73218334500001));
#267802=CARTESIAN_POINT('Ctrl Pts',(-11.0763114490001,11.6,-2.73218334500001));
#267803=CARTESIAN_POINT('Ctrl Pts',(-11.0726808780001,15.2,-2.73289925600002));
#267804=CARTESIAN_POINT('Ctrl Pts',(-11.0726808780001,11.6,-2.73289925600002));
#267805=CARTESIAN_POINT('Ctrl Pts',(-11.0690541960001,15.2,-2.73361151100001));
#267806=CARTESIAN_POINT('Ctrl Pts',(-11.0690541960001,11.6,-2.73361151100001));
#267807=CARTESIAN_POINT('Ctrl Pts',(-11.0654314110001,15.2,-2.73432011200001));
#267808=CARTESIAN_POINT('Ctrl Pts',(-11.0654314110001,11.6,-2.73432011200002));
#267809=CARTESIAN_POINT('Ctrl Pts',(-11.0618125300001,15.2,-2.73502506300002));
#267810=CARTESIAN_POINT('Ctrl Pts',(-11.0618125300001,11.6,-2.73502506300002));
#267811=CARTESIAN_POINT('Ctrl Pts',(-11.0581975630001,15.2,-2.73572637000001));
#267812=CARTESIAN_POINT('Ctrl Pts',(-11.0581975630001,11.6,-2.73572637000001));
#267813=CARTESIAN_POINT('Ctrl Pts',(-11.0545865170001,15.2,-2.73642403700002));
#267814=CARTESIAN_POINT('Ctrl Pts',(-11.0545865170001,11.6,-2.73642403700002));
#267815=CARTESIAN_POINT('Ctrl Pts',(-11.0509794010001,15.2,-2.73711806700002));
#267816=CARTESIAN_POINT('Ctrl Pts',(-11.0509794010001,11.6,-2.73711806700002));
#267817=CARTESIAN_POINT('Ctrl Pts',(-11.0473762230001,15.2,-2.73780846600001));
#267818=CARTESIAN_POINT('Ctrl Pts',(-11.0473762230001,11.6,-2.73780846600001));
#267819=CARTESIAN_POINT('Ctrl Pts',(-11.0437769920001,15.2,-2.73849523700001));
#267820=CARTESIAN_POINT('Ctrl Pts',(-11.0437769920001,11.6,-2.73849523700001));
#267821=CARTESIAN_POINT('Ctrl Pts',(-11.0401817150001,15.2,-2.73917838500001));
#267822=CARTESIAN_POINT('Ctrl Pts',(-11.0401817150001,11.6,-2.73917838500001));
#267823=CARTESIAN_POINT('Ctrl Pts',(-11.0365904010001,15.2,-2.73985791400001));
#267824=CARTESIAN_POINT('Ctrl Pts',(-11.0365904010001,11.6,-2.73985791400001));
#267825=CARTESIAN_POINT('Ctrl Pts',(-11.0330030590001,15.2,-2.74053382800002));
#267826=CARTESIAN_POINT('Ctrl Pts',(-11.0330030590001,11.6,-2.74053382800002));
#267827=CARTESIAN_POINT('Ctrl Pts',(-11.0294196970001,15.2,-2.74120613200001));
#267828=CARTESIAN_POINT('Ctrl Pts',(-11.0294196970001,11.6,-2.74120613200001));
#267829=CARTESIAN_POINT('Ctrl Pts',(-11.0258403220001,15.2,-2.74187483000001));
#267830=CARTESIAN_POINT('Ctrl Pts',(-11.0258403220001,11.6,-2.74187483000001));
#267831=CARTESIAN_POINT('Ctrl Pts',(-11.0222649450001,15.2,-2.74253992800002));
#267832=CARTESIAN_POINT('Ctrl Pts',(-11.0222649450001,11.6,-2.74253992800002));
#267833=CARTESIAN_POINT('Ctrl Pts',(-11.0186935710001,15.2,-2.74320142800001));
#267834=CARTESIAN_POINT('Ctrl Pts',(-11.0186935710001,11.6,-2.74320142800002));
#267835=CARTESIAN_POINT('Ctrl Pts',(-11.0151262110001,15.2,-2.74385933600001));
#267836=CARTESIAN_POINT('Ctrl Pts',(-11.0151262110001,11.6,-2.74385933600001));
#267837=CARTESIAN_POINT('Ctrl Pts',(-11.0115628720001,15.2,-2.74451365600001));
#267838=CARTESIAN_POINT('Ctrl Pts',(-11.0115628720001,11.6,-2.74451365600001));
#267839=CARTESIAN_POINT('Ctrl Pts',(-11.0080035640001,15.2,-2.74516439200001));
#267840=CARTESIAN_POINT('Ctrl Pts',(-11.0080035640001,11.6,-2.74516439200002));
#267841=CARTESIAN_POINT('Ctrl Pts',(-11.0044482940001,15.2,-2.74581155000002));
#267842=CARTESIAN_POINT('Ctrl Pts',(-11.0044482940001,11.6,-2.74581155000002));
#267843=CARTESIAN_POINT('Ctrl Pts',(-11.0008970700001,15.2,-2.74645513200001));
#267844=CARTESIAN_POINT('Ctrl Pts',(-11.0008970700001,11.6,-2.74645513200001));
#267845=CARTESIAN_POINT('Ctrl Pts',(-10.9973499030001,15.2,-2.74709514500001));
#267846=CARTESIAN_POINT('Ctrl Pts',(-10.9973499030001,11.6,-2.74709514500001));
#267847=CARTESIAN_POINT('Ctrl Pts',(-10.9938067980001,15.2,-2.74773159100001));
#267848=CARTESIAN_POINT('Ctrl Pts',(-10.9938067980001,11.6,-2.74773159100001));
#267849=CARTESIAN_POINT('Ctrl Pts',(-10.9902677660001,15.2,-2.74836447800002));
#267850=CARTESIAN_POINT('Ctrl Pts',(-10.9902677660001,11.6,-2.74836447800002));
#267851=CARTESIAN_POINT('Ctrl Pts',(-10.9867328140001,15.2,-2.74899380700001));
#267852=CARTESIAN_POINT('Ctrl Pts',(-10.9867328140001,11.6,-2.74899380700001));
#267853=CARTESIAN_POINT('Ctrl Pts',(-10.9832019520001,15.2,-2.74961958600001));
#267854=CARTESIAN_POINT('Ctrl Pts',(-10.9832019520001,11.6,-2.74961958600001));
#267855=CARTESIAN_POINT('Ctrl Pts',(-10.9796751870001,15.2,-2.75024181600001));
#267856=CARTESIAN_POINT('Ctrl Pts',(-10.9796751870001,11.6,-2.75024181600001));
#267857=CARTESIAN_POINT('Ctrl Pts',(-10.9761525290001,15.2,-2.75086050400001));
#267858=CARTESIAN_POINT('Ctrl Pts',(-10.9761525290001,11.6,-2.75086050400001));
#267859=CARTESIAN_POINT('Ctrl Pts',(-10.9726339840001,15.2,-2.75147565300002));
#267860=CARTESIAN_POINT('Ctrl Pts',(-10.9726339840001,11.6,-2.75147565300002));
#267861=CARTESIAN_POINT('Ctrl Pts',(-10.9691195640001,15.2,-2.75208727000001));
#267862=CARTESIAN_POINT('Ctrl Pts',(-10.9691195640001,11.6,-2.75208727000001));
#267863=CARTESIAN_POINT('Ctrl Pts',(-10.9656092750001,15.2,-2.75269535800001));
#267864=CARTESIAN_POINT('Ctrl Pts',(-10.9656092750001,11.6,-2.75269535800002));
#267865=CARTESIAN_POINT('Ctrl Pts',(-10.9621031260001,15.2,-2.75329992100001));
#267866=CARTESIAN_POINT('Ctrl Pts',(-10.9621031260001,11.6,-2.75329992100001));
#267867=CARTESIAN_POINT('Ctrl Pts',(-10.9586011260001,15.2,-2.75390096500002));
#267868=CARTESIAN_POINT('Ctrl Pts',(-10.9586011260001,11.6,-2.75390096500002));
#267869=CARTESIAN_POINT('Ctrl Pts',(-10.9551032830001,15.2,-2.75449849500002));
#267870=CARTESIAN_POINT('Ctrl Pts',(-10.9551032830001,11.6,-2.75449849500002));
#267871=CARTESIAN_POINT('Ctrl Pts',(-10.9516096070001,15.2,-2.75509251400001));
#267872=CARTESIAN_POINT('Ctrl Pts',(-10.9516096070001,11.6,-2.75509251400001));
#267873=CARTESIAN_POINT('Ctrl Pts',(-10.9481201050001,15.2,-2.75568302700002));
#267874=CARTESIAN_POINT('Ctrl Pts',(-10.9481201050001,11.6,-2.75568302700002));
#267875=CARTESIAN_POINT('Ctrl Pts',(-10.9446347860001,15.2,-2.75627004100001));
#267876=CARTESIAN_POINT('Ctrl Pts',(-10.9446347860001,11.6,-2.75627004100001));
#267877=CARTESIAN_POINT('Ctrl Pts',(-10.9411536590001,15.2,-2.75685355800002));
#267878=CARTESIAN_POINT('Ctrl Pts',(-10.9411536590001,11.6,-2.75685355800002));
#267879=CARTESIAN_POINT('Ctrl Pts',(-10.9376767320001,15.2,-2.75743358500002));
#267880=CARTESIAN_POINT('Ctrl Pts',(-10.9376767320001,11.6,-2.75743358500002));
#267881=CARTESIAN_POINT('Ctrl Pts',(-10.9342040160001,15.2,-2.75801012600001));
#267882=CARTESIAN_POINT('Ctrl Pts',(-10.9342040160001,11.6,-2.75801012600001));
#267883=CARTESIAN_POINT('Ctrl Pts',(-10.9307355160001,15.2,-2.75858318400001));
#267884=CARTESIAN_POINT('Ctrl Pts',(-10.9307355160001,11.6,-2.75858318400001));
#267885=CARTESIAN_POINT('Ctrl Pts',(-10.9272712420001,15.2,-2.75915276600001));
#267886=CARTESIAN_POINT('Ctrl Pts',(-10.9272712420001,11.6,-2.75915276600002));
#267887=CARTESIAN_POINT('Ctrl Pts',(-10.9238112040001,15.2,-2.75971887600001));
#267888=CARTESIAN_POINT('Ctrl Pts',(-10.9238112040001,11.6,-2.75971887600001));
#267889=CARTESIAN_POINT('Ctrl Pts',(-10.9203554100001,15.2,-2.76028151900002));
#267890=CARTESIAN_POINT('Ctrl Pts',(-10.9203554100001,11.6,-2.76028151900002));
#267891=CARTESIAN_POINT('Ctrl Pts',(-10.9169038680001,15.2,-2.76084070000001));
#267892=CARTESIAN_POINT('Ctrl Pts',(-10.9169038680001,11.6,-2.76084070000001));
#267893=CARTESIAN_POINT('Ctrl Pts',(-10.9134565880001,15.2,-2.76139642400001));
#267894=CARTESIAN_POINT('Ctrl Pts',(-10.9134565880001,11.6,-2.76139642400001));
#267895=CARTESIAN_POINT('Ctrl Pts',(-10.9100135780001,15.2,-2.76194869600001));
#267896=CARTESIAN_POINT('Ctrl Pts',(-10.9100135780001,11.6,-2.76194869600001));
#267897=CARTESIAN_POINT('Ctrl Pts',(-10.9065748460001,15.2,-2.76249752000002));
#267898=CARTESIAN_POINT('Ctrl Pts',(-10.9065748460001,11.6,-2.76249752000002));
#267899=CARTESIAN_POINT('Ctrl Pts',(-10.9031404020001,15.2,-2.76304290100001));
#267900=CARTESIAN_POINT('Ctrl Pts',(-10.9031404020001,11.6,-2.76304290100002));
#267901=CARTESIAN_POINT('Ctrl Pts',(-10.8997102540001,15.2,-2.76358484600001));
#267902=CARTESIAN_POINT('Ctrl Pts',(-10.8997102540001,11.6,-2.76358484600001));
#267903=CARTESIAN_POINT('Ctrl Pts',(-10.8962844110001,15.2,-2.76412335800002));
#267904=CARTESIAN_POINT('Ctrl Pts',(-10.8962844110001,11.6,-2.76412335800002));
#267905=CARTESIAN_POINT('Ctrl Pts',(-10.8928628820001,15.2,-2.76465844200001));
#267906=CARTESIAN_POINT('Ctrl Pts',(-10.8928628820001,11.6,-2.76465844200001));
#267907=CARTESIAN_POINT('Ctrl Pts',(-10.8894456750001,15.2,-2.76519010300001));
#267908=CARTESIAN_POINT('Ctrl Pts',(-10.8894456750001,11.6,-2.76519010300001));
#267909=CARTESIAN_POINT('Ctrl Pts',(-10.8860328000001,15.2,-2.76571834600002));
#267910=CARTESIAN_POINT('Ctrl Pts',(-10.8860328000001,11.6,-2.76571834600002));
#267911=CARTESIAN_POINT('Ctrl Pts',(-10.8826242650001,15.2,-2.76624317800001));
#267912=CARTESIAN_POINT('Ctrl Pts',(-10.8826242650001,11.6,-2.76624317800001));
#267913=CARTESIAN_POINT('Ctrl Pts',(-10.8792200800001,15.2,-2.76676460200001));
#267914=CARTESIAN_POINT('Ctrl Pts',(-10.8792200800001,11.6,-2.76676460200001));
#267915=CARTESIAN_POINT('Ctrl Pts',(-10.8758202520001,15.2,-2.76728262200002));
#267916=CARTESIAN_POINT('Ctrl Pts',(-10.8758202520001,11.6,-2.76728262200002));
#267917=CARTESIAN_POINT('Ctrl Pts',(-10.8724247920001,15.2,-2.76779724700001));
#267918=CARTESIAN_POINT('Ctrl Pts',(-10.8724247920001,11.6,-2.76779724700001));
#267919=CARTESIAN_POINT('Ctrl Pts',(-10.8690337060001,15.2,-2.76830847900001));
#267920=CARTESIAN_POINT('Ctrl Pts',(-10.8690337060001,11.6,-2.76830847900001));
#267921=CARTESIAN_POINT('Ctrl Pts',(-10.8656470060001,15.2,-2.76881632300002));
#267922=CARTESIAN_POINT('Ctrl Pts',(-10.8656470060001,11.6,-2.76881632300002));
#267923=CARTESIAN_POINT('Ctrl Pts',(-10.8622646980001,15.2,-2.76932078500002));
#267924=CARTESIAN_POINT('Ctrl Pts',(-10.8622646980001,11.6,-2.76932078500002));
#267925=CARTESIAN_POINT('Ctrl Pts',(-10.8588867940001,15.2,-2.76982187100002));
#267926=CARTESIAN_POINT('Ctrl Pts',(-10.8588867940001,11.6,-2.76982187100002));
#267927=CARTESIAN_POINT('Ctrl Pts',(-10.8555133010001,15.2,-2.77031958400002));
#267928=CARTESIAN_POINT('Ctrl Pts',(-10.8555133010001,11.6,-2.77031958400002));
#267929=CARTESIAN_POINT('Ctrl Pts',(-10.8521442280001,15.2,-2.77081393100001));
#267930=CARTESIAN_POINT('Ctrl Pts',(-10.8521442280001,11.6,-2.77081393100001));
#267931=CARTESIAN_POINT('Ctrl Pts',(-10.8487795840001,15.2,-2.77130491700001));
#267932=CARTESIAN_POINT('Ctrl Pts',(-10.8487795840001,11.6,-2.77130491700001));
#267933=CARTESIAN_POINT('Ctrl Pts',(-10.8454193790001,15.2,-2.77179254700001));
#267934=CARTESIAN_POINT('Ctrl Pts',(-10.8454193790001,11.6,-2.77179254700001));
#267935=CARTESIAN_POINT('Ctrl Pts',(-10.8420636210001,15.2,-2.77227682600001));
#267936=CARTESIAN_POINT('Ctrl Pts',(-10.8420636210001,11.6,-2.77227682600001));
#267937=CARTESIAN_POINT('Ctrl Pts',(-10.8387123200001,15.2,-2.77275775900002));
#267938=CARTESIAN_POINT('Ctrl Pts',(-10.8387123200001,11.6,-2.77275775900002));
#267939=CARTESIAN_POINT('Ctrl Pts',(-10.8353654830001,15.2,-2.77323535200001));
#267940=CARTESIAN_POINT('Ctrl Pts',(-10.8353654830001,11.6,-2.77323535200001));
#267941=CARTESIAN_POINT('Ctrl Pts',(-10.8320231210001,15.2,-2.77370961000001));
#267942=CARTESIAN_POINT('Ctrl Pts',(-10.8320231210001,11.6,-2.77370961000001));
#267943=CARTESIAN_POINT('Ctrl Pts',(-10.8286852410001,15.2,-2.77418053700002));
#267944=CARTESIAN_POINT('Ctrl Pts',(-10.8286852410001,11.6,-2.77418053700002));
#267945=CARTESIAN_POINT('Ctrl Pts',(-10.8253518550001,15.2,-2.77464814100002));
#267946=CARTESIAN_POINT('Ctrl Pts',(-10.8253518550001,11.6,-2.77464814100002));
#267947=CARTESIAN_POINT('Ctrl Pts',(-10.8220229700001,15.2,-2.77511242500001));
#267948=CARTESIAN_POINT('Ctrl Pts',(-10.8220229700001,11.6,-2.77511242500002));
#267949=CARTESIAN_POINT('Ctrl Pts',(-10.8186985940001,15.2,-2.77557339600001));
#267950=CARTESIAN_POINT('Ctrl Pts',(-10.8186985940001,11.6,-2.77557339600001));
#267951=CARTESIAN_POINT('Ctrl Pts',(-10.8153787400001,15.2,-2.77603105800001));
#267952=CARTESIAN_POINT('Ctrl Pts',(-10.8153787400001,11.6,-2.77603105800001));
#267953=CARTESIAN_POINT('Ctrl Pts',(-10.8120634130001,15.2,-2.77648541700001));
#267954=CARTESIAN_POINT('Ctrl Pts',(-10.8120634130001,11.6,-2.77648541700001));
#267955=CARTESIAN_POINT('Ctrl Pts',(-10.8087526240001,15.2,-2.77693647800001));
#267956=CARTESIAN_POINT('Ctrl Pts',(-10.8087526240001,11.6,-2.77693647800001));
#267957=CARTESIAN_POINT('Ctrl Pts',(-10.8054463820001,15.2,-2.77738424700001));
#267958=CARTESIAN_POINT('Ctrl Pts',(-10.8054463820001,11.6,-2.77738424700001));
#267959=CARTESIAN_POINT('Ctrl Pts',(-10.8021446960001,15.2,-2.77782872900001));
#267960=CARTESIAN_POINT('Ctrl Pts',(-10.8021446960001,11.6,-2.77782872900001));
#267961=CARTESIAN_POINT('Ctrl Pts',(-10.7988475760001,15.2,-2.77826993000001));
#267962=CARTESIAN_POINT('Ctrl Pts',(-10.7988475760001,11.6,-2.77826993000002));
#267963=CARTESIAN_POINT('Ctrl Pts',(-10.7955550300001,15.2,-2.77870785600001));
#267964=CARTESIAN_POINT('Ctrl Pts',(-10.7955550300001,11.6,-2.77870785600001));
#267965=CARTESIAN_POINT('Ctrl Pts',(-10.7922670680001,15.2,-2.77914251000002));
#267966=CARTESIAN_POINT('Ctrl Pts',(-10.7922670680001,11.6,-2.77914251000002));
#267967=CARTESIAN_POINT('Ctrl Pts',(-10.7889836990001,15.2,-2.77957390000001));
#267968=CARTESIAN_POINT('Ctrl Pts',(-10.7889836990001,11.6,-2.77957390000001));
#267969=CARTESIAN_POINT('Ctrl Pts',(-10.7857049310001,15.2,-2.78000203100001));
#267970=CARTESIAN_POINT('Ctrl Pts',(-10.7857049310001,11.6,-2.78000203100001));
#267971=CARTESIAN_POINT('Ctrl Pts',(-10.7824307750001,15.2,-2.78042690900001));
#267972=CARTESIAN_POINT('Ctrl Pts',(-10.7824307750001,11.6,-2.78042690900001));
#267973=CARTESIAN_POINT('Ctrl Pts',(-10.7791612390001,15.2,-2.78084853700001));
#267974=CARTESIAN_POINT('Ctrl Pts',(-10.7791612390001,11.6,-2.78084853700001));
#267975=CARTESIAN_POINT('Ctrl Pts',(-10.7758963330001,15.2,-2.78126692300001));
#267976=CARTESIAN_POINT('Ctrl Pts',(-10.7758963330001,11.6,-2.78126692300001));
#267977=CARTESIAN_POINT('Ctrl Pts',(-10.7726360660001,15.2,-2.78168207300002));
#267978=CARTESIAN_POINT('Ctrl Pts',(-10.7726360660001,11.6,-2.78168207300002));
#267979=CARTESIAN_POINT('Ctrl Pts',(-10.7693804470001,15.2,-2.78209399100001));
#267980=CARTESIAN_POINT('Ctrl Pts',(-10.7693804470001,11.6,-2.78209399100001));
#267981=CARTESIAN_POINT('Ctrl Pts',(-10.7661294860001,15.2,-2.78250268300001));
#267982=CARTESIAN_POINT('Ctrl Pts',(-10.7661294860001,11.6,-2.78250268300001));
#267983=CARTESIAN_POINT('Ctrl Pts',(-10.7628831920001,15.2,-2.78290815600001));
#267984=CARTESIAN_POINT('Ctrl Pts',(-10.7628831920001,11.6,-2.78290815600002));
#267985=CARTESIAN_POINT('Ctrl Pts',(-10.7596415740001,15.2,-2.78331041300001));
#267986=CARTESIAN_POINT('Ctrl Pts',(-10.7596415740001,11.6,-2.78331041300001));
#267987=CARTESIAN_POINT('Ctrl Pts',(-10.7564046420001,15.2,-2.78370946300001));
#267988=CARTESIAN_POINT('Ctrl Pts',(-10.7564046420001,11.6,-2.78370946300001));
#267989=CARTESIAN_POINT('Ctrl Pts',(-10.7531724040001,15.2,-2.78410530900001));
#267990=CARTESIAN_POINT('Ctrl Pts',(-10.7531724040001,11.6,-2.78410530900001));
#267991=CARTESIAN_POINT('Ctrl Pts',(-10.7499448710001,15.2,-2.78449795800002));
#267992=CARTESIAN_POINT('Ctrl Pts',(-10.7499448710001,11.6,-2.78449795800002));
#267993=CARTESIAN_POINT('Ctrl Pts',(-10.7467220520001,15.2,-2.78488741600002));
#267994=CARTESIAN_POINT('Ctrl Pts',(-10.7467220520001,11.6,-2.78488741600002));
#267995=CARTESIAN_POINT('Ctrl Pts',(-10.7435039560001,15.2,-2.78527368900002));
#267996=CARTESIAN_POINT('Ctrl Pts',(-10.7435039560001,11.6,-2.78527368900002));
#267997=CARTESIAN_POINT('Ctrl Pts',(-10.7402905920001,15.2,-2.78565678100001));
#267998=CARTESIAN_POINT('Ctrl Pts',(-10.7402905920001,11.6,-2.78565678100001));
#267999=CARTESIAN_POINT('Ctrl Pts',(-10.7370819700001,15.2,-2.78603669900002));
#268000=CARTESIAN_POINT('Ctrl Pts',(-10.7370819700001,11.6,-2.78603669900002));
#268001=CARTESIAN_POINT('Ctrl Pts',(-10.7338780990001,15.2,-2.78641345000001));
#268002=CARTESIAN_POINT('Ctrl Pts',(-10.7338780990001,11.6,-2.78641345000001));
#268003=CARTESIAN_POINT('Ctrl Pts',(-10.7306789900001,15.2,-2.78678703700002));
#268004=CARTESIAN_POINT('Ctrl Pts',(-10.7306789900001,11.6,-2.78678703700002));
#268005=CARTESIAN_POINT('Ctrl Pts',(-10.7274846510001,15.2,-2.78715746900001));
#268006=CARTESIAN_POINT('Ctrl Pts',(-10.7274846510001,11.6,-2.78715746900001));
#268007=CARTESIAN_POINT('Ctrl Pts',(-10.7242950910001,15.2,-2.78752475000001));
#268008=CARTESIAN_POINT('Ctrl Pts',(-10.7242950910001,11.6,-2.78752475000001));
#268009=CARTESIAN_POINT('Ctrl Pts',(-10.7211103210001,15.2,-2.78788888700001));
#268010=CARTESIAN_POINT('Ctrl Pts',(-10.7211103210001,11.6,-2.78788888700001));
#268011=CARTESIAN_POINT('Ctrl Pts',(-10.7179303500001,15.2,-2.78824988400002));
#268012=CARTESIAN_POINT('Ctrl Pts',(-10.7179303500001,11.6,-2.78824988400002));
#268013=CARTESIAN_POINT('Ctrl Pts',(-10.7147551880001,15.2,-2.78860774800001));
#268014=CARTESIAN_POINT('Ctrl Pts',(-10.7147551880001,11.6,-2.78860774800001));
#268015=CARTESIAN_POINT('Ctrl Pts',(-10.7115848430001,15.2,-2.78896248700002));
#268016=CARTESIAN_POINT('Ctrl Pts',(-10.7115848430001,11.6,-2.78896248700002));
#268017=CARTESIAN_POINT('Ctrl Pts',(-10.7084193250001,15.2,-2.78931410400002));
#268018=CARTESIAN_POINT('Ctrl Pts',(-10.7084193250001,11.6,-2.78931410400002));
#268019=CARTESIAN_POINT('Ctrl Pts',(-10.7052586450001,15.2,-2.78966260600002));
#268020=CARTESIAN_POINT('Ctrl Pts',(-10.7052586450001,11.6,-2.78966260600002));
#268021=CARTESIAN_POINT('Ctrl Pts',(-10.7021028110001,15.2,-2.79000800100001));
#268022=CARTESIAN_POINT('Ctrl Pts',(-10.7021028110001,11.6,-2.79000800100001));
#268023=CARTESIAN_POINT('Ctrl Pts',(-10.6989518340001,15.2,-2.79035029100001));
#268024=CARTESIAN_POINT('Ctrl Pts',(-10.6989518340001,11.6,-2.79035029100001));
#268025=CARTESIAN_POINT('Ctrl Pts',(-10.6958057220001,15.2,-2.79068948600001));
#268026=CARTESIAN_POINT('Ctrl Pts',(-10.6958057220001,11.6,-2.79068948600001));
#268027=CARTESIAN_POINT('Ctrl Pts',(-10.6926644870001,15.2,-2.79102559000002));
#268028=CARTESIAN_POINT('Ctrl Pts',(-10.6926644870001,11.6,-2.79102559000002));
#268029=CARTESIAN_POINT('Ctrl Pts',(-10.6895281350001,15.2,-2.79135861000002));
#268030=CARTESIAN_POINT('Ctrl Pts',(-10.6895281350001,11.6,-2.79135861000002));
#268031=CARTESIAN_POINT('Ctrl Pts',(-10.6863966800001,15.2,-2.79168855100002));
#268032=CARTESIAN_POINT('Ctrl Pts',(-10.6863966800001,11.6,-2.79168855100002));
#268033=CARTESIAN_POINT('Ctrl Pts',(-10.6832701290001,15.2,-2.79201542000001));
#268034=CARTESIAN_POINT('Ctrl Pts',(-10.6832701290001,11.6,-2.79201542000001));
#268035=CARTESIAN_POINT('Ctrl Pts',(-10.6801484920001,15.2,-2.79233922300001));
#268036=CARTESIAN_POINT('Ctrl Pts',(-10.6801484920001,11.6,-2.79233922300001));
#268037=CARTESIAN_POINT('Ctrl Pts',(-10.6770317790001,15.2,-2.79265996700001));
#268038=CARTESIAN_POINT('Ctrl Pts',(-10.6770317790001,11.6,-2.79265996700001));
#268039=CARTESIAN_POINT('Ctrl Pts',(-10.6739200000001,15.2,-2.79297765700001));
#268040=CARTESIAN_POINT('Ctrl Pts',(-10.6739200000001,11.6,-2.79297765700001));
#268041=CARTESIAN_POINT('Ctrl Pts',(-10.6708131640001,15.2,-2.79329230000001));
#268042=CARTESIAN_POINT('Ctrl Pts',(-10.6708131640001,11.6,-2.79329230000001));
#268043=CARTESIAN_POINT('Ctrl Pts',(-10.6677112820001,15.2,-2.79360390200001));
#268044=CARTESIAN_POINT('Ctrl Pts',(-10.6677112820001,11.6,-2.79360390200001));
#268045=CARTESIAN_POINT('Ctrl Pts',(-10.6646143620001,15.2,-2.79391246900001));
#268046=CARTESIAN_POINT('Ctrl Pts',(-10.6646143620001,11.6,-2.79391246900001));
#268047=CARTESIAN_POINT('Ctrl Pts',(-10.6615224160001,15.2,-2.79421800700002));
#268048=CARTESIAN_POINT('Ctrl Pts',(-10.6615224160001,11.6,-2.79421800700002));
#268049=CARTESIAN_POINT('Ctrl Pts',(-10.6584354520001,15.2,-2.79452052500002));
#268050=CARTESIAN_POINT('Ctrl Pts',(-10.6584354520001,11.6,-2.79452052500002));
#268051=CARTESIAN_POINT('Ctrl Pts',(-10.6553534800001,15.2,-2.79482002500002));
#268052=CARTESIAN_POINT('Ctrl Pts',(-10.6553534800001,11.6,-2.79482002500002));
#268053=CARTESIAN_POINT('Ctrl Pts',(-10.6522765120001,15.2,-2.79511651600002));
#268054=CARTESIAN_POINT('Ctrl Pts',(-10.6522765120001,11.6,-2.79511651600002));
#268055=CARTESIAN_POINT('Ctrl Pts',(-10.6492045550001,15.2,-2.79541000500001));
#268056=CARTESIAN_POINT('Ctrl Pts',(-10.6492045550001,11.6,-2.79541000500001));
#268057=CARTESIAN_POINT('Ctrl Pts',(-10.6461376210001,15.2,-2.79570049800002));
#268058=CARTESIAN_POINT('Ctrl Pts',(-10.6461376210001,11.6,-2.79570049800002));
#268059=CARTESIAN_POINT('Ctrl Pts',(-10.6430757180001,15.2,-2.79598800000001));
#268060=CARTESIAN_POINT('Ctrl Pts',(-10.6430757180001,11.6,-2.79598800000001));
#268061=CARTESIAN_POINT('Ctrl Pts',(-10.6400188580001,15.2,-2.79627251700001));
#268062=CARTESIAN_POINT('Ctrl Pts',(-10.6400188580001,11.6,-2.79627251700001));
#268063=CARTESIAN_POINT('Ctrl Pts',(-10.6369670490001,15.2,-2.79655405800002));
#268064=CARTESIAN_POINT('Ctrl Pts',(-10.6369670490001,11.6,-2.79655405800002));
#268065=CARTESIAN_POINT('Ctrl Pts',(-10.6339203020001,15.2,-2.79683262800001));
#268066=CARTESIAN_POINT('Ctrl Pts',(-10.6339203020001,11.6,-2.79683262800001));
#268067=CARTESIAN_POINT('Ctrl Pts',(-10.6308786260001,15.2,-2.79710823500002));
#268068=CARTESIAN_POINT('Ctrl Pts',(-10.6308786260001,11.6,-2.79710823500002));
#268069=CARTESIAN_POINT('Ctrl Pts',(-10.6278420330001,15.2,-2.79738088400002));
#268070=CARTESIAN_POINT('Ctrl Pts',(-10.6278420330001,11.6,-2.79738088400002));
#268071=CARTESIAN_POINT('Ctrl Pts',(-10.6248105320001,15.2,-2.79765058100002));
#268072=CARTESIAN_POINT('Ctrl Pts',(-10.6248105320001,11.6,-2.79765058100002));
#268073=CARTESIAN_POINT('Ctrl Pts',(-10.6217841320001,15.2,-2.79791733300002));
#268074=CARTESIAN_POINT('Ctrl Pts',(-10.6217841320001,11.6,-2.79791733300002));
#268075=CARTESIAN_POINT('Ctrl Pts',(-10.6187628440001,15.2,-2.79818114900001));
#268076=CARTESIAN_POINT('Ctrl Pts',(-10.6187628440001,11.6,-2.79818114900001));
#268077=CARTESIAN_POINT('Ctrl Pts',(-10.6157466780001,15.2,-2.79844203300001));
#268078=CARTESIAN_POINT('Ctrl Pts',(-10.6157466780001,11.6,-2.79844203300002));
#268079=CARTESIAN_POINT('Ctrl Pts',(-10.6127356450001,15.2,-2.79869999200002));
#268080=CARTESIAN_POINT('Ctrl Pts',(-10.6127356450001,11.6,-2.79869999200002));
#268081=CARTESIAN_POINT('Ctrl Pts',(-10.6097297520001,15.2,-2.79895503300001));
#268082=CARTESIAN_POINT('Ctrl Pts',(-10.6097297520001,11.6,-2.79895503300002));
#268083=CARTESIAN_POINT('Ctrl Pts',(-10.6067290130001,15.2,-2.79920716400001));
#268084=CARTESIAN_POINT('Ctrl Pts',(-10.6067290130001,11.6,-2.79920716400001));
#268085=CARTESIAN_POINT('Ctrl Pts',(-10.6037334350001,15.2,-2.79945638900001));
#268086=CARTESIAN_POINT('Ctrl Pts',(-10.6037334350001,11.6,-2.79945638900002));
#268087=CARTESIAN_POINT('Ctrl Pts',(-10.6007430310001,15.2,-2.79970271700002));
#268088=CARTESIAN_POINT('Ctrl Pts',(-10.6007430310001,11.6,-2.79970271700002));
#268089=CARTESIAN_POINT('Ctrl Pts',(-10.5977578070001,15.2,-2.79994615300001));
#268090=CARTESIAN_POINT('Ctrl Pts',(-10.5977578070001,11.6,-2.79994615300002));
#268091=CARTESIAN_POINT('Ctrl Pts',(-10.5947777780001,15.2,-2.80018670600001));
#268092=CARTESIAN_POINT('Ctrl Pts',(-10.5947777780001,11.6,-2.80018670600001));
#268093=CARTESIAN_POINT('Ctrl Pts',(-10.5918029510001,15.2,-2.80042438200002));
#268094=CARTESIAN_POINT('Ctrl Pts',(-10.5918029510001,11.6,-2.80042438200002));
#268095=CARTESIAN_POINT('Ctrl Pts',(-10.5888333380001,15.2,-2.80065918700001));
#268096=CARTESIAN_POINT('Ctrl Pts',(-10.5888333380001,11.6,-2.80065918700001));
#268097=CARTESIAN_POINT('Ctrl Pts',(-10.5858689480001,15.2,-2.80089112800002));
#268098=CARTESIAN_POINT('Ctrl Pts',(-10.5858689480001,11.6,-2.80089112800002));
#268099=CARTESIAN_POINT('Ctrl Pts',(-10.5829097920001,15.2,-2.80112021200001));
#268100=CARTESIAN_POINT('Ctrl Pts',(-10.5829097920001,11.6,-2.80112021200001));
#268101=CARTESIAN_POINT('Ctrl Pts',(-10.5799558780001,15.2,-2.80134644700002));
#268102=CARTESIAN_POINT('Ctrl Pts',(-10.5799558780001,11.6,-2.80134644700002));
#268103=CARTESIAN_POINT('Ctrl Pts',(-10.5770072200001,15.2,-2.80156983800001));
#268104=CARTESIAN_POINT('Ctrl Pts',(-10.5770072200001,11.6,-2.80156983800001));
#268105=CARTESIAN_POINT('Ctrl Pts',(-10.5740638260001,15.2,-2.80179039400001));
#268106=CARTESIAN_POINT('Ctrl Pts',(-10.5740638260001,11.6,-2.80179039400001));
#268107=CARTESIAN_POINT('Ctrl Pts',(-10.5711257080001,15.2,-2.80200812100002));
#268108=CARTESIAN_POINT('Ctrl Pts',(-10.5711257080001,11.6,-2.80200812100002));
#268109=CARTESIAN_POINT('Ctrl Pts',(-10.5681928730001,15.2,-2.80222302500002));
#268110=CARTESIAN_POINT('Ctrl Pts',(-10.5681928730001,11.6,-2.80222302500002));
#268111=CARTESIAN_POINT('Ctrl Pts',(-10.5652653350001,15.2,-2.80243511500001));
#268112=CARTESIAN_POINT('Ctrl Pts',(-10.5652653350001,11.6,-2.80243511500002));
#268113=CARTESIAN_POINT('Ctrl Pts',(-10.5623431030001,15.2,-2.80264439700002));
#268114=CARTESIAN_POINT('Ctrl Pts',(-10.5623431030001,11.6,-2.80264439700002));
#268115=CARTESIAN_POINT('Ctrl Pts',(-10.5594261870001,15.2,-2.80285087700001));
#268116=CARTESIAN_POINT('Ctrl Pts',(-10.5594261870001,11.6,-2.80285087700001));
#268117=CARTESIAN_POINT('Ctrl Pts',(-10.5565145980001,15.2,-2.80305456500002));
#268118=CARTESIAN_POINT('Ctrl Pts',(-10.5565145980001,11.6,-2.80305456500002));
#268119=CARTESIAN_POINT('Ctrl Pts',(-10.5536083460001,15.2,-2.80325546500002));
#268120=CARTESIAN_POINT('Ctrl Pts',(-10.5536083460001,11.6,-2.80325546500002));
#268121=CARTESIAN_POINT('Ctrl Pts',(-10.5507074410001,15.2,-2.80345358600002));
#268122=CARTESIAN_POINT('Ctrl Pts',(-10.5507074410001,11.6,-2.80345358600002));
#268123=CARTESIAN_POINT('Ctrl Pts',(-10.5478118940001,15.2,-2.80364893500002));
#268124=CARTESIAN_POINT('Ctrl Pts',(-10.5478118940001,11.6,-2.80364893500002));
#268125=CARTESIAN_POINT('Ctrl Pts',(-10.5449217170001,15.2,-2.80384151900002));
#268126=CARTESIAN_POINT('Ctrl Pts',(-10.5449217170001,11.6,-2.80384151900002));
#268127=CARTESIAN_POINT('Ctrl Pts',(-10.5420369180001,15.2,-2.80403134500002));
#268128=CARTESIAN_POINT('Ctrl Pts',(-10.5420369180001,11.6,-2.80403134500002));
#268129=CARTESIAN_POINT('Ctrl Pts',(-10.5391575100001,15.2,-2.80421842000001));
#268130=CARTESIAN_POINT('Ctrl Pts',(-10.5391575100001,11.6,-2.80421842000001));
#268131=CARTESIAN_POINT('Ctrl Pts',(-10.5362835010001,15.2,-2.80440275200001));
#268132=CARTESIAN_POINT('Ctrl Pts',(-10.5362835010001,11.6,-2.80440275200002));
#268133=CARTESIAN_POINT('Ctrl Pts',(-10.5334149020001,15.2,-2.80458434800002));
#268134=CARTESIAN_POINT('Ctrl Pts',(-10.5334149020001,11.6,-2.80458434800002));
#268135=CARTESIAN_POINT('Ctrl Pts',(-10.5305517260001,15.2,-2.80476321500001));
#268136=CARTESIAN_POINT('Ctrl Pts',(-10.5305517260001,11.6,-2.80476321500002));
#268137=CARTESIAN_POINT('Ctrl Pts',(-10.5276939810001,15.2,-2.80493936100001));
#268138=CARTESIAN_POINT('Ctrl Pts',(-10.5276939810001,11.6,-2.80493936100001));
#268139=CARTESIAN_POINT('Ctrl Pts',(-10.5248416780001,15.2,-2.80511279300002));
#268140=CARTESIAN_POINT('Ctrl Pts',(-10.5248416780001,11.6,-2.80511279300002));
#268141=CARTESIAN_POINT('Ctrl Pts',(-10.5219948290001,15.2,-2.80528351800001));
#268142=CARTESIAN_POINT('Ctrl Pts',(-10.5219948290001,11.6,-2.80528351800002));
#268143=CARTESIAN_POINT('Ctrl Pts',(-10.5191534450001,15.2,-2.80545154400002));
#268144=CARTESIAN_POINT('Ctrl Pts',(-10.5191534450001,11.6,-2.80545154400002));
#268145=CARTESIAN_POINT('Ctrl Pts',(-10.5163175340001,15.2,-2.80561687900001));
#268146=CARTESIAN_POINT('Ctrl Pts',(-10.5163175340001,11.6,-2.80561687900002));
#268147=CARTESIAN_POINT('Ctrl Pts',(-10.5134871080001,15.2,-2.80577952900002));
#268148=CARTESIAN_POINT('Ctrl Pts',(-10.5134871080001,11.6,-2.80577952900002));
#268149=CARTESIAN_POINT('Ctrl Pts',(-10.5106621790001,15.2,-2.80593950300001));
#268150=CARTESIAN_POINT('Ctrl Pts',(-10.5106621790001,11.6,-2.80593950300001));
#268151=CARTESIAN_POINT('Ctrl Pts',(-10.5078427570001,15.2,-2.80609680700001));
#268152=CARTESIAN_POINT('Ctrl Pts',(-10.5078427570001,11.6,-2.80609680700001));
#268153=CARTESIAN_POINT('Ctrl Pts',(-10.5050288510001,15.2,-2.80625145000001));
#268154=CARTESIAN_POINT('Ctrl Pts',(-10.5050288510001,11.6,-2.80625145000002));
#268155=CARTESIAN_POINT('Ctrl Pts',(-10.5022204750001,15.2,-2.80640343900001));
#268156=CARTESIAN_POINT('Ctrl Pts',(-10.5022204750001,11.6,-2.80640343900001));
#268157=CARTESIAN_POINT('Ctrl Pts',(-10.4994176380001,15.2,-2.80655278100001));
#268158=CARTESIAN_POINT('Ctrl Pts',(-10.4994176380001,11.6,-2.80655278100001));
#268159=CARTESIAN_POINT('Ctrl Pts',(-10.4966203510001,15.2,-2.80669948500002));
#268160=CARTESIAN_POINT('Ctrl Pts',(-10.4966203510001,11.6,-2.80669948500002));
#268161=CARTESIAN_POINT('Ctrl Pts',(-10.4938286240001,15.2,-2.80684355700001));
#268162=CARTESIAN_POINT('Ctrl Pts',(-10.4938286240001,11.6,-2.80684355700001));
#268163=CARTESIAN_POINT('Ctrl Pts',(-10.4910424700001,15.2,-2.80698500600002));
#268164=CARTESIAN_POINT('Ctrl Pts',(-10.4910424700001,11.6,-2.80698500600002));
#268165=CARTESIAN_POINT('Ctrl Pts',(-10.4882618970001,15.2,-2.80712384000001));
#268166=CARTESIAN_POINT('Ctrl Pts',(-10.4882618970001,11.6,-2.80712384000001));
#268167=CARTESIAN_POINT('Ctrl Pts',(-10.4854869180001,15.2,-2.80726006400001));
#268168=CARTESIAN_POINT('Ctrl Pts',(-10.4854869180001,11.6,-2.80726006400001));
#268169=CARTESIAN_POINT('Ctrl Pts',(-10.4827175440001,15.2,-2.80739369000001));
#268170=CARTESIAN_POINT('Ctrl Pts',(-10.4827175440001,11.6,-2.80739369000001));
#268171=CARTESIAN_POINT('Ctrl Pts',(-10.4799537850001,15.2,-2.80752472200001));
#268172=CARTESIAN_POINT('Ctrl Pts',(-10.4799537850001,11.6,-2.80752472200001));
#268173=CARTESIAN_POINT('Ctrl Pts',(-10.4771956530001,15.2,-2.80765317100002));
#268174=CARTESIAN_POINT('Ctrl Pts',(-10.4771956530001,11.6,-2.80765317100002));
#268175=CARTESIAN_POINT('Ctrl Pts',(-10.4744431570001,15.2,-2.80777904200002));
#268176=CARTESIAN_POINT('Ctrl Pts',(-10.4744431570001,11.6,-2.80777904200002));
#268177=CARTESIAN_POINT('Ctrl Pts',(-10.4716963110001,15.2,-2.80790234500001));
#268178=CARTESIAN_POINT('Ctrl Pts',(-10.4716963110001,11.6,-2.80790234500001));
#268179=CARTESIAN_POINT('Ctrl Pts',(-10.4689551240001,15.2,-2.80802308700002));
#268180=CARTESIAN_POINT('Ctrl Pts',(-10.4689551240001,11.6,-2.80802308700002));
#268181=CARTESIAN_POINT('Ctrl Pts',(-10.4662196070001,15.2,-2.80814127600001));
#268182=CARTESIAN_POINT('Ctrl Pts',(-10.4662196070001,11.6,-2.80814127600001));
#268183=CARTESIAN_POINT('Ctrl Pts',(-10.4634897720001,15.2,-2.80825691900001));
#268184=CARTESIAN_POINT('Ctrl Pts',(-10.4634897720001,11.6,-2.80825691900001));
#268185=CARTESIAN_POINT('Ctrl Pts',(-10.4607656300001,15.2,-2.80837002600002));
#268186=CARTESIAN_POINT('Ctrl Pts',(-10.4607656300001,11.6,-2.80837002600002));
#268187=CARTESIAN_POINT('Ctrl Pts',(-10.4580471910001,15.2,-2.80848060400002));
#268188=CARTESIAN_POINT('Ctrl Pts',(-10.4580471910001,11.6,-2.80848060400002));
#268189=CARTESIAN_POINT('Ctrl Pts',(-10.4553344680001,15.2,-2.80858866000001));
#268190=CARTESIAN_POINT('Ctrl Pts',(-10.4553344680001,11.6,-2.80858866000001));
#268191=CARTESIAN_POINT('Ctrl Pts',(-10.4526274700001,15.2,-2.80869420500002));
#268192=CARTESIAN_POINT('Ctrl Pts',(-10.4526274700001,11.6,-2.80869420500002));
#268193=CARTESIAN_POINT('Ctrl Pts',(-10.4499262110001,15.2,-2.80879724300001));
#268194=CARTESIAN_POINT('Ctrl Pts',(-10.4499262110001,11.6,-2.80879724300001));
#268195=CARTESIAN_POINT('Ctrl Pts',(-10.4472306990001,15.2,-2.80889778700002));
#268196=CARTESIAN_POINT('Ctrl Pts',(-10.4472306990001,11.6,-2.80889778700002));
#268197=CARTESIAN_POINT('Ctrl Pts',(-10.4445409480001,15.2,-2.80899584100001));
#268198=CARTESIAN_POINT('Ctrl Pts',(-10.4445409480001,11.6,-2.80899584100002));
#268199=CARTESIAN_POINT('Ctrl Pts',(-10.4418569680001,15.2,-2.80909141400001));
#268200=CARTESIAN_POINT('Ctrl Pts',(-10.4418569680001,11.6,-2.80909141400001));
#268201=CARTESIAN_POINT('Ctrl Pts',(-10.4391787700001,15.2,-2.80918451700002));
#268202=CARTESIAN_POINT('Ctrl Pts',(-10.4391787700001,11.6,-2.80918451700002));
#268203=CARTESIAN_POINT('Ctrl Pts',(-10.4365063660001,15.2,-2.80927515500002));
#268204=CARTESIAN_POINT('Ctrl Pts',(-10.4365063660001,11.6,-2.80927515500002));
#268205=CARTESIAN_POINT('Ctrl Pts',(-10.4338397670001,15.2,-2.80936333700001));
#268206=CARTESIAN_POINT('Ctrl Pts',(-10.4338397670001,11.6,-2.80936333700002));
#268207=CARTESIAN_POINT('Ctrl Pts',(-10.4311789840001,15.2,-2.80944907300002));
#268208=CARTESIAN_POINT('Ctrl Pts',(-10.4311789840001,11.6,-2.80944907300002));
#268209=CARTESIAN_POINT('Ctrl Pts',(-10.4285240300001,15.2,-2.80953237000002));
#268210=CARTESIAN_POINT('Ctrl Pts',(-10.4285240300001,11.6,-2.80953237000002));
#268211=CARTESIAN_POINT('Ctrl Pts',(-10.4258749130001,15.2,-2.80961323700001));
#268212=CARTESIAN_POINT('Ctrl Pts',(-10.4258749130001,11.6,-2.80961323700002));
#268213=CARTESIAN_POINT('Ctrl Pts',(-10.4232316480001,15.2,-2.80969168100001));
#268214=CARTESIAN_POINT('Ctrl Pts',(-10.4232316480001,11.6,-2.80969168100001));
#268215=CARTESIAN_POINT('Ctrl Pts',(-10.4205942460001,15.2,-2.80976771100002));
#268216=CARTESIAN_POINT('Ctrl Pts',(-10.4205942460001,11.6,-2.80976771100002));
#268217=CARTESIAN_POINT('Ctrl Pts',(-10.4179627160001,15.2,-2.80984133700001));
#268218=CARTESIAN_POINT('Ctrl Pts',(-10.4179627160001,11.6,-2.80984133700001));
#268219=CARTESIAN_POINT('Ctrl Pts',(-10.4153370720001,15.2,-2.80991256500001));
#268220=CARTESIAN_POINT('Ctrl Pts',(-10.4153370720001,11.6,-2.80991256500001));
#268221=CARTESIAN_POINT('Ctrl Pts',(-10.4127173250001,15.2,-2.80998140700001));
#268222=CARTESIAN_POINT('Ctrl Pts',(-10.4127173250001,11.6,-2.80998140700001));
#268223=CARTESIAN_POINT('Ctrl Pts',(-10.4101034850001,15.2,-2.81004786800001));
#268224=CARTESIAN_POINT('Ctrl Pts',(-10.4101034850001,11.6,-2.81004786800001));
#268225=CARTESIAN_POINT('Ctrl Pts',(-10.4074955650001,15.2,-2.81011195800001));
#268226=CARTESIAN_POINT('Ctrl Pts',(-10.4074955650001,11.6,-2.81011195800001));
#268227=CARTESIAN_POINT('Ctrl Pts',(-10.4048935770001,15.2,-2.81017368600001));
#268228=CARTESIAN_POINT('Ctrl Pts',(-10.4048935770001,11.6,-2.81017368600002));
#268229=CARTESIAN_POINT('Ctrl Pts',(-10.4022975320001,15.2,-2.81023306000002));
#268230=CARTESIAN_POINT('Ctrl Pts',(-10.4022975320001,11.6,-2.81023306000002));
#268231=CARTESIAN_POINT('Ctrl Pts',(-10.3997074400001,15.2,-2.81029008900001));
#268232=CARTESIAN_POINT('Ctrl Pts',(-10.3997074400001,11.6,-2.81029008900001));
#268233=CARTESIAN_POINT('Ctrl Pts',(-10.3971233170001,15.2,-2.81034478200001));
#268234=CARTESIAN_POINT('Ctrl Pts',(-10.3971233170001,11.6,-2.81034478200001));
#268235=CARTESIAN_POINT('Ctrl Pts',(-10.3945451690001,15.2,-2.81039714800002));
#268236=CARTESIAN_POINT('Ctrl Pts',(-10.3945451690001,11.6,-2.81039714800002));
#268237=CARTESIAN_POINT('Ctrl Pts',(-10.3919730120001,15.2,-2.81044719300001));
#268238=CARTESIAN_POINT('Ctrl Pts',(-10.3919730120001,11.6,-2.81044719300001));
#268239=CARTESIAN_POINT('Ctrl Pts',(-10.3894068560001,15.2,-2.81049493000001));
#268240=CARTESIAN_POINT('Ctrl Pts',(-10.3894068560001,11.6,-2.81049493000001));
#268241=CARTESIAN_POINT('Ctrl Pts',(-10.3868467140001,15.2,-2.81054036500001));
#268242=CARTESIAN_POINT('Ctrl Pts',(-10.3868467140001,11.6,-2.81054036500001));
#268243=CARTESIAN_POINT('Ctrl Pts',(-10.3842925970001,15.2,-2.81058350800001));
#268244=CARTESIAN_POINT('Ctrl Pts',(-10.3842925970001,11.6,-2.81058350800001));
#268245=CARTESIAN_POINT('Ctrl Pts',(-10.3817445160001,15.2,-2.81062436900001));
#268246=CARTESIAN_POINT('Ctrl Pts',(-10.3817445160001,11.6,-2.81062436900001));
#268247=CARTESIAN_POINT('Ctrl Pts',(-10.3792024840001,15.2,-2.81066295300001));
#268248=CARTESIAN_POINT('Ctrl Pts',(-10.3792024840001,11.6,-2.81066295300001));
#268249=CARTESIAN_POINT('Ctrl Pts',(-10.3766665130001,15.2,-2.81069927400001));
#268250=CARTESIAN_POINT('Ctrl Pts',(-10.3766665130001,11.6,-2.81069927400001));
#268251=CARTESIAN_POINT('Ctrl Pts',(-10.3741366140001,15.2,-2.81073333600002));
#268252=CARTESIAN_POINT('Ctrl Pts',(-10.3741366140001,11.6,-2.81073333600002));
#268253=CARTESIAN_POINT('Ctrl Pts',(-10.3716127990001,15.2,-2.81076515200001));
#268254=CARTESIAN_POINT('Ctrl Pts',(-10.3716127990001,11.6,-2.81076515200001));
#268255=CARTESIAN_POINT('Ctrl Pts',(-10.3690950810001,15.2,-2.81079473000001));
#268256=CARTESIAN_POINT('Ctrl Pts',(-10.3690950810001,11.6,-2.81079473000002));
#268257=CARTESIAN_POINT('Ctrl Pts',(-10.3665834700001,15.2,-2.81082207900001));
#268258=CARTESIAN_POINT('Ctrl Pts',(-10.3665834700001,11.6,-2.81082207900001));
#268259=CARTESIAN_POINT('Ctrl Pts',(-10.3640779820001,15.2,-2.81084720700001));
#268260=CARTESIAN_POINT('Ctrl Pts',(-10.3640779820001,11.6,-2.81084720700001));
#268261=CARTESIAN_POINT('Ctrl Pts',(-10.3615786240001,15.2,-2.81087012400001));
#268262=CARTESIAN_POINT('Ctrl Pts',(-10.3615786240001,11.6,-2.81087012400001));
#268263=CARTESIAN_POINT('Ctrl Pts',(-10.3590854110001,15.2,-2.81089083900001));
#268264=CARTESIAN_POINT('Ctrl Pts',(-10.3590854110001,11.6,-2.81089083900001));
#268265=CARTESIAN_POINT('Ctrl Pts',(-10.3565983540001,15.2,-2.81090936300001));
#268266=CARTESIAN_POINT('Ctrl Pts',(-10.3565983540001,11.6,-2.81090936300001));
#268267=CARTESIAN_POINT('Ctrl Pts',(-10.3541174660001,15.2,-2.81092570300002));
#268268=CARTESIAN_POINT('Ctrl Pts',(-10.3541174660001,11.6,-2.81092570300002));
#268269=CARTESIAN_POINT('Ctrl Pts',(-10.3516427590001,15.2,-2.81093986800002));
#268270=CARTESIAN_POINT('Ctrl Pts',(-10.3516427590001,11.6,-2.81093986800002));
#268271=CARTESIAN_POINT('Ctrl Pts',(-10.3491742450001,15.2,-2.81095186900002));
#268272=CARTESIAN_POINT('Ctrl Pts',(-10.3491742450001,11.6,-2.81095186900002));
#268273=CARTESIAN_POINT('Ctrl Pts',(-10.3467119360001,15.2,-2.81096171500002));
#268274=CARTESIAN_POINT('Ctrl Pts',(-10.3467119360001,11.6,-2.81096171500002));
#268275=CARTESIAN_POINT('Ctrl Pts',(-10.3442558440001,15.2,-2.81096941500001));
#268276=CARTESIAN_POINT('Ctrl Pts',(-10.3442558440001,11.6,-2.81096941500001));
#268277=CARTESIAN_POINT('Ctrl Pts',(-10.3418059810001,15.2,-2.81097497900001));
#268278=CARTESIAN_POINT('Ctrl Pts',(-10.3418059810001,11.6,-2.81097497900001));
#268279=CARTESIAN_POINT('Ctrl Pts',(-10.3393623600001,15.2,-2.81097841600001));
#268280=CARTESIAN_POINT('Ctrl Pts',(-10.3393623600001,11.6,-2.81097841600001));
#268281=CARTESIAN_POINT('Ctrl Pts',(-10.3369249940001,15.2,-2.81097973500001));
#268282=CARTESIAN_POINT('Ctrl Pts',(-10.3369249940001,11.6,-2.81097973500001));
#268283=CARTESIAN_POINT('Ctrl Pts',(-10.3344938940001,15.2,-2.81097894800002));
#268284=CARTESIAN_POINT('Ctrl Pts',(-10.3344938940001,11.6,-2.81097894800002));
#268285=CARTESIAN_POINT('Ctrl Pts',(-10.3320690720001,15.2,-2.81097606100001));
#268286=CARTESIAN_POINT('Ctrl Pts',(-10.3320690720001,11.6,-2.81097606100001));
#268287=CARTESIAN_POINT('Ctrl Pts',(-10.3296505420001,15.2,-2.81097108600001));
#268288=CARTESIAN_POINT('Ctrl Pts',(-10.3296505420001,11.6,-2.81097108600001));
#268289=CARTESIAN_POINT('Ctrl Pts',(-10.3272383160001,15.2,-2.81096403100001));
#268290=CARTESIAN_POINT('Ctrl Pts',(-10.3272383160001,11.6,-2.81096403100001));
#268291=CARTESIAN_POINT('Ctrl Pts',(-10.3248324060001,15.2,-2.81095490800002));
#268292=CARTESIAN_POINT('Ctrl Pts',(-10.3248324060001,11.6,-2.81095490800002));
#268293=CARTESIAN_POINT('Ctrl Pts',(-10.3224328240001,15.2,-2.81094372600001));
#268294=CARTESIAN_POINT('Ctrl Pts',(-10.3224328240001,11.6,-2.81094372600002));
#268295=CARTESIAN_POINT('Ctrl Pts',(-10.3200395830001,15.2,-2.81093049300001));
#268296=CARTESIAN_POINT('Ctrl Pts',(-10.3200395830001,11.6,-2.81093049300001));
#268297=CARTESIAN_POINT('Ctrl Pts',(-10.3176526950001,15.2,-2.81091522000001));
#268298=CARTESIAN_POINT('Ctrl Pts',(-10.3176526950001,11.6,-2.81091522000001));
#268299=CARTESIAN_POINT('Ctrl Pts',(-10.3152721750001,15.2,-2.81089791800001));
#268300=CARTESIAN_POINT('Ctrl Pts',(-10.3152721750001,11.6,-2.81089791800001));
#268301=CARTESIAN_POINT('Ctrl Pts',(-10.3128980330001,15.2,-2.81087859400001));
#268302=CARTESIAN_POINT('Ctrl Pts',(-10.3128980330001,11.6,-2.81087859400001));
#268303=CARTESIAN_POINT('Ctrl Pts',(-10.3105302810001,15.2,-2.81085726100001));
#268304=CARTESIAN_POINT('Ctrl Pts',(-10.3105302810001,11.6,-2.81085726100002));
#268305=CARTESIAN_POINT('Ctrl Pts',(-10.3081689340001,15.2,-2.81083392700001));
#268306=CARTESIAN_POINT('Ctrl Pts',(-10.3081689340001,11.6,-2.81083392700001));
#268307=CARTESIAN_POINT('Ctrl Pts',(-10.3058140040001,15.2,-2.81080860400001));
#268308=CARTESIAN_POINT('Ctrl Pts',(-10.3058140040001,11.6,-2.81080860400001));
#268309=CARTESIAN_POINT('Ctrl Pts',(-10.3034655040001,15.2,-2.81078129900001));
#268310=CARTESIAN_POINT('Ctrl Pts',(-10.3034655040001,11.6,-2.81078129900001));
#268311=CARTESIAN_POINT('Ctrl Pts',(-10.3011234450001,15.2,-2.81075202400002));
#268312=CARTESIAN_POINT('Ctrl Pts',(-10.3011234450001,11.6,-2.81075202400002));
#268313=CARTESIAN_POINT('Ctrl Pts',(-10.2987878420001,15.2,-2.81072079000001));
#268314=CARTESIAN_POINT('Ctrl Pts',(-10.2987878420001,11.6,-2.81072079000001));
#268315=CARTESIAN_POINT('Ctrl Pts',(-10.2964587060001,15.2,-2.81068760400002));
#268316=CARTESIAN_POINT('Ctrl Pts',(-10.2964587060001,11.6,-2.81068760400002));
#268317=CARTESIAN_POINT('Ctrl Pts',(-10.2941360500001,15.2,-2.81065248000001));
#268318=CARTESIAN_POINT('Ctrl Pts',(-10.2941360500001,11.6,-2.81065248000001));
#268319=CARTESIAN_POINT('Ctrl Pts',(-10.2918198870001,15.2,-2.81061542500002));
#268320=CARTESIAN_POINT('Ctrl Pts',(-10.2918198870001,11.6,-2.81061542500002));
#268321=CARTESIAN_POINT('Ctrl Pts',(-10.2895102320001,15.2,-2.81057645100002));
#268322=CARTESIAN_POINT('Ctrl Pts',(-10.2895102320001,11.6,-2.81057645100002));
#268323=CARTESIAN_POINT('Ctrl Pts',(-10.2872070960001,15.2,-2.81053556800002));
#268324=CARTESIAN_POINT('Ctrl Pts',(-10.2872070960001,11.6,-2.81053556800002));
#268325=CARTESIAN_POINT('Ctrl Pts',(-10.2849104920001,15.2,-2.81049278600001));
#268326=CARTESIAN_POINT('Ctrl Pts',(-10.2849104920001,11.6,-2.81049278600001));
#268327=CARTESIAN_POINT('Ctrl Pts',(-10.2826204320001,15.2,-2.81044811600001));
#268328=CARTESIAN_POINT('Ctrl Pts',(-10.2826204320001,11.6,-2.81044811600002));
#268329=CARTESIAN_POINT('Ctrl Pts',(-10.2803369320001,15.2,-2.81040156800001));
#268330=CARTESIAN_POINT('Ctrl Pts',(-10.2803369320001,11.6,-2.81040156800001));
#268331=CARTESIAN_POINT('Ctrl Pts',(-10.2780600020001,15.2,-2.81035315300001));
#268332=CARTESIAN_POINT('Ctrl Pts',(-10.2780600020001,11.6,-2.81035315300001));
#268333=CARTESIAN_POINT('Ctrl Pts',(-10.2757896570001,15.2,-2.81030288000002));
#268334=CARTESIAN_POINT('Ctrl Pts',(-10.2757896570001,11.6,-2.81030288000002));
#268335=CARTESIAN_POINT('Ctrl Pts',(-10.2735259090001,15.2,-2.81025076200002));
#268336=CARTESIAN_POINT('Ctrl Pts',(-10.2735259090001,11.6,-2.81025076200002));
#268337=CARTESIAN_POINT('Ctrl Pts',(-10.2712687710001,15.2,-2.81019680600001));
#268338=CARTESIAN_POINT('Ctrl Pts',(-10.2712687710001,11.6,-2.81019680600001));
#268339=CARTESIAN_POINT('Ctrl Pts',(-10.2690182590001,15.2,-2.81014102700002));
#268340=CARTESIAN_POINT('Ctrl Pts',(-10.2690182590001,11.6,-2.81014102700002));
#268341=CARTESIAN_POINT('Ctrl Pts',(-10.2667743820001,15.2,-2.81008343100002));
#268342=CARTESIAN_POINT('Ctrl Pts',(-10.2667743820001,11.6,-2.81008343100002));
#268343=CARTESIAN_POINT('Ctrl Pts',(-10.2645371560001,15.2,-2.81002403300001));
#268344=CARTESIAN_POINT('Ctrl Pts',(-10.2645371560001,11.6,-2.81002403300001));
#268345=CARTESIAN_POINT('Ctrl Pts',(-10.2623065940001,15.2,-2.80996284100001));
#268346=CARTESIAN_POINT('Ctrl Pts',(-10.2623065940001,11.6,-2.80996284100001));
#268347=CARTESIAN_POINT('Ctrl Pts',(-10.2600827090001,15.2,-2.80989986700002));
#268348=CARTESIAN_POINT('Ctrl Pts',(-10.2600827090001,11.6,-2.80989986700002));
#268349=CARTESIAN_POINT('Ctrl Pts',(-10.2578655120001,15.2,-2.80983512200002));
#268350=CARTESIAN_POINT('Ctrl Pts',(-10.2578655120001,11.6,-2.80983512200002));
#268351=CARTESIAN_POINT('Ctrl Pts',(-10.2556550210001,15.2,-2.80976861500001));
#268352=CARTESIAN_POINT('Ctrl Pts',(-10.2556550210001,11.6,-2.80976861500001));
#268353=CARTESIAN_POINT('Ctrl Pts',(-10.2534512460001,15.2,-2.80970035900001));
#268354=CARTESIAN_POINT('Ctrl Pts',(-10.2534512460001,11.6,-2.80970035900001));
#268355=CARTESIAN_POINT('Ctrl Pts',(-10.2512542030001,15.2,-2.80963036400002));
#268356=CARTESIAN_POINT('Ctrl Pts',(-10.2512542030001,11.6,-2.80963036400002));
#268357=CARTESIAN_POINT('Ctrl Pts',(-10.2490639020001,15.2,-2.80955864200001));
#268358=CARTESIAN_POINT('Ctrl Pts',(-10.2490639020001,11.6,-2.80955864200001));
#268359=CARTESIAN_POINT('Ctrl Pts',(-10.2468803590001,15.2,-2.80948520200001));
#268360=CARTESIAN_POINT('Ctrl Pts',(-10.2468803590001,11.6,-2.80948520200001));
#268361=CARTESIAN_POINT('Ctrl Pts',(-10.2447035880001,15.2,-2.80941005800001));
#268362=CARTESIAN_POINT('Ctrl Pts',(-10.2447035880001,11.6,-2.80941005800001));
#268363=CARTESIAN_POINT('Ctrl Pts',(-10.2425336010001,15.2,-2.80933321800001));
#268364=CARTESIAN_POINT('Ctrl Pts',(-10.2425336010001,11.6,-2.80933321800001));
#268365=CARTESIAN_POINT('Ctrl Pts',(-10.2403704120001,15.2,-2.80925469500001));
#268366=CARTESIAN_POINT('Ctrl Pts',(-10.2403704120001,11.6,-2.80925469500001));
#268367=CARTESIAN_POINT('Ctrl Pts',(-10.2382140350001,15.2,-2.80917450000001));
#268368=CARTESIAN_POINT('Ctrl Pts',(-10.2382140350001,11.6,-2.80917450000001));
#268369=CARTESIAN_POINT('Ctrl Pts',(-10.2360644840001,15.2,-2.80909264400002));
#268370=CARTESIAN_POINT('Ctrl Pts',(-10.2360644840001,11.6,-2.80909264400002));
#268371=CARTESIAN_POINT('Ctrl Pts',(-10.2339217720001,15.2,-2.80900913800001));
#268372=CARTESIAN_POINT('Ctrl Pts',(-10.2339217720001,11.6,-2.80900913800001));
#268373=CARTESIAN_POINT('Ctrl Pts',(-10.2317859140001,15.2,-2.80892399500001));
#268374=CARTESIAN_POINT('Ctrl Pts',(-10.2317859140001,11.6,-2.80892399500001));
#268375=CARTESIAN_POINT('Ctrl Pts',(-10.2296569220001,15.2,-2.80883722400001));
#268376=CARTESIAN_POINT('Ctrl Pts',(-10.2296569220001,11.6,-2.80883722400001));
#268377=CARTESIAN_POINT('Ctrl Pts',(-10.2275348110001,15.2,-2.80874883800001));
#268378=CARTESIAN_POINT('Ctrl Pts',(-10.2275348110001,11.6,-2.80874883800002));
#268379=CARTESIAN_POINT('Ctrl Pts',(-10.2254195960001,15.2,-2.80865884700002));
#268380=CARTESIAN_POINT('Ctrl Pts',(-10.2254195960001,11.6,-2.80865884700002));
#268381=CARTESIAN_POINT('Ctrl Pts',(-10.2233112870001,15.2,-2.80856726500001));
#268382=CARTESIAN_POINT('Ctrl Pts',(-10.2233112870001,11.6,-2.80856726500002));
#268383=CARTESIAN_POINT('Ctrl Pts',(-10.2212099030001,15.2,-2.80847410200002));
#268384=CARTESIAN_POINT('Ctrl Pts',(-10.2212099030001,11.6,-2.80847410200002));
#268385=CARTESIAN_POINT('Ctrl Pts',(-10.2191154540001,15.2,-2.80837937100001));
#268386=CARTESIAN_POINT('Ctrl Pts',(-10.2191154540001,11.6,-2.80837937100001));
#268387=CARTESIAN_POINT('Ctrl Pts',(-10.2170279560001,15.2,-2.80828308000002));
#268388=CARTESIAN_POINT('Ctrl Pts',(-10.2170279560001,11.6,-2.80828308000002));
#268389=CARTESIAN_POINT('Ctrl Pts',(-10.2149474230001,15.2,-2.80818524500001));
#268390=CARTESIAN_POINT('Ctrl Pts',(-10.2149474230001,11.6,-2.80818524500001));
#268391=CARTESIAN_POINT('Ctrl Pts',(-10.2128738680001,15.2,-2.80808587500001));
#268392=CARTESIAN_POINT('Ctrl Pts',(-10.2128738680001,11.6,-2.80808587500002));
#268393=CARTESIAN_POINT('Ctrl Pts',(-10.2108073070001,15.2,-2.80798498300001));
#268394=CARTESIAN_POINT('Ctrl Pts',(-10.2108073070001,11.6,-2.80798498300001));
#268395=CARTESIAN_POINT('Ctrl Pts',(-10.2087477520001,15.2,-2.80788258200001));
#268396=CARTESIAN_POINT('Ctrl Pts',(-10.2087477520001,11.6,-2.80788258200001));
#268397=CARTESIAN_POINT('Ctrl Pts',(-10.2066952180001,15.2,-2.80777868100001));
#268398=CARTESIAN_POINT('Ctrl Pts',(-10.2066952180001,11.6,-2.80777868100001));
#268399=CARTESIAN_POINT('Ctrl Pts',(-10.2046497210001,15.2,-2.80767329400001));
#268400=CARTESIAN_POINT('Ctrl Pts',(-10.2046497210001,11.6,-2.80767329400002));
#268401=CARTESIAN_POINT('Ctrl Pts',(-10.2026112720001,15.2,-2.80756643300001));
#268402=CARTESIAN_POINT('Ctrl Pts',(-10.2026112720001,11.6,-2.80756643300002));
#268403=CARTESIAN_POINT('Ctrl Pts',(-10.2005798890001,15.2,-2.80745810900001));
#268404=CARTESIAN_POINT('Ctrl Pts',(-10.2005798890001,11.6,-2.80745810900001));
#268405=CARTESIAN_POINT('Ctrl Pts',(-10.1985555830001,15.2,-2.80734833400002));
#268406=CARTESIAN_POINT('Ctrl Pts',(-10.1985555830001,11.6,-2.80734833400002));
#268407=CARTESIAN_POINT('Ctrl Pts',(-10.1965383710001,15.2,-2.80723712200002));
#268408=CARTESIAN_POINT('Ctrl Pts',(-10.1965383710001,11.6,-2.80723712200002));
#268409=CARTESIAN_POINT('Ctrl Pts',(-10.1945282670001,15.2,-2.80712448400001));
#268410=CARTESIAN_POINT('Ctrl Pts',(-10.1945282670001,11.6,-2.80712448400001));
#268411=CARTESIAN_POINT('Ctrl Pts',(-10.1925252840001,15.2,-2.80701043200001));
#268412=CARTESIAN_POINT('Ctrl Pts',(-10.1925252840001,11.6,-2.80701043200001));
#268413=CARTESIAN_POINT('Ctrl Pts',(-10.1905294380001,15.2,-2.80689497800001));
#268414=CARTESIAN_POINT('Ctrl Pts',(-10.1905294380001,11.6,-2.80689497800001));
#268415=CARTESIAN_POINT('Ctrl Pts',(-10.1885407420001,15.2,-2.80677813600001));
#268416=CARTESIAN_POINT('Ctrl Pts',(-10.1885407420001,11.6,-2.80677813600001));
#268417=CARTESIAN_POINT('Ctrl Pts',(-10.1865592120001,15.2,-2.80665991700001));
#268418=CARTESIAN_POINT('Ctrl Pts',(-10.1865592120001,11.6,-2.80665991700001));
#268419=CARTESIAN_POINT('Ctrl Pts',(-10.1845848630001,15.2,-2.80654033300001));
#268420=CARTESIAN_POINT('Ctrl Pts',(-10.1845848630001,11.6,-2.80654033300001));
#268421=CARTESIAN_POINT('Ctrl Pts',(-10.1826177100001,15.2,-2.80641939900002));
#268422=CARTESIAN_POINT('Ctrl Pts',(-10.1826177100001,11.6,-2.80641939900002));
#268423=CARTESIAN_POINT('Ctrl Pts',(-10.1806577650001,15.2,-2.80629712500001));
#268424=CARTESIAN_POINT('Ctrl Pts',(-10.1806577650001,11.6,-2.80629712500002));
#268425=CARTESIAN_POINT('Ctrl Pts',(-10.1787050450001,15.2,-2.80617352500002));
#268426=CARTESIAN_POINT('Ctrl Pts',(-10.1787050450001,11.6,-2.80617352500002));
#268427=CARTESIAN_POINT('Ctrl Pts',(-10.1767595650001,15.2,-2.80604861000001));
#268428=CARTESIAN_POINT('Ctrl Pts',(-10.1767595650001,11.6,-2.80604861000001));
#268429=CARTESIAN_POINT('Ctrl Pts',(-10.1748213380001,15.2,-2.80592239500002));
#268430=CARTESIAN_POINT('Ctrl Pts',(-10.1748213380001,11.6,-2.80592239500002));
#268431=CARTESIAN_POINT('Ctrl Pts',(-10.1728903810001,15.2,-2.80579489000001));
#268432=CARTESIAN_POINT('Ctrl Pts',(-10.1728903810001,11.6,-2.80579489000001));
#268433=CARTESIAN_POINT('Ctrl Pts',(-10.1709667090001,15.2,-2.80566611100001));
#268434=CARTESIAN_POINT('Ctrl Pts',(-10.1709667090001,11.6,-2.80566611100001));
#268435=CARTESIAN_POINT('Ctrl Pts',(-10.1690503350001,15.2,-2.80553606900002));
#268436=CARTESIAN_POINT('Ctrl Pts',(-10.1690503350001,11.6,-2.80553606900002));
#268437=CARTESIAN_POINT('Ctrl Pts',(-10.1671412760001,15.2,-2.80540477800002));
#268438=CARTESIAN_POINT('Ctrl Pts',(-10.1671412760001,11.6,-2.80540477800002));
#268439=CARTESIAN_POINT('Ctrl Pts',(-10.1652395470001,15.2,-2.80527224900001));
#268440=CARTESIAN_POINT('Ctrl Pts',(-10.1652395470001,11.6,-2.80527224900002));
#268441=CARTESIAN_POINT('Ctrl Pts',(-10.1633451610001,15.2,-2.80513849600001));
#268442=CARTESIAN_POINT('Ctrl Pts',(-10.1633451610001,11.6,-2.80513849600002));
#268443=CARTESIAN_POINT('Ctrl Pts',(-10.1614581350001,15.2,-2.80500353400001));
#268444=CARTESIAN_POINT('Ctrl Pts',(-10.1614581350001,11.6,-2.80500353400001));
#268445=CARTESIAN_POINT('Ctrl Pts',(-10.1595784840001,15.2,-2.80486737300001));
#268446=CARTESIAN_POINT('Ctrl Pts',(-10.1595784840001,11.6,-2.80486737300001));
#268447=CARTESIAN_POINT('Ctrl Pts',(-10.1577062240001,15.2,-2.80473002900001));
#268448=CARTESIAN_POINT('Ctrl Pts',(-10.1577062240001,11.6,-2.80473002900001));
#268449=CARTESIAN_POINT('Ctrl Pts',(-10.1558413680001,15.2,-2.80459151300001));
#268450=CARTESIAN_POINT('Ctrl Pts',(-10.1558413680001,11.6,-2.80459151300001));
#268451=CARTESIAN_POINT('Ctrl Pts',(-10.1539839340001,15.2,-2.80445183900001));
#268452=CARTESIAN_POINT('Ctrl Pts',(-10.1539839340001,11.6,-2.80445183900001));
#268453=CARTESIAN_POINT('Ctrl Pts',(-10.1521339360001,15.2,-2.80431102100001));
#268454=CARTESIAN_POINT('Ctrl Pts',(-10.1521339360001,11.6,-2.80431102100001));
#268455=CARTESIAN_POINT('Ctrl Pts',(-10.1502913890001,15.2,-2.80416907300001));
#268456=CARTESIAN_POINT('Ctrl Pts',(-10.1502913890001,11.6,-2.80416907300001));
#268457=CARTESIAN_POINT('Ctrl Pts',(-10.1484563090001,15.2,-2.80402600700001));
#268458=CARTESIAN_POINT('Ctrl Pts',(-10.1484563090001,11.6,-2.80402600700001));
#268459=CARTESIAN_POINT('Ctrl Pts',(-10.1466287130001,15.2,-2.80388183700001));
#268460=CARTESIAN_POINT('Ctrl Pts',(-10.1466287130001,11.6,-2.80388183700001));
#268461=CARTESIAN_POINT('Ctrl Pts',(-10.1448086140001,15.2,-2.80373657700002));
#268462=CARTESIAN_POINT('Ctrl Pts',(-10.1448086140001,11.6,-2.80373657700002));
#268463=CARTESIAN_POINT('Ctrl Pts',(-10.1429960300001,15.2,-2.80359024000001));
#268464=CARTESIAN_POINT('Ctrl Pts',(-10.1429960300001,11.6,-2.80359024000001));
#268465=CARTESIAN_POINT('Ctrl Pts',(-10.1411909760001,15.2,-2.80344284000002));
#268466=CARTESIAN_POINT('Ctrl Pts',(-10.1411909760001,11.6,-2.80344284000002));
#268467=CARTESIAN_POINT('Ctrl Pts',(-10.1393934660001,15.2,-2.80329439100001));
#268468=CARTESIAN_POINT('Ctrl Pts',(-10.1393934660001,11.6,-2.80329439100001));
#268469=CARTESIAN_POINT('Ctrl Pts',(-10.1376035180001,15.2,-2.80314490700002));
#268470=CARTESIAN_POINT('Ctrl Pts',(-10.1376035180001,11.6,-2.80314490700002));
#268471=CARTESIAN_POINT('Ctrl Pts',(-10.1358211480001,15.2,-2.80299440200002));
#268472=CARTESIAN_POINT('Ctrl Pts',(-10.1358211480001,11.6,-2.80299440200002));
#268473=CARTESIAN_POINT('Ctrl Pts',(-10.1340463700001,15.2,-2.80284288800001));
#268474=CARTESIAN_POINT('Ctrl Pts',(-10.1340463700001,11.6,-2.80284288800001));
#268475=CARTESIAN_POINT('Ctrl Pts',(-10.1322792010001,15.2,-2.80269038200001));
#268476=CARTESIAN_POINT('Ctrl Pts',(-10.1322792010001,11.6,-2.80269038200002));
#268477=CARTESIAN_POINT('Ctrl Pts',(-10.1305196570001,15.2,-2.80253689600002));
#268478=CARTESIAN_POINT('Ctrl Pts',(-10.1305196570001,11.6,-2.80253689600002));
#268479=CARTESIAN_POINT('Ctrl Pts',(-10.1287677530001,15.2,-2.80238244500001));
#268480=CARTESIAN_POINT('Ctrl Pts',(-10.1287677530001,11.6,-2.80238244500001));
#268481=CARTESIAN_POINT('Ctrl Pts',(-10.1270235070001,15.2,-2.80222704300002));
#268482=CARTESIAN_POINT('Ctrl Pts',(-10.1270235070001,11.6,-2.80222704300002));
#268483=CARTESIAN_POINT('Ctrl Pts',(-10.1252869340001,15.2,-2.80207070400001));
#268484=CARTESIAN_POINT('Ctrl Pts',(-10.1252869340001,11.6,-2.80207070400001));
#268485=CARTESIAN_POINT('Ctrl Pts',(-10.1235580500001,15.2,-2.80191344300002));
#268486=CARTESIAN_POINT('Ctrl Pts',(-10.1235580500001,11.6,-2.80191344300002));
#268487=CARTESIAN_POINT('Ctrl Pts',(-10.1218368710001,15.2,-2.80175527400001));
#268488=CARTESIAN_POINT('Ctrl Pts',(-10.1218368710001,11.6,-2.80175527400001));
#268489=CARTESIAN_POINT('Ctrl Pts',(-10.1201234150001,15.2,-2.80159621100001));
#268490=CARTESIAN_POINT('Ctrl Pts',(-10.1201234150001,11.6,-2.80159621100002));
#268491=CARTESIAN_POINT('Ctrl Pts',(-10.1184176970001,15.2,-2.80143626900001));
#268492=CARTESIAN_POINT('Ctrl Pts',(-10.1184176970001,11.6,-2.80143626900002));
#268493=CARTESIAN_POINT('Ctrl Pts',(-10.1167197340001,15.2,-2.80127546300001));
#268494=CARTESIAN_POINT('Ctrl Pts',(-10.1167197340001,11.6,-2.80127546300002));
#268495=CARTESIAN_POINT('Ctrl Pts',(-10.1150295420001,15.2,-2.80111380600002));
#268496=CARTESIAN_POINT('Ctrl Pts',(-10.1150295420001,11.6,-2.80111380600002));
#268497=CARTESIAN_POINT('Ctrl Pts',(-10.1133471370001,15.2,-2.80095131400001));
#268498=CARTESIAN_POINT('Ctrl Pts',(-10.1133471370001,11.6,-2.80095131400001));
#268499=CARTESIAN_POINT('Ctrl Pts',(-10.1116725360001,15.2,-2.80078800200001));
#268500=CARTESIAN_POINT('Ctrl Pts',(-10.1116725360001,11.6,-2.80078800200001));
#268501=CARTESIAN_POINT('Ctrl Pts',(-10.1100057560001,15.2,-2.80062388500002));
#268502=CARTESIAN_POINT('Ctrl Pts',(-10.1100057560001,11.6,-2.80062388500002));
#268503=CARTESIAN_POINT('Ctrl Pts',(-10.1083468140001,15.2,-2.80045897600001));
#268504=CARTESIAN_POINT('Ctrl Pts',(-10.1083468140001,11.6,-2.80045897600001));
#268505=CARTESIAN_POINT('Ctrl Pts',(-10.1066957250001,15.2,-2.80029329300001));
#268506=CARTESIAN_POINT('Ctrl Pts',(-10.1066957250001,11.6,-2.80029329300001));
#268507=CARTESIAN_POINT('Ctrl Pts',(-10.1050525090001,15.2,-2.80012684900001));
#268508=CARTESIAN_POINT('Ctrl Pts',(-10.1050525090001,11.6,-2.80012684900001));
#268509=CARTESIAN_POINT('Ctrl Pts',(-10.1034171790001,15.2,-2.79995965800001));
#268510=CARTESIAN_POINT('Ctrl Pts',(-10.1034171790001,11.6,-2.79995965800001));
#268511=CARTESIAN_POINT('Ctrl Pts',(-10.1017897540001,15.2,-2.79979173800001));
#268512=CARTESIAN_POINT('Ctrl Pts',(-10.1017897540001,11.6,-2.79979173800002));
#268513=CARTESIAN_POINT('Ctrl Pts',(-10.1001702510001,15.2,-2.79962310200002));
#268514=CARTESIAN_POINT('Ctrl Pts',(-10.1001702510001,11.6,-2.79962310200002));
#268515=CARTESIAN_POINT('Ctrl Pts',(-10.0985586870001,15.2,-2.79945376700002));
#268516=CARTESIAN_POINT('Ctrl Pts',(-10.0985586870001,11.6,-2.79945376700002));
#268517=CARTESIAN_POINT('Ctrl Pts',(-10.0969550780001,15.2,-2.79928374700001));
#268518=CARTESIAN_POINT('Ctrl Pts',(-10.0969550780001,11.6,-2.79928374700001));
#268519=CARTESIAN_POINT('Ctrl Pts',(-10.0953594420001,15.2,-2.79911305800002));
#268520=CARTESIAN_POINT('Ctrl Pts',(-10.0953594420001,11.6,-2.79911305800002));
#268521=CARTESIAN_POINT('Ctrl Pts',(-10.0937717960001,15.2,-2.79894171500001));
#268522=CARTESIAN_POINT('Ctrl Pts',(-10.0937717960001,11.6,-2.79894171500001));
#268523=CARTESIAN_POINT('Ctrl Pts',(-10.0921921570001,15.2,-2.79876973500001));
#268524=CARTESIAN_POINT('Ctrl Pts',(-10.0921921570001,11.6,-2.79876973500001));
#268525=CARTESIAN_POINT('Ctrl Pts',(-10.0906205420001,15.2,-2.79859713200001));
#268526=CARTESIAN_POINT('Ctrl Pts',(-10.0906205420001,11.6,-2.79859713200001));
#268527=CARTESIAN_POINT('Ctrl Pts',(-10.0890569700001,15.2,-2.79842392300001));
#268528=CARTESIAN_POINT('Ctrl Pts',(-10.0890569700001,11.6,-2.79842392300001));
#268529=CARTESIAN_POINT('Ctrl Pts',(-10.0875014570001,15.2,-2.79825012400002));
#268530=CARTESIAN_POINT('Ctrl Pts',(-10.0875014570001,11.6,-2.79825012400002));
#268531=CARTESIAN_POINT('Ctrl Pts',(-10.0859540200001,15.2,-2.79807574900001));
#268532=CARTESIAN_POINT('Ctrl Pts',(-10.0859540200001,11.6,-2.79807574900001));
#268533=CARTESIAN_POINT('Ctrl Pts',(-10.0844146780001,15.2,-2.79790081600002));
#268534=CARTESIAN_POINT('Ctrl Pts',(-10.0844146780001,11.6,-2.79790081600002));
#268535=CARTESIAN_POINT('Ctrl Pts',(-10.0828834480001,15.2,-2.79772534000001));
#268536=CARTESIAN_POINT('Ctrl Pts',(-10.0828834480001,11.6,-2.79772534000002));
#268537=CARTESIAN_POINT('Ctrl Pts',(-10.0813603480001,15.2,-2.79754933600001));
#268538=CARTESIAN_POINT('Ctrl Pts',(-10.0813603480001,11.6,-2.79754933600001));
#268539=CARTESIAN_POINT('Ctrl Pts',(-10.0798453950001,15.2,-2.79737282200001));
#268540=CARTESIAN_POINT('Ctrl Pts',(-10.0798453950001,11.6,-2.79737282200002));
#268541=CARTESIAN_POINT('Ctrl Pts',(-10.0783386060001,15.2,-2.79719581400002));
#268542=CARTESIAN_POINT('Ctrl Pts',(-10.0783386060001,11.6,-2.79719581400002));
#268543=CARTESIAN_POINT('Ctrl Pts',(-10.0768400010001,15.2,-2.79701832800002));
#268544=CARTESIAN_POINT('Ctrl Pts',(-10.0768400010001,11.6,-2.79701832800002));
#268545=CARTESIAN_POINT('Ctrl Pts',(-10.0753495960001,15.2,-2.79684038000001));
#268546=CARTESIAN_POINT('Ctrl Pts',(-10.0753495960001,11.6,-2.79684038000001));
#268547=CARTESIAN_POINT('Ctrl Pts',(-10.0738674120001,15.2,-2.79666198700002));
#268548=CARTESIAN_POINT('Ctrl Pts',(-10.0738674120001,11.6,-2.79666198700002));
#268549=CARTESIAN_POINT('Ctrl Pts',(-10.0723934620001,15.2,-2.79648316500001));
#268550=CARTESIAN_POINT('Ctrl Pts',(-10.0723934620001,11.6,-2.79648316500001));
#268551=CARTESIAN_POINT('Ctrl Pts',(-10.0709277690001,15.2,-2.79630393100001));
#268552=CARTESIAN_POINT('Ctrl Pts',(-10.0709277690001,11.6,-2.79630393100002));
#268553=CARTESIAN_POINT('Ctrl Pts',(-10.0694703480001,15.2,-2.79612430200002));
#268554=CARTESIAN_POINT('Ctrl Pts',(-10.0694703480001,11.6,-2.79612430200002));
#268555=CARTESIAN_POINT('Ctrl Pts',(-10.0680212180001,15.2,-2.79594429400001));
#268556=CARTESIAN_POINT('Ctrl Pts',(-10.0680212180001,11.6,-2.79594429400001));
#268557=CARTESIAN_POINT('Ctrl Pts',(-10.0665803990001,15.2,-2.79576392500001));
#268558=CARTESIAN_POINT('Ctrl Pts',(-10.0665803990001,11.6,-2.79576392500001));
#268559=CARTESIAN_POINT('Ctrl Pts',(-10.0651479080001,15.2,-2.79558321000001));
#268560=CARTESIAN_POINT('Ctrl Pts',(-10.0651479080001,11.6,-2.79558321000001));
#268561=CARTESIAN_POINT('Ctrl Pts',(-10.0637237620001,15.2,-2.79540216900001));
#268562=CARTESIAN_POINT('Ctrl Pts',(-10.0637237620001,11.6,-2.79540216900001));
#268563=CARTESIAN_POINT('Ctrl Pts',(-10.0623079820001,15.2,-2.79522081700001));
#268564=CARTESIAN_POINT('Ctrl Pts',(-10.0623079820001,11.6,-2.79522081700002));
#268565=CARTESIAN_POINT('Ctrl Pts',(-10.0609005850001,15.2,-2.79503917100001));
#268566=CARTESIAN_POINT('Ctrl Pts',(-10.0609005850001,11.6,-2.79503917100001));
#268567=CARTESIAN_POINT('Ctrl Pts',(-10.0595015910001,15.2,-2.79485724800002));
#268568=CARTESIAN_POINT('Ctrl Pts',(-10.0595015910001,11.6,-2.79485724800002));
#268569=CARTESIAN_POINT('Ctrl Pts',(-10.0581110160001,15.2,-2.79467506700001));
#268570=CARTESIAN_POINT('Ctrl Pts',(-10.0581110160001,11.6,-2.79467506700001));
#268571=CARTESIAN_POINT('Ctrl Pts',(-10.0567288820001,15.2,-2.79449264500002));
#268572=CARTESIAN_POINT('Ctrl Pts',(-10.0567288820001,11.6,-2.79449264500002));
#268573=CARTESIAN_POINT('Ctrl Pts',(-10.0553552060001,15.2,-2.79430999900002));
#268574=CARTESIAN_POINT('Ctrl Pts',(-10.0553552060001,11.6,-2.79430999900002));
#268575=CARTESIAN_POINT('Ctrl Pts',(-10.0539900080001,15.2,-2.79412714600001));
#268576=CARTESIAN_POINT('Ctrl Pts',(-10.0539900080001,11.6,-2.79412714600001));
#268577=CARTESIAN_POINT('Ctrl Pts',(-10.0526333070001,15.2,-2.79394410600001));
#268578=CARTESIAN_POINT('Ctrl Pts',(-10.0526333070001,11.6,-2.79394410600002));
#268579=CARTESIAN_POINT('Ctrl Pts',(-10.0512851200001,15.2,-2.79376089400001));
#268580=CARTESIAN_POINT('Ctrl Pts',(-10.0512851200001,11.6,-2.79376089400001));
#268581=CARTESIAN_POINT('Ctrl Pts',(-10.0499454690001,15.2,-2.79357752900002));
#268582=CARTESIAN_POINT('Ctrl Pts',(-10.0499454690001,11.6,-2.79357752900002));
#268583=CARTESIAN_POINT('Ctrl Pts',(-10.0486143700001,15.2,-2.79339402900002));
#268584=CARTESIAN_POINT('Ctrl Pts',(-10.0486143700001,11.6,-2.79339402900002));
#268585=CARTESIAN_POINT('Ctrl Pts',(-10.0472918460001,15.2,-2.79321041100001));
#268586=CARTESIAN_POINT('Ctrl Pts',(-10.0472918460001,11.6,-2.79321041100001));
#268587=CARTESIAN_POINT('Ctrl Pts',(-10.0459779130001,15.2,-2.79302669500002));
#268588=CARTESIAN_POINT('Ctrl Pts',(-10.0459779130001,11.6,-2.79302669500002));
#268589=CARTESIAN_POINT('Ctrl Pts',(-10.0446725930001,15.2,-2.79284289900001));
#268590=CARTESIAN_POINT('Ctrl Pts',(-10.0446725930001,11.6,-2.79284289900001));
#268591=CARTESIAN_POINT('Ctrl Pts',(-10.0433759040001,15.2,-2.79265904000002));
#268592=CARTESIAN_POINT('Ctrl Pts',(-10.0433759040001,11.6,-2.79265904000002));
#268593=CARTESIAN_POINT('Ctrl Pts',(-10.0420878650001,15.2,-2.79247513800001));
#268594=CARTESIAN_POINT('Ctrl Pts',(-10.0420878650001,11.6,-2.79247513800002));
#268595=CARTESIAN_POINT('Ctrl Pts',(-10.0408084970001,15.2,-2.79229120900002));
#268596=CARTESIAN_POINT('Ctrl Pts',(-10.0408084970001,11.6,-2.79229120900002));
#268597=CARTESIAN_POINT('Ctrl Pts',(-10.0395378210001,15.2,-2.79210727300002));
#268598=CARTESIAN_POINT('Ctrl Pts',(-10.0395378210001,11.6,-2.79210727300002));
#268599=CARTESIAN_POINT('Ctrl Pts',(-10.0382758530001,15.2,-2.79192335000001));
#268600=CARTESIAN_POINT('Ctrl Pts',(-10.0382758530001,11.6,-2.79192335000001));
#268601=CARTESIAN_POINT('Ctrl Pts',(-10.0370226160001,15.2,-2.79173945600002));
#268602=CARTESIAN_POINT('Ctrl Pts',(-10.0370226160001,11.6,-2.79173945600002));
#268603=CARTESIAN_POINT('Ctrl Pts',(-10.0357781300001,15.2,-2.79155561300001));
#268604=CARTESIAN_POINT('Ctrl Pts',(-10.0357781300001,11.6,-2.79155561300001));
#268605=CARTESIAN_POINT('Ctrl Pts',(-10.0345424120001,15.2,-2.79137183600001));
#268606=CARTESIAN_POINT('Ctrl Pts',(-10.0345424120001,11.6,-2.79137183600001));
#268607=CARTESIAN_POINT('Ctrl Pts',(-10.0333154850001,15.2,-2.79118814800002));
#268608=CARTESIAN_POINT('Ctrl Pts',(-10.0333154850001,11.6,-2.79118814800002));
#268609=CARTESIAN_POINT('Ctrl Pts',(-10.0320973690001,15.2,-2.79100456500001));
#268610=CARTESIAN_POINT('Ctrl Pts',(-10.0320973690001,11.6,-2.79100456500002));
#268611=CARTESIAN_POINT('Ctrl Pts',(-10.0308880840001,15.2,-2.79082110900001));
#268612=CARTESIAN_POINT('Ctrl Pts',(-10.0308880840001,11.6,-2.79082110900002));
#268613=CARTESIAN_POINT('Ctrl Pts',(-10.0296876490001,15.2,-2.79063779700001));
#268614=CARTESIAN_POINT('Ctrl Pts',(-10.0296876490001,11.6,-2.79063779700001));
#268615=CARTESIAN_POINT('Ctrl Pts',(-10.0284960860001,15.2,-2.79045465000001));
#268616=CARTESIAN_POINT('Ctrl Pts',(-10.0284960860001,11.6,-2.79045465000001));
#268617=CARTESIAN_POINT('Ctrl Pts',(-10.0273134150001,15.2,-2.79027168600001));
#268618=CARTESIAN_POINT('Ctrl Pts',(-10.0273134150001,11.6,-2.79027168600001));
#268619=CARTESIAN_POINT('Ctrl Pts',(-10.0261396570001,15.2,-2.79008892600002));
#268620=CARTESIAN_POINT('Ctrl Pts',(-10.0261396570001,11.6,-2.79008892600002));
#268621=CARTESIAN_POINT('Ctrl Pts',(-10.0249748320001,15.2,-2.78990638900002));
#268622=CARTESIAN_POINT('Ctrl Pts',(-10.0249748320001,11.6,-2.78990638900002));
#268623=CARTESIAN_POINT('Ctrl Pts',(-10.0238189610001,15.2,-2.78972409500001));
#268624=CARTESIAN_POINT('Ctrl Pts',(-10.0238189610001,11.6,-2.78972409500002));
#268625=CARTESIAN_POINT('Ctrl Pts',(-10.0226720660001,15.2,-2.78954206400002));
#268626=CARTESIAN_POINT('Ctrl Pts',(-10.0226720660001,11.6,-2.78954206400002));
#268627=CARTESIAN_POINT('Ctrl Pts',(-10.0215341660001,15.2,-2.78936031700002));
#268628=CARTESIAN_POINT('Ctrl Pts',(-10.0215341660001,11.6,-2.78936031700002));
#268629=CARTESIAN_POINT('Ctrl Pts',(-10.0204052840001,15.2,-2.78917887200001));
#268630=CARTESIAN_POINT('Ctrl Pts',(-10.0204052840001,11.6,-2.78917887200001));
#268631=CARTESIAN_POINT('Ctrl Pts',(-10.0192854400001,15.2,-2.78899774900002));
#268632=CARTESIAN_POINT('Ctrl Pts',(-10.0192854400001,11.6,-2.78899774900002));
#268633=CARTESIAN_POINT('Ctrl Pts',(-10.0181746550001,15.2,-2.78881697100001));
#268634=CARTESIAN_POINT('Ctrl Pts',(-10.0181746550001,11.6,-2.78881697100001));
#268635=CARTESIAN_POINT('Ctrl Pts',(-10.0170729510001,15.2,-2.78863655800001));
#268636=CARTESIAN_POINT('Ctrl Pts',(-10.0170729510001,11.6,-2.78863655800001));
#268637=CARTESIAN_POINT('Ctrl Pts',(-10.0159803500001,15.2,-2.78845652900001));
#268638=CARTESIAN_POINT('Ctrl Pts',(-10.0159803500001,11.6,-2.78845652900001));
#268639=CARTESIAN_POINT('Ctrl Pts',(-10.0148968710001,15.2,-2.78827690400002));
#268640=CARTESIAN_POINT('Ctrl Pts',(-10.0148968710001,11.6,-2.78827690400002));
#268641=CARTESIAN_POINT('Ctrl Pts',(-10.0138225390001,15.2,-2.78809770600001));
#268642=CARTESIAN_POINT('Ctrl Pts',(-10.0138225390001,11.6,-2.78809770600001));
#268643=CARTESIAN_POINT('Ctrl Pts',(-10.0127573730001,15.2,-2.78791895500001));
#268644=CARTESIAN_POINT('Ctrl Pts',(-10.0127573730001,11.6,-2.78791895500001));
#268645=CARTESIAN_POINT('Ctrl Pts',(-10.0117013970001,15.2,-2.78774067200001));
#268646=CARTESIAN_POINT('Ctrl Pts',(-10.0117013970001,11.6,-2.78774067200001));
#268647=CARTESIAN_POINT('Ctrl Pts',(-10.0106546300001,15.2,-2.78756287700002));
#268648=CARTESIAN_POINT('Ctrl Pts',(-10.0106546300001,11.6,-2.78756287700002));
#268649=CARTESIAN_POINT('Ctrl Pts',(-10.0096170970001,15.2,-2.78738559300002));
#268650=CARTESIAN_POINT('Ctrl Pts',(-10.0096170970001,11.6,-2.78738559300002));
#268651=CARTESIAN_POINT('Ctrl Pts',(-10.0085888180001,15.2,-2.78720884000002));
#268652=CARTESIAN_POINT('Ctrl Pts',(-10.0085888180001,11.6,-2.78720884000002));
#268653=CARTESIAN_POINT('Ctrl Pts',(-10.0075698160001,15.2,-2.78703264000002));
#268654=CARTESIAN_POINT('Ctrl Pts',(-10.0075698160001,11.6,-2.78703264000002));
#268655=CARTESIAN_POINT('Ctrl Pts',(-10.0065601130001,15.2,-2.78685701400001));
#268656=CARTESIAN_POINT('Ctrl Pts',(-10.0065601130001,11.6,-2.78685701400002));
#268657=CARTESIAN_POINT('Ctrl Pts',(-10.0055597320001,15.2,-2.78668198500001));
#268658=CARTESIAN_POINT('Ctrl Pts',(-10.0055597320001,11.6,-2.78668198500002));
#268659=CARTESIAN_POINT('Ctrl Pts',(-10.0045686950001,15.2,-2.78650757300001));
#268660=CARTESIAN_POINT('Ctrl Pts',(-10.0045686950001,11.6,-2.78650757300001));
#268661=CARTESIAN_POINT('Ctrl Pts',(-10.0035870240001,15.2,-2.78633380100001));
#268662=CARTESIAN_POINT('Ctrl Pts',(-10.0035870240001,11.6,-2.78633380100001));
#268663=CARTESIAN_POINT('Ctrl Pts',(-10.0026147430001,15.2,-2.78616069100002));
#268664=CARTESIAN_POINT('Ctrl Pts',(-10.0026147430001,11.6,-2.78616069100002));
#268665=CARTESIAN_POINT('Ctrl Pts',(-10.0016518730001,15.2,-2.78598826400001));
#268666=CARTESIAN_POINT('Ctrl Pts',(-10.0016518730001,11.6,-2.78598826400001));
#268667=CARTESIAN_POINT('Ctrl Pts',(-10.0006984370001,15.2,-2.78581654400002));
#268668=CARTESIAN_POINT('Ctrl Pts',(-10.0006984370001,11.6,-2.78581654400002));
#268669=CARTESIAN_POINT('Ctrl Pts',(-9.99975446000006,15.2,-2.78564555200001));
#268670=CARTESIAN_POINT('Ctrl Pts',(-9.99975446000006,11.6,-2.78564555200001));
#268671=CARTESIAN_POINT('Ctrl Pts',(-9.99881996400006,15.2,-2.78547531100001));
#268672=CARTESIAN_POINT('Ctrl Pts',(-9.99881996400006,11.6,-2.78547531100001));
#268673=CARTESIAN_POINT('Ctrl Pts',(-9.99789497300006,15.2,-2.78530584400002));
#268674=CARTESIAN_POINT('Ctrl Pts',(-9.99789497300006,11.6,-2.78530584400002));
#268675=CARTESIAN_POINT('Ctrl Pts',(-9.99697950700006,15.2,-2.78513717200001));
#268676=CARTESIAN_POINT('Ctrl Pts',(-9.99697950700006,11.6,-2.78513717200001));
#268677=CARTESIAN_POINT('Ctrl Pts',(-9.99607881100006,15.2,-2.78497028600002));
#268678=CARTESIAN_POINT('Ctrl Pts',(-9.99607881100006,11.6,-2.78497028600002));
#268679=CARTESIAN_POINT('Ctrl Pts',(-9.99536684700006,15.2,-2.78483763500001));
#268680=CARTESIAN_POINT('Ctrl Pts',(-9.99536684700006,11.6,-2.78483763500002));
#268681=CARTESIAN_POINT('Ctrl Pts',(-9.99483840000006,15.2,-2.78473877000001));
#268682=CARTESIAN_POINT('Ctrl Pts',(-9.99483840000006,11.6,-2.78473877000002));
#268683=CARTESIAN_POINT('Ctrl Pts',(-9.99448967800006,15.2,-2.78467334900002));
#268684=CARTESIAN_POINT('Ctrl Pts',(-9.99448967800006,11.6,-2.78467334900002));
#268685=CARTESIAN_POINT('Ctrl Pts',(-9.99431831700005,15.2,-2.78464115900002));
#268686=CARTESIAN_POINT('Ctrl Pts',(-9.99431831700005,11.6,-2.78464115900002));
#268687=CARTESIAN_POINT('',(-9.99431831700005,12.2,-2.78464115900002));
#268688=CARTESIAN_POINT('',(-9.99431831700005,15.2,-2.78464115900002));
#268689=CARTESIAN_POINT('',(-9.99431831700005,12.2,-2.78464115900002));
#268690=CARTESIAN_POINT('Ctrl Pts',(-11.1757778680001,12.2,-2.71145515300002));
#268691=CARTESIAN_POINT('Ctrl Pts',(-11.1750309950001,12.2,-2.71161876900001));
#268692=CARTESIAN_POINT('Ctrl Pts',(-11.1735376180001,12.2,-2.71194562400002));
#268693=CARTESIAN_POINT('Ctrl Pts',(-11.1712986600001,12.2,-2.71243478000001));
#268694=CARTESIAN_POINT('Ctrl Pts',(-11.1683155990001,12.2,-2.71308473500001));
#268695=CARTESIAN_POINT('Ctrl Pts',(-11.1645904650001,12.2,-2.71389342400001));
#268696=CARTESIAN_POINT('Ctrl Pts',(-11.1608690250001,12.2,-2.71469835800001));
#268697=CARTESIAN_POINT('Ctrl Pts',(-11.1571512810001,12.2,-2.71549953800001));
#268698=CARTESIAN_POINT('Ctrl Pts',(-11.1534372360001,12.2,-2.71629696600002));
#268699=CARTESIAN_POINT('Ctrl Pts',(-11.1497268980001,12.2,-2.71709064400001));
#268700=CARTESIAN_POINT('Ctrl Pts',(-11.1460202710001,12.2,-2.71788057600002));
#268701=CARTESIAN_POINT('Ctrl Pts',(-11.1423173660001,12.2,-2.71866676600002));
#268702=CARTESIAN_POINT('Ctrl Pts',(-11.1386181920001,12.2,-2.71944921800001));
#268703=CARTESIAN_POINT('Ctrl Pts',(-11.1349227590001,12.2,-2.72022793900002));
#268704=CARTESIAN_POINT('Ctrl Pts',(-11.1312310760001,12.2,-2.72100293300001));
#268705=CARTESIAN_POINT('Ctrl Pts',(-11.1275431540001,12.2,-2.72177420400002));
#268706=CARTESIAN_POINT('Ctrl Pts',(-11.1238590000001,12.2,-2.72254175700001));
#268707=CARTESIAN_POINT('Ctrl Pts',(-11.1201786230001,12.2,-2.72330559600002));
#268708=CARTESIAN_POINT('Ctrl Pts',(-11.1165020290001,12.2,-2.72406572300001));
#268709=CARTESIAN_POINT('Ctrl Pts',(-11.1128292270001,12.2,-2.72482214500001));
#268710=CARTESIAN_POINT('Ctrl Pts',(-11.1091602230001,12.2,-2.72557486300002));
#268711=CARTESIAN_POINT('Ctrl Pts',(-11.1054950240001,12.2,-2.72632388100002));
#268712=CARTESIAN_POINT('Ctrl Pts',(-11.1018336410001,12.2,-2.72706920300001));
#268713=CARTESIAN_POINT('Ctrl Pts',(-11.0981760790001,12.2,-2.72781083400002));
#268714=CARTESIAN_POINT('Ctrl Pts',(-11.0945223470001,12.2,-2.72854877900001));
#268715=CARTESIAN_POINT('Ctrl Pts',(-11.0908724560001,12.2,-2.72928304000001));
#268716=CARTESIAN_POINT('Ctrl Pts',(-11.0872264110001,12.2,-2.73001362300001));
#268717=CARTESIAN_POINT('Ctrl Pts',(-11.0835842240001,12.2,-2.73074053200002));
#268718=CARTESIAN_POINT('Ctrl Pts',(-11.0799458990001,12.2,-2.73146377200002));
#268719=CARTESIAN_POINT('Ctrl Pts',(-11.0763114490001,12.2,-2.73218334500001));
#268720=CARTESIAN_POINT('Ctrl Pts',(-11.0726808780001,12.2,-2.73289925600002));
#268721=CARTESIAN_POINT('Ctrl Pts',(-11.0690541960001,12.2,-2.73361151100001));
#268722=CARTESIAN_POINT('Ctrl Pts',(-11.0654314110001,12.2,-2.73432011200001));
#268723=CARTESIAN_POINT('Ctrl Pts',(-11.0618125300001,12.2,-2.73502506300002));
#268724=CARTESIAN_POINT('Ctrl Pts',(-11.0581975630001,12.2,-2.73572637000001));
#268725=CARTESIAN_POINT('Ctrl Pts',(-11.0545865170001,12.2,-2.73642403700002));
#268726=CARTESIAN_POINT('Ctrl Pts',(-11.0509794010001,12.2,-2.73711806700002));
#268727=CARTESIAN_POINT('Ctrl Pts',(-11.0473762230001,12.2,-2.73780846600001));
#268728=CARTESIAN_POINT('Ctrl Pts',(-11.0437769920001,12.2,-2.73849523700001));
#268729=CARTESIAN_POINT('Ctrl Pts',(-11.0401817150001,12.2,-2.73917838500001));
#268730=CARTESIAN_POINT('Ctrl Pts',(-11.0365904010001,12.2,-2.73985791400001));
#268731=CARTESIAN_POINT('Ctrl Pts',(-11.0330030590001,12.2,-2.74053382800002));
#268732=CARTESIAN_POINT('Ctrl Pts',(-11.0294196970001,12.2,-2.74120613200001));
#268733=CARTESIAN_POINT('Ctrl Pts',(-11.0258403220001,12.2,-2.74187483000001));
#268734=CARTESIAN_POINT('Ctrl Pts',(-11.0222649450001,12.2,-2.74253992800002));
#268735=CARTESIAN_POINT('Ctrl Pts',(-11.0186935710001,12.2,-2.74320142800001));
#268736=CARTESIAN_POINT('Ctrl Pts',(-11.0151262110001,12.2,-2.74385933600001));
#268737=CARTESIAN_POINT('Ctrl Pts',(-11.0115628720001,12.2,-2.74451365600001));
#268738=CARTESIAN_POINT('Ctrl Pts',(-11.0080035640001,12.2,-2.74516439200001));
#268739=CARTESIAN_POINT('Ctrl Pts',(-11.0044482940001,12.2,-2.74581155000002));
#268740=CARTESIAN_POINT('Ctrl Pts',(-11.0008970700001,12.2,-2.74645513200001));
#268741=CARTESIAN_POINT('Ctrl Pts',(-10.9973499030001,12.2,-2.74709514500001));
#268742=CARTESIAN_POINT('Ctrl Pts',(-10.9938067980001,12.2,-2.74773159100001));
#268743=CARTESIAN_POINT('Ctrl Pts',(-10.9902677660001,12.2,-2.74836447800002));
#268744=CARTESIAN_POINT('Ctrl Pts',(-10.9867328140001,12.2,-2.74899380700001));
#268745=CARTESIAN_POINT('Ctrl Pts',(-10.9832019520001,12.2,-2.74961958600001));
#268746=CARTESIAN_POINT('Ctrl Pts',(-10.9796751870001,12.2,-2.75024181600001));
#268747=CARTESIAN_POINT('Ctrl Pts',(-10.9761525290001,12.2,-2.75086050400001));
#268748=CARTESIAN_POINT('Ctrl Pts',(-10.9726339840001,12.2,-2.75147565300002));
#268749=CARTESIAN_POINT('Ctrl Pts',(-10.9691195640001,12.2,-2.75208727000001));
#268750=CARTESIAN_POINT('Ctrl Pts',(-10.9656092750001,12.2,-2.75269535800001));
#268751=CARTESIAN_POINT('Ctrl Pts',(-10.9621031260001,12.2,-2.75329992100001));
#268752=CARTESIAN_POINT('Ctrl Pts',(-10.9586011260001,12.2,-2.75390096500002));
#268753=CARTESIAN_POINT('Ctrl Pts',(-10.9551032830001,12.2,-2.75449849500002));
#268754=CARTESIAN_POINT('Ctrl Pts',(-10.9516096070001,12.2,-2.75509251400001));
#268755=CARTESIAN_POINT('Ctrl Pts',(-10.9481201050001,12.2,-2.75568302700002));
#268756=CARTESIAN_POINT('Ctrl Pts',(-10.9446347860001,12.2,-2.75627004100001));
#268757=CARTESIAN_POINT('Ctrl Pts',(-10.9411536590001,12.2,-2.75685355800002));
#268758=CARTESIAN_POINT('Ctrl Pts',(-10.9376767320001,12.2,-2.75743358500002));
#268759=CARTESIAN_POINT('Ctrl Pts',(-10.9342040160001,12.2,-2.75801012600001));
#268760=CARTESIAN_POINT('Ctrl Pts',(-10.9307355160001,12.2,-2.75858318400001));
#268761=CARTESIAN_POINT('Ctrl Pts',(-10.9272712420001,12.2,-2.75915276600001));
#268762=CARTESIAN_POINT('Ctrl Pts',(-10.9238112040001,12.2,-2.75971887600001));
#268763=CARTESIAN_POINT('Ctrl Pts',(-10.9203554100001,12.2,-2.76028151900002));
#268764=CARTESIAN_POINT('Ctrl Pts',(-10.9169038680001,12.2,-2.76084070000001));
#268765=CARTESIAN_POINT('Ctrl Pts',(-10.9134565880001,12.2,-2.76139642400001));
#268766=CARTESIAN_POINT('Ctrl Pts',(-10.9100135780001,12.2,-2.76194869600001));
#268767=CARTESIAN_POINT('Ctrl Pts',(-10.9065748460001,12.2,-2.76249752000002));
#268768=CARTESIAN_POINT('Ctrl Pts',(-10.9031404020001,12.2,-2.76304290100001));
#268769=CARTESIAN_POINT('Ctrl Pts',(-10.8997102540001,12.2,-2.76358484600001));
#268770=CARTESIAN_POINT('Ctrl Pts',(-10.8962844110001,12.2,-2.76412335800002));
#268771=CARTESIAN_POINT('Ctrl Pts',(-10.8928628820001,12.2,-2.76465844200001));
#268772=CARTESIAN_POINT('Ctrl Pts',(-10.8894456750001,12.2,-2.76519010300001));
#268773=CARTESIAN_POINT('Ctrl Pts',(-10.8860328000001,12.2,-2.76571834600002));
#268774=CARTESIAN_POINT('Ctrl Pts',(-10.8826242650001,12.2,-2.76624317800001));
#268775=CARTESIAN_POINT('Ctrl Pts',(-10.8792200800001,12.2,-2.76676460200001));
#268776=CARTESIAN_POINT('Ctrl Pts',(-10.8758202520001,12.2,-2.76728262200002));
#268777=CARTESIAN_POINT('Ctrl Pts',(-10.8724247920001,12.2,-2.76779724700001));
#268778=CARTESIAN_POINT('Ctrl Pts',(-10.8690337060001,12.2,-2.76830847900001));
#268779=CARTESIAN_POINT('Ctrl Pts',(-10.8656470060001,12.2,-2.76881632300002));
#268780=CARTESIAN_POINT('Ctrl Pts',(-10.8622646980001,12.2,-2.76932078500002));
#268781=CARTESIAN_POINT('Ctrl Pts',(-10.8588867940001,12.2,-2.76982187100002));
#268782=CARTESIAN_POINT('Ctrl Pts',(-10.8555133010001,12.2,-2.77031958400002));
#268783=CARTESIAN_POINT('Ctrl Pts',(-10.8521442280001,12.2,-2.77081393100001));
#268784=CARTESIAN_POINT('Ctrl Pts',(-10.8487795840001,12.2,-2.77130491700001));
#268785=CARTESIAN_POINT('Ctrl Pts',(-10.8454193790001,12.2,-2.77179254700001));
#268786=CARTESIAN_POINT('Ctrl Pts',(-10.8420636210001,12.2,-2.77227682600001));
#268787=CARTESIAN_POINT('Ctrl Pts',(-10.8387123200001,12.2,-2.77275775900002));
#268788=CARTESIAN_POINT('Ctrl Pts',(-10.8353654830001,12.2,-2.77323535200001));
#268789=CARTESIAN_POINT('Ctrl Pts',(-10.8320231210001,12.2,-2.77370961000001));
#268790=CARTESIAN_POINT('Ctrl Pts',(-10.8286852410001,12.2,-2.77418053700002));
#268791=CARTESIAN_POINT('Ctrl Pts',(-10.8253518550001,12.2,-2.77464814100002));
#268792=CARTESIAN_POINT('Ctrl Pts',(-10.8220229700001,12.2,-2.77511242500001));
#268793=CARTESIAN_POINT('Ctrl Pts',(-10.8186985940001,12.2,-2.77557339600001));
#268794=CARTESIAN_POINT('Ctrl Pts',(-10.8153787400001,12.2,-2.77603105800001));
#268795=CARTESIAN_POINT('Ctrl Pts',(-10.8120634130001,12.2,-2.77648541700001));
#268796=CARTESIAN_POINT('Ctrl Pts',(-10.8087526240001,12.2,-2.77693647800001));
#268797=CARTESIAN_POINT('Ctrl Pts',(-10.8054463820001,12.2,-2.77738424700001));
#268798=CARTESIAN_POINT('Ctrl Pts',(-10.8021446960001,12.2,-2.77782872900001));
#268799=CARTESIAN_POINT('Ctrl Pts',(-10.7988475760001,12.2,-2.77826993000001));
#268800=CARTESIAN_POINT('Ctrl Pts',(-10.7955550300001,12.2,-2.77870785600001));
#268801=CARTESIAN_POINT('Ctrl Pts',(-10.7922670680001,12.2,-2.77914251000002));
#268802=CARTESIAN_POINT('Ctrl Pts',(-10.7889836990001,12.2,-2.77957390000001));
#268803=CARTESIAN_POINT('Ctrl Pts',(-10.7857049310001,12.2,-2.78000203100001));
#268804=CARTESIAN_POINT('Ctrl Pts',(-10.7824307750001,12.2,-2.78042690900001));
#268805=CARTESIAN_POINT('Ctrl Pts',(-10.7791612390001,12.2,-2.78084853700001));
#268806=CARTESIAN_POINT('Ctrl Pts',(-10.7758963330001,12.2,-2.78126692300001));
#268807=CARTESIAN_POINT('Ctrl Pts',(-10.7726360660001,12.2,-2.78168207300002));
#268808=CARTESIAN_POINT('Ctrl Pts',(-10.7693804470001,12.2,-2.78209399100001));
#268809=CARTESIAN_POINT('Ctrl Pts',(-10.7661294860001,12.2,-2.78250268300001));
#268810=CARTESIAN_POINT('Ctrl Pts',(-10.7628831920001,12.2,-2.78290815600001));
#268811=CARTESIAN_POINT('Ctrl Pts',(-10.7596415740001,12.2,-2.78331041300001));
#268812=CARTESIAN_POINT('Ctrl Pts',(-10.7564046420001,12.2,-2.78370946300001));
#268813=CARTESIAN_POINT('Ctrl Pts',(-10.7531724040001,12.2,-2.78410530900001));
#268814=CARTESIAN_POINT('Ctrl Pts',(-10.7499448710001,12.2,-2.78449795800002));
#268815=CARTESIAN_POINT('Ctrl Pts',(-10.7467220520001,12.2,-2.78488741600002));
#268816=CARTESIAN_POINT('Ctrl Pts',(-10.7435039560001,12.2,-2.78527368900002));
#268817=CARTESIAN_POINT('Ctrl Pts',(-10.7402905920001,12.2,-2.78565678100001));
#268818=CARTESIAN_POINT('Ctrl Pts',(-10.7370819700001,12.2,-2.78603669900002));
#268819=CARTESIAN_POINT('Ctrl Pts',(-10.7338780990001,12.2,-2.78641345000001));
#268820=CARTESIAN_POINT('Ctrl Pts',(-10.7306789900001,12.2,-2.78678703700002));
#268821=CARTESIAN_POINT('Ctrl Pts',(-10.7274846510001,12.2,-2.78715746900001));
#268822=CARTESIAN_POINT('Ctrl Pts',(-10.7242950910001,12.2,-2.78752475000001));
#268823=CARTESIAN_POINT('Ctrl Pts',(-10.7211103210001,12.2,-2.78788888700001));
#268824=CARTESIAN_POINT('Ctrl Pts',(-10.7179303500001,12.2,-2.78824988400002));
#268825=CARTESIAN_POINT('Ctrl Pts',(-10.7147551880001,12.2,-2.78860774800001));
#268826=CARTESIAN_POINT('Ctrl Pts',(-10.7115848430001,12.2,-2.78896248700002));
#268827=CARTESIAN_POINT('Ctrl Pts',(-10.7084193250001,12.2,-2.78931410400002));
#268828=CARTESIAN_POINT('Ctrl Pts',(-10.7052586450001,12.2,-2.78966260600002));
#268829=CARTESIAN_POINT('Ctrl Pts',(-10.7021028110001,12.2,-2.79000800100001));
#268830=CARTESIAN_POINT('Ctrl Pts',(-10.6989518340001,12.2,-2.79035029100001));
#268831=CARTESIAN_POINT('Ctrl Pts',(-10.6958057220001,12.2,-2.79068948600001));
#268832=CARTESIAN_POINT('Ctrl Pts',(-10.6926644870001,12.2,-2.79102559000002));
#268833=CARTESIAN_POINT('Ctrl Pts',(-10.6895281350001,12.2,-2.79135861000002));
#268834=CARTESIAN_POINT('Ctrl Pts',(-10.6863966800001,12.2,-2.79168855100002));
#268835=CARTESIAN_POINT('Ctrl Pts',(-10.6832701290001,12.2,-2.79201542000001));
#268836=CARTESIAN_POINT('Ctrl Pts',(-10.6801484920001,12.2,-2.79233922300001));
#268837=CARTESIAN_POINT('Ctrl Pts',(-10.6770317790001,12.2,-2.79265996700001));
#268838=CARTESIAN_POINT('Ctrl Pts',(-10.6739200000001,12.2,-2.79297765700001));
#268839=CARTESIAN_POINT('Ctrl Pts',(-10.6708131640001,12.2,-2.79329230000001));
#268840=CARTESIAN_POINT('Ctrl Pts',(-10.6677112820001,12.2,-2.79360390200001));
#268841=CARTESIAN_POINT('Ctrl Pts',(-10.6646143620001,12.2,-2.79391246900001));
#268842=CARTESIAN_POINT('Ctrl Pts',(-10.6615224160001,12.2,-2.79421800700002));
#268843=CARTESIAN_POINT('Ctrl Pts',(-10.6584354520001,12.2,-2.79452052500002));
#268844=CARTESIAN_POINT('Ctrl Pts',(-10.6553534800001,12.2,-2.79482002500002));
#268845=CARTESIAN_POINT('Ctrl Pts',(-10.6522765120001,12.2,-2.79511651600002));
#268846=CARTESIAN_POINT('Ctrl Pts',(-10.6492045550001,12.2,-2.79541000500001));
#268847=CARTESIAN_POINT('Ctrl Pts',(-10.6461376210001,12.2,-2.79570049800002));
#268848=CARTESIAN_POINT('Ctrl Pts',(-10.6430757180001,12.2,-2.79598800000001));
#268849=CARTESIAN_POINT('Ctrl Pts',(-10.6400188580001,12.2,-2.79627251700001));
#268850=CARTESIAN_POINT('Ctrl Pts',(-10.6369670490001,12.2,-2.79655405800002));
#268851=CARTESIAN_POINT('Ctrl Pts',(-10.6339203020001,12.2,-2.79683262800001));
#268852=CARTESIAN_POINT('Ctrl Pts',(-10.6308786260001,12.2,-2.79710823500002));
#268853=CARTESIAN_POINT('Ctrl Pts',(-10.6278420330001,12.2,-2.79738088400002));
#268854=CARTESIAN_POINT('Ctrl Pts',(-10.6248105320001,12.2,-2.79765058100002));
#268855=CARTESIAN_POINT('Ctrl Pts',(-10.6217841320001,12.2,-2.79791733300002));
#268856=CARTESIAN_POINT('Ctrl Pts',(-10.6187628440001,12.2,-2.79818114900001));
#268857=CARTESIAN_POINT('Ctrl Pts',(-10.6157466780001,12.2,-2.79844203300001));
#268858=CARTESIAN_POINT('Ctrl Pts',(-10.6127356450001,12.2,-2.79869999200002));
#268859=CARTESIAN_POINT('Ctrl Pts',(-10.6097297520001,12.2,-2.79895503300001));
#268860=CARTESIAN_POINT('Ctrl Pts',(-10.6067290130001,12.2,-2.79920716400001));
#268861=CARTESIAN_POINT('Ctrl Pts',(-10.6037334350001,12.2,-2.79945638900001));
#268862=CARTESIAN_POINT('Ctrl Pts',(-10.6007430310001,12.2,-2.79970271700002));
#268863=CARTESIAN_POINT('Ctrl Pts',(-10.5977578070001,12.2,-2.79994615300001));
#268864=CARTESIAN_POINT('Ctrl Pts',(-10.5947777780001,12.2,-2.80018670600001));
#268865=CARTESIAN_POINT('Ctrl Pts',(-10.5918029510001,12.2,-2.80042438200002));
#268866=CARTESIAN_POINT('Ctrl Pts',(-10.5888333380001,12.2,-2.80065918700001));
#268867=CARTESIAN_POINT('Ctrl Pts',(-10.5858689480001,12.2,-2.80089112800002));
#268868=CARTESIAN_POINT('Ctrl Pts',(-10.5829097920001,12.2,-2.80112021200001));
#268869=CARTESIAN_POINT('Ctrl Pts',(-10.5799558780001,12.2,-2.80134644700002));
#268870=CARTESIAN_POINT('Ctrl Pts',(-10.5770072200001,12.2,-2.80156983800001));
#268871=CARTESIAN_POINT('Ctrl Pts',(-10.5740638260001,12.2,-2.80179039400001));
#268872=CARTESIAN_POINT('Ctrl Pts',(-10.5711257080001,12.2,-2.80200812100002));
#268873=CARTESIAN_POINT('Ctrl Pts',(-10.5681928730001,12.2,-2.80222302500002));
#268874=CARTESIAN_POINT('Ctrl Pts',(-10.5652653350001,12.2,-2.80243511500001));
#268875=CARTESIAN_POINT('Ctrl Pts',(-10.5623431030001,12.2,-2.80264439700002));
#268876=CARTESIAN_POINT('Ctrl Pts',(-10.5594261870001,12.2,-2.80285087700001));
#268877=CARTESIAN_POINT('Ctrl Pts',(-10.5565145980001,12.2,-2.80305456500002));
#268878=CARTESIAN_POINT('Ctrl Pts',(-10.5536083460001,12.2,-2.80325546500002));
#268879=CARTESIAN_POINT('Ctrl Pts',(-10.5507074410001,12.2,-2.80345358600002));
#268880=CARTESIAN_POINT('Ctrl Pts',(-10.5478118940001,12.2,-2.80364893500002));
#268881=CARTESIAN_POINT('Ctrl Pts',(-10.5449217170001,12.2,-2.80384151900002));
#268882=CARTESIAN_POINT('Ctrl Pts',(-10.5420369180001,12.2,-2.80403134500002));
#268883=CARTESIAN_POINT('Ctrl Pts',(-10.5391575100001,12.2,-2.80421842000001));
#268884=CARTESIAN_POINT('Ctrl Pts',(-10.5362835010001,12.2,-2.80440275200001));
#268885=CARTESIAN_POINT('Ctrl Pts',(-10.5328411820124,12.2,-2.80462066721189));
#268886=CARTESIAN_POINT('Ctrl Pts',(-10.5294069978379,12.2,-2.80483448890378));
#268887=CARTESIAN_POINT('Ctrl Pts',(-10.5259809641622,12.2,-2.80504423309624));
#268888=CARTESIAN_POINT('Ctrl Pts',(-10.5225631056757,12.2,-2.80524991280756));
#268889=CARTESIAN_POINT('Ctrl Pts',(-10.5191534450001,12.2,-2.80545154400002));
#268890=CARTESIAN_POINT('Ctrl Pts',(-10.5163175340001,12.2,-2.80561687900001));
#268891=CARTESIAN_POINT('Ctrl Pts',(-10.5134871080001,12.2,-2.80577952900002));
#268892=CARTESIAN_POINT('Ctrl Pts',(-10.5106621790001,12.2,-2.80593950300001));
#268893=CARTESIAN_POINT('Ctrl Pts',(-10.5078427570001,12.2,-2.80609680700001));
#268894=CARTESIAN_POINT('Ctrl Pts',(-10.5050288510001,12.2,-2.80625145000001));
#268895=CARTESIAN_POINT('Ctrl Pts',(-10.5022204750001,12.2,-2.80640343900001));
#268896=CARTESIAN_POINT('Ctrl Pts',(-10.4994176380001,12.2,-2.80655278100001));
#268897=CARTESIAN_POINT('Ctrl Pts',(-10.4966203510001,12.2,-2.80669948500002));
#268898=CARTESIAN_POINT('Ctrl Pts',(-10.4938286240001,12.2,-2.80684355700001));
#268899=CARTESIAN_POINT('Ctrl Pts',(-10.4910424700001,12.2,-2.80698500600002));
#268900=CARTESIAN_POINT('Ctrl Pts',(-10.4882618970001,12.2,-2.80712384000001));
#268901=CARTESIAN_POINT('Ctrl Pts',(-10.4854869180001,12.2,-2.80726006400001));
#268902=CARTESIAN_POINT('Ctrl Pts',(-10.4827175440001,12.2,-2.80739369000001));
#268903=CARTESIAN_POINT('Ctrl Pts',(-10.4799537850001,12.2,-2.80752472200001));
#268904=CARTESIAN_POINT('Ctrl Pts',(-10.4771956530001,12.2,-2.80765317100002));
#268905=CARTESIAN_POINT('Ctrl Pts',(-10.4744431570001,12.2,-2.80777904200002));
#268906=CARTESIAN_POINT('Ctrl Pts',(-10.4716963110001,12.2,-2.80790234500001));
#268907=CARTESIAN_POINT('Ctrl Pts',(-10.4689551240001,12.2,-2.80802308700002));
#268908=CARTESIAN_POINT('Ctrl Pts',(-10.4662196070001,12.2,-2.80814127600001));
#268909=CARTESIAN_POINT('Ctrl Pts',(-10.4634897720001,12.2,-2.80825691900001));
#268910=CARTESIAN_POINT('Ctrl Pts',(-10.4607656300001,12.2,-2.80837002600002));
#268911=CARTESIAN_POINT('Ctrl Pts',(-10.4580471910001,12.2,-2.80848060400002));
#268912=CARTESIAN_POINT('Ctrl Pts',(-10.4553344680001,12.2,-2.80858866000001));
#268913=CARTESIAN_POINT('Ctrl Pts',(-10.4526274700001,12.2,-2.80869420500002));
#268914=CARTESIAN_POINT('Ctrl Pts',(-10.4499262110001,12.2,-2.80879724300001));
#268915=CARTESIAN_POINT('Ctrl Pts',(-10.4472306990001,12.2,-2.80889778700002));
#268916=CARTESIAN_POINT('Ctrl Pts',(-10.4445409480001,12.2,-2.80899584100001));
#268917=CARTESIAN_POINT('Ctrl Pts',(-10.4418569680001,12.2,-2.80909141400001));
#268918=CARTESIAN_POINT('Ctrl Pts',(-10.4391787700001,12.2,-2.80918451700002));
#268919=CARTESIAN_POINT('Ctrl Pts',(-10.4365063660001,12.2,-2.80927515500002));
#268920=CARTESIAN_POINT('Ctrl Pts',(-10.4338397670001,12.2,-2.80936333700001));
#268921=CARTESIAN_POINT('Ctrl Pts',(-10.4311789840001,12.2,-2.80944907300002));
#268922=CARTESIAN_POINT('Ctrl Pts',(-10.4285240300001,12.2,-2.80953237000002));
#268923=CARTESIAN_POINT('Ctrl Pts',(-10.4258749130001,12.2,-2.80961323700001));
#268924=CARTESIAN_POINT('Ctrl Pts',(-10.4232316480001,12.2,-2.80969168100001));
#268925=CARTESIAN_POINT('Ctrl Pts',(-10.4205942460001,12.2,-2.80976771100002));
#268926=CARTESIAN_POINT('Ctrl Pts',(-10.4179627160001,12.2,-2.80984133700001));
#268927=CARTESIAN_POINT('Ctrl Pts',(-10.4153370720001,12.2,-2.80991256500001));
#268928=CARTESIAN_POINT('Ctrl Pts',(-10.4127173250001,12.2,-2.80998140700001));
#268929=CARTESIAN_POINT('Ctrl Pts',(-10.4101034850001,12.2,-2.81004786800001));
#268930=CARTESIAN_POINT('Ctrl Pts',(-10.4074955650001,12.2,-2.81011195800001));
#268931=CARTESIAN_POINT('Ctrl Pts',(-10.4048935770001,12.2,-2.81017368600001));
#268932=CARTESIAN_POINT('Ctrl Pts',(-10.4022975320001,12.2,-2.81023306000002));
#268933=CARTESIAN_POINT('Ctrl Pts',(-10.3997074400001,12.2,-2.81029008900001));
#268934=CARTESIAN_POINT('Ctrl Pts',(-10.3971233170001,12.2,-2.81034478200001));
#268935=CARTESIAN_POINT('Ctrl Pts',(-10.3945451690001,12.2,-2.81039714800002));
#268936=CARTESIAN_POINT('Ctrl Pts',(-10.3919730120001,12.2,-2.81044719300001));
#268937=CARTESIAN_POINT('Ctrl Pts',(-10.3894068560001,12.2,-2.81049493000001));
#268938=CARTESIAN_POINT('Ctrl Pts',(-10.3868467140001,12.2,-2.81054036500001));
#268939=CARTESIAN_POINT('Ctrl Pts',(-10.3842925970001,12.2,-2.81058350800001));
#268940=CARTESIAN_POINT('Ctrl Pts',(-10.3817445160001,12.2,-2.81062436900001));
#268941=CARTESIAN_POINT('Ctrl Pts',(-10.3792024840001,12.2,-2.81066295300001));
#268942=CARTESIAN_POINT('Ctrl Pts',(-10.3766665130001,12.2,-2.81069927400001));
#268943=CARTESIAN_POINT('Ctrl Pts',(-10.3741366140001,12.2,-2.81073333600002));
#268944=CARTESIAN_POINT('Ctrl Pts',(-10.3716127990001,12.2,-2.81076515200001));
#268945=CARTESIAN_POINT('Ctrl Pts',(-10.3690950810001,12.2,-2.81079473000001));
#268946=CARTESIAN_POINT('Ctrl Pts',(-10.3665834700001,12.2,-2.81082207900001));
#268947=CARTESIAN_POINT('Ctrl Pts',(-10.3640779820001,12.2,-2.81084720700001));
#268948=CARTESIAN_POINT('Ctrl Pts',(-10.3615786240001,12.2,-2.81087012400001));
#268949=CARTESIAN_POINT('Ctrl Pts',(-10.3590854110001,12.2,-2.81089083900001));
#268950=CARTESIAN_POINT('Ctrl Pts',(-10.3565983540001,12.2,-2.81090936300001));
#268951=CARTESIAN_POINT('Ctrl Pts',(-10.3541174660001,12.2,-2.81092570300002));
#268952=CARTESIAN_POINT('Ctrl Pts',(-10.3516427590001,12.2,-2.81093986800002));
#268953=CARTESIAN_POINT('Ctrl Pts',(-10.3491742450001,12.2,-2.81095186900002));
#268954=CARTESIAN_POINT('Ctrl Pts',(-10.3467119360001,12.2,-2.81096171500002));
#268955=CARTESIAN_POINT('Ctrl Pts',(-10.3442558440001,12.2,-2.81096941500001));
#268956=CARTESIAN_POINT('Ctrl Pts',(-10.3418059810001,12.2,-2.81097497900001));
#268957=CARTESIAN_POINT('Ctrl Pts',(-10.3393623600001,12.2,-2.81097841600001));
#268958=CARTESIAN_POINT('Ctrl Pts',(-10.3369249940001,12.2,-2.81097973500001));
#268959=CARTESIAN_POINT('Ctrl Pts',(-10.3344938940001,12.2,-2.81097894800002));
#268960=CARTESIAN_POINT('Ctrl Pts',(-10.3320690720001,12.2,-2.81097606100001));
#268961=CARTESIAN_POINT('Ctrl Pts',(-10.3296505420001,12.2,-2.81097108600001));
#268962=CARTESIAN_POINT('Ctrl Pts',(-10.3272383160001,12.2,-2.81096403100001));
#268963=CARTESIAN_POINT('Ctrl Pts',(-10.3248324060001,12.2,-2.81095490800002));
#268964=CARTESIAN_POINT('Ctrl Pts',(-10.3224328240001,12.2,-2.81094372600001));
#268965=CARTESIAN_POINT('Ctrl Pts',(-10.3200395830001,12.2,-2.81093049300001));
#268966=CARTESIAN_POINT('Ctrl Pts',(-10.3176526950001,12.2,-2.81091522000001));
#268967=CARTESIAN_POINT('Ctrl Pts',(-10.3152721750001,12.2,-2.81089791800001));
#268968=CARTESIAN_POINT('Ctrl Pts',(-10.3128980330001,12.2,-2.81087859400001));
#268969=CARTESIAN_POINT('Ctrl Pts',(-10.3105302810001,12.2,-2.81085726100001));
#268970=CARTESIAN_POINT('Ctrl Pts',(-10.3081689340001,12.2,-2.81083392700001));
#268971=CARTESIAN_POINT('Ctrl Pts',(-10.3058140040001,12.2,-2.81080860400001));
#268972=CARTESIAN_POINT('Ctrl Pts',(-10.3034655040001,12.2,-2.81078129900001));
#268973=CARTESIAN_POINT('Ctrl Pts',(-10.3011234450001,12.2,-2.81075202400002));
#268974=CARTESIAN_POINT('Ctrl Pts',(-10.2987878420001,12.2,-2.81072079000001));
#268975=CARTESIAN_POINT('Ctrl Pts',(-10.2964587060001,12.2,-2.81068760400002));
#268976=CARTESIAN_POINT('Ctrl Pts',(-10.2941360500001,12.2,-2.81065248000001));
#268977=CARTESIAN_POINT('Ctrl Pts',(-10.2918198870001,12.2,-2.81061542500002));
#268978=CARTESIAN_POINT('Ctrl Pts',(-10.2895102320001,12.2,-2.81057645100002));
#268979=CARTESIAN_POINT('Ctrl Pts',(-10.2872070960001,12.2,-2.81053556800002));
#268980=CARTESIAN_POINT('Ctrl Pts',(-10.2849104920001,12.2,-2.81049278600001));
#268981=CARTESIAN_POINT('Ctrl Pts',(-10.2826204320001,12.2,-2.81044811600001));
#268982=CARTESIAN_POINT('Ctrl Pts',(-10.2803369320001,12.2,-2.81040156800001));
#268983=CARTESIAN_POINT('Ctrl Pts',(-10.2780600020001,12.2,-2.81035315300001));
#268984=CARTESIAN_POINT('Ctrl Pts',(-10.2757896570001,12.2,-2.81030288000002));
#268985=CARTESIAN_POINT('Ctrl Pts',(-10.2735259090001,12.2,-2.81025076200002));
#268986=CARTESIAN_POINT('Ctrl Pts',(-10.2712687710001,12.2,-2.81019680600001));
#268987=CARTESIAN_POINT('Ctrl Pts',(-10.2690182590001,12.2,-2.81014102700002));
#268988=CARTESIAN_POINT('Ctrl Pts',(-10.2667743820001,12.2,-2.81008343100002));
#268989=CARTESIAN_POINT('Ctrl Pts',(-10.2645371560001,12.2,-2.81002403300001));
#268990=CARTESIAN_POINT('Ctrl Pts',(-10.2623065940001,12.2,-2.80996284100001));
#268991=CARTESIAN_POINT('Ctrl Pts',(-10.2600827090001,12.2,-2.80989986700002));
#268992=CARTESIAN_POINT('Ctrl Pts',(-10.2578655120001,12.2,-2.80983512200002));
#268993=CARTESIAN_POINT('Ctrl Pts',(-10.2556550210001,12.2,-2.80976861500001));
#268994=CARTESIAN_POINT('Ctrl Pts',(-10.2534512460001,12.2,-2.80970035900001));
#268995=CARTESIAN_POINT('Ctrl Pts',(-10.2512542030001,12.2,-2.80963036400002));
#268996=CARTESIAN_POINT('Ctrl Pts',(-10.2490639020001,12.2,-2.80955864200001));
#268997=CARTESIAN_POINT('Ctrl Pts',(-10.2468803590001,12.2,-2.80948520200001));
#268998=CARTESIAN_POINT('Ctrl Pts',(-10.2447035880001,12.2,-2.80941005800001));
#268999=CARTESIAN_POINT('Ctrl Pts',(-10.2425336010001,12.2,-2.80933321800001));
#269000=CARTESIAN_POINT('Ctrl Pts',(-10.2403704120001,12.2,-2.80925469500001));
#269001=CARTESIAN_POINT('Ctrl Pts',(-10.2382140350001,12.2,-2.80917450000001));
#269002=CARTESIAN_POINT('Ctrl Pts',(-10.2360644840001,12.2,-2.80909264400002));
#269003=CARTESIAN_POINT('Ctrl Pts',(-10.2339217720001,12.2,-2.80900913800001));
#269004=CARTESIAN_POINT('Ctrl Pts',(-10.2317859140001,12.2,-2.80892399500001));
#269005=CARTESIAN_POINT('Ctrl Pts',(-10.2296569220001,12.2,-2.80883722400001));
#269006=CARTESIAN_POINT('Ctrl Pts',(-10.2275348110001,12.2,-2.80874883800001));
#269007=CARTESIAN_POINT('Ctrl Pts',(-10.2254195960001,12.2,-2.80865884700002));
#269008=CARTESIAN_POINT('Ctrl Pts',(-10.2233112870001,12.2,-2.80856726500001));
#269009=CARTESIAN_POINT('Ctrl Pts',(-10.2212099030001,12.2,-2.80847410200002));
#269010=CARTESIAN_POINT('Ctrl Pts',(-10.2191154540001,12.2,-2.80837937100001));
#269011=CARTESIAN_POINT('Ctrl Pts',(-10.2170279560001,12.2,-2.80828308000002));
#269012=CARTESIAN_POINT('Ctrl Pts',(-10.2149474230001,12.2,-2.80818524500001));
#269013=CARTESIAN_POINT('Ctrl Pts',(-10.2128738680001,12.2,-2.80808587500001));
#269014=CARTESIAN_POINT('Ctrl Pts',(-10.2108073070001,12.2,-2.80798498300001));
#269015=CARTESIAN_POINT('Ctrl Pts',(-10.2087477520001,12.2,-2.80788258200001));
#269016=CARTESIAN_POINT('Ctrl Pts',(-10.2066952180001,12.2,-2.80777868100001));
#269017=CARTESIAN_POINT('Ctrl Pts',(-10.2046497210001,12.2,-2.80767329400001));
#269018=CARTESIAN_POINT('Ctrl Pts',(-10.2026112720001,12.2,-2.80756643300001));
#269019=CARTESIAN_POINT('Ctrl Pts',(-10.2005798890001,12.2,-2.80745810900001));
#269020=CARTESIAN_POINT('Ctrl Pts',(-10.1985555830001,12.2,-2.80734833400002));
#269021=CARTESIAN_POINT('Ctrl Pts',(-10.1965383710001,12.2,-2.80723712200002));
#269022=CARTESIAN_POINT('Ctrl Pts',(-10.1945282670001,12.2,-2.80712448400001));
#269023=CARTESIAN_POINT('Ctrl Pts',(-10.1925252840001,12.2,-2.80701043200001));
#269024=CARTESIAN_POINT('Ctrl Pts',(-10.1905294380001,12.2,-2.80689497800001));
#269025=CARTESIAN_POINT('Ctrl Pts',(-10.1885407420001,12.2,-2.80677813600001));
#269026=CARTESIAN_POINT('Ctrl Pts',(-10.1865592120001,12.2,-2.80665991700001));
#269027=CARTESIAN_POINT('Ctrl Pts',(-10.1845848630001,12.2,-2.80654033300001));
#269028=CARTESIAN_POINT('Ctrl Pts',(-10.1826177100001,12.2,-2.80641939900002));
#269029=CARTESIAN_POINT('Ctrl Pts',(-10.1806577650001,12.2,-2.80629712500001));
#269030=CARTESIAN_POINT('Ctrl Pts',(-10.1787050450001,12.2,-2.80617352500002));
#269031=CARTESIAN_POINT('Ctrl Pts',(-10.1767595650001,12.2,-2.80604861000001));
#269032=CARTESIAN_POINT('Ctrl Pts',(-10.1748213380001,12.2,-2.80592239500002));
#269033=CARTESIAN_POINT('Ctrl Pts',(-10.1728903810001,12.2,-2.80579489000001));
#269034=CARTESIAN_POINT('Ctrl Pts',(-10.1709667090001,12.2,-2.80566611100001));
#269035=CARTESIAN_POINT('Ctrl Pts',(-10.1690503350001,12.2,-2.80553606900002));
#269036=CARTESIAN_POINT('Ctrl Pts',(-10.1671412760001,12.2,-2.80540477800002));
#269037=CARTESIAN_POINT('Ctrl Pts',(-10.1652395470001,12.2,-2.80527224900001));
#269038=CARTESIAN_POINT('Ctrl Pts',(-10.1633451610001,12.2,-2.80513849600001));
#269039=CARTESIAN_POINT('Ctrl Pts',(-10.1614581350001,12.2,-2.80500353400001));
#269040=CARTESIAN_POINT('Ctrl Pts',(-10.1595784840001,12.2,-2.80486737300001));
#269041=CARTESIAN_POINT('Ctrl Pts',(-10.1577062240001,12.2,-2.80473002900001));
#269042=CARTESIAN_POINT('Ctrl Pts',(-10.1558413680001,12.2,-2.80459151300001));
#269043=CARTESIAN_POINT('Ctrl Pts',(-10.1539839340001,12.2,-2.80445183900001));
#269044=CARTESIAN_POINT('Ctrl Pts',(-10.1521339360001,12.2,-2.80431102100001));
#269045=CARTESIAN_POINT('Ctrl Pts',(-10.1502913890001,12.2,-2.80416907300001));
#269046=CARTESIAN_POINT('Ctrl Pts',(-10.1484563090001,12.2,-2.80402600700001));
#269047=CARTESIAN_POINT('Ctrl Pts',(-10.1466287130001,12.2,-2.80388183700001));
#269048=CARTESIAN_POINT('Ctrl Pts',(-10.1448086140001,12.2,-2.80373657700002));
#269049=CARTESIAN_POINT('Ctrl Pts',(-10.1429960300001,12.2,-2.80359024000001));
#269050=CARTESIAN_POINT('Ctrl Pts',(-10.1411909760001,12.2,-2.80344284000002));
#269051=CARTESIAN_POINT('Ctrl Pts',(-10.1393934660001,12.2,-2.80329439100001));
#269052=CARTESIAN_POINT('Ctrl Pts',(-10.1376035180001,12.2,-2.80314490700002));
#269053=CARTESIAN_POINT('Ctrl Pts',(-10.1358211480001,12.2,-2.80299440200002));
#269054=CARTESIAN_POINT('Ctrl Pts',(-10.1340463700001,12.2,-2.80284288800001));
#269055=CARTESIAN_POINT('Ctrl Pts',(-10.1322792010001,12.2,-2.80269038200001));
#269056=CARTESIAN_POINT('Ctrl Pts',(-10.1305196570001,12.2,-2.80253689600002));
#269057=CARTESIAN_POINT('Ctrl Pts',(-10.1287677530001,12.2,-2.80238244500001));
#269058=CARTESIAN_POINT('Ctrl Pts',(-10.1270235070001,12.2,-2.80222704300002));
#269059=CARTESIAN_POINT('Ctrl Pts',(-10.1252869340001,12.2,-2.80207070400001));
#269060=CARTESIAN_POINT('Ctrl Pts',(-10.1235580500001,12.2,-2.80191344300002));
#269061=CARTESIAN_POINT('Ctrl Pts',(-10.1218368710001,12.2,-2.80175527400001));
#269062=CARTESIAN_POINT('Ctrl Pts',(-10.1201234150001,12.2,-2.80159621100001));
#269063=CARTESIAN_POINT('Ctrl Pts',(-10.1184176970001,12.2,-2.80143626900001));
#269064=CARTESIAN_POINT('Ctrl Pts',(-10.1167197340001,12.2,-2.80127546300001));
#269065=CARTESIAN_POINT('Ctrl Pts',(-10.1150295420001,12.2,-2.80111380600002));
#269066=CARTESIAN_POINT('Ctrl Pts',(-10.1133471370001,12.2,-2.80095131400001));
#269067=CARTESIAN_POINT('Ctrl Pts',(-10.1116725360001,12.2,-2.80078800200001));
#269068=CARTESIAN_POINT('Ctrl Pts',(-10.1100057560001,12.2,-2.80062388500002));
#269069=CARTESIAN_POINT('Ctrl Pts',(-10.1083468140001,12.2,-2.80045897600001));
#269070=CARTESIAN_POINT('Ctrl Pts',(-10.1066957250001,12.2,-2.80029329300001));
#269071=CARTESIAN_POINT('Ctrl Pts',(-10.1050525090001,12.2,-2.80012684900001));
#269072=CARTESIAN_POINT('Ctrl Pts',(-10.1034171790001,12.2,-2.79995965800001));
#269073=CARTESIAN_POINT('Ctrl Pts',(-10.1017897540001,12.2,-2.79979173800001));
#269074=CARTESIAN_POINT('Ctrl Pts',(-10.1001702510001,12.2,-2.79962310200002));
#269075=CARTESIAN_POINT('Ctrl Pts',(-10.0985586870001,12.2,-2.79945376700002));
#269076=CARTESIAN_POINT('Ctrl Pts',(-10.0969550780001,12.2,-2.79928374700001));
#269077=CARTESIAN_POINT('Ctrl Pts',(-10.0953594420001,12.2,-2.79911305800002));
#269078=CARTESIAN_POINT('Ctrl Pts',(-10.0937717960001,12.2,-2.79894171500001));
#269079=CARTESIAN_POINT('Ctrl Pts',(-10.0921921570001,12.2,-2.79876973500001));
#269080=CARTESIAN_POINT('Ctrl Pts',(-10.0906205420001,12.2,-2.79859713200001));
#269081=CARTESIAN_POINT('Ctrl Pts',(-10.0890569700001,12.2,-2.79842392300001));
#269082=CARTESIAN_POINT('Ctrl Pts',(-10.0875014570001,12.2,-2.79825012400002));
#269083=CARTESIAN_POINT('Ctrl Pts',(-10.0859540200001,12.2,-2.79807574900001));
#269084=CARTESIAN_POINT('Ctrl Pts',(-10.0844146780001,12.2,-2.79790081600002));
#269085=CARTESIAN_POINT('Ctrl Pts',(-10.0828834480001,12.2,-2.79772534000001));
#269086=CARTESIAN_POINT('Ctrl Pts',(-10.0813603480001,12.2,-2.79754933600001));
#269087=CARTESIAN_POINT('Ctrl Pts',(-10.0798453950001,12.2,-2.79737282200001));
#269088=CARTESIAN_POINT('Ctrl Pts',(-10.0783386060001,12.2,-2.79719581400002));
#269089=CARTESIAN_POINT('Ctrl Pts',(-10.0768400010001,12.2,-2.79701832800002));
#269090=CARTESIAN_POINT('Ctrl Pts',(-10.0753495960001,12.2,-2.79684038000001));
#269091=CARTESIAN_POINT('Ctrl Pts',(-10.0738674120001,12.2,-2.79666198700002));
#269092=CARTESIAN_POINT('Ctrl Pts',(-10.0723934620001,12.2,-2.79648316500001));
#269093=CARTESIAN_POINT('Ctrl Pts',(-10.0709277690001,12.2,-2.79630393100001));
#269094=CARTESIAN_POINT('Ctrl Pts',(-10.0694703480001,12.2,-2.79612430200002));
#269095=CARTESIAN_POINT('Ctrl Pts',(-10.0680212180001,12.2,-2.79594429400001));
#269096=CARTESIAN_POINT('Ctrl Pts',(-10.0665803990001,12.2,-2.79576392500001));
#269097=CARTESIAN_POINT('Ctrl Pts',(-10.0651479080001,12.2,-2.79558321000001));
#269098=CARTESIAN_POINT('Ctrl Pts',(-10.0637237620001,12.2,-2.79540216900001));
#269099=CARTESIAN_POINT('Ctrl Pts',(-10.0623079820001,12.2,-2.79522081700001));
#269100=CARTESIAN_POINT('Ctrl Pts',(-10.0609005850001,12.2,-2.79503917100001));
#269101=CARTESIAN_POINT('Ctrl Pts',(-10.0595015910001,12.2,-2.79485724800002));
#269102=CARTESIAN_POINT('Ctrl Pts',(-10.0581110160001,12.2,-2.79467506700001));
#269103=CARTESIAN_POINT('Ctrl Pts',(-10.0567288820001,12.2,-2.79449264500002));
#269104=CARTESIAN_POINT('Ctrl Pts',(-10.0553552060001,12.2,-2.79430999900002));
#269105=CARTESIAN_POINT('Ctrl Pts',(-10.0539900080001,12.2,-2.79412714600001));
#269106=CARTESIAN_POINT('Ctrl Pts',(-10.0526333070001,12.2,-2.79394410600001));
#269107=CARTESIAN_POINT('Ctrl Pts',(-10.0512851200001,12.2,-2.79376089400001));
#269108=CARTESIAN_POINT('Ctrl Pts',(-10.0499454690001,12.2,-2.79357752900002));
#269109=CARTESIAN_POINT('Ctrl Pts',(-10.0486143700001,12.2,-2.79339402900002));
#269110=CARTESIAN_POINT('Ctrl Pts',(-10.0472918460001,12.2,-2.79321041100001));
#269111=CARTESIAN_POINT('Ctrl Pts',(-10.0459779130001,12.2,-2.79302669500002));
#269112=CARTESIAN_POINT('Ctrl Pts',(-10.0446725930001,12.2,-2.79284289900001));
#269113=CARTESIAN_POINT('Ctrl Pts',(-10.0433759040001,12.2,-2.79265904000002));
#269114=CARTESIAN_POINT('Ctrl Pts',(-10.0420878650001,12.2,-2.79247513800001));
#269115=CARTESIAN_POINT('Ctrl Pts',(-10.0408084970001,12.2,-2.79229120900002));
#269116=CARTESIAN_POINT('Ctrl Pts',(-10.0395378210001,12.2,-2.79210727300002));
#269117=CARTESIAN_POINT('Ctrl Pts',(-10.0382758530001,12.2,-2.79192335000001));
#269118=CARTESIAN_POINT('Ctrl Pts',(-10.0370226160001,12.2,-2.79173945600002));
#269119=CARTESIAN_POINT('Ctrl Pts',(-10.0357781300001,12.2,-2.79155561300001));
#269120=CARTESIAN_POINT('Ctrl Pts',(-10.0345424120001,12.2,-2.79137183600001));
#269121=CARTESIAN_POINT('Ctrl Pts',(-10.0333154850001,12.2,-2.79118814800002));
#269122=CARTESIAN_POINT('Ctrl Pts',(-10.0320973690001,12.2,-2.79100456500001));
#269123=CARTESIAN_POINT('Ctrl Pts',(-10.0308880840001,12.2,-2.79082110900001));
#269124=CARTESIAN_POINT('Ctrl Pts',(-10.0296876490001,12.2,-2.79063779700001));
#269125=CARTESIAN_POINT('Ctrl Pts',(-10.0284960860001,12.2,-2.79045465000001));
#269126=CARTESIAN_POINT('Ctrl Pts',(-10.0273134150001,12.2,-2.79027168600001));
#269127=CARTESIAN_POINT('Ctrl Pts',(-10.0261396570001,12.2,-2.79008892600002));
#269128=CARTESIAN_POINT('Ctrl Pts',(-10.0249748320001,12.2,-2.78990638900002));
#269129=CARTESIAN_POINT('Ctrl Pts',(-10.0238189610001,12.2,-2.78972409500001));
#269130=CARTESIAN_POINT('Ctrl Pts',(-10.0226720660001,12.2,-2.78954206400002));
#269131=CARTESIAN_POINT('Ctrl Pts',(-10.0215341660001,12.2,-2.78936031700002));
#269132=CARTESIAN_POINT('Ctrl Pts',(-10.0204052840001,12.2,-2.78917887200001));
#269133=CARTESIAN_POINT('Ctrl Pts',(-10.0192854400001,12.2,-2.78899774900002));
#269134=CARTESIAN_POINT('Ctrl Pts',(-10.0181746550001,12.2,-2.78881697100001));
#269135=CARTESIAN_POINT('Ctrl Pts',(-10.0170729510001,12.2,-2.78863655800001));
#269136=CARTESIAN_POINT('Ctrl Pts',(-10.0159803500001,12.2,-2.78845652900001));
#269137=CARTESIAN_POINT('Ctrl Pts',(-10.0148968710001,12.2,-2.78827690400002));
#269138=CARTESIAN_POINT('Ctrl Pts',(-10.0138225390001,12.2,-2.78809770600001));
#269139=CARTESIAN_POINT('Ctrl Pts',(-10.0127573730001,12.2,-2.78791895500001));
#269140=CARTESIAN_POINT('Ctrl Pts',(-10.0117013970001,12.2,-2.78774067200001));
#269141=CARTESIAN_POINT('Ctrl Pts',(-10.0106546300001,12.2,-2.78756287700002));
#269142=CARTESIAN_POINT('Ctrl Pts',(-10.0096170970001,12.2,-2.78738559300002));
#269143=CARTESIAN_POINT('Ctrl Pts',(-10.0085888180001,12.2,-2.78720884000002));
#269144=CARTESIAN_POINT('Ctrl Pts',(-10.0075698160001,12.2,-2.78703264000002));
#269145=CARTESIAN_POINT('Ctrl Pts',(-10.0065601130001,12.2,-2.78685701400001));
#269146=CARTESIAN_POINT('Ctrl Pts',(-10.0055597320001,12.2,-2.78668198500001));
#269147=CARTESIAN_POINT('Ctrl Pts',(-10.0045686950001,12.2,-2.78650757300001));
#269148=CARTESIAN_POINT('Ctrl Pts',(-10.0035870240001,12.2,-2.78633380100001));
#269149=CARTESIAN_POINT('Ctrl Pts',(-10.0026147430001,12.2,-2.78616069100002));
#269150=CARTESIAN_POINT('Ctrl Pts',(-10.0016518730001,12.2,-2.78598826400001));
#269151=CARTESIAN_POINT('Ctrl Pts',(-10.0006984370001,12.2,-2.78581654400002));
#269152=CARTESIAN_POINT('Ctrl Pts',(-9.99975446000006,12.2,-2.78564555200001));
#269153=CARTESIAN_POINT('Ctrl Pts',(-9.99881996400006,12.2,-2.78547531100001));
#269154=CARTESIAN_POINT('Ctrl Pts',(-9.99789497300006,12.2,-2.78530584400002));
#269155=CARTESIAN_POINT('Ctrl Pts',(-9.99697950700006,12.2,-2.78513717200001));
#269156=CARTESIAN_POINT('Ctrl Pts',(-9.99607881100006,12.2,-2.78497028600002));
#269157=CARTESIAN_POINT('Ctrl Pts',(-9.99536684700006,12.2,-2.78483763500001));
#269158=CARTESIAN_POINT('Ctrl Pts',(-9.99483840000006,12.2,-2.78473877000001));
#269159=CARTESIAN_POINT('Ctrl Pts',(-9.99448967700006,12.2,-2.78467334900002));
#269160=CARTESIAN_POINT('Ctrl Pts',(-9.99431831700005,12.2,-2.78464115900002));
#269161=CARTESIAN_POINT('Ctrl Pts',(-9.99431831700005,15.2,-2.78464115900002));
#269162=CARTESIAN_POINT('Ctrl Pts',(-9.99448967700006,15.2,-2.78467334900002));
#269163=CARTESIAN_POINT('Ctrl Pts',(-9.99483840000006,15.2,-2.78473877000001));
#269164=CARTESIAN_POINT('Ctrl Pts',(-9.99536684700006,15.2,-2.78483763500001));
#269165=CARTESIAN_POINT('Ctrl Pts',(-9.99607881100006,15.2,-2.78497028600002));
#269166=CARTESIAN_POINT('Ctrl Pts',(-9.99697950700006,15.2,-2.78513717200001));
#269167=CARTESIAN_POINT('Ctrl Pts',(-9.99789497300006,15.2,-2.78530584400002));
#269168=CARTESIAN_POINT('Ctrl Pts',(-9.99881996400006,15.2,-2.78547531100001));
#269169=CARTESIAN_POINT('Ctrl Pts',(-9.99975446000006,15.2,-2.78564555200001));
#269170=CARTESIAN_POINT('Ctrl Pts',(-10.0006984370001,15.2,-2.78581654400002));
#269171=CARTESIAN_POINT('Ctrl Pts',(-10.0016518730001,15.2,-2.78598826400001));
#269172=CARTESIAN_POINT('Ctrl Pts',(-10.0026147430001,15.2,-2.78616069100002));
#269173=CARTESIAN_POINT('Ctrl Pts',(-10.0035870240001,15.2,-2.78633380100001));
#269174=CARTESIAN_POINT('Ctrl Pts',(-10.0045686950001,15.2,-2.78650757300001));
#269175=CARTESIAN_POINT('Ctrl Pts',(-10.0055597320001,15.2,-2.78668198500001));
#269176=CARTESIAN_POINT('Ctrl Pts',(-10.0065601130001,15.2,-2.78685701400001));
#269177=CARTESIAN_POINT('Ctrl Pts',(-10.0075698160001,15.2,-2.78703264000002));
#269178=CARTESIAN_POINT('Ctrl Pts',(-10.0085888180001,15.2,-2.78720884000002));
#269179=CARTESIAN_POINT('Ctrl Pts',(-10.0096170970001,15.2,-2.78738559300002));
#269180=CARTESIAN_POINT('Ctrl Pts',(-10.0106546300001,15.2,-2.78756287700002));
#269181=CARTESIAN_POINT('Ctrl Pts',(-10.0117013970001,15.2,-2.78774067200001));
#269182=CARTESIAN_POINT('Ctrl Pts',(-10.0127573730001,15.2,-2.78791895500001));
#269183=CARTESIAN_POINT('Ctrl Pts',(-10.0138225390001,15.2,-2.78809770600001));
#269184=CARTESIAN_POINT('Ctrl Pts',(-10.0148968710001,15.2,-2.78827690400002));
#269185=CARTESIAN_POINT('Ctrl Pts',(-10.0159803500001,15.2,-2.78845652900001));
#269186=CARTESIAN_POINT('Ctrl Pts',(-10.0170729510001,15.2,-2.78863655800001));
#269187=CARTESIAN_POINT('Ctrl Pts',(-10.0181746550001,15.2,-2.78881697100001));
#269188=CARTESIAN_POINT('Ctrl Pts',(-10.0192854400001,15.2,-2.78899774900002));
#269189=CARTESIAN_POINT('Ctrl Pts',(-10.0204052840001,15.2,-2.78917887200001));
#269190=CARTESIAN_POINT('Ctrl Pts',(-10.0215341660001,15.2,-2.78936031700002));
#269191=CARTESIAN_POINT('Ctrl Pts',(-10.0226720660001,15.2,-2.78954206400002));
#269192=CARTESIAN_POINT('Ctrl Pts',(-10.0238189610001,15.2,-2.78972409500001));
#269193=CARTESIAN_POINT('Ctrl Pts',(-10.0249748320001,15.2,-2.78990638900002));
#269194=CARTESIAN_POINT('Ctrl Pts',(-10.0261396570001,15.2,-2.79008892600002));
#269195=CARTESIAN_POINT('Ctrl Pts',(-10.0273134150001,15.2,-2.79027168600001));
#269196=CARTESIAN_POINT('Ctrl Pts',(-10.0284960860001,15.2,-2.79045465000001));
#269197=CARTESIAN_POINT('Ctrl Pts',(-10.0296876490001,15.2,-2.79063779700001));
#269198=CARTESIAN_POINT('Ctrl Pts',(-10.0308880840001,15.2,-2.79082110900001));
#269199=CARTESIAN_POINT('Ctrl Pts',(-10.0320973690001,15.2,-2.79100456500001));
#269200=CARTESIAN_POINT('Ctrl Pts',(-10.0333154850001,15.2,-2.79118814800002));
#269201=CARTESIAN_POINT('Ctrl Pts',(-10.0345424120001,15.2,-2.79137183600001));
#269202=CARTESIAN_POINT('Ctrl Pts',(-10.0357781300001,15.2,-2.79155561300001));
#269203=CARTESIAN_POINT('Ctrl Pts',(-10.0370226160001,15.2,-2.79173945600002));
#269204=CARTESIAN_POINT('Ctrl Pts',(-10.0382758530001,15.2,-2.79192335000001));
#269205=CARTESIAN_POINT('Ctrl Pts',(-10.0395378210001,15.2,-2.79210727300002));
#269206=CARTESIAN_POINT('Ctrl Pts',(-10.0408084970001,15.2,-2.79229120900002));
#269207=CARTESIAN_POINT('Ctrl Pts',(-10.0420878650001,15.2,-2.79247513800001));
#269208=CARTESIAN_POINT('Ctrl Pts',(-10.0433759040001,15.2,-2.79265904000002));
#269209=CARTESIAN_POINT('Ctrl Pts',(-10.0446725930001,15.2,-2.79284289900001));
#269210=CARTESIAN_POINT('Ctrl Pts',(-10.0459779130001,15.2,-2.79302669500002));
#269211=CARTESIAN_POINT('Ctrl Pts',(-10.0472918460001,15.2,-2.79321041100001));
#269212=CARTESIAN_POINT('Ctrl Pts',(-10.0486143700001,15.2,-2.79339402900002));
#269213=CARTESIAN_POINT('Ctrl Pts',(-10.0499454690001,15.2,-2.79357752900002));
#269214=CARTESIAN_POINT('Ctrl Pts',(-10.0512851200001,15.2,-2.79376089400001));
#269215=CARTESIAN_POINT('Ctrl Pts',(-10.0526333070001,15.2,-2.79394410600001));
#269216=CARTESIAN_POINT('Ctrl Pts',(-10.0539900080001,15.2,-2.79412714600001));
#269217=CARTESIAN_POINT('Ctrl Pts',(-10.0553552060001,15.2,-2.79430999900002));
#269218=CARTESIAN_POINT('Ctrl Pts',(-10.0567288820001,15.2,-2.79449264500002));
#269219=CARTESIAN_POINT('Ctrl Pts',(-10.0581110160001,15.2,-2.79467506700001));
#269220=CARTESIAN_POINT('Ctrl Pts',(-10.0595015910001,15.2,-2.79485724800002));
#269221=CARTESIAN_POINT('Ctrl Pts',(-10.0609005850001,15.2,-2.79503917100001));
#269222=CARTESIAN_POINT('Ctrl Pts',(-10.0623079820001,15.2,-2.79522081700001));
#269223=CARTESIAN_POINT('Ctrl Pts',(-10.0637237620001,15.2,-2.79540216900001));
#269224=CARTESIAN_POINT('Ctrl Pts',(-10.0651479080001,15.2,-2.79558321000001));
#269225=CARTESIAN_POINT('Ctrl Pts',(-10.0665803990001,15.2,-2.79576392500001));
#269226=CARTESIAN_POINT('Ctrl Pts',(-10.0680212180001,15.2,-2.79594429400001));
#269227=CARTESIAN_POINT('Ctrl Pts',(-10.0694703480001,15.2,-2.79612430200002));
#269228=CARTESIAN_POINT('Ctrl Pts',(-10.0709277690001,15.2,-2.79630393100001));
#269229=CARTESIAN_POINT('Ctrl Pts',(-10.0723934620001,15.2,-2.79648316500001));
#269230=CARTESIAN_POINT('Ctrl Pts',(-10.0738674120001,15.2,-2.79666198700002));
#269231=CARTESIAN_POINT('Ctrl Pts',(-10.0753495960001,15.2,-2.79684038000001));
#269232=CARTESIAN_POINT('Ctrl Pts',(-10.0768400010001,15.2,-2.79701832800002));
#269233=CARTESIAN_POINT('Ctrl Pts',(-10.0783386060001,15.2,-2.79719581400002));
#269234=CARTESIAN_POINT('Ctrl Pts',(-10.0798453950001,15.2,-2.79737282200001));
#269235=CARTESIAN_POINT('Ctrl Pts',(-10.0813603480001,15.2,-2.79754933600001));
#269236=CARTESIAN_POINT('Ctrl Pts',(-10.0828834480001,15.2,-2.79772534000001));
#269237=CARTESIAN_POINT('Ctrl Pts',(-10.0844146780001,15.2,-2.79790081600002));
#269238=CARTESIAN_POINT('Ctrl Pts',(-10.0859540200001,15.2,-2.79807574900001));
#269239=CARTESIAN_POINT('Ctrl Pts',(-10.0875014570001,15.2,-2.79825012400002));
#269240=CARTESIAN_POINT('Ctrl Pts',(-10.0890569700001,15.2,-2.79842392300001));
#269241=CARTESIAN_POINT('Ctrl Pts',(-10.0906205420001,15.2,-2.79859713200001));
#269242=CARTESIAN_POINT('Ctrl Pts',(-10.0921921570001,15.2,-2.79876973500001));
#269243=CARTESIAN_POINT('Ctrl Pts',(-10.0937717960001,15.2,-2.79894171500001));
#269244=CARTESIAN_POINT('Ctrl Pts',(-10.0953594420001,15.2,-2.79911305800002));
#269245=CARTESIAN_POINT('Ctrl Pts',(-10.0969550780001,15.2,-2.79928374700001));
#269246=CARTESIAN_POINT('Ctrl Pts',(-10.0985586870001,15.2,-2.79945376700002));
#269247=CARTESIAN_POINT('Ctrl Pts',(-10.1001702510001,15.2,-2.79962310200002));
#269248=CARTESIAN_POINT('Ctrl Pts',(-10.1017897540001,15.2,-2.79979173800001));
#269249=CARTESIAN_POINT('Ctrl Pts',(-10.1034171790001,15.2,-2.79995965800001));
#269250=CARTESIAN_POINT('Ctrl Pts',(-10.1050525090001,15.2,-2.80012684900001));
#269251=CARTESIAN_POINT('Ctrl Pts',(-10.1066957250001,15.2,-2.80029329300001));
#269252=CARTESIAN_POINT('Ctrl Pts',(-10.1083468140001,15.2,-2.80045897600001));
#269253=CARTESIAN_POINT('Ctrl Pts',(-10.1100057560001,15.2,-2.80062388500002));
#269254=CARTESIAN_POINT('Ctrl Pts',(-10.1116725360001,15.2,-2.80078800200001));
#269255=CARTESIAN_POINT('Ctrl Pts',(-10.1133471370001,15.2,-2.80095131400001));
#269256=CARTESIAN_POINT('Ctrl Pts',(-10.1150295420001,15.2,-2.80111380600002));
#269257=CARTESIAN_POINT('Ctrl Pts',(-10.1167197340001,15.2,-2.80127546300001));
#269258=CARTESIAN_POINT('Ctrl Pts',(-10.1184176970001,15.2,-2.80143626900001));
#269259=CARTESIAN_POINT('Ctrl Pts',(-10.1201234150001,15.2,-2.80159621100001));
#269260=CARTESIAN_POINT('Ctrl Pts',(-10.1218368710001,15.2,-2.80175527400001));
#269261=CARTESIAN_POINT('Ctrl Pts',(-10.1235580500001,15.2,-2.80191344300002));
#269262=CARTESIAN_POINT('Ctrl Pts',(-10.1252869340001,15.2,-2.80207070400001));
#269263=CARTESIAN_POINT('Ctrl Pts',(-10.1270235070001,15.2,-2.80222704300002));
#269264=CARTESIAN_POINT('Ctrl Pts',(-10.1287677530001,15.2,-2.80238244500001));
#269265=CARTESIAN_POINT('Ctrl Pts',(-10.1305196570001,15.2,-2.80253689600002));
#269266=CARTESIAN_POINT('Ctrl Pts',(-10.1322792010001,15.2,-2.80269038200001));
#269267=CARTESIAN_POINT('Ctrl Pts',(-10.1340463700001,15.2,-2.80284288800001));
#269268=CARTESIAN_POINT('Ctrl Pts',(-10.1358211480001,15.2,-2.80299440200002));
#269269=CARTESIAN_POINT('Ctrl Pts',(-10.1376035180001,15.2,-2.80314490700002));
#269270=CARTESIAN_POINT('Ctrl Pts',(-10.1393934660001,15.2,-2.80329439100001));
#269271=CARTESIAN_POINT('Ctrl Pts',(-10.1411909760001,15.2,-2.80344284000002));
#269272=CARTESIAN_POINT('Ctrl Pts',(-10.1429960300001,15.2,-2.80359024000001));
#269273=CARTESIAN_POINT('Ctrl Pts',(-10.1448086140001,15.2,-2.80373657700002));
#269274=CARTESIAN_POINT('Ctrl Pts',(-10.1466287130001,15.2,-2.80388183700001));
#269275=CARTESIAN_POINT('Ctrl Pts',(-10.1484563090001,15.2,-2.80402600700001));
#269276=CARTESIAN_POINT('Ctrl Pts',(-10.1502913890001,15.2,-2.80416907300001));
#269277=CARTESIAN_POINT('Ctrl Pts',(-10.1521339360001,15.2,-2.80431102100001));
#269278=CARTESIAN_POINT('Ctrl Pts',(-10.1539839340001,15.2,-2.80445183900001));
#269279=CARTESIAN_POINT('Ctrl Pts',(-10.1558413680001,15.2,-2.80459151300001));
#269280=CARTESIAN_POINT('Ctrl Pts',(-10.1577062240001,15.2,-2.80473002900001));
#269281=CARTESIAN_POINT('Ctrl Pts',(-10.1595784840001,15.2,-2.80486737300001));
#269282=CARTESIAN_POINT('Ctrl Pts',(-10.1614581350001,15.2,-2.80500353400001));
#269283=CARTESIAN_POINT('Ctrl Pts',(-10.1633451610001,15.2,-2.80513849600001));
#269284=CARTESIAN_POINT('Ctrl Pts',(-10.1652395470001,15.2,-2.80527224900001));
#269285=CARTESIAN_POINT('Ctrl Pts',(-10.1671412760001,15.2,-2.80540477800002));
#269286=CARTESIAN_POINT('Ctrl Pts',(-10.1690503350001,15.2,-2.80553606900002));
#269287=CARTESIAN_POINT('Ctrl Pts',(-10.1709667090001,15.2,-2.80566611100001));
#269288=CARTESIAN_POINT('Ctrl Pts',(-10.1728903810001,15.2,-2.80579489000001));
#269289=CARTESIAN_POINT('Ctrl Pts',(-10.1748213380001,15.2,-2.80592239500002));
#269290=CARTESIAN_POINT('Ctrl Pts',(-10.1767595650001,15.2,-2.80604861000001));
#269291=CARTESIAN_POINT('Ctrl Pts',(-10.1787050450001,15.2,-2.80617352500002));
#269292=CARTESIAN_POINT('Ctrl Pts',(-10.1806577650001,15.2,-2.80629712500001));
#269293=CARTESIAN_POINT('Ctrl Pts',(-10.1826177100001,15.2,-2.80641939900002));
#269294=CARTESIAN_POINT('Ctrl Pts',(-10.1845848630001,15.2,-2.80654033300001));
#269295=CARTESIAN_POINT('Ctrl Pts',(-10.1865592120001,15.2,-2.80665991700001));
#269296=CARTESIAN_POINT('Ctrl Pts',(-10.1885407420001,15.2,-2.80677813600001));
#269297=CARTESIAN_POINT('Ctrl Pts',(-10.1905294380001,15.2,-2.80689497800001));
#269298=CARTESIAN_POINT('Ctrl Pts',(-10.1925252840001,15.2,-2.80701043200001));
#269299=CARTESIAN_POINT('Ctrl Pts',(-10.1945282670001,15.2,-2.80712448400001));
#269300=CARTESIAN_POINT('Ctrl Pts',(-10.1965383710001,15.2,-2.80723712200002));
#269301=CARTESIAN_POINT('Ctrl Pts',(-10.1985555830001,15.2,-2.80734833400002));
#269302=CARTESIAN_POINT('Ctrl Pts',(-10.2005798890001,15.2,-2.80745810900001));
#269303=CARTESIAN_POINT('Ctrl Pts',(-10.2026112720001,15.2,-2.80756643300001));
#269304=CARTESIAN_POINT('Ctrl Pts',(-10.2046497210001,15.2,-2.80767329400001));
#269305=CARTESIAN_POINT('Ctrl Pts',(-10.2066952180001,15.2,-2.80777868100001));
#269306=CARTESIAN_POINT('Ctrl Pts',(-10.2087477520001,15.2,-2.80788258200001));
#269307=CARTESIAN_POINT('Ctrl Pts',(-10.2108073070001,15.2,-2.80798498300001));
#269308=CARTESIAN_POINT('Ctrl Pts',(-10.2128738680001,15.2,-2.80808587500001));
#269309=CARTESIAN_POINT('Ctrl Pts',(-10.2149474230001,15.2,-2.80818524500001));
#269310=CARTESIAN_POINT('Ctrl Pts',(-10.2170279560001,15.2,-2.80828308000002));
#269311=CARTESIAN_POINT('Ctrl Pts',(-10.2191154540001,15.2,-2.80837937100001));
#269312=CARTESIAN_POINT('Ctrl Pts',(-10.2212099030001,15.2,-2.80847410200002));
#269313=CARTESIAN_POINT('Ctrl Pts',(-10.2233112870001,15.2,-2.80856726500001));
#269314=CARTESIAN_POINT('Ctrl Pts',(-10.2254195960001,15.2,-2.80865884700002));
#269315=CARTESIAN_POINT('Ctrl Pts',(-10.2275348110001,15.2,-2.80874883800001));
#269316=CARTESIAN_POINT('Ctrl Pts',(-10.2296569220001,15.2,-2.80883722400001));
#269317=CARTESIAN_POINT('Ctrl Pts',(-10.2317859140001,15.2,-2.80892399500001));
#269318=CARTESIAN_POINT('Ctrl Pts',(-10.2339217720001,15.2,-2.80900913800001));
#269319=CARTESIAN_POINT('Ctrl Pts',(-10.2360644840001,15.2,-2.80909264400002));
#269320=CARTESIAN_POINT('Ctrl Pts',(-10.2382140350001,15.2,-2.80917450000001));
#269321=CARTESIAN_POINT('Ctrl Pts',(-10.2403704120001,15.2,-2.80925469500001));
#269322=CARTESIAN_POINT('Ctrl Pts',(-10.2425336010001,15.2,-2.80933321800001));
#269323=CARTESIAN_POINT('Ctrl Pts',(-10.2447035880001,15.2,-2.80941005800001));
#269324=CARTESIAN_POINT('Ctrl Pts',(-10.2468803590001,15.2,-2.80948520200001));
#269325=CARTESIAN_POINT('Ctrl Pts',(-10.2490639020001,15.2,-2.80955864200001));
#269326=CARTESIAN_POINT('Ctrl Pts',(-10.2512542030001,15.2,-2.80963036400002));
#269327=CARTESIAN_POINT('Ctrl Pts',(-10.2534512460001,15.2,-2.80970035900001));
#269328=CARTESIAN_POINT('Ctrl Pts',(-10.2556550210001,15.2,-2.80976861500001));
#269329=CARTESIAN_POINT('Ctrl Pts',(-10.2578655120001,15.2,-2.80983512200002));
#269330=CARTESIAN_POINT('Ctrl Pts',(-10.2600827090001,15.2,-2.80989986700002));
#269331=CARTESIAN_POINT('Ctrl Pts',(-10.2623065940001,15.2,-2.80996284100001));
#269332=CARTESIAN_POINT('Ctrl Pts',(-10.2645371560001,15.2,-2.81002403300001));
#269333=CARTESIAN_POINT('Ctrl Pts',(-10.2667743820001,15.2,-2.81008343100002));
#269334=CARTESIAN_POINT('Ctrl Pts',(-10.2690182590001,15.2,-2.81014102700002));
#269335=CARTESIAN_POINT('Ctrl Pts',(-10.2712687710001,15.2,-2.81019680600001));
#269336=CARTESIAN_POINT('Ctrl Pts',(-10.2735259090001,15.2,-2.81025076200002));
#269337=CARTESIAN_POINT('Ctrl Pts',(-10.2757896570001,15.2,-2.81030288000002));
#269338=CARTESIAN_POINT('Ctrl Pts',(-10.2780600020001,15.2,-2.81035315300001));
#269339=CARTESIAN_POINT('Ctrl Pts',(-10.2803369320001,15.2,-2.81040156800001));
#269340=CARTESIAN_POINT('Ctrl Pts',(-10.2826204320001,15.2,-2.81044811600001));
#269341=CARTESIAN_POINT('Ctrl Pts',(-10.2849104920001,15.2,-2.81049278600001));
#269342=CARTESIAN_POINT('Ctrl Pts',(-10.2872070960001,15.2,-2.81053556800002));
#269343=CARTESIAN_POINT('Ctrl Pts',(-10.2895102320001,15.2,-2.81057645100002));
#269344=CARTESIAN_POINT('Ctrl Pts',(-10.2918198870001,15.2,-2.81061542500002));
#269345=CARTESIAN_POINT('Ctrl Pts',(-10.2941360500001,15.2,-2.81065248000001));
#269346=CARTESIAN_POINT('Ctrl Pts',(-10.2964587060001,15.2,-2.81068760400002));
#269347=CARTESIAN_POINT('Ctrl Pts',(-10.2987878420001,15.2,-2.81072079000001));
#269348=CARTESIAN_POINT('Ctrl Pts',(-10.3011234450001,15.2,-2.81075202400002));
#269349=CARTESIAN_POINT('Ctrl Pts',(-10.3034655040001,15.2,-2.81078129900001));
#269350=CARTESIAN_POINT('Ctrl Pts',(-10.3058140040001,15.2,-2.81080860400001));
#269351=CARTESIAN_POINT('Ctrl Pts',(-10.3081689340001,15.2,-2.81083392700001));
#269352=CARTESIAN_POINT('Ctrl Pts',(-10.3105302810001,15.2,-2.81085726100001));
#269353=CARTESIAN_POINT('Ctrl Pts',(-10.3128980330001,15.2,-2.81087859400001));
#269354=CARTESIAN_POINT('Ctrl Pts',(-10.3152721750001,15.2,-2.81089791800001));
#269355=CARTESIAN_POINT('Ctrl Pts',(-10.3176526950001,15.2,-2.81091522000001));
#269356=CARTESIAN_POINT('Ctrl Pts',(-10.3200395830001,15.2,-2.81093049300001));
#269357=CARTESIAN_POINT('Ctrl Pts',(-10.3224328240001,15.2,-2.81094372600001));
#269358=CARTESIAN_POINT('Ctrl Pts',(-10.3248324060001,15.2,-2.81095490800002));
#269359=CARTESIAN_POINT('Ctrl Pts',(-10.3272383160001,15.2,-2.81096403100001));
#269360=CARTESIAN_POINT('Ctrl Pts',(-10.3296505420001,15.2,-2.81097108600001));
#269361=CARTESIAN_POINT('Ctrl Pts',(-10.3320690720001,15.2,-2.81097606100001));
#269362=CARTESIAN_POINT('Ctrl Pts',(-10.3344938940001,15.2,-2.81097894800002));
#269363=CARTESIAN_POINT('Ctrl Pts',(-10.3369249940001,15.2,-2.81097973500001));
#269364=CARTESIAN_POINT('Ctrl Pts',(-10.3393623600001,15.2,-2.81097841600001));
#269365=CARTESIAN_POINT('Ctrl Pts',(-10.3418059810001,15.2,-2.81097497900001));
#269366=CARTESIAN_POINT('Ctrl Pts',(-10.3442558440001,15.2,-2.81096941500001));
#269367=CARTESIAN_POINT('Ctrl Pts',(-10.3467119360001,15.2,-2.81096171500002));
#269368=CARTESIAN_POINT('Ctrl Pts',(-10.3491742450001,15.2,-2.81095186900002));
#269369=CARTESIAN_POINT('Ctrl Pts',(-10.3516427590001,15.2,-2.81093986800002));
#269370=CARTESIAN_POINT('Ctrl Pts',(-10.3541174660001,15.2,-2.81092570300002));
#269371=CARTESIAN_POINT('Ctrl Pts',(-10.3565983540001,15.2,-2.81090936300001));
#269372=CARTESIAN_POINT('Ctrl Pts',(-10.3590854110001,15.2,-2.81089083900001));
#269373=CARTESIAN_POINT('Ctrl Pts',(-10.3615786240001,15.2,-2.81087012400001));
#269374=CARTESIAN_POINT('Ctrl Pts',(-10.3640779820001,15.2,-2.81084720700001));
#269375=CARTESIAN_POINT('Ctrl Pts',(-10.3665834700001,15.2,-2.81082207900001));
#269376=CARTESIAN_POINT('Ctrl Pts',(-10.3690950810001,15.2,-2.81079473000001));
#269377=CARTESIAN_POINT('Ctrl Pts',(-10.3716127990001,15.2,-2.81076515200001));
#269378=CARTESIAN_POINT('Ctrl Pts',(-10.3741366140001,15.2,-2.81073333600002));
#269379=CARTESIAN_POINT('Ctrl Pts',(-10.3766665130001,15.2,-2.81069927400001));
#269380=CARTESIAN_POINT('Ctrl Pts',(-10.3792024840001,15.2,-2.81066295300001));
#269381=CARTESIAN_POINT('Ctrl Pts',(-10.3817445160001,15.2,-2.81062436900001));
#269382=CARTESIAN_POINT('Ctrl Pts',(-10.3842925970001,15.2,-2.81058350800001));
#269383=CARTESIAN_POINT('Ctrl Pts',(-10.3868467140001,15.2,-2.81054036500001));
#269384=CARTESIAN_POINT('Ctrl Pts',(-10.3894068560001,15.2,-2.81049493000001));
#269385=CARTESIAN_POINT('Ctrl Pts',(-10.3919730120001,15.2,-2.81044719300001));
#269386=CARTESIAN_POINT('Ctrl Pts',(-10.3945451690001,15.2,-2.81039714800002));
#269387=CARTESIAN_POINT('Ctrl Pts',(-10.3971233170001,15.2,-2.81034478200001));
#269388=CARTESIAN_POINT('Ctrl Pts',(-10.3997074400001,15.2,-2.81029008900001));
#269389=CARTESIAN_POINT('Ctrl Pts',(-10.4022975320001,15.2,-2.81023306000002));
#269390=CARTESIAN_POINT('Ctrl Pts',(-10.4048935770001,15.2,-2.81017368600001));
#269391=CARTESIAN_POINT('Ctrl Pts',(-10.4074955650001,15.2,-2.81011195800001));
#269392=CARTESIAN_POINT('Ctrl Pts',(-10.4101034850001,15.2,-2.81004786800001));
#269393=CARTESIAN_POINT('Ctrl Pts',(-10.4127173250001,15.2,-2.80998140700001));
#269394=CARTESIAN_POINT('Ctrl Pts',(-10.4153370720001,15.2,-2.80991256500001));
#269395=CARTESIAN_POINT('Ctrl Pts',(-10.4179627160001,15.2,-2.80984133700001));
#269396=CARTESIAN_POINT('Ctrl Pts',(-10.4205942460001,15.2,-2.80976771100002));
#269397=CARTESIAN_POINT('Ctrl Pts',(-10.4232316480001,15.2,-2.80969168100001));
#269398=CARTESIAN_POINT('Ctrl Pts',(-10.4258749130001,15.2,-2.80961323700001));
#269399=CARTESIAN_POINT('Ctrl Pts',(-10.4285240300001,15.2,-2.80953237000002));
#269400=CARTESIAN_POINT('Ctrl Pts',(-10.4311789840001,15.2,-2.80944907300002));
#269401=CARTESIAN_POINT('Ctrl Pts',(-10.4338397670001,15.2,-2.80936333700001));
#269402=CARTESIAN_POINT('Ctrl Pts',(-10.4365063660001,15.2,-2.80927515500002));
#269403=CARTESIAN_POINT('Ctrl Pts',(-10.4391787700001,15.2,-2.80918451700002));
#269404=CARTESIAN_POINT('Ctrl Pts',(-10.4418569680001,15.2,-2.80909141400001));
#269405=CARTESIAN_POINT('Ctrl Pts',(-10.4445409480001,15.2,-2.80899584100001));
#269406=CARTESIAN_POINT('Ctrl Pts',(-10.4472306990001,15.2,-2.80889778700002));
#269407=CARTESIAN_POINT('Ctrl Pts',(-10.4499262110001,15.2,-2.80879724300001));
#269408=CARTESIAN_POINT('Ctrl Pts',(-10.4526274700001,15.2,-2.80869420500002));
#269409=CARTESIAN_POINT('Ctrl Pts',(-10.4553344680001,15.2,-2.80858866000001));
#269410=CARTESIAN_POINT('Ctrl Pts',(-10.4580471910001,15.2,-2.80848060400002));
#269411=CARTESIAN_POINT('Ctrl Pts',(-10.4607656300001,15.2,-2.80837002600002));
#269412=CARTESIAN_POINT('Ctrl Pts',(-10.4634897720001,15.2,-2.80825691900001));
#269413=CARTESIAN_POINT('Ctrl Pts',(-10.4662196070001,15.2,-2.80814127600001));
#269414=CARTESIAN_POINT('Ctrl Pts',(-10.4689551240001,15.2,-2.80802308700002));
#269415=CARTESIAN_POINT('Ctrl Pts',(-10.4716963110001,15.2,-2.80790234500001));
#269416=CARTESIAN_POINT('Ctrl Pts',(-10.4744431570001,15.2,-2.80777904200002));
#269417=CARTESIAN_POINT('Ctrl Pts',(-10.4771956530001,15.2,-2.80765317100002));
#269418=CARTESIAN_POINT('Ctrl Pts',(-10.4799537850001,15.2,-2.80752472200001));
#269419=CARTESIAN_POINT('Ctrl Pts',(-10.4827175440001,15.2,-2.80739369000001));
#269420=CARTESIAN_POINT('Ctrl Pts',(-10.4854869180001,15.2,-2.80726006400001));
#269421=CARTESIAN_POINT('Ctrl Pts',(-10.4882618970001,15.2,-2.80712384000001));
#269422=CARTESIAN_POINT('Ctrl Pts',(-10.4910424700001,15.2,-2.80698500600002));
#269423=CARTESIAN_POINT('Ctrl Pts',(-10.4938286240001,15.2,-2.80684355700001));
#269424=CARTESIAN_POINT('Ctrl Pts',(-10.4966203510001,15.2,-2.80669948500002));
#269425=CARTESIAN_POINT('Ctrl Pts',(-10.4994176380001,15.2,-2.80655278100001));
#269426=CARTESIAN_POINT('Ctrl Pts',(-10.5022204750001,15.2,-2.80640343900001));
#269427=CARTESIAN_POINT('Ctrl Pts',(-10.5050288510001,15.2,-2.80625145000001));
#269428=CARTESIAN_POINT('Ctrl Pts',(-10.5078427570001,15.2,-2.80609680700001));
#269429=CARTESIAN_POINT('Ctrl Pts',(-10.5106621790001,15.2,-2.80593950300001));
#269430=CARTESIAN_POINT('Ctrl Pts',(-10.5134871080001,15.2,-2.80577952900002));
#269431=CARTESIAN_POINT('Ctrl Pts',(-10.5163175340001,15.2,-2.80561687900001));
#269432=CARTESIAN_POINT('Ctrl Pts',(-10.5191534450001,15.2,-2.80545154400002));
#269433=CARTESIAN_POINT('Ctrl Pts',(-10.5225631056762,15.2,-2.80524991280734));
#269434=CARTESIAN_POINT('Ctrl Pts',(-10.525980964162,15.2,-2.80504423309635));
#269435=CARTESIAN_POINT('Ctrl Pts',(-10.5294069978381,15.2,-2.80483448890367));
#269436=CARTESIAN_POINT('Ctrl Pts',(-10.532841182012,15.2,-2.80462066721212));
#269437=CARTESIAN_POINT('Ctrl Pts',(-10.5362835010001,15.2,-2.80440275200001));
#269438=CARTESIAN_POINT('Ctrl Pts',(-10.5391575100001,15.2,-2.80421842000001));
#269439=CARTESIAN_POINT('Ctrl Pts',(-10.5420369180001,15.2,-2.80403134500002));
#269440=CARTESIAN_POINT('Ctrl Pts',(-10.5449217170001,15.2,-2.80384151900002));
#269441=CARTESIAN_POINT('Ctrl Pts',(-10.5478118940001,15.2,-2.80364893500002));
#269442=CARTESIAN_POINT('Ctrl Pts',(-10.5507074410001,15.2,-2.80345358600002));
#269443=CARTESIAN_POINT('Ctrl Pts',(-10.5536083460001,15.2,-2.80325546500002));
#269444=CARTESIAN_POINT('Ctrl Pts',(-10.5565145980001,15.2,-2.80305456500002));
#269445=CARTESIAN_POINT('Ctrl Pts',(-10.5594261870001,15.2,-2.80285087700001));
#269446=CARTESIAN_POINT('Ctrl Pts',(-10.5623431030001,15.2,-2.80264439700002));
#269447=CARTESIAN_POINT('Ctrl Pts',(-10.5652653350001,15.2,-2.80243511500001));
#269448=CARTESIAN_POINT('Ctrl Pts',(-10.5681928730001,15.2,-2.80222302500002));
#269449=CARTESIAN_POINT('Ctrl Pts',(-10.5711257080001,15.2,-2.80200812100002));
#269450=CARTESIAN_POINT('Ctrl Pts',(-10.5740638260001,15.2,-2.80179039400001));
#269451=CARTESIAN_POINT('Ctrl Pts',(-10.5770072200001,15.2,-2.80156983800001));
#269452=CARTESIAN_POINT('Ctrl Pts',(-10.5799558780001,15.2,-2.80134644700002));
#269453=CARTESIAN_POINT('Ctrl Pts',(-10.5829097920001,15.2,-2.80112021200001));
#269454=CARTESIAN_POINT('Ctrl Pts',(-10.5858689480001,15.2,-2.80089112800002));
#269455=CARTESIAN_POINT('Ctrl Pts',(-10.5888333380001,15.2,-2.80065918700001));
#269456=CARTESIAN_POINT('Ctrl Pts',(-10.5918029510001,15.2,-2.80042438200002));
#269457=CARTESIAN_POINT('Ctrl Pts',(-10.5947777780001,15.2,-2.80018670600001));
#269458=CARTESIAN_POINT('Ctrl Pts',(-10.5977578070001,15.2,-2.79994615300001));
#269459=CARTESIAN_POINT('Ctrl Pts',(-10.6007430310001,15.2,-2.79970271700002));
#269460=CARTESIAN_POINT('Ctrl Pts',(-10.6037334350001,15.2,-2.79945638900001));
#269461=CARTESIAN_POINT('Ctrl Pts',(-10.6067290130001,15.2,-2.79920716400001));
#269462=CARTESIAN_POINT('Ctrl Pts',(-10.6097297520001,15.2,-2.79895503300001));
#269463=CARTESIAN_POINT('Ctrl Pts',(-10.6127356450001,15.2,-2.79869999200002));
#269464=CARTESIAN_POINT('Ctrl Pts',(-10.6157466780001,15.2,-2.79844203300001));
#269465=CARTESIAN_POINT('Ctrl Pts',(-10.6187628440001,15.2,-2.79818114900001));
#269466=CARTESIAN_POINT('Ctrl Pts',(-10.6217841320001,15.2,-2.79791733300002));
#269467=CARTESIAN_POINT('Ctrl Pts',(-10.6248105320001,15.2,-2.79765058100002));
#269468=CARTESIAN_POINT('Ctrl Pts',(-10.6278420330001,15.2,-2.79738088400002));
#269469=CARTESIAN_POINT('Ctrl Pts',(-10.6308786260001,15.2,-2.79710823500002));
#269470=CARTESIAN_POINT('Ctrl Pts',(-10.6339203020001,15.2,-2.79683262800001));
#269471=CARTESIAN_POINT('Ctrl Pts',(-10.6369670490001,15.2,-2.79655405800002));
#269472=CARTESIAN_POINT('Ctrl Pts',(-10.6400188580001,15.2,-2.79627251700001));
#269473=CARTESIAN_POINT('Ctrl Pts',(-10.6430757180001,15.2,-2.79598800000001));
#269474=CARTESIAN_POINT('Ctrl Pts',(-10.6461376210001,15.2,-2.79570049800002));
#269475=CARTESIAN_POINT('Ctrl Pts',(-10.6492045550001,15.2,-2.79541000500001));
#269476=CARTESIAN_POINT('Ctrl Pts',(-10.6522765120001,15.2,-2.79511651600002));
#269477=CARTESIAN_POINT('Ctrl Pts',(-10.6553534800001,15.2,-2.79482002500002));
#269478=CARTESIAN_POINT('Ctrl Pts',(-10.6584354520001,15.2,-2.79452052500002));
#269479=CARTESIAN_POINT('Ctrl Pts',(-10.6615224160001,15.2,-2.79421800700002));
#269480=CARTESIAN_POINT('Ctrl Pts',(-10.6646143620001,15.2,-2.79391246900001));
#269481=CARTESIAN_POINT('Ctrl Pts',(-10.6677112820001,15.2,-2.79360390200001));
#269482=CARTESIAN_POINT('Ctrl Pts',(-10.6708131640001,15.2,-2.79329230000001));
#269483=CARTESIAN_POINT('Ctrl Pts',(-10.6739200000001,15.2,-2.79297765700001));
#269484=CARTESIAN_POINT('Ctrl Pts',(-10.6770317790001,15.2,-2.79265996700001));
#269485=CARTESIAN_POINT('Ctrl Pts',(-10.6801484920001,15.2,-2.79233922300001));
#269486=CARTESIAN_POINT('Ctrl Pts',(-10.6832701290001,15.2,-2.79201542000001));
#269487=CARTESIAN_POINT('Ctrl Pts',(-10.6863966800001,15.2,-2.79168855100002));
#269488=CARTESIAN_POINT('Ctrl Pts',(-10.6895281350001,15.2,-2.79135861000002));
#269489=CARTESIAN_POINT('Ctrl Pts',(-10.6926644870001,15.2,-2.79102559000002));
#269490=CARTESIAN_POINT('Ctrl Pts',(-10.6958057220001,15.2,-2.79068948600001));
#269491=CARTESIAN_POINT('Ctrl Pts',(-10.6989518340001,15.2,-2.79035029100001));
#269492=CARTESIAN_POINT('Ctrl Pts',(-10.7021028110001,15.2,-2.79000800100001));
#269493=CARTESIAN_POINT('Ctrl Pts',(-10.7052586450001,15.2,-2.78966260600002));
#269494=CARTESIAN_POINT('Ctrl Pts',(-10.7084193250001,15.2,-2.78931410400002));
#269495=CARTESIAN_POINT('Ctrl Pts',(-10.7115848430001,15.2,-2.78896248700002));
#269496=CARTESIAN_POINT('Ctrl Pts',(-10.7147551880001,15.2,-2.78860774800001));
#269497=CARTESIAN_POINT('Ctrl Pts',(-10.7179303500001,15.2,-2.78824988400002));
#269498=CARTESIAN_POINT('Ctrl Pts',(-10.7211103210001,15.2,-2.78788888700001));
#269499=CARTESIAN_POINT('Ctrl Pts',(-10.7242950910001,15.2,-2.78752475000001));
#269500=CARTESIAN_POINT('Ctrl Pts',(-10.7274846510001,15.2,-2.78715746900001));
#269501=CARTESIAN_POINT('Ctrl Pts',(-10.7306789900001,15.2,-2.78678703700002));
#269502=CARTESIAN_POINT('Ctrl Pts',(-10.7338780990001,15.2,-2.78641345000001));
#269503=CARTESIAN_POINT('Ctrl Pts',(-10.7370819700001,15.2,-2.78603669900002));
#269504=CARTESIAN_POINT('Ctrl Pts',(-10.7402905920001,15.2,-2.78565678100001));
#269505=CARTESIAN_POINT('Ctrl Pts',(-10.7435039560001,15.2,-2.78527368900002));
#269506=CARTESIAN_POINT('Ctrl Pts',(-10.7467220520001,15.2,-2.78488741600002));
#269507=CARTESIAN_POINT('Ctrl Pts',(-10.7499448710001,15.2,-2.78449795800002));
#269508=CARTESIAN_POINT('Ctrl Pts',(-10.7531724040001,15.2,-2.78410530900001));
#269509=CARTESIAN_POINT('Ctrl Pts',(-10.7564046420001,15.2,-2.78370946300001));
#269510=CARTESIAN_POINT('Ctrl Pts',(-10.7596415740001,15.2,-2.78331041300001));
#269511=CARTESIAN_POINT('Ctrl Pts',(-10.7628831920001,15.2,-2.78290815600001));
#269512=CARTESIAN_POINT('Ctrl Pts',(-10.7661294860001,15.2,-2.78250268300001));
#269513=CARTESIAN_POINT('Ctrl Pts',(-10.7693804470001,15.2,-2.78209399100001));
#269514=CARTESIAN_POINT('Ctrl Pts',(-10.7726360660001,15.2,-2.78168207300002));
#269515=CARTESIAN_POINT('Ctrl Pts',(-10.7758963330001,15.2,-2.78126692300001));
#269516=CARTESIAN_POINT('Ctrl Pts',(-10.7791612390001,15.2,-2.78084853700001));
#269517=CARTESIAN_POINT('Ctrl Pts',(-10.7824307750001,15.2,-2.78042690900001));
#269518=CARTESIAN_POINT('Ctrl Pts',(-10.7857049310001,15.2,-2.78000203100001));
#269519=CARTESIAN_POINT('Ctrl Pts',(-10.7889836990001,15.2,-2.77957390000001));
#269520=CARTESIAN_POINT('Ctrl Pts',(-10.7922670680001,15.2,-2.77914251000002));
#269521=CARTESIAN_POINT('Ctrl Pts',(-10.7955550300001,15.2,-2.77870785600001));
#269522=CARTESIAN_POINT('Ctrl Pts',(-10.7988475760001,15.2,-2.77826993000001));
#269523=CARTESIAN_POINT('Ctrl Pts',(-10.8021446960001,15.2,-2.77782872900001));
#269524=CARTESIAN_POINT('Ctrl Pts',(-10.8054463820001,15.2,-2.77738424700001));
#269525=CARTESIAN_POINT('Ctrl Pts',(-10.8087526240001,15.2,-2.77693647800001));
#269526=CARTESIAN_POINT('Ctrl Pts',(-10.8120634130001,15.2,-2.77648541700001));
#269527=CARTESIAN_POINT('Ctrl Pts',(-10.8153787400001,15.2,-2.77603105800001));
#269528=CARTESIAN_POINT('Ctrl Pts',(-10.8186985940001,15.2,-2.77557339600001));
#269529=CARTESIAN_POINT('Ctrl Pts',(-10.8220229700001,15.2,-2.77511242500001));
#269530=CARTESIAN_POINT('Ctrl Pts',(-10.8253518550001,15.2,-2.77464814100002));
#269531=CARTESIAN_POINT('Ctrl Pts',(-10.8286852410001,15.2,-2.77418053700002));
#269532=CARTESIAN_POINT('Ctrl Pts',(-10.8320231210001,15.2,-2.77370961000001));
#269533=CARTESIAN_POINT('Ctrl Pts',(-10.8353654830001,15.2,-2.77323535200001));
#269534=CARTESIAN_POINT('Ctrl Pts',(-10.8387123200001,15.2,-2.77275775900002));
#269535=CARTESIAN_POINT('Ctrl Pts',(-10.8420636210001,15.2,-2.77227682600001));
#269536=CARTESIAN_POINT('Ctrl Pts',(-10.8454193790001,15.2,-2.77179254700001));
#269537=CARTESIAN_POINT('Ctrl Pts',(-10.8487795840001,15.2,-2.77130491700001));
#269538=CARTESIAN_POINT('Ctrl Pts',(-10.8521442280001,15.2,-2.77081393100001));
#269539=CARTESIAN_POINT('Ctrl Pts',(-10.8555133010001,15.2,-2.77031958400002));
#269540=CARTESIAN_POINT('Ctrl Pts',(-10.8588867940001,15.2,-2.76982187100002));
#269541=CARTESIAN_POINT('Ctrl Pts',(-10.8622646980001,15.2,-2.76932078500002));
#269542=CARTESIAN_POINT('Ctrl Pts',(-10.8656470060001,15.2,-2.76881632300002));
#269543=CARTESIAN_POINT('Ctrl Pts',(-10.8690337060001,15.2,-2.76830847900001));
#269544=CARTESIAN_POINT('Ctrl Pts',(-10.8724247920001,15.2,-2.76779724700001));
#269545=CARTESIAN_POINT('Ctrl Pts',(-10.8758202520001,15.2,-2.76728262200002));
#269546=CARTESIAN_POINT('Ctrl Pts',(-10.8792200800001,15.2,-2.76676460200001));
#269547=CARTESIAN_POINT('Ctrl Pts',(-10.8826242650001,15.2,-2.76624317800001));
#269548=CARTESIAN_POINT('Ctrl Pts',(-10.8860328000001,15.2,-2.76571834600002));
#269549=CARTESIAN_POINT('Ctrl Pts',(-10.8894456750001,15.2,-2.76519010300001));
#269550=CARTESIAN_POINT('Ctrl Pts',(-10.8928628820001,15.2,-2.76465844200001));
#269551=CARTESIAN_POINT('Ctrl Pts',(-10.8962844110001,15.2,-2.76412335800002));
#269552=CARTESIAN_POINT('Ctrl Pts',(-10.8997102540001,15.2,-2.76358484600001));
#269553=CARTESIAN_POINT('Ctrl Pts',(-10.9031404020001,15.2,-2.76304290100001));
#269554=CARTESIAN_POINT('Ctrl Pts',(-10.9065748460001,15.2,-2.76249752000002));
#269555=CARTESIAN_POINT('Ctrl Pts',(-10.9100135780001,15.2,-2.76194869600001));
#269556=CARTESIAN_POINT('Ctrl Pts',(-10.9134565880001,15.2,-2.76139642400001));
#269557=CARTESIAN_POINT('Ctrl Pts',(-10.9169038680001,15.2,-2.76084070000001));
#269558=CARTESIAN_POINT('Ctrl Pts',(-10.9203554100001,15.2,-2.76028151900002));
#269559=CARTESIAN_POINT('Ctrl Pts',(-10.9238112040001,15.2,-2.75971887600001));
#269560=CARTESIAN_POINT('Ctrl Pts',(-10.9272712420001,15.2,-2.75915276600001));
#269561=CARTESIAN_POINT('Ctrl Pts',(-10.9307355160001,15.2,-2.75858318400001));
#269562=CARTESIAN_POINT('Ctrl Pts',(-10.9342040160001,15.2,-2.75801012600001));
#269563=CARTESIAN_POINT('Ctrl Pts',(-10.9376767320001,15.2,-2.75743358500002));
#269564=CARTESIAN_POINT('Ctrl Pts',(-10.9411536590001,15.2,-2.75685355800002));
#269565=CARTESIAN_POINT('Ctrl Pts',(-10.9446347860001,15.2,-2.75627004100001));
#269566=CARTESIAN_POINT('Ctrl Pts',(-10.9481201050001,15.2,-2.75568302700002));
#269567=CARTESIAN_POINT('Ctrl Pts',(-10.9516096070001,15.2,-2.75509251400001));
#269568=CARTESIAN_POINT('Ctrl Pts',(-10.9551032830001,15.2,-2.75449849500002));
#269569=CARTESIAN_POINT('Ctrl Pts',(-10.9586011260001,15.2,-2.75390096500002));
#269570=CARTESIAN_POINT('Ctrl Pts',(-10.9621031260001,15.2,-2.75329992100001));
#269571=CARTESIAN_POINT('Ctrl Pts',(-10.9656092750001,15.2,-2.75269535800001));
#269572=CARTESIAN_POINT('Ctrl Pts',(-10.9691195640001,15.2,-2.75208727000001));
#269573=CARTESIAN_POINT('Ctrl Pts',(-10.9726339840001,15.2,-2.75147565300002));
#269574=CARTESIAN_POINT('Ctrl Pts',(-10.9761525290001,15.2,-2.75086050400001));
#269575=CARTESIAN_POINT('Ctrl Pts',(-10.9796751870001,15.2,-2.75024181600001));
#269576=CARTESIAN_POINT('Ctrl Pts',(-10.9832019520001,15.2,-2.74961958600001));
#269577=CARTESIAN_POINT('Ctrl Pts',(-10.9867328140001,15.2,-2.74899380700001));
#269578=CARTESIAN_POINT('Ctrl Pts',(-10.9902677660001,15.2,-2.74836447800002));
#269579=CARTESIAN_POINT('Ctrl Pts',(-10.9938067980001,15.2,-2.74773159100001));
#269580=CARTESIAN_POINT('Ctrl Pts',(-10.9973499030001,15.2,-2.74709514500001));
#269581=CARTESIAN_POINT('Ctrl Pts',(-11.0008970700001,15.2,-2.74645513200001));
#269582=CARTESIAN_POINT('Ctrl Pts',(-11.0044482940001,15.2,-2.74581155000002));
#269583=CARTESIAN_POINT('Ctrl Pts',(-11.0080035640001,15.2,-2.74516439200001));
#269584=CARTESIAN_POINT('Ctrl Pts',(-11.0115628720001,15.2,-2.74451365600001));
#269585=CARTESIAN_POINT('Ctrl Pts',(-11.0151262110001,15.2,-2.74385933600001));
#269586=CARTESIAN_POINT('Ctrl Pts',(-11.0186935710001,15.2,-2.74320142800001));
#269587=CARTESIAN_POINT('Ctrl Pts',(-11.0222649450001,15.2,-2.74253992800002));
#269588=CARTESIAN_POINT('Ctrl Pts',(-11.0258403220001,15.2,-2.74187483000001));
#269589=CARTESIAN_POINT('Ctrl Pts',(-11.0294196970001,15.2,-2.74120613200001));
#269590=CARTESIAN_POINT('Ctrl Pts',(-11.0330030590001,15.2,-2.74053382800002));
#269591=CARTESIAN_POINT('Ctrl Pts',(-11.0365904010001,15.2,-2.73985791400001));
#269592=CARTESIAN_POINT('Ctrl Pts',(-11.0401817150001,15.2,-2.73917838500001));
#269593=CARTESIAN_POINT('Ctrl Pts',(-11.0437769920001,15.2,-2.73849523700001));
#269594=CARTESIAN_POINT('Ctrl Pts',(-11.0473762230001,15.2,-2.73780846600001));
#269595=CARTESIAN_POINT('Ctrl Pts',(-11.0509794010001,15.2,-2.73711806700002));
#269596=CARTESIAN_POINT('Ctrl Pts',(-11.0545865170001,15.2,-2.73642403700002));
#269597=CARTESIAN_POINT('Ctrl Pts',(-11.0581975630001,15.2,-2.73572637000001));
#269598=CARTESIAN_POINT('Ctrl Pts',(-11.0618125300001,15.2,-2.73502506300002));
#269599=CARTESIAN_POINT('Ctrl Pts',(-11.0654314110001,15.2,-2.73432011200001));
#269600=CARTESIAN_POINT('Ctrl Pts',(-11.0690541960001,15.2,-2.73361151100001));
#269601=CARTESIAN_POINT('Ctrl Pts',(-11.0726808780001,15.2,-2.73289925600002));
#269602=CARTESIAN_POINT('Ctrl Pts',(-11.0763114490001,15.2,-2.73218334500001));
#269603=CARTESIAN_POINT('Ctrl Pts',(-11.0799458990001,15.2,-2.73146377200002));
#269604=CARTESIAN_POINT('Ctrl Pts',(-11.0835842240001,15.2,-2.73074053200002));
#269605=CARTESIAN_POINT('Ctrl Pts',(-11.0872264110001,15.2,-2.73001362300001));
#269606=CARTESIAN_POINT('Ctrl Pts',(-11.0908724560001,15.2,-2.72928304000001));
#269607=CARTESIAN_POINT('Ctrl Pts',(-11.0945223470001,15.2,-2.72854877900001));
#269608=CARTESIAN_POINT('Ctrl Pts',(-11.0981760790001,15.2,-2.72781083400002));
#269609=CARTESIAN_POINT('Ctrl Pts',(-11.1018336410001,15.2,-2.72706920300001));
#269610=CARTESIAN_POINT('Ctrl Pts',(-11.1054950240001,15.2,-2.72632388100002));
#269611=CARTESIAN_POINT('Ctrl Pts',(-11.1091602230001,15.2,-2.72557486300002));
#269612=CARTESIAN_POINT('Ctrl Pts',(-11.1128292270001,15.2,-2.72482214500001));
#269613=CARTESIAN_POINT('Ctrl Pts',(-11.1165020290001,15.2,-2.72406572300001));
#269614=CARTESIAN_POINT('Ctrl Pts',(-11.1201786230001,15.2,-2.72330559600002));
#269615=CARTESIAN_POINT('Ctrl Pts',(-11.1238590000001,15.2,-2.72254175700001));
#269616=CARTESIAN_POINT('Ctrl Pts',(-11.1275431540001,15.2,-2.72177420400002));
#269617=CARTESIAN_POINT('Ctrl Pts',(-11.1312310760001,15.2,-2.72100293300001));
#269618=CARTESIAN_POINT('Ctrl Pts',(-11.1349227590001,15.2,-2.72022793900002));
#269619=CARTESIAN_POINT('Ctrl Pts',(-11.1386181920001,15.2,-2.71944921800001));
#269620=CARTESIAN_POINT('Ctrl Pts',(-11.1423173660001,15.2,-2.71866676600002));
#269621=CARTESIAN_POINT('Ctrl Pts',(-11.1460202710001,15.2,-2.71788057600002));
#269622=CARTESIAN_POINT('Ctrl Pts',(-11.1497268980001,15.2,-2.71709064400001));
#269623=CARTESIAN_POINT('Ctrl Pts',(-11.1534372360001,15.2,-2.71629696600002));
#269624=CARTESIAN_POINT('Ctrl Pts',(-11.1571512810001,15.2,-2.71549953800001));
#269625=CARTESIAN_POINT('Ctrl Pts',(-11.1608690250001,15.2,-2.71469835800001));
#269626=CARTESIAN_POINT('Ctrl Pts',(-11.1645904650001,15.2,-2.71389342400001));
#269627=CARTESIAN_POINT('Ctrl Pts',(-11.1683155990001,15.2,-2.71308473500001));
#269628=CARTESIAN_POINT('Ctrl Pts',(-11.1712986600001,15.2,-2.71243478000001));
#269629=CARTESIAN_POINT('Ctrl Pts',(-11.1735376180001,15.2,-2.71194562400002));
#269630=CARTESIAN_POINT('Ctrl Pts',(-11.1750309950001,15.2,-2.71161876900001));
#269631=CARTESIAN_POINT('Ctrl Pts',(-11.1757778680001,15.2,-2.71145515300002));
#269632=CARTESIAN_POINT('Origin',(-5.66257110645729E-14,15.2,-1.77635683940025E-14));
#269633=CARTESIAN_POINT('',(-9.86852965800006,15.2,-3.20199116200001));
#269634=CARTESIAN_POINT('',(-9.86852965800006,12.2,-3.20199116200001));
#269635=CARTESIAN_POINT('',(-9.86852965800006,15.2,-3.20199116200001));
#269636=CARTESIAN_POINT('Origin',(-5.66257110645729E-14,12.2,-1.77635683940025E-14));
#269637=CARTESIAN_POINT('Origin',(-5.66257110645729E-14,15.2,-1.77635683940025E-14));
#269638=CARTESIAN_POINT('Origin',(-5.66257110645729E-14,15.2,-1.77635683940025E-14));
#269639=CARTESIAN_POINT('',(-10.8127719254279,15.2,-3.91586047903425));
#269640=CARTESIAN_POINT('',(-10.6761442620001,15.2,-4.27433546900001));
#269641=CARTESIAN_POINT('Origin',(-5.66257110645729E-14,15.2,-1.77635683940025E-14));
#269642=CARTESIAN_POINT('',(-10.6761442620001,12.2,-4.27433546900001));
#269643=CARTESIAN_POINT('',(-10.6761442620001,15.2,-4.27433546900001));
#269644=CARTESIAN_POINT('',(-10.8127719250001,12.2,-3.91586047900002));
#269645=CARTESIAN_POINT('Origin',(-5.66257110645729E-14,12.2,-1.77635683940025E-14));
#269646=CARTESIAN_POINT('',(-10.8127719250001,15.2,-3.91586047900002));
#269647=CARTESIAN_POINT('Ctrl Pts',(-10.6761442620001,15.2,-4.27433546900001));
#269648=CARTESIAN_POINT('Ctrl Pts',(-10.6761442620001,11.6,-4.27433546900002));
#269649=CARTESIAN_POINT('Ctrl Pts',(-10.6753817060001,15.2,-4.27439112800001));
#269650=CARTESIAN_POINT('Ctrl Pts',(-10.6753817060001,11.6,-4.27439112800002));
#269651=CARTESIAN_POINT('Ctrl Pts',(-10.6738570140001,15.2,-4.27450212700001));
#269652=CARTESIAN_POINT('Ctrl Pts',(-10.6738570140001,11.6,-4.27450212700002));
#269653=CARTESIAN_POINT('Ctrl Pts',(-10.6715712310001,15.2,-4.27466766700002));
#269654=CARTESIAN_POINT('Ctrl Pts',(-10.6715712310001,11.6,-4.27466766700002));
#269655=CARTESIAN_POINT('Ctrl Pts',(-10.6685260340001,15.2,-4.27488647300001));
#269656=CARTESIAN_POINT('Ctrl Pts',(-10.6685260340001,11.6,-4.27488647300002));
#269657=CARTESIAN_POINT('Ctrl Pts',(-10.6647237270001,15.2,-4.27515678900001));
#269658=CARTESIAN_POINT('Ctrl Pts',(-10.6647237270001,11.6,-4.27515678900001));
#269659=CARTESIAN_POINT('Ctrl Pts',(-10.6609256130001,15.2,-4.27542391400001));
#269660=CARTESIAN_POINT('Ctrl Pts',(-10.6609256130001,11.6,-4.27542391400001));
#269661=CARTESIAN_POINT('Ctrl Pts',(-10.6571316910001,15.2,-4.27568784800001));
#269662=CARTESIAN_POINT('Ctrl Pts',(-10.6571316910001,11.6,-4.27568784800001));
#269663=CARTESIAN_POINT('Ctrl Pts',(-10.6533419640001,15.2,-4.27594859600001));
#269664=CARTESIAN_POINT('Ctrl Pts',(-10.6533419640001,11.6,-4.27594859600002));
#269665=CARTESIAN_POINT('Ctrl Pts',(-10.6495564390001,15.2,-4.27620616000001));
#269666=CARTESIAN_POINT('Ctrl Pts',(-10.6495564390001,11.6,-4.27620616000001));
#269667=CARTESIAN_POINT('Ctrl Pts',(-10.6457751210001,15.2,-4.27646054300002));
#269668=CARTESIAN_POINT('Ctrl Pts',(-10.6457751210001,11.6,-4.27646054300002));
#269669=CARTESIAN_POINT('Ctrl Pts',(-10.6419980200001,15.2,-4.27671175200001));
#269670=CARTESIAN_POINT('Ctrl Pts',(-10.6419980200001,11.6,-4.27671175200001));
#269671=CARTESIAN_POINT('Ctrl Pts',(-10.6382251440001,15.2,-4.27695979300001));
#269672=CARTESIAN_POINT('Ctrl Pts',(-10.6382251440001,11.6,-4.27695979300002));
#269673=CARTESIAN_POINT('Ctrl Pts',(-10.6344565010001,15.2,-4.27720467200002));
#269674=CARTESIAN_POINT('Ctrl Pts',(-10.6344565010001,11.6,-4.27720467200002));
#269675=CARTESIAN_POINT('Ctrl Pts',(-10.6306921010001,15.2,-4.27744639700002));
#269676=CARTESIAN_POINT('Ctrl Pts',(-10.6306921010001,11.6,-4.27744639700002));
#269677=CARTESIAN_POINT('Ctrl Pts',(-10.6269319530001,15.2,-4.27768497100002));
#269678=CARTESIAN_POINT('Ctrl Pts',(-10.6269319530001,11.6,-4.27768497100002));
#269679=CARTESIAN_POINT('Ctrl Pts',(-10.6231760650001,15.2,-4.27792040200002));
#269680=CARTESIAN_POINT('Ctrl Pts',(-10.6231760650001,11.6,-4.27792040200002));
#269681=CARTESIAN_POINT('Ctrl Pts',(-10.6194244440001,15.2,-4.27815269400002));
#269682=CARTESIAN_POINT('Ctrl Pts',(-10.6194244440001,11.6,-4.27815269400002));
#269683=CARTESIAN_POINT('Ctrl Pts',(-10.6156770940001,15.2,-4.27838185100001));
#269684=CARTESIAN_POINT('Ctrl Pts',(-10.6156770940001,11.6,-4.27838185100002));
#269685=CARTESIAN_POINT('Ctrl Pts',(-10.6119340260001,15.2,-4.27860787900002));
#269686=CARTESIAN_POINT('Ctrl Pts',(-10.6119340260001,11.6,-4.27860787900002));
#269687=CARTESIAN_POINT('Ctrl Pts',(-10.6081952440001,15.2,-4.27883078100002));
#269688=CARTESIAN_POINT('Ctrl Pts',(-10.6081952440001,11.6,-4.27883078100002));
#269689=CARTESIAN_POINT('Ctrl Pts',(-10.6044607560001,15.2,-4.27905056300002));
#269690=CARTESIAN_POINT('Ctrl Pts',(-10.6044607560001,11.6,-4.27905056300002));
#269691=CARTESIAN_POINT('Ctrl Pts',(-10.6007305690001,15.2,-4.27926723000001));
#269692=CARTESIAN_POINT('Ctrl Pts',(-10.6007305690001,11.6,-4.27926723000002));
#269693=CARTESIAN_POINT('Ctrl Pts',(-10.5970046900001,15.2,-4.27948078700001));
#269694=CARTESIAN_POINT('Ctrl Pts',(-10.5970046900001,11.6,-4.27948078700001));
#269695=CARTESIAN_POINT('Ctrl Pts',(-10.5932831290001,15.2,-4.27969124000001));
#269696=CARTESIAN_POINT('Ctrl Pts',(-10.5932831290001,11.6,-4.27969124000002));
#269697=CARTESIAN_POINT('Ctrl Pts',(-10.5895658910001,15.2,-4.27989859400002));
#269698=CARTESIAN_POINT('Ctrl Pts',(-10.5895658910001,11.6,-4.27989859400002));
#269699=CARTESIAN_POINT('Ctrl Pts',(-10.5858529860001,15.2,-4.28010285500001));
#269700=CARTESIAN_POINT('Ctrl Pts',(-10.5858529860001,11.6,-4.28010285500002));
#269701=CARTESIAN_POINT('Ctrl Pts',(-10.5821444200001,15.2,-4.28030402700001));
#269702=CARTESIAN_POINT('Ctrl Pts',(-10.5821444200001,11.6,-4.28030402700002));
#269703=CARTESIAN_POINT('Ctrl Pts',(-10.5784402020001,15.2,-4.28050211700001));
#269704=CARTESIAN_POINT('Ctrl Pts',(-10.5784402020001,11.6,-4.28050211700001));
#269705=CARTESIAN_POINT('Ctrl Pts',(-10.5747403380001,15.2,-4.28069713100002));
#269706=CARTESIAN_POINT('Ctrl Pts',(-10.5747403380001,11.6,-4.28069713100002));
#269707=CARTESIAN_POINT('Ctrl Pts',(-10.5710448370001,15.2,-4.28088907100001));
#269708=CARTESIAN_POINT('Ctrl Pts',(-10.5710448370001,11.6,-4.28088907100001));
#269709=CARTESIAN_POINT('Ctrl Pts',(-10.5673537050001,15.2,-4.28107794500002));
#269710=CARTESIAN_POINT('Ctrl Pts',(-10.5673537050001,11.6,-4.28107794500002));
#269711=CARTESIAN_POINT('Ctrl Pts',(-10.5636669500001,15.2,-4.28126375800002));
#269712=CARTESIAN_POINT('Ctrl Pts',(-10.5636669500001,11.6,-4.28126375800002));
#269713=CARTESIAN_POINT('Ctrl Pts',(-10.5599845790001,15.2,-4.28144651300002));
#269714=CARTESIAN_POINT('Ctrl Pts',(-10.5599845790001,11.6,-4.28144651300002));
#269715=CARTESIAN_POINT('Ctrl Pts',(-10.5563066010001,15.2,-4.28162621800002));
#269716=CARTESIAN_POINT('Ctrl Pts',(-10.5563066010001,11.6,-4.28162621800002));
#269717=CARTESIAN_POINT('Ctrl Pts',(-10.5526330210001,15.2,-4.28180287800001));
#269718=CARTESIAN_POINT('Ctrl Pts',(-10.5526330210001,11.6,-4.28180287800001));
#269719=CARTESIAN_POINT('Ctrl Pts',(-10.5489638500001,15.2,-4.28197649800001));
#269720=CARTESIAN_POINT('Ctrl Pts',(-10.5489638500001,11.6,-4.28197649800001));
#269721=CARTESIAN_POINT('Ctrl Pts',(-10.5452990930001,15.2,-4.28214708400001));
#269722=CARTESIAN_POINT('Ctrl Pts',(-10.5452990930001,11.6,-4.28214708400002));
#269723=CARTESIAN_POINT('Ctrl Pts',(-10.5416387590001,15.2,-4.28231464000001));
#269724=CARTESIAN_POINT('Ctrl Pts',(-10.5416387590001,11.6,-4.28231464000001));
#269725=CARTESIAN_POINT('Ctrl Pts',(-10.5379828550001,15.2,-4.28247917300002));
#269726=CARTESIAN_POINT('Ctrl Pts',(-10.5379828550001,11.6,-4.28247917300002));
#269727=CARTESIAN_POINT('Ctrl Pts',(-10.5343313890001,15.2,-4.28264068800001));
#269728=CARTESIAN_POINT('Ctrl Pts',(-10.5343313890001,11.6,-4.28264068800001));
#269729=CARTESIAN_POINT('Ctrl Pts',(-10.5306843670001,15.2,-4.28279919100001));
#269730=CARTESIAN_POINT('Ctrl Pts',(-10.5306843670001,11.6,-4.28279919100001));
#269731=CARTESIAN_POINT('Ctrl Pts',(-10.5270418000001,15.2,-4.28295468600002));
#269732=CARTESIAN_POINT('Ctrl Pts',(-10.5270418000001,11.6,-4.28295468600002));
#269733=CARTESIAN_POINT('Ctrl Pts',(-10.5234036920001,15.2,-4.28310718100001));
#269734=CARTESIAN_POINT('Ctrl Pts',(-10.5234036920001,11.6,-4.28310718100002));
#269735=CARTESIAN_POINT('Ctrl Pts',(-10.5197700540001,15.2,-4.28325667900001));
#269736=CARTESIAN_POINT('Ctrl Pts',(-10.5197700540001,11.6,-4.28325667900001));
#269737=CARTESIAN_POINT('Ctrl Pts',(-10.5161408910001,15.2,-4.28340318700001));
#269738=CARTESIAN_POINT('Ctrl Pts',(-10.5161408910001,11.6,-4.28340318700002));
#269739=CARTESIAN_POINT('Ctrl Pts',(-10.5125162110001,15.2,-4.28354671000001));
#269740=CARTESIAN_POINT('Ctrl Pts',(-10.5125162110001,11.6,-4.28354671000002));
#269741=CARTESIAN_POINT('Ctrl Pts',(-10.5088960220001,15.2,-4.28368725300002));
#269742=CARTESIAN_POINT('Ctrl Pts',(-10.5088960220001,11.6,-4.28368725300002));
#269743=CARTESIAN_POINT('Ctrl Pts',(-10.5052803340001,15.2,-4.28382482400002));
#269744=CARTESIAN_POINT('Ctrl Pts',(-10.5052803340001,11.6,-4.28382482400002));
#269745=CARTESIAN_POINT('Ctrl Pts',(-10.5016691510001,15.2,-4.28395942600002));
#269746=CARTESIAN_POINT('Ctrl Pts',(-10.5016691510001,11.6,-4.28395942600002));
#269747=CARTESIAN_POINT('Ctrl Pts',(-10.4980624830001,15.2,-4.28409106600002));
#269748=CARTESIAN_POINT('Ctrl Pts',(-10.4980624830001,11.6,-4.28409106600002));
#269749=CARTESIAN_POINT('Ctrl Pts',(-10.4944603360001,15.2,-4.28421975000001));
#269750=CARTESIAN_POINT('Ctrl Pts',(-10.4944603360001,11.6,-4.28421975000001));
#269751=CARTESIAN_POINT('Ctrl Pts',(-10.4908627200001,15.2,-4.28434548200002));
#269752=CARTESIAN_POINT('Ctrl Pts',(-10.4908627200001,11.6,-4.28434548200002));
#269753=CARTESIAN_POINT('Ctrl Pts',(-10.4872696400001,15.2,-4.28446827000001));
#269754=CARTESIAN_POINT('Ctrl Pts',(-10.4872696400001,11.6,-4.28446827000002));
#269755=CARTESIAN_POINT('Ctrl Pts',(-10.4836811070001,15.2,-4.28458811800001));
#269756=CARTESIAN_POINT('Ctrl Pts',(-10.4836811070001,11.6,-4.28458811800002));
#269757=CARTESIAN_POINT('Ctrl Pts',(-10.4800971270001,15.2,-4.28470503200002));
#269758=CARTESIAN_POINT('Ctrl Pts',(-10.4800971270001,11.6,-4.28470503200002));
#269759=CARTESIAN_POINT('Ctrl Pts',(-10.4765177060001,15.2,-4.28481901800001));
#269760=CARTESIAN_POINT('Ctrl Pts',(-10.4765177060001,11.6,-4.28481901800002));
#269761=CARTESIAN_POINT('Ctrl Pts',(-10.4729428540001,15.2,-4.28493008200002));
#269762=CARTESIAN_POINT('Ctrl Pts',(-10.4729428540001,11.6,-4.28493008200002));
#269763=CARTESIAN_POINT('Ctrl Pts',(-10.4693725790001,15.2,-4.28503823000002));
#269764=CARTESIAN_POINT('Ctrl Pts',(-10.4693725790001,11.6,-4.28503823000002));
#269765=CARTESIAN_POINT('Ctrl Pts',(-10.4658068880001,15.2,-4.28514346700001));
#269766=CARTESIAN_POINT('Ctrl Pts',(-10.4658068880001,11.6,-4.28514346700002));
#269767=CARTESIAN_POINT('Ctrl Pts',(-10.4622457890001,15.2,-4.28524579800001));
#269768=CARTESIAN_POINT('Ctrl Pts',(-10.4622457890001,11.6,-4.28524579800001));
#269769=CARTESIAN_POINT('Ctrl Pts',(-10.4586892890001,15.2,-4.28534523100002));
#269770=CARTESIAN_POINT('Ctrl Pts',(-10.4586892890001,11.6,-4.28534523100002));
#269771=CARTESIAN_POINT('Ctrl Pts',(-10.4551373970001,15.2,-4.28544177200001));
#269772=CARTESIAN_POINT('Ctrl Pts',(-10.4551373970001,11.6,-4.28544177200001));
#269773=CARTESIAN_POINT('Ctrl Pts',(-10.4515901200001,15.2,-4.28553542300001));
#269774=CARTESIAN_POINT('Ctrl Pts',(-10.4515901200001,11.6,-4.28553542300001));
#269775=CARTESIAN_POINT('Ctrl Pts',(-10.4480474660001,15.2,-4.28562619500001));
#269776=CARTESIAN_POINT('Ctrl Pts',(-10.4480474660001,11.6,-4.28562619500001));
#269777=CARTESIAN_POINT('Ctrl Pts',(-10.4445094430001,15.2,-4.28571409000002));
#269778=CARTESIAN_POINT('Ctrl Pts',(-10.4445094430001,11.6,-4.28571409000002));
#269779=CARTESIAN_POINT('Ctrl Pts',(-10.4409760600001,15.2,-4.28579911600002));
#269780=CARTESIAN_POINT('Ctrl Pts',(-10.4409760600001,11.6,-4.28579911600002));
#269781=CARTESIAN_POINT('Ctrl Pts',(-10.4374473230001,15.2,-4.28588127800001));
#269782=CARTESIAN_POINT('Ctrl Pts',(-10.4374473230001,11.6,-4.28588127800001));
#269783=CARTESIAN_POINT('Ctrl Pts',(-10.4339232400001,15.2,-4.28596058300001));
#269784=CARTESIAN_POINT('Ctrl Pts',(-10.4339232400001,11.6,-4.28596058300002));
#269785=CARTESIAN_POINT('Ctrl Pts',(-10.4304038200001,15.2,-4.28603703500002));
#269786=CARTESIAN_POINT('Ctrl Pts',(-10.4304038200001,11.6,-4.28603703500002));
#269787=CARTESIAN_POINT('Ctrl Pts',(-10.4268890690001,15.2,-4.28611064100001));
#269788=CARTESIAN_POINT('Ctrl Pts',(-10.4268890690001,11.6,-4.28611064100001));
#269789=CARTESIAN_POINT('Ctrl Pts',(-10.4233789970001,15.2,-4.28618140900001));
#269790=CARTESIAN_POINT('Ctrl Pts',(-10.4233789970001,11.6,-4.28618140900001));
#269791=CARTESIAN_POINT('Ctrl Pts',(-10.4198736120001,15.2,-4.28624934200001));
#269792=CARTESIAN_POINT('Ctrl Pts',(-10.4198736120001,11.6,-4.28624934200002));
#269793=CARTESIAN_POINT('Ctrl Pts',(-10.4163729200001,15.2,-4.28631444700001));
#269794=CARTESIAN_POINT('Ctrl Pts',(-10.4163729200001,11.6,-4.28631444700002));
#269795=CARTESIAN_POINT('Ctrl Pts',(-10.4128769310001,15.2,-4.28637673200001));
#269796=CARTESIAN_POINT('Ctrl Pts',(-10.4128769310001,11.6,-4.28637673200001));
#269797=CARTESIAN_POINT('Ctrl Pts',(-10.4093856500001,15.2,-4.28643620000001));
#269798=CARTESIAN_POINT('Ctrl Pts',(-10.4093856500001,11.6,-4.28643620000001));
#269799=CARTESIAN_POINT('Ctrl Pts',(-10.4058990890001,15.2,-4.28649285900002));
#269800=CARTESIAN_POINT('Ctrl Pts',(-10.4058990890001,11.6,-4.28649285900002));
#269801=CARTESIAN_POINT('Ctrl Pts',(-10.4024172520001,15.2,-4.28654671400002));
#269802=CARTESIAN_POINT('Ctrl Pts',(-10.4024172520001,11.6,-4.28654671400002));
#269803=CARTESIAN_POINT('Ctrl Pts',(-10.3989401500001,15.2,-4.28659777200001));
#269804=CARTESIAN_POINT('Ctrl Pts',(-10.3989401500001,11.6,-4.28659777200001));
#269805=CARTESIAN_POINT('Ctrl Pts',(-10.3954677890001,15.2,-4.28664603900001));
#269806=CARTESIAN_POINT('Ctrl Pts',(-10.3954677890001,11.6,-4.28664603900002));
#269807=CARTESIAN_POINT('Ctrl Pts',(-10.3920001780001,15.2,-4.28669152100001));
#269808=CARTESIAN_POINT('Ctrl Pts',(-10.3920001780001,11.6,-4.28669152100001));
#269809=CARTESIAN_POINT('Ctrl Pts',(-10.3885373250001,15.2,-4.28673422400002));
#269810=CARTESIAN_POINT('Ctrl Pts',(-10.3885373250001,11.6,-4.28673422400002));
#269811=CARTESIAN_POINT('Ctrl Pts',(-10.3850792370001,15.2,-4.28677415500001));
#269812=CARTESIAN_POINT('Ctrl Pts',(-10.3850792370001,11.6,-4.28677415500002));
#269813=CARTESIAN_POINT('Ctrl Pts',(-10.3816259240001,15.2,-4.28681132000001));
#269814=CARTESIAN_POINT('Ctrl Pts',(-10.3816259240001,11.6,-4.28681132000001));
#269815=CARTESIAN_POINT('Ctrl Pts',(-10.3781773920001,15.2,-4.28684572300002));
#269816=CARTESIAN_POINT('Ctrl Pts',(-10.3781773920001,11.6,-4.28684572300002));
#269817=CARTESIAN_POINT('Ctrl Pts',(-10.3747336490001,15.2,-4.28687737300002));
#269818=CARTESIAN_POINT('Ctrl Pts',(-10.3747336490001,11.6,-4.28687737300002));
#269819=CARTESIAN_POINT('Ctrl Pts',(-10.3712947050001,15.2,-4.28690627600002));
#269820=CARTESIAN_POINT('Ctrl Pts',(-10.3712947050001,11.6,-4.28690627600002));
#269821=CARTESIAN_POINT('Ctrl Pts',(-10.3678605660001,15.2,-4.28693243800002));
#269822=CARTESIAN_POINT('Ctrl Pts',(-10.3678605660001,11.6,-4.28693243800002));
#269823=CARTESIAN_POINT('Ctrl Pts',(-10.3644312410001,15.2,-4.28695586400002));
#269824=CARTESIAN_POINT('Ctrl Pts',(-10.3644312410001,11.6,-4.28695586400002));
#269825=CARTESIAN_POINT('Ctrl Pts',(-10.3610067390001,15.2,-4.28697656100002));
#269826=CARTESIAN_POINT('Ctrl Pts',(-10.3610067390001,11.6,-4.28697656100002));
#269827=CARTESIAN_POINT('Ctrl Pts',(-10.3575870660001,15.2,-4.28699453700002));
#269828=CARTESIAN_POINT('Ctrl Pts',(-10.3575870660001,11.6,-4.28699453700002));
#269829=CARTESIAN_POINT('Ctrl Pts',(-10.3541722320001,15.2,-4.28700979600002));
#269830=CARTESIAN_POINT('Ctrl Pts',(-10.3541722320001,11.6,-4.28700979600002));
#269831=CARTESIAN_POINT('Ctrl Pts',(-10.3507622440001,15.2,-4.28702234500001));
#269832=CARTESIAN_POINT('Ctrl Pts',(-10.3507622440001,11.6,-4.28702234500001));
#269833=CARTESIAN_POINT('Ctrl Pts',(-10.3473571110001,15.2,-4.28703219200001));
#269834=CARTESIAN_POINT('Ctrl Pts',(-10.3473571110001,11.6,-4.28703219200001));
#269835=CARTESIAN_POINT('Ctrl Pts',(-10.3439568400001,15.2,-4.28703934200001));
#269836=CARTESIAN_POINT('Ctrl Pts',(-10.3439568400001,11.6,-4.28703934200002));
#269837=CARTESIAN_POINT('Ctrl Pts',(-10.3405614400001,15.2,-4.28704380100001));
#269838=CARTESIAN_POINT('Ctrl Pts',(-10.3405614400001,11.6,-4.28704380100002));
#269839=CARTESIAN_POINT('Ctrl Pts',(-10.3371709180001,15.2,-4.28704557600001));
#269840=CARTESIAN_POINT('Ctrl Pts',(-10.3371709180001,11.6,-4.28704557600002));
#269841=CARTESIAN_POINT('Ctrl Pts',(-10.3337852840001,15.2,-4.28704467400001));
#269842=CARTESIAN_POINT('Ctrl Pts',(-10.3337852840001,11.6,-4.28704467400001));
#269843=CARTESIAN_POINT('Ctrl Pts',(-10.3304045450001,15.2,-4.28704110100002));
#269844=CARTESIAN_POINT('Ctrl Pts',(-10.3304045450001,11.6,-4.28704110100002));
#269845=CARTESIAN_POINT('Ctrl Pts',(-10.3270287090001,15.2,-4.28703486400002));
#269846=CARTESIAN_POINT('Ctrl Pts',(-10.3270287090001,11.6,-4.28703486400002));
#269847=CARTESIAN_POINT('Ctrl Pts',(-10.3236577850001,15.2,-4.28702596900001));
#269848=CARTESIAN_POINT('Ctrl Pts',(-10.3236577850001,11.6,-4.28702596900001));
#269849=CARTESIAN_POINT('Ctrl Pts',(-10.3202917800001,15.2,-4.28701442200001));
#269850=CARTESIAN_POINT('Ctrl Pts',(-10.3202917800001,11.6,-4.28701442200001));
#269851=CARTESIAN_POINT('Ctrl Pts',(-10.3169307040001,15.2,-4.28700023100001));
#269852=CARTESIAN_POINT('Ctrl Pts',(-10.3169307040001,11.6,-4.28700023100001));
#269853=CARTESIAN_POINT('Ctrl Pts',(-10.3135745630001,15.2,-4.28698340100001));
#269854=CARTESIAN_POINT('Ctrl Pts',(-10.3135745630001,11.6,-4.28698340100001));
#269855=CARTESIAN_POINT('Ctrl Pts',(-10.3102233670001,15.2,-4.28696394000001));
#269856=CARTESIAN_POINT('Ctrl Pts',(-10.3102233670001,11.6,-4.28696394000002));
#269857=CARTESIAN_POINT('Ctrl Pts',(-10.3068771240001,15.2,-4.28694185400001));
#269858=CARTESIAN_POINT('Ctrl Pts',(-10.3068771240001,11.6,-4.28694185400001));
#269859=CARTESIAN_POINT('Ctrl Pts',(-10.3035358420001,15.2,-4.28691715000001));
#269860=CARTESIAN_POINT('Ctrl Pts',(-10.3035358420001,11.6,-4.28691715000001));
#269861=CARTESIAN_POINT('Ctrl Pts',(-10.3001995280001,15.2,-4.28688983400002));
#269862=CARTESIAN_POINT('Ctrl Pts',(-10.3001995280001,11.6,-4.28688983400002));
#269863=CARTESIAN_POINT('Ctrl Pts',(-10.2968681930001,15.2,-4.28685991300001));
#269864=CARTESIAN_POINT('Ctrl Pts',(-10.2968681930001,11.6,-4.28685991300001));
#269865=CARTESIAN_POINT('Ctrl Pts',(-10.2935418440001,15.2,-4.28682739500001));
#269866=CARTESIAN_POINT('Ctrl Pts',(-10.2935418440001,11.6,-4.28682739500002));
#269867=CARTESIAN_POINT('Ctrl Pts',(-10.2902204880001,15.2,-4.28679228400001));
#269868=CARTESIAN_POINT('Ctrl Pts',(-10.2902204880001,11.6,-4.28679228400001));
#269869=CARTESIAN_POINT('Ctrl Pts',(-10.2869041340001,15.2,-4.28675458900001));
#269870=CARTESIAN_POINT('Ctrl Pts',(-10.2869041340001,11.6,-4.28675458900001));
#269871=CARTESIAN_POINT('Ctrl Pts',(-10.2835927920001,15.2,-4.28671431600002));
#269872=CARTESIAN_POINT('Ctrl Pts',(-10.2835927920001,11.6,-4.28671431600002));
#269873=CARTESIAN_POINT('Ctrl Pts',(-10.2802864670001,15.2,-4.28667147200001));
#269874=CARTESIAN_POINT('Ctrl Pts',(-10.2802864670001,11.6,-4.28667147200002));
#269875=CARTESIAN_POINT('Ctrl Pts',(-10.2769851700001,15.2,-4.28662606300001));
#269876=CARTESIAN_POINT('Ctrl Pts',(-10.2769851700001,11.6,-4.28662606300002));
#269877=CARTESIAN_POINT('Ctrl Pts',(-10.2736889100001,15.2,-4.28657809700002));
#269878=CARTESIAN_POINT('Ctrl Pts',(-10.2736889100001,11.6,-4.28657809700002));
#269879=CARTESIAN_POINT('Ctrl Pts',(-10.2703976930001,15.2,-4.28652758000001));
#269880=CARTESIAN_POINT('Ctrl Pts',(-10.2703976930001,11.6,-4.28652758000002));
#269881=CARTESIAN_POINT('Ctrl Pts',(-10.2671115300001,15.2,-4.28647452000002));
#269882=CARTESIAN_POINT('Ctrl Pts',(-10.2671115300001,11.6,-4.28647452000002));
#269883=CARTESIAN_POINT('Ctrl Pts',(-10.2638304270001,15.2,-4.28641892300002));
#269884=CARTESIAN_POINT('Ctrl Pts',(-10.2638304270001,11.6,-4.28641892300002));
#269885=CARTESIAN_POINT('Ctrl Pts',(-10.2605543930001,15.2,-4.28636079400002));
#269886=CARTESIAN_POINT('Ctrl Pts',(-10.2605543930001,11.6,-4.28636079400002));
#269887=CARTESIAN_POINT('Ctrl Pts',(-10.2572834360001,15.2,-4.28630014400001));
#269888=CARTESIAN_POINT('Ctrl Pts',(-10.2572834360001,11.6,-4.28630014400001));
#269889=CARTESIAN_POINT('Ctrl Pts',(-10.2540175660001,15.2,-4.28623697700001));
#269890=CARTESIAN_POINT('Ctrl Pts',(-10.2540175660001,11.6,-4.28623697700001));
#269891=CARTESIAN_POINT('Ctrl Pts',(-10.2507567900001,15.2,-4.28617130100001));
#269892=CARTESIAN_POINT('Ctrl Pts',(-10.2507567900001,11.6,-4.28617130100002));
#269893=CARTESIAN_POINT('Ctrl Pts',(-10.2475011180001,15.2,-4.28610312300002));
#269894=CARTESIAN_POINT('Ctrl Pts',(-10.2475011180001,11.6,-4.28610312300002));
#269895=CARTESIAN_POINT('Ctrl Pts',(-10.2442505560001,15.2,-4.28603245000001));
#269896=CARTESIAN_POINT('Ctrl Pts',(-10.2442505560001,11.6,-4.28603245000002));
#269897=CARTESIAN_POINT('Ctrl Pts',(-10.2410051150001,15.2,-4.28595928900001));
#269898=CARTESIAN_POINT('Ctrl Pts',(-10.2410051150001,11.6,-4.28595928900002));
#269899=CARTESIAN_POINT('Ctrl Pts',(-10.2377648020001,15.2,-4.28588364700001));
#269900=CARTESIAN_POINT('Ctrl Pts',(-10.2377648020001,11.6,-4.28588364700001));
#269901=CARTESIAN_POINT('Ctrl Pts',(-10.2345296260001,15.2,-4.28580553000002));
#269902=CARTESIAN_POINT('Ctrl Pts',(-10.2345296260001,11.6,-4.28580553000002));
#269903=CARTESIAN_POINT('Ctrl Pts',(-10.2312995950001,15.2,-4.28572494700001));
#269904=CARTESIAN_POINT('Ctrl Pts',(-10.2312995950001,11.6,-4.28572494700001));
#269905=CARTESIAN_POINT('Ctrl Pts',(-10.2280747180001,15.2,-4.28564190400001));
#269906=CARTESIAN_POINT('Ctrl Pts',(-10.2280747180001,11.6,-4.28564190400001));
#269907=CARTESIAN_POINT('Ctrl Pts',(-10.2248550040001,15.2,-4.28555640900001));
#269908=CARTESIAN_POINT('Ctrl Pts',(-10.2248550040001,11.6,-4.28555640900001));
#269909=CARTESIAN_POINT('Ctrl Pts',(-10.2216404610001,15.2,-4.28546846800002));
#269910=CARTESIAN_POINT('Ctrl Pts',(-10.2216404610001,11.6,-4.28546846800002));
#269911=CARTESIAN_POINT('Ctrl Pts',(-10.2184310970001,15.2,-4.28537808900002));
#269912=CARTESIAN_POINT('Ctrl Pts',(-10.2184310970001,11.6,-4.28537808900002));
#269913=CARTESIAN_POINT('Ctrl Pts',(-10.2152269210001,15.2,-4.28528527800002));
#269914=CARTESIAN_POINT('Ctrl Pts',(-10.2152269210001,11.6,-4.28528527800002));
#269915=CARTESIAN_POINT('Ctrl Pts',(-10.2120279420001,15.2,-4.28519004500002));
#269916=CARTESIAN_POINT('Ctrl Pts',(-10.2120279420001,11.6,-4.28519004500002));
#269917=CARTESIAN_POINT('Ctrl Pts',(-10.2088341690001,15.2,-4.28509239400002));
#269918=CARTESIAN_POINT('Ctrl Pts',(-10.2088341690001,11.6,-4.28509239400002));
#269919=CARTESIAN_POINT('Ctrl Pts',(-10.2056456080001,15.2,-4.28499233500002));
#269920=CARTESIAN_POINT('Ctrl Pts',(-10.2056456080001,11.6,-4.28499233500002));
#269921=CARTESIAN_POINT('Ctrl Pts',(-10.2024622710001,15.2,-4.28488987200002));
#269922=CARTESIAN_POINT('Ctrl Pts',(-10.2024622710001,11.6,-4.28488987200002));
#269923=CARTESIAN_POINT('Ctrl Pts',(-10.1992841650001,15.2,-4.28478501600001));
#269924=CARTESIAN_POINT('Ctrl Pts',(-10.1992841650001,11.6,-4.28478501600001));
#269925=CARTESIAN_POINT('Ctrl Pts',(-10.1961112980001,15.2,-4.28467777200002));
#269926=CARTESIAN_POINT('Ctrl Pts',(-10.1961112980001,11.6,-4.28467777200002));
#269927=CARTESIAN_POINT('Ctrl Pts',(-10.1929436800001,15.2,-4.28456814900001));
#269928=CARTESIAN_POINT('Ctrl Pts',(-10.1929436800001,11.6,-4.28456814900002));
#269929=CARTESIAN_POINT('Ctrl Pts',(-10.1897813190001,15.2,-4.28445615300001));
#269930=CARTESIAN_POINT('Ctrl Pts',(-10.1897813190001,11.6,-4.28445615300001));
#269931=CARTESIAN_POINT('Ctrl Pts',(-10.1866242240001,15.2,-4.28434179100002));
#269932=CARTESIAN_POINT('Ctrl Pts',(-10.1866242240001,11.6,-4.28434179100002));
#269933=CARTESIAN_POINT('Ctrl Pts',(-10.1834724030001,15.2,-4.28422507100001));
#269934=CARTESIAN_POINT('Ctrl Pts',(-10.1834724030001,11.6,-4.28422507100001));
#269935=CARTESIAN_POINT('Ctrl Pts',(-10.1803258660001,15.2,-4.28410600200001));
#269936=CARTESIAN_POINT('Ctrl Pts',(-10.1803258660001,11.6,-4.28410600200001));
#269937=CARTESIAN_POINT('Ctrl Pts',(-10.1771846200001,15.2,-4.28398458900002));
#269938=CARTESIAN_POINT('Ctrl Pts',(-10.1771846200001,11.6,-4.28398458900002));
#269939=CARTESIAN_POINT('Ctrl Pts',(-10.1740486750001,15.2,-4.28386084200001));
#269940=CARTESIAN_POINT('Ctrl Pts',(-10.1740486750001,11.6,-4.28386084200001));
#269941=CARTESIAN_POINT('Ctrl Pts',(-10.1709180390001,15.2,-4.28373476600001));
#269942=CARTESIAN_POINT('Ctrl Pts',(-10.1709180390001,11.6,-4.28373476600001));
#269943=CARTESIAN_POINT('Ctrl Pts',(-10.1677927210001,15.2,-4.28360637000001));
#269944=CARTESIAN_POINT('Ctrl Pts',(-10.1677927210001,11.6,-4.28360637000001));
#269945=CARTESIAN_POINT('Ctrl Pts',(-10.1646727300001,15.2,-4.28347566200001));
#269946=CARTESIAN_POINT('Ctrl Pts',(-10.1646727300001,11.6,-4.28347566200001));
#269947=CARTESIAN_POINT('Ctrl Pts',(-10.1615580750001,15.2,-4.28334264800001));
#269948=CARTESIAN_POINT('Ctrl Pts',(-10.1615580750001,11.6,-4.28334264800002));
#269949=CARTESIAN_POINT('Ctrl Pts',(-10.1584487640001,15.2,-4.28320733700001));
#269950=CARTESIAN_POINT('Ctrl Pts',(-10.1584487640001,11.6,-4.28320733700002));
#269951=CARTESIAN_POINT('Ctrl Pts',(-10.1553448070001,15.2,-4.28306973600002));
#269952=CARTESIAN_POINT('Ctrl Pts',(-10.1553448070001,11.6,-4.28306973600002));
#269953=CARTESIAN_POINT('Ctrl Pts',(-10.1522462110001,15.2,-4.28292985300001));
#269954=CARTESIAN_POINT('Ctrl Pts',(-10.1522462110001,11.6,-4.28292985300002));
#269955=CARTESIAN_POINT('Ctrl Pts',(-10.1491529860001,15.2,-4.28278769400002));
#269956=CARTESIAN_POINT('Ctrl Pts',(-10.1491529860001,11.6,-4.28278769400002));
#269957=CARTESIAN_POINT('Ctrl Pts',(-10.1460651410001,15.2,-4.28264327000001));
#269958=CARTESIAN_POINT('Ctrl Pts',(-10.1460651410001,11.6,-4.28264327000001));
#269959=CARTESIAN_POINT('Ctrl Pts',(-10.1429826850001,15.2,-4.28249658600001));
#269960=CARTESIAN_POINT('Ctrl Pts',(-10.1429826850001,11.6,-4.28249658600001));
#269961=CARTESIAN_POINT('Ctrl Pts',(-10.1399056260001,15.2,-4.28234765100001));
#269962=CARTESIAN_POINT('Ctrl Pts',(-10.1399056260001,11.6,-4.28234765100001));
#269963=CARTESIAN_POINT('Ctrl Pts',(-10.1368339730001,15.2,-4.28219647200001));
#269964=CARTESIAN_POINT('Ctrl Pts',(-10.1368339730001,11.6,-4.28219647200002));
#269965=CARTESIAN_POINT('Ctrl Pts',(-10.1337677360001,15.2,-4.28204305800001));
#269966=CARTESIAN_POINT('Ctrl Pts',(-10.1337677360001,11.6,-4.28204305800001));
#269967=CARTESIAN_POINT('Ctrl Pts',(-10.1307069230001,15.2,-4.28188741500001));
#269968=CARTESIAN_POINT('Ctrl Pts',(-10.1307069230001,11.6,-4.28188741500002));
#269969=CARTESIAN_POINT('Ctrl Pts',(-10.1276515430001,15.2,-4.28172955400001));
#269970=CARTESIAN_POINT('Ctrl Pts',(-10.1276515430001,11.6,-4.28172955400001));
#269971=CARTESIAN_POINT('Ctrl Pts',(-10.1246016050001,15.2,-4.28156947900002));
#269972=CARTESIAN_POINT('Ctrl Pts',(-10.1246016050001,11.6,-4.28156947900002));
#269973=CARTESIAN_POINT('Ctrl Pts',(-10.1215571180001,15.2,-4.28140719900002));
#269974=CARTESIAN_POINT('Ctrl Pts',(-10.1215571180001,11.6,-4.28140719900002));
#269975=CARTESIAN_POINT('Ctrl Pts',(-10.1185180900001,15.2,-4.28124272500002));
#269976=CARTESIAN_POINT('Ctrl Pts',(-10.1185180900001,11.6,-4.28124272500002));
#269977=CARTESIAN_POINT('Ctrl Pts',(-10.1154845320001,15.2,-4.28107606000002));
#269978=CARTESIAN_POINT('Ctrl Pts',(-10.1154845320001,11.6,-4.28107606000002));
#269979=CARTESIAN_POINT('Ctrl Pts',(-10.1124564520001,15.2,-4.28090721700002));
#269980=CARTESIAN_POINT('Ctrl Pts',(-10.1124564520001,11.6,-4.28090721700002));
#269981=CARTESIAN_POINT('Ctrl Pts',(-10.1094338590001,15.2,-4.28073619900001));
#269982=CARTESIAN_POINT('Ctrl Pts',(-10.1094338590001,11.6,-4.28073619900002));
#269983=CARTESIAN_POINT('Ctrl Pts',(-10.1064167610001,15.2,-4.28056301800002));
#269984=CARTESIAN_POINT('Ctrl Pts',(-10.1064167610001,11.6,-4.28056301800002));
#269985=CARTESIAN_POINT('Ctrl Pts',(-10.1034051690001,15.2,-4.28038768100001));
#269986=CARTESIAN_POINT('Ctrl Pts',(-10.1034051690001,11.6,-4.28038768100001));
#269987=CARTESIAN_POINT('Ctrl Pts',(-10.1003990900001,15.2,-4.28021019400001));
#269988=CARTESIAN_POINT('Ctrl Pts',(-10.1003990900001,11.6,-4.28021019400001));
#269989=CARTESIAN_POINT('Ctrl Pts',(-10.0973985350001,15.2,-4.28003056800002));
#269990=CARTESIAN_POINT('Ctrl Pts',(-10.0973985350001,11.6,-4.28003056800002));
#269991=CARTESIAN_POINT('Ctrl Pts',(-10.0944035120001,15.2,-4.27984881000001));
#269992=CARTESIAN_POINT('Ctrl Pts',(-10.0944035120001,11.6,-4.27984881000001));
#269993=CARTESIAN_POINT('Ctrl Pts',(-10.0914140300001,15.2,-4.27966492700001));
#269994=CARTESIAN_POINT('Ctrl Pts',(-10.0914140300001,11.6,-4.27966492700001));
#269995=CARTESIAN_POINT('Ctrl Pts',(-10.0884300980001,15.2,-4.27947892900002));
#269996=CARTESIAN_POINT('Ctrl Pts',(-10.0884300980001,11.6,-4.27947892900002));
#269997=CARTESIAN_POINT('Ctrl Pts',(-10.0854517260001,15.2,-4.27929082300002));
#269998=CARTESIAN_POINT('Ctrl Pts',(-10.0854517260001,11.6,-4.27929082300002));
#269999=CARTESIAN_POINT('Ctrl Pts',(-10.0824789230001,15.2,-4.27910061900001));
#270000=CARTESIAN_POINT('Ctrl Pts',(-10.0824789230001,11.6,-4.27910061900001));
#270001=CARTESIAN_POINT('Ctrl Pts',(-10.0795116980001,15.2,-4.27890832200001));
#270002=CARTESIAN_POINT('Ctrl Pts',(-10.0795116980001,11.6,-4.27890832200002));
#270003=CARTESIAN_POINT('Ctrl Pts',(-10.0765500590001,15.2,-4.27871394200002));
#270004=CARTESIAN_POINT('Ctrl Pts',(-10.0765500590001,11.6,-4.27871394200002));
#270005=CARTESIAN_POINT('Ctrl Pts',(-10.0735940170001,15.2,-4.27851748900002));
#270006=CARTESIAN_POINT('Ctrl Pts',(-10.0735940170001,11.6,-4.27851748900002));
#270007=CARTESIAN_POINT('Ctrl Pts',(-10.0706435790001,15.2,-4.27831896900001));
#270008=CARTESIAN_POINT('Ctrl Pts',(-10.0706435790001,11.6,-4.27831896900001));
#270009=CARTESIAN_POINT('Ctrl Pts',(-10.0676987560001,15.2,-4.27811839100002));
#270010=CARTESIAN_POINT('Ctrl Pts',(-10.0676987560001,11.6,-4.27811839100002));
#270011=CARTESIAN_POINT('Ctrl Pts',(-10.0647595580001,15.2,-4.27791576300002));
#270012=CARTESIAN_POINT('Ctrl Pts',(-10.0647595580001,11.6,-4.27791576300002));
#270013=CARTESIAN_POINT('Ctrl Pts',(-10.0618259920001,15.2,-4.27771109500001));
#270014=CARTESIAN_POINT('Ctrl Pts',(-10.0618259920001,11.6,-4.27771109500002));
#270015=CARTESIAN_POINT('Ctrl Pts',(-10.0588980670001,15.2,-4.27750439400001));
#270016=CARTESIAN_POINT('Ctrl Pts',(-10.0588980670001,11.6,-4.27750439400001));
#270017=CARTESIAN_POINT('Ctrl Pts',(-10.0559757960001,15.2,-4.27729566900001));
#270018=CARTESIAN_POINT('Ctrl Pts',(-10.0559757960001,11.6,-4.27729566900002));
#270019=CARTESIAN_POINT('Ctrl Pts',(-10.0530591850001,15.2,-4.27708492700001));
#270020=CARTESIAN_POINT('Ctrl Pts',(-10.0530591850001,11.6,-4.27708492700001));
#270021=CARTESIAN_POINT('Ctrl Pts',(-10.0501482430001,15.2,-4.27687217800001));
#270022=CARTESIAN_POINT('Ctrl Pts',(-10.0501482430001,11.6,-4.27687217800001));
#270023=CARTESIAN_POINT('Ctrl Pts',(-10.0472429820001,15.2,-4.27665743200001));
#270024=CARTESIAN_POINT('Ctrl Pts',(-10.0472429820001,11.6,-4.27665743200001));
#270025=CARTESIAN_POINT('Ctrl Pts',(-10.0443434090001,15.2,-4.27644069400001));
#270026=CARTESIAN_POINT('Ctrl Pts',(-10.0443434090001,11.6,-4.27644069400001));
#270027=CARTESIAN_POINT('Ctrl Pts',(-10.0414495340001,15.2,-4.27622197600002));
#270028=CARTESIAN_POINT('Ctrl Pts',(-10.0414495340001,11.6,-4.27622197600002));
#270029=CARTESIAN_POINT('Ctrl Pts',(-10.0385613660001,15.2,-4.27600128400002));
#270030=CARTESIAN_POINT('Ctrl Pts',(-10.0385613660001,11.6,-4.27600128400002));
#270031=CARTESIAN_POINT('Ctrl Pts',(-10.0356789150001,15.2,-4.27577862800002));
#270032=CARTESIAN_POINT('Ctrl Pts',(-10.0356789150001,11.6,-4.27577862800002));
#270033=CARTESIAN_POINT('Ctrl Pts',(-10.0328021910001,15.2,-4.27555401600001));
#270034=CARTESIAN_POINT('Ctrl Pts',(-10.0328021910001,11.6,-4.27555401600001));
#270035=CARTESIAN_POINT('Ctrl Pts',(-10.0299312030001,15.2,-4.27532745800002));
#270036=CARTESIAN_POINT('Ctrl Pts',(-10.0299312030001,11.6,-4.27532745800002));
#270037=CARTESIAN_POINT('Ctrl Pts',(-10.0270659590001,15.2,-4.27509896100001));
#270038=CARTESIAN_POINT('Ctrl Pts',(-10.0270659590001,11.6,-4.27509896100002));
#270039=CARTESIAN_POINT('Ctrl Pts',(-10.0242064700001,15.2,-4.27486853600001));
#270040=CARTESIAN_POINT('Ctrl Pts',(-10.0242064700001,11.6,-4.27486853600001));
#270041=CARTESIAN_POINT('Ctrl Pts',(-10.0213527440001,15.2,-4.27463618900001));
#270042=CARTESIAN_POINT('Ctrl Pts',(-10.0213527440001,11.6,-4.27463618900001));
#270043=CARTESIAN_POINT('Ctrl Pts',(-10.0185047920001,15.2,-4.27440193000002));
#270044=CARTESIAN_POINT('Ctrl Pts',(-10.0185047920001,11.6,-4.27440193000002));
#270045=CARTESIAN_POINT('Ctrl Pts',(-10.0156626230001,15.2,-4.27416576900002));
#270046=CARTESIAN_POINT('Ctrl Pts',(-10.0156626230001,11.6,-4.27416576900002));
#270047=CARTESIAN_POINT('Ctrl Pts',(-10.0128262460001,15.2,-4.27392771400001));
#270048=CARTESIAN_POINT('Ctrl Pts',(-10.0128262460001,11.6,-4.27392771400002));
#270049=CARTESIAN_POINT('Ctrl Pts',(-10.0099956720001,15.2,-4.27368777300002));
#270050=CARTESIAN_POINT('Ctrl Pts',(-10.0099956720001,11.6,-4.27368777300002));
#270051=CARTESIAN_POINT('Ctrl Pts',(-10.0071709090001,15.2,-4.27344595700001));
#270052=CARTESIAN_POINT('Ctrl Pts',(-10.0071709090001,11.6,-4.27344595700002));
#270053=CARTESIAN_POINT('Ctrl Pts',(-10.0043519670001,15.2,-4.27320227300001));
#270054=CARTESIAN_POINT('Ctrl Pts',(-10.0043519670001,11.6,-4.27320227300001));
#270055=CARTESIAN_POINT('Ctrl Pts',(-10.0015388550001,15.2,-4.27295673000001));
#270056=CARTESIAN_POINT('Ctrl Pts',(-10.0015388550001,11.6,-4.27295673000002));
#270057=CARTESIAN_POINT('Ctrl Pts',(-9.99873158400005,15.2,-4.27270933800001));
#270058=CARTESIAN_POINT('Ctrl Pts',(-9.99873158400005,11.6,-4.27270933800001));
#270059=CARTESIAN_POINT('Ctrl Pts',(-9.99593016200006,15.2,-4.27246010600001));
#270060=CARTESIAN_POINT('Ctrl Pts',(-9.99593016200006,11.6,-4.27246010600001));
#270061=CARTESIAN_POINT('Ctrl Pts',(-9.99313460000005,15.2,-4.27220904400002));
#270062=CARTESIAN_POINT('Ctrl Pts',(-9.99313460000005,11.6,-4.27220904400002));
#270063=CARTESIAN_POINT('Ctrl Pts',(-9.99034490700006,15.2,-4.27195615900001));
#270064=CARTESIAN_POINT('Ctrl Pts',(-9.99034490700006,11.6,-4.27195615900002));
#270065=CARTESIAN_POINT('Ctrl Pts',(-9.98756109300006,15.2,-4.27170146000002));
#270066=CARTESIAN_POINT('Ctrl Pts',(-9.98756109300006,11.6,-4.27170146000002));
#270067=CARTESIAN_POINT('Ctrl Pts',(-9.98478316600006,15.2,-4.27144495800002));
#270068=CARTESIAN_POINT('Ctrl Pts',(-9.98478316600006,11.6,-4.27144495800002));
#270069=CARTESIAN_POINT('Ctrl Pts',(-9.98201113900006,15.2,-4.27118666200001));
#270070=CARTESIAN_POINT('Ctrl Pts',(-9.98201113900006,11.6,-4.27118666200002));
#270071=CARTESIAN_POINT('Ctrl Pts',(-9.97924501800006,15.2,-4.27092658000001));
#270072=CARTESIAN_POINT('Ctrl Pts',(-9.97924501800006,11.6,-4.27092658000001));
#270073=CARTESIAN_POINT('Ctrl Pts',(-9.97648481500006,15.2,-4.27066472200002));
#270074=CARTESIAN_POINT('Ctrl Pts',(-9.97648481500006,11.6,-4.27066472200002));
#270075=CARTESIAN_POINT('Ctrl Pts',(-9.97373054000006,15.2,-4.27040109700001));
#270076=CARTESIAN_POINT('Ctrl Pts',(-9.97373054000006,11.6,-4.27040109700001));
#270077=CARTESIAN_POINT('Ctrl Pts',(-9.97098220100006,15.2,-4.27013571500002));
#270078=CARTESIAN_POINT('Ctrl Pts',(-9.97098220100006,11.6,-4.27013571500002));
#270079=CARTESIAN_POINT('Ctrl Pts',(-9.96823980900006,15.2,-4.26986858400001));
#270080=CARTESIAN_POINT('Ctrl Pts',(-9.96823980900006,11.6,-4.26986858400001));
#270081=CARTESIAN_POINT('Ctrl Pts',(-9.96550337400006,15.2,-4.26959971500001));
#270082=CARTESIAN_POINT('Ctrl Pts',(-9.96550337400006,11.6,-4.26959971500002));
#270083=CARTESIAN_POINT('Ctrl Pts',(-9.96277290400006,15.2,-4.26932911600002));
#270084=CARTESIAN_POINT('Ctrl Pts',(-9.96277290400006,11.6,-4.26932911600002));
#270085=CARTESIAN_POINT('Ctrl Pts',(-9.96004841100006,15.2,-4.26905679700001));
#270086=CARTESIAN_POINT('Ctrl Pts',(-9.96004841100006,11.6,-4.26905679700001));
#270087=CARTESIAN_POINT('Ctrl Pts',(-9.95732990400005,15.2,-4.26878276700001));
#270088=CARTESIAN_POINT('Ctrl Pts',(-9.95732990400005,11.6,-4.26878276700002));
#270089=CARTESIAN_POINT('Ctrl Pts',(-9.95461739200006,15.2,-4.26850703700001));
#270090=CARTESIAN_POINT('Ctrl Pts',(-9.95461739200006,11.6,-4.26850703700001));
#270091=CARTESIAN_POINT('Ctrl Pts',(-9.95191088700006,15.2,-4.26822961500001));
#270092=CARTESIAN_POINT('Ctrl Pts',(-9.95191088700006,11.6,-4.26822961500002));
#270093=CARTESIAN_POINT('Ctrl Pts',(-9.94921039800006,15.2,-4.26795051200001));
#270094=CARTESIAN_POINT('Ctrl Pts',(-9.94921039800006,11.6,-4.26795051200001));
#270095=CARTESIAN_POINT('Ctrl Pts',(-9.94651593300006,15.2,-4.26766973600001));
#270096=CARTESIAN_POINT('Ctrl Pts',(-9.94651593300006,11.6,-4.26766973600001));
#270097=CARTESIAN_POINT('Ctrl Pts',(-9.94382750400005,15.2,-4.26738729700002));
#270098=CARTESIAN_POINT('Ctrl Pts',(-9.94382750400005,11.6,-4.26738729700002));
#270099=CARTESIAN_POINT('Ctrl Pts',(-9.94114512000005,15.2,-4.26710320400002));
#270100=CARTESIAN_POINT('Ctrl Pts',(-9.94114512000005,11.6,-4.26710320400002));
#270101=CARTESIAN_POINT('Ctrl Pts',(-9.93846879200006,15.2,-4.26681746900002));
#270102=CARTESIAN_POINT('Ctrl Pts',(-9.93846879200006,11.6,-4.26681746900002));
#270103=CARTESIAN_POINT('Ctrl Pts',(-9.93579852900006,15.2,-4.26653010000001));
#270104=CARTESIAN_POINT('Ctrl Pts',(-9.93579852900006,11.6,-4.26653010000001));
#270105=CARTESIAN_POINT('Ctrl Pts',(-9.93313434200006,15.2,-4.26624110700002));
#270106=CARTESIAN_POINT('Ctrl Pts',(-9.93313434200006,11.6,-4.26624110700002));
#270107=CARTESIAN_POINT('Ctrl Pts',(-9.93047624000006,15.2,-4.26595050000001));
#270108=CARTESIAN_POINT('Ctrl Pts',(-9.93047624000006,11.6,-4.26595050000001));
#270109=CARTESIAN_POINT('Ctrl Pts',(-9.92782423400006,15.2,-4.26565828900001));
#270110=CARTESIAN_POINT('Ctrl Pts',(-9.92782423400006,11.6,-4.26565828900001));
#270111=CARTESIAN_POINT('Ctrl Pts',(-9.92517833200005,15.2,-4.26536448200002));
#270112=CARTESIAN_POINT('Ctrl Pts',(-9.92517833200005,11.6,-4.26536448200002));
#270113=CARTESIAN_POINT('Ctrl Pts',(-9.92253854700006,15.2,-4.26506909300001));
#270114=CARTESIAN_POINT('Ctrl Pts',(-9.92253854700006,11.6,-4.26506909300001));
#270115=CARTESIAN_POINT('Ctrl Pts',(-9.91990488700005,15.2,-4.26477212700001));
#270116=CARTESIAN_POINT('Ctrl Pts',(-9.91990488700005,11.6,-4.26477212700001));
#270117=CARTESIAN_POINT('Ctrl Pts',(-9.91727736300006,15.2,-4.26447359700001));
#270118=CARTESIAN_POINT('Ctrl Pts',(-9.91727736300006,11.6,-4.26447359700001));
#270119=CARTESIAN_POINT('Ctrl Pts',(-9.91465598400006,15.2,-4.26417351200001));
#270120=CARTESIAN_POINT('Ctrl Pts',(-9.91465598400006,11.6,-4.26417351200001));
#270121=CARTESIAN_POINT('Ctrl Pts',(-9.91204076300006,15.2,-4.26387188200001));
#270122=CARTESIAN_POINT('Ctrl Pts',(-9.91204076300006,11.6,-4.26387188200002));
#270123=CARTESIAN_POINT('Ctrl Pts',(-9.90943170700006,15.2,-4.26356871900001));
#270124=CARTESIAN_POINT('Ctrl Pts',(-9.90943170700006,11.6,-4.26356871900001));
#270125=CARTESIAN_POINT('Ctrl Pts',(-9.90682882700006,15.2,-4.26326402900001));
#270126=CARTESIAN_POINT('Ctrl Pts',(-9.90682882700006,11.6,-4.26326402900001));
#270127=CARTESIAN_POINT('Ctrl Pts',(-9.90423213500006,15.2,-4.26295782600001));
#270128=CARTESIAN_POINT('Ctrl Pts',(-9.90423213500006,11.6,-4.26295782600001));
#270129=CARTESIAN_POINT('Ctrl Pts',(-9.90164163800006,15.2,-4.26265011800002));
#270130=CARTESIAN_POINT('Ctrl Pts',(-9.90164163800006,11.6,-4.26265011800002));
#270131=CARTESIAN_POINT('Ctrl Pts',(-9.89905735000006,15.2,-4.26234091600001));
#270132=CARTESIAN_POINT('Ctrl Pts',(-9.89905735000006,11.6,-4.26234091600001));
#270133=CARTESIAN_POINT('Ctrl Pts',(-9.89647927900006,15.2,-4.26203023000001));
#270134=CARTESIAN_POINT('Ctrl Pts',(-9.89647927900006,11.6,-4.26203023000001));
#270135=CARTESIAN_POINT('Ctrl Pts',(-9.89390743400006,15.2,-4.26171807000001));
#270136=CARTESIAN_POINT('Ctrl Pts',(-9.89390743400006,11.6,-4.26171807000001));
#270137=CARTESIAN_POINT('Ctrl Pts',(-9.89134182900005,15.2,-4.26140444800001));
#270138=CARTESIAN_POINT('Ctrl Pts',(-9.89134182900005,11.6,-4.26140444800002));
#270139=CARTESIAN_POINT('Ctrl Pts',(-9.88878247200006,15.2,-4.26108937200001));
#270140=CARTESIAN_POINT('Ctrl Pts',(-9.88878247200006,11.6,-4.26108937200001));
#270141=CARTESIAN_POINT('Ctrl Pts',(-9.88622937300006,15.2,-4.26077285200002));
#270142=CARTESIAN_POINT('Ctrl Pts',(-9.88622937300006,11.6,-4.26077285200002));
#270143=CARTESIAN_POINT('Ctrl Pts',(-9.88368254300006,15.2,-4.26045490100002));
#270144=CARTESIAN_POINT('Ctrl Pts',(-9.88368254300006,11.6,-4.26045490100002));
#270145=CARTESIAN_POINT('Ctrl Pts',(-9.88114199400006,15.2,-4.26013552700002));
#270146=CARTESIAN_POINT('Ctrl Pts',(-9.88114199400006,11.6,-4.26013552700002));
#270147=CARTESIAN_POINT('Ctrl Pts',(-9.87860773400006,15.2,-4.25981474300002));
#270148=CARTESIAN_POINT('Ctrl Pts',(-9.87860773400006,11.6,-4.25981474300002));
#270149=CARTESIAN_POINT('Ctrl Pts',(-9.87607977400006,15.2,-4.25949255600001));
#270150=CARTESIAN_POINT('Ctrl Pts',(-9.87607977400006,11.6,-4.25949255600001));
#270151=CARTESIAN_POINT('Ctrl Pts',(-9.87355812500006,15.2,-4.25916898000001));
#270152=CARTESIAN_POINT('Ctrl Pts',(-9.87355812500006,11.6,-4.25916898000002));
#270153=CARTESIAN_POINT('Ctrl Pts',(-9.87104279700005,15.2,-4.25884402400001));
#270154=CARTESIAN_POINT('Ctrl Pts',(-9.87104279700005,11.6,-4.25884402400001));
#270155=CARTESIAN_POINT('Ctrl Pts',(-9.86853380100005,15.2,-4.25851769800001));
#270156=CARTESIAN_POINT('Ctrl Pts',(-9.86853380100005,11.6,-4.25851769800001));
#270157=CARTESIAN_POINT('Ctrl Pts',(-9.86603114800005,15.2,-4.25819001500002));
#270158=CARTESIAN_POINT('Ctrl Pts',(-9.86603114800005,11.6,-4.25819001500002));
#270159=CARTESIAN_POINT('Ctrl Pts',(-9.86353484600006,15.2,-4.25786098200001));
#270160=CARTESIAN_POINT('Ctrl Pts',(-9.86353484600006,11.6,-4.25786098200002));
#270161=CARTESIAN_POINT('Ctrl Pts',(-9.86104490900006,15.2,-4.25753061300002));
#270162=CARTESIAN_POINT('Ctrl Pts',(-9.86104490900006,11.6,-4.25753061300002));
#270163=CARTESIAN_POINT('Ctrl Pts',(-9.85856134500006,15.2,-4.25719891600002));
#270164=CARTESIAN_POINT('Ctrl Pts',(-9.85856134500006,11.6,-4.25719891600002));
#270165=CARTESIAN_POINT('Ctrl Pts',(-9.85608416600006,15.2,-4.25686590500002));
#270166=CARTESIAN_POINT('Ctrl Pts',(-9.85608416600006,11.6,-4.25686590500002));
#270167=CARTESIAN_POINT('Ctrl Pts',(-9.85361338300006,15.2,-4.25653158900001));
#270168=CARTESIAN_POINT('Ctrl Pts',(-9.85361338300006,11.6,-4.25653158900001));
#270169=CARTESIAN_POINT('Ctrl Pts',(-9.85114900400006,15.2,-4.25619597800001));
#270170=CARTESIAN_POINT('Ctrl Pts',(-9.85114900400006,11.6,-4.25619597800001));
#270171=CARTESIAN_POINT('Ctrl Pts',(-9.84869104300006,15.2,-4.25585908400001));
#270172=CARTESIAN_POINT('Ctrl Pts',(-9.84869104300006,11.6,-4.25585908400001));
#270173=CARTESIAN_POINT('Ctrl Pts',(-9.84623950900006,15.2,-4.25552091800002));
#270174=CARTESIAN_POINT('Ctrl Pts',(-9.84623950900006,11.6,-4.25552091800002));
#270175=CARTESIAN_POINT('Ctrl Pts',(-9.84379441200005,15.2,-4.25518149100002));
#270176=CARTESIAN_POINT('Ctrl Pts',(-9.84379441200005,11.6,-4.25518149100002));
#270177=CARTESIAN_POINT('Ctrl Pts',(-9.84135576400006,15.2,-4.25484081400001));
#270178=CARTESIAN_POINT('Ctrl Pts',(-9.84135576400006,11.6,-4.25484081400001));
#270179=CARTESIAN_POINT('Ctrl Pts',(-9.83892357600006,15.2,-4.25449889700001));
#270180=CARTESIAN_POINT('Ctrl Pts',(-9.83892357600006,11.6,-4.25449889700001));
#270181=CARTESIAN_POINT('Ctrl Pts',(-9.83649785800005,15.2,-4.25415575300002));
#270182=CARTESIAN_POINT('Ctrl Pts',(-9.83649785800005,11.6,-4.25415575300002));
#270183=CARTESIAN_POINT('Ctrl Pts',(-9.83407862100006,15.2,-4.25381139100002));
#270184=CARTESIAN_POINT('Ctrl Pts',(-9.83407862100006,11.6,-4.25381139100002));
#270185=CARTESIAN_POINT('Ctrl Pts',(-9.83166587600006,15.2,-4.25346582400001));
#270186=CARTESIAN_POINT('Ctrl Pts',(-9.83166587600006,11.6,-4.25346582400001));
#270187=CARTESIAN_POINT('Ctrl Pts',(-9.82925963200006,15.2,-4.25311906200001));
#270188=CARTESIAN_POINT('Ctrl Pts',(-9.82925963200006,11.6,-4.25311906200002));
#270189=CARTESIAN_POINT('Ctrl Pts',(-9.82685990300006,15.2,-4.25277111600002));
#270190=CARTESIAN_POINT('Ctrl Pts',(-9.82685990300006,11.6,-4.25277111600002));
#270191=CARTESIAN_POINT('Ctrl Pts',(-9.82446669800006,15.2,-4.25242200000001));
#270192=CARTESIAN_POINT('Ctrl Pts',(-9.82446669800006,11.6,-4.25242200000001));
#270193=CARTESIAN_POINT('Ctrl Pts',(-9.82208002800006,15.2,-4.25207172100002));
#270194=CARTESIAN_POINT('Ctrl Pts',(-9.82208002800006,11.6,-4.25207172100002));
#270195=CARTESIAN_POINT('Ctrl Pts',(-9.81969990500006,15.2,-4.25172029500001));
#270196=CARTESIAN_POINT('Ctrl Pts',(-9.81969990500006,11.6,-4.25172029500002));
#270197=CARTESIAN_POINT('Ctrl Pts',(-9.81732633900006,15.2,-4.25136772900002));
#270198=CARTESIAN_POINT('Ctrl Pts',(-9.81732633900006,11.6,-4.25136772900002));
#270199=CARTESIAN_POINT('Ctrl Pts',(-9.81495934200005,15.2,-4.25101403800001));
#270200=CARTESIAN_POINT('Ctrl Pts',(-9.81495934200005,11.6,-4.25101403800001));
#270201=CARTESIAN_POINT('Ctrl Pts',(-9.81259892300006,15.2,-4.25065923100002));
#270202=CARTESIAN_POINT('Ctrl Pts',(-9.81259892300006,11.6,-4.25065923100002));
#270203=CARTESIAN_POINT('Ctrl Pts',(-9.81024509500006,15.2,-4.25030332100001));
#270204=CARTESIAN_POINT('Ctrl Pts',(-9.81024509500006,11.6,-4.25030332100001));
#270205=CARTESIAN_POINT('Ctrl Pts',(-9.80789786800005,15.2,-4.24994631800002));
#270206=CARTESIAN_POINT('Ctrl Pts',(-9.80789786800005,11.6,-4.24994631800002));
#270207=CARTESIAN_POINT('Ctrl Pts',(-9.80555725300006,15.2,-4.24958823700001));
#270208=CARTESIAN_POINT('Ctrl Pts',(-9.80555725300006,11.6,-4.24958823700001));
#270209=CARTESIAN_POINT('Ctrl Pts',(-9.80322326200006,15.2,-4.24922908500001));
#270210=CARTESIAN_POINT('Ctrl Pts',(-9.80322326200006,11.6,-4.24922908500002));
#270211=CARTESIAN_POINT('Ctrl Pts',(-9.80089590600006,15.2,-4.24886887800001));
#270212=CARTESIAN_POINT('Ctrl Pts',(-9.80089590600006,11.6,-4.24886887800001));
#270213=CARTESIAN_POINT('Ctrl Pts',(-9.79857519500005,15.2,-4.24850762500002));
#270214=CARTESIAN_POINT('Ctrl Pts',(-9.79857519500005,11.6,-4.24850762500002));
#270215=CARTESIAN_POINT('Ctrl Pts',(-9.79626114100006,15.2,-4.24814533800001));
#270216=CARTESIAN_POINT('Ctrl Pts',(-9.79626114100006,11.6,-4.24814533800001));
#270217=CARTESIAN_POINT('Ctrl Pts',(-9.79395375600006,15.2,-4.24778203100002));
#270218=CARTESIAN_POINT('Ctrl Pts',(-9.79395375600006,11.6,-4.24778203100002));
#270219=CARTESIAN_POINT('Ctrl Pts',(-9.79165305000006,15.2,-4.24741771300001));
#270220=CARTESIAN_POINT('Ctrl Pts',(-9.79165305000006,11.6,-4.24741771300001));
#270221=CARTESIAN_POINT('Ctrl Pts',(-9.78935903500006,15.2,-4.24705239700002));
#270222=CARTESIAN_POINT('Ctrl Pts',(-9.78935903500006,11.6,-4.24705239700002));
#270223=CARTESIAN_POINT('Ctrl Pts',(-9.78707172100006,15.2,-4.24668609500001));
#270224=CARTESIAN_POINT('Ctrl Pts',(-9.78707172100006,11.6,-4.24668609500001));
#270225=CARTESIAN_POINT('Ctrl Pts',(-9.78479112100005,15.2,-4.24631882000002));
#270226=CARTESIAN_POINT('Ctrl Pts',(-9.78479112100005,11.6,-4.24631882000002));
#270227=CARTESIAN_POINT('Ctrl Pts',(-9.78251724500005,15.2,-4.24595058300001));
#270228=CARTESIAN_POINT('Ctrl Pts',(-9.78251724500005,11.6,-4.24595058300001));
#270229=CARTESIAN_POINT('Ctrl Pts',(-9.78025010600006,15.2,-4.24558139600002));
#270230=CARTESIAN_POINT('Ctrl Pts',(-9.78025010600006,11.6,-4.24558139600002));
#270231=CARTESIAN_POINT('Ctrl Pts',(-9.77798971300006,15.2,-4.24521127100002));
#270232=CARTESIAN_POINT('Ctrl Pts',(-9.77798971300006,11.6,-4.24521127100002));
#270233=CARTESIAN_POINT('Ctrl Pts',(-9.77573607900006,15.2,-4.24484022000001));
#270234=CARTESIAN_POINT('Ctrl Pts',(-9.77573607900006,11.6,-4.24484022000002));
#270235=CARTESIAN_POINT('Ctrl Pts',(-9.77348921600005,15.2,-4.24446825700001));
#270236=CARTESIAN_POINT('Ctrl Pts',(-9.77348921600005,11.6,-4.24446825700001));
#270237=CARTESIAN_POINT('Ctrl Pts',(-9.77124913500005,15.2,-4.24409539200001));
#270238=CARTESIAN_POINT('Ctrl Pts',(-9.77124913500005,11.6,-4.24409539200001));
#270239=CARTESIAN_POINT('Ctrl Pts',(-9.76901584600006,15.2,-4.24372163900001));
#270240=CARTESIAN_POINT('Ctrl Pts',(-9.76901584600006,11.6,-4.24372163900001));
#270241=CARTESIAN_POINT('Ctrl Pts',(-9.76678936200006,15.2,-4.24334700900001));
#270242=CARTESIAN_POINT('Ctrl Pts',(-9.76678936200006,11.6,-4.24334700900001));
#270243=CARTESIAN_POINT('Ctrl Pts',(-9.76456969400006,15.2,-4.24297151500001));
#270244=CARTESIAN_POINT('Ctrl Pts',(-9.76456969400006,11.6,-4.24297151500001));
#270245=CARTESIAN_POINT('Ctrl Pts',(-9.76235685400006,15.2,-4.24259517000001));
#270246=CARTESIAN_POINT('Ctrl Pts',(-9.76235685400006,11.6,-4.24259517000001));
#270247=CARTESIAN_POINT('Ctrl Pts',(-9.76015085200006,15.2,-4.24221798600001));
#270248=CARTESIAN_POINT('Ctrl Pts',(-9.76015085200006,11.6,-4.24221798600002));
#270249=CARTESIAN_POINT('Ctrl Pts',(-9.75795170300006,15.2,-4.24183997400001));
#270250=CARTESIAN_POINT('Ctrl Pts',(-9.75795170300006,11.6,-4.24183997400002));
#270251=CARTESIAN_POINT('Ctrl Pts',(-9.75575941400006,15.2,-4.24146115000001));
#270252=CARTESIAN_POINT('Ctrl Pts',(-9.75575941400006,11.6,-4.24146115000002));
#270253=CARTESIAN_POINT('Ctrl Pts',(-9.75357400200006,15.2,-4.24108152300001));
#270254=CARTESIAN_POINT('Ctrl Pts',(-9.75357400200006,11.6,-4.24108152300002));
#270255=CARTESIAN_POINT('Ctrl Pts',(-9.75139547400006,15.2,-4.24070110800002));
#270256=CARTESIAN_POINT('Ctrl Pts',(-9.75139547400006,11.6,-4.24070110800002));
#270257=CARTESIAN_POINT('Ctrl Pts',(-9.74922384500006,15.2,-4.24031991600001));
#270258=CARTESIAN_POINT('Ctrl Pts',(-9.74922384500006,11.6,-4.24031991600002));
#270259=CARTESIAN_POINT('Ctrl Pts',(-9.74705912500006,15.2,-4.23993796200001));
#270260=CARTESIAN_POINT('Ctrl Pts',(-9.74705912500006,11.6,-4.23993796200001));
#270261=CARTESIAN_POINT('Ctrl Pts',(-9.74490132600006,15.2,-4.23955525700002));
#270262=CARTESIAN_POINT('Ctrl Pts',(-9.74490132600006,11.6,-4.23955525700002));
#270263=CARTESIAN_POINT('Ctrl Pts',(-9.74275046000006,15.2,-4.23917181500002));
#270264=CARTESIAN_POINT('Ctrl Pts',(-9.74275046000006,11.6,-4.23917181500002));
#270265=CARTESIAN_POINT('Ctrl Pts',(-9.74060653900005,15.2,-4.23878764800001));
#270266=CARTESIAN_POINT('Ctrl Pts',(-9.74060653900005,11.6,-4.23878764800001));
#270267=CARTESIAN_POINT('Ctrl Pts',(-9.73846957500006,15.2,-4.23840276900001));
#270268=CARTESIAN_POINT('Ctrl Pts',(-9.73846957500006,11.6,-4.23840276900001));
#270269=CARTESIAN_POINT('Ctrl Pts',(-9.73633957900006,15.2,-4.23801719200001));
#270270=CARTESIAN_POINT('Ctrl Pts',(-9.73633957900006,11.6,-4.23801719200002));
#270271=CARTESIAN_POINT('Ctrl Pts',(-9.73421656400006,15.2,-4.23763092800002));
#270272=CARTESIAN_POINT('Ctrl Pts',(-9.73421656400006,11.6,-4.23763092800002));
#270273=CARTESIAN_POINT('Ctrl Pts',(-9.73210054100005,15.2,-4.23724399300001));
#270274=CARTESIAN_POINT('Ctrl Pts',(-9.73210054100005,11.6,-4.23724399300002));
#270275=CARTESIAN_POINT('Ctrl Pts',(-9.72999152300006,15.2,-4.23685639700001));
#270276=CARTESIAN_POINT('Ctrl Pts',(-9.72999152300006,11.6,-4.23685639700001));
#270277=CARTESIAN_POINT('Ctrl Pts',(-9.72788952300006,15.2,-4.23646815600002));
#270278=CARTESIAN_POINT('Ctrl Pts',(-9.72788952300006,11.6,-4.23646815600002));
#270279=CARTESIAN_POINT('Ctrl Pts',(-9.72579454900006,15.2,-4.23607928100001));
#270280=CARTESIAN_POINT('Ctrl Pts',(-9.72579454900006,11.6,-4.23607928100001));
#270281=CARTESIAN_POINT('Ctrl Pts',(-9.72370661700005,15.2,-4.23568978700001));
#270282=CARTESIAN_POINT('Ctrl Pts',(-9.72370661700005,11.6,-4.23568978700002));
#270283=CARTESIAN_POINT('Ctrl Pts',(-9.72162573800006,15.2,-4.23529968600001));
#270284=CARTESIAN_POINT('Ctrl Pts',(-9.72162573800006,11.6,-4.23529968600001));
#270285=CARTESIAN_POINT('Ctrl Pts',(-9.71955192300006,15.2,-4.23490899300001));
#270286=CARTESIAN_POINT('Ctrl Pts',(-9.71955192300006,11.6,-4.23490899300001));
#270287=CARTESIAN_POINT('Ctrl Pts',(-9.71748518600006,15.2,-4.23451771900002));
#270288=CARTESIAN_POINT('Ctrl Pts',(-9.71748518600006,11.6,-4.23451771900002));
#270289=CARTESIAN_POINT('Ctrl Pts',(-9.71542553800005,15.2,-4.23412588100001));
#270290=CARTESIAN_POINT('Ctrl Pts',(-9.71542553800005,11.6,-4.23412588100002));
#270291=CARTESIAN_POINT('Ctrl Pts',(-9.71337299100006,15.2,-4.23373348900002));
#270292=CARTESIAN_POINT('Ctrl Pts',(-9.71337299100006,11.6,-4.23373348900002));
#270293=CARTESIAN_POINT('Ctrl Pts',(-9.71132755700006,15.2,-4.23334055800002));
#270294=CARTESIAN_POINT('Ctrl Pts',(-9.71132755700006,11.6,-4.23334055800002));
#270295=CARTESIAN_POINT('Ctrl Pts',(-9.70928925100005,15.2,-4.23294710300001));
#270296=CARTESIAN_POINT('Ctrl Pts',(-9.70928925100005,11.6,-4.23294710300001));
#270297=CARTESIAN_POINT('Ctrl Pts',(-9.70725808200006,15.2,-4.23255313500002));
#270298=CARTESIAN_POINT('Ctrl Pts',(-9.70725808200006,11.6,-4.23255313500002));
#270299=CARTESIAN_POINT('Ctrl Pts',(-9.70523406400006,15.2,-4.23215867100001));
#270300=CARTESIAN_POINT('Ctrl Pts',(-9.70523406400006,11.6,-4.23215867100002));
#270301=CARTESIAN_POINT('Ctrl Pts',(-9.70321720900006,15.2,-4.23176372200002));
#270302=CARTESIAN_POINT('Ctrl Pts',(-9.70321720900006,11.6,-4.23176372200002));
#270303=CARTESIAN_POINT('Ctrl Pts',(-9.70120753000005,15.2,-4.23136830300002));
#270304=CARTESIAN_POINT('Ctrl Pts',(-9.70120753000005,11.6,-4.23136830300002));
#270305=CARTESIAN_POINT('Ctrl Pts',(-9.69920503800006,15.2,-4.23097242800001));
#270306=CARTESIAN_POINT('Ctrl Pts',(-9.69920503800006,11.6,-4.23097242800001));
#270307=CARTESIAN_POINT('Ctrl Pts',(-9.69720974700006,15.2,-4.23057611000001));
#270308=CARTESIAN_POINT('Ctrl Pts',(-9.69720974700006,11.6,-4.23057611000001));
#270309=CARTESIAN_POINT('Ctrl Pts',(-9.69522166900006,15.2,-4.23017936500001));
#270310=CARTESIAN_POINT('Ctrl Pts',(-9.69522166900006,11.6,-4.23017936500001));
#270311=CARTESIAN_POINT('Ctrl Pts',(-9.69324081600006,15.2,-4.22978220500001));
#270312=CARTESIAN_POINT('Ctrl Pts',(-9.69324081600006,11.6,-4.22978220500002));
#270313=CARTESIAN_POINT('Ctrl Pts',(-9.69126720200006,15.2,-4.22938464600001));
#270314=CARTESIAN_POINT('Ctrl Pts',(-9.69126720200006,11.6,-4.22938464600001));
#270315=CARTESIAN_POINT('Ctrl Pts',(-9.68930083800006,15.2,-4.22898670000002));
#270316=CARTESIAN_POINT('Ctrl Pts',(-9.68930083800006,11.6,-4.22898670000002));
#270317=CARTESIAN_POINT('Ctrl Pts',(-9.68734173700006,15.2,-4.22858838400002));
#270318=CARTESIAN_POINT('Ctrl Pts',(-9.68734173700006,11.6,-4.22858838400002));
#270319=CARTESIAN_POINT('Ctrl Pts',(-9.68538991200005,15.2,-4.22818971000002));
#270320=CARTESIAN_POINT('Ctrl Pts',(-9.68538991200005,11.6,-4.22818971000002));
#270321=CARTESIAN_POINT('Ctrl Pts',(-9.68344537600006,15.2,-4.22779069300002));
#270322=CARTESIAN_POINT('Ctrl Pts',(-9.68344537600006,11.6,-4.22779069300002));
#270323=CARTESIAN_POINT('Ctrl Pts',(-9.68150814100006,15.2,-4.22739134800001));
#270324=CARTESIAN_POINT('Ctrl Pts',(-9.68150814100006,11.6,-4.22739134800001));
#270325=CARTESIAN_POINT('Ctrl Pts',(-9.67957822000006,15.2,-4.22699168800001));
#270326=CARTESIAN_POINT('Ctrl Pts',(-9.67957822000006,11.6,-4.22699168800001));
#270327=CARTESIAN_POINT('Ctrl Pts',(-9.67765562600006,15.2,-4.22659173000001));
#270328=CARTESIAN_POINT('Ctrl Pts',(-9.67765562600006,11.6,-4.22659173000001));
#270329=CARTESIAN_POINT('Ctrl Pts',(-9.67574037300006,15.2,-4.22619148600001));
#270330=CARTESIAN_POINT('Ctrl Pts',(-9.67574037300006,11.6,-4.22619148600001));
#270331=CARTESIAN_POINT('Ctrl Pts',(-9.67383247200006,15.2,-4.22579097300002));
#270332=CARTESIAN_POINT('Ctrl Pts',(-9.67383247200006,11.6,-4.22579097300002));
#270333=CARTESIAN_POINT('Ctrl Pts',(-9.67193193600006,15.2,-4.22539020400002));
#270334=CARTESIAN_POINT('Ctrl Pts',(-9.67193193600006,11.6,-4.22539020400002));
#270335=CARTESIAN_POINT('Ctrl Pts',(-9.67003878000006,15.2,-4.22498919400002));
#270336=CARTESIAN_POINT('Ctrl Pts',(-9.67003878000006,11.6,-4.22498919400002));
#270337=CARTESIAN_POINT('Ctrl Pts',(-9.66815301400005,15.2,-4.22458795800001));
#270338=CARTESIAN_POINT('Ctrl Pts',(-9.66815301400005,11.6,-4.22458795800001));
#270339=CARTESIAN_POINT('Ctrl Pts',(-9.66627465400006,15.2,-4.22418651100001));
#270340=CARTESIAN_POINT('Ctrl Pts',(-9.66627465400006,11.6,-4.22418651100002));
#270341=CARTESIAN_POINT('Ctrl Pts',(-9.66440371000006,15.2,-4.22378486900001));
#270342=CARTESIAN_POINT('Ctrl Pts',(-9.66440371000006,11.6,-4.22378486900001));
#270343=CARTESIAN_POINT('Ctrl Pts',(-9.66254019900006,15.2,-4.22338304400002));
#270344=CARTESIAN_POINT('Ctrl Pts',(-9.66254019900006,11.6,-4.22338304400002));
#270345=CARTESIAN_POINT('Ctrl Pts',(-9.66068413000006,15.2,-4.22298105400001));
#270346=CARTESIAN_POINT('Ctrl Pts',(-9.66068413000006,11.6,-4.22298105400001));
#270347=CARTESIAN_POINT('Ctrl Pts',(-9.65883551800006,15.2,-4.22257891400001));
#270348=CARTESIAN_POINT('Ctrl Pts',(-9.65883551800006,11.6,-4.22257891400002));
#270349=CARTESIAN_POINT('Ctrl Pts',(-9.65699437800006,15.2,-4.22217663600001));
#270350=CARTESIAN_POINT('Ctrl Pts',(-9.65699437800006,11.6,-4.22217663600002));
#270351=CARTESIAN_POINT('Ctrl Pts',(-9.65516071900005,15.2,-4.22177424000001));
#270352=CARTESIAN_POINT('Ctrl Pts',(-9.65516071900005,11.6,-4.22177424000001));
#270353=CARTESIAN_POINT('Ctrl Pts',(-9.65333455800006,15.2,-4.22137173700001));
#270354=CARTESIAN_POINT('Ctrl Pts',(-9.65333455800006,11.6,-4.22137173700001));
#270355=CARTESIAN_POINT('Ctrl Pts',(-9.65151590800006,15.2,-4.22096914500001));
#270356=CARTESIAN_POINT('Ctrl Pts',(-9.65151590800006,11.6,-4.22096914500001));
#270357=CARTESIAN_POINT('Ctrl Pts',(-9.64970478100006,15.2,-4.22056647800002));
#270358=CARTESIAN_POINT('Ctrl Pts',(-9.64970478100006,11.6,-4.22056647800002));
#270359=CARTESIAN_POINT('Ctrl Pts',(-9.64790118900006,15.2,-4.22016375300001));
#270360=CARTESIAN_POINT('Ctrl Pts',(-9.64790118900006,11.6,-4.22016375300002));
#270361=CARTESIAN_POINT('Ctrl Pts',(-9.64610514900006,15.2,-4.21976098400001));
#270362=CARTESIAN_POINT('Ctrl Pts',(-9.64610514900006,11.6,-4.21976098400001));
#270363=CARTESIAN_POINT('Ctrl Pts',(-9.64431667200006,15.2,-4.21935818700002));
#270364=CARTESIAN_POINT('Ctrl Pts',(-9.64431667200006,11.6,-4.21935818700002));
#270365=CARTESIAN_POINT('Ctrl Pts',(-9.64253577200006,15.2,-4.21895537800001));
#270366=CARTESIAN_POINT('Ctrl Pts',(-9.64253577200006,11.6,-4.21895537800001));
#270367=CARTESIAN_POINT('Ctrl Pts',(-9.64076246400005,15.2,-4.21855257300002));
#270368=CARTESIAN_POINT('Ctrl Pts',(-9.64076246400005,11.6,-4.21855257300002));
#270369=CARTESIAN_POINT('Ctrl Pts',(-9.63899675900005,15.2,-4.21814978700001));
#270370=CARTESIAN_POINT('Ctrl Pts',(-9.63899675900005,11.6,-4.21814978700001));
#270371=CARTESIAN_POINT('Ctrl Pts',(-9.63723867300006,15.2,-4.21774703800001));
#270372=CARTESIAN_POINT('Ctrl Pts',(-9.63723867300006,11.6,-4.21774703800002));
#270373=CARTESIAN_POINT('Ctrl Pts',(-9.63548821800006,15.2,-4.21734433900002));
#270374=CARTESIAN_POINT('Ctrl Pts',(-9.63548821800006,11.6,-4.21734433900002));
#270375=CARTESIAN_POINT('Ctrl Pts',(-9.63374540700006,15.2,-4.21694170700002));
#270376=CARTESIAN_POINT('Ctrl Pts',(-9.63374540700006,11.6,-4.21694170700002));
#270377=CARTESIAN_POINT('Ctrl Pts',(-9.63201025800006,15.2,-4.21653915900002));
#270378=CARTESIAN_POINT('Ctrl Pts',(-9.63201025800006,11.6,-4.21653915900002));
#270379=CARTESIAN_POINT('Ctrl Pts',(-9.63028278000005,15.2,-4.21613671100001));
#270380=CARTESIAN_POINT('Ctrl Pts',(-9.63028278000005,11.6,-4.21613671100001));
#270381=CARTESIAN_POINT('Ctrl Pts',(-9.62856298800006,15.2,-4.21573437800001));
#270382=CARTESIAN_POINT('Ctrl Pts',(-9.62856298800006,11.6,-4.21573437800001));
#270383=CARTESIAN_POINT('Ctrl Pts',(-9.62685089700006,15.2,-4.21533217700001));
#270384=CARTESIAN_POINT('Ctrl Pts',(-9.62685089700006,11.6,-4.21533217700001));
#270385=CARTESIAN_POINT('Ctrl Pts',(-9.62514652100005,15.2,-4.21493012500001));
#270386=CARTESIAN_POINT('Ctrl Pts',(-9.62514652100005,11.6,-4.21493012500001));
#270387=CARTESIAN_POINT('Ctrl Pts',(-9.62344987300006,15.2,-4.21452823700001));
#270388=CARTESIAN_POINT('Ctrl Pts',(-9.62344987300006,11.6,-4.21452823700002));
#270389=CARTESIAN_POINT('Ctrl Pts',(-9.62176096800006,15.2,-4.21412653000001));
#270390=CARTESIAN_POINT('Ctrl Pts',(-9.62176096800006,11.6,-4.21412653000001));
#270391=CARTESIAN_POINT('Ctrl Pts',(-9.62007981900006,15.2,-4.21372502300001));
#270392=CARTESIAN_POINT('Ctrl Pts',(-9.62007981900006,11.6,-4.21372502300002));
#270393=CARTESIAN_POINT('Ctrl Pts',(-9.61840643900005,15.2,-4.21332372800002));
#270394=CARTESIAN_POINT('Ctrl Pts',(-9.61840643900005,11.6,-4.21332372800002));
#270395=CARTESIAN_POINT('Ctrl Pts',(-9.61674084500006,15.2,-4.21292266500001));
#270396=CARTESIAN_POINT('Ctrl Pts',(-9.61674084500006,11.6,-4.21292266500001));
#270397=CARTESIAN_POINT('Ctrl Pts',(-9.61508305000006,15.2,-4.21252185000002));
#270398=CARTESIAN_POINT('Ctrl Pts',(-9.61508305000006,11.6,-4.21252185000002));
#270399=CARTESIAN_POINT('Ctrl Pts',(-9.61343306700006,15.2,-4.21212129900002));
#270400=CARTESIAN_POINT('Ctrl Pts',(-9.61343306700006,11.6,-4.21212129900002));
#270401=CARTESIAN_POINT('Ctrl Pts',(-9.61179091200006,15.2,-4.21172103000002));
#270402=CARTESIAN_POINT('Ctrl Pts',(-9.61179091200006,11.6,-4.21172103000002));
#270403=CARTESIAN_POINT('Ctrl Pts',(-9.61015659800006,15.2,-4.21132106100002));
#270404=CARTESIAN_POINT('Ctrl Pts',(-9.61015659800006,11.6,-4.21132106100002));
#270405=CARTESIAN_POINT('Ctrl Pts',(-9.60853014000006,15.2,-4.21092140600001));
#270406=CARTESIAN_POINT('Ctrl Pts',(-9.60853014000006,11.6,-4.21092140600001));
#270407=CARTESIAN_POINT('Ctrl Pts',(-9.60691155200006,15.2,-4.21052208500001));
#270408=CARTESIAN_POINT('Ctrl Pts',(-9.60691155200006,11.6,-4.21052208500001));
#270409=CARTESIAN_POINT('Ctrl Pts',(-9.60530084800006,15.2,-4.21012311200001));
#270410=CARTESIAN_POINT('Ctrl Pts',(-9.60530084800006,11.6,-4.21012311200002));
#270411=CARTESIAN_POINT('Ctrl Pts',(-9.60369804400005,15.2,-4.20972450700001));
#270412=CARTESIAN_POINT('Ctrl Pts',(-9.60369804400005,11.6,-4.20972450700001));
#270413=CARTESIAN_POINT('Ctrl Pts',(-9.60210315400005,15.2,-4.20932628800001));
#270414=CARTESIAN_POINT('Ctrl Pts',(-9.60210315400005,11.6,-4.20932628800002));
#270415=CARTESIAN_POINT('Ctrl Pts',(-9.60051619200006,15.2,-4.20892847000002));
#270416=CARTESIAN_POINT('Ctrl Pts',(-9.60051619200006,11.6,-4.20892847000002));
#270417=CARTESIAN_POINT('Ctrl Pts',(-9.59893717200006,15.2,-4.20853107100001));
#270418=CARTESIAN_POINT('Ctrl Pts',(-9.59893717200006,11.6,-4.20853107100002));
#270419=CARTESIAN_POINT('Ctrl Pts',(-9.59736611000006,15.2,-4.20813411000001));
#270420=CARTESIAN_POINT('Ctrl Pts',(-9.59736611000006,11.6,-4.20813411000002));
#270421=CARTESIAN_POINT('Ctrl Pts',(-9.59580302000006,15.2,-4.20773760300001));
#270422=CARTESIAN_POINT('Ctrl Pts',(-9.59580302000006,11.6,-4.20773760300001));
#270423=CARTESIAN_POINT('Ctrl Pts',(-9.59424791700006,15.2,-4.20734157000001));
#270424=CARTESIAN_POINT('Ctrl Pts',(-9.59424791700006,11.6,-4.20734157000001));
#270425=CARTESIAN_POINT('Ctrl Pts',(-9.59270081500006,15.2,-4.20694602600001));
#270426=CARTESIAN_POINT('Ctrl Pts',(-9.59270081500006,11.6,-4.20694602600001));
#270427=CARTESIAN_POINT('Ctrl Pts',(-9.59116173000006,15.2,-4.20655099000002));
#270428=CARTESIAN_POINT('Ctrl Pts',(-9.59116173000006,11.6,-4.20655099000002));
#270429=CARTESIAN_POINT('Ctrl Pts',(-9.58963067700006,15.2,-4.20615648000001));
#270430=CARTESIAN_POINT('Ctrl Pts',(-9.58963067700006,11.6,-4.20615648000001));
#270431=CARTESIAN_POINT('Ctrl Pts',(-9.58810767000006,15.2,-4.20576251400002));
#270432=CARTESIAN_POINT('Ctrl Pts',(-9.58810767000006,11.6,-4.20576251400002));
#270433=CARTESIAN_POINT('Ctrl Pts',(-9.58659272300006,15.2,-4.20536911000001));
#270434=CARTESIAN_POINT('Ctrl Pts',(-9.58659272300006,11.6,-4.20536911000002));
#270435=CARTESIAN_POINT('Ctrl Pts',(-9.58508585400006,15.2,-4.20497628800002));
#270436=CARTESIAN_POINT('Ctrl Pts',(-9.58508585400006,11.6,-4.20497628800002));
#270437=CARTESIAN_POINT('Ctrl Pts',(-9.58358707600006,15.2,-4.20458406300002));
#270438=CARTESIAN_POINT('Ctrl Pts',(-9.58358707600006,11.6,-4.20458406300002));
#270439=CARTESIAN_POINT('Ctrl Pts',(-9.58209640400005,15.2,-4.20419245700002));
#270440=CARTESIAN_POINT('Ctrl Pts',(-9.58209640400005,11.6,-4.20419245700002));
#270441=CARTESIAN_POINT('Ctrl Pts',(-9.58061385500006,15.2,-4.20380148500001));
#270442=CARTESIAN_POINT('Ctrl Pts',(-9.58061385500006,11.6,-4.20380148500001));
#270443=CARTESIAN_POINT('Ctrl Pts',(-9.57913944200006,15.2,-4.20341116800001));
#270444=CARTESIAN_POINT('Ctrl Pts',(-9.57913944200006,11.6,-4.20341116800001));
#270445=CARTESIAN_POINT('Ctrl Pts',(-9.57767318100006,15.2,-4.20302152200001));
#270446=CARTESIAN_POINT('Ctrl Pts',(-9.57767318100006,11.6,-4.20302152200002));
#270447=CARTESIAN_POINT('Ctrl Pts',(-9.57621508800005,15.2,-4.20263256900002));
#270448=CARTESIAN_POINT('Ctrl Pts',(-9.57621508800005,11.6,-4.20263256900002));
#270449=CARTESIAN_POINT('Ctrl Pts',(-9.57476517900006,15.2,-4.20224432500001));
#270450=CARTESIAN_POINT('Ctrl Pts',(-9.57476517900006,11.6,-4.20224432500001));
#270451=CARTESIAN_POINT('Ctrl Pts',(-9.57332346800005,15.2,-4.20185681100001));
#270452=CARTESIAN_POINT('Ctrl Pts',(-9.57332346800005,11.6,-4.20185681100001));
#270453=CARTESIAN_POINT('Ctrl Pts',(-9.57188997100006,15.2,-4.20147004400001));
#270454=CARTESIAN_POINT('Ctrl Pts',(-9.57188997100006,11.6,-4.20147004400001));
#270455=CARTESIAN_POINT('Ctrl Pts',(-9.57046470400006,15.2,-4.20108404600001));
#270456=CARTESIAN_POINT('Ctrl Pts',(-9.57046470400006,11.6,-4.20108404600002));
#270457=CARTESIAN_POINT('Ctrl Pts',(-9.56904768100006,15.2,-4.20069883200001));
#270458=CARTESIAN_POINT('Ctrl Pts',(-9.56904768100006,11.6,-4.20069883200001));
#270459=CARTESIAN_POINT('Ctrl Pts',(-9.56763891900006,15.2,-4.20031442400001));
#270460=CARTESIAN_POINT('Ctrl Pts',(-9.56763891900006,11.6,-4.20031442400001));
#270461=CARTESIAN_POINT('Ctrl Pts',(-9.56623843400006,15.2,-4.19993084100001));
#270462=CARTESIAN_POINT('Ctrl Pts',(-9.56623843400006,11.6,-4.19993084100002));
#270463=CARTESIAN_POINT('Ctrl Pts',(-9.56484624200005,15.2,-4.19954810100001));
#270464=CARTESIAN_POINT('Ctrl Pts',(-9.56484624200005,11.6,-4.19954810100002));
#270465=CARTESIAN_POINT('Ctrl Pts',(-9.56346235700006,15.2,-4.19916622400001));
#270466=CARTESIAN_POINT('Ctrl Pts',(-9.56346235700006,11.6,-4.19916622400002));
#270467=CARTESIAN_POINT('Ctrl Pts',(-9.56208679700006,15.2,-4.19878523200001));
#270468=CARTESIAN_POINT('Ctrl Pts',(-9.56208679700006,11.6,-4.19878523200001));
#270469=CARTESIAN_POINT('Ctrl Pts',(-9.56071957600006,15.2,-4.19840514100001));
#270470=CARTESIAN_POINT('Ctrl Pts',(-9.56071957600006,11.6,-4.19840514100002));
#270471=CARTESIAN_POINT('Ctrl Pts',(-9.55936071100006,15.2,-4.19802597300002));
#270472=CARTESIAN_POINT('Ctrl Pts',(-9.55936071100006,11.6,-4.19802597300002));
#270473=CARTESIAN_POINT('Ctrl Pts',(-9.55801021900006,15.2,-4.19764774700001));
#270474=CARTESIAN_POINT('Ctrl Pts',(-9.55801021900006,11.6,-4.19764774700001));
#270475=CARTESIAN_POINT('Ctrl Pts',(-9.55666811400006,15.2,-4.19727048300001));
#270476=CARTESIAN_POINT('Ctrl Pts',(-9.55666811400006,11.6,-4.19727048300001));
#270477=CARTESIAN_POINT('Ctrl Pts',(-9.55533441300006,15.2,-4.19689420200001));
#270478=CARTESIAN_POINT('Ctrl Pts',(-9.55533441300006,11.6,-4.19689420200002));
#270479=CARTESIAN_POINT('Ctrl Pts',(-9.55400913300006,15.2,-4.19651892300001));
#270480=CARTESIAN_POINT('Ctrl Pts',(-9.55400913300006,11.6,-4.19651892300002));
#270481=CARTESIAN_POINT('Ctrl Pts',(-9.55269229000006,15.2,-4.19614466600001));
#270482=CARTESIAN_POINT('Ctrl Pts',(-9.55269229000006,11.6,-4.19614466600002));
#270483=CARTESIAN_POINT('Ctrl Pts',(-9.55138390100006,15.2,-4.19577145200002));
#270484=CARTESIAN_POINT('Ctrl Pts',(-9.55138390100006,11.6,-4.19577145200002));
#270485=CARTESIAN_POINT('Ctrl Pts',(-9.55008398000006,15.2,-4.19539930100001));
#270486=CARTESIAN_POINT('Ctrl Pts',(-9.55008398000006,11.6,-4.19539930100001));
#270487=CARTESIAN_POINT('Ctrl Pts',(-9.54879254600005,15.2,-4.19502823400002));
#270488=CARTESIAN_POINT('Ctrl Pts',(-9.54879254600005,11.6,-4.19502823400002));
#270489=CARTESIAN_POINT('Ctrl Pts',(-9.54750961400006,15.2,-4.19465827100002));
#270490=CARTESIAN_POINT('Ctrl Pts',(-9.54750961400006,11.6,-4.19465827100002));
#270491=CARTESIAN_POINT('Ctrl Pts',(-9.54623520100006,15.2,-4.19428943400002));
#270492=CARTESIAN_POINT('Ctrl Pts',(-9.54623520100006,11.6,-4.19428943400002));
#270493=CARTESIAN_POINT('Ctrl Pts',(-9.54496932400006,15.2,-4.19392174100001));
#270494=CARTESIAN_POINT('Ctrl Pts',(-9.54496932400006,11.6,-4.19392174100001));
#270495=CARTESIAN_POINT('Ctrl Pts',(-9.54371199900006,15.2,-4.19355521600002));
#270496=CARTESIAN_POINT('Ctrl Pts',(-9.54371199900006,11.6,-4.19355521600002));
#270497=CARTESIAN_POINT('Ctrl Pts',(-9.54246324300006,15.2,-4.19318987800001));
#270498=CARTESIAN_POINT('Ctrl Pts',(-9.54246324300006,11.6,-4.19318987800002));
#270499=CARTESIAN_POINT('Ctrl Pts',(-9.54122307300005,15.2,-4.19282574800001));
#270500=CARTESIAN_POINT('Ctrl Pts',(-9.54122307300005,11.6,-4.19282574800001));
#270501=CARTESIAN_POINT('Ctrl Pts',(-9.53999150600006,15.2,-4.19246284900002));
#270502=CARTESIAN_POINT('Ctrl Pts',(-9.53999150600006,11.6,-4.19246284900002));
#270503=CARTESIAN_POINT('Ctrl Pts',(-9.53876855900005,15.2,-4.19210120000002));
#270504=CARTESIAN_POINT('Ctrl Pts',(-9.53876855900005,11.6,-4.19210120000002));
#270505=CARTESIAN_POINT('Ctrl Pts',(-9.53755424900006,15.2,-4.19174082400001));
#270506=CARTESIAN_POINT('Ctrl Pts',(-9.53755424900006,11.6,-4.19174082400002));
#270507=CARTESIAN_POINT('Ctrl Pts',(-9.53634859300006,15.2,-4.19138174200001));
#270508=CARTESIAN_POINT('Ctrl Pts',(-9.53634859300006,11.6,-4.19138174200001));
#270509=CARTESIAN_POINT('Ctrl Pts',(-9.53515160800006,15.2,-4.19102397600001));
#270510=CARTESIAN_POINT('Ctrl Pts',(-9.53515160800006,11.6,-4.19102397600002));
#270511=CARTESIAN_POINT('Ctrl Pts',(-9.53396331100006,15.2,-4.19066754700001));
#270512=CARTESIAN_POINT('Ctrl Pts',(-9.53396331100006,11.6,-4.19066754700001));
#270513=CARTESIAN_POINT('Ctrl Pts',(-9.53278371900005,15.2,-4.19031247800001));
#270514=CARTESIAN_POINT('Ctrl Pts',(-9.53278371900005,11.6,-4.19031247800001));
#270515=CARTESIAN_POINT('Ctrl Pts',(-9.53161285100006,15.2,-4.18995879000001));
#270516=CARTESIAN_POINT('Ctrl Pts',(-9.53161285100006,11.6,-4.18995879000002));
#270517=CARTESIAN_POINT('Ctrl Pts',(-9.53045072400006,15.2,-4.18960650400001));
#270518=CARTESIAN_POINT('Ctrl Pts',(-9.53045072400006,11.6,-4.18960650400001));
#270519=CARTESIAN_POINT('Ctrl Pts',(-9.52929735300006,15.2,-4.18925564400002));
#270520=CARTESIAN_POINT('Ctrl Pts',(-9.52929735300006,11.6,-4.18925564400002));
#270521=CARTESIAN_POINT('Ctrl Pts',(-9.52815275900005,15.2,-4.18890623000001));
#270522=CARTESIAN_POINT('Ctrl Pts',(-9.52815275900005,11.6,-4.18890623000001));
#270523=CARTESIAN_POINT('Ctrl Pts',(-9.52701695800006,15.2,-4.18855828800002));
#270524=CARTESIAN_POINT('Ctrl Pts',(-9.52701695800006,11.6,-4.18855828800002));
#270525=CARTESIAN_POINT('Ctrl Pts',(-9.52588996700005,15.2,-4.18821183700001));
#270526=CARTESIAN_POINT('Ctrl Pts',(-9.52588996700005,11.6,-4.18821183700001));
#270527=CARTESIAN_POINT('Ctrl Pts',(-9.52477180300006,15.2,-4.18786690100001));
#270528=CARTESIAN_POINT('Ctrl Pts',(-9.52477180300006,11.6,-4.18786690100002));
#270529=CARTESIAN_POINT('Ctrl Pts',(-9.52366248800006,15.2,-4.18752350200001));
#270530=CARTESIAN_POINT('Ctrl Pts',(-9.52366248800006,11.6,-4.18752350200002));
#270531=CARTESIAN_POINT('Ctrl Pts',(-9.52256203600006,15.2,-4.18718166400001));
#270532=CARTESIAN_POINT('Ctrl Pts',(-9.52256203600006,11.6,-4.18718166400002));
#270533=CARTESIAN_POINT('Ctrl Pts',(-9.52147046600006,15.2,-4.18684141000002));
#270534=CARTESIAN_POINT('Ctrl Pts',(-9.52147046600006,11.6,-4.18684141000002));
#270535=CARTESIAN_POINT('Ctrl Pts',(-9.52038779700005,15.2,-4.18650276100001));
#270536=CARTESIAN_POINT('Ctrl Pts',(-9.52038779700005,11.6,-4.18650276100002));
#270537=CARTESIAN_POINT('Ctrl Pts',(-9.51931404600005,15.2,-4.18616574200001));
#270538=CARTESIAN_POINT('Ctrl Pts',(-9.51931404600005,11.6,-4.18616574200002));
#270539=CARTESIAN_POINT('Ctrl Pts',(-9.51824923100006,15.2,-4.18583037500001));
#270540=CARTESIAN_POINT('Ctrl Pts',(-9.51824923100006,11.6,-4.18583037500001));
#270541=CARTESIAN_POINT('Ctrl Pts',(-9.51719337200006,15.2,-4.18549668500001));
#270542=CARTESIAN_POINT('Ctrl Pts',(-9.51719337200006,11.6,-4.18549668500001));
#270543=CARTESIAN_POINT('Ctrl Pts',(-9.51614648500006,15.2,-4.18516469500001));
#270544=CARTESIAN_POINT('Ctrl Pts',(-9.51614648500006,11.6,-4.18516469500002));
#270545=CARTESIAN_POINT('Ctrl Pts',(-9.51510859000006,15.2,-4.18483442700001));
#270546=CARTESIAN_POINT('Ctrl Pts',(-9.51510859000006,11.6,-4.18483442700001));
#270547=CARTESIAN_POINT('Ctrl Pts',(-9.51407970500006,15.2,-4.18450590600001));
#270548=CARTESIAN_POINT('Ctrl Pts',(-9.51407970500006,11.6,-4.18450590600001));
#270549=CARTESIAN_POINT('Ctrl Pts',(-9.51305984900005,15.2,-4.18417915700001));
#270550=CARTESIAN_POINT('Ctrl Pts',(-9.51305984900005,11.6,-4.18417915700002));
#270551=CARTESIAN_POINT('Ctrl Pts',(-9.51204904000006,15.2,-4.18385420100002));
#270552=CARTESIAN_POINT('Ctrl Pts',(-9.51204904000006,11.6,-4.18385420100002));
#270553=CARTESIAN_POINT('Ctrl Pts',(-9.51104729800005,15.2,-4.18353106500001));
#270554=CARTESIAN_POINT('Ctrl Pts',(-9.51104729800005,11.6,-4.18353106500002));
#270555=CARTESIAN_POINT('Ctrl Pts',(-9.51005464000006,15.2,-4.18320977200001));
#270556=CARTESIAN_POINT('Ctrl Pts',(-9.51005464000006,11.6,-4.18320977200001));
#270557=CARTESIAN_POINT('Ctrl Pts',(-9.50907108500006,15.2,-4.18289034600001));
#270558=CARTESIAN_POINT('Ctrl Pts',(-9.50907108500006,11.6,-4.18289034600001));
#270559=CARTESIAN_POINT('Ctrl Pts',(-9.50809665400006,15.2,-4.18257281300002));
#270560=CARTESIAN_POINT('Ctrl Pts',(-9.50809665400006,11.6,-4.18257281300002));
#270561=CARTESIAN_POINT('Ctrl Pts',(-9.50713136500006,15.2,-4.18225719500001));
#270562=CARTESIAN_POINT('Ctrl Pts',(-9.50713136500006,11.6,-4.18225719500002));
#270563=CARTESIAN_POINT('Ctrl Pts',(-9.50617523600006,15.2,-4.18194352000001));
#270564=CARTESIAN_POINT('Ctrl Pts',(-9.50617523600006,11.6,-4.18194352000001));
#270565=CARTESIAN_POINT('Ctrl Pts',(-9.50522828800005,15.2,-4.18163181000001));
#270566=CARTESIAN_POINT('Ctrl Pts',(-9.50522828800005,11.6,-4.18163181000002));
#270567=CARTESIAN_POINT('Ctrl Pts',(-9.50429053900006,15.2,-4.18132209200001));
#270568=CARTESIAN_POINT('Ctrl Pts',(-9.50429053900006,11.6,-4.18132209200001));
#270569=CARTESIAN_POINT('Ctrl Pts',(-9.50336200900006,15.2,-4.18101439000001));
#270570=CARTESIAN_POINT('Ctrl Pts',(-9.50336200900006,11.6,-4.18101439000001));
#270571=CARTESIAN_POINT('Ctrl Pts',(-9.50244271700006,15.2,-4.18070872900001));
#270572=CARTESIAN_POINT('Ctrl Pts',(-9.50244271700006,11.6,-4.18070872900001));
#270573=CARTESIAN_POINT('Ctrl Pts',(-9.50153268200006,15.2,-4.18040513500001));
#270574=CARTESIAN_POINT('Ctrl Pts',(-9.50153268200006,11.6,-4.18040513500001));
#270575=CARTESIAN_POINT('Ctrl Pts',(-9.50063192600006,15.2,-4.18010363500001));
#270576=CARTESIAN_POINT('Ctrl Pts',(-9.50063192600006,11.6,-4.18010363500002));
#270577=CARTESIAN_POINT('Ctrl Pts',(-9.49974046700006,15.2,-4.17980425200001));
#270578=CARTESIAN_POINT('Ctrl Pts',(-9.49974046700006,11.6,-4.17980425200002));
#270579=CARTESIAN_POINT('Ctrl Pts',(-9.49885832400006,15.2,-4.17950701300001));
#270580=CARTESIAN_POINT('Ctrl Pts',(-9.49885832400006,11.6,-4.17950701300002));
#270581=CARTESIAN_POINT('Ctrl Pts',(-9.49799054600006,15.2,-4.17921364400001));
#270582=CARTESIAN_POINT('Ctrl Pts',(-9.49799054600006,11.6,-4.17921364400002));
#270583=CARTESIAN_POINT('Ctrl Pts',(-9.49730470600005,15.2,-4.17898101900001));
#270584=CARTESIAN_POINT('Ctrl Pts',(-9.49730470600005,11.6,-4.17898101900002));
#270585=CARTESIAN_POINT('Ctrl Pts',(-9.49679571000006,15.2,-4.17880795400002));
#270586=CARTESIAN_POINT('Ctrl Pts',(-9.49679571000006,11.6,-4.17880795400002));
#270587=CARTESIAN_POINT('Ctrl Pts',(-9.49645984700006,15.2,-4.17869357200002));
#270588=CARTESIAN_POINT('Ctrl Pts',(-9.49645984700006,11.6,-4.17869357200002));
#270589=CARTESIAN_POINT('Ctrl Pts',(-9.49629481200006,15.2,-4.17863732200002));
#270590=CARTESIAN_POINT('Ctrl Pts',(-9.49629481200006,11.6,-4.17863732200002));
#270591=CARTESIAN_POINT('',(-9.49629481136457,12.2,-4.17863732134707));
#270592=CARTESIAN_POINT('',(-9.49629481136457,15.2,-4.17863732134707));
#270593=CARTESIAN_POINT('',(-9.49629481100006,12.2,-4.17863732100002));
#270594=CARTESIAN_POINT('Ctrl Pts',(-10.6761442620001,12.2,-4.27433546900002));
#270595=CARTESIAN_POINT('Ctrl Pts',(-10.6723314813074,12.2,-4.27461376405057));
#270596=CARTESIAN_POINT('Ctrl Pts',(-10.6685249858623,12.2,-4.27488727070577));
#270597=CARTESIAN_POINT('Ctrl Pts',(-10.664724775623,12.2,-4.27515599121663));
#270598=CARTESIAN_POINT('Ctrl Pts',(-10.6609245653838,12.2,-4.2754247117275));
#270599=CARTESIAN_POINT('Ctrl Pts',(-10.6571306407685,12.2,-4.27568864374578));
#270600=CARTESIAN_POINT('Ctrl Pts',(-10.6533430152162,12.2,-4.27594779995819));
#270601=CARTESIAN_POINT('Ctrl Pts',(-10.6495553896639,12.2,-4.27620695617061));
#270602=CARTESIAN_POINT('Ctrl Pts',(-10.64577406477,12.2,-4.27646133445405));
#270603=CARTESIAN_POINT('Ctrl Pts',(-10.641999077073,12.2,-4.27671095994562));
#270604=CARTESIAN_POINT('Ctrl Pts',(-10.6382240886901,12.2,-4.27696058548255));
#270605=CARTESIAN_POINT('Ctrl Pts',(-10.6344554370091,12.2,-4.27720545935147));
#270606=CARTESIAN_POINT('Ctrl Pts',(-10.6306931631715,12.2,-4.27744560934406));
#270607=CARTESIAN_POINT('Ctrl Pts',(-10.6269308900174,12.2,-4.27768575929303));
#270608=CARTESIAN_POINT('Ctrl Pts',(-10.623174996138,12.2,-4.27792118538392));
#270609=CARTESIAN_POINT('Ctrl Pts',(-10.6194255113997,12.2,-4.27815191029179));
#270610=CARTESIAN_POINT('Ctrl Pts',(-10.6156760266615,12.2,-4.27838263519966));
#270611=CARTESIAN_POINT('Ctrl Pts',(-10.6119329517445,12.2,-4.27860865854064));
#270612=CARTESIAN_POINT('Ctrl Pts',(-10.6081963174883,12.2,-4.27883000099191));
#270613=CARTESIAN_POINT('Ctrl Pts',(-10.6019685935017,12.2,-4.27919890509078));
#270614=CARTESIAN_POINT('Ctrl Pts',(-10.5957587585331,12.2,-4.27955480756196));
#270615=CARTESIAN_POINT('Ctrl Pts',(-10.5895669738118,12.2,-4.27989782075574));
#270616=CARTESIAN_POINT('Ctrl Pts',(-10.585851903114,12.2,-4.28010362866452));
#270617=CARTESIAN_POINT('Ctrl Pts',(-10.5821433307655,12.2,-4.28030479564053));
#270618=CARTESIAN_POINT('Ctrl Pts',(-10.578441290525,12.2,-4.28050134796672));
#270619=CARTESIAN_POINT('Ctrl Pts',(-10.5747392502845,12.2,-4.28069790029291));
#270620=CARTESIAN_POINT('Ctrl Pts',(-10.5710437423854,12.2,-4.28088983588595));
#270621=CARTESIAN_POINT('Ctrl Pts',(-10.5673547996439,12.2,-4.28107717971288));
#270622=CARTESIAN_POINT('Ctrl Pts',(-10.5636658569023,12.2,-4.28126452353981));
#270623=CARTESIAN_POINT('Ctrl Pts',(-10.5599834796454,12.2,-4.2814472737959));
#270624=CARTESIAN_POINT('Ctrl Pts',(-10.5563077012612,12.2,-4.28162545671553));
#270625=CARTESIAN_POINT('Ctrl Pts',(-10.5526319228771,12.2,-4.28180363963515));
#270626=CARTESIAN_POINT('Ctrl Pts',(-10.548962744233,12.2,-4.28197725503537));
#270627=CARTESIAN_POINT('Ctrl Pts',(-10.5453001995318,12.2,-4.28214632648818));
#270628=CARTESIAN_POINT('Ctrl Pts',(-10.5416376541652,12.2,-4.28231539797171));
#270629=CARTESIAN_POINT('Ctrl Pts',(-10.5379817430673,12.2,-4.28247992557895));
#270630=CARTESIAN_POINT('Ctrl Pts',(-10.5343324992462,12.2,-4.28263993501826));
#270631=CARTESIAN_POINT('Ctrl Pts',(-10.5294668419229,12.2,-4.28285328088888));
#270632=CARTESIAN_POINT('Ctrl Pts',(-10.524613039387,12.2,-4.28305859348278));
#270633=CARTESIAN_POINT('Ctrl Pts',(-10.5197711731709,12.2,-4.28325593146717));
#270634=CARTESIAN_POINT('Ctrl Pts',(-10.5161397733439,12.2,-4.28340393496218));
#270635=CARTESIAN_POINT('Ctrl Pts',(-10.5125150858668,12.2,-4.28354745247069));
#270636=CARTESIAN_POINT('Ctrl Pts',(-10.5088971479001,12.2,-4.28368650993143));
#270637=CARTESIAN_POINT('Ctrl Pts',(-10.5040732301729,12.2,-4.28387191989594));
#270638=CARTESIAN_POINT('Ctrl Pts',(-10.4992613097435,12.2,-4.28404940070511));
#270639=CARTESIAN_POINT('Ctrl Pts',(-10.4944614683161,12.2,-4.28421901204717));
#270640=CARTESIAN_POINT('Ctrl Pts',(-10.4908615875725,12.2,-4.28434622054216));
#270641=CARTESIAN_POINT('Ctrl Pts',(-10.4872685011197,12.2,-4.28446900300435));
#270642=CARTESIAN_POINT('Ctrl Pts',(-10.48368224525,12.2,-4.28458738450005));
#270643=CARTESIAN_POINT('Ctrl Pts',(-10.4800959893803,12.2,-4.28470576599575));
#270644=CARTESIAN_POINT('Ctrl Pts',(-10.476516561377,12.2,-4.28481974652496));
#270645=CARTESIAN_POINT('Ctrl Pts',(-10.4729439986312,12.2,-4.28492935297969));
#270646=CARTESIAN_POINT('Ctrl Pts',(-10.4693714358854,12.2,-4.28503895943442));
#270647=CARTESIAN_POINT('Ctrl Pts',(-10.4658057382475,12.2,-4.28514419088112));
#270648=CARTESIAN_POINT('Ctrl Pts',(-10.4622469395425,12.2,-4.28524507346138));
#270649=CARTESIAN_POINT('Ctrl Pts',(-10.458688140191,12.2,-4.28534595605997));
#270650=CARTESIAN_POINT('Ctrl Pts',(-10.4551362403248,12.2,-4.28544249114066));
#270651=CARTESIAN_POINT('Ctrl Pts',(-10.4515912749772,12.2,-4.28553470319514));
#270652=CARTESIAN_POINT('Ctrl Pts',(-10.4480463102736,12.2,-4.28562691523287));
#270653=CARTESIAN_POINT('Ctrl Pts',(-10.4445082802975,12.2,-4.28571480553221));
#270654=CARTESIAN_POINT('Ctrl Pts',(-10.4409772208336,12.2,-4.28579840003284));
#270655=CARTESIAN_POINT('Ctrl Pts',(-10.4374461613696,12.2,-4.28588199453348));
#270656=CARTESIAN_POINT('Ctrl Pts',(-10.433922071605,12.2,-4.28596129389458));
#270657=CARTESIAN_POINT('Ctrl Pts',(-10.4304049869001,12.2,-4.28603632351648));
#270658=CARTESIAN_POINT('Ctrl Pts',(-10.4268879021952,12.2,-4.28611135313839));
#270659=CARTESIAN_POINT('Ctrl Pts',(-10.4233778229894,12.2,-4.2861821153858));
#270660=CARTESIAN_POINT('Ctrl Pts',(-10.4198747852833,12.2,-4.28624863500838));
#270661=CARTESIAN_POINT('Ctrl Pts',(-10.4163717475773,12.2,-4.28631515463096));
#270662=CARTESIAN_POINT('Ctrl Pts',(-10.4128757505209,12.2,-4.28637743367872));
#270663=CARTESIAN_POINT('Ctrl Pts',(-10.4093868303138,12.2,-4.28643549771864));
#270664=CARTESIAN_POINT('Ctrl Pts',(-10.4058979101066,12.2,-4.28649356175857));
#270665=CARTESIAN_POINT('Ctrl Pts',(-10.4024160668705,12.2,-4.28654741123923));
#270666=CARTESIAN_POINT('Ctrl Pts',(-10.3989413359473,12.2,-4.28659707424039));
#270667=CARTESIAN_POINT('Ctrl Pts',(-10.3954666050242,12.2,-4.28664673724155));
#270668=CARTESIAN_POINT('Ctrl Pts',(-10.3919989866963,12.2,-4.28669221344197));
#270669=CARTESIAN_POINT('Ctrl Pts',(-10.3885385170294,12.2,-4.2867335309827));
#270670=CARTESIAN_POINT('Ctrl Pts',(-10.3850780467338,12.2,-4.28677484853094));
#270671=CARTESIAN_POINT('Ctrl Pts',(-10.3816247257653,12.2,-4.286812007603));
#270672=CARTESIAN_POINT('Ctrl Pts',(-10.3781785885154,12.2,-4.28684503473224));
#270673=CARTESIAN_POINT('Ctrl Pts',(-10.3747324518916,12.2,-4.28687806185548));
#270674=CARTESIAN_POINT('Ctrl Pts',(-10.3712935002508,12.2,-4.2869069595206));
#270675=CARTESIAN_POINT('Ctrl Pts',(-10.3678617691261,12.2,-4.28693175401935));
#270676=CARTESIAN_POINT('Ctrl Pts',(-10.3644300380014,12.2,-4.28695654851809));
#270677=CARTESIAN_POINT('Ctrl Pts',(-10.3610055284049,12.2,-4.28697723981727));
#270678=CARTESIAN_POINT('Ctrl Pts',(-10.3575882757219,12.2,-4.28699385777506));
#270679=CARTESIAN_POINT('Ctrl Pts',(-10.3541710230389,12.2,-4.28701047573284));
#270680=CARTESIAN_POINT('Ctrl Pts',(-10.3507610277449,12.2,-4.28702301880028));
#270681=CARTESIAN_POINT('Ctrl Pts',(-10.3473583265198,12.2,-4.28703151775837));
#270682=CARTESIAN_POINT('Ctrl Pts',(-10.3439556252946,12.2,-4.28704001671645));
#270683=CARTESIAN_POINT('Ctrl Pts',(-10.3405602175136,12.2,-4.28704446969959));
#270684=CARTESIAN_POINT('Ctrl Pts',(-10.3371721403444,12.2,-4.28704490674159));
#270685=CARTESIAN_POINT('Ctrl Pts',(-10.3337840631752,12.2,-4.28704534378359));
#270686=CARTESIAN_POINT('Ctrl Pts',(-10.3304033169305,12.2,-4.28704176500087));
#270687=CARTESIAN_POINT('Ctrl Pts',(-10.3270299377187,12.2,-4.28703419950169));
#270688=CARTESIAN_POINT('Ctrl Pts',(-10.3236565578941,12.2,-4.28702663400113));
#270689=CARTESIAN_POINT('Ctrl Pts',(-10.3202905453716,12.2,-4.28701508123278));
#270690=CARTESIAN_POINT('Ctrl Pts',(-10.3169319370512,12.2,-4.28699957127166));
#270691=CARTESIAN_POINT('Ctrl Pts',(-10.3135733293409,12.2,-4.28698406131335));
#270692=CARTESIAN_POINT('Ctrl Pts',(-10.3102221255145,12.2,-4.28696459394625));
#270693=CARTESIAN_POINT('Ctrl Pts',(-10.3068783635948,12.2,-4.28694119948714));
#270694=CARTESIAN_POINT('Ctrl Pts',(-10.302420014571,12.2,-4.28691000687642));
#270695=CARTESIAN_POINT('Ctrl Pts',(-10.2979748947121,12.2,-4.28687183206897));
#270696=CARTESIAN_POINT('Ctrl Pts',(-10.2935430926291,12.2,-4.28682674679533));
#270697=CARTESIAN_POINT('Ctrl Pts',(-10.2891112899422,12.2,-4.28678166151554));
#270698=CARTESIAN_POINT('Ctrl Pts',(-10.2846928040848,12.2,-4.28672966532104));
#270699=CARTESIAN_POINT('Ctrl Pts',(-10.2802877236233,12.2,-4.28667083076183));
#270700=CARTESIAN_POINT('Ctrl Pts',(-10.2758826437621,12.2,-4.28661199621064));
#270701=CARTESIAN_POINT('Ctrl Pts',(-10.2714909720224,12.2,-4.28654632313818));
#270702=CARTESIAN_POINT('Ctrl Pts',(-10.2671127956604,12.2,-4.28647388575218));
#270703=CARTESIAN_POINT('Ctrl Pts',(-10.2616400747605,12.2,-4.28638333901228));
#270704=CARTESIAN_POINT('Ctrl Pts',(-10.2561884385453,12.2,-4.2862822195345));
#270705=CARTESIAN_POINT('Ctrl Pts',(-10.2507580663219,12.2,-4.28617067550727));
#270706=CARTESIAN_POINT('Ctrl Pts',(-10.2464137683065,12.2,-4.28608144028063));
#270707=CARTESIAN_POINT('Ctrl Pts',(-10.2420830778455,12.2,-4.28598553343928));
#270708=CARTESIAN_POINT('Ctrl Pts',(-10.2377660858889,12.2,-4.2858830282666));
#270709=CARTESIAN_POINT('Ctrl Pts',(-10.2334490945205,12.2,-4.28578052310788));
#270710=CARTESIAN_POINT('Ctrl Pts',(-10.2291458010151,12.2,-4.28567142075143));
#270711=CARTESIAN_POINT('Ctrl Pts',(-10.2248562973725,12.2,-4.28555579753345));
#270712=CARTESIAN_POINT('Ctrl Pts',(-10.2205667931455,12.2,-4.28544017429972));
#270713=CARTESIAN_POINT('Ctrl Pts',(-10.2162910771914,12.2,-4.28531802910246));
#270714=CARTESIAN_POINT('Ctrl Pts',(-10.2120292431267,12.2,-4.28518944053947));
#270715=CARTESIAN_POINT('Ctrl Pts',(-10.2056364926104,12.2,-4.28499655771251));
#270716=CARTESIAN_POINT('Ctrl Pts',(-10.1992749719582,12.2,-4.28478917367839));
#270717=CARTESIAN_POINT('Ctrl Pts',(-10.1929449946034,12.2,-4.28456755577039));
#270718=CARTESIAN_POINT('Ctrl Pts',(-10.188725009317,12.2,-4.28441981048497));
#270719=CARTESIAN_POINT('Ctrl Pts',(-10.1845190429924,12.2,-4.2842657365357));
#270720=CARTESIAN_POINT('Ctrl Pts',(-10.1803271881668,12.2,-4.28410541601841));
#270721=CARTESIAN_POINT('Ctrl Pts',(-10.1761353339124,12.2,-4.28394509552296));
#270722=CARTESIAN_POINT('Ctrl Pts',(-10.1719575910844,12.2,-4.28377852720513));
#270723=CARTESIAN_POINT('Ctrl Pts',(-10.1677940530905,12.2,-4.28360579199743));
#270724=CARTESIAN_POINT('Ctrl Pts',(-10.1636305145293,12.2,-4.2834330567662));
#270725=CARTESIAN_POINT('Ctrl Pts',(-10.1594811815504,12.2,-4.28325415403423));
#270726=CARTESIAN_POINT('Ctrl Pts',(-10.1553461469371,12.2,-4.28306916546819));
#270727=CARTESIAN_POINT('Ctrl Pts',(-10.1512111128872,12.2,-4.28288417692736));
#270728=CARTESIAN_POINT('Ctrl Pts',(-10.1470903771138,12.2,-4.28269310169959));
#270729=CARTESIAN_POINT('Ctrl Pts',(-10.1429840348543,12.2,-4.28249602326193));
#270730=CARTESIAN_POINT('Ctrl Pts',(-10.1388776920352,12.2,-4.28229894479743));
#270731=CARTESIAN_POINT('Ctrl Pts',(-10.1347857421381,12.2,-4.28209586226968));
#270732=CARTESIAN_POINT('Ctrl Pts',(-10.1307082809168,12.2,-4.28188686042456));
#270733=CARTESIAN_POINT('Ctrl Pts',(-10.1266308202511,12.2,-4.28167785860793));
#270734=CARTESIAN_POINT('Ctrl Pts',(-10.1225678474186,12.2,-4.28146293579527));
#270735=CARTESIAN_POINT('Ctrl Pts',(-10.1185194581369,12.2,-4.28124217736946));
#270736=CARTESIAN_POINT('Ctrl Pts',(-10.1144710683037,12.2,-4.28102141891358));
#270737=CARTESIAN_POINT('Ctrl Pts',(-10.1104372633524,12.2,-4.28079482361548));
#270738=CARTESIAN_POINT('Ctrl Pts',(-10.1064181374667,12.2,-4.28056247899171));
#270739=CARTESIAN_POINT('Ctrl Pts',(-10.102399011581,12.2,-4.28033013436793));
#270740=CARTESIAN_POINT('Ctrl Pts',(-10.0983945658136,12.2,-4.28009203847127));
#270741=CARTESIAN_POINT('Ctrl Pts',(-10.0944048965977,12.2,-4.27984827873518));
#270742=CARTESIAN_POINT('Ctrl Pts',(-10.0894178108932,12.2,-4.27954357911489));
#270743=CARTESIAN_POINT('Ctrl Pts',(-10.0844538133152,12.2,-4.27923003070079));
#270744=CARTESIAN_POINT('Ctrl Pts',(-10.0795130951712,12.2,-4.27890780129218));
#270745=CARTESIAN_POINT('Ctrl Pts',(-10.0755605200098,12.2,-4.27865001772314));
#270746=CARTESIAN_POINT('Ctrl Pts',(-10.071622842161,12.2,-4.27838668153135));
#270747=CARTESIAN_POINT('Ctrl Pts',(-10.067700162225,12.2,-4.27811787851671));
#270748=CARTESIAN_POINT('Ctrl Pts',(-10.063777482289,12.2,-4.27784907550205));
#270749=CARTESIAN_POINT('Ctrl Pts',(-10.0598697977658,12.2,-4.27757480846732));
#270750=CARTESIAN_POINT('Ctrl Pts',(-10.0559772103886,12.2,-4.27729516472931));
#270751=CARTESIAN_POINT('Ctrl Pts',(-10.0520846235417,12.2,-4.2770155210294));
#270752=CARTESIAN_POINT('Ctrl Pts',(-10.0482071308073,12.2,-4.2767305019278));
#270753=CARTESIAN_POINT('Ctrl Pts',(-10.0443448334943,12.2,-4.27644019895023));
#270754=CARTESIAN_POINT('Ctrl Pts',(-10.0404825356551,12.2,-4.27614989593311));
#270755=CARTESIAN_POINT('Ctrl Pts',(-10.036635431628,12.2,-4.27585430849834));
#270756=CARTESIAN_POINT('Ctrl Pts',(-10.0328036243652,12.2,-4.27555352942585));
#270757=CARTESIAN_POINT('Ctrl Pts',(-10.0289718176244,12.2,-4.27525275039435));
#270758=CARTESIAN_POINT('Ctrl Pts',(-10.02515530504,12.2,-4.27494678055521));
#270759=CARTESIAN_POINT('Ctrl Pts',(-10.0213541877942,12.2,-4.27463571102542));
#270760=CARTESIAN_POINT('Ctrl Pts',(-10.0166027908485,12.2,-4.27424687408139));
#270761=CARTESIAN_POINT('Ctrl Pts',(-10.0118754504462,12.2,-4.27385007224096));
#270762=CARTESIAN_POINT('Ctrl Pts',(-10.0071723642442,12.2,-4.27344549001692));
#270763=CARTESIAN_POINT('Ctrl Pts',(-10.0034098950776,12.2,-4.27312182422005));
#270764=CARTESIAN_POINT('Ctrl Pts',(-9.99966294813059,12.2,-4.27279317682806));
#270765=CARTESIAN_POINT('Ctrl Pts',(-9.99593162637327,12.2,-4.2724596484205));
#270766=CARTESIAN_POINT('Ctrl Pts',(-9.99220030512434,12.2,-4.27212612005838));
#270767=CARTESIAN_POINT('Ctrl Pts',(-9.98848460922062,12.2,-4.27178770721357));
#270768=CARTESIAN_POINT('Ctrl Pts',(-9.98478464124428,12.2,-4.27144450951971));
#270769=CARTESIAN_POINT('Ctrl Pts',(-9.98108467276383,12.2,-4.2711013117791));
#270770=CARTESIAN_POINT('Ctrl Pts',(-9.97740043215235,12.2,-4.27075332805274));
#270771=CARTESIAN_POINT('Ctrl Pts',(-9.97373202349277,12.2,-4.27040065768217));
#270772=CARTESIAN_POINT('Ctrl Pts',(-9.97006361533301,12.2,-4.27004798735964));
#270773=CARTESIAN_POINT('Ctrl Pts',(-9.96641103905952,12.2,-4.26969063026913));
#270774=CARTESIAN_POINT('Ctrl Pts',(-9.96277439852244,12.2,-4.26932868602124));
#270775=CARTESIAN_POINT('Ctrl Pts',(-9.95913775748987,12.2,-4.26896674172404));
#270776=CARTESIAN_POINT('Ctrl Pts',(-9.95551705261475,12.2,-4.26860021032628));
#270777=CARTESIAN_POINT('Ctrl Pts',(-9.95191239069714,12.2,-4.26822919469466));
#270778=CARTESIAN_POINT('Ctrl Pts',(-9.94830772927065,12.2,-4.26785817911359));
#270779=CARTESIAN_POINT('Ctrl Pts',(-9.94471910794518,12.2,-4.26748267773156));
#270780=CARTESIAN_POINT('Ctrl Pts',(-9.9411466345018,12.2,-4.2671027935218));
#270781=CARTESIAN_POINT('Ctrl Pts',(-9.93668104233251,12.2,-4.26662793822077));
#270782=CARTESIAN_POINT('Ctrl Pts',(-9.93224068220688,12.2,-4.26614623688713));
#270783=CARTESIAN_POINT('Ctrl Pts',(-9.92782576033055,12.2,-4.26565789008193));
#270784=CARTESIAN_POINT('Ctrl Pts',(-9.92429382263698,12.2,-4.26526721261647));
#270785=CARTESIAN_POINT('Ctrl Pts',(-9.9207781666315,12.2,-4.26487228385883));
#270786=CARTESIAN_POINT('Ctrl Pts',(-9.91727889899741,12.2,-4.2644732082257));
#270787=CARTESIAN_POINT('Ctrl Pts',(-9.91377963184011,12.2,-4.26407413264694));
#270788=CARTESIAN_POINT('Ctrl Pts',(-9.91029675463041,12.2,-4.26367091152358));
#270789=CARTESIAN_POINT('Ctrl Pts',(-9.90683037446141,12.2,-4.2632636507591));
#270790=CARTESIAN_POINT('Ctrl Pts',(-9.9033639938201,12.2,-4.26285638993914));
#270791=CARTESIAN_POINT('Ctrl Pts',(-9.89991411150273,12.2,-4.26244509095004));
#270792=CARTESIAN_POINT('Ctrl Pts',(-9.89648083526114,12.2,-4.26202986148271));
#270793=CARTESIAN_POINT('Ctrl Pts',(-9.89304755948733,12.2,-4.26161463207195));
#270794=CARTESIAN_POINT('Ctrl Pts',(-9.88963089192687,12.2,-4.26119547374255));
#270795=CARTESIAN_POINT('Ctrl Pts',(-9.88623094081422,12.2,-4.26077249427752));
#270796=CARTESIAN_POINT('Ctrl Pts',(-9.88283098923834,12.2,-4.26034951475486));
#270797=CARTESIAN_POINT('Ctrl Pts',(-9.87944775677138,12.2,-4.25992271612239));
#270798=CARTESIAN_POINT('Ctrl Pts',(-9.87608135173937,12.2,-4.25949220870807));
#270799=CARTESIAN_POINT('Ctrl Pts',(-9.87271494716603,12.2,-4.25906170135241));
#270800=CARTESIAN_POINT('Ctrl Pts',(-9.86936537151861,12.2,-4.25862748709378));
#270801=CARTESIAN_POINT('Ctrl Pts',(-9.86603273634488,12.2,-4.25818967762994));
#270802=CARTESIAN_POINT('Ctrl Pts',(-9.86270010071707,12.2,-4.25775186810645));
#270803=CARTESIAN_POINT('Ctrl Pts',(-9.85938440543254,12.2,-4.25731046239373));
#270804=CARTESIAN_POINT('Ctrl Pts',(-9.85608576497498,12.2,-4.25686557875836));
#270805=CARTESIAN_POINT('Ctrl Pts',(-9.85196246462775,12.2,-4.25630947424447));
#270806=CARTESIAN_POINT('Ctrl Pts',(-9.84786581016064,12.2,-4.25574793036898));
#270807=CARTESIAN_POINT('Ctrl Pts',(-9.84379602423943,12.2,-4.25518117849139));
#270808=CARTESIAN_POINT('Ctrl Pts',(-9.83972623831823,12.2,-4.25461442661379));
#270809=CARTESIAN_POINT('Ctrl Pts',(-9.83568332359722,12.2,-4.25404246459586));
#270810=CARTESIAN_POINT('Ctrl Pts',(-9.83166750102918,12.2,-4.2534655252206));
#270811=CARTESIAN_POINT('Ctrl Pts',(-9.82765167846116,12.2,-4.25288858584534));
#270812=CARTESIAN_POINT('Ctrl Pts',(-9.82366294997854,12.2,-4.25230666850077));
#270813=CARTESIAN_POINT('Ctrl Pts',(-9.81970154400775,12.2,-4.2517200100283));
#270814=CARTESIAN_POINT('Ctrl Pts',(-9.81574013803695,12.2,-4.25113335155583));
#270815=CARTESIAN_POINT('Ctrl Pts',(-9.81180605415433,12.2,-4.25054195020015));
#270816=CARTESIAN_POINT('Ctrl Pts',(-9.807899520753,12.2,-4.24994604839436));
#270817=CARTESIAN_POINT('Ctrl Pts',(-9.80399298735167,12.2,-4.24935014658857));
#270818=CARTESIAN_POINT('Ctrl Pts',(-9.8001140056157,12.2,-4.2487497429881));
#270819=CARTESIAN_POINT('Ctrl Pts',(-9.79626280778635,12.2,-4.24814508288815));
#270820=CARTESIAN_POINT('Ctrl Pts',(-9.79241160995701,12.2,-4.24754042278821));
#270821=CARTESIAN_POINT('Ctrl Pts',(-9.78858819659571,12.2,-4.24693150449796));
#270822=CARTESIAN_POINT('Ctrl Pts',(-9.78479280152856,12.2,-4.24631857942819));
#270823=CARTESIAN_POINT('Ctrl Pts',(-9.7809974064614,12.2,-4.24570565435841));
#270824=CARTESIAN_POINT('Ctrl Pts',(-9.77723002954193,12.2,-4.24508871978581));
#270825=CARTESIAN_POINT('Ctrl Pts',(-9.77349091100259,12.2,-4.24446803145217));
#270826=CARTESIAN_POINT('Ctrl Pts',(-9.76975179287081,12.2,-4.24384734318619));
#270827=CARTESIAN_POINT('Ctrl Pts',(-9.7660409302215,12.2,-4.2432228994912));
#270828=CARTESIAN_POINT('Ctrl Pts',(-9.76235856402331,12.2,-4.24259496032382));
#270829=CARTESIAN_POINT('Ctrl Pts',(-9.75867619742375,12.2,-4.241967021088));
#270830=CARTESIAN_POINT('Ctrl Pts',(-9.75502232828207,12.2,-4.24133558456055));
#270831=CARTESIAN_POINT('Ctrl Pts',(-9.75139719918249,12.2,-4.24070091386637));
#270832=CARTESIAN_POINT('Ctrl Pts',(-9.74777207008294,12.2,-4.2400662431722));
#270833=CARTESIAN_POINT('Ctrl Pts',(-9.74417568140555,12.2,-4.23942833990622));
#270834=CARTESIAN_POINT('Ctrl Pts',(-9.74060827865587,12.2,-4.23878747008274));
#270835=CARTESIAN_POINT('Ctrl Pts',(-9.73704087590621,12.2,-4.23814660025926));
#270836=CARTESIAN_POINT('Ctrl Pts',(-9.73350245789784,12.2,-4.23750276470881));
#270837=CARTESIAN_POINT('Ctrl Pts',(-9.729993277688,12.2,-4.23685623575062));
#270838=CARTESIAN_POINT('Ctrl Pts',(-9.72648409747816,12.2,-4.23620970679243));
#270839=CARTESIAN_POINT('Ctrl Pts',(-9.72300415096625,12.2,-4.23556048506471));
#270840=CARTESIAN_POINT('Ctrl Pts',(-9.71955369270082,12.2,-4.23490884784262));
#270841=CARTESIAN_POINT('Ctrl Pts',(-9.7161032344354,12.2,-4.23425721062053));
#270842=CARTESIAN_POINT('Ctrl Pts',(-9.71268226287843,12.2,-4.23360315869224));
#270843=CARTESIAN_POINT('Ctrl Pts',(-9.70929103529349,12.2,-4.23294697480038));
#270844=CARTESIAN_POINT('Ctrl Pts',(-9.70589980770855,12.2,-4.23229079090851));
#270845=CARTESIAN_POINT('Ctrl Pts',(-9.70253832226108,12.2,-4.23163247609447));
#270846=CARTESIAN_POINT('Ctrl Pts',(-9.69920683823331,12.2,-4.23097231727502));
#270847=CARTESIAN_POINT('Ctrl Pts',(-9.69587535420553,12.2,-4.23031215845557));
#270848=CARTESIAN_POINT('Ctrl Pts',(-9.69257387279077,12.2,-4.22965015711379));
#270849=CARTESIAN_POINT('Ctrl Pts',(-9.6893026537482,12.2,-4.22898660745799));
#270850=CARTESIAN_POINT('Ctrl Pts',(-9.68537719103977,12.2,-4.22819034789997));
#270851=CARTESIAN_POINT('Ctrl Pts',(-9.68149530621348,12.2,-4.22739185813947));
#270852=CARTESIAN_POINT('Ctrl Pts',(-9.67765746143433,12.2,-4.22659165858529));
#270853=CARTESIAN_POINT('Ctrl Pts',(-9.67381961630657,12.2,-4.22579145895842));
#270854=CARTESIAN_POINT('Ctrl Pts',(-9.67002580960094,12.2,-4.22498954883965));
#270855=CARTESIAN_POINT('Ctrl Pts',(-9.66627650764965,12.2,-4.22418646212915));
#270856=CARTESIAN_POINT('Ctrl Pts',(-9.66252720603892,12.2,-4.22338337549158));
#270857=CARTESIAN_POINT('Ctrl Pts',(-9.65882241063247,12.2,-4.22257910981861));
#270858=CARTESIAN_POINT('Ctrl Pts',(-9.65516259326737,12.2,-4.22177421326448));
#270859=CARTESIAN_POINT('Ctrl Pts',(-9.65150277590228,12.2,-4.22096931671035));
#270860=CARTESIAN_POINT('Ctrl Pts',(-9.64788794090864,12.2,-4.22016378734798));
#270861=CARTESIAN_POINT('Ctrl Pts',(-9.64431856645303,12.2,-4.21935818404392));
#270862=CARTESIAN_POINT('Ctrl Pts',(-9.64074919199741,12.2,-4.21855258073986));
#270863=CARTESIAN_POINT('Ctrl Pts',(-9.63722528043084,12.2,-4.21774690530022));
#270864=CARTESIAN_POINT('Ctrl Pts',(-9.63374732280408,12.2,-4.21694172807945));
#270865=CARTESIAN_POINT('Ctrl Pts',(-9.6302693648614,12.2,-4.21613655078553));
#270866=CARTESIAN_POINT('Ctrl Pts',(-9.62683735939812,12.2,-4.21533187426664));
#270867=CARTESIAN_POINT('Ctrl Pts',(-9.62345180854899,12.2,-4.21452828222289));
#270868=CARTESIAN_POINT('Ctrl Pts',(-9.62006625800738,12.2,-4.21372469025214));
#270869=CARTESIAN_POINT('Ctrl Pts',(-9.61672715945526,12.2,-4.21292218647492));
#270870=CARTESIAN_POINT('Ctrl Pts',(-9.61343502397647,12.2,-4.21212136950038));
#270871=CARTESIAN_POINT('Ctrl Pts',(-9.61014288849769,12.2,-4.21132055252583));
#270872=CARTESIAN_POINT('Ctrl Pts',(-9.60689771440225,12.2,-4.21052142478306));
#270873=CARTESIAN_POINT('Ctrl Pts',(-9.60370002284853,12.2,-4.20972460356186));
#270874=CARTESIAN_POINT('Ctrl Pts',(-9.60050233100436,12.2,-4.20892778226828));
#270875=CARTESIAN_POINT('Ctrl Pts',(-9.59735211976474,12.2,-4.20813326644989));
#270876=CARTESIAN_POINT('Ctrl Pts',(-9.59424991709778,12.2,-4.20734169224021));
#270877=CARTESIAN_POINT('Ctrl Pts',(-9.59063068107566,12.2,-4.20641818910345));
#270878=CARTESIAN_POINT('Ctrl Pts',(-9.58707679118468,12.2,-4.20549868362322));
#270879=CARTESIAN_POINT('Ctrl Pts',(-9.58358910284248,12.2,-4.20458421777711));
#270880=CARTESIAN_POINT('Ctrl Pts',(-9.58059965534293,12.2,-4.20380038981747));
#270881=CARTESIAN_POINT('Ctrl Pts',(-9.57765884601473,12.2,-4.20302026229984));
#270882=CARTESIAN_POINT('Ctrl Pts',(-9.57476722835925,12.2,-4.20224450742441));
#270883=CARTESIAN_POINT('Ctrl Pts',(-9.57187561096643,12.2,-4.20146875261945));
#270884=CARTESIAN_POINT('Ctrl Pts',(-9.5690331816459,12.2,-4.200697371576));
#270885=CARTESIAN_POINT('Ctrl Pts',(-9.56624050723457,12.2,-4.19993105176702));
#270886=CARTESIAN_POINT('Ctrl Pts',(-9.56344783282325,12.2,-4.19916473195804));
#270887=CARTESIAN_POINT('Ctrl Pts',(-9.56070491039072,12.2,-4.19840347414696));
#270888=CARTESIAN_POINT('Ctrl Pts',(-9.55801231606847,12.2,-4.19764798759069));
#270889=CARTESIAN_POINT('Ctrl Pts',(-9.55531972150164,12.2,-4.19689250096579));
#270890=CARTESIAN_POINT('Ctrl Pts',(-9.55267745390051,12.2,-4.19614278658039));
#270891=CARTESIAN_POINT('Ctrl Pts',(-9.55008610146608,12.2,-4.19539957191979));
#270892=CARTESIAN_POINT('Ctrl Pts',(-9.54749474926703,12.2,-4.1946563573267));
#270893=CARTESIAN_POINT('Ctrl Pts',(-9.54495431257621,12.2,-4.1939196443235));
#270894=CARTESIAN_POINT('Ctrl Pts',(-9.54246538949996,12.2,-4.19319018001667));
#270895=CARTESIAN_POINT('Ctrl Pts',(-9.53997646642371,12.2,-4.19246071570983));
#270896=CARTESIAN_POINT('Ctrl Pts',(-9.53753905943302,12.2,-4.19173850167931));
#270897=CARTESIAN_POINT('Ctrl Pts',(-9.53515378023084,12.2,-4.19102431033578));
#270898=CARTESIAN_POINT('Ctrl Pts',(-9.532768500812,12.2,-4.19031011892737));
#270899=CARTESIAN_POINT('Ctrl Pts',(-9.53043534938044,12.2,-4.18960395015306));
#270900=CARTESIAN_POINT('Ctrl Pts',(-9.52815495700975,12.2,-4.18890659786566));
#270901=CARTESIAN_POINT('Ctrl Pts',(-9.52587456484618,12.2,-4.18820924564159));
#270902=CARTESIAN_POINT('Ctrl Pts',(-9.52364692716305,12.2,-4.18752071042808));
#270903=CARTESIAN_POINT('Ctrl Pts',(-9.52147269123231,12.2,-4.18684181128302));
#270904=CARTESIAN_POINT('Ctrl Pts',(-9.51929845530156,12.2,-4.18616291213796));
#270905=CARTESIAN_POINT('Ctrl Pts',(-9.51717761946508,12.2,-4.1854936485958));
#270906=CARTESIAN_POINT('Ctrl Pts',(-9.51511084262116,12.2,-4.18483486378594));
#270907=CARTESIAN_POINT('Ctrl Pts',(-9.51304406558951,12.2,-4.18417607891625));
#270908=CARTESIAN_POINT('Ctrl Pts',(-9.51103134861454,12.2,-4.18352777418118));
#270909=CARTESIAN_POINT('Ctrl Pts',(-9.50907336576156,12.2,-4.18289081914723));
#270910=CARTESIAN_POINT('Ctrl Pts',(-9.50711538308643,12.2,-4.18225386417116));
#270911=CARTESIAN_POINT('Ctrl Pts',(-9.50521213716328,12.2,-4.18162825895214));
#270912=CARTESIAN_POINT('Ctrl Pts',(-9.50336431839948,12.2,-4.18101490022495));
#270913=CARTESIAN_POINT('Ctrl Pts',(-9.5009094281732,12.2,-4.18020003224435));
#270914=CARTESIAN_POINT('Ctrl Pts',(-9.49855236068315,12.2,-4.17940677765138));
#270915=CARTESIAN_POINT('Ctrl Pts',(-9.49629481200006,12.2,-4.17863732200002));
#270916=CARTESIAN_POINT('Ctrl Pts',(-9.49629481200006,15.2,-4.17863732200002));
#270917=CARTESIAN_POINT('Ctrl Pts',(-9.49798593465032,15.2,-4.17921371881934));
#270918=CARTESIAN_POINT('Ctrl Pts',(-9.49973290438102,15.2,-4.17980347257967));
#270919=CARTESIAN_POINT('Ctrl Pts',(-9.50153500151926,15.2,-4.18040565840071));
#270920=CARTESIAN_POINT('Ctrl Pts',(-9.50334578928083,15.2,-4.18101074826615));
#270921=CARTESIAN_POINT('Ctrl Pts',(-9.5052122402571,15.2,-4.18162839186116));
#270922=CARTESIAN_POINT('Ctrl Pts',(-9.50713365521097,15.2,-4.1822576807609));
#270923=CARTESIAN_POINT('Ctrl Pts',(-9.50905506999029,15.2,-4.18288696960348));
#270924=CARTESIAN_POINT('Ctrl Pts',(-9.51103144900704,15.2,-4.18352790432366));
#270925=CARTESIAN_POINT('Ctrl Pts',(-9.51306211076662,15.2,-4.1841796053));
#270926=CARTESIAN_POINT('Ctrl Pts',(-9.5150927725262,15.2,-4.18483130627633));
#270927=CARTESIAN_POINT('Ctrl Pts',(-9.5171777169505,15.2,-4.18549377286806));
#270928=CARTESIAN_POINT('Ctrl Pts',(-9.51931627980988,15.2,-4.18616615495998));
#270929=CARTESIAN_POINT('Ctrl Pts',(-9.52145484286351,15.2,-4.18683853711298));
#270930=CARTESIAN_POINT('Ctrl Pts',(-9.5236470221604,15.2,-4.18752083260373));
#270931=CARTESIAN_POINT('Ctrl Pts',(-9.52589217403637,15.2,-4.18821221580869));
#270932=CARTESIAN_POINT('Ctrl Pts',(-9.52813732570841,15.2,-4.18890359895087));
#270933=CARTESIAN_POINT('Ctrl Pts',(-9.53043544305898,15.2,-4.18960406977284));
#270934=CARTESIAN_POINT('Ctrl Pts',(-9.53278589998437,15.2,-4.19031282325032));
#270935=CARTESIAN_POINT('Ctrl Pts',(-9.53513635690976,15.2,-4.1910215767278));
#270936=CARTESIAN_POINT('Ctrl Pts',(-9.53753914979115,15.2,-4.19173861702053));
#270937=CARTESIAN_POINT('Ctrl Pts',(-9.53999366086641,15.2,-4.19246316149388));
#270938=CARTESIAN_POINT('Ctrl Pts',(-9.54244817216462,15.2,-4.19318770603304));
#270939=CARTESIAN_POINT('Ctrl Pts',(-9.54495440171918,15.2,-4.1939197558398));
#270940=CARTESIAN_POINT('Ctrl Pts',(-9.54751174402873,15.2,-4.1946585525472));
#270941=CARTESIAN_POINT('Ctrl Pts',(-9.55006908610598,15.2,-4.1953973491875));
#270942=CARTESIAN_POINT('Ctrl Pts',(-9.55267754023118,15.2,-4.19614289582637));
#270943=CARTESIAN_POINT('Ctrl Pts',(-9.55533651838677,15.2,-4.19689445254932));
#270944=CARTESIAN_POINT('Ctrl Pts',(-9.5584386597293,15.2,-4.19777126877162));
#270945=CARTESIAN_POINT('Ctrl Pts',(-9.56160956564257,15.2,-4.19865626775237));
#270946=CARTESIAN_POINT('Ctrl Pts',(-9.5648483190859,15.2,-4.19954831685002));
#270947=CARTESIAN_POINT('Ctrl Pts',(-9.56762439332181,15.2,-4.2003129303226));
#270948=CARTESIAN_POINT('Ctrl Pts',(-9.57045031642585,15.2,-4.20108272011183));
#270949=CARTESIAN_POINT('Ctrl Pts',(-9.57332552165687,15.2,-4.20185699783389));
#270950=CARTESIAN_POINT('Ctrl Pts',(-9.57620072688789,15.2,-4.20263127555595));
#270951=CARTESIAN_POINT('Ctrl Pts',(-9.57912521616496,15.2,-4.20341004053597));
#270952=CARTESIAN_POINT('Ctrl Pts',(-9.5820984345548,15.2,-4.20419261550737));
#270953=CARTESIAN_POINT('Ctrl Pts',(-9.58507165294463,15.2,-4.20497519047877));
#270954=CARTESIAN_POINT('Ctrl Pts',(-9.58809360218851,15.2,-4.20576157844286));
#270955=CARTESIAN_POINT('Ctrl Pts',(-9.59116373765701,15.2,-4.20655112141395));
#270956=CARTESIAN_POINT('Ctrl Pts',(-9.59423387340437,15.2,-4.20734066445676));
#270957=CARTESIAN_POINT('Ctrl Pts',(-9.59735219801478,15.2,-4.20813336084157));
#270958=CARTESIAN_POINT('Ctrl Pts',(-9.60051817768938,15.2,-4.20892857480169));
#270959=CARTESIAN_POINT('Ctrl Pts',(-9.60368415707643,15.2,-4.20972378868958));
#270960=CARTESIAN_POINT('Ctrl Pts',(-9.60689779235132,15.2,-4.21052151836891));
#270961=CARTESIAN_POINT('Ctrl Pts',(-9.61015856181413,15.2,-4.21132113950644));
#270962=CARTESIAN_POINT('Ctrl Pts',(-9.61341933127693,15.2,-4.21212076064398));
#270963=CARTESIAN_POINT('Ctrl Pts',(-9.61672723454271,15.2,-4.2129222766751));
#270964=CARTESIAN_POINT('Ctrl Pts',(-9.62008176091767,15.2,-4.21372507597917));
#270965=CARTESIAN_POINT('Ctrl Pts',(-9.62343628759735,15.2,-4.21452787535618));
#270966=CARTESIAN_POINT('Ctrl Pts',(-9.62683743399816,15.2,-4.21533196143331));
#270967=CARTESIAN_POINT('Ctrl Pts',(-9.63028470168804,15.2,-4.21613673981054));
#270968=CARTESIAN_POINT('Ctrl Pts',(-9.6337319690648,15.2,-4.21694151811467));
#270969=CARTESIAN_POINT('Ctrl Pts',(-9.63722535415264,15.2,-4.21774698955026));
#270970=CARTESIAN_POINT('Ctrl Pts',(-9.64076436479004,15.2,-4.21855257777465));
#270971=CARTESIAN_POINT('Ctrl Pts',(-9.64430337542743,15.2,-4.21935816599903));
#270972=CARTESIAN_POINT('Ctrl Pts',(-9.64788801348929,15.2,-4.2201638697998));
#270973=CARTESIAN_POINT('Ctrl Pts',(-9.65151778835434,15.2,-4.22096912618724));
#270974=CARTESIAN_POINT('Ctrl Pts',(-9.65575252591672,15.2,-4.22190859202135));
#270975=CARTESIAN_POINT('Ctrl Pts',(-9.66004870645519,15.2,-4.22284744803079));
#270976=CARTESIAN_POINT('Ctrl Pts',(-9.66440556818162,15.2,-4.22378482329965));
#270977=CARTESIAN_POINT('Ctrl Pts',(-9.66814002089615,15.2,-4.22458828777411));
#270978=CARTESIAN_POINT('Ctrl Pts',(-9.67191905874185,15.2,-4.22539066415839));
#270979=CARTESIAN_POINT('Ctrl Pts',(-9.67574221059993,15.2,-4.2261914186294));
#270980=CARTESIAN_POINT('Ctrl Pts',(-9.67956536280529,15.2,-4.22699217317315));
#270981=CARTESIAN_POINT('Ctrl Pts',(-9.68343263213405,15.2,-4.22779130676898));
#270982=CARTESIAN_POINT('Ctrl Pts',(-9.68734355637842,15.2,-4.22858829460211));
#270983=CARTESIAN_POINT('Ctrl Pts',(-9.6906026597378,15.2,-4.22925245109352));
#270984=CARTESIAN_POINT('Ctrl Pts',(-9.69389207818172,15.2,-4.22991511941438));
#270985=CARTESIAN_POINT('Ctrl Pts',(-9.69721155068418,15.2,-4.23057600330313));
#270986=CARTESIAN_POINT('Ctrl Pts',(-9.70053102318663,15.2,-4.23123688719186));
#270987=CARTESIAN_POINT('Ctrl Pts',(-9.70388054947846,15.2,-4.23189598631391));
#270988=CARTESIAN_POINT('Ctrl Pts',(-9.70725987017534,15.2,-4.23255301103596));
#270989=CARTESIAN_POINT('Ctrl Pts',(-9.71063919050386,15.2,-4.23321003568639));
#270990=CARTESIAN_POINT('Ctrl Pts',(-9.71404830561634,15.2,-4.23386498646894));
#270991=CARTESIAN_POINT('Ctrl Pts',(-9.71748695780855,15.2,-4.23451757785633));
#270992=CARTESIAN_POINT('Ctrl Pts',(-9.72092561037556,15.2,-4.23517016931485));
#270993=CARTESIAN_POINT('Ctrl Pts',(-9.72439380244493,15.2,-4.23582040258733));
#270994=CARTESIAN_POINT('Ctrl Pts',(-9.72789127910919,15.2,-4.23646799744865));
#270995=CARTESIAN_POINT('Ctrl Pts',(-9.73138875577346,15.2,-4.23711559230997));
#270996=CARTESIAN_POINT('Ctrl Pts',(-9.73491551809502,15.2,-4.23776054943765));
#270997=CARTESIAN_POINT('Ctrl Pts',(-9.73847131660398,15.2,-4.23840259440048));
#270998=CARTESIAN_POINT('Ctrl Pts',(-9.74273827504728,15.2,-4.23917304839787));
#270999=CARTESIAN_POINT('Ctrl Pts',(-9.74704704402595,15.2,-4.23993930899185));
#271000=CARTESIAN_POINT('Ctrl Pts',(-9.75139719918249,15.2,-4.24070091386637));
#271001=CARTESIAN_POINT('Ctrl Pts',(-9.75502232828206,15.2,-4.24133558456055));
#271002=CARTESIAN_POINT('Ctrl Pts',(-9.75867619742377,15.2,-4.241967021088));
#271003=CARTESIAN_POINT('Ctrl Pts',(-9.76235856402332,15.2,-4.24259496032382));
#271004=CARTESIAN_POINT('Ctrl Pts',(-9.7660409302215,15.2,-4.2432228994912));
#271005=CARTESIAN_POINT('Ctrl Pts',(-9.76975179287081,15.2,-4.24384734318619));
#271006=CARTESIAN_POINT('Ctrl Pts',(-9.77349091100258,15.2,-4.24446803145217));
#271007=CARTESIAN_POINT('Ctrl Pts',(-9.77723002954193,15.2,-4.24508871978581));
#271008=CARTESIAN_POINT('Ctrl Pts',(-9.78099740646142,15.2,-4.24570565435842));
#271009=CARTESIAN_POINT('Ctrl Pts',(-9.78479280152856,15.2,-4.24631857942819));
#271010=CARTESIAN_POINT('Ctrl Pts',(-9.78858819659569,15.2,-4.24693150449795));
#271011=CARTESIAN_POINT('Ctrl Pts',(-9.792411609957,15.2,-4.24754042278821));
#271012=CARTESIAN_POINT('Ctrl Pts',(-9.79626280778635,15.2,-4.24814508288815));
#271013=CARTESIAN_POINT('Ctrl Pts',(-9.8001140056157,15.2,-4.2487497429881));
#271014=CARTESIAN_POINT('Ctrl Pts',(-9.80399298735165,15.2,-4.24935014658857));
#271015=CARTESIAN_POINT('Ctrl Pts',(-9.807899520753,15.2,-4.24994604839436));
#271016=CARTESIAN_POINT('Ctrl Pts',(-9.8125873610901,15.2,-4.25066113060029));
#271017=CARTESIAN_POINT('Ctrl Pts',(-9.8173148738238,15.2,-4.25136973113041));
#271018=CARTESIAN_POINT('Ctrl Pts',(-9.82208166525291,15.2,-4.25207143425151));
#271019=CARTESIAN_POINT('Ctrl Pts',(-9.82605399122733,15.2,-4.25265618682056));
#271020=CARTESIAN_POINT('Ctrl Pts',(-9.83005359423003,15.2,-4.25323615056453));
#271021=CARTESIAN_POINT('Ctrl Pts',(-9.83408024451002,15.2,-4.25381108980023));
#271022=CARTESIAN_POINT('Ctrl Pts',(-9.8381068943511,15.2,-4.25438602897326));
#271023=CARTESIAN_POINT('Ctrl Pts',(-9.84216059387434,15.2,-4.25495594343173));
#271024=CARTESIAN_POINT('Ctrl Pts',(-9.84624111773293,15.2,-4.25552060267617));
#271025=CARTESIAN_POINT('Ctrl Pts',(-9.8503216420363,15.2,-4.25608526198215));
#271026=CARTESIAN_POINT('Ctrl Pts',(-9.85442898980036,15.2,-4.25664466564936));
#271027=CARTESIAN_POINT('Ctrl Pts',(-9.85856294070094,15.2,-4.25719858738591));
#271028=CARTESIAN_POINT('Ctrl Pts',(-9.86187010160164,15.2,-4.25764172479931));
#271029=CARTESIAN_POINT('Ctrl Pts',(-9.86519428825217,15.2,-4.2580813537857));
#271030=CARTESIAN_POINT('Ctrl Pts',(-9.86853538672727,15.2,-4.25851735870032));
#271031=CARTESIAN_POINT('Ctrl Pts',(-9.87187648474714,15.2,-4.25895336355554));
#271032=CARTESIAN_POINT('Ctrl Pts',(-9.87523449661472,15.2,-4.25938574610627));
#271033=CARTESIAN_POINT('Ctrl Pts',(-9.87860930844822,15.2,-4.25981439223828));
#271034=CARTESIAN_POINT('Ctrl Pts',(-9.88198412074152,15.2,-4.26024303842869));
#271035=CARTESIAN_POINT('Ctrl Pts',(-9.88537573348923,15.2,-4.26066794827986));
#271036=CARTESIAN_POINT('Ctrl Pts',(-9.88878403650832,15.2,-4.26108901102503));
#271037=CARTESIAN_POINT('Ctrl Pts',(-9.8921923395274,15.2,-4.2615100737702));
#271038=CARTESIAN_POINT('Ctrl Pts',(-9.89561733290955,15.2,-4.26192728748992));
#271039=CARTESIAN_POINT('Ctrl Pts',(-9.89905890482103,15.2,-4.26234054506759));
#271040=CARTESIAN_POINT('Ctrl Pts',(-9.90250047626358,15.2,-4.26275380258896));
#271041=CARTESIAN_POINT('Ctrl Pts',(-9.90595862855205,15.2,-4.26316310312547));
#271042=CARTESIAN_POINT('Ctrl Pts',(-9.90943325100597,15.2,-4.26356833731642));
#271043=CARTESIAN_POINT('Ctrl Pts',(-9.9129078739333,15.2,-4.26397357156258));
#271044=CARTESIAN_POINT('Ctrl Pts',(-9.91639896647509,15.2,-4.26437473989929));
#271045=CARTESIAN_POINT('Ctrl Pts',(-9.91990642155681,15.2,-4.2647717360316));
#271046=CARTESIAN_POINT('Ctrl Pts',(-9.92341387616062,15.2,-4.26516873210983));
#271047=CARTESIAN_POINT('Ctrl Pts',(-9.92693769303174,15.2,-4.26556155464971));
#271048=CARTESIAN_POINT('Ctrl Pts',(-9.93047776368575,15.2,-4.26595009895156));
#271049=CARTESIAN_POINT('Ctrl Pts',(-9.93401783482209,15.2,-4.26633864330635));
#271050=CARTESIAN_POINT('Ctrl Pts',(-9.93757416057167,15.2,-4.26672290926028));
#271051=CARTESIAN_POINT('Ctrl Pts',(-9.9411466345018,15.2,-4.2671027935218));
#271052=CARTESIAN_POINT('Ctrl Pts',(-9.94471910794518,15.2,-4.26748267773156));
#271053=CARTESIAN_POINT('Ctrl Pts',(-9.94830772927064,15.2,-4.26785817911359));
#271054=CARTESIAN_POINT('Ctrl Pts',(-9.95191239069713,15.2,-4.26822919469466));
#271055=CARTESIAN_POINT('Ctrl Pts',(-9.95551705261475,15.2,-4.26860021032628));
#271056=CARTESIAN_POINT('Ctrl Pts',(-9.95913775748988,15.2,-4.26896674172404));
#271057=CARTESIAN_POINT('Ctrl Pts',(-9.96277439852244,15.2,-4.26932868602124));
#271058=CARTESIAN_POINT('Ctrl Pts',(-9.96641103905951,15.2,-4.26969063026913));
#271059=CARTESIAN_POINT('Ctrl Pts',(-9.970063615333,15.2,-4.27004798735964));
#271060=CARTESIAN_POINT('Ctrl Pts',(-9.97373202349277,15.2,-4.27040065768217));
#271061=CARTESIAN_POINT('Ctrl Pts',(-9.97740043215235,15.2,-4.27075332805274));
#271062=CARTESIAN_POINT('Ctrl Pts',(-9.98108467276382,15.2,-4.2711013117791));
#271063=CARTESIAN_POINT('Ctrl Pts',(-9.98478464124428,15.2,-4.27144450951971));
#271064=CARTESIAN_POINT('Ctrl Pts',(-9.98848460922063,15.2,-4.27178770721357));
#271065=CARTESIAN_POINT('Ctrl Pts',(-9.99220030512435,15.2,-4.27212612005838));
#271066=CARTESIAN_POINT('Ctrl Pts',(-9.99593162637327,15.2,-4.2724596484205));
#271067=CARTESIAN_POINT('Ctrl Pts',(-9.99966294813057,15.2,-4.27279317682806));
#271068=CARTESIAN_POINT('Ctrl Pts',(-10.0034098950776,15.2,-4.27312182422005));
#271069=CARTESIAN_POINT('Ctrl Pts',(-10.0071723642442,15.2,-4.27344549001692));
#271070=CARTESIAN_POINT('Ctrl Pts',(-10.0109348328982,15.2,-4.2737691557697));
#271071=CARTESIAN_POINT('Ctrl Pts',(-10.0147128244415,15.2,-4.27408784212387));
#271072=CARTESIAN_POINT('Ctrl Pts',(-10.0185062371298,15.2,-4.27440145443209));
#271073=CARTESIAN_POINT('Ctrl Pts',(-10.0222996503349,15.2,-4.27471506678303));
#271074=CARTESIAN_POINT('Ctrl Pts',(-10.0261084852055,15.2,-4.27502360426684));
#271075=CARTESIAN_POINT('Ctrl Pts',(-10.029932639025,15.2,-4.27532697328337));
#271076=CARTESIAN_POINT('Ctrl Pts',(-10.0337567928445,15.2,-4.2756303422999));
#271077=CARTESIAN_POINT('Ctrl Pts',(-10.0375962668992,15.2,-4.27592854345473));
#271078=CARTESIAN_POINT('Ctrl Pts',(-10.0414509613886,15.2,-4.27622148258126));
#271079=CARTESIAN_POINT('Ctrl Pts',(-10.0453056553528,15.2,-4.27651442166789));
#271080=CARTESIAN_POINT('Ctrl Pts',(-10.0491755684057,15.2,-4.2768020990494));
#271081=CARTESIAN_POINT('Ctrl Pts',(-10.0530606022724,15.2,-4.27708442524984));
#271082=CARTESIAN_POINT('Ctrl Pts',(-10.0569456366684,15.2,-4.27736675148875));
#271083=CARTESIAN_POINT('Ctrl Pts',(-10.0608457913308,15.2,-4.27764372328296));
#271084=CARTESIAN_POINT('Ctrl Pts',(-10.0647609666568,15.2,-4.27791525301943));
#271085=CARTESIAN_POINT('Ctrl Pts',(-10.0686761414494,15.2,-4.2781867827189));
#271086=CARTESIAN_POINT('Ctrl Pts',(-10.0726063385511,15.2,-4.27845286927185));
#271087=CARTESIAN_POINT('Ctrl Pts',(-10.0765514578943,15.2,-4.27871342369535));
#271088=CARTESIAN_POINT('Ctrl Pts',(-10.080496577775,15.2,-4.27897397815436));
#271089=CARTESIAN_POINT('Ctrl Pts',(-10.0844566198742,15.2,-4.27922900031341));
#271090=CARTESIAN_POINT('Ctrl Pts',(-10.0884314885685,15.2,-4.2794784020612));
#271091=CARTESIAN_POINT('Ctrl Pts',(-10.0924063567212,15.2,-4.279727803775));
#271092=CARTESIAN_POINT('Ctrl Pts',(-10.096396049365,15.2,-4.27997158488294));
#271093=CARTESIAN_POINT('Ctrl Pts',(-10.1004004706478,15.2,-4.28020965919719));
#271094=CARTESIAN_POINT('Ctrl Pts',(-10.1054059976604,15.2,-4.28050725211432));
#271095=CARTESIAN_POINT('Ctrl Pts',(-10.1104345373599,15.2,-4.280795926509));
#271096=CARTESIAN_POINT('Ctrl Pts',(-10.1154859011781,15.2,-4.28107551539837));
#271097=CARTESIAN_POINT('Ctrl Pts',(-10.1195269924529,15.2,-4.28129918652205));
#271098=CARTESIAN_POINT('Ctrl Pts',(-10.1235826926101,15.2,-4.2815170439367));
#271099=CARTESIAN_POINT('Ctrl Pts',(-10.1276529038329,15.2,-4.28172900055897));
#271100=CARTESIAN_POINT('Ctrl Pts',(-10.1317231145011,15.2,-4.28194095715237));
#271101=CARTESIAN_POINT('Ctrl Pts',(-10.1358078367674,15.2,-4.28214701488237));
#271102=CARTESIAN_POINT('Ctrl Pts',(-10.1399069769136,15.2,-4.28234708998764));
#271103=CARTESIAN_POINT('Ctrl Pts',(-10.1450309025152,15.2,-4.28259718388967));
#271104=CARTESIAN_POINT('Ctrl Pts',(-10.1501773539521,15.2,-4.28283792977325));
#271105=CARTESIAN_POINT('Ctrl Pts',(-10.1553461469371,15.2,-4.28306916546819));
#271106=CARTESIAN_POINT('Ctrl Pts',(-10.1594811815504,15.2,-4.28325415403423));
#271107=CARTESIAN_POINT('Ctrl Pts',(-10.1636305145293,15.2,-4.2834330567662));
#271108=CARTESIAN_POINT('Ctrl Pts',(-10.1677940530905,15.2,-4.28360579199743));
#271109=CARTESIAN_POINT('Ctrl Pts',(-10.1719575910844,15.2,-4.28377852720513));
#271110=CARTESIAN_POINT('Ctrl Pts',(-10.1761353339124,15.2,-4.28394509552296));
#271111=CARTESIAN_POINT('Ctrl Pts',(-10.1803271881668,15.2,-4.28410541601841));
#271112=CARTESIAN_POINT('Ctrl Pts',(-10.1855670064132,15.2,-4.2843058166541));
#271113=CARTESIAN_POINT('Ctrl Pts',(-10.1908288736391,15.2,-4.28449645575431));
#271114=CARTESIAN_POINT('Ctrl Pts',(-10.1961126098879,15.2,-4.28467717721316));
#271115=CARTESIAN_POINT('Ctrl Pts',(-10.2003395991174,15.2,-4.28482175438812));
#271116=CARTESIAN_POINT('Ctrl Pts',(-10.2045805838318,15.2,-4.2849599860651));
#271117=CARTESIAN_POINT('Ctrl Pts',(-10.208835472398,15.2,-4.28509179196076));
#271118=CARTESIAN_POINT('Ctrl Pts',(-10.2130903603844,15.2,-4.28522359783845));
#271119=CARTESIAN_POINT('Ctrl Pts',(-10.2173591515521,15.2,-4.28534897924708));
#271120=CARTESIAN_POINT('Ctrl Pts',(-10.221641755137,15.2,-4.28546785846609));
#271121=CARTESIAN_POINT('Ctrl Pts',(-10.2269950100557,15.2,-4.285616457502));
#271122=CARTESIAN_POINT('Ctrl Pts',(-10.2323698462372,15.2,-4.28575489680773));
#271123=CARTESIAN_POINT('Ctrl Pts',(-10.2377660858889,15.2,-4.2858830282666));
#271124=CARTESIAN_POINT('Ctrl Pts',(-10.2420830778455,15.2,-4.28598553343928));
#271125=CARTESIAN_POINT('Ctrl Pts',(-10.2464137683065,15.2,-4.28608144028063));
#271126=CARTESIAN_POINT('Ctrl Pts',(-10.2507580663219,15.2,-4.28617067550727));
#271127=CARTESIAN_POINT('Ctrl Pts',(-10.2551023637455,15.2,-4.28625991072176));
#271128=CARTESIAN_POINT('Ctrl Pts',(-10.2594602700253,15.2,-4.28634247359639));
#271129=CARTESIAN_POINT('Ctrl Pts',(-10.2638316936074,15.2,-4.286418290039));
#271130=CARTESIAN_POINT('Ctrl Pts',(-10.2692959735317,15.2,-4.28651306060003));
#271131=CARTESIAN_POINT('Ctrl Pts',(-10.2747813733467,15.2,-4.28659728756683));
#271132=CARTESIAN_POINT('Ctrl Pts',(-10.2802877236233,15.2,-4.28667083076183));
#271133=CARTESIAN_POINT('Ctrl Pts',(-10.2857940739,15.2,-4.28674437395684));
#271134=CARTESIAN_POINT('Ctrl Pts',(-10.2913213701106,15.2,-4.28680723204601));
#271135=CARTESIAN_POINT('Ctrl Pts',(-10.2968694391373,15.2,-4.28685926371324));
#271136=CARTESIAN_POINT('Ctrl Pts',(-10.3013078946005,15.2,-4.2869008890493));
#271137=CARTESIAN_POINT('Ctrl Pts',(-10.305759646986,15.2,-4.28693558648229));
#271138=CARTESIAN_POINT('Ctrl Pts',(-10.310224605898,15.2,-4.28696328376236));
#271139=CARTESIAN_POINT('Ctrl Pts',(-10.3135733247778,15.2,-4.28698405672052));
#271140=CARTESIAN_POINT('Ctrl Pts',(-10.3169294728717,15.2,-4.28700089251886));
#271141=CARTESIAN_POINT('Ctrl Pts',(-10.3202930125834,15.2,-4.28701376097638));
#271142=CARTESIAN_POINT('Ctrl Pts',(-10.3236565522952,15.2,-4.2870266294339));
#271143=CARTESIAN_POINT('Ctrl Pts',(-10.3270274840894,15.2,-4.28703553053356));
#271144=CARTESIAN_POINT('Ctrl Pts',(-10.3304057707583,15.2,-4.28704043499171));
#271145=CARTESIAN_POINT('Ctrl Pts',(-10.3337840574273,15.2,-4.28704533944986));
#271146=CARTESIAN_POINT('Ctrl Pts',(-10.3371696989875,15.2,-4.28704624758318));
#271147=CARTESIAN_POINT('Ctrl Pts',(-10.3405626591553,15.2,-4.28704313000032));
#271148=CARTESIAN_POINT('Ctrl Pts',(-10.3439556193231,15.2,-4.28704001241745));
#271149=CARTESIAN_POINT('Ctrl Pts',(-10.3473558971952,15.2,-4.28703286801852));
#271150=CARTESIAN_POINT('Ctrl Pts',(-10.3507634570741,15.2,-4.28702166947717));
#271151=CARTESIAN_POINT('Ctrl Pts',(-10.354171016953,15.2,-4.28701047093582));
#271152=CARTESIAN_POINT('Ctrl Pts',(-10.3575858588293,15.2,-4.28699521771966));
#271153=CARTESIAN_POINT('Ctrl Pts',(-10.3610079455373,15.2,-4.28697588072092));
#271154=CARTESIAN_POINT('Ctrl Pts',(-10.364430032867,15.2,-4.28695654371867));
#271155=CARTESIAN_POINT('Ctrl Pts',(-10.3678593656488,15.2,-4.2869331236986));
#271156=CARTESIAN_POINT('Ctrl Pts',(-10.3712959070242,15.2,-4.28690559073571));
#271157=CARTESIAN_POINT('Ctrl Pts',(-10.3758779611509,15.2,-4.28686888012685));
#271158=CARTESIAN_POINT('Ctrl Pts',(-10.3804728309398,15.2,-4.28682486137171));
#271159=CARTESIAN_POINT('Ctrl Pts',(-10.3850804303401,15.2,-4.28677346348751));
#271160=CARTESIAN_POINT('Ctrl Pts',(-10.3885361300473,15.2,-4.2867349150726));
#271161=CARTESIAN_POINT('Ctrl Pts',(-10.3919989904823,15.2,-4.28669221775923));
#271162=CARTESIAN_POINT('Ctrl Pts',(-10.3954689758204,15.2,-4.28664534275907));
#271163=CARTESIAN_POINT('Ctrl Pts',(-10.3989389611585,15.2,-4.28659846775892));
#271164=CARTESIAN_POINT('Ctrl Pts',(-10.4024160710514,15.2,-4.28654741552617));
#271165=CARTESIAN_POINT('Ctrl Pts',(-10.4059002692988,15.2,-4.28649215802875));
#271166=CARTESIAN_POINT('Ctrl Pts',(-10.4093844681792,15.2,-4.2864369005213));
#271167=CARTESIAN_POINT('Ctrl Pts',(-10.4128757560866,15.2,-4.28637743741266));
#271168=CARTESIAN_POINT('Ctrl Pts',(-10.416374096471,15.2,-4.28631374194449));
#271169=CARTESIAN_POINT('Ctrl Pts',(-10.4210385492576,15.2,-4.28622881467288));
#271170=CARTESIAN_POINT('Ctrl Pts',(-10.4257155408398,15.2,-4.28613636300781));
#271171=CARTESIAN_POINT('Ctrl Pts',(-10.4304049869001,15.2,-4.28603632351649));
#271172=CARTESIAN_POINT('Ctrl Pts',(-10.433922071605,15.2,-4.28596129389459));
#271173=CARTESIAN_POINT('Ctrl Pts',(-10.4374461613696,15.2,-4.28588199453348));
#271174=CARTESIAN_POINT('Ctrl Pts',(-10.4409772208336,15.2,-4.28579840003285));
#271175=CARTESIAN_POINT('Ctrl Pts',(-10.4445082802975,15.2,-4.28571480553221));
#271176=CARTESIAN_POINT('Ctrl Pts',(-10.4480463102736,15.2,-4.28562691523287));
#271177=CARTESIAN_POINT('Ctrl Pts',(-10.4515912749772,15.2,-4.28553470319514));
#271178=CARTESIAN_POINT('Ctrl Pts',(-10.4551362403248,15.2,-4.28544249114066));
#271179=CARTESIAN_POINT('Ctrl Pts',(-10.458688140191,15.2,-4.28534595605997));
#271180=CARTESIAN_POINT('Ctrl Pts',(-10.4622469395425,15.2,-4.28524507346138));
#271181=CARTESIAN_POINT('Ctrl Pts',(-10.4658057382475,15.2,-4.28514419088112));
#271182=CARTESIAN_POINT('Ctrl Pts',(-10.4693714358854,15.2,-4.28503895943442));
#271183=CARTESIAN_POINT('Ctrl Pts',(-10.4729439986312,15.2,-4.28492935297969));
#271184=CARTESIAN_POINT('Ctrl Pts',(-10.4777074154093,15.2,-4.28478321104668));
#271185=CARTESIAN_POINT('Ctrl Pts',(-10.4824830352626,15.2,-4.28462929291802));
#271186=CARTESIAN_POINT('Ctrl Pts',(-10.4872707759256,15.2,-4.28446753504316));
#271187=CARTESIAN_POINT('Ctrl Pts',(-10.4908615822381,15.2,-4.28434621660946));
#271188=CARTESIAN_POINT('Ctrl Pts',(-10.494459206711,15.2,-4.28422048939119));
#271189=CARTESIAN_POINT('Ctrl Pts',(-10.4980636140691,15.2,-4.284090326955));
#271190=CARTESIAN_POINT('Ctrl Pts',(-10.5028694894552,15.2,-4.28391677707949));
#271191=CARTESIAN_POINT('Ctrl Pts',(-10.5076874224697,15.2,-4.28373534306608));
#271192=CARTESIAN_POINT('Ctrl Pts',(-10.5125173337634,15.2,-4.28354596502517));
#271193=CARTESIAN_POINT('Ctrl Pts',(-10.5161397673982,15.2,-4.28340393148804));
#271194=CARTESIAN_POINT('Ctrl Pts',(-10.5197689368532,15.2,-4.28325742871055));
#271195=CARTESIAN_POINT('Ctrl Pts',(-10.5234048090538,15.2,-4.28310643179976));
#271196=CARTESIAN_POINT('Ctrl Pts',(-10.5270406812545,15.2,-4.28295543488898));
#271197=CARTESIAN_POINT('Ctrl Pts',(-10.530683256088,15.2,-4.28279994442849));
#271198=CARTESIAN_POINT('Ctrl Pts',(-10.5343324992461,15.2,-4.28263993501826));
#271199=CARTESIAN_POINT('Ctrl Pts',(-10.5379817430673,15.2,-4.28247992557895));
#271200=CARTESIAN_POINT('Ctrl Pts',(-10.5416376541653,15.2,-4.28231539797171));
#271201=CARTESIAN_POINT('Ctrl Pts',(-10.5453001995318,15.2,-4.28214632648818));
#271202=CARTESIAN_POINT('Ctrl Pts',(-10.5489627442329,15.2,-4.28197725503537));
#271203=CARTESIAN_POINT('Ctrl Pts',(-10.5526319228771,15.2,-4.28180363963515));
#271204=CARTESIAN_POINT('Ctrl Pts',(-10.5563077012613,15.2,-4.28162545671553));
#271205=CARTESIAN_POINT('Ctrl Pts',(-10.5599834796454,15.2,-4.28144727379591));
#271206=CARTESIAN_POINT('Ctrl Pts',(-10.5636658569023,15.2,-4.28126452353981));
#271207=CARTESIAN_POINT('Ctrl Pts',(-10.5673547996439,15.2,-4.28107717971288));
#271208=CARTESIAN_POINT('Ctrl Pts',(-10.5710437423854,15.2,-4.28088983588595));
#271209=CARTESIAN_POINT('Ctrl Pts',(-10.5747392502845,15.2,-4.28069790029291));
#271210=CARTESIAN_POINT('Ctrl Pts',(-10.578441290525,15.2,-4.28050134796672));
#271211=CARTESIAN_POINT('Ctrl Pts',(-10.5821433307655,15.2,-4.28030479564053));
#271212=CARTESIAN_POINT('Ctrl Pts',(-10.585851903114,15.2,-4.28010362866452));
#271213=CARTESIAN_POINT('Ctrl Pts',(-10.5895669738118,15.2,-4.27989782075574));
#271214=CARTESIAN_POINT('Ctrl Pts',(-10.5932820445096,15.2,-4.27969201284695));
#271215=CARTESIAN_POINT('Ctrl Pts',(-10.5970036129621,15.2,-4.27948156501067));
#271216=CARTESIAN_POINT('Ctrl Pts',(-10.6007316453038,15.2,-4.27926645254995));
#271217=CARTESIAN_POINT('Ctrl Pts',(-10.6044596776455,15.2,-4.27905134008923));
#271218=CARTESIAN_POINT('Ctrl Pts',(-10.6081941723546,15.2,-4.27883156294018));
#271219=CARTESIAN_POINT('Ctrl Pts',(-10.6119350967178,15.2,-4.27860709757398));
#271220=CARTESIAN_POINT('Ctrl Pts',(-10.6156760217606,15.2,-4.27838263216699));
#271221=CARTESIAN_POINT('Ctrl Pts',(-10.6194233779552,15.2,-4.27815347906703));
#271222=CARTESIAN_POINT('Ctrl Pts',(-10.6231771325433,15.2,-4.27791961719906));
#271223=CARTESIAN_POINT('Ctrl Pts',(-10.6269308864495,15.2,-4.27768575537358));
#271224=CARTESIAN_POINT('Ctrl Pts',(-10.6306910415803,15.2,-4.27744718588169));
#271225=CARTESIAN_POINT('Ctrl Pts',(-10.6344575621523,15.2,-4.27720388343178));
#271226=CARTESIAN_POINT('Ctrl Pts',(-10.6382240827244,15.2,-4.27696058098188));
#271227=CARTESIAN_POINT('Ctrl Pts',(-10.6419969666069,15.2,-4.27671254602513));
#271228=CARTESIAN_POINT('Ctrl Pts',(-10.6457761752368,15.2,-4.27645974949148));
#271229=CARTESIAN_POINT('Ctrl Pts',(-10.6495553838666,15.2,-4.27620695295783));
#271230=CARTESIAN_POINT('Ctrl Pts',(-10.6533409158171,15.2,-4.27594939275859));
#271231=CARTESIAN_POINT('Ctrl Pts',(-10.6571327397799,15.2,-4.27568705147528));
#271232=CARTESIAN_POINT('Ctrl Pts',(-10.6634524466141,15.2,-4.27524981598722));
#271233=CARTESIAN_POINT('Ctrl Pts',(-10.6697896272814,15.2,-4.27479929410113));
#271234=CARTESIAN_POINT('Ctrl Pts',(-10.6761442620001,15.2,-4.27433546900001));
#271235=CARTESIAN_POINT('Ctrl Pts',(-9.86852965800006,15.2,-3.20199116200001));
#271236=CARTESIAN_POINT('Ctrl Pts',(-9.86852965800006,11.6,-3.20199116200001));
#271237=CARTESIAN_POINT('Ctrl Pts',(-9.86869026600005,15.2,-3.20205902700001));
#271238=CARTESIAN_POINT('Ctrl Pts',(-9.86869026600005,11.6,-3.20205902700002));
#271239=CARTESIAN_POINT('Ctrl Pts',(-9.86901705900006,15.2,-3.20219720600001));
#271240=CARTESIAN_POINT('Ctrl Pts',(-9.86901705900006,11.6,-3.20219720600001));
#271241=CARTESIAN_POINT('Ctrl Pts',(-9.86951212500006,15.2,-3.20240682500001));
#271242=CARTESIAN_POINT('Ctrl Pts',(-9.86951212500006,11.6,-3.20240682500002));
#271243=CARTESIAN_POINT('Ctrl Pts',(-9.87017881200006,15.2,-3.20268969800001));
#271244=CARTESIAN_POINT('Ctrl Pts',(-9.87017881200006,11.6,-3.20268969800001));
#271245=CARTESIAN_POINT('Ctrl Pts',(-9.87102171700006,15.2,-3.20304833000002));
#271246=CARTESIAN_POINT('Ctrl Pts',(-9.87102171700006,11.6,-3.20304833000002));
#271247=CARTESIAN_POINT('Ctrl Pts',(-9.87187791600006,15.2,-3.20341363600001));
#271248=CARTESIAN_POINT('Ctrl Pts',(-9.87187791600006,11.6,-3.20341363600001));
#271249=CARTESIAN_POINT('Ctrl Pts',(-9.87274249600006,15.2,-3.20378354300002));
#271250=CARTESIAN_POINT('Ctrl Pts',(-9.87274249600006,11.6,-3.20378354300002));
#271251=CARTESIAN_POINT('Ctrl Pts',(-9.87361542500006,15.2,-3.20415805700001));
#271252=CARTESIAN_POINT('Ctrl Pts',(-9.87361542500006,11.6,-3.20415805700002));
#271253=CARTESIAN_POINT('Ctrl Pts',(-9.87449667000006,15.2,-3.20453718400001));
#271254=CARTESIAN_POINT('Ctrl Pts',(-9.87449667000006,11.6,-3.20453718400001));
#271255=CARTESIAN_POINT('Ctrl Pts',(-9.87538620100005,15.2,-3.20492093000002));
#271256=CARTESIAN_POINT('Ctrl Pts',(-9.87538620100005,11.6,-3.20492093000002));
#271257=CARTESIAN_POINT('Ctrl Pts',(-9.87628398500006,15.2,-3.20530930200002));
#271258=CARTESIAN_POINT('Ctrl Pts',(-9.87628398500006,11.6,-3.20530930200002));
#271259=CARTESIAN_POINT('Ctrl Pts',(-9.87718999100006,15.2,-3.20570230600001));
#271260=CARTESIAN_POINT('Ctrl Pts',(-9.87718999100006,11.6,-3.20570230600001));
#271261=CARTESIAN_POINT('Ctrl Pts',(-9.87810418900006,15.2,-3.20609994500002));
#271262=CARTESIAN_POINT('Ctrl Pts',(-9.87810418900006,11.6,-3.20609994500002));
#271263=CARTESIAN_POINT('Ctrl Pts',(-9.87902654600006,15.2,-3.20650222700001));
#271264=CARTESIAN_POINT('Ctrl Pts',(-9.87902654600006,11.6,-3.20650222700001));
#271265=CARTESIAN_POINT('Ctrl Pts',(-9.87995703200006,15.2,-3.20690915900002));
#271266=CARTESIAN_POINT('Ctrl Pts',(-9.87995703200006,11.6,-3.20690915900002));
#271267=CARTESIAN_POINT('Ctrl Pts',(-9.88089561700006,15.2,-3.20732074400001));
#271268=CARTESIAN_POINT('Ctrl Pts',(-9.88089561700006,11.6,-3.20732074400001));
#271269=CARTESIAN_POINT('Ctrl Pts',(-9.88184227000006,15.2,-3.20773698900001));
#271270=CARTESIAN_POINT('Ctrl Pts',(-9.88184227000006,11.6,-3.20773698900001));
#271271=CARTESIAN_POINT('Ctrl Pts',(-9.88279696000006,15.2,-3.20815790000001));
#271272=CARTESIAN_POINT('Ctrl Pts',(-9.88279696000006,11.6,-3.20815790000002));
#271273=CARTESIAN_POINT('Ctrl Pts',(-9.88375965700006,15.2,-3.20858348200002));
#271274=CARTESIAN_POINT('Ctrl Pts',(-9.88375965700006,11.6,-3.20858348200002));
#271275=CARTESIAN_POINT('Ctrl Pts',(-9.88473033100006,15.2,-3.20901374200002));
#271276=CARTESIAN_POINT('Ctrl Pts',(-9.88473033100006,11.6,-3.20901374200002));
#271277=CARTESIAN_POINT('Ctrl Pts',(-9.88570895100005,15.2,-3.20944868300002));
#271278=CARTESIAN_POINT('Ctrl Pts',(-9.88570895100005,11.6,-3.20944868300002));
#271279=CARTESIAN_POINT('Ctrl Pts',(-9.88669548900006,15.2,-3.20988831100002));
#271280=CARTESIAN_POINT('Ctrl Pts',(-9.88669548900006,11.6,-3.20988831100002));
#271281=CARTESIAN_POINT('Ctrl Pts',(-9.88768991400006,15.2,-3.21033263400002));
#271282=CARTESIAN_POINT('Ctrl Pts',(-9.88768991400006,11.6,-3.21033263400002));
#271283=CARTESIAN_POINT('Ctrl Pts',(-9.88869219600006,15.2,-3.21078165400001));
#271284=CARTESIAN_POINT('Ctrl Pts',(-9.88869219600006,11.6,-3.21078165400001));
#271285=CARTESIAN_POINT('Ctrl Pts',(-9.88970230600006,15.2,-3.21123537900001));
#271286=CARTESIAN_POINT('Ctrl Pts',(-9.88970230600006,11.6,-3.21123537900002));
#271287=CARTESIAN_POINT('Ctrl Pts',(-9.89072021400006,15.2,-3.21169381400002));
#271288=CARTESIAN_POINT('Ctrl Pts',(-9.89072021400006,11.6,-3.21169381400002));
#271289=CARTESIAN_POINT('Ctrl Pts',(-9.89174589300006,15.2,-3.21215696200001));
#271290=CARTESIAN_POINT('Ctrl Pts',(-9.89174589300006,11.6,-3.21215696200001));
#271291=CARTESIAN_POINT('Ctrl Pts',(-9.89277931200006,15.2,-3.21262483100002));
#271292=CARTESIAN_POINT('Ctrl Pts',(-9.89277931200006,11.6,-3.21262483100002));
#271293=CARTESIAN_POINT('Ctrl Pts',(-9.89382044300006,15.2,-3.21309742400001));
#271294=CARTESIAN_POINT('Ctrl Pts',(-9.89382044300006,11.6,-3.21309742400001));
#271295=CARTESIAN_POINT('Ctrl Pts',(-9.89486925600006,15.2,-3.21357474900001));
#271296=CARTESIAN_POINT('Ctrl Pts',(-9.89486925600006,11.6,-3.21357474900001));
#271297=CARTESIAN_POINT('Ctrl Pts',(-9.89592572400005,15.2,-3.21405680800002));
#271298=CARTESIAN_POINT('Ctrl Pts',(-9.89592572400005,11.6,-3.21405680800002));
#271299=CARTESIAN_POINT('Ctrl Pts',(-9.89698981700006,15.2,-3.21454360700002));
#271300=CARTESIAN_POINT('Ctrl Pts',(-9.89698981700006,11.6,-3.21454360700002));
#271301=CARTESIAN_POINT('Ctrl Pts',(-9.89806150700005,15.2,-3.21503515300002));
#271302=CARTESIAN_POINT('Ctrl Pts',(-9.89806150700005,11.6,-3.21503515300002));
#271303=CARTESIAN_POINT('Ctrl Pts',(-9.89914076600006,15.2,-3.21553144900002));
#271304=CARTESIAN_POINT('Ctrl Pts',(-9.89914076600006,11.6,-3.21553144900002));
#271305=CARTESIAN_POINT('Ctrl Pts',(-9.90022756600006,15.2,-3.21603250000001));
#271306=CARTESIAN_POINT('Ctrl Pts',(-9.90022756600006,11.6,-3.21603250000001));
#271307=CARTESIAN_POINT('Ctrl Pts',(-9.90132187900005,15.2,-3.21653831200001));
#271308=CARTESIAN_POINT('Ctrl Pts',(-9.90132187900005,11.6,-3.21653831200001));
#271309=CARTESIAN_POINT('Ctrl Pts',(-9.90242367500005,15.2,-3.21704889000001));
#271310=CARTESIAN_POINT('Ctrl Pts',(-9.90242367500005,11.6,-3.21704889000001));
#271311=CARTESIAN_POINT('Ctrl Pts',(-9.90353292900006,15.2,-3.21756423800001));
#271312=CARTESIAN_POINT('Ctrl Pts',(-9.90353292900006,11.6,-3.21756423800002));
#271313=CARTESIAN_POINT('Ctrl Pts',(-9.90464961300006,15.2,-3.21808436100001));
#271314=CARTESIAN_POINT('Ctrl Pts',(-9.90464961300006,11.6,-3.21808436100001));
#271315=CARTESIAN_POINT('Ctrl Pts',(-9.90577369800006,15.2,-3.21860926300001));
#271316=CARTESIAN_POINT('Ctrl Pts',(-9.90577369800006,11.6,-3.21860926300001));
#271317=CARTESIAN_POINT('Ctrl Pts',(-9.90690515800006,15.2,-3.21913895100002));
#271318=CARTESIAN_POINT('Ctrl Pts',(-9.90690515800006,11.6,-3.21913895100002));
#271319=CARTESIAN_POINT('Ctrl Pts',(-9.90804396400006,15.2,-3.21967342800002));
#271320=CARTESIAN_POINT('Ctrl Pts',(-9.90804396400006,11.6,-3.21967342800002));
#271321=CARTESIAN_POINT('Ctrl Pts',(-9.90919009200006,15.2,-3.22021269900001));
#271322=CARTESIAN_POINT('Ctrl Pts',(-9.90919009200006,11.6,-3.22021269900001));
#271323=CARTESIAN_POINT('Ctrl Pts',(-9.91034351100006,15.2,-3.22075677000001));
#271324=CARTESIAN_POINT('Ctrl Pts',(-9.91034351100006,11.6,-3.22075677000001));
#271325=CARTESIAN_POINT('Ctrl Pts',(-9.91150419600006,15.2,-3.22130564300001));
#271326=CARTESIAN_POINT('Ctrl Pts',(-9.91150419600006,11.6,-3.22130564300001));
#271327=CARTESIAN_POINT('Ctrl Pts',(-9.91267212100006,15.2,-3.22185932500001));
#271328=CARTESIAN_POINT('Ctrl Pts',(-9.91267212100006,11.6,-3.22185932500001));
#271329=CARTESIAN_POINT('Ctrl Pts',(-9.91384725800006,15.2,-3.22241781900001));
#271330=CARTESIAN_POINT('Ctrl Pts',(-9.91384725800006,11.6,-3.22241781900001));
#271331=CARTESIAN_POINT('Ctrl Pts',(-9.91502958100006,15.2,-3.22298113000001));
#271332=CARTESIAN_POINT('Ctrl Pts',(-9.91502958100006,11.6,-3.22298113000001));
#271333=CARTESIAN_POINT('Ctrl Pts',(-9.91621906300006,15.2,-3.22354926400001));
#271334=CARTESIAN_POINT('Ctrl Pts',(-9.91621906300006,11.6,-3.22354926400001));
#271335=CARTESIAN_POINT('Ctrl Pts',(-9.91741567800006,15.2,-3.22412222300001));
#271336=CARTESIAN_POINT('Ctrl Pts',(-9.91741567800006,11.6,-3.22412222300001));
#271337=CARTESIAN_POINT('Ctrl Pts',(-9.91861940000006,15.2,-3.22470001300001));
#271338=CARTESIAN_POINT('Ctrl Pts',(-9.91861940000006,11.6,-3.22470001300002));
#271339=CARTESIAN_POINT('Ctrl Pts',(-9.91983020200006,15.2,-3.22528263800002));
#271340=CARTESIAN_POINT('Ctrl Pts',(-9.91983020200006,11.6,-3.22528263800002));
#271341=CARTESIAN_POINT('Ctrl Pts',(-9.92104805900006,15.2,-3.22587010200001));
#271342=CARTESIAN_POINT('Ctrl Pts',(-9.92104805900006,11.6,-3.22587010200001));
#271343=CARTESIAN_POINT('Ctrl Pts',(-9.92227294400006,15.2,-3.22646241000001));
#271344=CARTESIAN_POINT('Ctrl Pts',(-9.92227294400006,11.6,-3.22646241000002));
#271345=CARTESIAN_POINT('Ctrl Pts',(-9.92350483300006,15.2,-3.22705956700001));
#271346=CARTESIAN_POINT('Ctrl Pts',(-9.92350483300006,11.6,-3.22705956700002));
#271347=CARTESIAN_POINT('Ctrl Pts',(-9.92474369700006,15.2,-3.22766157500002));
#271348=CARTESIAN_POINT('Ctrl Pts',(-9.92474369700006,11.6,-3.22766157500002));
#271349=CARTESIAN_POINT('Ctrl Pts',(-9.92598951400005,15.2,-3.22826844000002));
#271350=CARTESIAN_POINT('Ctrl Pts',(-9.92598951400005,11.6,-3.22826844000002));
#271351=CARTESIAN_POINT('Ctrl Pts',(-9.92724225800006,15.2,-3.22888016500002));
#271352=CARTESIAN_POINT('Ctrl Pts',(-9.92724225800006,11.6,-3.22888016500002));
#271353=CARTESIAN_POINT('Ctrl Pts',(-9.92850190000006,15.2,-3.22949675600002));
#271354=CARTESIAN_POINT('Ctrl Pts',(-9.92850190000006,11.6,-3.22949675600002));
#271355=CARTESIAN_POINT('Ctrl Pts',(-9.92976841900006,15.2,-3.23011821500002));
#271356=CARTESIAN_POINT('Ctrl Pts',(-9.92976841900006,11.6,-3.23011821500002));
#271357=CARTESIAN_POINT('Ctrl Pts',(-9.93104178800005,15.2,-3.23074454800001));
#271358=CARTESIAN_POINT('Ctrl Pts',(-9.93104178800005,11.6,-3.23074454800001));
#271359=CARTESIAN_POINT('Ctrl Pts',(-9.93232198100005,15.2,-3.23137575800001));
#271360=CARTESIAN_POINT('Ctrl Pts',(-9.93232198100005,11.6,-3.23137575800002));
#271361=CARTESIAN_POINT('Ctrl Pts',(-9.93360897600006,15.2,-3.23201184900002));
#271362=CARTESIAN_POINT('Ctrl Pts',(-9.93360897600006,11.6,-3.23201184900002));
#271363=CARTESIAN_POINT('Ctrl Pts',(-9.93490274500006,15.2,-3.23265282600001));
#271364=CARTESIAN_POINT('Ctrl Pts',(-9.93490274500006,11.6,-3.23265282600001));
#271365=CARTESIAN_POINT('Ctrl Pts',(-9.93620326500006,15.2,-3.23329869300002));
#271366=CARTESIAN_POINT('Ctrl Pts',(-9.93620326500006,11.6,-3.23329869300002));
#271367=CARTESIAN_POINT('Ctrl Pts',(-9.93751051000006,15.2,-3.23394945100001));
#271368=CARTESIAN_POINT('Ctrl Pts',(-9.93751051000006,11.6,-3.23394945100001));
#271369=CARTESIAN_POINT('Ctrl Pts',(-9.93882445700006,15.2,-3.23460510900001));
#271370=CARTESIAN_POINT('Ctrl Pts',(-9.93882445700006,11.6,-3.23460510900001));
#271371=CARTESIAN_POINT('Ctrl Pts',(-9.94014508100006,15.2,-3.23526566700002));
#271372=CARTESIAN_POINT('Ctrl Pts',(-9.94014508100006,11.6,-3.23526566700002));
#271373=CARTESIAN_POINT('Ctrl Pts',(-9.94147235700006,15.2,-3.23593113000001));
#271374=CARTESIAN_POINT('Ctrl Pts',(-9.94147235700006,11.6,-3.23593113000001));
#271375=CARTESIAN_POINT('Ctrl Pts',(-9.94280626000006,15.2,-3.23660150200002));
#271376=CARTESIAN_POINT('Ctrl Pts',(-9.94280626000006,11.6,-3.23660150200002));
#271377=CARTESIAN_POINT('Ctrl Pts',(-9.94414676800006,15.2,-3.23727678600001));
#271378=CARTESIAN_POINT('Ctrl Pts',(-9.94414676800006,11.6,-3.23727678600001));
#271379=CARTESIAN_POINT('Ctrl Pts',(-9.94549385600006,15.2,-3.23795698700001));
#271380=CARTESIAN_POINT('Ctrl Pts',(-9.94549385600006,11.6,-3.23795698700002));
#271381=CARTESIAN_POINT('Ctrl Pts',(-9.94684750000006,15.2,-3.23864211000001));
#271382=CARTESIAN_POINT('Ctrl Pts',(-9.94684750000006,11.6,-3.23864211000001));
#271383=CARTESIAN_POINT('Ctrl Pts',(-9.94820767500006,15.2,-3.23933215500002));
#271384=CARTESIAN_POINT('Ctrl Pts',(-9.94820767500006,11.6,-3.23933215500002));
#271385=CARTESIAN_POINT('Ctrl Pts',(-9.94957435800006,15.2,-3.24002712800001));
#271386=CARTESIAN_POINT('Ctrl Pts',(-9.94957435800006,11.6,-3.24002712800001));
#271387=CARTESIAN_POINT('Ctrl Pts',(-9.95094752700006,15.2,-3.24072703300001));
#271388=CARTESIAN_POINT('Ctrl Pts',(-9.95094752700006,11.6,-3.24072703300002));
#271389=CARTESIAN_POINT('Ctrl Pts',(-9.95232715600006,15.2,-3.24143187300002));
#271390=CARTESIAN_POINT('Ctrl Pts',(-9.95232715600006,11.6,-3.24143187300002));
#271391=CARTESIAN_POINT('Ctrl Pts',(-9.95371322300005,15.2,-3.24214165200001));
#271392=CARTESIAN_POINT('Ctrl Pts',(-9.95371322300005,11.6,-3.24214165200001));
#271393=CARTESIAN_POINT('Ctrl Pts',(-9.95510570200006,15.2,-3.24285637300001));
#271394=CARTESIAN_POINT('Ctrl Pts',(-9.95510570200006,11.6,-3.24285637300001));
#271395=CARTESIAN_POINT('Ctrl Pts',(-9.95650457300006,15.2,-3.24357604000001));
#271396=CARTESIAN_POINT('Ctrl Pts',(-9.95650457300006,11.6,-3.24357604000001));
#271397=CARTESIAN_POINT('Ctrl Pts',(-9.95790981200006,15.2,-3.24430065600001));
#271398=CARTESIAN_POINT('Ctrl Pts',(-9.95790981200006,11.6,-3.24430065600001));
#271399=CARTESIAN_POINT('Ctrl Pts',(-9.95932139400006,15.2,-3.24503022600001));
#271400=CARTESIAN_POINT('Ctrl Pts',(-9.95932139400006,11.6,-3.24503022600001));
#271401=CARTESIAN_POINT('Ctrl Pts',(-9.96073929800006,15.2,-3.24576475100002));
#271402=CARTESIAN_POINT('Ctrl Pts',(-9.96073929800006,11.6,-3.24576475100002));
#271403=CARTESIAN_POINT('Ctrl Pts',(-9.96216349900006,15.2,-3.24650423600001));
#271404=CARTESIAN_POINT('Ctrl Pts',(-9.96216349900006,11.6,-3.24650423600001));
#271405=CARTESIAN_POINT('Ctrl Pts',(-9.96359397600006,15.2,-3.24724868500001));
#271406=CARTESIAN_POINT('Ctrl Pts',(-9.96359397600006,11.6,-3.24724868500002));
#271407=CARTESIAN_POINT('Ctrl Pts',(-9.96503070500006,15.2,-3.24799810100002));
#271408=CARTESIAN_POINT('Ctrl Pts',(-9.96503070500006,11.6,-3.24799810100002));
#271409=CARTESIAN_POINT('Ctrl Pts',(-9.96647366400006,15.2,-3.24875248700002));
#271410=CARTESIAN_POINT('Ctrl Pts',(-9.96647366400006,11.6,-3.24875248700002));
#271411=CARTESIAN_POINT('Ctrl Pts',(-9.96792283000006,15.2,-3.24951184700002));
#271412=CARTESIAN_POINT('Ctrl Pts',(-9.96792283000006,11.6,-3.24951184700002));
#271413=CARTESIAN_POINT('Ctrl Pts',(-9.96937818100006,15.2,-3.25027618300001));
#271414=CARTESIAN_POINT('Ctrl Pts',(-9.96937818100006,11.6,-3.25027618300001));
#271415=CARTESIAN_POINT('Ctrl Pts',(-9.97083969300006,15.2,-3.25104549900002));
#271416=CARTESIAN_POINT('Ctrl Pts',(-9.97083969300006,11.6,-3.25104549900002));
#271417=CARTESIAN_POINT('Ctrl Pts',(-9.97230734500006,15.2,-3.25181979900002));
#271418=CARTESIAN_POINT('Ctrl Pts',(-9.97230734500006,11.6,-3.25181979900002));
#271419=CARTESIAN_POINT('Ctrl Pts',(-9.97378111500005,15.2,-3.25259908500001));
#271420=CARTESIAN_POINT('Ctrl Pts',(-9.97378111500005,11.6,-3.25259908500001));
#271421=CARTESIAN_POINT('Ctrl Pts',(-9.97526098000005,15.2,-3.25338336200002));
#271422=CARTESIAN_POINT('Ctrl Pts',(-9.97526098000005,11.6,-3.25338336200002));
#271423=CARTESIAN_POINT('Ctrl Pts',(-9.97674691800006,15.2,-3.25417263100002));
#271424=CARTESIAN_POINT('Ctrl Pts',(-9.97674691800006,11.6,-3.25417263100002));
#271425=CARTESIAN_POINT('Ctrl Pts',(-9.97823890700005,15.2,-3.25496689800001));
#271426=CARTESIAN_POINT('Ctrl Pts',(-9.97823890700005,11.6,-3.25496689800001));
#271427=CARTESIAN_POINT('Ctrl Pts',(-9.97973692500006,15.2,-3.25576616200001));
#271428=CARTESIAN_POINT('Ctrl Pts',(-9.97973692500006,11.6,-3.25576616200001));
#271429=CARTESIAN_POINT('Ctrl Pts',(-9.98124095000006,15.2,-3.25657043100001));
#271430=CARTESIAN_POINT('Ctrl Pts',(-9.98124095000006,11.6,-3.25657043100001));
#271431=CARTESIAN_POINT('Ctrl Pts',(-9.98275096100006,15.2,-3.25737970400001));
#271432=CARTESIAN_POINT('Ctrl Pts',(-9.98275096100006,11.6,-3.25737970400001));
#271433=CARTESIAN_POINT('Ctrl Pts',(-9.98426693400006,15.2,-3.25819398700002));
#271434=CARTESIAN_POINT('Ctrl Pts',(-9.98426693400006,11.6,-3.25819398700002));
#271435=CARTESIAN_POINT('Ctrl Pts',(-9.98578885000006,15.2,-3.25901328100001));
#271436=CARTESIAN_POINT('Ctrl Pts',(-9.98578885000006,11.6,-3.25901328100001));
#271437=CARTESIAN_POINT('Ctrl Pts',(-9.98731668700006,15.2,-3.25983759000001));
#271438=CARTESIAN_POINT('Ctrl Pts',(-9.98731668700006,11.6,-3.25983759000001));
#271439=CARTESIAN_POINT('Ctrl Pts',(-9.98885042200006,15.2,-3.26066691800001));
#271440=CARTESIAN_POINT('Ctrl Pts',(-9.98885042200006,11.6,-3.26066691800001));
#271441=CARTESIAN_POINT('Ctrl Pts',(-9.99039003500006,15.2,-3.26150126600002));
#271442=CARTESIAN_POINT('Ctrl Pts',(-9.99039003500006,11.6,-3.26150126600002));
#271443=CARTESIAN_POINT('Ctrl Pts',(-9.99193550400006,15.2,-3.26234063800001));
#271444=CARTESIAN_POINT('Ctrl Pts',(-9.99193550400006,11.6,-3.26234063800001));
#271445=CARTESIAN_POINT('Ctrl Pts',(-9.99348680900006,15.2,-3.26318503700001));
#271446=CARTESIAN_POINT('Ctrl Pts',(-9.99348680900006,11.6,-3.26318503700001));
#271447=CARTESIAN_POINT('Ctrl Pts',(-9.99504392600005,15.2,-3.26403446500001));
#271448=CARTESIAN_POINT('Ctrl Pts',(-9.99504392600005,11.6,-3.26403446500001));
#271449=CARTESIAN_POINT('Ctrl Pts',(-9.99660683700006,15.2,-3.26488892600001));
#271450=CARTESIAN_POINT('Ctrl Pts',(-9.99660683700006,11.6,-3.26488892600001));
#271451=CARTESIAN_POINT('Ctrl Pts',(-9.99817551900006,15.2,-3.26574842300001));
#271452=CARTESIAN_POINT('Ctrl Pts',(-9.99817551900006,11.6,-3.26574842300001));
#271453=CARTESIAN_POINT('Ctrl Pts',(-9.99974995100006,15.2,-3.26661295800001));
#271454=CARTESIAN_POINT('Ctrl Pts',(-9.99974995100006,11.6,-3.26661295800002));
#271455=CARTESIAN_POINT('Ctrl Pts',(-10.0013301140001,15.2,-3.26748253400002));
#271456=CARTESIAN_POINT('Ctrl Pts',(-10.0013301140001,11.6,-3.26748253400002));
#271457=CARTESIAN_POINT('Ctrl Pts',(-10.0029159850001,15.2,-3.26835715400001));
#271458=CARTESIAN_POINT('Ctrl Pts',(-10.0029159850001,11.6,-3.26835715400001));
#271459=CARTESIAN_POINT('Ctrl Pts',(-10.0045075450001,15.2,-3.26923682200002));
#271460=CARTESIAN_POINT('Ctrl Pts',(-10.0045075450001,11.6,-3.26923682200002));
#271461=CARTESIAN_POINT('Ctrl Pts',(-10.0061047720001,15.2,-3.27012153700001));
#271462=CARTESIAN_POINT('Ctrl Pts',(-10.0061047720001,11.6,-3.27012153700002));
#271463=CARTESIAN_POINT('Ctrl Pts',(-10.0077076460001,15.2,-3.27101130600001));
#271464=CARTESIAN_POINT('Ctrl Pts',(-10.0077076460001,11.6,-3.27101130600001));
#271465=CARTESIAN_POINT('Ctrl Pts',(-10.0093161470001,15.2,-3.27190613000001));
#271466=CARTESIAN_POINT('Ctrl Pts',(-10.0093161470001,11.6,-3.27190613000001));
#271467=CARTESIAN_POINT('Ctrl Pts',(-10.0109302540001,15.2,-3.27280601200002));
#271468=CARTESIAN_POINT('Ctrl Pts',(-10.0109302540001,11.6,-3.27280601200002));
#271469=CARTESIAN_POINT('Ctrl Pts',(-10.0125499470001,15.2,-3.27371095300002));
#271470=CARTESIAN_POINT('Ctrl Pts',(-10.0125499470001,11.6,-3.27371095300002));
#271471=CARTESIAN_POINT('Ctrl Pts',(-10.0141752040001,15.2,-3.27462095800001));
#271472=CARTESIAN_POINT('Ctrl Pts',(-10.0141752040001,11.6,-3.27462095800001));
#271473=CARTESIAN_POINT('Ctrl Pts',(-10.0158060070001,15.2,-3.27553602900001));
#271474=CARTESIAN_POINT('Ctrl Pts',(-10.0158060070001,11.6,-3.27553602900002));
#271475=CARTESIAN_POINT('Ctrl Pts',(-10.0174423360001,15.2,-3.27645616800002));
#271476=CARTESIAN_POINT('Ctrl Pts',(-10.0174423360001,11.6,-3.27645616800002));
#271477=CARTESIAN_POINT('Ctrl Pts',(-10.0190841680001,15.2,-3.27738137700001));
#271478=CARTESIAN_POINT('Ctrl Pts',(-10.0190841680001,11.6,-3.27738137700001));
#271479=CARTESIAN_POINT('Ctrl Pts',(-10.0207314860001,15.2,-3.27831166000002));
#271480=CARTESIAN_POINT('Ctrl Pts',(-10.0207314860001,11.6,-3.27831166000002));
#271481=CARTESIAN_POINT('Ctrl Pts',(-10.0223842680001,15.2,-3.27924701900002));
#271482=CARTESIAN_POINT('Ctrl Pts',(-10.0223842680001,11.6,-3.27924701900002));
#271483=CARTESIAN_POINT('Ctrl Pts',(-10.0240424950001,15.2,-3.28018745500001));
#271484=CARTESIAN_POINT('Ctrl Pts',(-10.0240424950001,11.6,-3.28018745500001));
#271485=CARTESIAN_POINT('Ctrl Pts',(-10.0257061490001,15.2,-3.28113297400002));
#271486=CARTESIAN_POINT('Ctrl Pts',(-10.0257061490001,11.6,-3.28113297400002));
#271487=CARTESIAN_POINT('Ctrl Pts',(-10.0273752060001,15.2,-3.28208357600001));
#271488=CARTESIAN_POINT('Ctrl Pts',(-10.0273752060001,11.6,-3.28208357600001));
#271489=CARTESIAN_POINT('Ctrl Pts',(-10.0290496500001,15.2,-3.28303926300002));
#271490=CARTESIAN_POINT('Ctrl Pts',(-10.0290496500001,11.6,-3.28303926300002));
#271491=CARTESIAN_POINT('Ctrl Pts',(-10.0307294600001,15.2,-3.28400003900001));
#271492=CARTESIAN_POINT('Ctrl Pts',(-10.0307294600001,11.6,-3.28400003900002));
#271493=CARTESIAN_POINT('Ctrl Pts',(-10.0324146170001,15.2,-3.28496590500002));
#271494=CARTESIAN_POINT('Ctrl Pts',(-10.0324146170001,11.6,-3.28496590500002));
#271495=CARTESIAN_POINT('Ctrl Pts',(-10.0341051000001,15.2,-3.28593686500001));
#271496=CARTESIAN_POINT('Ctrl Pts',(-10.0341051000001,11.6,-3.28593686500001));
#271497=CARTESIAN_POINT('Ctrl Pts',(-10.0358008910001,15.2,-3.28691292000002));
#271498=CARTESIAN_POINT('Ctrl Pts',(-10.0358008910001,11.6,-3.28691292000002));
#271499=CARTESIAN_POINT('Ctrl Pts',(-10.0375019710001,15.2,-3.28789407300001));
#271500=CARTESIAN_POINT('Ctrl Pts',(-10.0375019710001,11.6,-3.28789407300001));
#271501=CARTESIAN_POINT('Ctrl Pts',(-10.0392083190001,15.2,-3.28888032700001));
#271502=CARTESIAN_POINT('Ctrl Pts',(-10.0392083190001,11.6,-3.28888032700001));
#271503=CARTESIAN_POINT('Ctrl Pts',(-10.0409199180001,15.2,-3.28987168200001));
#271504=CARTESIAN_POINT('Ctrl Pts',(-10.0409199180001,11.6,-3.28987168200001));
#271505=CARTESIAN_POINT('Ctrl Pts',(-10.0426367470001,15.2,-3.29086814300001));
#271506=CARTESIAN_POINT('Ctrl Pts',(-10.0426367470001,11.6,-3.29086814300001));
#271507=CARTESIAN_POINT('Ctrl Pts',(-10.0443587870001,15.2,-3.29186971100001));
#271508=CARTESIAN_POINT('Ctrl Pts',(-10.0443587870001,11.6,-3.29186971100001));
#271509=CARTESIAN_POINT('Ctrl Pts',(-10.0460860200001,15.2,-3.29287638800002));
#271510=CARTESIAN_POINT('Ctrl Pts',(-10.0460860200001,11.6,-3.29287638800002));
#271511=CARTESIAN_POINT('Ctrl Pts',(-10.0478184260001,15.2,-3.29388817600002));
#271512=CARTESIAN_POINT('Ctrl Pts',(-10.0478184260001,11.6,-3.29388817600002));
#271513=CARTESIAN_POINT('Ctrl Pts',(-10.0495559880001,15.2,-3.29490507900001));
#271514=CARTESIAN_POINT('Ctrl Pts',(-10.0495559880001,11.6,-3.29490507900001));
#271515=CARTESIAN_POINT('Ctrl Pts',(-10.0512986840001,15.2,-3.29592709700002));
#271516=CARTESIAN_POINT('Ctrl Pts',(-10.0512986840001,11.6,-3.29592709700002));
#271517=CARTESIAN_POINT('Ctrl Pts',(-10.0530464980001,15.2,-3.29695423400001));
#271518=CARTESIAN_POINT('Ctrl Pts',(-10.0530464980001,11.6,-3.29695423400001));
#271519=CARTESIAN_POINT('Ctrl Pts',(-10.0547994090001,15.2,-3.29798649200002));
#271520=CARTESIAN_POINT('Ctrl Pts',(-10.0547994090001,11.6,-3.29798649200002));
#271521=CARTESIAN_POINT('Ctrl Pts',(-10.0565574010001,15.2,-3.29902387100002));
#271522=CARTESIAN_POINT('Ctrl Pts',(-10.0565574010001,11.6,-3.29902387100002));
#271523=CARTESIAN_POINT('Ctrl Pts',(-10.0583204520001,15.2,-3.30006637500002));
#271524=CARTESIAN_POINT('Ctrl Pts',(-10.0583204520001,11.6,-3.30006637500002));
#271525=CARTESIAN_POINT('Ctrl Pts',(-10.0600885460001,15.2,-3.30111400600002));
#271526=CARTESIAN_POINT('Ctrl Pts',(-10.0600885460001,11.6,-3.30111400600002));
#271527=CARTESIAN_POINT('Ctrl Pts',(-10.0618616650001,15.2,-3.30216676600001));
#271528=CARTESIAN_POINT('Ctrl Pts',(-10.0618616650001,11.6,-3.30216676600001));
#271529=CARTESIAN_POINT('Ctrl Pts',(-10.0636397890001,15.2,-3.30322465600001));
#271530=CARTESIAN_POINT('Ctrl Pts',(-10.0636397890001,11.6,-3.30322465600001));
#271531=CARTESIAN_POINT('Ctrl Pts',(-10.0654229000001,15.2,-3.30428768000001));
#271532=CARTESIAN_POINT('Ctrl Pts',(-10.0654229000001,11.6,-3.30428768000001));
#271533=CARTESIAN_POINT('Ctrl Pts',(-10.0672109790001,15.2,-3.30535583800001));
#271534=CARTESIAN_POINT('Ctrl Pts',(-10.0672109790001,11.6,-3.30535583800002));
#271535=CARTESIAN_POINT('Ctrl Pts',(-10.0690040090001,15.2,-3.30642913300002));
#271536=CARTESIAN_POINT('Ctrl Pts',(-10.0690040090001,11.6,-3.30642913300002));
#271537=CARTESIAN_POINT('Ctrl Pts',(-10.0708019710001,15.2,-3.30750756800001));
#271538=CARTESIAN_POINT('Ctrl Pts',(-10.0708019710001,11.6,-3.30750756800001));
#271539=CARTESIAN_POINT('Ctrl Pts',(-10.0726048470001,15.2,-3.30859114400001));
#271540=CARTESIAN_POINT('Ctrl Pts',(-10.0726048470001,11.6,-3.30859114400001));
#271541=CARTESIAN_POINT('Ctrl Pts',(-10.0744126190001,15.2,-3.30967986200001));
#271542=CARTESIAN_POINT('Ctrl Pts',(-10.0744126190001,11.6,-3.30967986200001));
#271543=CARTESIAN_POINT('Ctrl Pts',(-10.0762252700001,15.2,-3.31077372500001));
#271544=CARTESIAN_POINT('Ctrl Pts',(-10.0762252700001,11.6,-3.31077372500001));
#271545=CARTESIAN_POINT('Ctrl Pts',(-10.0780427800001,15.2,-3.31187273500001));
#271546=CARTESIAN_POINT('Ctrl Pts',(-10.0780427800001,11.6,-3.31187273500001));
#271547=CARTESIAN_POINT('Ctrl Pts',(-10.0798651330001,15.2,-3.31297689300001));
#271548=CARTESIAN_POINT('Ctrl Pts',(-10.0798651330001,11.6,-3.31297689300001));
#271549=CARTESIAN_POINT('Ctrl Pts',(-10.0816923090001,15.2,-3.31408620300001));
#271550=CARTESIAN_POINT('Ctrl Pts',(-10.0816923090001,11.6,-3.31408620300001));
#271551=CARTESIAN_POINT('Ctrl Pts',(-10.0835242930001,15.2,-3.31520066400001));
#271552=CARTESIAN_POINT('Ctrl Pts',(-10.0835242930001,11.6,-3.31520066400001));
#271553=CARTESIAN_POINT('Ctrl Pts',(-10.0853610650001,15.2,-3.31632027900001));
#271554=CARTESIAN_POINT('Ctrl Pts',(-10.0853610650001,11.6,-3.31632027900001));
#271555=CARTESIAN_POINT('Ctrl Pts',(-10.0872026080001,15.2,-3.31744505100001));
#271556=CARTESIAN_POINT('Ctrl Pts',(-10.0872026080001,11.6,-3.31744505100001));
#271557=CARTESIAN_POINT('Ctrl Pts',(-10.0890489030001,15.2,-3.31857498100002));
#271558=CARTESIAN_POINT('Ctrl Pts',(-10.0890489030001,11.6,-3.31857498100002));
#271559=CARTESIAN_POINT('Ctrl Pts',(-10.0908999360001,15.2,-3.31971007100002));
#271560=CARTESIAN_POINT('Ctrl Pts',(-10.0908999360001,11.6,-3.31971007100002));
#271561=CARTESIAN_POINT('Ctrl Pts',(-10.0927556870001,15.2,-3.32085032200002));
#271562=CARTESIAN_POINT('Ctrl Pts',(-10.0927556870001,11.6,-3.32085032200002));
#271563=CARTESIAN_POINT('Ctrl Pts',(-10.0946161380001,15.2,-3.32199573500001));
#271564=CARTESIAN_POINT('Ctrl Pts',(-10.0946161380001,11.6,-3.32199573500001));
#271565=CARTESIAN_POINT('Ctrl Pts',(-10.0964812720001,15.2,-3.32314631500001));
#271566=CARTESIAN_POINT('Ctrl Pts',(-10.0964812720001,11.6,-3.32314631500001));
#271567=CARTESIAN_POINT('Ctrl Pts',(-10.0983510720001,15.2,-3.32430206100002));
#271568=CARTESIAN_POINT('Ctrl Pts',(-10.0983510720001,11.6,-3.32430206100002));
#271569=CARTESIAN_POINT('Ctrl Pts',(-10.1002255210001,15.2,-3.32546297600001));
#271570=CARTESIAN_POINT('Ctrl Pts',(-10.1002255210001,11.6,-3.32546297600001));
#271571=CARTESIAN_POINT('Ctrl Pts',(-10.1021046020001,15.2,-3.32662906000001));
#271572=CARTESIAN_POINT('Ctrl Pts',(-10.1021046020001,11.6,-3.32662906000001));
#271573=CARTESIAN_POINT('Ctrl Pts',(-10.1039882970001,15.2,-3.32780031700001));
#271574=CARTESIAN_POINT('Ctrl Pts',(-10.1039882970001,11.6,-3.32780031700001));
#271575=CARTESIAN_POINT('Ctrl Pts',(-10.1058765880001,15.2,-3.32897674700002));
#271576=CARTESIAN_POINT('Ctrl Pts',(-10.1058765880001,11.6,-3.32897674700002));
#271577=CARTESIAN_POINT('Ctrl Pts',(-10.1077694590001,15.2,-3.33015835100001));
#271578=CARTESIAN_POINT('Ctrl Pts',(-10.1077694590001,11.6,-3.33015835100001));
#271579=CARTESIAN_POINT('Ctrl Pts',(-10.1096668940001,15.2,-3.33134513300001));
#271580=CARTESIAN_POINT('Ctrl Pts',(-10.1096668940001,11.6,-3.33134513300001));
#271581=CARTESIAN_POINT('Ctrl Pts',(-10.1115688740001,15.2,-3.33253709300001));
#271582=CARTESIAN_POINT('Ctrl Pts',(-10.1115688740001,11.6,-3.33253709300001));
#271583=CARTESIAN_POINT('Ctrl Pts',(-10.1134753840001,15.2,-3.33373423300001));
#271584=CARTESIAN_POINT('Ctrl Pts',(-10.1134753840001,11.6,-3.33373423300001));
#271585=CARTESIAN_POINT('Ctrl Pts',(-10.1153864040001,15.2,-3.33493655500002));
#271586=CARTESIAN_POINT('Ctrl Pts',(-10.1153864040001,11.6,-3.33493655500002));
#271587=CARTESIAN_POINT('Ctrl Pts',(-10.1173019210001,15.2,-3.33614406000001));
#271588=CARTESIAN_POINT('Ctrl Pts',(-10.1173019210001,11.6,-3.33614406000002));
#271589=CARTESIAN_POINT('Ctrl Pts',(-10.1192219160001,15.2,-3.33735675000002));
#271590=CARTESIAN_POINT('Ctrl Pts',(-10.1192219160001,11.6,-3.33735675000002));
#271591=CARTESIAN_POINT('Ctrl Pts',(-10.1211463720001,15.2,-3.33857462500001));
#271592=CARTESIAN_POINT('Ctrl Pts',(-10.1211463720001,11.6,-3.33857462500002));
#271593=CARTESIAN_POINT('Ctrl Pts',(-10.1230752720001,15.2,-3.33979768900001));
#271594=CARTESIAN_POINT('Ctrl Pts',(-10.1230752720001,11.6,-3.33979768900001));
#271595=CARTESIAN_POINT('Ctrl Pts',(-10.1250086010001,15.2,-3.34102594200001));
#271596=CARTESIAN_POINT('Ctrl Pts',(-10.1250086010001,11.6,-3.34102594200001));
#271597=CARTESIAN_POINT('Ctrl Pts',(-10.1269463420001,15.2,-3.34225938500001));
#271598=CARTESIAN_POINT('Ctrl Pts',(-10.1269463420001,11.6,-3.34225938500001));
#271599=CARTESIAN_POINT('Ctrl Pts',(-10.1288884770001,15.2,-3.34349802000002));
#271600=CARTESIAN_POINT('Ctrl Pts',(-10.1288884770001,11.6,-3.34349802000002));
#271601=CARTESIAN_POINT('Ctrl Pts',(-10.1308349920001,15.2,-3.34474185000001));
#271602=CARTESIAN_POINT('Ctrl Pts',(-10.1308349920001,11.6,-3.34474185000001));
#271603=CARTESIAN_POINT('Ctrl Pts',(-10.1327858680001,15.2,-3.34599087400001));
#271604=CARTESIAN_POINT('Ctrl Pts',(-10.1327858680001,11.6,-3.34599087400001));
#271605=CARTESIAN_POINT('Ctrl Pts',(-10.1347410890001,15.2,-3.34724509500001));
#271606=CARTESIAN_POINT('Ctrl Pts',(-10.1347410890001,11.6,-3.34724509500001));
#271607=CARTESIAN_POINT('Ctrl Pts',(-10.1367006410001,15.2,-3.34850451400001));
#271608=CARTESIAN_POINT('Ctrl Pts',(-10.1367006410001,11.6,-3.34850451400001));
#271609=CARTESIAN_POINT('Ctrl Pts',(-10.1386645040001,15.2,-3.34976913200002));
#271610=CARTESIAN_POINT('Ctrl Pts',(-10.1386645040001,11.6,-3.34976913200002));
#271611=CARTESIAN_POINT('Ctrl Pts',(-10.1406326650001,15.2,-3.35103895100001));
#271612=CARTESIAN_POINT('Ctrl Pts',(-10.1406326650001,11.6,-3.35103895100001));
#271613=CARTESIAN_POINT('Ctrl Pts',(-10.1426051060001,15.2,-3.35231397200001));
#271614=CARTESIAN_POINT('Ctrl Pts',(-10.1426051060001,11.6,-3.35231397200001));
#271615=CARTESIAN_POINT('Ctrl Pts',(-10.1445818110001,15.2,-3.35359419500001));
#271616=CARTESIAN_POINT('Ctrl Pts',(-10.1445818110001,11.6,-3.35359419500001));
#271617=CARTESIAN_POINT('Ctrl Pts',(-10.1465627640001,15.2,-3.35487962500002));
#271618=CARTESIAN_POINT('Ctrl Pts',(-10.1465627640001,11.6,-3.35487962500002));
#271619=CARTESIAN_POINT('Ctrl Pts',(-10.1485479490001,15.2,-3.35617026000001));
#271620=CARTESIAN_POINT('Ctrl Pts',(-10.1485479490001,11.6,-3.35617026000001));
#271621=CARTESIAN_POINT('Ctrl Pts',(-10.1505373510001,15.2,-3.35746610300002));
#271622=CARTESIAN_POINT('Ctrl Pts',(-10.1505373510001,11.6,-3.35746610300002));
#271623=CARTESIAN_POINT('Ctrl Pts',(-10.1525309520001,15.2,-3.35876715300001));
#271624=CARTESIAN_POINT('Ctrl Pts',(-10.1525309520001,11.6,-3.35876715300001));
#271625=CARTESIAN_POINT('Ctrl Pts',(-10.1545287380001,15.2,-3.36007341400002));
#271626=CARTESIAN_POINT('Ctrl Pts',(-10.1545287380001,11.6,-3.36007341400002));
#271627=CARTESIAN_POINT('Ctrl Pts',(-10.1565306900001,15.2,-3.36138488700001));
#271628=CARTESIAN_POINT('Ctrl Pts',(-10.1565306900001,11.6,-3.36138488700001));
#271629=CARTESIAN_POINT('Ctrl Pts',(-10.1585367960001,15.2,-3.36270157200001));
#271630=CARTESIAN_POINT('Ctrl Pts',(-10.1585367960001,11.6,-3.36270157200001));
#271631=CARTESIAN_POINT('Ctrl Pts',(-10.1605470380001,15.2,-3.36402347000002));
#271632=CARTESIAN_POINT('Ctrl Pts',(-10.1605470380001,11.6,-3.36402347000002));
#271633=CARTESIAN_POINT('Ctrl Pts',(-10.1625614000001,15.2,-3.36535058300001));
#271634=CARTESIAN_POINT('Ctrl Pts',(-10.1625614000001,11.6,-3.36535058300001));
#271635=CARTESIAN_POINT('Ctrl Pts',(-10.1645798690001,15.2,-3.36668291200001));
#271636=CARTESIAN_POINT('Ctrl Pts',(-10.1645798690001,11.6,-3.36668291200001));
#271637=CARTESIAN_POINT('Ctrl Pts',(-10.1666024250001,15.2,-3.36802045800002));
#271638=CARTESIAN_POINT('Ctrl Pts',(-10.1666024250001,11.6,-3.36802045800002));
#271639=CARTESIAN_POINT('Ctrl Pts',(-10.1686290550001,15.2,-3.36936322300001));
#271640=CARTESIAN_POINT('Ctrl Pts',(-10.1686290550001,11.6,-3.36936322300002));
#271641=CARTESIAN_POINT('Ctrl Pts',(-10.1706597440001,15.2,-3.37071120800001));
#271642=CARTESIAN_POINT('Ctrl Pts',(-10.1706597440001,11.6,-3.37071120800002));
#271643=CARTESIAN_POINT('Ctrl Pts',(-10.1726944750001,15.2,-3.37206441300001));
#271644=CARTESIAN_POINT('Ctrl Pts',(-10.1726944750001,11.6,-3.37206441300001));
#271645=CARTESIAN_POINT('Ctrl Pts',(-10.1747332320001,15.2,-3.37342284000002));
#271646=CARTESIAN_POINT('Ctrl Pts',(-10.1747332320001,11.6,-3.37342284000002));
#271647=CARTESIAN_POINT('Ctrl Pts',(-10.1767760010001,15.2,-3.37478649100001));
#271648=CARTESIAN_POINT('Ctrl Pts',(-10.1767760010001,11.6,-3.37478649100001));
#271649=CARTESIAN_POINT('Ctrl Pts',(-10.1788227660001,15.2,-3.37615536500001));
#271650=CARTESIAN_POINT('Ctrl Pts',(-10.1788227660001,11.6,-3.37615536500001));
#271651=CARTESIAN_POINT('Ctrl Pts',(-10.1808735120001,15.2,-3.37752946400002));
#271652=CARTESIAN_POINT('Ctrl Pts',(-10.1808735120001,11.6,-3.37752946400002));
#271653=CARTESIAN_POINT('Ctrl Pts',(-10.1829282230001,15.2,-3.37890879000001));
#271654=CARTESIAN_POINT('Ctrl Pts',(-10.1829282230001,11.6,-3.37890879000002));
#271655=CARTESIAN_POINT('Ctrl Pts',(-10.1849868840001,15.2,-3.38029334300002));
#271656=CARTESIAN_POINT('Ctrl Pts',(-10.1849868840001,11.6,-3.38029334300002));
#271657=CARTESIAN_POINT('Ctrl Pts',(-10.1870494800001,15.2,-3.38168312400001));
#271658=CARTESIAN_POINT('Ctrl Pts',(-10.1870494800001,11.6,-3.38168312400001));
#271659=CARTESIAN_POINT('Ctrl Pts',(-10.1891159950001,15.2,-3.38307813400001));
#271660=CARTESIAN_POINT('Ctrl Pts',(-10.1891159950001,11.6,-3.38307813400002));
#271661=CARTESIAN_POINT('Ctrl Pts',(-10.1911864150001,15.2,-3.38447837600001));
#271662=CARTESIAN_POINT('Ctrl Pts',(-10.1911864150001,11.6,-3.38447837600001));
#271663=CARTESIAN_POINT('Ctrl Pts',(-10.1932607240001,15.2,-3.38588384800001));
#271664=CARTESIAN_POINT('Ctrl Pts',(-10.1932607240001,11.6,-3.38588384800001));
#271665=CARTESIAN_POINT('Ctrl Pts',(-10.1953389060001,15.2,-3.38729455300002));
#271666=CARTESIAN_POINT('Ctrl Pts',(-10.1953389060001,11.6,-3.38729455300002));
#271667=CARTESIAN_POINT('Ctrl Pts',(-10.1974209480001,15.2,-3.38871049100002));
#271668=CARTESIAN_POINT('Ctrl Pts',(-10.1974209480001,11.6,-3.38871049100002));
#271669=CARTESIAN_POINT('Ctrl Pts',(-10.1995068350001,15.2,-3.39013166400001));
#271670=CARTESIAN_POINT('Ctrl Pts',(-10.1995068350001,11.6,-3.39013166400001));
#271671=CARTESIAN_POINT('Ctrl Pts',(-10.2015965500001,15.2,-3.39155807200001));
#271672=CARTESIAN_POINT('Ctrl Pts',(-10.2015965500001,11.6,-3.39155807200001));
#271673=CARTESIAN_POINT('Ctrl Pts',(-10.2036900790001,15.2,-3.39298971600002));
#271674=CARTESIAN_POINT('Ctrl Pts',(-10.2036900790001,11.6,-3.39298971600002));
#271675=CARTESIAN_POINT('Ctrl Pts',(-10.2057874080001,15.2,-3.39442659900001));
#271676=CARTESIAN_POINT('Ctrl Pts',(-10.2057874080001,11.6,-3.39442659900001));
#271677=CARTESIAN_POINT('Ctrl Pts',(-10.2078885200001,15.2,-3.39586871800002));
#271678=CARTESIAN_POINT('Ctrl Pts',(-10.2078885200001,11.6,-3.39586871800002));
#271679=CARTESIAN_POINT('Ctrl Pts',(-10.2099934030001,15.2,-3.39731607600001));
#271680=CARTESIAN_POINT('Ctrl Pts',(-10.2099934030001,11.6,-3.39731607600001));
#271681=CARTESIAN_POINT('Ctrl Pts',(-10.2121020400001,15.2,-3.39876867400001));
#271682=CARTESIAN_POINT('Ctrl Pts',(-10.2121020400001,11.6,-3.39876867400001));
#271683=CARTESIAN_POINT('Ctrl Pts',(-10.2142144180001,15.2,-3.40022651400002));
#271684=CARTESIAN_POINT('Ctrl Pts',(-10.2142144180001,11.6,-3.40022651400002));
#271685=CARTESIAN_POINT('Ctrl Pts',(-10.2163305200001,15.2,-3.40168959500001));
#271686=CARTESIAN_POINT('Ctrl Pts',(-10.2163305200001,11.6,-3.40168959500002));
#271687=CARTESIAN_POINT('Ctrl Pts',(-10.2184503330001,15.2,-3.40315791800001));
#271688=CARTESIAN_POINT('Ctrl Pts',(-10.2184503330001,11.6,-3.40315791800002));
#271689=CARTESIAN_POINT('Ctrl Pts',(-10.2205738430001,15.2,-3.40463148500001));
#271690=CARTESIAN_POINT('Ctrl Pts',(-10.2205738430001,11.6,-3.40463148500001));
#271691=CARTESIAN_POINT('Ctrl Pts',(-10.2227010340001,15.2,-3.40611029600002));
#271692=CARTESIAN_POINT('Ctrl Pts',(-10.2227010340001,11.6,-3.40611029600002));
#271693=CARTESIAN_POINT('Ctrl Pts',(-10.2248318930001,15.2,-3.40759435200002));
#271694=CARTESIAN_POINT('Ctrl Pts',(-10.2248318930001,11.6,-3.40759435200002));
#271695=CARTESIAN_POINT('Ctrl Pts',(-10.2269664030001,15.2,-3.40908365300002));
#271696=CARTESIAN_POINT('Ctrl Pts',(-10.2269664030001,11.6,-3.40908365300002));
#271697=CARTESIAN_POINT('Ctrl Pts',(-10.2291045510001,15.2,-3.41057820100001));
#271698=CARTESIAN_POINT('Ctrl Pts',(-10.2291045510001,11.6,-3.41057820100001));
#271699=CARTESIAN_POINT('Ctrl Pts',(-10.2312463240001,15.2,-3.41207799600001));
#271700=CARTESIAN_POINT('Ctrl Pts',(-10.2312463240001,11.6,-3.41207799600001));
#271701=CARTESIAN_POINT('Ctrl Pts',(-10.2333917050001,15.2,-3.41358304000002));
#271702=CARTESIAN_POINT('Ctrl Pts',(-10.2333917050001,11.6,-3.41358304000002));
#271703=CARTESIAN_POINT('Ctrl Pts',(-10.2355406810001,15.2,-3.41509333200001));
#271704=CARTESIAN_POINT('Ctrl Pts',(-10.2355406810001,11.6,-3.41509333200001));
#271705=CARTESIAN_POINT('Ctrl Pts',(-10.2376932380001,15.2,-3.41660887400002));
#271706=CARTESIAN_POINT('Ctrl Pts',(-10.2376932380001,11.6,-3.41660887400002));
#271707=CARTESIAN_POINT('Ctrl Pts',(-10.2398493600001,15.2,-3.41812966500001));
#271708=CARTESIAN_POINT('Ctrl Pts',(-10.2398493600001,11.6,-3.41812966500001));
#271709=CARTESIAN_POINT('Ctrl Pts',(-10.2420090360001,15.2,-3.41965571000001));
#271710=CARTESIAN_POINT('Ctrl Pts',(-10.2420090360001,11.6,-3.41965571000001));
#271711=CARTESIAN_POINT('Ctrl Pts',(-10.2441722480001,15.2,-3.42118700400002));
#271712=CARTESIAN_POINT('Ctrl Pts',(-10.2441722480001,11.6,-3.42118700400002));
#271713=CARTESIAN_POINT('Ctrl Pts',(-10.2463389840001,15.2,-3.42272355100001));
#271714=CARTESIAN_POINT('Ctrl Pts',(-10.2463389840001,11.6,-3.42272355100001));
#271715=CARTESIAN_POINT('Ctrl Pts',(-10.2485092300001,15.2,-3.42426535100001));
#271716=CARTESIAN_POINT('Ctrl Pts',(-10.2485092300001,11.6,-3.42426535100001));
#271717=CARTESIAN_POINT('Ctrl Pts',(-10.2506829710001,15.2,-3.42581240500001));
#271718=CARTESIAN_POINT('Ctrl Pts',(-10.2506829710001,11.6,-3.42581240500001));
#271719=CARTESIAN_POINT('Ctrl Pts',(-10.2528601940001,15.2,-3.42736471300002));
#271720=CARTESIAN_POINT('Ctrl Pts',(-10.2528601940001,11.6,-3.42736471300002));
#271721=CARTESIAN_POINT('Ctrl Pts',(-10.2550408840001,15.2,-3.42892227700001));
#271722=CARTESIAN_POINT('Ctrl Pts',(-10.2550408840001,11.6,-3.42892227700002));
#271723=CARTESIAN_POINT('Ctrl Pts',(-10.2572250270001,15.2,-3.43048509600001));
#271724=CARTESIAN_POINT('Ctrl Pts',(-10.2572250270001,11.6,-3.43048509600001));
#271725=CARTESIAN_POINT('Ctrl Pts',(-10.2594126090001,15.2,-3.43205317100002));
#271726=CARTESIAN_POINT('Ctrl Pts',(-10.2594126090001,11.6,-3.43205317100002));
#271727=CARTESIAN_POINT('Ctrl Pts',(-10.2616036170001,15.2,-3.43362650300001));
#271728=CARTESIAN_POINT('Ctrl Pts',(-10.2616036170001,11.6,-3.43362650300001));
#271729=CARTESIAN_POINT('Ctrl Pts',(-10.2637980370001,15.2,-3.43520509300001));
#271730=CARTESIAN_POINT('Ctrl Pts',(-10.2637980370001,11.6,-3.43520509300001));
#271731=CARTESIAN_POINT('Ctrl Pts',(-10.2659958540001,15.2,-3.43678894100002));
#271732=CARTESIAN_POINT('Ctrl Pts',(-10.2659958540001,11.6,-3.43678894100002));
#271733=CARTESIAN_POINT('Ctrl Pts',(-10.2681970550001,15.2,-3.43837804700001));
#271734=CARTESIAN_POINT('Ctrl Pts',(-10.2681970550001,11.6,-3.43837804700002));
#271735=CARTESIAN_POINT('Ctrl Pts',(-10.2704016260001,15.2,-3.43997241200002));
#271736=CARTESIAN_POINT('Ctrl Pts',(-10.2704016260001,11.6,-3.43997241200002));
#271737=CARTESIAN_POINT('Ctrl Pts',(-10.2726095530001,15.2,-3.44157203700002));
#271738=CARTESIAN_POINT('Ctrl Pts',(-10.2726095530001,11.6,-3.44157203700002));
#271739=CARTESIAN_POINT('Ctrl Pts',(-10.2748208240001,15.2,-3.44317692300002));
#271740=CARTESIAN_POINT('Ctrl Pts',(-10.2748208240001,11.6,-3.44317692300002));
#271741=CARTESIAN_POINT('Ctrl Pts',(-10.2770354230001,15.2,-3.44478706900002));
#271742=CARTESIAN_POINT('Ctrl Pts',(-10.2770354230001,11.6,-3.44478706900002));
#271743=CARTESIAN_POINT('Ctrl Pts',(-10.2792533370001,15.2,-3.44640247600001));
#271744=CARTESIAN_POINT('Ctrl Pts',(-10.2792533370001,11.6,-3.44640247600001));
#271745=CARTESIAN_POINT('Ctrl Pts',(-10.2814745530001,15.2,-3.44802314500001));
#271746=CARTESIAN_POINT('Ctrl Pts',(-10.2814745530001,11.6,-3.44802314500001));
#271747=CARTESIAN_POINT('Ctrl Pts',(-10.2836990580001,15.2,-3.44964907700001));
#271748=CARTESIAN_POINT('Ctrl Pts',(-10.2836990580001,11.6,-3.44964907700001));
#271749=CARTESIAN_POINT('Ctrl Pts',(-10.2859268370001,15.2,-3.45128027200001));
#271750=CARTESIAN_POINT('Ctrl Pts',(-10.2859268370001,11.6,-3.45128027200001));
#271751=CARTESIAN_POINT('Ctrl Pts',(-10.2881578770001,15.2,-3.45291672900002));
#271752=CARTESIAN_POINT('Ctrl Pts',(-10.2881578770001,11.6,-3.45291672900002));
#271753=CARTESIAN_POINT('Ctrl Pts',(-10.2903921640001,15.2,-3.45455845000001));
#271754=CARTESIAN_POINT('Ctrl Pts',(-10.2903921640001,11.6,-3.45455845000001));
#271755=CARTESIAN_POINT('Ctrl Pts',(-10.2926296860001,15.2,-3.45620543600001));
#271756=CARTESIAN_POINT('Ctrl Pts',(-10.2926296860001,11.6,-3.45620543600001));
#271757=CARTESIAN_POINT('Ctrl Pts',(-10.2948704290001,15.2,-3.45785768600001));
#271758=CARTESIAN_POINT('Ctrl Pts',(-10.2948704290001,11.6,-3.45785768600001));
#271759=CARTESIAN_POINT('Ctrl Pts',(-10.2971143780001,15.2,-3.45951520100002));
#271760=CARTESIAN_POINT('Ctrl Pts',(-10.2971143780001,11.6,-3.45951520100002));
#271761=CARTESIAN_POINT('Ctrl Pts',(-10.2993615220001,15.2,-3.46117798000002));
#271762=CARTESIAN_POINT('Ctrl Pts',(-10.2993615220001,11.6,-3.46117798000002));
#271763=CARTESIAN_POINT('Ctrl Pts',(-10.3016118470001,15.2,-3.46284602700001));
#271764=CARTESIAN_POINT('Ctrl Pts',(-10.3016118470001,11.6,-3.46284602700001));
#271765=CARTESIAN_POINT('Ctrl Pts',(-10.3038653390001,15.2,-3.46451933900001));
#271766=CARTESIAN_POINT('Ctrl Pts',(-10.3038653390001,11.6,-3.46451933900001));
#271767=CARTESIAN_POINT('Ctrl Pts',(-10.3061219850001,15.2,-3.46619791800002));
#271768=CARTESIAN_POINT('Ctrl Pts',(-10.3061219850001,11.6,-3.46619791800002));
#271769=CARTESIAN_POINT('Ctrl Pts',(-10.3083817730001,15.2,-3.46788176400001));
#271770=CARTESIAN_POINT('Ctrl Pts',(-10.3083817730001,11.6,-3.46788176400001));
#271771=CARTESIAN_POINT('Ctrl Pts',(-10.3106446870001,15.2,-3.46957087800002));
#271772=CARTESIAN_POINT('Ctrl Pts',(-10.3106446870001,11.6,-3.46957087800002));
#271773=CARTESIAN_POINT('Ctrl Pts',(-10.3129107160001,15.2,-3.47126525800002));
#271774=CARTESIAN_POINT('Ctrl Pts',(-10.3129107160001,11.6,-3.47126525800002));
#271775=CARTESIAN_POINT('Ctrl Pts',(-10.3151798480001,15.2,-3.47296490700002));
#271776=CARTESIAN_POINT('Ctrl Pts',(-10.3151798480001,11.6,-3.47296490700002));
#271777=CARTESIAN_POINT('Ctrl Pts',(-10.3174520670001,15.2,-3.47466982400002));
#271778=CARTESIAN_POINT('Ctrl Pts',(-10.3174520670001,11.6,-3.47466982400002));
#271779=CARTESIAN_POINT('Ctrl Pts',(-10.3197273620001,15.2,-3.47638001000002));
#271780=CARTESIAN_POINT('Ctrl Pts',(-10.3197273620001,11.6,-3.47638001000002));
#271781=CARTESIAN_POINT('Ctrl Pts',(-10.3220057200001,15.2,-3.47809546500002));
#271782=CARTESIAN_POINT('Ctrl Pts',(-10.3220057200001,11.6,-3.47809546500002));
#271783=CARTESIAN_POINT('Ctrl Pts',(-10.3242871260001,15.2,-3.47981618900001));
#271784=CARTESIAN_POINT('Ctrl Pts',(-10.3242871260001,11.6,-3.47981618900001));
#271785=CARTESIAN_POINT('Ctrl Pts',(-10.3265715690001,15.2,-3.48154218200001));
#271786=CARTESIAN_POINT('Ctrl Pts',(-10.3265715690001,11.6,-3.48154218200001));
#271787=CARTESIAN_POINT('Ctrl Pts',(-10.3288590360001,15.2,-3.48327344600001));
#271788=CARTESIAN_POINT('Ctrl Pts',(-10.3288590360001,11.6,-3.48327344600001));
#271789=CARTESIAN_POINT('Ctrl Pts',(-10.3311495120001,15.2,-3.48500997900001));
#271790=CARTESIAN_POINT('Ctrl Pts',(-10.3311495120001,11.6,-3.48500997900001));
#271791=CARTESIAN_POINT('Ctrl Pts',(-10.3334429860001,15.2,-3.48675178300001));
#271792=CARTESIAN_POINT('Ctrl Pts',(-10.3334429860001,11.6,-3.48675178300002));
#271793=CARTESIAN_POINT('Ctrl Pts',(-10.3357394460001,15.2,-3.48849885700002));
#271794=CARTESIAN_POINT('Ctrl Pts',(-10.3357394460001,11.6,-3.48849885700002));
#271795=CARTESIAN_POINT('Ctrl Pts',(-10.3380388780001,15.2,-3.49025120200002));
#271796=CARTESIAN_POINT('Ctrl Pts',(-10.3380388780001,11.6,-3.49025120200002));
#271797=CARTESIAN_POINT('Ctrl Pts',(-10.3403412680001,15.2,-3.49200881800002));
#271798=CARTESIAN_POINT('Ctrl Pts',(-10.3403412680001,11.6,-3.49200881800002));
#271799=CARTESIAN_POINT('Ctrl Pts',(-10.3426466050001,15.2,-3.49377170500001));
#271800=CARTESIAN_POINT('Ctrl Pts',(-10.3426466050001,11.6,-3.49377170500001));
#271801=CARTESIAN_POINT('Ctrl Pts',(-10.3449548750001,15.2,-3.49553986400001));
#271802=CARTESIAN_POINT('Ctrl Pts',(-10.3449548750001,11.6,-3.49553986400002));
#271803=CARTESIAN_POINT('Ctrl Pts',(-10.3472660680001,15.2,-3.49731329400001));
#271804=CARTESIAN_POINT('Ctrl Pts',(-10.3472660680001,11.6,-3.49731329400001));
#271805=CARTESIAN_POINT('Ctrl Pts',(-10.3495801680001,15.2,-3.49909199600001));
#271806=CARTESIAN_POINT('Ctrl Pts',(-10.3495801680001,11.6,-3.49909199600001));
#271807=CARTESIAN_POINT('Ctrl Pts',(-10.3518971640001,15.2,-3.50087597000002));
#271808=CARTESIAN_POINT('Ctrl Pts',(-10.3518971640001,11.6,-3.50087597000002));
#271809=CARTESIAN_POINT('Ctrl Pts',(-10.3542170430001,15.2,-3.50266521600001));
#271810=CARTESIAN_POINT('Ctrl Pts',(-10.3542170430001,11.6,-3.50266521600001));
#271811=CARTESIAN_POINT('Ctrl Pts',(-10.3565397920001,15.2,-3.50445973500001));
#271812=CARTESIAN_POINT('Ctrl Pts',(-10.3565397920001,11.6,-3.50445973500001));
#271813=CARTESIAN_POINT('Ctrl Pts',(-10.3588654000001,15.2,-3.50625952500002));
#271814=CARTESIAN_POINT('Ctrl Pts',(-10.3588654000001,11.6,-3.50625952500002));
#271815=CARTESIAN_POINT('Ctrl Pts',(-10.3611938520001,15.2,-3.50806458800001));
#271816=CARTESIAN_POINT('Ctrl Pts',(-10.3611938520001,11.6,-3.50806458800002));
#271817=CARTESIAN_POINT('Ctrl Pts',(-10.3635251390001,15.2,-3.50987492500002));
#271818=CARTESIAN_POINT('Ctrl Pts',(-10.3635251390001,11.6,-3.50987492500002));
#271819=CARTESIAN_POINT('Ctrl Pts',(-10.3658592460001,15.2,-3.51169053400001));
#271820=CARTESIAN_POINT('Ctrl Pts',(-10.3658592460001,11.6,-3.51169053400001));
#271821=CARTESIAN_POINT('Ctrl Pts',(-10.3681961610001,15.2,-3.51351141600002));
#271822=CARTESIAN_POINT('Ctrl Pts',(-10.3681961610001,11.6,-3.51351141600002));
#271823=CARTESIAN_POINT('Ctrl Pts',(-10.3705358710001,15.2,-3.51533757000002));
#271824=CARTESIAN_POINT('Ctrl Pts',(-10.3705358710001,11.6,-3.51533757000002));
#271825=CARTESIAN_POINT('Ctrl Pts',(-10.3728783650001,15.2,-3.51716899900001));
#271826=CARTESIAN_POINT('Ctrl Pts',(-10.3728783650001,11.6,-3.51716899900001));
#271827=CARTESIAN_POINT('Ctrl Pts',(-10.3752236290001,15.2,-3.51900569900002));
#271828=CARTESIAN_POINT('Ctrl Pts',(-10.3752236290001,11.6,-3.51900569900002));
#271829=CARTESIAN_POINT('Ctrl Pts',(-10.3775716530001,15.2,-3.52084767400001));
#271830=CARTESIAN_POINT('Ctrl Pts',(-10.3775716530001,11.6,-3.52084767400001));
#271831=CARTESIAN_POINT('Ctrl Pts',(-10.3799224230001,15.2,-3.52269492200001));
#271832=CARTESIAN_POINT('Ctrl Pts',(-10.3799224230001,11.6,-3.52269492200001));
#271833=CARTESIAN_POINT('Ctrl Pts',(-10.3822759270001,15.2,-3.52454744300001));
#271834=CARTESIAN_POINT('Ctrl Pts',(-10.3822759270001,11.6,-3.52454744300001));
#271835=CARTESIAN_POINT('Ctrl Pts',(-10.3846321520001,15.2,-3.52640523800002));
#271836=CARTESIAN_POINT('Ctrl Pts',(-10.3846321520001,11.6,-3.52640523800002));
#271837=CARTESIAN_POINT('Ctrl Pts',(-10.3869910880001,15.2,-3.52826830500002));
#271838=CARTESIAN_POINT('Ctrl Pts',(-10.3869910880001,11.6,-3.52826830500002));
#271839=CARTESIAN_POINT('Ctrl Pts',(-10.3893527210001,15.2,-3.53013664700002));
#271840=CARTESIAN_POINT('Ctrl Pts',(-10.3893527210001,11.6,-3.53013664700002));
#271841=CARTESIAN_POINT('Ctrl Pts',(-10.3917170390001,15.2,-3.53201026100002));
#271842=CARTESIAN_POINT('Ctrl Pts',(-10.3917170390001,11.6,-3.53201026100002));
#271843=CARTESIAN_POINT('Ctrl Pts',(-10.3940840300001,15.2,-3.53388914800002));
#271844=CARTESIAN_POINT('Ctrl Pts',(-10.3940840300001,11.6,-3.53388914800002));
#271845=CARTESIAN_POINT('Ctrl Pts',(-10.3964536830001,15.2,-3.53577331000002));
#271846=CARTESIAN_POINT('Ctrl Pts',(-10.3964536830001,11.6,-3.53577331000002));
#271847=CARTESIAN_POINT('Ctrl Pts',(-10.3988259850001,15.2,-3.53766274500002));
#271848=CARTESIAN_POINT('Ctrl Pts',(-10.3988259850001,11.6,-3.53766274500002));
#271849=CARTESIAN_POINT('Ctrl Pts',(-10.4012009230001,15.2,-3.53955745300001));
#271850=CARTESIAN_POINT('Ctrl Pts',(-10.4012009230001,11.6,-3.53955745300001));
#271851=CARTESIAN_POINT('Ctrl Pts',(-10.4035784870001,15.2,-3.54145743400001));
#271852=CARTESIAN_POINT('Ctrl Pts',(-10.4035784870001,11.6,-3.54145743400002));
#271853=CARTESIAN_POINT('Ctrl Pts',(-10.4059586630001,15.2,-3.54336268900001));
#271854=CARTESIAN_POINT('Ctrl Pts',(-10.4059586630001,11.6,-3.54336268900001));
#271855=CARTESIAN_POINT('Ctrl Pts',(-10.4083414410001,15.2,-3.54527321700001));
#271856=CARTESIAN_POINT('Ctrl Pts',(-10.4083414410001,11.6,-3.54527321700001));
#271857=CARTESIAN_POINT('Ctrl Pts',(-10.4107268080001,15.2,-3.54718901800001));
#271858=CARTESIAN_POINT('Ctrl Pts',(-10.4107268080001,11.6,-3.54718901800001));
#271859=CARTESIAN_POINT('Ctrl Pts',(-10.4131147520001,15.2,-3.54911009300002));
#271860=CARTESIAN_POINT('Ctrl Pts',(-10.4131147520001,11.6,-3.54911009300002));
#271861=CARTESIAN_POINT('Ctrl Pts',(-10.4155052600001,15.2,-3.55103644000001));
#271862=CARTESIAN_POINT('Ctrl Pts',(-10.4155052600001,11.6,-3.55103644000002));
#271863=CARTESIAN_POINT('Ctrl Pts',(-10.4178983230001,15.2,-3.55296805900001));
#271864=CARTESIAN_POINT('Ctrl Pts',(-10.4178983230001,11.6,-3.55296805900001));
#271865=CARTESIAN_POINT('Ctrl Pts',(-10.4202939270001,15.2,-3.55490495200002));
#271866=CARTESIAN_POINT('Ctrl Pts',(-10.4202939270001,11.6,-3.55490495200002));
#271867=CARTESIAN_POINT('Ctrl Pts',(-10.4226920610001,15.2,-3.55684711800001));
#271868=CARTESIAN_POINT('Ctrl Pts',(-10.4226920610001,11.6,-3.55684711800001));
#271869=CARTESIAN_POINT('Ctrl Pts',(-10.4250927130001,15.2,-3.55879455600002));
#271870=CARTESIAN_POINT('Ctrl Pts',(-10.4250927130001,11.6,-3.55879455600002));
#271871=CARTESIAN_POINT('Ctrl Pts',(-10.4274958710001,15.2,-3.56074726700002));
#271872=CARTESIAN_POINT('Ctrl Pts',(-10.4274958710001,11.6,-3.56074726700002));
#271873=CARTESIAN_POINT('Ctrl Pts',(-10.4299015240001,15.2,-3.56270525000001));
#271874=CARTESIAN_POINT('Ctrl Pts',(-10.4299015240001,11.6,-3.56270525000001));
#271875=CARTESIAN_POINT('Ctrl Pts',(-10.4323096600001,15.2,-3.56466850500002));
#271876=CARTESIAN_POINT('Ctrl Pts',(-10.4323096600001,11.6,-3.56466850500002));
#271877=CARTESIAN_POINT('Ctrl Pts',(-10.4347202660001,15.2,-3.56663703300002));
#271878=CARTESIAN_POINT('Ctrl Pts',(-10.4347202660001,11.6,-3.56663703300002));
#271879=CARTESIAN_POINT('Ctrl Pts',(-10.4371333320001,15.2,-3.56861083100001));
#271880=CARTESIAN_POINT('Ctrl Pts',(-10.4371333320001,11.6,-3.56861083100001));
#271881=CARTESIAN_POINT('Ctrl Pts',(-10.4395488460001,15.2,-3.57058990100001));
#271882=CARTESIAN_POINT('Ctrl Pts',(-10.4395488460001,11.6,-3.57058990100001));
#271883=CARTESIAN_POINT('Ctrl Pts',(-10.4419667960001,15.2,-3.57257424500002));
#271884=CARTESIAN_POINT('Ctrl Pts',(-10.4419667960001,11.6,-3.57257424500002));
#271885=CARTESIAN_POINT('Ctrl Pts',(-10.4443871710001,15.2,-3.57456385800001));
#271886=CARTESIAN_POINT('Ctrl Pts',(-10.4443871710001,11.6,-3.57456385800001));
#271887=CARTESIAN_POINT('Ctrl Pts',(-10.4468099580001,15.2,-3.57655874200002));
#271888=CARTESIAN_POINT('Ctrl Pts',(-10.4468099580001,11.6,-3.57655874200002));
#271889=CARTESIAN_POINT('Ctrl Pts',(-10.4492351490001,15.2,-3.57855889700001));
#271890=CARTESIAN_POINT('Ctrl Pts',(-10.4492351490001,11.6,-3.57855889700002));
#271891=CARTESIAN_POINT('Ctrl Pts',(-10.4516627280001,15.2,-3.58056432300002));
#271892=CARTESIAN_POINT('Ctrl Pts',(-10.4516627280001,11.6,-3.58056432300002));
#271893=CARTESIAN_POINT('Ctrl Pts',(-10.4540926860001,15.2,-3.58257502100002));
#271894=CARTESIAN_POINT('Ctrl Pts',(-10.4540926860001,11.6,-3.58257502100002));
#271895=CARTESIAN_POINT('Ctrl Pts',(-10.4565250110001,15.2,-3.58459098700001));
#271896=CARTESIAN_POINT('Ctrl Pts',(-10.4565250110001,11.6,-3.58459098700001));
#271897=CARTESIAN_POINT('Ctrl Pts',(-10.4589596920001,15.2,-3.58661222400002));
#271898=CARTESIAN_POINT('Ctrl Pts',(-10.4589596920001,11.6,-3.58661222400002));
#271899=CARTESIAN_POINT('Ctrl Pts',(-10.4613967180001,15.2,-3.58863873100002));
#271900=CARTESIAN_POINT('Ctrl Pts',(-10.4613967180001,11.6,-3.58863873100002));
#271901=CARTESIAN_POINT('Ctrl Pts',(-10.4638360760001,15.2,-3.59067050700002));
#271902=CARTESIAN_POINT('Ctrl Pts',(-10.4638360760001,11.6,-3.59067050700002));
#271903=CARTESIAN_POINT('Ctrl Pts',(-10.4662777560001,15.2,-3.59270755200002));
#271904=CARTESIAN_POINT('Ctrl Pts',(-10.4662777560001,11.6,-3.59270755200002));
#271905=CARTESIAN_POINT('Ctrl Pts',(-10.4687217460001,15.2,-3.59474986700001));
#271906=CARTESIAN_POINT('Ctrl Pts',(-10.4687217460001,11.6,-3.59474986700001));
#271907=CARTESIAN_POINT('Ctrl Pts',(-10.4711680340001,15.2,-3.59679744900001));
#271908=CARTESIAN_POINT('Ctrl Pts',(-10.4711680340001,11.6,-3.59679744900001));
#271909=CARTESIAN_POINT('Ctrl Pts',(-10.4736166110001,15.2,-3.59885030100001));
#271910=CARTESIAN_POINT('Ctrl Pts',(-10.4736166110001,11.6,-3.59885030100001));
#271911=CARTESIAN_POINT('Ctrl Pts',(-10.4760674640001,15.2,-3.60090842000002));
#271912=CARTESIAN_POINT('Ctrl Pts',(-10.4760674640001,11.6,-3.60090842000002));
#271913=CARTESIAN_POINT('Ctrl Pts',(-10.4785205830001,15.2,-3.60297180700002));
#271914=CARTESIAN_POINT('Ctrl Pts',(-10.4785205830001,11.6,-3.60297180700002));
#271915=CARTESIAN_POINT('Ctrl Pts',(-10.4809759550001,15.2,-3.60504046200001));
#271916=CARTESIAN_POINT('Ctrl Pts',(-10.4809759550001,11.6,-3.60504046200001));
#271917=CARTESIAN_POINT('Ctrl Pts',(-10.4834335690001,15.2,-3.60711438300001));
#271918=CARTESIAN_POINT('Ctrl Pts',(-10.4834335690001,11.6,-3.60711438300001));
#271919=CARTESIAN_POINT('Ctrl Pts',(-10.4858934160001,15.2,-3.60919357300002));
#271920=CARTESIAN_POINT('Ctrl Pts',(-10.4858934160001,11.6,-3.60919357300002));
#271921=CARTESIAN_POINT('Ctrl Pts',(-10.4883554830001,15.2,-3.61127802800001));
#271922=CARTESIAN_POINT('Ctrl Pts',(-10.4883554830001,11.6,-3.61127802800001));
#271923=CARTESIAN_POINT('Ctrl Pts',(-10.4908197590001,15.2,-3.61336774900002));
#271924=CARTESIAN_POINT('Ctrl Pts',(-10.4908197590001,11.6,-3.61336774900002));
#271925=CARTESIAN_POINT('Ctrl Pts',(-10.4932862330001,15.2,-3.61546273600001));
#271926=CARTESIAN_POINT('Ctrl Pts',(-10.4932862330001,11.6,-3.61546273600002));
#271927=CARTESIAN_POINT('Ctrl Pts',(-10.4957548950001,15.2,-3.61756298900001));
#271928=CARTESIAN_POINT('Ctrl Pts',(-10.4957548950001,11.6,-3.61756298900001));
#271929=CARTESIAN_POINT('Ctrl Pts',(-10.4982257320001,15.2,-3.61966850600002));
#271930=CARTESIAN_POINT('Ctrl Pts',(-10.4982257320001,11.6,-3.61966850600002));
#271931=CARTESIAN_POINT('Ctrl Pts',(-10.5006987350001,15.2,-3.62177928800001));
#271932=CARTESIAN_POINT('Ctrl Pts',(-10.5006987350001,11.6,-3.62177928800001));
#271933=CARTESIAN_POINT('Ctrl Pts',(-10.5031738910001,15.2,-3.62389533400002));
#271934=CARTESIAN_POINT('Ctrl Pts',(-10.5031738910001,11.6,-3.62389533400002));
#271935=CARTESIAN_POINT('Ctrl Pts',(-10.5056511920001,15.2,-3.62601664500001));
#271936=CARTESIAN_POINT('Ctrl Pts',(-10.5056511920001,11.6,-3.62601664500001));
#271937=CARTESIAN_POINT('Ctrl Pts',(-10.5081306230001,15.2,-3.62814321800002));
#271938=CARTESIAN_POINT('Ctrl Pts',(-10.5081306230001,11.6,-3.62814321800002));
#271939=CARTESIAN_POINT('Ctrl Pts',(-10.5106121760001,15.2,-3.63027505600002));
#271940=CARTESIAN_POINT('Ctrl Pts',(-10.5106121760001,11.6,-3.63027505600002));
#271941=CARTESIAN_POINT('Ctrl Pts',(-10.5130958400001,15.2,-3.63241215500001));
#271942=CARTESIAN_POINT('Ctrl Pts',(-10.5130958400001,11.6,-3.63241215500001));
#271943=CARTESIAN_POINT('Ctrl Pts',(-10.5155816020001,15.2,-3.63455451700001));
#271944=CARTESIAN_POINT('Ctrl Pts',(-10.5155816020001,11.6,-3.63455451700002));
#271945=CARTESIAN_POINT('Ctrl Pts',(-10.5180694530001,15.2,-3.63670214000001));
#271946=CARTESIAN_POINT('Ctrl Pts',(-10.5180694530001,11.6,-3.63670214000001));
#271947=CARTESIAN_POINT('Ctrl Pts',(-10.5205593820001,15.2,-3.63885502500001));
#271948=CARTESIAN_POINT('Ctrl Pts',(-10.5205593820001,11.6,-3.63885502500001));
#271949=CARTESIAN_POINT('Ctrl Pts',(-10.5230513770001,15.2,-3.64101317100001));
#271950=CARTESIAN_POINT('Ctrl Pts',(-10.5230513770001,11.6,-3.64101317100001));
#271951=CARTESIAN_POINT('Ctrl Pts',(-10.5255454300001,15.2,-3.64317657700001));
#271952=CARTESIAN_POINT('Ctrl Pts',(-10.5255454300001,11.6,-3.64317657700001));
#271953=CARTESIAN_POINT('Ctrl Pts',(-10.5280415260001,15.2,-3.64534524300002));
#271954=CARTESIAN_POINT('Ctrl Pts',(-10.5280415260001,11.6,-3.64534524300002));
#271955=CARTESIAN_POINT('Ctrl Pts',(-10.5305396570001,15.2,-3.64751916900001));
#271956=CARTESIAN_POINT('Ctrl Pts',(-10.5305396570001,11.6,-3.64751916900001));
#271957=CARTESIAN_POINT('Ctrl Pts',(-10.5330398120001,15.2,-3.64969835300001));
#271958=CARTESIAN_POINT('Ctrl Pts',(-10.5330398120001,11.6,-3.64969835300002));
#271959=CARTESIAN_POINT('Ctrl Pts',(-10.5355419810001,15.2,-3.65188279700002));
#271960=CARTESIAN_POINT('Ctrl Pts',(-10.5355419810001,11.6,-3.65188279700002));
#271961=CARTESIAN_POINT('Ctrl Pts',(-10.5380461510001,15.2,-3.65407249800001));
#271962=CARTESIAN_POINT('Ctrl Pts',(-10.5380461510001,11.6,-3.65407249800001));
#271963=CARTESIAN_POINT('Ctrl Pts',(-10.5405523130001,15.2,-3.65626745600002));
#271964=CARTESIAN_POINT('Ctrl Pts',(-10.5405523130001,11.6,-3.65626745600002));
#271965=CARTESIAN_POINT('Ctrl Pts',(-10.5430604560001,15.2,-3.65846767300001));
#271966=CARTESIAN_POINT('Ctrl Pts',(-10.5430604560001,11.6,-3.65846767300001));
#271967=CARTESIAN_POINT('Ctrl Pts',(-10.5455705700001,15.2,-3.66067314500001));
#271968=CARTESIAN_POINT('Ctrl Pts',(-10.5455705700001,11.6,-3.66067314500001));
#271969=CARTESIAN_POINT('Ctrl Pts',(-10.5480826430001,15.2,-3.66288387400001));
#271970=CARTESIAN_POINT('Ctrl Pts',(-10.5480826430001,11.6,-3.66288387400001));
#271971=CARTESIAN_POINT('Ctrl Pts',(-10.5505966660001,15.2,-3.66509985700001));
#271972=CARTESIAN_POINT('Ctrl Pts',(-10.5505966660001,11.6,-3.66509985700001));
#271973=CARTESIAN_POINT('Ctrl Pts',(-10.5531126260001,15.2,-3.66732109700001));
#271974=CARTESIAN_POINT('Ctrl Pts',(-10.5531126260001,11.6,-3.66732109700001));
#271975=CARTESIAN_POINT('Ctrl Pts',(-10.5556305150001,15.2,-3.66954758900001));
#271976=CARTESIAN_POINT('Ctrl Pts',(-10.5556305150001,11.6,-3.66954758900001));
#271977=CARTESIAN_POINT('Ctrl Pts',(-10.5581503220001,15.2,-3.67177933600002));
#271978=CARTESIAN_POINT('Ctrl Pts',(-10.5581503220001,11.6,-3.67177933600002));
#271979=CARTESIAN_POINT('Ctrl Pts',(-10.5606720350001,15.2,-3.67401633600001));
#271980=CARTESIAN_POINT('Ctrl Pts',(-10.5606720350001,11.6,-3.67401633600001));
#271981=CARTESIAN_POINT('Ctrl Pts',(-10.5631956460001,15.2,-3.67625858900002));
#271982=CARTESIAN_POINT('Ctrl Pts',(-10.5631956460001,11.6,-3.67625858900002));
#271983=CARTESIAN_POINT('Ctrl Pts',(-10.5657211420001,15.2,-3.67850609400001));
#271984=CARTESIAN_POINT('Ctrl Pts',(-10.5657211420001,11.6,-3.67850609400001));
#271985=CARTESIAN_POINT('Ctrl Pts',(-10.5682485140001,15.2,-3.68075885100001));
#271986=CARTESIAN_POINT('Ctrl Pts',(-10.5682485140001,11.6,-3.68075885100001));
#271987=CARTESIAN_POINT('Ctrl Pts',(-10.5707777510001,15.2,-3.68301685800001));
#271988=CARTESIAN_POINT('Ctrl Pts',(-10.5707777510001,11.6,-3.68301685800001));
#271989=CARTESIAN_POINT('Ctrl Pts',(-10.5733088430001,15.2,-3.68528011600001));
#271990=CARTESIAN_POINT('Ctrl Pts',(-10.5733088430001,11.6,-3.68528011600001));
#271991=CARTESIAN_POINT('Ctrl Pts',(-10.5758417790001,15.2,-3.68754862400001));
#271992=CARTESIAN_POINT('Ctrl Pts',(-10.5758417790001,11.6,-3.68754862400001));
#271993=CARTESIAN_POINT('Ctrl Pts',(-10.5783765500001,15.2,-3.68982238000001));
#271994=CARTESIAN_POINT('Ctrl Pts',(-10.5783765500001,11.6,-3.68982238000001));
#271995=CARTESIAN_POINT('Ctrl Pts',(-10.5809131450001,15.2,-3.69210138500002));
#271996=CARTESIAN_POINT('Ctrl Pts',(-10.5809131450001,11.6,-3.69210138500002));
#271997=CARTESIAN_POINT('Ctrl Pts',(-10.5834515520001,15.2,-3.69438563900002));
#271998=CARTESIAN_POINT('Ctrl Pts',(-10.5834515520001,11.6,-3.69438563900002));
#271999=CARTESIAN_POINT('Ctrl Pts',(-10.5859917630001,15.2,-3.69667513900001));
#272000=CARTESIAN_POINT('Ctrl Pts',(-10.5859917630001,11.6,-3.69667513900001));
#272001=CARTESIAN_POINT('Ctrl Pts',(-10.5885337670001,15.2,-3.69896988600001));
#272002=CARTESIAN_POINT('Ctrl Pts',(-10.5885337670001,11.6,-3.69896988600001));
#272003=CARTESIAN_POINT('Ctrl Pts',(-10.5910775530001,15.2,-3.70126987800001));
#272004=CARTESIAN_POINT('Ctrl Pts',(-10.5910775530001,11.6,-3.70126987800001));
#272005=CARTESIAN_POINT('Ctrl Pts',(-10.5936231110001,15.2,-3.70357511600002));
#272006=CARTESIAN_POINT('Ctrl Pts',(-10.5936231110001,11.6,-3.70357511600002));
#272007=CARTESIAN_POINT('Ctrl Pts',(-10.5961704330001,15.2,-3.70588560000002));
#272008=CARTESIAN_POINT('Ctrl Pts',(-10.5961704330001,11.6,-3.70588560000002));
#272009=CARTESIAN_POINT('Ctrl Pts',(-10.5987195050001,15.2,-3.70820132600001));
#272010=CARTESIAN_POINT('Ctrl Pts',(-10.5987195050001,11.6,-3.70820132600001));
#272011=CARTESIAN_POINT('Ctrl Pts',(-10.6012703200001,15.2,-3.71052229700001));
#272012=CARTESIAN_POINT('Ctrl Pts',(-10.6012703200001,11.6,-3.71052229700001));
#272013=CARTESIAN_POINT('Ctrl Pts',(-10.6038228660001,15.2,-3.71284850900001));
#272014=CARTESIAN_POINT('Ctrl Pts',(-10.6038228660001,11.6,-3.71284850900001));
#272015=CARTESIAN_POINT('Ctrl Pts',(-10.6063771330001,15.2,-3.71517996400001));
#272016=CARTESIAN_POINT('Ctrl Pts',(-10.6063771330001,11.6,-3.71517996400002));
#272017=CARTESIAN_POINT('Ctrl Pts',(-10.6089331120001,15.2,-3.71751666000002));
#272018=CARTESIAN_POINT('Ctrl Pts',(-10.6089331120001,11.6,-3.71751666000002));
#272019=CARTESIAN_POINT('Ctrl Pts',(-10.6114907930001,15.2,-3.71985859600001));
#272020=CARTESIAN_POINT('Ctrl Pts',(-10.6114907930001,11.6,-3.71985859600001));
#272021=CARTESIAN_POINT('Ctrl Pts',(-10.6140501650001,15.2,-3.72220577200002));
#272022=CARTESIAN_POINT('Ctrl Pts',(-10.6140501650001,11.6,-3.72220577200002));
#272023=CARTESIAN_POINT('Ctrl Pts',(-10.6166112170001,15.2,-3.72455818700002));
#272024=CARTESIAN_POINT('Ctrl Pts',(-10.6166112170001,11.6,-3.72455818700002));
#272025=CARTESIAN_POINT('Ctrl Pts',(-10.6191739410001,15.2,-3.72691584200001));
#272026=CARTESIAN_POINT('Ctrl Pts',(-10.6191739410001,11.6,-3.72691584200001));
#272027=CARTESIAN_POINT('Ctrl Pts',(-10.6217383260001,15.2,-3.72927873300001));
#272028=CARTESIAN_POINT('Ctrl Pts',(-10.6217383260001,11.6,-3.72927873300001));
#272029=CARTESIAN_POINT('Ctrl Pts',(-10.6243043610001,15.2,-3.73164686100001));
#272030=CARTESIAN_POINT('Ctrl Pts',(-10.6243043610001,11.6,-3.73164686100001));
#272031=CARTESIAN_POINT('Ctrl Pts',(-10.6268720380001,15.2,-3.73402022600001));
#272032=CARTESIAN_POINT('Ctrl Pts',(-10.6268720380001,11.6,-3.73402022600001));
#272033=CARTESIAN_POINT('Ctrl Pts',(-10.6294413450001,15.2,-3.73639882600001));
#272034=CARTESIAN_POINT('Ctrl Pts',(-10.6294413450001,11.6,-3.73639882600001));
#272035=CARTESIAN_POINT('Ctrl Pts',(-10.6320122750001,15.2,-3.73878266000002));
#272036=CARTESIAN_POINT('Ctrl Pts',(-10.6320122750001,11.6,-3.73878266000002));
#272037=CARTESIAN_POINT('Ctrl Pts',(-10.6345848160001,15.2,-3.74117172800001));
#272038=CARTESIAN_POINT('Ctrl Pts',(-10.6345848160001,11.6,-3.74117172800001));
#272039=CARTESIAN_POINT('Ctrl Pts',(-10.6371589570001,15.2,-3.74356603100002));
#272040=CARTESIAN_POINT('Ctrl Pts',(-10.6371589570001,11.6,-3.74356603100002));
#272041=CARTESIAN_POINT('Ctrl Pts',(-10.6397346900001,15.2,-3.74596556400002));
#272042=CARTESIAN_POINT('Ctrl Pts',(-10.6397346900001,11.6,-3.74596556400002));
#272043=CARTESIAN_POINT('Ctrl Pts',(-10.6423120040001,15.2,-3.74837033000002));
#272044=CARTESIAN_POINT('Ctrl Pts',(-10.6423120040001,11.6,-3.74837033000002));
#272045=CARTESIAN_POINT('Ctrl Pts',(-10.6448908910001,15.2,-3.75078032600001));
#272046=CARTESIAN_POINT('Ctrl Pts',(-10.6448908910001,11.6,-3.75078032600001));
#272047=CARTESIAN_POINT('Ctrl Pts',(-10.6474713390001,15.2,-3.75319555200001));
#272048=CARTESIAN_POINT('Ctrl Pts',(-10.6474713390001,11.6,-3.75319555200001));
#272049=CARTESIAN_POINT('Ctrl Pts',(-10.6500533400001,15.2,-3.75561600800001));
#272050=CARTESIAN_POINT('Ctrl Pts',(-10.6500533400001,11.6,-3.75561600800001));
#272051=CARTESIAN_POINT('Ctrl Pts',(-10.6526368820001,15.2,-3.75804169200002));
#272052=CARTESIAN_POINT('Ctrl Pts',(-10.6526368820001,11.6,-3.75804169200002));
#272053=CARTESIAN_POINT('Ctrl Pts',(-10.6552219570001,15.2,-3.76047260400002));
#272054=CARTESIAN_POINT('Ctrl Pts',(-10.6552219570001,11.6,-3.76047260400002));
#272055=CARTESIAN_POINT('Ctrl Pts',(-10.6578085550001,15.2,-3.76290874200001));
#272056=CARTESIAN_POINT('Ctrl Pts',(-10.6578085550001,11.6,-3.76290874200001));
#272057=CARTESIAN_POINT('Ctrl Pts',(-10.6603966660001,15.2,-3.76535010600001));
#272058=CARTESIAN_POINT('Ctrl Pts',(-10.6603966660001,11.6,-3.76535010600001));
#272059=CARTESIAN_POINT('Ctrl Pts',(-10.6629862800001,15.2,-3.76779669600001));
#272060=CARTESIAN_POINT('Ctrl Pts',(-10.6629862800001,11.6,-3.76779669600001));
#272061=CARTESIAN_POINT('Ctrl Pts',(-10.6655773880001,15.2,-3.77024850900002));
#272062=CARTESIAN_POINT('Ctrl Pts',(-10.6655773880001,11.6,-3.77024850900002));
#272063=CARTESIAN_POINT('Ctrl Pts',(-10.6681699790001,15.2,-3.77270554500001));
#272064=CARTESIAN_POINT('Ctrl Pts',(-10.6681699790001,11.6,-3.77270554500001));
#272065=CARTESIAN_POINT('Ctrl Pts',(-10.6707640450001,15.2,-3.77516780500001));
#272066=CARTESIAN_POINT('Ctrl Pts',(-10.6707640450001,11.6,-3.77516780500002));
#272067=CARTESIAN_POINT('Ctrl Pts',(-10.6733595760001,15.2,-3.77763528600001));
#272068=CARTESIAN_POINT('Ctrl Pts',(-10.6733595760001,11.6,-3.77763528600001));
#272069=CARTESIAN_POINT('Ctrl Pts',(-10.6759565610001,15.2,-3.78010798800001));
#272070=CARTESIAN_POINT('Ctrl Pts',(-10.6759565610001,11.6,-3.78010798800001));
#272071=CARTESIAN_POINT('Ctrl Pts',(-10.6785549920001,15.2,-3.78258590900002));
#272072=CARTESIAN_POINT('Ctrl Pts',(-10.6785549920001,11.6,-3.78258590900002));
#272073=CARTESIAN_POINT('Ctrl Pts',(-10.6811548570001,15.2,-3.78506905000001));
#272074=CARTESIAN_POINT('Ctrl Pts',(-10.6811548570001,11.6,-3.78506905000001));
#272075=CARTESIAN_POINT('Ctrl Pts',(-10.6837561510001,15.2,-3.78755740900001));
#272076=CARTESIAN_POINT('Ctrl Pts',(-10.6837561510001,11.6,-3.78755740900001));
#272077=CARTESIAN_POINT('Ctrl Pts',(-10.6863588600001,15.2,-3.79005098500001));
#272078=CARTESIAN_POINT('Ctrl Pts',(-10.6863588600001,11.6,-3.79005098500001));
#272079=CARTESIAN_POINT('Ctrl Pts',(-10.6889629760001,15.2,-3.79254977800001));
#272080=CARTESIAN_POINT('Ctrl Pts',(-10.6889629760001,11.6,-3.79254977800001));
#272081=CARTESIAN_POINT('Ctrl Pts',(-10.6915684890001,15.2,-3.79505378600001));
#272082=CARTESIAN_POINT('Ctrl Pts',(-10.6915684890001,11.6,-3.79505378600001));
#272083=CARTESIAN_POINT('Ctrl Pts',(-10.6941753910001,15.2,-3.79756300900001));
#272084=CARTESIAN_POINT('Ctrl Pts',(-10.6941753910001,11.6,-3.79756300900001));
#272085=CARTESIAN_POINT('Ctrl Pts',(-10.6967836710001,15.2,-3.80007744500002));
#272086=CARTESIAN_POINT('Ctrl Pts',(-10.6967836710001,11.6,-3.80007744500002));
#272087=CARTESIAN_POINT('Ctrl Pts',(-10.6993933200001,15.2,-3.80259709400002));
#272088=CARTESIAN_POINT('Ctrl Pts',(-10.6993933200001,11.6,-3.80259709400002));
#272089=CARTESIAN_POINT('Ctrl Pts',(-10.7020043290001,15.2,-3.80512195600001));
#272090=CARTESIAN_POINT('Ctrl Pts',(-10.7020043290001,11.6,-3.80512195600002));
#272091=CARTESIAN_POINT('Ctrl Pts',(-10.7046166880001,15.2,-3.80765202700001));
#272092=CARTESIAN_POINT('Ctrl Pts',(-10.7046166880001,11.6,-3.80765202700002));
#272093=CARTESIAN_POINT('Ctrl Pts',(-10.7072303880001,15.2,-3.81018730900001));
#272094=CARTESIAN_POINT('Ctrl Pts',(-10.7072303880001,11.6,-3.81018730900002));
#272095=CARTESIAN_POINT('Ctrl Pts',(-10.7098454180001,15.2,-3.81272780000002));
#272096=CARTESIAN_POINT('Ctrl Pts',(-10.7098454180001,11.6,-3.81272780000002));
#272097=CARTESIAN_POINT('Ctrl Pts',(-10.7124617720001,15.2,-3.81527349900002));
#272098=CARTESIAN_POINT('Ctrl Pts',(-10.7124617720001,11.6,-3.81527349900002));
#272099=CARTESIAN_POINT('Ctrl Pts',(-10.7150794370001,15.2,-3.81782440400002));
#272100=CARTESIAN_POINT('Ctrl Pts',(-10.7150794370001,11.6,-3.81782440400002));
#272101=CARTESIAN_POINT('Ctrl Pts',(-10.7176984060001,15.2,-3.82038051600002));
#272102=CARTESIAN_POINT('Ctrl Pts',(-10.7176984060001,11.6,-3.82038051600002));
#272103=CARTESIAN_POINT('Ctrl Pts',(-10.7203186690001,15.2,-3.82294183300001));
#272104=CARTESIAN_POINT('Ctrl Pts',(-10.7203186690001,11.6,-3.82294183300001));
#272105=CARTESIAN_POINT('Ctrl Pts',(-10.7229402150001,15.2,-3.82550835400002));
#272106=CARTESIAN_POINT('Ctrl Pts',(-10.7229402150001,11.6,-3.82550835400002));
#272107=CARTESIAN_POINT('Ctrl Pts',(-10.7255630380001,15.2,-3.82808007900001));
#272108=CARTESIAN_POINT('Ctrl Pts',(-10.7255630380001,11.6,-3.82808007900001));
#272109=CARTESIAN_POINT('Ctrl Pts',(-10.7281871270001,15.2,-3.83065700500001));
#272110=CARTESIAN_POINT('Ctrl Pts',(-10.7281871270001,11.6,-3.83065700500001));
#272111=CARTESIAN_POINT('Ctrl Pts',(-10.7308124710001,15.2,-3.83323913300002));
#272112=CARTESIAN_POINT('Ctrl Pts',(-10.7308124710001,11.6,-3.83323913300002));
#272113=CARTESIAN_POINT('Ctrl Pts',(-10.7334390640001,15.2,-3.83582646100002));
#272114=CARTESIAN_POINT('Ctrl Pts',(-10.7334390640001,11.6,-3.83582646100002));
#272115=CARTESIAN_POINT('Ctrl Pts',(-10.7360668940001,15.2,-3.83841898800001));
#272116=CARTESIAN_POINT('Ctrl Pts',(-10.7360668940001,11.6,-3.83841898800001));
#272117=CARTESIAN_POINT('Ctrl Pts',(-10.7386959530001,15.2,-3.84101671300002));
#272118=CARTESIAN_POINT('Ctrl Pts',(-10.7386959530001,11.6,-3.84101671300002));
#272119=CARTESIAN_POINT('Ctrl Pts',(-10.7413262330001,15.2,-3.84361963500002));
#272120=CARTESIAN_POINT('Ctrl Pts',(-10.7413262330001,11.6,-3.84361963500002));
#272121=CARTESIAN_POINT('Ctrl Pts',(-10.7439577220001,15.2,-3.84622775400001));
#272122=CARTESIAN_POINT('Ctrl Pts',(-10.7439577220001,11.6,-3.84622775400001));
#272123=CARTESIAN_POINT('Ctrl Pts',(-10.7465904140001,15.2,-3.84884106800001));
#272124=CARTESIAN_POINT('Ctrl Pts',(-10.7465904140001,11.6,-3.84884106800001));
#272125=CARTESIAN_POINT('Ctrl Pts',(-10.7492242980001,15.2,-3.85145957500002));
#272126=CARTESIAN_POINT('Ctrl Pts',(-10.7492242980001,11.6,-3.85145957500002));
#272127=CARTESIAN_POINT('Ctrl Pts',(-10.7518593670001,15.2,-3.85408327600001));
#272128=CARTESIAN_POINT('Ctrl Pts',(-10.7518593670001,11.6,-3.85408327600001));
#272129=CARTESIAN_POINT('Ctrl Pts',(-10.7544956090001,15.2,-3.85671216900001));
#272130=CARTESIAN_POINT('Ctrl Pts',(-10.7544956090001,11.6,-3.85671216900001));
#272131=CARTESIAN_POINT('Ctrl Pts',(-10.7571330160001,15.2,-3.85934625200001));
#272132=CARTESIAN_POINT('Ctrl Pts',(-10.7571330160001,11.6,-3.85934625200001));
#272133=CARTESIAN_POINT('Ctrl Pts',(-10.7597715780001,15.2,-3.86198552600002));
#272134=CARTESIAN_POINT('Ctrl Pts',(-10.7597715780001,11.6,-3.86198552600002));
#272135=CARTESIAN_POINT('Ctrl Pts',(-10.7624112860001,15.2,-3.86462998800001));
#272136=CARTESIAN_POINT('Ctrl Pts',(-10.7624112860001,11.6,-3.86462998800001));
#272137=CARTESIAN_POINT('Ctrl Pts',(-10.7650521310001,15.2,-3.86727963800002));
#272138=CARTESIAN_POINT('Ctrl Pts',(-10.7650521310001,11.6,-3.86727963800002));
#272139=CARTESIAN_POINT('Ctrl Pts',(-10.7676941040001,15.2,-3.86993447500001));
#272140=CARTESIAN_POINT('Ctrl Pts',(-10.7676941040001,11.6,-3.86993447500001));
#272141=CARTESIAN_POINT('Ctrl Pts',(-10.7703371960001,15.2,-3.87259449700001));
#272142=CARTESIAN_POINT('Ctrl Pts',(-10.7703371960001,11.6,-3.87259449700002));
#272143=CARTESIAN_POINT('Ctrl Pts',(-10.7729813980001,15.2,-3.87525970300001));
#272144=CARTESIAN_POINT('Ctrl Pts',(-10.7729813980001,11.6,-3.87525970300001));
#272145=CARTESIAN_POINT('Ctrl Pts',(-10.7756267050001,15.2,-3.87793009300001));
#272146=CARTESIAN_POINT('Ctrl Pts',(-10.7756267050001,11.6,-3.87793009300002));
#272147=CARTESIAN_POINT('Ctrl Pts',(-10.7782731050001,15.2,-3.88060566600001));
#272148=CARTESIAN_POINT('Ctrl Pts',(-10.7782731050001,11.6,-3.88060566600001));
#272149=CARTESIAN_POINT('Ctrl Pts',(-10.7809205920001,15.2,-3.88328642000001));
#272150=CARTESIAN_POINT('Ctrl Pts',(-10.7809205920001,11.6,-3.88328642000001));
#272151=CARTESIAN_POINT('Ctrl Pts',(-10.7835691560001,15.2,-3.88597235400002));
#272152=CARTESIAN_POINT('Ctrl Pts',(-10.7835691560001,11.6,-3.88597235400002));
#272153=CARTESIAN_POINT('Ctrl Pts',(-10.7862187870001,15.2,-3.88866346700001));
#272154=CARTESIAN_POINT('Ctrl Pts',(-10.7862187870001,11.6,-3.88866346700001));
#272155=CARTESIAN_POINT('Ctrl Pts',(-10.7888694730001,15.2,-3.89135975900002));
#272156=CARTESIAN_POINT('Ctrl Pts',(-10.7888694730001,11.6,-3.89135975900002));
#272157=CARTESIAN_POINT('Ctrl Pts',(-10.7915212030001,15.2,-3.89406122600001));
#272158=CARTESIAN_POINT('Ctrl Pts',(-10.7915212030001,11.6,-3.89406122600001));
#272159=CARTESIAN_POINT('Ctrl Pts',(-10.7941739680001,15.2,-3.89676786900001));
#272160=CARTESIAN_POINT('Ctrl Pts',(-10.7941739680001,11.6,-3.89676786900001));
#272161=CARTESIAN_POINT('Ctrl Pts',(-10.7968277560001,15.2,-3.89947968500001));
#272162=CARTESIAN_POINT('Ctrl Pts',(-10.7968277560001,11.6,-3.89947968500001));
#272163=CARTESIAN_POINT('Ctrl Pts',(-10.7994825590001,15.2,-3.90219667400002));
#272164=CARTESIAN_POINT('Ctrl Pts',(-10.7994825590001,11.6,-3.90219667400002));
#272165=CARTESIAN_POINT('Ctrl Pts',(-10.8021383740001,15.2,-3.90491883400002));
#272166=CARTESIAN_POINT('Ctrl Pts',(-10.8021383740001,11.6,-3.90491883400002));
#272167=CARTESIAN_POINT('Ctrl Pts',(-10.8047951940001,15.2,-3.90764616700002));
#272168=CARTESIAN_POINT('Ctrl Pts',(-10.8047951940001,11.6,-3.90764616700002));
#272169=CARTESIAN_POINT('Ctrl Pts',(-10.8074530190001,15.2,-3.91037866900001));
#272170=CARTESIAN_POINT('Ctrl Pts',(-10.8074530190001,11.6,-3.91037866900001));
#272171=CARTESIAN_POINT('Ctrl Pts',(-10.8095800800001,15.2,-3.91256880900002));
#272172=CARTESIAN_POINT('Ctrl Pts',(-10.8095800800001,11.6,-3.91256880900002));
#272173=CARTESIAN_POINT('Ctrl Pts',(-10.8111758270001,15.2,-3.91421373900001));
#272174=CARTESIAN_POINT('Ctrl Pts',(-10.8111758270001,11.6,-3.91421373900001));
#272175=CARTESIAN_POINT('Ctrl Pts',(-10.8122398590001,15.2,-3.91531139400001));
#272176=CARTESIAN_POINT('Ctrl Pts',(-10.8122398590001,11.6,-3.91531139400001));
#272177=CARTESIAN_POINT('Ctrl Pts',(-10.8127719260001,15.2,-3.91586047900002));
#272178=CARTESIAN_POINT('Ctrl Pts',(-10.8127719260001,11.6,-3.91586047900002));
#272179=CARTESIAN_POINT('Ctrl Pts',(-9.86852965800006,15.2,-3.20199116200001));
#272180=CARTESIAN_POINT('Ctrl Pts',(-9.87017542455281,15.2,-3.20268658157505));
#272181=CARTESIAN_POINT('Ctrl Pts',(-9.87187175388031,15.2,-3.20340918512851));
#272182=CARTESIAN_POINT('Ctrl Pts',(-9.87361750383377,15.2,-3.20415921016782));
#272183=CARTESIAN_POINT('Ctrl Pts',(-9.87537167267595,15.2,-3.204912852207));
#272184=CARTESIAN_POINT('Ctrl Pts',(-9.87717574023296,15.2,-3.20569417462551));
#272185=CARTESIAN_POINT('Ctrl Pts',(-9.87902857842933,15.2,-3.20650338954498));
#272186=CARTESIAN_POINT('Ctrl Pts',(-9.88088141645739,15.2,-3.20731260439096));
#272187=CARTESIAN_POINT('Ctrl Pts',(-9.88278302851245,15.2,-3.2081497105564));
#272188=CARTESIAN_POINT('Ctrl Pts',(-9.88473231752497,15.2,-3.20901491227497));
#272189=CARTESIAN_POINT('Ctrl Pts',(-9.88668160653749,15.2,-3.20988011399353));
#272190=CARTESIAN_POINT('Ctrl Pts',(-9.88867857432724,15.1999999999999,
-3.21077340827496));
#272191=CARTESIAN_POINT('Ctrl Pts',(-9.89072215651906,15.2,-3.21169499220255));
#272192=CARTESIAN_POINT('Ctrl Pts',(-9.89276573889652,15.2,-3.21261657621385));
#272193=CARTESIAN_POINT('Ctrl Pts',(-9.89485593802995,15.2,-3.21356644793468));
#272194=CARTESIAN_POINT('Ctrl Pts',(-9.89699171648278,15.2,-3.21454479382328));
#272195=CARTESIAN_POINT('Ctrl Pts',(-9.89912749474164,15.2,-3.21552313962301));
#272196=CARTESIAN_POINT('Ctrl Pts',(-9.90130885331331,15.2,-3.21652996002495));
#272197=CARTESIAN_POINT('Ctrl Pts',(-9.90353478649266,15.2,-3.2175654317421));
#272198=CARTESIAN_POINT('Ctrl Pts',(-9.90576071967203,15.2,-3.21860090345925));
#272199=CARTESIAN_POINT('Ctrl Pts',(-9.90803122770171,15.2,-3.21966502577316));
#272200=CARTESIAN_POINT('Ctrl Pts',(-9.91034532736571,15.2,-3.22075797048219));
#272201=CARTESIAN_POINT('Ctrl Pts',(-9.91265942723992,15.2,-3.22185091529049));
#272202=CARTESIAN_POINT('Ctrl Pts',(-9.91501712228624,15.2,-3.22297268096072));
#272203=CARTESIAN_POINT('Ctrl Pts',(-9.91741745500329,15.2,-3.22412343085873));
#272204=CARTESIAN_POINT('Ctrl Pts',(-9.91981778750232,15.2,-3.22527418065224));
#272205=CARTESIAN_POINT('Ctrl Pts',(-9.92226075844071,15.2,-3.22645391558363));
#272206=CARTESIAN_POINT('Ctrl Pts',(-9.92474543535224,15.2,-3.22766278929097));
#272207=CARTESIAN_POINT('Ctrl Pts',(-9.92723011226377,15.2,-3.22887166299831));
#272208=CARTESIAN_POINT('Ctrl Pts',(-9.92975649757194,15.2,-3.23010967648666));
#272209=CARTESIAN_POINT('Ctrl Pts',(-9.93232368131025,15.2,-3.23137697818935));
#272210=CARTESIAN_POINT('Ctrl Pts',(-9.93489086504854,15.2,-3.23264427989204));
#272211=CARTESIAN_POINT('Ctrl Pts',(-9.937498847977,15.2,-3.23394087139731));
#272212=CARTESIAN_POINT('Ctrl Pts',(-9.94014674371137,15.2,-3.2352668930971));
#272213=CARTESIAN_POINT('Ctrl Pts',(-9.94279463968627,15.2,-3.23659291491734));
#272214=CARTESIAN_POINT('Ctrl Pts',(-9.94548244775676,15.2,-3.2379483681488));
#272215=CARTESIAN_POINT('Ctrl Pts',(-9.9482093021571,15.2,-3.23933338705891));
#272216=CARTESIAN_POINT('Ctrl Pts',(-9.95093615630974,15.2,-3.24071840584321));
#272217=CARTESIAN_POINT('Ctrl Pts',(-9.95370205916299,15.2,-3.24213299364531));
#272218=CARTESIAN_POINT('Ctrl Pts',(-9.95650616499038,15.2,-3.24357727726597));
#272219=CARTESIAN_POINT('Ctrl Pts',(-9.95931027081778,15.2,-3.24502156088664));
#272220=CARTESIAN_POINT('Ctrl Pts',(-9.96215257803497,15.2,-3.24649554081774));
#272221=CARTESIAN_POINT('Ctrl Pts',(-9.96503226217778,15.2,-3.24799934334439));
#272222=CARTESIAN_POINT('Ctrl Pts',(-9.96791194658215,15.2,-3.24950314600764));
#272223=CARTESIAN_POINT('Ctrl Pts',(-9.97082900750689,15.2,-3.25103676921545));
#272224=CARTESIAN_POINT('Ctrl Pts',(-9.97378263891945,15.2,-3.25260033280197));
#272225=CARTESIAN_POINT('Ctrl Pts',(-9.97673627006372,15.2,-3.25416389624646));
#272226=CARTESIAN_POINT('Ctrl Pts',(-9.9797264712199,15.2,-3.2557573999259));
#272227=CARTESIAN_POINT('Ctrl Pts',(-9.98275245154029,15.2,-3.25738095645756));
#272228=CARTESIAN_POINT('Ctrl Pts',(-9.9857784318607,15.2,-3.25900451298922));
#272229=CARTESIAN_POINT('Ctrl Pts',(-9.98884019241067,15.2,-3.26065812320466));
#272230=CARTESIAN_POINT('Ctrl Pts',(-9.99193696262913,15.2,-3.2623418945581));
#272231=CARTESIAN_POINT('Ctrl Pts',(-9.99503373312888,15.2,-3.26402566606449));
#272232=CARTESIAN_POINT('Ctrl Pts',(-9.998165510507,15.2,-3.26573959840982));
#272233=CARTESIAN_POINT('Ctrl Pts',(-10.0013315413397,15.2,-3.2674837951771));
#272234=CARTESIAN_POINT('Ctrl Pts',(-10.0044975718848,15.2,-3.26922799178594));
#272235=CARTESIAN_POINT('Ctrl Pts',(-10.0076978541008,15.2,-3.27100245334886));
#272236=CARTESIAN_POINT('Ctrl Pts',(-10.0109316504833,15.2,-3.27280727678329));
#272237=CARTESIAN_POINT('Ctrl Pts',(-10.0141654468658,15.2,-3.27461210021773));
#272238=CARTESIAN_POINT('Ctrl Pts',(-10.0174327550794,15.2,-3.27644728653758));
#272239=CARTESIAN_POINT('Ctrl Pts',(-10.0207328517058,15.2,-3.27831292881123));
#272240=CARTESIAN_POINT('Ctrl Pts',(-10.024032948632,15.2,-3.28017857125434));
#272241=CARTESIAN_POINT('Ctrl Pts',(-10.0273658332479,15.2,-3.28207466921122));
#272242=CARTESIAN_POINT('Ctrl Pts',(-10.0307307971001,15.2,-3.28400131173497));
#272243=CARTESIAN_POINT('Ctrl Pts',(-10.0340957606467,15.2,-3.28592795408372));
#272244=CARTESIAN_POINT('Ctrl Pts',(-10.0374928009605,15.2,-3.28788514203065));
#272245=CARTESIAN_POINT('Ctrl Pts',(-10.0409212255182,15.2,-3.28987295846753));
#272246=CARTESIAN_POINT('Ctrl Pts',(-10.044349650076,15.2,-3.29186077490442));
#272247=CARTESIAN_POINT('Ctrl Pts',(-10.0478094564797,15.2,-3.29387922119752));
#272248=CARTESIAN_POINT('Ctrl Pts',(-10.0512999632682,15.2,-3.29592837662175));
#272249=CARTESIAN_POINT('Ctrl Pts',(-10.054208719031,15.2,-3.29763600620398));
#272250=CARTESIAN_POINT('Ctrl Pts',(-10.0571387938471,15.2,-3.29936496208675));
#272251=CARTESIAN_POINT('Ctrl Pts',(-10.0600898020405,15.2,-3.30111528812729));
#272252=CARTESIAN_POINT('Ctrl Pts',(-10.0630408102338,15.2,-3.30286561416783));
#272253=CARTESIAN_POINT('Ctrl Pts',(-10.0660127512293,15.2,-3.30463730936312));
#272254=CARTESIAN_POINT('Ctrl Pts',(-10.0690052420067,15.2,-3.30643041798232));
#272255=CARTESIAN_POINT('Ctrl Pts',(-10.0719977327841,15.2,-3.30822352660152));
#272256=CARTESIAN_POINT('Ctrl Pts',(-10.07501077405,15.2,-3.31003804834439));
#272257=CARTESIAN_POINT('Ctrl Pts',(-10.0780439907167,15.2,-3.31187402202496));
#272258=CARTESIAN_POINT('Ctrl Pts',(-10.0810772073834,15.2,-3.31370999570553));
#272259=CARTESIAN_POINT('Ctrl Pts',(-10.0841305999877,15.2,-3.31556742195907));
#272260=CARTESIAN_POINT('Ctrl Pts',(-10.0872037960433,15.2,-3.31744634050932));
#272261=CARTESIAN_POINT('Ctrl Pts',(-10.090276992099,15.2,-3.31932525905957));
#272262=CARTESIAN_POINT('Ctrl Pts',(-10.0933699960638,15.2,-3.32122566818577));
#272263=CARTESIAN_POINT('Ctrl Pts',(-10.0964824387037,15.2,-3.32314760665912));
#272264=CARTESIAN_POINT('Ctrl Pts',(-10.0995948813436,15.2,-3.32506954513246));
#272265=CARTESIAN_POINT('Ctrl Pts',(-10.1027267670941,15.2,-3.32701301197191));
#272266=CARTESIAN_POINT('Ctrl Pts',(-10.1058777332062,15.2,-3.32897804065361));
#272267=CARTESIAN_POINT('Ctrl Pts',(-10.1090286993183,15.2,-3.3309430693353));
#272268=CARTESIAN_POINT('Ctrl Pts',(-10.1121987497985,15.2,-3.33292966151468));
#272269=CARTESIAN_POINT('Ctrl Pts',(-10.1153875285702,15.2,-3.33493785099149));
#272270=CARTESIAN_POINT('Ctrl Pts',(-10.1185763073419,15.2,-3.3369460404683));
#272271=CARTESIAN_POINT('Ctrl Pts',(-10.121783815176,15.2,-3.3389758262332));
#272272=CARTESIAN_POINT('Ctrl Pts',(-10.1250097044136,15.2,-3.34102723977663));
#272273=CARTESIAN_POINT('Ctrl Pts',(-10.1282355936513,15.2,-3.34307865332005));
#272274=CARTESIAN_POINT('Ctrl Pts',(-10.131479863653,15.2,-3.3451516946333));
#272275=CARTESIAN_POINT('Ctrl Pts',(-10.1347421721267,15.2,-3.34724639477395));
#272276=CARTESIAN_POINT('Ctrl Pts',(-10.1380044802448,15.2,-3.34934109468628));
#272277=CARTESIAN_POINT('Ctrl Pts',(-10.1412848268184,15.2,-3.35145745227179));
#272278=CARTESIAN_POINT('Ctrl Pts',(-10.1445828725686,15.2,-3.35359549641198));
#272279=CARTESIAN_POINT('Ctrl Pts',(-10.1478809186783,15.2,-3.35573354078522));
#272280=CARTESIAN_POINT('Ctrl Pts',(-10.1511966662766,15.2,-3.35789327163863));
#272281=CARTESIAN_POINT('Ctrl Pts',(-10.1545297791224,15.2,-3.3600747167063));
#272282=CARTESIAN_POINT('Ctrl Pts',(-10.1578628919682,15.2,-3.36225616177396));
#272283=CARTESIAN_POINT('Ctrl Pts',(-10.1612133718276,15.2,-3.36445931992739));
#272284=CARTESIAN_POINT('Ctrl Pts',(-10.1645808903679,15.2,-3.36668421596729));
#272285=CARTESIAN_POINT('Ctrl Pts',(-10.1679484089082,15.2,-3.36890911200718));
#272286=CARTESIAN_POINT('Ctrl Pts',(-10.1713329648365,15.2,-3.37115574719711));
#272287=CARTESIAN_POINT('Ctrl Pts',(-10.1747342345886,15.2,-3.37342414571171));
#272288=CARTESIAN_POINT('Ctrl Pts',(-10.1781355043407,15.2,-3.37569254422632));
#272289=CARTESIAN_POINT('Ctrl Pts',(-10.1815534888375,15.2,-3.37798270471114));
#272290=CARTESIAN_POINT('Ctrl Pts',(-10.1849878675172,15.2,-3.38029464984889));
#272291=CARTESIAN_POINT('Ctrl Pts',(-10.1891091221574,15.2,-3.3830689841654));
#272292=CARTESIAN_POINT('Ctrl Pts',(-10.1932539831256,15.2,-3.38587468871912));
#272293=CARTESIAN_POINT('Ctrl Pts',(-10.1974219096877,15.2,-3.38871180004254));
#272294=CARTESIAN_POINT('Ctrl Pts',(-10.2002005270171,15.2,-3.39060320733379));
#272295=CARTESIAN_POINT('Ctrl Pts',(-10.2029893949504,15.2,-3.39250857353023));
#272296=CARTESIAN_POINT('Ctrl Pts',(-10.2057883537898,15.2,-3.39442790804865));
#272297=CARTESIAN_POINT('Ctrl Pts',(-10.2085873130105,15.2,-3.39634724282858));
#272298=CARTESIAN_POINT('Ctrl Pts',(-10.2113963643396,15.2,-3.39828054381079));
#272299=CARTESIAN_POINT('Ctrl Pts',(-10.2142153494943,15.2,-3.40022782458501));
#272300=CARTESIAN_POINT('Ctrl Pts',(-10.2170343342648,15.2,-3.40217510509392));
#272301=CARTESIAN_POINT('Ctrl Pts',(-10.2198632526341,15.2,-3.40413636252046));
#272302=CARTESIAN_POINT('Ctrl Pts',(-10.2227019507347,15.2,-3.40611160708028));
#272303=CARTESIAN_POINT('Ctrl Pts',(-10.2255406492221,15.2,-3.40808685190924));
#272304=CARTESIAN_POINT('Ctrl Pts',(-10.2283891251487,15.2,-3.4100760822497));
#272305=CARTESIAN_POINT('Ctrl Pts',(-10.2312472264481,15.2,-3.41207930851572));
#272306=CARTESIAN_POINT('Ctrl Pts',(-10.2341053273581,15.2,-3.4140825345088));
#272307=CARTESIAN_POINT('Ctrl Pts',(-10.2369730513868,15.2,-3.41609975441768));
#272308=CARTESIAN_POINT('Ctrl Pts',(-10.2398502482066,15.2,-3.4181309782507));
#272309=CARTESIAN_POINT('Ctrl Pts',(-10.2427274454183,15.2,-3.42016220236048));
#272310=CARTESIAN_POINT('Ctrl Pts',(-10.2456141140673,15.2,-3.42220742849139));
#272311=CARTESIAN_POINT('Ctrl Pts',(-10.2485101040035,15.2,-3.4242666646601));
#272312=CARTESIAN_POINT('Ctrl Pts',(-10.2514060935452,15.2,-3.42632590054824));
#272313=CARTESIAN_POINT('Ctrl Pts',(-10.2543114045956,15.2,-3.42839914698696));
#272314=CARTESIAN_POINT('Ctrl Pts',(-10.2572258863355,15.2,-3.43048640969716));
#272315=CARTESIAN_POINT('Ctrl Pts',(-10.2601403684725,15.2,-3.43257367269175));
#272316=CARTESIAN_POINT('Ctrl Pts',(-10.2630640229044,15.2,-3.43467495284292));
#272317=CARTESIAN_POINT('Ctrl Pts',(-10.2659967002315,15.2,-3.43679025568135));
#272318=CARTESIAN_POINT('Ctrl Pts',(-10.268929377159,15.2,-3.43890555823157));
#272319=CARTESIAN_POINT('Ctrl Pts',(-10.2718710773958,15.2,-3.44103488317618));
#272320=CARTESIAN_POINT('Ctrl Pts',(-10.2748216555426,15.2,-3.44317823766619));
#272321=CARTESIAN_POINT('Ctrl Pts',(-10.2785098785276,15.2,-3.44585743099772));
#272322=CARTESIAN_POINT('Ctrl Pts',(-10.2822119710007,15.2,-3.44855854367164));
#272323=CARTESIAN_POINT('Ctrl Pts',(-10.2859276518104,15.2,-3.45128158720893));
#272324=CARTESIAN_POINT('Ctrl Pts',(-10.2889001966201,15.2,-3.45346002215749));
#272325=CARTESIAN_POINT('Ctrl Pts',(-10.2918814373921,15.2,-3.45565249229263));
#272326=CARTESIAN_POINT('Ctrl Pts',(-10.2948712307779,15.2,-3.45785900241381));
#272327=CARTESIAN_POINT('Ctrl Pts',(-10.2978610237562,15.2,-3.46006551223434));
#272328=CARTESIAN_POINT('Ctrl Pts',(-10.3008593699856,15.2,-3.46228606144095));
#272329=CARTESIAN_POINT('Ctrl Pts',(-10.3038661270168,15.2,-3.46452065536794));
#272330=CARTESIAN_POINT('Ctrl Pts',(-10.3068728844575,15.2,-3.4667552495994));
#272331=CARTESIAN_POINT('Ctrl Pts',(-10.3098880524291,15.2,-3.46900388897341));
#272332=CARTESIAN_POINT('Ctrl Pts',(-10.3129114917188,15.2,-3.47126657521817));
#272333=CARTESIAN_POINT('Ctrl Pts',(-10.3159349305965,15.2,-3.47352926115465));
#272334=CARTESIAN_POINT('Ctrl Pts',(-10.3189666405635,15.2,-3.47580599606413));
#272335=CARTESIAN_POINT('Ctrl Pts',(-10.3220064815363,15.2,-3.47809678187542));
#272336=CARTESIAN_POINT('Ctrl Pts',(-10.3250463229234,15.2,-3.48038756799883));
#272337=CARTESIAN_POINT('Ctrl Pts',(-10.3280942959362,15.2,-3.48269240520968));
#272338=CARTESIAN_POINT('Ctrl Pts',(-10.3311502614917,15.2,-3.48501129672495));
#272339=CARTESIAN_POINT('Ctrl Pts',(-10.3342062270471,15.2,-3.48733018824023));
#272340=CARTESIAN_POINT('Ctrl Pts',(-10.3372701884479,15.2,-3.48966313395713));
#272341=CARTESIAN_POINT('Ctrl Pts',(-10.3403420052273,15.2,-3.49201013614203));
#272342=CARTESIAN_POINT('Ctrl Pts',(-10.3434138215881,15.2,-3.49435713800716));
#272343=CARTESIAN_POINT('Ctrl Pts',(-10.3464934962197,15.2,-3.49671819684843));
#272344=CARTESIAN_POINT('Ctrl Pts',(-10.3495808919813,15.2,-3.49909331399834));
#272345=CARTESIAN_POINT('Ctrl Pts',(-10.3526682881635,15.2,-3.50146843147186));
#272346=CARTESIAN_POINT('Ctrl Pts',(-10.3557634060541,15.2,-3.50385760800215));
#272347=CARTESIAN_POINT('Ctrl Pts',(-10.3588661115573,15.2,-3.50626084363456));
#272348=CARTESIAN_POINT('Ctrl Pts',(-10.3619688166378,15.2,-3.50866407893954));
#272349=CARTESIAN_POINT('Ctrl Pts',(-10.3650791111006,15.2,-3.5110813765899));
#272350=CARTESIAN_POINT('Ctrl Pts',(-10.3681968595119,15.2,-3.51351273383466));
#272351=CARTESIAN_POINT('Ctrl Pts',(-10.371314608348,15.2,-3.5159440914107));
#272352=CARTESIAN_POINT('Ctrl Pts',(-10.3744398117545,15.2,-3.51838951047657));
#272353=CARTESIAN_POINT('Ctrl Pts',(-10.3775723399713,15.2,-3.52084899262359));
#272354=CARTESIAN_POINT('Ctrl Pts',(-10.3807048677612,15.2,-3.52330847443551));
#272355=CARTESIAN_POINT('Ctrl Pts',(-10.3838447177117,15.2,-3.52578201770102));
#272356=CARTESIAN_POINT('Ctrl Pts',(-10.3869917620095,15.2,-3.52826962349673));
#272357=CARTESIAN_POINT('Ctrl Pts',(-10.3901388067361,15.2,-3.53075722963138));
#272358=CARTESIAN_POINT('Ctrl Pts',(-10.3932930434469,15.2,-3.53325889711217));
#272359=CARTESIAN_POINT('Ctrl Pts',(-10.3964543455085,15.2,-3.53577462847242));
#272360=CARTESIAN_POINT('Ctrl Pts',(-10.3996156471394,15.2,-3.53829035948991));
#272361=CARTESIAN_POINT('Ctrl Pts',(-10.4027840118273,15.2,-3.540820151774));
#272362=CARTESIAN_POINT('Ctrl Pts',(-10.4059593129559,15.2,-3.54336400684238));
#272363=CARTESIAN_POINT('Ctrl Pts',(-10.4091346145171,15.2,-3.54590786225736));
#272364=CARTESIAN_POINT('Ctrl Pts',(-10.4123168524667,15.2,-3.54846578042204));
#272365=CARTESIAN_POINT('Ctrl Pts',(-10.4155058987105,15.2,-3.55103775801838));
#272366=CARTESIAN_POINT('Ctrl Pts',(-10.4186949445199,15.2,-3.55360973526429));
#272367=CARTESIAN_POINT('Ctrl Pts',(-10.421890800525,15.2,-3.55619577468885));
#272368=CARTESIAN_POINT('Ctrl Pts',(-10.4250933389847,15.2,-3.55879587380818));
#272369=CARTESIAN_POINT('Ctrl Pts',(-10.4282958778808,15.2,-3.56139597328176));
#272370=CARTESIAN_POINT('Ctrl Pts',(-10.431505100697,15.2,-3.5640101331206));
#272371=CARTESIAN_POINT('Ctrl Pts',(-10.4347208809834,15.2,-3.56663835054162));
#272372=CARTESIAN_POINT('Ctrl Pts',(-10.4379366612697,15.2,-3.56926656796264));
#272373=CARTESIAN_POINT('Ctrl Pts',(-10.441159000893,15.2,-3.57190884457696));
#272374=CARTESIAN_POINT('Ctrl Pts',(-10.4443877745696,15.2,-3.57456517616761));
#272375=CARTESIAN_POINT('Ctrl Pts',(-10.4476165478063,15.2,-3.57722150739633));
#272376=CARTESIAN_POINT('Ctrl Pts',(-10.4508517572842,15.2,-3.57989189565267));
#272377=CARTESIAN_POINT('Ctrl Pts',(-10.4540932777562,15.2,-3.58257633805647));
#272378=CARTESIAN_POINT('Ctrl Pts',(-10.4573347986697,15.2,-3.58526078082602));
#272379=CARTESIAN_POINT('Ctrl Pts',(-10.4605826327263,15.2,-3.58795927716365));
#272380=CARTESIAN_POINT('Ctrl Pts',(-10.4638366570154,15.2,-3.5906718247018));
#272381=CARTESIAN_POINT('Ctrl Pts',(-10.4670906808611,15.2,-3.59338437187037));
#272382=CARTESIAN_POINT('Ctrl Pts',(-10.4703508946366,15.2,-3.59611097056212));
#272383=CARTESIAN_POINT('Ctrl Pts',(-10.4736171797581,15.2,-3.59885161755938));
#272384=CARTESIAN_POINT('Ctrl Pts',(-10.4768834653246,15.2,-3.60159226493005));
#272385=CARTESIAN_POINT('Ctrl Pts',(-10.4801558212383,15.2,-3.6043469596919));
#272386=CARTESIAN_POINT('Ctrl Pts',(-10.4834341276924,15.2,-3.60711570059347));
#272387=CARTESIAN_POINT('Ctrl Pts',(-10.4867124336999,15.2,-3.60988444111779));
#272388=CARTESIAN_POINT('Ctrl Pts',(-10.4899966905866,15.2,-3.61266722592879));
#272389=CARTESIAN_POINT('Ctrl Pts',(-10.4932867797061,15.2,-3.61546405225478));
#272390=CARTESIAN_POINT('Ctrl Pts',(-10.4965768692739,15.2,-3.61826087896184));
#272391=CARTESIAN_POINT('Ctrl Pts',(-10.4998727905591,15.2,-3.62107174573727));
#272392=CARTESIAN_POINT('Ctrl Pts',(-10.5031744274617,15.2,-3.6238966504477));
#272393=CARTESIAN_POINT('Ctrl Pts',(-10.5064760639143,15.2,-3.62672155477323));
#272394=CARTESIAN_POINT('Ctrl Pts',(-10.509783414714,15.2,-3.62956049639464));
#272395=CARTESIAN_POINT('Ctrl Pts',(-10.5130963640527,15.2,-3.63241347030272));
#272396=CARTESIAN_POINT('Ctrl Pts',(-10.5164093138427,15.2,-3.63526644459952));
#272397=CARTESIAN_POINT('Ctrl Pts',(-10.5197278608097,15.2,-3.6381334514749));
#272398=CARTESIAN_POINT('Ctrl Pts',(-10.5230518917135,15.2,-3.64101448624395));
#272399=CARTESIAN_POINT('Ctrl Pts',(-10.5263759221644,15.2,-3.64389552062046));
#272400=CARTESIAN_POINT('Ctrl Pts',(-10.5297054338141,15.2,-3.64679058244413));
#272401=CARTESIAN_POINT('Ctrl Pts',(-10.5330403149298,15.2,-3.64969966748266));
#272402=CARTESIAN_POINT('Ctrl Pts',(-10.5363751964999,15.2,-3.65260875291756));
#272403=CARTESIAN_POINT('Ctrl Pts',(-10.5397154450937,15.2,-3.65553186073961));
#272404=CARTESIAN_POINT('Ctrl Pts',(-10.5430609487356,15.2,-3.65846898680196));
#272405=CARTESIAN_POINT('Ctrl Pts',(-10.5464064519218,15.2,-3.66140611246413));
#272406=CARTESIAN_POINT('Ctrl Pts',(-10.5497572096734,15.2,-3.6643572552701));
#272407=CARTESIAN_POINT('Ctrl Pts',(-10.5531131076764,15.2,-3.66732240958183));
#272408=CARTESIAN_POINT('Ctrl Pts',(-10.5556300317501,15.2,-3.66954627582062));
#272409=CARTESIAN_POINT('Ctrl Pts',(-10.5581498485163,15.2,-3.67177802294497));
#272410=CARTESIAN_POINT('Ctrl Pts',(-10.5606725100083,15.2,-3.67401764972987));
#272411=CARTESIAN_POINT('Ctrl Pts',(-10.563195171042,15.2,-3.67625727610791));
#272412=CARTESIAN_POINT('Ctrl Pts',(-10.5657206770006,15.2,-3.67850478189386));
#272413=CARTESIAN_POINT('Ctrl Pts',(-10.568248980534,15.2,-3.68076016377093));
#272414=CARTESIAN_POINT('Ctrl Pts',(-10.5707772840674,15.2,-3.68301554564799));
#272415=CARTESIAN_POINT('Ctrl Pts',(-10.5733083851495,15.2,-3.68527880414086));
#272416=CARTESIAN_POINT('Ctrl Pts',(-10.5758422377357,15.2,-3.68754993602703));
#272417=CARTESIAN_POINT('Ctrl Pts',(-10.5783760903218,15.2,-3.68982106791319));
#272418=CARTESIAN_POINT('Ctrl Pts',(-10.5809126948451,15.2,-3.69210007368729));
#272419=CARTESIAN_POINT('Ctrl Pts',(-10.5834520029727,15.2,-3.69438695053122));
#272420=CARTESIAN_POINT('Ctrl Pts',(-10.5868377474504,15.2,-3.69743611993342));
#272421=CARTESIAN_POINT('Ctrl Pts',(-10.5902283002085,15.2,-3.70049928002284));
#272422=CARTESIAN_POINT('Ctrl Pts',(-10.5936235525052,15.2,-3.70357642796975));
#272423=CARTESIAN_POINT('Ctrl Pts',(-10.5961699914963,15.2,-3.7058842887203));
#272424=CARTESIAN_POINT('Ctrl Pts',(-10.598719073554,15.2,-3.70820001622045));
#272425=CARTESIAN_POINT('Ctrl Pts',(-10.6012707530449,15.2,-3.71052360755336));
#272426=CARTESIAN_POINT('Ctrl Pts',(-10.6038224325357,15.2,-3.71284719888628));
#272427=CARTESIAN_POINT('Ctrl Pts',(-10.6063767084503,15.2,-3.71517865412643));
#272428=CARTESIAN_POINT('Ctrl Pts',(-10.608933537494,15.2,-3.71751797001042));
#272429=CARTESIAN_POINT('Ctrl Pts',(-10.6114903665377,15.2,-3.7198572858944));
#272430=CARTESIAN_POINT('Ctrl Pts',(-10.6140497478458,15.2,-3.72220446215606));
#272431=CARTESIAN_POINT('Ctrl Pts',(-10.6166116349727,15.2,-3.72455949695616));
#272432=CARTESIAN_POINT('Ctrl Pts',(-10.6191735220996,15.2,-3.72691453175626));
#272433=CARTESIAN_POINT('Ctrl Pts',(-10.6217379161138,15.2,-3.72927742364517));
#272434=CARTESIAN_POINT('Ctrl Pts',(-10.624304771187,15.2,-3.73164816997501));
#272435=CARTESIAN_POINT('Ctrl Pts',(-10.6268716262601,15.2,-3.73401891630486));
#272436=CARTESIAN_POINT('Ctrl Pts',(-10.6294409427498,15.2,-3.73639751703417));
#272437=CARTESIAN_POINT('Ctrl Pts',(-10.6320126771977,15.2,-3.73878396798805));
#272438=CARTESIAN_POINT('Ctrl Pts',(-10.6345844121128,15.2,-3.74117041937548));
#272439=CARTESIAN_POINT('Ctrl Pts',(-10.6371585627536,15.2,-3.74356472287346));
#272440=CARTESIAN_POINT('Ctrl Pts',(-10.6397350858367,15.2,-3.74596687272364));
#272441=CARTESIAN_POINT('Ctrl Pts',(-10.6423116084518,15.2,-3.74836902213742));
#272442=CARTESIAN_POINT('Ctrl Pts',(-10.644890504014,15.2,-3.75077901900063));
#272443=CARTESIAN_POINT('Ctrl Pts',(-10.6474717277161,15.2,-3.75319685995116));
#272444=CARTESIAN_POINT('Ctrl Pts',(-10.6500529514182,15.2,-3.75561470090168));
#272445=CARTESIAN_POINT('Ctrl Pts',(-10.652636502459,15.2,-3.75804038595309));
#272446=CARTESIAN_POINT('Ctrl Pts',(-10.6552223380319,15.2,-3.76047391078201));
#272447=CARTESIAN_POINT('Ctrl Pts',(-10.6578081736048,15.2,-3.76290743561094));
#272448=CARTESIAN_POINT('Ctrl Pts',(-10.6603962934108,15.2,-3.76534880048895));
#272449=CARTESIAN_POINT('Ctrl Pts',(-10.6629866534834,15.2,-3.76779800177495));
#272450=CARTESIAN_POINT('Ctrl Pts',(-10.6655770135559,15.2,-3.77024720306095));
#272451=CARTESIAN_POINT('Ctrl Pts',(-10.6681696134284,15.2,-3.77270423972167));
#272452=CARTESIAN_POINT('Ctrl Pts',(-10.6707644109589,15.2,-3.77516911000642));
#272453=CARTESIAN_POINT('Ctrl Pts',(-10.6733592084894,15.2,-3.77763398029118));
#272454=CARTESIAN_POINT('Ctrl Pts',(-10.6759562027948,15.2,-3.78010668256707));
#272455=CARTESIAN_POINT('Ctrl Pts',(-10.6785553499918,15.2,-3.78258721343421));
#272456=CARTESIAN_POINT('Ctrl Pts',(-10.6811544976609,15.2,-3.78506774475199));
#272457=CARTESIAN_POINT('Ctrl Pts',(-10.6837558001723,15.2,-3.78755610499696));
#272458=CARTESIAN_POINT('Ctrl Pts',(-10.6863592123009,15.2,-3.79005228977747));
#272459=CARTESIAN_POINT('Ctrl Pts',(-10.6889626239566,15.2,-3.7925484741045));
#272460=CARTESIAN_POINT('Ctrl Pts',(-10.6915681458188,15.2,-3.79505248330087));
#272461=CARTESIAN_POINT('Ctrl Pts',(-10.6941757360212,15.2,-3.79756431275268));
#272462=CARTESIAN_POINT('Ctrl Pts',(-10.6967833262237,15.2,-3.80007614220449));
#272463=CARTESIAN_POINT('Ctrl Pts',(-10.6993929836795,15.2,-3.80259579225008));
#272464=CARTESIAN_POINT('Ctrl Pts',(-10.7020046667931,15.2,-3.80512325857559));
#272465=CARTESIAN_POINT('Ctrl Pts',(-10.7046163499067,15.2,-3.8076507249011));
#272466=CARTESIAN_POINT('Ctrl Pts',(-10.7072300578284,15.2,-3.81018600720901));
#272467=CARTESIAN_POINT('Ctrl Pts',(-10.7098457489417,15.2,-3.81272910199162));
#272468=CARTESIAN_POINT('Ctrl Pts',(-10.712461440055,15.2,-3.81527219677424));
#272469=CARTESIAN_POINT('Ctrl Pts',(-10.7150791141766,15.2,-3.81782310269817));
#272470=CARTESIAN_POINT('Ctrl Pts',(-10.7176987292062,15.2,-3.82038181697953));
#272471=CARTESIAN_POINT('Ctrl Pts',(-10.721191549563,15.2,-3.82379343633122));
#272472=CARTESIAN_POINT('Ctrl Pts',(-10.7246878198781,15.2,-3.82721893633585));
#272473=CARTESIAN_POINT('Ctrl Pts',(-10.7281874412995,15.2,-3.83065830597411));
#272474=CARTESIAN_POINT('Ctrl Pts',(-10.7308121571272,15.2,-3.83323783296851));
#272475=CARTESIAN_POINT('Ctrl Pts',(-10.7334387577986,15.2,-3.8358251619599));
#272476=CARTESIAN_POINT('Ctrl Pts',(-10.7360672015366,15.2,-3.83842028778296));
#272477=CARTESIAN_POINT('Ctrl Pts',(-10.7386956452746,15.2,-3.84101541360602));
#272478=CARTESIAN_POINT('Ctrl Pts',(-10.7413259330123,15.2,-3.84361833651148));
#272479=CARTESIAN_POINT('Ctrl Pts',(-10.7439580227084,15.2,-3.84622905274996));
#272480=CARTESIAN_POINT('Ctrl Pts',(-10.7474674759552,15.2,-3.84971000805078));
#272481=CARTESIAN_POINT('Ctrl Pts',(-10.7509801356163,15.2,-3.85320481629488));
#272482=CARTESIAN_POINT('Ctrl Pts',(-10.7544959008082,15.2,-3.85671346709863));
#272483=CARTESIAN_POINT('Ctrl Pts',(-10.7580116655211,15.2,-3.86022211742432));
#272484=CARTESIAN_POINT('Ctrl Pts',(-10.7615305356029,15.2,-3.8637446105123));
#272485=CARTESIAN_POINT('Ctrl Pts',(-10.7650524129976,15.2,-3.86728093473922));
#272486=CARTESIAN_POINT('Ctrl Pts',(-10.7676938211637,15.2,-3.86993317802986));
#272487=CARTESIAN_POINT('Ctrl Pts',(-10.770336920208,15.2,-3.87259320084024));
#272488=CARTESIAN_POINT('Ctrl Pts',(-10.7729816739035,15.2,-3.87526099870097));
#272489=CARTESIAN_POINT('Ctrl Pts',(-10.7756264275989,15.2,-3.87792879656169));
#272490=CARTESIAN_POINT('Ctrl Pts',(-10.7782728361025,15.2,-3.88060437059689));
#272491=CARTESIAN_POINT('Ctrl Pts',(-10.7809208606728,15.2,-3.883287714415));
#272492=CARTESIAN_POINT('Ctrl Pts',(-10.7835688857241,15.2,-3.88597105872058));
#272493=CARTESIAN_POINT('Ctrl Pts',(-10.7862185270425,15.2,-3.88866217361171));
#272494=CARTESIAN_POINT('Ctrl Pts',(-10.7888697345947,15.2,-3.89136105337999));
#272495=CARTESIAN_POINT('Ctrl Pts',(-10.7915209416652,15.2,-3.89405993265798));
#272496=CARTESIAN_POINT('Ctrl Pts',(-10.7941737152272,15.2,-3.89676657630398));
#272497=CARTESIAN_POINT('Ctrl Pts',(-10.7968280103053,15.2,-3.89948097875854));
#272498=CARTESIAN_POINT('Ctrl Pts',(-10.7994823053833,15.2,-3.9021953812131));
#272499=CARTESIAN_POINT('Ctrl Pts',(-10.802138123266,15.2,-3.9049175422178));
#272500=CARTESIAN_POINT('Ctrl Pts',(-10.8047954455073,15.2,-3.90764745961307));
#272501=CARTESIAN_POINT('Ctrl Pts',(-10.8074527677486,15.2,-3.91037737700834));
#272502=CARTESIAN_POINT('Ctrl Pts',(-10.8101115924531,15.2,-3.91311505550024));
#272503=CARTESIAN_POINT('Ctrl Pts',(-10.8127719255158,15.2,-3.91586047850026));
#272504=CARTESIAN_POINT('Ctrl Pts',(-9.86852965800006,12.2,-3.20199116200001));
#272505=CARTESIAN_POINT('Ctrl Pts',(-9.87017542455281,12.2,-3.20268658157505));
#272506=CARTESIAN_POINT('Ctrl Pts',(-9.87187175388031,12.2,-3.2034091851285));
#272507=CARTESIAN_POINT('Ctrl Pts',(-9.87361750383377,12.2,-3.20415921016783));
#272508=CARTESIAN_POINT('Ctrl Pts',(-9.87537167267595,12.2,-3.204912852207));
#272509=CARTESIAN_POINT('Ctrl Pts',(-9.87717574023296,12.2,-3.20569417462551));
#272510=CARTESIAN_POINT('Ctrl Pts',(-9.87902857842933,12.2,-3.20650338954498));
#272511=CARTESIAN_POINT('Ctrl Pts',(-9.88088141645739,12.2,-3.20731260439096));
#272512=CARTESIAN_POINT('Ctrl Pts',(-9.88278302851245,12.2,-3.2081497105564));
#272513=CARTESIAN_POINT('Ctrl Pts',(-9.88473231752497,12.2,-3.20901491227497));
#272514=CARTESIAN_POINT('Ctrl Pts',(-9.88668160653749,12.2,-3.20988011399353));
#272515=CARTESIAN_POINT('Ctrl Pts',(-9.88867857432724,12.2,-3.21077340827496));
#272516=CARTESIAN_POINT('Ctrl Pts',(-9.89072215651907,12.2,-3.21169499220255));
#272517=CARTESIAN_POINT('Ctrl Pts',(-9.89276573889652,12.2,-3.21261657621385));
#272518=CARTESIAN_POINT('Ctrl Pts',(-9.89485593802995,12.2,-3.21356644793469));
#272519=CARTESIAN_POINT('Ctrl Pts',(-9.89699171648278,12.2,-3.21454479382328));
#272520=CARTESIAN_POINT('Ctrl Pts',(-9.89912749474163,12.2,-3.21552313962301));
#272521=CARTESIAN_POINT('Ctrl Pts',(-9.90130885331331,12.2,-3.21652996002495));
#272522=CARTESIAN_POINT('Ctrl Pts',(-9.90353478649266,12.2,-3.2175654317421));
#272523=CARTESIAN_POINT('Ctrl Pts',(-9.90576071967203,12.2,-3.21860090345926));
#272524=CARTESIAN_POINT('Ctrl Pts',(-9.90803122770171,12.2,-3.21966502577315));
#272525=CARTESIAN_POINT('Ctrl Pts',(-9.91034532736571,12.2,-3.22075797048219));
#272526=CARTESIAN_POINT('Ctrl Pts',(-9.91265942723992,12.2,-3.22185091529049));
#272527=CARTESIAN_POINT('Ctrl Pts',(-9.91501712228624,12.2,-3.22297268096071));
#272528=CARTESIAN_POINT('Ctrl Pts',(-9.91741745500329,12.2,-3.22412343085874));
#272529=CARTESIAN_POINT('Ctrl Pts',(-9.91981778750232,12.2,-3.22527418065224));
#272530=CARTESIAN_POINT('Ctrl Pts',(-9.92226075844071,12.2,-3.22645391558362));
#272531=CARTESIAN_POINT('Ctrl Pts',(-9.92474543535223,12.2,-3.22766278929097));
#272532=CARTESIAN_POINT('Ctrl Pts',(-9.92723011226377,12.2,-3.22887166299831));
#272533=CARTESIAN_POINT('Ctrl Pts',(-9.92975649757194,12.2,-3.23010967648667));
#272534=CARTESIAN_POINT('Ctrl Pts',(-9.93232368131025,12.2,-3.23137697818935));
#272535=CARTESIAN_POINT('Ctrl Pts',(-9.93489086504854,12.2,-3.23264427989204));
#272536=CARTESIAN_POINT('Ctrl Pts',(-9.937498847977,12.2,-3.23394087139731));
#272537=CARTESIAN_POINT('Ctrl Pts',(-9.94014674371137,12.2,-3.2352668930971));
#272538=CARTESIAN_POINT('Ctrl Pts',(-9.94279463968627,12.2,-3.23659291491734));
#272539=CARTESIAN_POINT('Ctrl Pts',(-9.94548244775676,12.2,-3.2379483681488));
#272540=CARTESIAN_POINT('Ctrl Pts',(-9.9482093021571,12.2,-3.23933338705891));
#272541=CARTESIAN_POINT('Ctrl Pts',(-9.95093615630974,12.2,-3.24071840584321));
#272542=CARTESIAN_POINT('Ctrl Pts',(-9.953702059163,12.2,-3.24213299364531));
#272543=CARTESIAN_POINT('Ctrl Pts',(-9.95650616499039,12.2,-3.24357727726598));
#272544=CARTESIAN_POINT('Ctrl Pts',(-9.95931027081779,12.2,-3.24502156088664));
#272545=CARTESIAN_POINT('Ctrl Pts',(-9.96215257803497,12.2,-3.24649554081773));
#272546=CARTESIAN_POINT('Ctrl Pts',(-9.96503226217778,12.2,-3.24799934334439));
#272547=CARTESIAN_POINT('Ctrl Pts',(-9.96791194658215,12.2,-3.24950314600764));
#272548=CARTESIAN_POINT('Ctrl Pts',(-9.97082900750689,12.2,-3.25103676921545));
#272549=CARTESIAN_POINT('Ctrl Pts',(-9.97378263891945,12.2,-3.25260033280197));
#272550=CARTESIAN_POINT('Ctrl Pts',(-9.97673627006372,12.2,-3.25416389624646));
#272551=CARTESIAN_POINT('Ctrl Pts',(-9.97972647121991,12.2,-3.25575739992591));
#272552=CARTESIAN_POINT('Ctrl Pts',(-9.9827524515403,12.2,-3.25738095645757));
#272553=CARTESIAN_POINT('Ctrl Pts',(-9.98577843186071,12.2,-3.25900451298923));
#272554=CARTESIAN_POINT('Ctrl Pts',(-9.98884019241067,12.2,-3.26065812320466));
#272555=CARTESIAN_POINT('Ctrl Pts',(-9.99193696262912,12.2,-3.26234189455811));
#272556=CARTESIAN_POINT('Ctrl Pts',(-9.99503373312888,12.2,-3.26402566606449));
#272557=CARTESIAN_POINT('Ctrl Pts',(-9.99816551050701,12.2,-3.26573959840983));
#272558=CARTESIAN_POINT('Ctrl Pts',(-10.0013315413397,12.2,-3.2674837951771));
#272559=CARTESIAN_POINT('Ctrl Pts',(-10.0044975718848,12.2,-3.26922799178594));
#272560=CARTESIAN_POINT('Ctrl Pts',(-10.0076978541008,12.2,-3.27100245334886));
#272561=CARTESIAN_POINT('Ctrl Pts',(-10.0109316504833,12.2,-3.27280727678329));
#272562=CARTESIAN_POINT('Ctrl Pts',(-10.0141654468658,12.2,-3.27461210021773));
#272563=CARTESIAN_POINT('Ctrl Pts',(-10.0174327550794,12.2,-3.27644728653758));
#272564=CARTESIAN_POINT('Ctrl Pts',(-10.0207328517058,12.2,-3.27831292881123));
#272565=CARTESIAN_POINT('Ctrl Pts',(-10.024032948632,12.2,-3.28017857125434));
#272566=CARTESIAN_POINT('Ctrl Pts',(-10.0273658332478,12.2,-3.28207466921121));
#272567=CARTESIAN_POINT('Ctrl Pts',(-10.0307307971001,12.2,-3.28400131173497));
#272568=CARTESIAN_POINT('Ctrl Pts',(-10.0340957606467,12.2,-3.28592795408371));
#272569=CARTESIAN_POINT('Ctrl Pts',(-10.0374928009605,12.2,-3.28788514203065));
#272570=CARTESIAN_POINT('Ctrl Pts',(-10.0409212255182,12.2,-3.28987295846753));
#272571=CARTESIAN_POINT('Ctrl Pts',(-10.044349650076,12.2,-3.29186077490442));
#272572=CARTESIAN_POINT('Ctrl Pts',(-10.0478094564797,12.2,-3.29387922119753));
#272573=CARTESIAN_POINT('Ctrl Pts',(-10.0512999632682,12.2,-3.29592837662175));
#272574=CARTESIAN_POINT('Ctrl Pts',(-10.054208719031,12.2,-3.29763600620398));
#272575=CARTESIAN_POINT('Ctrl Pts',(-10.0571387938471,12.2,-3.29936496208675));
#272576=CARTESIAN_POINT('Ctrl Pts',(-10.0600898020405,12.2,-3.30111528812729));
#272577=CARTESIAN_POINT('Ctrl Pts',(-10.0630408102338,12.2,-3.30286561416783));
#272578=CARTESIAN_POINT('Ctrl Pts',(-10.0660127512293,12.2,-3.30463730936312));
#272579=CARTESIAN_POINT('Ctrl Pts',(-10.0690052420067,12.2,-3.30643041798232));
#272580=CARTESIAN_POINT('Ctrl Pts',(-10.0719977327841,12.2,-3.30822352660152));
#272581=CARTESIAN_POINT('Ctrl Pts',(-10.07501077405,12.2,-3.31003804834439));
#272582=CARTESIAN_POINT('Ctrl Pts',(-10.0780439907167,12.2,-3.31187402202496));
#272583=CARTESIAN_POINT('Ctrl Pts',(-10.0810772073834,12.2,-3.31370999570553));
#272584=CARTESIAN_POINT('Ctrl Pts',(-10.0841305999877,12.2,-3.31556742195907));
#272585=CARTESIAN_POINT('Ctrl Pts',(-10.0872037960433,12.2,-3.31744634050932));
#272586=CARTESIAN_POINT('Ctrl Pts',(-10.090276992099,12.2,-3.31932525905957));
#272587=CARTESIAN_POINT('Ctrl Pts',(-10.0933699960638,12.2,-3.32122566818577));
#272588=CARTESIAN_POINT('Ctrl Pts',(-10.0964824387037,12.2,-3.32314760665912));
#272589=CARTESIAN_POINT('Ctrl Pts',(-10.0995948813436,12.2,-3.32506954513246));
#272590=CARTESIAN_POINT('Ctrl Pts',(-10.1027267670941,12.2,-3.32701301197191));
#272591=CARTESIAN_POINT('Ctrl Pts',(-10.1058777332062,12.2,-3.32897804065361));
#272592=CARTESIAN_POINT('Ctrl Pts',(-10.1090286993183,12.2,-3.3309430693353));
#272593=CARTESIAN_POINT('Ctrl Pts',(-10.1121987497985,12.2,-3.33292966151467));
#272594=CARTESIAN_POINT('Ctrl Pts',(-10.1153875285702,12.2,-3.33493785099149));
#272595=CARTESIAN_POINT('Ctrl Pts',(-10.1185763073419,12.2,-3.3369460404683));
#272596=CARTESIAN_POINT('Ctrl Pts',(-10.121783815176,12.2,-3.3389758262332));
#272597=CARTESIAN_POINT('Ctrl Pts',(-10.1250097044136,12.2,-3.34102723977662));
#272598=CARTESIAN_POINT('Ctrl Pts',(-10.1282355936512,12.2,-3.34307865332006));
#272599=CARTESIAN_POINT('Ctrl Pts',(-10.131479863653,12.2,-3.3451516946333));
#272600=CARTESIAN_POINT('Ctrl Pts',(-10.1347421721267,12.2,-3.34724639477395));
#272601=CARTESIAN_POINT('Ctrl Pts',(-10.1380044802448,12.2,-3.34934109468629));
#272602=CARTESIAN_POINT('Ctrl Pts',(-10.1412848268184,12.2,-3.35145745227179));
#272603=CARTESIAN_POINT('Ctrl Pts',(-10.1445828725686,12.2,-3.35359549641198));
#272604=CARTESIAN_POINT('Ctrl Pts',(-10.1485405281159,12.2,-3.35616114979969));
#272605=CARTESIAN_POINT('Ctrl Pts',(-10.152523672949,12.2,-3.35875803192372));
#272606=CARTESIAN_POINT('Ctrl Pts',(-10.1565317286685,12.2,-3.36138619015165));
#272607=CARTESIAN_POINT('Ctrl Pts',(-10.1598717749195,12.2,-3.36357632188889));
#272608=CARTESIAN_POINT('Ctrl Pts',(-10.1632291239811,12.2,-3.36578817017837));
#272609=CARTESIAN_POINT('Ctrl Pts',(-10.1666034437041,12.2,-3.36802176288784));
#272610=CARTESIAN_POINT('Ctrl Pts',(-10.1699777634272,12.2,-3.3702553555973));
#272611=CARTESIAN_POINT('Ctrl Pts',(-10.1733690573854,12.2,-3.37251069268799));
#272612=CARTESIAN_POINT('Ctrl Pts',(-10.176777000404,12.2,-3.37478779703937));
#272613=CARTESIAN_POINT('Ctrl Pts',(-10.1801849434227,12.2,-3.37706490139075));
#272614=CARTESIAN_POINT('Ctrl Pts',(-10.1836095364654,12.2,-3.37936377212395));
#272615=CARTESIAN_POINT('Ctrl Pts',(-10.1870504602168,12.2,-3.38168443157018));
#272616=CARTESIAN_POINT('Ctrl Pts',(-10.1898031989928,12.2,-3.3835409589754));
#272617=CARTESIAN_POINT('Ctrl Pts',(-10.192566389873,12.2,-3.38541143248989));
#272618=CARTESIAN_POINT('Ctrl Pts',(-10.1953398707567,12.2,-3.38729586111271));
#272619=CARTESIAN_POINT('Ctrl Pts',(-10.1988067221448,12.2,-3.38965139708379));
#272620=CARTESIAN_POINT('Ctrl Pts',(-10.2022896549545,12.2,-3.3920287397045));
#272621=CARTESIAN_POINT('Ctrl Pts',(-10.2057883537898,12.2,-3.39442790804865));
#272622=CARTESIAN_POINT('Ctrl Pts',(-10.2085873130105,12.2,-3.39634724282858));
#272623=CARTESIAN_POINT('Ctrl Pts',(-10.2113963643396,12.2,-3.39828054381079));
#272624=CARTESIAN_POINT('Ctrl Pts',(-10.2142153494943,12.2,-3.40022782458501));
#272625=CARTESIAN_POINT('Ctrl Pts',(-10.2170343342648,12.2,-3.40217510509392));
#272626=CARTESIAN_POINT('Ctrl Pts',(-10.2198632526341,12.2,-3.40413636252046));
#272627=CARTESIAN_POINT('Ctrl Pts',(-10.2227019507347,12.2,-3.40611160708028));
#272628=CARTESIAN_POINT('Ctrl Pts',(-10.2255406492221,12.2,-3.40808685190924));
#272629=CARTESIAN_POINT('Ctrl Pts',(-10.2283891251487,12.2,-3.4100760822497));
#272630=CARTESIAN_POINT('Ctrl Pts',(-10.2312472264481,12.2,-3.41207930851572));
#272631=CARTESIAN_POINT('Ctrl Pts',(-10.2341053273581,12.2,-3.4140825345088));
#272632=CARTESIAN_POINT('Ctrl Pts',(-10.2369730513868,12.2,-3.41609975441768));
#272633=CARTESIAN_POINT('Ctrl Pts',(-10.2398502482066,12.2,-3.41813097825071));
#272634=CARTESIAN_POINT('Ctrl Pts',(-10.2427274454183,12.2,-3.42016220236049));
#272635=CARTESIAN_POINT('Ctrl Pts',(-10.2456141140673,12.2,-3.42220742849139));
#272636=CARTESIAN_POINT('Ctrl Pts',(-10.2485101040035,12.2,-3.4242666646601));
#272637=CARTESIAN_POINT('Ctrl Pts',(-10.2514060935452,12.2,-3.42632590054824));
#272638=CARTESIAN_POINT('Ctrl Pts',(-10.2543114045956,12.2,-3.42839914698696));
#272639=CARTESIAN_POINT('Ctrl Pts',(-10.2572258863355,12.2,-3.43048640969716));
#272640=CARTESIAN_POINT('Ctrl Pts',(-10.2601403684725,12.2,-3.43257367269174));
#272641=CARTESIAN_POINT('Ctrl Pts',(-10.2630640229044,12.2,-3.43467495284292));
#272642=CARTESIAN_POINT('Ctrl Pts',(-10.2659967002315,12.2,-3.43679025568135));
#272643=CARTESIAN_POINT('Ctrl Pts',(-10.268929377159,12.2,-3.43890555823157));
#272644=CARTESIAN_POINT('Ctrl Pts',(-10.2718710773958,12.2,-3.44103488317619));
#272645=CARTESIAN_POINT('Ctrl Pts',(-10.2748216555426,12.2,-3.4431782376662));
#272646=CARTESIAN_POINT('Ctrl Pts',(-10.2777722340914,12.2,-3.44532159244823));
#272647=CARTESIAN_POINT('Ctrl Pts',(-10.2807316885656,12.2,-3.4474789746704));
#272648=CARTESIAN_POINT('Ctrl Pts',(-10.2836998765187,12.2,-3.44965039274311));
#272649=CARTESIAN_POINT('Ctrl Pts',(-10.2866680640674,12.2,-3.45182181051995));
#272650=CARTESIAN_POINT('Ctrl Pts',(-10.2896449826096,12.2,-3.45400726117158));
#272651=CARTESIAN_POINT('Ctrl Pts',(-10.2926304907536,12.2,-3.45620675165702));
#272652=CARTESIAN_POINT('Ctrl Pts',(-10.2956159993043,12.2,-3.45840624244214));
#272653=CARTESIAN_POINT('Ctrl Pts',(-10.2986100954281,12.2,-3.46061977055912));
#272654=CARTESIAN_POINT('Ctrl Pts',(-10.3016126387584,12.2,-3.46284734329163));
#272655=CARTESIAN_POINT('Ctrl Pts',(-10.3046151820887,12.2,-3.46507491602413));
#272656=CARTESIAN_POINT('Ctrl Pts',(-10.3076261720144,12.2,-3.46731653206384));
#272657=CARTESIAN_POINT('Ctrl Pts',(-10.3106454662354,12.2,-3.46957219491044));
#272658=CARTESIAN_POINT('Ctrl Pts',(-10.3136647600449,12.2,-3.4718278574497));
#272659=CARTESIAN_POINT('Ctrl Pts',(-10.3166923608546,12.2,-3.47409756675812));
#272660=CARTESIAN_POINT('Ctrl Pts',(-10.3197281277313,12.2,-3.47638132724841));
#272661=CARTESIAN_POINT('Ctrl Pts',(-10.3227638950216,12.2,-3.47866508804986));
#272662=CARTESIAN_POINT('Ctrl Pts',(-10.3258078280596,12.2,-3.48096289886718));
#272663=CARTESIAN_POINT('Ctrl Pts',(-10.3288597887824,12.2,-3.48327476366129));
#272664=CARTESIAN_POINT('Ctrl Pts',(-10.3319117490892,12.2,-3.4855866281404));
#272665=CARTESIAN_POINT('Ctrl Pts',(-10.3349717375812,12.2,-3.48791254575102));
#272666=CARTESIAN_POINT('Ctrl Pts',(-10.3380396172743,12.2,-3.4902525195588));
#272667=CARTESIAN_POINT('Ctrl Pts',(-10.3411074973854,12.2,-3.49259249368541));
#272668=CARTESIAN_POINT('Ctrl Pts',(-10.3441832677497,12.2,-3.49494652403118));
#272669=CARTESIAN_POINT('Ctrl Pts',(-10.3472667952392,12.2,-3.49731461233533));
#272670=CARTESIAN_POINT('Ctrl Pts',(-10.3503503223085,12.2,-3.49968270031683));
#272671=CARTESIAN_POINT('Ctrl Pts',(-10.3534416034951,12.2,-3.50206484678435));
#272672=CARTESIAN_POINT('Ctrl Pts',(-10.3565405064634,12.2,-3.50446105258753));
#272673=CARTESIAN_POINT('Ctrl Pts',(-10.359639409854,12.2,-3.5068572587172));
#272674=CARTESIAN_POINT('Ctrl Pts',(-10.3627459347984,12.2,-3.50926752496524));
#272675=CARTESIAN_POINT('Ctrl Pts',(-10.3658599482463,12.2,-3.51169185243161));
#272676=CARTESIAN_POINT('Ctrl Pts',(-10.36897396127,12.2,-3.51411617956767));
#272677=CARTESIAN_POINT('Ctrl Pts',(-10.3720954612795,12.2,-3.51655456731226));
#272678=CARTESIAN_POINT('Ctrl Pts',(-10.3752243185127,12.2,-3.51900701734417));
#272679=CARTESIAN_POINT('Ctrl Pts',(-10.3783531761722,12.2,-3.52145946771024));
#272680=CARTESIAN_POINT('Ctrl Pts',(-10.3814893904686,12.2,-3.52392598138622));
#272681=CARTESIAN_POINT('Ctrl Pts',(-10.3846328299737,12.2,-3.52640655624455));
#272682=CARTESIAN_POINT('Ctrl Pts',(-10.3877762690506,12.2,-3.5288871307649));
#272683=CARTESIAN_POINT('Ctrl Pts',(-10.3909269338926,12.2,-3.53138176717965));
#272684=CARTESIAN_POINT('Ctrl Pts',(-10.3940846949671,12.2,-3.53389046630646));
#272685=CARTESIAN_POINT('Ctrl Pts',(-10.3972424564718,12.2,-3.53639916577509));
#272686=CARTESIAN_POINT('Ctrl Pts',(-10.4004073145271,12.2,-3.53892192834503));
#272687=CARTESIAN_POINT('Ctrl Pts',(-10.4035791400333,12.2,-3.54145875248328));
#272688=CARTESIAN_POINT('Ctrl Pts',(-10.4067509655395,12.2,-3.54399557662153));
#272689=CARTESIAN_POINT('Ctrl Pts',(-10.4099297599355,12.2,-3.54654646340589));
#272690=CARTESIAN_POINT('Ctrl Pts',(-10.4131153935542,12.2,-3.549111411436));
#272691=CARTESIAN_POINT('Ctrl Pts',(-10.4163010267389,12.2,-3.55167635911664));
#272692=CARTESIAN_POINT('Ctrl Pts',(-10.4194935014115,12.2,-3.55425536688178));
#272693=CARTESIAN_POINT('Ctrl Pts',(-10.4226926904979,12.2,-3.55684843601486));
#272694=CARTESIAN_POINT('Ctrl Pts',(-10.42589188002,12.2,-3.55944150550125));
#272695=CARTESIAN_POINT('Ctrl Pts',(-10.4290977844856,12.2,-3.56204863494535));
#272696=CARTESIAN_POINT('Ctrl Pts',(-10.4323102780503,12.2,-3.5646698236452));
#272697=CARTESIAN_POINT('Ctrl Pts',(-10.4355227711772,12.2,-3.56729101198792));
#272698=CARTESIAN_POINT('Ctrl Pts',(-10.4387418535672,12.2,-3.56992625780935));
#272699=CARTESIAN_POINT('Ctrl Pts',(-10.4419674019697,12.2,-3.57257556209185));
#272700=CARTESIAN_POINT('Ctrl Pts',(-10.4459993378026,12.2,-3.5758871927157));
#272701=CARTESIAN_POINT('Ctrl Pts',(-10.450041376835,12.2,-3.5792207847774));
#272702=CARTESIAN_POINT('Ctrl Pts',(-10.4540932777562,12.2,-3.58257633805647));
#272703=CARTESIAN_POINT('Ctrl Pts',(-10.4573347986697,12.2,-3.58526078082602));
#272704=CARTESIAN_POINT('Ctrl Pts',(-10.4605826327263,12.2,-3.58795927716365));
#272705=CARTESIAN_POINT('Ctrl Pts',(-10.4638366570154,12.2,-3.5906718247018));
#272706=CARTESIAN_POINT('Ctrl Pts',(-10.4670906808611,12.2,-3.59338437187037));
#272707=CARTESIAN_POINT('Ctrl Pts',(-10.4703508946366,12.2,-3.59611097056212));
#272708=CARTESIAN_POINT('Ctrl Pts',(-10.4736171797581,12.2,-3.59885161755938));
#272709=CARTESIAN_POINT('Ctrl Pts',(-10.4768834653246,12.2,-3.60159226493005));
#272710=CARTESIAN_POINT('Ctrl Pts',(-10.4801558212383,12.2,-3.60434695969191));
#272711=CARTESIAN_POINT('Ctrl Pts',(-10.4834341276924,12.2,-3.60711570059347));
#272712=CARTESIAN_POINT('Ctrl Pts',(-10.4867124336999,12.2,-3.60988444111779));
#272713=CARTESIAN_POINT('Ctrl Pts',(-10.4899966905866,12.2,-3.61266722592879));
#272714=CARTESIAN_POINT('Ctrl Pts',(-10.4932867797061,12.2,-3.61546405225478));
#272715=CARTESIAN_POINT('Ctrl Pts',(-10.4965768692739,12.2,-3.61826087896184));
#272716=CARTESIAN_POINT('Ctrl Pts',(-10.4998727905591,12.2,-3.62107174573727));
#272717=CARTESIAN_POINT('Ctrl Pts',(-10.5031744274617,12.2,-3.6238966504477));
#272718=CARTESIAN_POINT('Ctrl Pts',(-10.5064760639143,12.2,-3.62672155477323));
#272719=CARTESIAN_POINT('Ctrl Pts',(-10.509783414714,12.2,-3.62956049639464));
#272720=CARTESIAN_POINT('Ctrl Pts',(-10.5130963640527,12.2,-3.63241347030272));
#272721=CARTESIAN_POINT('Ctrl Pts',(-10.5164093138427,12.2,-3.63526644459952));
#272722=CARTESIAN_POINT('Ctrl Pts',(-10.5197278608097,12.2,-3.6381334514749));
#272723=CARTESIAN_POINT('Ctrl Pts',(-10.5230518917135,12.2,-3.64101448624395));
#272724=CARTESIAN_POINT('Ctrl Pts',(-10.5263759221644,12.2,-3.64389552062046));
#272725=CARTESIAN_POINT('Ctrl Pts',(-10.529705433814,12.2,-3.64679058244413));
#272726=CARTESIAN_POINT('Ctrl Pts',(-10.5330403149298,12.2,-3.64969966748266));
#272727=CARTESIAN_POINT('Ctrl Pts',(-10.5363751964999,12.2,-3.65260875291756));
#272728=CARTESIAN_POINT('Ctrl Pts',(-10.5397154450937,12.2,-3.65553186073961));
#272729=CARTESIAN_POINT('Ctrl Pts',(-10.5430609487356,12.2,-3.65846898680196));
#272730=CARTESIAN_POINT('Ctrl Pts',(-10.5464064519218,12.2,-3.66140611246413));
#272731=CARTESIAN_POINT('Ctrl Pts',(-10.5497572096734,12.2,-3.66435725527011));
#272732=CARTESIAN_POINT('Ctrl Pts',(-10.5531131076764,12.2,-3.66732240958183));
#272733=CARTESIAN_POINT('Ctrl Pts',(-10.5556300317501,12.2,-3.66954627582063));
#272734=CARTESIAN_POINT('Ctrl Pts',(-10.5581498485163,12.2,-3.67177802294497));
#272735=CARTESIAN_POINT('Ctrl Pts',(-10.5606725100083,12.2,-3.67401764972988));
#272736=CARTESIAN_POINT('Ctrl Pts',(-10.5631951710421,12.2,-3.67625727610791));
#272737=CARTESIAN_POINT('Ctrl Pts',(-10.5657206770006,12.2,-3.67850478189387));
#272738=CARTESIAN_POINT('Ctrl Pts',(-10.568248980534,12.2,-3.68076016377093));
#272739=CARTESIAN_POINT('Ctrl Pts',(-10.5707772840674,12.2,-3.68301554564799));
#272740=CARTESIAN_POINT('Ctrl Pts',(-10.5733083851495,12.2,-3.68527880414086));
#272741=CARTESIAN_POINT('Ctrl Pts',(-10.5758422377357,12.2,-3.68754993602703));
#272742=CARTESIAN_POINT('Ctrl Pts',(-10.5783760903218,12.2,-3.68982106791319));
#272743=CARTESIAN_POINT('Ctrl Pts',(-10.5809126948451,12.2,-3.69210007368729));
#272744=CARTESIAN_POINT('Ctrl Pts',(-10.5834520029727,12.2,-3.69438695053122));
#272745=CARTESIAN_POINT('Ctrl Pts',(-10.5859913111003,12.2,-3.69667382737515));
#272746=CARTESIAN_POINT('Ctrl Pts',(-10.5885333245821,12.2,-3.69896857428344));
#272747=CARTESIAN_POINT('Ctrl Pts',(-10.5910779957394,12.2,-3.70127118924078));
#272748=CARTESIAN_POINT('Ctrl Pts',(-10.5936226668967,12.2,-3.70357380419811));
#272749=CARTESIAN_POINT('Ctrl Pts',(-10.5961699975372,12.2,-3.70588428831321));
#272750=CARTESIAN_POINT('Ctrl Pts',(-10.5987199401525,12.2,-3.70820263668624));
#272751=CARTESIAN_POINT('Ctrl Pts',(-10.6012698832311,12.2,-3.71052098548043));
#272752=CARTESIAN_POINT('Ctrl Pts',(-10.6038224389687,12.2,-3.71284719905183));
#272753=CARTESIAN_POINT('Ctrl Pts',(-10.6063775615487,12.2,-3.71518127476713));
#272754=CARTESIAN_POINT('Ctrl Pts',(-10.6089326836646,12.2,-3.7175153500584));
#272755=CARTESIAN_POINT('Ctrl Pts',(-10.6114903742769,12.2,-3.7198572866884));
#272756=CARTESIAN_POINT('Ctrl Pts',(-10.6140505855204,12.2,-3.72220708222133));
#272757=CARTESIAN_POINT('Ctrl Pts',(-10.6166107967639,12.2,-3.72455687775426));
#272758=CARTESIAN_POINT('Ctrl Pts',(-10.6191735296894,12.2,-3.7269145330432));
#272759=CARTESIAN_POINT('Ctrl Pts',(-10.6217387388047,12.2,-3.7292800424996));
#272760=CARTESIAN_POINT('Ctrl Pts',(-10.62430394792,12.2,-3.73164555195599));
#272761=CARTESIAN_POINT('Ctrl Pts',(-10.6268716330934,12.2,-3.73401891763647));
#272762=CARTESIAN_POINT('Ctrl Pts',(-10.6294417507084,12.2,-3.73640013450829));
#272763=CARTESIAN_POINT('Ctrl Pts',(-10.6320118683233,12.2,-3.73878135138012));
#272764=CARTESIAN_POINT('Ctrl Pts',(-10.6345844185798,12.2,-3.7411704204766));
#272765=CARTESIAN_POINT('Ctrl Pts',(-10.6371593546944,12.2,-3.74356733830549));
#272766=CARTESIAN_POINT('Ctrl Pts',(-10.639734290809,12.2,-3.74596425613438));
#272767=CARTESIAN_POINT('Ctrl Pts',(-10.6423116140828,12.2,-3.74836902200129));
#272768=CARTESIAN_POINT('Ctrl Pts',(-10.6448912807843,12.2,-3.75078163303326));
#272769=CARTESIAN_POINT('Ctrl Pts',(-10.6474709474858,12.2,-3.75319424406522));
#272770=CARTESIAN_POINT('Ctrl Pts',(-10.6500529570142,12.2,-3.75561470062656));
#272771=CARTESIAN_POINT('Ctrl Pts',(-10.65263726467,12.2,-3.75804299845393));
#272772=CARTESIAN_POINT('Ctrl Pts',(-10.6552215727953,12.2,-3.76047129672244));
#272773=CARTESIAN_POINT('Ctrl Pts',(-10.6578081802379,12.2,-3.7629074357765));
#272774=CARTESIAN_POINT('Ctrl Pts',(-10.6603970423227,12.2,-3.76535141300775));
#272775=CARTESIAN_POINT('Ctrl Pts',(-10.6638488576521,12.2,-3.76861004857612));
#272776=CARTESIAN_POINT('Ctrl Pts',(-10.6673046810753,12.2,-3.77188261644268));
#272777=CARTESIAN_POINT('Ctrl Pts',(-10.6707644109589,12.2,-3.77516911000642));
#272778=CARTESIAN_POINT('Ctrl Pts',(-10.6733592084894,12.2,-3.77763398029118));
#272779=CARTESIAN_POINT('Ctrl Pts',(-10.6759562027948,12.2,-3.78010668256707));
#272780=CARTESIAN_POINT('Ctrl Pts',(-10.6785553499918,12.2,-3.78258721343421));
#272781=CARTESIAN_POINT('Ctrl Pts',(-10.6811544976609,12.2,-3.78506774475199));
#272782=CARTESIAN_POINT('Ctrl Pts',(-10.6837558001723,12.2,-3.78755610499696));
#272783=CARTESIAN_POINT('Ctrl Pts',(-10.6863592123009,12.2,-3.79005228977747));
#272784=CARTESIAN_POINT('Ctrl Pts',(-10.6906982314118,12.2,-3.79421259668688));
#272785=CARTESIAN_POINT('Ctrl Pts',(-10.6950431128834,12.2,-3.79839463823787));
#272786=CARTESIAN_POINT('Ctrl Pts',(-10.6993936594227,12.2,-3.80259839666678));
#272787=CARTESIAN_POINT('Ctrl Pts',(-10.7020039880101,12.2,-3.80512065236562));
#272788=CARTESIAN_POINT('Ctrl Pts',(-10.7046163564398,12.2,-3.80765072506667));
#272789=CARTESIAN_POINT('Ctrl Pts',(-10.7072307211116,12.2,-3.81018861181157));
#272790=CARTESIAN_POINT('Ctrl Pts',(-10.7098450853086,12.2,-3.81272649809541));
#272791=CARTESIAN_POINT('Ctrl Pts',(-10.7124614470638,12.2,-3.81527219763719));
#272792=CARTESIAN_POINT('Ctrl Pts',(-10.7150797632605,12.2,-3.81782570600342));
#272793=CARTESIAN_POINT('Ctrl Pts',(-10.7176980794572,12.2,-3.82037921436965));
#272794=CARTESIAN_POINT('Ctrl Pts',(-10.7203183505024,12.2,-3.82294053218393));
#272795=CARTESIAN_POINT('Ctrl Pts',(-10.7229405342108,12.2,-3.8255096549773));
#272796=CARTESIAN_POINT('Ctrl Pts',(-10.7255627179191,12.2,-3.82807877777066));
#272797=CARTESIAN_POINT('Ctrl Pts',(-10.7281868155311,12.2,-3.83065570521315));
#272798=CARTESIAN_POINT('Ctrl Pts',(-10.7308127831977,12.2,-3.83324043300595));
#272799=CARTESIAN_POINT('Ctrl Pts',(-10.7334387508642,12.2,-3.83582516079875));
#272800=CARTESIAN_POINT('Ctrl Pts',(-10.7360665893591,12.2,-3.83841768861181));
#272801=CARTESIAN_POINT('Ctrl Pts',(-10.7386962579301,12.2,-3.84101801197499));
#272802=CARTESIAN_POINT('Ctrl Pts',(-10.7413259265011,12.2,-3.84361833533817));
#272803=CARTESIAN_POINT('Ctrl Pts',(-10.7439574243052,12.2,-3.84622645534246));
#272804=CARTESIAN_POINT('Ctrl Pts',(-10.7465907114593,12.2,-3.8488423657047));
#272805=CARTESIAN_POINT('Ctrl Pts',(-10.7492239990918,12.2,-3.85145827654216));
#272806=CARTESIAN_POINT('Ctrl Pts',(-10.7518590766748,12.2,-3.8540819787568));
#272807=CARTESIAN_POINT('Ctrl Pts',(-10.7544959008082,12.2,-3.85671346709864));
#272808=CARTESIAN_POINT('Ctrl Pts',(-10.7580116655211,12.2,-3.86022211742433));
#272809=CARTESIAN_POINT('Ctrl Pts',(-10.7615305356029,12.2,-3.86374461051231));
#272810=CARTESIAN_POINT('Ctrl Pts',(-10.7650524129976,12.2,-3.86728093473922));
#272811=CARTESIAN_POINT('Ctrl Pts',(-10.7676938211637,12.2,-3.86993317802987));
#272812=CARTESIAN_POINT('Ctrl Pts',(-10.770336920208,12.2,-3.87259320084024));
#272813=CARTESIAN_POINT('Ctrl Pts',(-10.7729816739035,12.2,-3.87526099870097));
#272814=CARTESIAN_POINT('Ctrl Pts',(-10.7756264275989,12.2,-3.87792879656169));
#272815=CARTESIAN_POINT('Ctrl Pts',(-10.7782728361025,12.2,-3.88060437059689));
#272816=CARTESIAN_POINT('Ctrl Pts',(-10.7809208606728,12.2,-3.883287714415));
#272817=CARTESIAN_POINT('Ctrl Pts',(-10.7835688857241,12.2,-3.88597105872058));
#272818=CARTESIAN_POINT('Ctrl Pts',(-10.7862185270425,12.2,-3.88866217361171));
#272819=CARTESIAN_POINT('Ctrl Pts',(-10.7888697345947,12.2,-3.89136105337999));
#272820=CARTESIAN_POINT('Ctrl Pts',(-10.7915209416652,12.2,-3.89405993265798));
#272821=CARTESIAN_POINT('Ctrl Pts',(-10.7941737152272,12.2,-3.89676657630398));
#272822=CARTESIAN_POINT('Ctrl Pts',(-10.7968280103053,12.2,-3.89948097875854));
#272823=CARTESIAN_POINT('Ctrl Pts',(-10.7994823053833,12.2,-3.9021953812131));
#272824=CARTESIAN_POINT('Ctrl Pts',(-10.802138123266,12.2,-3.9049175422178));
#272825=CARTESIAN_POINT('Ctrl Pts',(-10.8047954455073,12.2,-3.90764745961308));
#272826=CARTESIAN_POINT('Ctrl Pts',(-10.8074527677486,12.2,-3.91037737700835));
#272827=CARTESIAN_POINT('Ctrl Pts',(-10.8101115924531,12.2,-3.91311505550024));
#272828=CARTESIAN_POINT('Ctrl Pts',(-10.8127719255158,12.2,-3.91586047850026));
#272829=CARTESIAN_POINT('Origin',(-5.66257110645729E-14,15.2,-1.77635683940025E-14));
#272830=CARTESIAN_POINT('',(-9.31239140042914,15.2,-4.57383771138038));
#272831=CARTESIAN_POINT('',(-9.31239140042914,12.2,-4.57383771138038));
#272832=CARTESIAN_POINT('',(-9.31239140000006,15.2,-4.57383771100002));
#272833=CARTESIAN_POINT('Origin',(-5.66257110645729E-14,12.2,-1.77635683940025E-14));
#272834=CARTESIAN_POINT('Origin',(-5.66257110645729E-14,15.2,-1.77635683940025E-14));
#272835=CARTESIAN_POINT('Origin',(-5.66257110645729E-14,15.2,-1.77635683940025E-14));
#272836=CARTESIAN_POINT('',(-10.1454284470001,15.2,-5.41482055400001));
#272837=CARTESIAN_POINT('',(-9.95917514600006,15.2,-5.75020264100001));
#272838=CARTESIAN_POINT('Origin',(-5.66257110645729E-14,15.2,-1.77635683940025E-14));
#272839=CARTESIAN_POINT('',(-9.95917514600006,12.2,-5.75020264100001));
#272840=CARTESIAN_POINT('',(-9.95917514600006,15.2,-5.75020264100001));
#272841=CARTESIAN_POINT('',(-10.1454284470001,12.2,-5.41482055400001));
#272842=CARTESIAN_POINT('Origin',(-5.66257110645729E-14,12.2,-1.77635683940025E-14));
#272843=CARTESIAN_POINT('',(-10.1454284470001,15.2,-5.41482055400001));
#272844=CARTESIAN_POINT('Ctrl Pts',(-9.31239140100006,15.2,-4.57383771200002));
#272845=CARTESIAN_POINT('Ctrl Pts',(-9.31239140100006,11.6,-4.57383771200002));
#272846=CARTESIAN_POINT('Ctrl Pts',(-9.31254071700006,15.2,-4.57392774200001));
#272847=CARTESIAN_POINT('Ctrl Pts',(-9.31254071700006,11.6,-4.57392774200002));
#272848=CARTESIAN_POINT('Ctrl Pts',(-9.31284451800006,15.2,-4.57411102300001));
#272849=CARTESIAN_POINT('Ctrl Pts',(-9.31284451800006,11.6,-4.57411102300001));
#272850=CARTESIAN_POINT('Ctrl Pts',(-9.31330471300006,15.2,-4.57438896200001));
#272851=CARTESIAN_POINT('Ctrl Pts',(-9.31330471300006,11.6,-4.57438896200001));
#272852=CARTESIAN_POINT('Ctrl Pts',(-9.31392435800005,15.2,-4.57476383600001));
#272853=CARTESIAN_POINT('Ctrl Pts',(-9.31392435800005,11.6,-4.57476383600001));
#272854=CARTESIAN_POINT('Ctrl Pts',(-9.31470764300006,15.2,-4.57523877600002));
#272855=CARTESIAN_POINT('Ctrl Pts',(-9.31470764300006,11.6,-4.57523877600002));
#272856=CARTESIAN_POINT('Ctrl Pts',(-9.31550313900006,15.2,-4.57572221300001));
#272857=CARTESIAN_POINT('Ctrl Pts',(-9.31550313900006,11.6,-4.57572221300001));
#272858=CARTESIAN_POINT('Ctrl Pts',(-9.31630627600006,15.2,-4.57621139800001));
#272859=CARTESIAN_POINT('Ctrl Pts',(-9.31630627600006,11.6,-4.57621139800001));
#272860=CARTESIAN_POINT('Ctrl Pts',(-9.31711702100005,15.2,-4.57670633100001));
#272861=CARTESIAN_POINT('Ctrl Pts',(-9.31711702100005,11.6,-4.57670633100001));
#272862=CARTESIAN_POINT('Ctrl Pts',(-9.31793534100006,15.2,-4.57720701200001));
#272863=CARTESIAN_POINT('Ctrl Pts',(-9.31793534100006,11.6,-4.57720701200001));
#272864=CARTESIAN_POINT('Ctrl Pts',(-9.31876120500006,15.2,-4.57771344700001));
#272865=CARTESIAN_POINT('Ctrl Pts',(-9.31876120500006,11.6,-4.57771344700001));
#272866=CARTESIAN_POINT('Ctrl Pts',(-9.31959457900006,15.2,-4.57822563400001));
#272867=CARTESIAN_POINT('Ctrl Pts',(-9.31959457900006,11.6,-4.57822563400002));
#272868=CARTESIAN_POINT('Ctrl Pts',(-9.32043543400006,15.2,-4.57874357400001));
#272869=CARTESIAN_POINT('Ctrl Pts',(-9.32043543400006,11.6,-4.57874357400002));
#272870=CARTESIAN_POINT('Ctrl Pts',(-9.32128373600005,15.2,-4.57926727100002));
#272871=CARTESIAN_POINT('Ctrl Pts',(-9.32128373600005,11.6,-4.57926727100002));
#272872=CARTESIAN_POINT('Ctrl Pts',(-9.32213945400006,15.2,-4.57979672400001));
#272873=CARTESIAN_POINT('Ctrl Pts',(-9.32213945400006,11.6,-4.57979672400001));
#272874=CARTESIAN_POINT('Ctrl Pts',(-9.32300255700006,15.2,-4.58033193400002));
#272875=CARTESIAN_POINT('Ctrl Pts',(-9.32300255700006,11.6,-4.58033193400002));
#272876=CARTESIAN_POINT('Ctrl Pts',(-9.32387301400006,15.2,-4.58087290600002));
#272877=CARTESIAN_POINT('Ctrl Pts',(-9.32387301400006,11.6,-4.58087290600002));
#272878=CARTESIAN_POINT('Ctrl Pts',(-9.32475079300006,15.2,-4.58141963700001));
#272879=CARTESIAN_POINT('Ctrl Pts',(-9.32475079300006,11.6,-4.58141963700002));
#272880=CARTESIAN_POINT('Ctrl Pts',(-9.32563586400006,15.2,-4.58197212900001));
#272881=CARTESIAN_POINT('Ctrl Pts',(-9.32563586400006,11.6,-4.58197212900001));
#272882=CARTESIAN_POINT('Ctrl Pts',(-9.32652819500005,15.2,-4.58253038500001));
#272883=CARTESIAN_POINT('Ctrl Pts',(-9.32652819500005,11.6,-4.58253038500002));
#272884=CARTESIAN_POINT('Ctrl Pts',(-9.32742775700006,15.2,-4.58309440600001));
#272885=CARTESIAN_POINT('Ctrl Pts',(-9.32742775700006,11.6,-4.58309440600001));
#272886=CARTESIAN_POINT('Ctrl Pts',(-9.32833451800006,15.2,-4.58366419300001));
#272887=CARTESIAN_POINT('Ctrl Pts',(-9.32833451800006,11.6,-4.58366419300001));
#272888=CARTESIAN_POINT('Ctrl Pts',(-9.32924844800005,15.2,-4.58423974600001));
#272889=CARTESIAN_POINT('Ctrl Pts',(-9.32924844800005,11.6,-4.58423974600001));
#272890=CARTESIAN_POINT('Ctrl Pts',(-9.33016951800006,15.2,-4.58482106700002));
#272891=CARTESIAN_POINT('Ctrl Pts',(-9.33016951800006,11.6,-4.58482106700002));
#272892=CARTESIAN_POINT('Ctrl Pts',(-9.33109769500006,15.2,-4.58540815700001));
#272893=CARTESIAN_POINT('Ctrl Pts',(-9.33109769500006,11.6,-4.58540815700002));
#272894=CARTESIAN_POINT('Ctrl Pts',(-9.33203295300006,15.2,-4.58600101800001));
#272895=CARTESIAN_POINT('Ctrl Pts',(-9.33203295300006,11.6,-4.58600101800002));
#272896=CARTESIAN_POINT('Ctrl Pts',(-9.33297525900005,15.2,-4.58659964900002));
#272897=CARTESIAN_POINT('Ctrl Pts',(-9.33297525900005,11.6,-4.58659964900002));
#272898=CARTESIAN_POINT('Ctrl Pts',(-9.33392458400006,15.2,-4.58720405300001));
#272899=CARTESIAN_POINT('Ctrl Pts',(-9.33392458400006,11.6,-4.58720405300001));
#272900=CARTESIAN_POINT('Ctrl Pts',(-9.33488090000005,15.2,-4.58781423000001));
#272901=CARTESIAN_POINT('Ctrl Pts',(-9.33488090000005,11.6,-4.58781423000001));
#272902=CARTESIAN_POINT('Ctrl Pts',(-9.33584417700006,15.2,-4.58843018200001));
#272903=CARTESIAN_POINT('Ctrl Pts',(-9.33584417700006,11.6,-4.58843018200001));
#272904=CARTESIAN_POINT('Ctrl Pts',(-9.33681438400006,15.2,-4.58905190900001));
#272905=CARTESIAN_POINT('Ctrl Pts',(-9.33681438400006,11.6,-4.58905190900001));
#272906=CARTESIAN_POINT('Ctrl Pts',(-9.33779149400005,15.2,-4.58967941300001));
#272907=CARTESIAN_POINT('Ctrl Pts',(-9.33779149400005,11.6,-4.58967941300001));
#272908=CARTESIAN_POINT('Ctrl Pts',(-9.33877547800006,15.2,-4.59031269400001));
#272909=CARTESIAN_POINT('Ctrl Pts',(-9.33877547800006,11.6,-4.59031269400001));
#272910=CARTESIAN_POINT('Ctrl Pts',(-9.33976630500006,15.2,-4.59095175300002));
#272911=CARTESIAN_POINT('Ctrl Pts',(-9.33976630500006,11.6,-4.59095175300002));
#272912=CARTESIAN_POINT('Ctrl Pts',(-9.34076394800006,15.2,-4.59159659300001));
#272913=CARTESIAN_POINT('Ctrl Pts',(-9.34076394800006,11.6,-4.59159659300001));
#272914=CARTESIAN_POINT('Ctrl Pts',(-9.34176837900005,15.2,-4.59224721100002));
#272915=CARTESIAN_POINT('Ctrl Pts',(-9.34176837900005,11.6,-4.59224721100002));
#272916=CARTESIAN_POINT('Ctrl Pts',(-9.34277956900005,15.2,-4.59290361300001));
#272917=CARTESIAN_POINT('Ctrl Pts',(-9.34277956900005,11.6,-4.59290361300001));
#272918=CARTESIAN_POINT('Ctrl Pts',(-9.34379748800006,15.2,-4.59356579500001));
#272919=CARTESIAN_POINT('Ctrl Pts',(-9.34379748800006,11.6,-4.59356579500002));
#272920=CARTESIAN_POINT('Ctrl Pts',(-9.34482211000006,15.2,-4.59423376000001));
#272921=CARTESIAN_POINT('Ctrl Pts',(-9.34482211000006,11.6,-4.59423376000002));
#272922=CARTESIAN_POINT('Ctrl Pts',(-9.34585340600006,15.2,-4.59490751000001));
#272923=CARTESIAN_POINT('Ctrl Pts',(-9.34585340600006,11.6,-4.59490751000002));
#272924=CARTESIAN_POINT('Ctrl Pts',(-9.34689134900006,15.2,-4.59558704400001));
#272925=CARTESIAN_POINT('Ctrl Pts',(-9.34689134900006,11.6,-4.59558704400001));
#272926=CARTESIAN_POINT('Ctrl Pts',(-9.34793590900006,15.2,-4.59627236300001));
#272927=CARTESIAN_POINT('Ctrl Pts',(-9.34793590900006,11.6,-4.59627236300001));
#272928=CARTESIAN_POINT('Ctrl Pts',(-9.34898706000006,15.2,-4.59696346900001));
#272929=CARTESIAN_POINT('Ctrl Pts',(-9.34898706000006,11.6,-4.59696346900001));
#272930=CARTESIAN_POINT('Ctrl Pts',(-9.35004477500006,15.2,-4.59766036300001));
#272931=CARTESIAN_POINT('Ctrl Pts',(-9.35004477500006,11.6,-4.59766036300001));
#272932=CARTESIAN_POINT('Ctrl Pts',(-9.35110902500006,15.2,-4.59836304300001));
#272933=CARTESIAN_POINT('Ctrl Pts',(-9.35110902500006,11.6,-4.59836304300001));
#272934=CARTESIAN_POINT('Ctrl Pts',(-9.35217978400006,15.2,-4.59907151300001));
#272935=CARTESIAN_POINT('Ctrl Pts',(-9.35217978400006,11.6,-4.59907151300001));
#272936=CARTESIAN_POINT('Ctrl Pts',(-9.35325702300006,15.2,-4.59978577200001));
#272937=CARTESIAN_POINT('Ctrl Pts',(-9.35325702300006,11.6,-4.59978577200001));
#272938=CARTESIAN_POINT('Ctrl Pts',(-9.35434071700006,15.2,-4.60050582100001));
#272939=CARTESIAN_POINT('Ctrl Pts',(-9.35434071700006,11.6,-4.60050582100001));
#272940=CARTESIAN_POINT('Ctrl Pts',(-9.35543083700006,15.2,-4.60123166100002));
#272941=CARTESIAN_POINT('Ctrl Pts',(-9.35543083700006,11.6,-4.60123166100002));
#272942=CARTESIAN_POINT('Ctrl Pts',(-9.35652735900005,15.2,-4.60196329200001));
#272943=CARTESIAN_POINT('Ctrl Pts',(-9.35652735900005,11.6,-4.60196329200001));
#272944=CARTESIAN_POINT('Ctrl Pts',(-9.35763025400006,15.2,-4.60270071600001));
#272945=CARTESIAN_POINT('Ctrl Pts',(-9.35763025400006,11.6,-4.60270071600002));
#272946=CARTESIAN_POINT('Ctrl Pts',(-9.35873949500006,15.2,-4.60344393200002));
#272947=CARTESIAN_POINT('Ctrl Pts',(-9.35873949500006,11.6,-4.60344393200002));
#272948=CARTESIAN_POINT('Ctrl Pts',(-9.35985505600006,15.2,-4.60419294200001));
#272949=CARTESIAN_POINT('Ctrl Pts',(-9.35985505600006,11.6,-4.60419294200001));
#272950=CARTESIAN_POINT('Ctrl Pts',(-9.36097691300006,15.2,-4.60494774600001));
#272951=CARTESIAN_POINT('Ctrl Pts',(-9.36097691300006,11.6,-4.60494774600001));
#272952=CARTESIAN_POINT('Ctrl Pts',(-9.36210503700006,15.2,-4.60570834500002));
#272953=CARTESIAN_POINT('Ctrl Pts',(-9.36210503700006,11.6,-4.60570834500002));
#272954=CARTESIAN_POINT('Ctrl Pts',(-9.36323940100005,15.2,-4.60647473800002));
#272955=CARTESIAN_POINT('Ctrl Pts',(-9.36323940100005,11.6,-4.60647473800002));
#272956=CARTESIAN_POINT('Ctrl Pts',(-9.36437998200006,15.2,-4.60724692800001));
#272957=CARTESIAN_POINT('Ctrl Pts',(-9.36437998200006,11.6,-4.60724692800001));
#272958=CARTESIAN_POINT('Ctrl Pts',(-9.36552675200006,15.2,-4.60802491300001));
#272959=CARTESIAN_POINT('Ctrl Pts',(-9.36552675200006,11.6,-4.60802491300001));
#272960=CARTESIAN_POINT('Ctrl Pts',(-9.36667968600006,15.2,-4.60880869700001));
#272961=CARTESIAN_POINT('Ctrl Pts',(-9.36667968600006,11.6,-4.60880869700001));
#272962=CARTESIAN_POINT('Ctrl Pts',(-9.36783875800005,15.2,-4.60959827800002));
#272963=CARTESIAN_POINT('Ctrl Pts',(-9.36783875800005,11.6,-4.60959827800002));
#272964=CARTESIAN_POINT('Ctrl Pts',(-9.36900394300006,15.2,-4.61039365500001));
#272965=CARTESIAN_POINT('Ctrl Pts',(-9.36900394300006,11.6,-4.61039365500001));
#272966=CARTESIAN_POINT('Ctrl Pts',(-9.37017521400006,15.2,-4.61119483300001));
#272967=CARTESIAN_POINT('Ctrl Pts',(-9.37017521400006,11.6,-4.61119483300001));
#272968=CARTESIAN_POINT('Ctrl Pts',(-9.37135254700006,15.2,-4.61200180900001));
#272969=CARTESIAN_POINT('Ctrl Pts',(-9.37135254700006,11.6,-4.61200180900002));
#272970=CARTESIAN_POINT('Ctrl Pts',(-9.37253591600006,15.2,-4.61281458400002));
#272971=CARTESIAN_POINT('Ctrl Pts',(-9.37253591600006,11.6,-4.61281458400002));
#272972=CARTESIAN_POINT('Ctrl Pts',(-9.37372529600006,15.2,-4.61363315900002));
#272973=CARTESIAN_POINT('Ctrl Pts',(-9.37372529600006,11.6,-4.61363315900002));
#272974=CARTESIAN_POINT('Ctrl Pts',(-9.37492066200006,15.2,-4.61445753500001));
#272975=CARTESIAN_POINT('Ctrl Pts',(-9.37492066200006,11.6,-4.61445753500001));
#272976=CARTESIAN_POINT('Ctrl Pts',(-9.37612198900006,15.2,-4.61528771100001));
#272977=CARTESIAN_POINT('Ctrl Pts',(-9.37612198900006,11.6,-4.61528771100001));
#272978=CARTESIAN_POINT('Ctrl Pts',(-9.37732925200006,15.2,-4.61612368800001));
#272979=CARTESIAN_POINT('Ctrl Pts',(-9.37732925200006,11.6,-4.61612368800001));
#272980=CARTESIAN_POINT('Ctrl Pts',(-9.37854242600006,15.2,-4.61696546600002));
#272981=CARTESIAN_POINT('Ctrl Pts',(-9.37854242600006,11.6,-4.61696546600002));
#272982=CARTESIAN_POINT('Ctrl Pts',(-9.37976148700006,15.2,-4.61781304700001));
#272983=CARTESIAN_POINT('Ctrl Pts',(-9.37976148700006,11.6,-4.61781304700002));
#272984=CARTESIAN_POINT('Ctrl Pts',(-9.38098641000006,15.2,-4.61866643000001));
#272985=CARTESIAN_POINT('Ctrl Pts',(-9.38098641000006,11.6,-4.61866643000001));
#272986=CARTESIAN_POINT('Ctrl Pts',(-9.38221717000006,15.2,-4.61952561600001));
#272987=CARTESIAN_POINT('Ctrl Pts',(-9.38221717000006,11.6,-4.61952561600001));
#272988=CARTESIAN_POINT('Ctrl Pts',(-9.38345374400006,15.2,-4.62039060400001));
#272989=CARTESIAN_POINT('Ctrl Pts',(-9.38345374400006,11.6,-4.62039060400001));
#272990=CARTESIAN_POINT('Ctrl Pts',(-9.38469610600006,15.2,-4.62126139500001));
#272991=CARTESIAN_POINT('Ctrl Pts',(-9.38469610600006,11.6,-4.62126139500001));
#272992=CARTESIAN_POINT('Ctrl Pts',(-9.38594423300006,15.2,-4.62213799100001));
#272993=CARTESIAN_POINT('Ctrl Pts',(-9.38594423300006,11.6,-4.62213799100002));
#272994=CARTESIAN_POINT('Ctrl Pts',(-9.38719810100006,15.2,-4.62302038900001));
#272995=CARTESIAN_POINT('Ctrl Pts',(-9.38719810100006,11.6,-4.62302038900001));
#272996=CARTESIAN_POINT('Ctrl Pts',(-9.38845768500006,15.2,-4.62390859300001));
#272997=CARTESIAN_POINT('Ctrl Pts',(-9.38845768500006,11.6,-4.62390859300002));
#272998=CARTESIAN_POINT('Ctrl Pts',(-9.38972296200006,15.2,-4.62480260000001));
#272999=CARTESIAN_POINT('Ctrl Pts',(-9.38972296200006,11.6,-4.62480260000001));
#273000=CARTESIAN_POINT('Ctrl Pts',(-9.39099390900006,15.2,-4.62570241200002));
#273001=CARTESIAN_POINT('Ctrl Pts',(-9.39099390900006,11.6,-4.62570241200002));
#273002=CARTESIAN_POINT('Ctrl Pts',(-9.39227050100006,15.2,-4.62660802900002));
#273003=CARTESIAN_POINT('Ctrl Pts',(-9.39227050100006,11.6,-4.62660802900002));
#273004=CARTESIAN_POINT('Ctrl Pts',(-9.39355271300006,15.2,-4.62751945000001));
#273005=CARTESIAN_POINT('Ctrl Pts',(-9.39355271300006,11.6,-4.62751945000001));
#273006=CARTESIAN_POINT('Ctrl Pts',(-9.39484052500006,15.2,-4.62843667700001));
#273007=CARTESIAN_POINT('Ctrl Pts',(-9.39484052500006,11.6,-4.62843667700001));
#273008=CARTESIAN_POINT('Ctrl Pts',(-9.39613391000006,15.2,-4.62935971000002));
#273009=CARTESIAN_POINT('Ctrl Pts',(-9.39613391000006,11.6,-4.62935971000002));
#273010=CARTESIAN_POINT('Ctrl Pts',(-9.39743284800005,15.2,-4.63028854700001));
#273011=CARTESIAN_POINT('Ctrl Pts',(-9.39743284800005,11.6,-4.63028854700002));
#273012=CARTESIAN_POINT('Ctrl Pts',(-9.39873731400005,15.2,-4.63122319200002));
#273013=CARTESIAN_POINT('Ctrl Pts',(-9.39873731400005,11.6,-4.63122319200002));
#273014=CARTESIAN_POINT('Ctrl Pts',(-9.40004728400006,15.2,-4.63216364100001));
#273015=CARTESIAN_POINT('Ctrl Pts',(-9.40004728400006,11.6,-4.63216364100001));
#273016=CARTESIAN_POINT('Ctrl Pts',(-9.40136273700006,15.2,-4.63310989700001));
#273017=CARTESIAN_POINT('Ctrl Pts',(-9.40136273700006,11.6,-4.63310989700001));
#273018=CARTESIAN_POINT('Ctrl Pts',(-9.40268364800006,15.2,-4.63406195800002));
#273019=CARTESIAN_POINT('Ctrl Pts',(-9.40268364800006,11.6,-4.63406195800002));
#273020=CARTESIAN_POINT('Ctrl Pts',(-9.40400999600006,15.2,-4.63501982600001));
#273021=CARTESIAN_POINT('Ctrl Pts',(-9.40400999600006,11.6,-4.63501982600001));
#273022=CARTESIAN_POINT('Ctrl Pts',(-9.40534175600006,15.2,-4.63598350100002));
#273023=CARTESIAN_POINT('Ctrl Pts',(-9.40534175600006,11.6,-4.63598350100002));
#273024=CARTESIAN_POINT('Ctrl Pts',(-9.40667890800006,15.2,-4.63695298200001));
#273025=CARTESIAN_POINT('Ctrl Pts',(-9.40667890800006,11.6,-4.63695298200001));
#273026=CARTESIAN_POINT('Ctrl Pts',(-9.40802142700005,15.2,-4.63792826900002));
#273027=CARTESIAN_POINT('Ctrl Pts',(-9.40802142700005,11.6,-4.63792826900002));
#273028=CARTESIAN_POINT('Ctrl Pts',(-9.40936929200006,15.2,-4.63890936200002));
#273029=CARTESIAN_POINT('Ctrl Pts',(-9.40936929200006,11.6,-4.63890936200002));
#273030=CARTESIAN_POINT('Ctrl Pts',(-9.41072247900006,15.2,-4.63989626300001));
#273031=CARTESIAN_POINT('Ctrl Pts',(-9.41072247900006,11.6,-4.63989626300001));
#273032=CARTESIAN_POINT('Ctrl Pts',(-9.41208096700005,15.2,-4.64088897000002));
#273033=CARTESIAN_POINT('Ctrl Pts',(-9.41208096700005,11.6,-4.64088897000002));
#273034=CARTESIAN_POINT('Ctrl Pts',(-9.41344473500006,15.2,-4.64188748400002));
#273035=CARTESIAN_POINT('Ctrl Pts',(-9.41344473500006,11.6,-4.64188748400002));
#273036=CARTESIAN_POINT('Ctrl Pts',(-9.41481375700005,15.2,-4.64289180400002));
#273037=CARTESIAN_POINT('Ctrl Pts',(-9.41481375700005,11.6,-4.64289180400002));
#273038=CARTESIAN_POINT('Ctrl Pts',(-9.41618801500006,15.2,-4.64390193100002));
#273039=CARTESIAN_POINT('Ctrl Pts',(-9.41618801500006,11.6,-4.64390193100002));
#273040=CARTESIAN_POINT('Ctrl Pts',(-9.41756748400006,15.2,-4.64491786400002));
#273041=CARTESIAN_POINT('Ctrl Pts',(-9.41756748400006,11.6,-4.64491786400002));
#273042=CARTESIAN_POINT('Ctrl Pts',(-9.41895214300006,15.2,-4.64593960400002));
#273043=CARTESIAN_POINT('Ctrl Pts',(-9.41895214300006,11.6,-4.64593960400002));
#273044=CARTESIAN_POINT('Ctrl Pts',(-9.42034197000006,15.2,-4.64696715000001));
#273045=CARTESIAN_POINT('Ctrl Pts',(-9.42034197000006,11.6,-4.64696715000002));
#273046=CARTESIAN_POINT('Ctrl Pts',(-9.42173694400006,15.2,-4.64800050400001));
#273047=CARTESIAN_POINT('Ctrl Pts',(-9.42173694400006,11.6,-4.64800050400001));
#273048=CARTESIAN_POINT('Ctrl Pts',(-9.42313704200006,15.2,-4.64903966200001));
#273049=CARTESIAN_POINT('Ctrl Pts',(-9.42313704200006,11.6,-4.64903966200001));
#273050=CARTESIAN_POINT('Ctrl Pts',(-9.42454224400005,15.2,-4.65008462800002));
#273051=CARTESIAN_POINT('Ctrl Pts',(-9.42454224400005,11.6,-4.65008462800002));
#273052=CARTESIAN_POINT('Ctrl Pts',(-9.42595252800006,15.2,-4.65113539900001));
#273053=CARTESIAN_POINT('Ctrl Pts',(-9.42595252800006,11.6,-4.65113539900001));
#273054=CARTESIAN_POINT('Ctrl Pts',(-9.42736787200005,15.2,-4.65219197700002));
#273055=CARTESIAN_POINT('Ctrl Pts',(-9.42736787200005,11.6,-4.65219197700002));
#273056=CARTESIAN_POINT('Ctrl Pts',(-9.42878825300006,15.2,-4.65325436100001));
#273057=CARTESIAN_POINT('Ctrl Pts',(-9.42878825300006,11.6,-4.65325436100002));
#273058=CARTESIAN_POINT('Ctrl Pts',(-9.43021365300006,15.2,-4.65432255000001));
#273059=CARTESIAN_POINT('Ctrl Pts',(-9.43021365300006,11.6,-4.65432255000001));
#273060=CARTESIAN_POINT('Ctrl Pts',(-9.43164405000006,15.2,-4.65539654500001));
#273061=CARTESIAN_POINT('Ctrl Pts',(-9.43164405000006,11.6,-4.65539654500002));
#273062=CARTESIAN_POINT('Ctrl Pts',(-9.43307942100006,15.2,-4.65647634500002));
#273063=CARTESIAN_POINT('Ctrl Pts',(-9.43307942100006,11.6,-4.65647634500002));
#273064=CARTESIAN_POINT('Ctrl Pts',(-9.43451974600006,15.2,-4.65756195100001));
#273065=CARTESIAN_POINT('Ctrl Pts',(-9.43451974600006,11.6,-4.65756195100001));
#273066=CARTESIAN_POINT('Ctrl Pts',(-9.43596500400006,15.2,-4.65865336200002));
#273067=CARTESIAN_POINT('Ctrl Pts',(-9.43596500400006,11.6,-4.65865336200002));
#273068=CARTESIAN_POINT('Ctrl Pts',(-9.43741517400005,15.2,-4.65975057700001));
#273069=CARTESIAN_POINT('Ctrl Pts',(-9.43741517400005,11.6,-4.65975057700002));
#273070=CARTESIAN_POINT('Ctrl Pts',(-9.43887023600006,15.2,-4.66085359800001));
#273071=CARTESIAN_POINT('Ctrl Pts',(-9.43887023600006,11.6,-4.66085359800002));
#273072=CARTESIAN_POINT('Ctrl Pts',(-9.44033016700006,15.2,-4.66196242300001));
#273073=CARTESIAN_POINT('Ctrl Pts',(-9.44033016700006,11.6,-4.66196242300002));
#273074=CARTESIAN_POINT('Ctrl Pts',(-9.44179495000006,15.2,-4.66307705300002));
#273075=CARTESIAN_POINT('Ctrl Pts',(-9.44179495000006,11.6,-4.66307705300002));
#273076=CARTESIAN_POINT('Ctrl Pts',(-9.44326456000006,15.2,-4.66419748500002));
#273077=CARTESIAN_POINT('Ctrl Pts',(-9.44326456000006,11.6,-4.66419748500002));
#273078=CARTESIAN_POINT('Ctrl Pts',(-9.44473898000006,15.2,-4.66532372300001));
#273079=CARTESIAN_POINT('Ctrl Pts',(-9.44473898000006,11.6,-4.66532372300002));
#273080=CARTESIAN_POINT('Ctrl Pts',(-9.44621818800006,15.2,-4.66645576400001));
#273081=CARTESIAN_POINT('Ctrl Pts',(-9.44621818800006,11.6,-4.66645576400001));
#273082=CARTESIAN_POINT('Ctrl Pts',(-9.44770216400006,15.2,-4.66759360700001));
#273083=CARTESIAN_POINT('Ctrl Pts',(-9.44770216400006,11.6,-4.66759360700001));
#273084=CARTESIAN_POINT('Ctrl Pts',(-9.44919088600006,15.2,-4.66873725400001));
#273085=CARTESIAN_POINT('Ctrl Pts',(-9.44919088600006,11.6,-4.66873725400002));
#273086=CARTESIAN_POINT('Ctrl Pts',(-9.45068433700006,15.2,-4.66988670300001));
#273087=CARTESIAN_POINT('Ctrl Pts',(-9.45068433700006,11.6,-4.66988670300002));
#273088=CARTESIAN_POINT('Ctrl Pts',(-9.45218249400006,15.2,-4.67104195400001));
#273089=CARTESIAN_POINT('Ctrl Pts',(-9.45218249400006,11.6,-4.67104195400002));
#273090=CARTESIAN_POINT('Ctrl Pts',(-9.45368533800006,15.2,-4.67220300800001));
#273091=CARTESIAN_POINT('Ctrl Pts',(-9.45368533800006,11.6,-4.67220300800001));
#273092=CARTESIAN_POINT('Ctrl Pts',(-9.45519284900006,15.2,-4.67336986400001));
#273093=CARTESIAN_POINT('Ctrl Pts',(-9.45519284900006,11.6,-4.67336986400001));
#273094=CARTESIAN_POINT('Ctrl Pts',(-9.45670500700006,15.2,-4.67454252000001));
#273095=CARTESIAN_POINT('Ctrl Pts',(-9.45670500700006,11.6,-4.67454252000001));
#273096=CARTESIAN_POINT('Ctrl Pts',(-9.45822179200006,15.2,-4.67572097700002));
#273097=CARTESIAN_POINT('Ctrl Pts',(-9.45822179200006,11.6,-4.67572097700002));
#273098=CARTESIAN_POINT('Ctrl Pts',(-9.45974318400006,15.2,-4.67690523600002));
#273099=CARTESIAN_POINT('Ctrl Pts',(-9.45974318400006,11.6,-4.67690523600002));
#273100=CARTESIAN_POINT('Ctrl Pts',(-9.46126916300006,15.2,-4.67809529500002));
#273101=CARTESIAN_POINT('Ctrl Pts',(-9.46126916300006,11.6,-4.67809529500002));
#273102=CARTESIAN_POINT('Ctrl Pts',(-9.46279971000006,15.2,-4.67929115300001));
#273103=CARTESIAN_POINT('Ctrl Pts',(-9.46279971000006,11.6,-4.67929115300001));
#273104=CARTESIAN_POINT('Ctrl Pts',(-9.46433480500006,15.2,-4.68049281000001));
#273105=CARTESIAN_POINT('Ctrl Pts',(-9.46433480500006,11.6,-4.68049281000001));
#273106=CARTESIAN_POINT('Ctrl Pts',(-9.46587442900006,15.2,-4.68170026700002));
#273107=CARTESIAN_POINT('Ctrl Pts',(-9.46587442900006,11.6,-4.68170026700002));
#273108=CARTESIAN_POINT('Ctrl Pts',(-9.46741856000006,15.2,-4.68291352200001));
#273109=CARTESIAN_POINT('Ctrl Pts',(-9.46741856000006,11.6,-4.68291352200001));
#273110=CARTESIAN_POINT('Ctrl Pts',(-9.46896718300006,15.2,-4.68413257500002));
#273111=CARTESIAN_POINT('Ctrl Pts',(-9.46896718300006,11.6,-4.68413257500002));
#273112=CARTESIAN_POINT('Ctrl Pts',(-9.47052027400006,15.2,-4.68535742600002));
#273113=CARTESIAN_POINT('Ctrl Pts',(-9.47052027400006,11.6,-4.68535742600002));
#273114=CARTESIAN_POINT('Ctrl Pts',(-9.47207781800006,15.2,-4.68658807500002));
#273115=CARTESIAN_POINT('Ctrl Pts',(-9.47207781800006,11.6,-4.68658807500002));
#273116=CARTESIAN_POINT('Ctrl Pts',(-9.47363979200006,15.2,-4.68782452000001));
#273117=CARTESIAN_POINT('Ctrl Pts',(-9.47363979200006,11.6,-4.68782452000002));
#273118=CARTESIAN_POINT('Ctrl Pts',(-9.47520617900006,15.2,-4.68906676100001));
#273119=CARTESIAN_POINT('Ctrl Pts',(-9.47520617900006,11.6,-4.68906676100001));
#273120=CARTESIAN_POINT('Ctrl Pts',(-9.47677695900006,15.2,-4.69031479900002));
#273121=CARTESIAN_POINT('Ctrl Pts',(-9.47677695900006,11.6,-4.69031479900002));
#273122=CARTESIAN_POINT('Ctrl Pts',(-9.47835211500006,15.2,-4.69156863100002));
#273123=CARTESIAN_POINT('Ctrl Pts',(-9.47835211500006,11.6,-4.69156863100002));
#273124=CARTESIAN_POINT('Ctrl Pts',(-9.47993162400006,15.2,-4.69282825900001));
#273125=CARTESIAN_POINT('Ctrl Pts',(-9.47993162400006,11.6,-4.69282825900002));
#273126=CARTESIAN_POINT('Ctrl Pts',(-9.48151547100006,15.2,-4.69409368000001));
#273127=CARTESIAN_POINT('Ctrl Pts',(-9.48151547100006,11.6,-4.69409368000001));
#273128=CARTESIAN_POINT('Ctrl Pts',(-9.48310363400006,15.2,-4.69536489600001));
#273129=CARTESIAN_POINT('Ctrl Pts',(-9.48310363400006,11.6,-4.69536489600001));
#273130=CARTESIAN_POINT('Ctrl Pts',(-9.48469609800006,15.2,-4.69664190500001));
#273131=CARTESIAN_POINT('Ctrl Pts',(-9.48469609800006,11.6,-4.69664190500001));
#273132=CARTESIAN_POINT('Ctrl Pts',(-9.48629284000006,15.2,-4.69792470600002));
#273133=CARTESIAN_POINT('Ctrl Pts',(-9.48629284000006,11.6,-4.69792470600002));
#273134=CARTESIAN_POINT('Ctrl Pts',(-9.48789384500006,15.2,-4.69921330000002));
#273135=CARTESIAN_POINT('Ctrl Pts',(-9.48789384500006,11.6,-4.69921330000002));
#273136=CARTESIAN_POINT('Ctrl Pts',(-9.48949909200006,15.2,-4.70050768500001));
#273137=CARTESIAN_POINT('Ctrl Pts',(-9.48949909200006,11.6,-4.70050768500002));
#273138=CARTESIAN_POINT('Ctrl Pts',(-9.49110856400005,15.2,-4.70180786200002));
#273139=CARTESIAN_POINT('Ctrl Pts',(-9.49110856400005,11.6,-4.70180786200002));
#273140=CARTESIAN_POINT('Ctrl Pts',(-9.49272224000006,15.2,-4.70311382800002));
#273141=CARTESIAN_POINT('Ctrl Pts',(-9.49272224000006,11.6,-4.70311382800002));
#273142=CARTESIAN_POINT('Ctrl Pts',(-9.49434010600006,15.2,-4.70442558400002));
#273143=CARTESIAN_POINT('Ctrl Pts',(-9.49434010600006,11.6,-4.70442558400002));
#273144=CARTESIAN_POINT('Ctrl Pts',(-9.49596213900006,15.2,-4.70574313000002));
#273145=CARTESIAN_POINT('Ctrl Pts',(-9.49596213900006,11.6,-4.70574313000002));
#273146=CARTESIAN_POINT('Ctrl Pts',(-9.49758832300006,15.2,-4.70706646400001));
#273147=CARTESIAN_POINT('Ctrl Pts',(-9.49758832300006,11.6,-4.70706646400001));
#273148=CARTESIAN_POINT('Ctrl Pts',(-9.49921864000006,15.2,-4.70839558600002));
#273149=CARTESIAN_POINT('Ctrl Pts',(-9.49921864000006,11.6,-4.70839558600002));
#273150=CARTESIAN_POINT('Ctrl Pts',(-9.50085307100006,15.2,-4.70973049600001));
#273151=CARTESIAN_POINT('Ctrl Pts',(-9.50085307100006,11.6,-4.70973049600001));
#273152=CARTESIAN_POINT('Ctrl Pts',(-9.50249159800006,15.2,-4.71107119200001));
#273153=CARTESIAN_POINT('Ctrl Pts',(-9.50249159800006,11.6,-4.71107119200001));
#273154=CARTESIAN_POINT('Ctrl Pts',(-9.50413420300006,15.2,-4.71241767400001));
#273155=CARTESIAN_POINT('Ctrl Pts',(-9.50413420300006,11.6,-4.71241767400001));
#273156=CARTESIAN_POINT('Ctrl Pts',(-9.50578086900006,15.2,-4.71376994100002));
#273157=CARTESIAN_POINT('Ctrl Pts',(-9.50578086900006,11.6,-4.71376994100002));
#273158=CARTESIAN_POINT('Ctrl Pts',(-9.50743157600006,15.2,-4.71512799400001));
#273159=CARTESIAN_POINT('Ctrl Pts',(-9.50743157600006,11.6,-4.71512799400002));
#273160=CARTESIAN_POINT('Ctrl Pts',(-9.50908630800006,15.2,-4.71649183000002));
#273161=CARTESIAN_POINT('Ctrl Pts',(-9.50908630800006,11.6,-4.71649183000002));
#273162=CARTESIAN_POINT('Ctrl Pts',(-9.51074504700006,15.2,-4.71786145000001));
#273163=CARTESIAN_POINT('Ctrl Pts',(-9.51074504700006,11.6,-4.71786145000001));
#273164=CARTESIAN_POINT('Ctrl Pts',(-9.51240777300006,15.2,-4.71923685200001));
#273165=CARTESIAN_POINT('Ctrl Pts',(-9.51240777300006,11.6,-4.71923685200002));
#273166=CARTESIAN_POINT('Ctrl Pts',(-9.51407447200006,15.2,-4.72061803600001));
#273167=CARTESIAN_POINT('Ctrl Pts',(-9.51407447200006,11.6,-4.72061803600001));
#273168=CARTESIAN_POINT('Ctrl Pts',(-9.51574512200006,15.2,-4.72200500100001));
#273169=CARTESIAN_POINT('Ctrl Pts',(-9.51574512200006,11.6,-4.72200500100001));
#273170=CARTESIAN_POINT('Ctrl Pts',(-9.51741970900006,15.2,-4.72339774700002));
#273171=CARTESIAN_POINT('Ctrl Pts',(-9.51741970900006,11.6,-4.72339774700002));
#273172=CARTESIAN_POINT('Ctrl Pts',(-9.51909821500006,15.2,-4.72479627200002));
#273173=CARTESIAN_POINT('Ctrl Pts',(-9.51909821500006,11.6,-4.72479627200002));
#273174=CARTESIAN_POINT('Ctrl Pts',(-9.52078062000006,15.2,-4.72620057600002));
#273175=CARTESIAN_POINT('Ctrl Pts',(-9.52078062000006,11.6,-4.72620057600002));
#273176=CARTESIAN_POINT('Ctrl Pts',(-9.52246690900006,15.2,-4.72761065900002));
#273177=CARTESIAN_POINT('Ctrl Pts',(-9.52246690900006,11.6,-4.72761065900002));
#273178=CARTESIAN_POINT('Ctrl Pts',(-9.52415706300006,15.2,-4.72902651900001));
#273179=CARTESIAN_POINT('Ctrl Pts',(-9.52415706300006,11.6,-4.72902651900002));
#273180=CARTESIAN_POINT('Ctrl Pts',(-9.52585106700005,15.2,-4.73044815500002));
#273181=CARTESIAN_POINT('Ctrl Pts',(-9.52585106700005,11.6,-4.73044815500002));
#273182=CARTESIAN_POINT('Ctrl Pts',(-9.52754890100006,15.2,-4.73187556700001));
#273183=CARTESIAN_POINT('Ctrl Pts',(-9.52754890100006,11.6,-4.73187556700002));
#273184=CARTESIAN_POINT('Ctrl Pts',(-9.52925054900006,15.2,-4.73330875500002));
#273185=CARTESIAN_POINT('Ctrl Pts',(-9.52925054900006,11.6,-4.73330875500002));
#273186=CARTESIAN_POINT('Ctrl Pts',(-9.53095599400006,15.2,-4.73474771700001));
#273187=CARTESIAN_POINT('Ctrl Pts',(-9.53095599400006,11.6,-4.73474771700001));
#273188=CARTESIAN_POINT('Ctrl Pts',(-9.53266521800006,15.2,-4.73619245200001));
#273189=CARTESIAN_POINT('Ctrl Pts',(-9.53266521800006,11.6,-4.73619245200002));
#273190=CARTESIAN_POINT('Ctrl Pts',(-9.53437820600006,15.2,-4.73764296000001));
#273191=CARTESIAN_POINT('Ctrl Pts',(-9.53437820600006,11.6,-4.73764296000002));
#273192=CARTESIAN_POINT('Ctrl Pts',(-9.53609493900006,15.2,-4.73909923900001));
#273193=CARTESIAN_POINT('Ctrl Pts',(-9.53609493900006,11.6,-4.73909923900001));
#273194=CARTESIAN_POINT('Ctrl Pts',(-9.53781539900006,15.2,-4.74056129000001));
#273195=CARTESIAN_POINT('Ctrl Pts',(-9.53781539900006,11.6,-4.74056129000001));
#273196=CARTESIAN_POINT('Ctrl Pts',(-9.53953957300006,15.2,-4.74202911000001));
#273197=CARTESIAN_POINT('Ctrl Pts',(-9.53953957300006,11.6,-4.74202911000001));
#273198=CARTESIAN_POINT('Ctrl Pts',(-9.54126744000006,15.2,-4.74350270000001));
#273199=CARTESIAN_POINT('Ctrl Pts',(-9.54126744000006,11.6,-4.74350270000001));
#273200=CARTESIAN_POINT('Ctrl Pts',(-9.54299898700006,15.2,-4.74498205800002));
#273201=CARTESIAN_POINT('Ctrl Pts',(-9.54299898700006,11.6,-4.74498205800002));
#273202=CARTESIAN_POINT('Ctrl Pts',(-9.54473419400006,15.2,-4.74646718400002));
#273203=CARTESIAN_POINT('Ctrl Pts',(-9.54473419400006,11.6,-4.74646718400002));
#273204=CARTESIAN_POINT('Ctrl Pts',(-9.54647304600006,15.2,-4.74795807600001));
#273205=CARTESIAN_POINT('Ctrl Pts',(-9.54647304600006,11.6,-4.74795807600001));
#273206=CARTESIAN_POINT('Ctrl Pts',(-9.54821552600006,15.2,-4.74945473400001));
#273207=CARTESIAN_POINT('Ctrl Pts',(-9.54821552600006,11.6,-4.74945473400001));
#273208=CARTESIAN_POINT('Ctrl Pts',(-9.54996161700005,15.2,-4.75095715700002));
#273209=CARTESIAN_POINT('Ctrl Pts',(-9.54996161700005,11.6,-4.75095715700002));
#273210=CARTESIAN_POINT('Ctrl Pts',(-9.55171130400006,15.2,-4.75246534400001));
#273211=CARTESIAN_POINT('Ctrl Pts',(-9.55171130400006,11.6,-4.75246534400002));
#273212=CARTESIAN_POINT('Ctrl Pts',(-9.55346456800006,15.2,-4.75397929300001));
#273213=CARTESIAN_POINT('Ctrl Pts',(-9.55346456800006,11.6,-4.75397929300002));
#273214=CARTESIAN_POINT('Ctrl Pts',(-9.55522139400006,15.2,-4.75549900500001));
#273215=CARTESIAN_POINT('Ctrl Pts',(-9.55522139400006,11.6,-4.75549900500001));
#273216=CARTESIAN_POINT('Ctrl Pts',(-9.55698176600006,15.2,-4.75702447800002));
#273217=CARTESIAN_POINT('Ctrl Pts',(-9.55698176600006,11.6,-4.75702447800002));
#273218=CARTESIAN_POINT('Ctrl Pts',(-9.55874566600006,15.2,-4.75855571100002));
#273219=CARTESIAN_POINT('Ctrl Pts',(-9.55874566600006,11.6,-4.75855571100002));
#273220=CARTESIAN_POINT('Ctrl Pts',(-9.56051308000006,15.2,-4.76009270400001));
#273221=CARTESIAN_POINT('Ctrl Pts',(-9.56051308000006,11.6,-4.76009270400001));
#273222=CARTESIAN_POINT('Ctrl Pts',(-9.56228398900006,15.2,-4.76163545400001));
#273223=CARTESIAN_POINT('Ctrl Pts',(-9.56228398900006,11.6,-4.76163545400001));
#273224=CARTESIAN_POINT('Ctrl Pts',(-9.56405838000006,15.2,-4.76318396200002));
#273225=CARTESIAN_POINT('Ctrl Pts',(-9.56405838000006,11.6,-4.76318396200002));
#273226=CARTESIAN_POINT('Ctrl Pts',(-9.56583623400006,15.2,-4.76473822600001));
#273227=CARTESIAN_POINT('Ctrl Pts',(-9.56583623400006,11.6,-4.76473822600001));
#273228=CARTESIAN_POINT('Ctrl Pts',(-9.56761753700006,15.2,-4.76629824700002));
#273229=CARTESIAN_POINT('Ctrl Pts',(-9.56761753700006,11.6,-4.76629824700002));
#273230=CARTESIAN_POINT('Ctrl Pts',(-9.56940227100005,15.2,-4.76786402000001));
#273231=CARTESIAN_POINT('Ctrl Pts',(-9.56940227100005,11.6,-4.76786402000002));
#273232=CARTESIAN_POINT('Ctrl Pts',(-9.57119042200006,15.2,-4.76943554800001));
#273233=CARTESIAN_POINT('Ctrl Pts',(-9.57119042200006,11.6,-4.76943554800001));
#273234=CARTESIAN_POINT('Ctrl Pts',(-9.57298197200006,15.2,-4.77101282700001));
#273235=CARTESIAN_POINT('Ctrl Pts',(-9.57298197200006,11.6,-4.77101282700001));
#273236=CARTESIAN_POINT('Ctrl Pts',(-9.57477690700006,15.2,-4.77259585800001));
#273237=CARTESIAN_POINT('Ctrl Pts',(-9.57477690700006,11.6,-4.77259585800002));
#273238=CARTESIAN_POINT('Ctrl Pts',(-9.57657520800005,15.2,-4.77418463900001));
#273239=CARTESIAN_POINT('Ctrl Pts',(-9.57657520800005,11.6,-4.77418463900001));
#273240=CARTESIAN_POINT('Ctrl Pts',(-9.57837686400006,15.2,-4.77577917000001));
#273241=CARTESIAN_POINT('Ctrl Pts',(-9.57837686400006,11.6,-4.77577917000001));
#273242=CARTESIAN_POINT('Ctrl Pts',(-9.58018185400006,15.2,-4.77737944900001));
#273243=CARTESIAN_POINT('Ctrl Pts',(-9.58018185400006,11.6,-4.77737944900001));
#273244=CARTESIAN_POINT('Ctrl Pts',(-9.58199016700006,15.2,-4.77898547400001));
#273245=CARTESIAN_POINT('Ctrl Pts',(-9.58199016700006,11.6,-4.77898547400002));
#273246=CARTESIAN_POINT('Ctrl Pts',(-9.58380178400006,15.2,-4.78059724600001));
#273247=CARTESIAN_POINT('Ctrl Pts',(-9.58380178400006,11.6,-4.78059724600001));
#273248=CARTESIAN_POINT('Ctrl Pts',(-9.58561669100006,15.2,-4.78221476300002));
#273249=CARTESIAN_POINT('Ctrl Pts',(-9.58561669100006,11.6,-4.78221476300002));
#273250=CARTESIAN_POINT('Ctrl Pts',(-9.58743487200006,15.2,-4.78383802400002));
#273251=CARTESIAN_POINT('Ctrl Pts',(-9.58743487200006,11.6,-4.78383802400002));
#273252=CARTESIAN_POINT('Ctrl Pts',(-9.58925631100006,15.2,-4.78546702800001));
#273253=CARTESIAN_POINT('Ctrl Pts',(-9.58925631100006,11.6,-4.78546702800002));
#273254=CARTESIAN_POINT('Ctrl Pts',(-9.59108099300006,15.2,-4.78710177400002));
#273255=CARTESIAN_POINT('Ctrl Pts',(-9.59108099300006,11.6,-4.78710177400002));
#273256=CARTESIAN_POINT('Ctrl Pts',(-9.59290890200006,15.2,-4.78874226000002));
#273257=CARTESIAN_POINT('Ctrl Pts',(-9.59290890200006,11.6,-4.78874226000002));
#273258=CARTESIAN_POINT('Ctrl Pts',(-9.59474002200006,15.2,-4.79038848600001));
#273259=CARTESIAN_POINT('Ctrl Pts',(-9.59474002200006,11.6,-4.79038848600002));
#273260=CARTESIAN_POINT('Ctrl Pts',(-9.59657434000006,15.2,-4.79204045100001));
#273261=CARTESIAN_POINT('Ctrl Pts',(-9.59657434000006,11.6,-4.79204045100001));
#273262=CARTESIAN_POINT('Ctrl Pts',(-9.59841183800006,15.2,-4.79369815300001));
#273263=CARTESIAN_POINT('Ctrl Pts',(-9.59841183800006,11.6,-4.79369815300002));
#273264=CARTESIAN_POINT('Ctrl Pts',(-9.60025250300006,15.2,-4.79536159100002));
#273265=CARTESIAN_POINT('Ctrl Pts',(-9.60025250300006,11.6,-4.79536159100002));
#273266=CARTESIAN_POINT('Ctrl Pts',(-9.60209631800006,15.2,-4.79703076500002));
#273267=CARTESIAN_POINT('Ctrl Pts',(-9.60209631800006,11.6,-4.79703076500002));
#273268=CARTESIAN_POINT('Ctrl Pts',(-9.60394326800006,15.2,-4.79870567200001));
#273269=CARTESIAN_POINT('Ctrl Pts',(-9.60394326800006,11.6,-4.79870567200001));
#273270=CARTESIAN_POINT('Ctrl Pts',(-9.60579333900006,15.2,-4.80038631200001));
#273271=CARTESIAN_POINT('Ctrl Pts',(-9.60579333900006,11.6,-4.80038631200001));
#273272=CARTESIAN_POINT('Ctrl Pts',(-9.60764651500006,15.2,-4.80207268400001));
#273273=CARTESIAN_POINT('Ctrl Pts',(-9.60764651500006,11.6,-4.80207268400001));
#273274=CARTESIAN_POINT('Ctrl Pts',(-9.60950278100006,15.2,-4.80376478600002));
#273275=CARTESIAN_POINT('Ctrl Pts',(-9.60950278100006,11.6,-4.80376478600002));
#273276=CARTESIAN_POINT('Ctrl Pts',(-9.61136212100006,15.2,-4.80546261800002));
#273277=CARTESIAN_POINT('Ctrl Pts',(-9.61136212100006,11.6,-4.80546261800002));
#273278=CARTESIAN_POINT('Ctrl Pts',(-9.61322452200006,15.2,-4.80716617800002));
#273279=CARTESIAN_POINT('Ctrl Pts',(-9.61322452200006,11.6,-4.80716617800002));
#273280=CARTESIAN_POINT('Ctrl Pts',(-9.61508996800006,15.2,-4.80887546500002));
#273281=CARTESIAN_POINT('Ctrl Pts',(-9.61508996800006,11.6,-4.80887546500002));
#273282=CARTESIAN_POINT('Ctrl Pts',(-9.61695844300005,15.2,-4.81059047700001));
#273283=CARTESIAN_POINT('Ctrl Pts',(-9.61695844300005,11.6,-4.81059047700001));
#273284=CARTESIAN_POINT('Ctrl Pts',(-9.61882993500006,15.2,-4.81231121400001));
#273285=CARTESIAN_POINT('Ctrl Pts',(-9.61882993500006,11.6,-4.81231121400001));
#273286=CARTESIAN_POINT('Ctrl Pts',(-9.62070442700006,15.2,-4.81403767400002));
#273287=CARTESIAN_POINT('Ctrl Pts',(-9.62070442700006,11.6,-4.81403767400002));
#273288=CARTESIAN_POINT('Ctrl Pts',(-9.62258190400006,15.2,-4.81576985800002));
#273289=CARTESIAN_POINT('Ctrl Pts',(-9.62258190400006,11.6,-4.81576985800002));
#273290=CARTESIAN_POINT('Ctrl Pts',(-9.62446235200006,15.2,-4.81750776100001));
#273291=CARTESIAN_POINT('Ctrl Pts',(-9.62446235200006,11.6,-4.81750776100002));
#273292=CARTESIAN_POINT('Ctrl Pts',(-9.62634575600006,15.2,-4.81925138300001));
#273293=CARTESIAN_POINT('Ctrl Pts',(-9.62634575600006,11.6,-4.81925138300001));
#273294=CARTESIAN_POINT('Ctrl Pts',(-9.62823210200006,15.2,-4.82100072500002));
#273295=CARTESIAN_POINT('Ctrl Pts',(-9.62823210200006,11.6,-4.82100072500002));
#273296=CARTESIAN_POINT('Ctrl Pts',(-9.63012137400005,15.2,-4.82275578400001));
#273297=CARTESIAN_POINT('Ctrl Pts',(-9.63012137400005,11.6,-4.82275578400001));
#273298=CARTESIAN_POINT('Ctrl Pts',(-9.63201355900006,15.2,-4.82451655900002));
#273299=CARTESIAN_POINT('Ctrl Pts',(-9.63201355900006,11.6,-4.82451655900002));
#273300=CARTESIAN_POINT('Ctrl Pts',(-9.63390864200005,15.2,-4.82628304800001));
#273301=CARTESIAN_POINT('Ctrl Pts',(-9.63390864200005,11.6,-4.82628304800001));
#273302=CARTESIAN_POINT('Ctrl Pts',(-9.63580660800006,15.2,-4.82805525200002));
#273303=CARTESIAN_POINT('Ctrl Pts',(-9.63580660800006,11.6,-4.82805525200002));
#273304=CARTESIAN_POINT('Ctrl Pts',(-9.63770744300006,15.2,-4.82983316700001));
#273305=CARTESIAN_POINT('Ctrl Pts',(-9.63770744300006,11.6,-4.82983316700001));
#273306=CARTESIAN_POINT('Ctrl Pts',(-9.63961113100006,15.2,-4.83161679200002));
#273307=CARTESIAN_POINT('Ctrl Pts',(-9.63961113100006,11.6,-4.83161679200002));
#273308=CARTESIAN_POINT('Ctrl Pts',(-9.64151766000005,15.2,-4.83340612800002));
#273309=CARTESIAN_POINT('Ctrl Pts',(-9.64151766000005,11.6,-4.83340612800002));
#273310=CARTESIAN_POINT('Ctrl Pts',(-9.64342701400006,15.2,-4.83520117200001));
#273311=CARTESIAN_POINT('Ctrl Pts',(-9.64342701400006,11.6,-4.83520117200001));
#273312=CARTESIAN_POINT('Ctrl Pts',(-9.64533918000006,15.2,-4.83700192200001));
#273313=CARTESIAN_POINT('Ctrl Pts',(-9.64533918000006,11.6,-4.83700192200002));
#273314=CARTESIAN_POINT('Ctrl Pts',(-9.64725414300006,15.2,-4.83880837900001));
#273315=CARTESIAN_POINT('Ctrl Pts',(-9.64725414300006,11.6,-4.83880837900002));
#273316=CARTESIAN_POINT('Ctrl Pts',(-9.64917188800005,15.2,-4.84062054000002));
#273317=CARTESIAN_POINT('Ctrl Pts',(-9.64917188800005,11.6,-4.84062054000002));
#273318=CARTESIAN_POINT('Ctrl Pts',(-9.65109240200006,15.2,-4.84243840400001));
#273319=CARTESIAN_POINT('Ctrl Pts',(-9.65109240200006,11.6,-4.84243840400001));
#273320=CARTESIAN_POINT('Ctrl Pts',(-9.65301567100006,15.2,-4.84426196900001));
#273321=CARTESIAN_POINT('Ctrl Pts',(-9.65301567100006,11.6,-4.84426196900001));
#273322=CARTESIAN_POINT('Ctrl Pts',(-9.65494167900006,15.2,-4.84609123600002));
#273323=CARTESIAN_POINT('Ctrl Pts',(-9.65494167900006,11.6,-4.84609123600002));
#273324=CARTESIAN_POINT('Ctrl Pts',(-9.65687041400006,15.2,-4.84792620100002));
#273325=CARTESIAN_POINT('Ctrl Pts',(-9.65687041400006,11.6,-4.84792620100002));
#273326=CARTESIAN_POINT('Ctrl Pts',(-9.65880186100006,15.2,-4.84976686400001));
#273327=CARTESIAN_POINT('Ctrl Pts',(-9.65880186100006,11.6,-4.84976686400001));
#273328=CARTESIAN_POINT('Ctrl Pts',(-9.66073600600006,15.2,-4.85161322300002));
#273329=CARTESIAN_POINT('Ctrl Pts',(-9.66073600600006,11.6,-4.85161322300002));
#273330=CARTESIAN_POINT('Ctrl Pts',(-9.66267283500006,15.2,-4.85346527800001));
#273331=CARTESIAN_POINT('Ctrl Pts',(-9.66267283500006,11.6,-4.85346527800001));
#273332=CARTESIAN_POINT('Ctrl Pts',(-9.66461233400006,15.2,-4.85532302500001));
#273333=CARTESIAN_POINT('Ctrl Pts',(-9.66461233400006,11.6,-4.85532302500001));
#273334=CARTESIAN_POINT('Ctrl Pts',(-9.66655449000006,15.2,-4.85718646500001));
#273335=CARTESIAN_POINT('Ctrl Pts',(-9.66655449000006,11.6,-4.85718646500001));
#273336=CARTESIAN_POINT('Ctrl Pts',(-9.66849928800006,15.2,-4.85905559500001));
#273337=CARTESIAN_POINT('Ctrl Pts',(-9.66849928800006,11.6,-4.85905559500001));
#273338=CARTESIAN_POINT('Ctrl Pts',(-9.67044671500006,15.2,-4.86093041600002));
#273339=CARTESIAN_POINT('Ctrl Pts',(-9.67044671500006,11.6,-4.86093041600002));
#273340=CARTESIAN_POINT('Ctrl Pts',(-9.67239675600006,15.2,-4.86281092400001));
#273341=CARTESIAN_POINT('Ctrl Pts',(-9.67239675600006,11.6,-4.86281092400001));
#273342=CARTESIAN_POINT('Ctrl Pts',(-9.67434939900006,15.2,-4.86469711900002));
#273343=CARTESIAN_POINT('Ctrl Pts',(-9.67434939900006,11.6,-4.86469711900002));
#273344=CARTESIAN_POINT('Ctrl Pts',(-9.67630462800006,15.2,-4.86658900000001));
#273345=CARTESIAN_POINT('Ctrl Pts',(-9.67630462800006,11.6,-4.86658900000002));
#273346=CARTESIAN_POINT('Ctrl Pts',(-9.67826243300006,15.2,-4.86848656300001));
#273347=CARTESIAN_POINT('Ctrl Pts',(-9.67826243300006,11.6,-4.86848656300001));
#273348=CARTESIAN_POINT('Ctrl Pts',(-9.68022279600006,15.2,-4.87038981000001));
#273349=CARTESIAN_POINT('Ctrl Pts',(-9.68022279600006,11.6,-4.87038981000001));
#273350=CARTESIAN_POINT('Ctrl Pts',(-9.68218570600006,15.2,-4.87229873800001));
#273351=CARTESIAN_POINT('Ctrl Pts',(-9.68218570600006,11.6,-4.87229873800001));
#273352=CARTESIAN_POINT('Ctrl Pts',(-9.68415114900005,15.2,-4.87421334500001));
#273353=CARTESIAN_POINT('Ctrl Pts',(-9.68415114900005,11.6,-4.87421334500001));
#273354=CARTESIAN_POINT('Ctrl Pts',(-9.68611911100006,15.2,-4.87613363000001));
#273355=CARTESIAN_POINT('Ctrl Pts',(-9.68611911100006,11.6,-4.87613363000001));
#273356=CARTESIAN_POINT('Ctrl Pts',(-9.68808957900006,15.2,-4.87805959100001));
#273357=CARTESIAN_POINT('Ctrl Pts',(-9.68808957900006,11.6,-4.87805959100002));
#273358=CARTESIAN_POINT('Ctrl Pts',(-9.69006253900006,15.2,-4.87999122800002));
#273359=CARTESIAN_POINT('Ctrl Pts',(-9.69006253900006,11.6,-4.87999122800002));
#273360=CARTESIAN_POINT('Ctrl Pts',(-9.69203797800006,15.2,-4.88192854000001));
#273361=CARTESIAN_POINT('Ctrl Pts',(-9.69203797800006,11.6,-4.88192854000001));
#273362=CARTESIAN_POINT('Ctrl Pts',(-9.69401588300006,15.2,-4.88387152300001));
#273363=CARTESIAN_POINT('Ctrl Pts',(-9.69401588300006,11.6,-4.88387152300001));
#273364=CARTESIAN_POINT('Ctrl Pts',(-9.69599623900006,15.2,-4.88582017700002));
#273365=CARTESIAN_POINT('Ctrl Pts',(-9.69599623900006,11.6,-4.88582017700002));
#273366=CARTESIAN_POINT('Ctrl Pts',(-9.69797903400006,15.2,-4.88777450000002));
#273367=CARTESIAN_POINT('Ctrl Pts',(-9.69797903400006,11.6,-4.88777450000002));
#273368=CARTESIAN_POINT('Ctrl Pts',(-9.69996425500005,15.2,-4.88973449200001));
#273369=CARTESIAN_POINT('Ctrl Pts',(-9.69996425500005,11.6,-4.88973449200001));
#273370=CARTESIAN_POINT('Ctrl Pts',(-9.70195188800006,15.2,-4.89170014900001));
#273371=CARTESIAN_POINT('Ctrl Pts',(-9.70195188800006,11.6,-4.89170014900001));
#273372=CARTESIAN_POINT('Ctrl Pts',(-9.70394191900006,15.2,-4.89367147200001));
#273373=CARTESIAN_POINT('Ctrl Pts',(-9.70394191900006,11.6,-4.89367147200001));
#273374=CARTESIAN_POINT('Ctrl Pts',(-9.70593433700006,15.2,-4.89564845700002));
#273375=CARTESIAN_POINT('Ctrl Pts',(-9.70593433700006,11.6,-4.89564845700002));
#273376=CARTESIAN_POINT('Ctrl Pts',(-9.70792912700006,15.2,-4.89763110500002));
#273377=CARTESIAN_POINT('Ctrl Pts',(-9.70792912700006,11.6,-4.89763110500002));
#273378=CARTESIAN_POINT('Ctrl Pts',(-9.70992627600006,15.2,-4.89961941300002));
#273379=CARTESIAN_POINT('Ctrl Pts',(-9.70992627600006,11.6,-4.89961941300002));
#273380=CARTESIAN_POINT('Ctrl Pts',(-9.71192577300006,15.2,-4.90161338000001));
#273381=CARTESIAN_POINT('Ctrl Pts',(-9.71192577300006,11.6,-4.90161338000001));
#273382=CARTESIAN_POINT('Ctrl Pts',(-9.71392760200006,15.2,-4.90361300400001));
#273383=CARTESIAN_POINT('Ctrl Pts',(-9.71392760200006,11.6,-4.90361300400001));
#273384=CARTESIAN_POINT('Ctrl Pts',(-9.71593175100006,15.2,-4.90561828400002));
#273385=CARTESIAN_POINT('Ctrl Pts',(-9.71593175100006,11.6,-4.90561828400002));
#273386=CARTESIAN_POINT('Ctrl Pts',(-9.71793820800006,15.2,-4.90762921800002));
#273387=CARTESIAN_POINT('Ctrl Pts',(-9.71793820800006,11.6,-4.90762921800002));
#273388=CARTESIAN_POINT('Ctrl Pts',(-9.71994695800005,15.2,-4.90964580500002));
#273389=CARTESIAN_POINT('Ctrl Pts',(-9.71994695800005,11.6,-4.90964580500002));
#273390=CARTESIAN_POINT('Ctrl Pts',(-9.72195799100006,15.2,-4.91166804200001));
#273391=CARTESIAN_POINT('Ctrl Pts',(-9.72195799100006,11.6,-4.91166804200002));
#273392=CARTESIAN_POINT('Ctrl Pts',(-9.72397129100005,15.2,-4.91369593000002));
#273393=CARTESIAN_POINT('Ctrl Pts',(-9.72397129100005,11.6,-4.91369593000002));
#273394=CARTESIAN_POINT('Ctrl Pts',(-9.72598684800005,15.2,-4.91572946500002));
#273395=CARTESIAN_POINT('Ctrl Pts',(-9.72598684800005,11.6,-4.91572946500002));
#273396=CARTESIAN_POINT('Ctrl Pts',(-9.72800464700006,15.2,-4.91776864800002));
#273397=CARTESIAN_POINT('Ctrl Pts',(-9.72800464700006,11.6,-4.91776864800002));
#273398=CARTESIAN_POINT('Ctrl Pts',(-9.73002467500006,15.2,-4.91981347400001));
#273399=CARTESIAN_POINT('Ctrl Pts',(-9.73002467500006,11.6,-4.91981347400001));
#273400=CARTESIAN_POINT('Ctrl Pts',(-9.73204692100006,15.2,-4.92186394400001));
#273401=CARTESIAN_POINT('Ctrl Pts',(-9.73204692100006,11.6,-4.92186394400001));
#273402=CARTESIAN_POINT('Ctrl Pts',(-9.73407137000006,15.2,-4.92392005600002));
#273403=CARTESIAN_POINT('Ctrl Pts',(-9.73407137000006,11.6,-4.92392005600002));
#273404=CARTESIAN_POINT('Ctrl Pts',(-9.73609801200006,15.2,-4.92598180800002));
#273405=CARTESIAN_POINT('Ctrl Pts',(-9.73609801200006,11.6,-4.92598180800002));
#273406=CARTESIAN_POINT('Ctrl Pts',(-9.73812683300006,15.2,-4.92804919800002));
#273407=CARTESIAN_POINT('Ctrl Pts',(-9.73812683300006,11.6,-4.92804919800002));
#273408=CARTESIAN_POINT('Ctrl Pts',(-9.74015782000006,15.2,-4.93012222600001));
#273409=CARTESIAN_POINT('Ctrl Pts',(-9.74015782000006,11.6,-4.93012222600001));
#273410=CARTESIAN_POINT('Ctrl Pts',(-9.74219096100006,15.2,-4.93220088800001));
#273411=CARTESIAN_POINT('Ctrl Pts',(-9.74219096100006,11.6,-4.93220088800001));
#273412=CARTESIAN_POINT('Ctrl Pts',(-9.74422624200006,15.2,-4.93428518400002));
#273413=CARTESIAN_POINT('Ctrl Pts',(-9.74422624200006,11.6,-4.93428518400002));
#273414=CARTESIAN_POINT('Ctrl Pts',(-9.74626365300006,15.2,-4.93637511300001));
#273415=CARTESIAN_POINT('Ctrl Pts',(-9.74626365300006,11.6,-4.93637511300001));
#273416=CARTESIAN_POINT('Ctrl Pts',(-9.74830317900006,15.2,-4.93847067000001));
#273417=CARTESIAN_POINT('Ctrl Pts',(-9.74830317900006,11.6,-4.93847067000001));
#273418=CARTESIAN_POINT('Ctrl Pts',(-9.75034480900005,15.2,-4.94057185800001));
#273419=CARTESIAN_POINT('Ctrl Pts',(-9.75034480900005,11.6,-4.94057185800001));
#273420=CARTESIAN_POINT('Ctrl Pts',(-9.75238852900006,15.2,-4.94267867300001));
#273421=CARTESIAN_POINT('Ctrl Pts',(-9.75238852900006,11.6,-4.94267867300001));
#273422=CARTESIAN_POINT('Ctrl Pts',(-9.75443432900006,15.2,-4.94479111400001));
#273423=CARTESIAN_POINT('Ctrl Pts',(-9.75443432900006,11.6,-4.94479111400001));
#273424=CARTESIAN_POINT('Ctrl Pts',(-9.75648219500006,15.2,-4.94690917700002));
#273425=CARTESIAN_POINT('Ctrl Pts',(-9.75648219500006,11.6,-4.94690917700002));
#273426=CARTESIAN_POINT('Ctrl Pts',(-9.75853211400005,15.2,-4.94903286300001));
#273427=CARTESIAN_POINT('Ctrl Pts',(-9.75853211400005,11.6,-4.94903286300001));
#273428=CARTESIAN_POINT('Ctrl Pts',(-9.76058407400006,15.2,-4.95116217000001));
#273429=CARTESIAN_POINT('Ctrl Pts',(-9.76058407400006,11.6,-4.95116217000002));
#273430=CARTESIAN_POINT('Ctrl Pts',(-9.76263806400006,15.2,-4.95329709600002));
#273431=CARTESIAN_POINT('Ctrl Pts',(-9.76263806400006,11.6,-4.95329709600002));
#273432=CARTESIAN_POINT('Ctrl Pts',(-9.76469407100006,15.2,-4.95543763800002));
#273433=CARTESIAN_POINT('Ctrl Pts',(-9.76469407100006,11.6,-4.95543763800002));
#273434=CARTESIAN_POINT('Ctrl Pts',(-9.76675208200006,15.2,-4.95758379600002));
#273435=CARTESIAN_POINT('Ctrl Pts',(-9.76675208200006,11.6,-4.95758379600002));
#273436=CARTESIAN_POINT('Ctrl Pts',(-9.76881208600006,15.2,-4.95973556900001));
#273437=CARTESIAN_POINT('Ctrl Pts',(-9.76881208600006,11.6,-4.95973556900002));
#273438=CARTESIAN_POINT('Ctrl Pts',(-9.77087406900005,15.2,-4.96189295300002));
#273439=CARTESIAN_POINT('Ctrl Pts',(-9.77087406900005,11.6,-4.96189295300002));
#273440=CARTESIAN_POINT('Ctrl Pts',(-9.77293802100006,15.2,-4.96405594800001));
#273441=CARTESIAN_POINT('Ctrl Pts',(-9.77293802100006,11.6,-4.96405594800002));
#273442=CARTESIAN_POINT('Ctrl Pts',(-9.77500392800006,15.2,-4.96622455100002));
#273443=CARTESIAN_POINT('Ctrl Pts',(-9.77500392800006,11.6,-4.96622455100002));
#273444=CARTESIAN_POINT('Ctrl Pts',(-9.77707178000006,15.2,-4.96839876200001));
#273445=CARTESIAN_POINT('Ctrl Pts',(-9.77707178000006,11.6,-4.96839876200002));
#273446=CARTESIAN_POINT('Ctrl Pts',(-9.77914156200006,15.2,-4.97057857700002));
#273447=CARTESIAN_POINT('Ctrl Pts',(-9.77914156200006,11.6,-4.97057857700002));
#273448=CARTESIAN_POINT('Ctrl Pts',(-9.78121326400006,15.2,-4.97276399700001));
#273449=CARTESIAN_POINT('Ctrl Pts',(-9.78121326400006,11.6,-4.97276399700001));
#273450=CARTESIAN_POINT('Ctrl Pts',(-9.78328687400005,15.2,-4.97495501800001));
#273451=CARTESIAN_POINT('Ctrl Pts',(-9.78328687400005,11.6,-4.97495501800001));
#273452=CARTESIAN_POINT('Ctrl Pts',(-9.78536237900006,15.2,-4.97715164000001));
#273453=CARTESIAN_POINT('Ctrl Pts',(-9.78536237900006,11.6,-4.97715164000002));
#273454=CARTESIAN_POINT('Ctrl Pts',(-9.78743976900006,15.2,-4.97935386100002));
#273455=CARTESIAN_POINT('Ctrl Pts',(-9.78743976900006,11.6,-4.97935386100002));
#273456=CARTESIAN_POINT('Ctrl Pts',(-9.78951902900006,15.2,-4.98156167700001));
#273457=CARTESIAN_POINT('Ctrl Pts',(-9.78951902900006,11.6,-4.98156167700001));
#273458=CARTESIAN_POINT('Ctrl Pts',(-9.79160014900006,15.2,-4.98377508900001));
#273459=CARTESIAN_POINT('Ctrl Pts',(-9.79160014900006,11.6,-4.98377508900001));
#273460=CARTESIAN_POINT('Ctrl Pts',(-9.79368311700006,15.2,-4.98599409400001));
#273461=CARTESIAN_POINT('Ctrl Pts',(-9.79368311700006,11.6,-4.98599409400002));
#273462=CARTESIAN_POINT('Ctrl Pts',(-9.79576792100006,15.2,-4.98821869000002));
#273463=CARTESIAN_POINT('Ctrl Pts',(-9.79576792100006,11.6,-4.98821869000002));
#273464=CARTESIAN_POINT('Ctrl Pts',(-9.79785454900006,15.2,-4.99044887600002));
#273465=CARTESIAN_POINT('Ctrl Pts',(-9.79785454900006,11.6,-4.99044887600002));
#273466=CARTESIAN_POINT('Ctrl Pts',(-9.79994298800005,15.2,-4.99268465100001));
#273467=CARTESIAN_POINT('Ctrl Pts',(-9.79994298800005,11.6,-4.99268465100002));
#273468=CARTESIAN_POINT('Ctrl Pts',(-9.80203322900006,15.2,-4.99492601000001));
#273469=CARTESIAN_POINT('Ctrl Pts',(-9.80203322900006,11.6,-4.99492601000001));
#273470=CARTESIAN_POINT('Ctrl Pts',(-9.80412525900006,15.2,-4.99717295500002));
#273471=CARTESIAN_POINT('Ctrl Pts',(-9.80412525900006,11.6,-4.99717295500002));
#273472=CARTESIAN_POINT('Ctrl Pts',(-9.80621906500006,15.2,-4.99942548300002));
#273473=CARTESIAN_POINT('Ctrl Pts',(-9.80621906500006,11.6,-4.99942548300002));
#273474=CARTESIAN_POINT('Ctrl Pts',(-9.80831463700006,15.2,-5.00168359100002));
#273475=CARTESIAN_POINT('Ctrl Pts',(-9.80831463700006,11.6,-5.00168359100002));
#273476=CARTESIAN_POINT('Ctrl Pts',(-9.81041196200006,15.2,-5.00394727800002));
#273477=CARTESIAN_POINT('Ctrl Pts',(-9.81041196200006,11.6,-5.00394727800002));
#273478=CARTESIAN_POINT('Ctrl Pts',(-9.81251102900006,15.2,-5.00621654300001));
#273479=CARTESIAN_POINT('Ctrl Pts',(-9.81251102900006,11.6,-5.00621654300001));
#273480=CARTESIAN_POINT('Ctrl Pts',(-9.81461182700006,15.2,-5.00849138200001));
#273481=CARTESIAN_POINT('Ctrl Pts',(-9.81461182700006,11.6,-5.00849138200001));
#273482=CARTESIAN_POINT('Ctrl Pts',(-9.81671434400005,15.2,-5.01077179600002));
#273483=CARTESIAN_POINT('Ctrl Pts',(-9.81671434400005,11.6,-5.01077179600002));
#273484=CARTESIAN_POINT('Ctrl Pts',(-9.81881856700005,15.2,-5.01305778200001));
#273485=CARTESIAN_POINT('Ctrl Pts',(-9.81881856700005,11.6,-5.01305778200001));
#273486=CARTESIAN_POINT('Ctrl Pts',(-9.82092448700006,15.2,-5.01534933700002));
#273487=CARTESIAN_POINT('Ctrl Pts',(-9.82092448700006,11.6,-5.01534933700002));
#273488=CARTESIAN_POINT('Ctrl Pts',(-9.82303209100006,15.2,-5.01764646100002));
#273489=CARTESIAN_POINT('Ctrl Pts',(-9.82303209100006,11.6,-5.01764646100002));
#273490=CARTESIAN_POINT('Ctrl Pts',(-9.82514136700006,15.2,-5.01994915000001));
#273491=CARTESIAN_POINT('Ctrl Pts',(-9.82514136700006,11.6,-5.01994915000001));
#273492=CARTESIAN_POINT('Ctrl Pts',(-9.82725230400006,15.2,-5.02225740500001));
#273493=CARTESIAN_POINT('Ctrl Pts',(-9.82725230400006,11.6,-5.02225740500001));
#273494=CARTESIAN_POINT('Ctrl Pts',(-9.82936489100006,15.2,-5.02457122300001));
#273495=CARTESIAN_POINT('Ctrl Pts',(-9.82936489100006,11.6,-5.02457122300001));
#273496=CARTESIAN_POINT('Ctrl Pts',(-9.83147911800006,15.2,-5.02689060100002));
#273497=CARTESIAN_POINT('Ctrl Pts',(-9.83147911800006,11.6,-5.02689060100002));
#273498=CARTESIAN_POINT('Ctrl Pts',(-9.83359497000006,15.2,-5.02921553800002));
#273499=CARTESIAN_POINT('Ctrl Pts',(-9.83359497000006,11.6,-5.02921553800002));
#273500=CARTESIAN_POINT('Ctrl Pts',(-9.83571243900006,15.2,-5.03154603200001));
#273501=CARTESIAN_POINT('Ctrl Pts',(-9.83571243900006,11.6,-5.03154603200001));
#273502=CARTESIAN_POINT('Ctrl Pts',(-9.83783151200005,15.2,-5.03388208200001));
#273503=CARTESIAN_POINT('Ctrl Pts',(-9.83783151200005,11.6,-5.03388208200001));
#273504=CARTESIAN_POINT('Ctrl Pts',(-9.83995217700006,15.2,-5.03622368500002));
#273505=CARTESIAN_POINT('Ctrl Pts',(-9.83995217700006,11.6,-5.03622368500002));
#273506=CARTESIAN_POINT('Ctrl Pts',(-9.84207442500006,15.2,-5.03857084000002));
#273507=CARTESIAN_POINT('Ctrl Pts',(-9.84207442500006,11.6,-5.03857084000002));
#273508=CARTESIAN_POINT('Ctrl Pts',(-9.84419824200006,15.2,-5.04092354500001));
#273509=CARTESIAN_POINT('Ctrl Pts',(-9.84419824200006,11.6,-5.04092354500001));
#273510=CARTESIAN_POINT('Ctrl Pts',(-9.84632361900006,15.2,-5.04328179700002));
#273511=CARTESIAN_POINT('Ctrl Pts',(-9.84632361900006,11.6,-5.04328179700002));
#273512=CARTESIAN_POINT('Ctrl Pts',(-9.84845054500006,15.2,-5.04564559600002));
#273513=CARTESIAN_POINT('Ctrl Pts',(-9.84845054500006,11.6,-5.04564559600002));
#273514=CARTESIAN_POINT('Ctrl Pts',(-9.85057900700006,15.2,-5.04801493900001));
#273515=CARTESIAN_POINT('Ctrl Pts',(-9.85057900700006,11.6,-5.04801493900001));
#273516=CARTESIAN_POINT('Ctrl Pts',(-9.85270899400006,15.2,-5.05038982300002));
#273517=CARTESIAN_POINT('Ctrl Pts',(-9.85270899400006,11.6,-5.05038982300002));
#273518=CARTESIAN_POINT('Ctrl Pts',(-9.85484049700006,15.2,-5.05277024800002));
#273519=CARTESIAN_POINT('Ctrl Pts',(-9.85484049700006,11.6,-5.05277024800002));
#273520=CARTESIAN_POINT('Ctrl Pts',(-9.85697350300006,15.2,-5.05515621100002));
#273521=CARTESIAN_POINT('Ctrl Pts',(-9.85697350300006,11.6,-5.05515621100002));
#273522=CARTESIAN_POINT('Ctrl Pts',(-9.85910800200006,15.2,-5.05754771100001));
#273523=CARTESIAN_POINT('Ctrl Pts',(-9.85910800200006,11.6,-5.05754771100001));
#273524=CARTESIAN_POINT('Ctrl Pts',(-9.86124398100005,15.2,-5.05994474600001));
#273525=CARTESIAN_POINT('Ctrl Pts',(-9.86124398100005,11.6,-5.05994474600001));
#273526=CARTESIAN_POINT('Ctrl Pts',(-9.86338143200006,15.2,-5.06234731400002));
#273527=CARTESIAN_POINT('Ctrl Pts',(-9.86338143200006,11.6,-5.06234731400002));
#273528=CARTESIAN_POINT('Ctrl Pts',(-9.86552034100006,15.2,-5.06475541200002));
#273529=CARTESIAN_POINT('Ctrl Pts',(-9.86552034100006,11.6,-5.06475541200002));
#273530=CARTESIAN_POINT('Ctrl Pts',(-9.86766069800005,15.2,-5.06716903800001));
#273531=CARTESIAN_POINT('Ctrl Pts',(-9.86766069800005,11.6,-5.06716903800001));
#273532=CARTESIAN_POINT('Ctrl Pts',(-9.86980249400006,15.2,-5.06958819300001));
#273533=CARTESIAN_POINT('Ctrl Pts',(-9.86980249400006,11.6,-5.06958819300001));
#273534=CARTESIAN_POINT('Ctrl Pts',(-9.87194571500006,15.2,-5.07201287100001));
#273535=CARTESIAN_POINT('Ctrl Pts',(-9.87194571500006,11.6,-5.07201287100001));
#273536=CARTESIAN_POINT('Ctrl Pts',(-9.87409035200006,15.2,-5.07444307400001));
#273537=CARTESIAN_POINT('Ctrl Pts',(-9.87409035200006,11.6,-5.07444307400001));
#273538=CARTESIAN_POINT('Ctrl Pts',(-9.87623639400006,15.2,-5.07687879700002));
#273539=CARTESIAN_POINT('Ctrl Pts',(-9.87623639400006,11.6,-5.07687879700002));
#273540=CARTESIAN_POINT('Ctrl Pts',(-9.87838382900006,15.2,-5.07932003900001));
#273541=CARTESIAN_POINT('Ctrl Pts',(-9.87838382900006,11.6,-5.07932003900001));
#273542=CARTESIAN_POINT('Ctrl Pts',(-9.88053264700006,15.2,-5.08176679900001));
#273543=CARTESIAN_POINT('Ctrl Pts',(-9.88053264700006,11.6,-5.08176679900001));
#273544=CARTESIAN_POINT('Ctrl Pts',(-9.88268283700006,15.2,-5.08421907400002));
#273545=CARTESIAN_POINT('Ctrl Pts',(-9.88268283700006,11.6,-5.08421907400002));
#273546=CARTESIAN_POINT('Ctrl Pts',(-9.88483438900005,15.2,-5.08667686300001));
#273547=CARTESIAN_POINT('Ctrl Pts',(-9.88483438900005,11.6,-5.08667686300001));
#273548=CARTESIAN_POINT('Ctrl Pts',(-9.88698729100006,15.2,-5.08914016200002));
#273549=CARTESIAN_POINT('Ctrl Pts',(-9.88698729100006,11.6,-5.08914016200002));
#273550=CARTESIAN_POINT('Ctrl Pts',(-9.88914153400006,15.2,-5.09160897000001));
#273551=CARTESIAN_POINT('Ctrl Pts',(-9.88914153400006,11.6,-5.09160897000001));
#273552=CARTESIAN_POINT('Ctrl Pts',(-9.89129710500006,15.2,-5.09408328800002));
#273553=CARTESIAN_POINT('Ctrl Pts',(-9.89129710500006,11.6,-5.09408328800002));
#273554=CARTESIAN_POINT('Ctrl Pts',(-9.89345399500005,15.2,-5.09656310900001));
#273555=CARTESIAN_POINT('Ctrl Pts',(-9.89345399500005,11.6,-5.09656310900001));
#273556=CARTESIAN_POINT('Ctrl Pts',(-9.89561219300005,15.2,-5.09904843500002));
#273557=CARTESIAN_POINT('Ctrl Pts',(-9.89561219300005,11.6,-5.09904843500002));
#273558=CARTESIAN_POINT('Ctrl Pts',(-9.89777168700006,15.2,-5.10153926100001));
#273559=CARTESIAN_POINT('Ctrl Pts',(-9.89777168700006,11.6,-5.10153926100001));
#273560=CARTESIAN_POINT('Ctrl Pts',(-9.89993246800006,15.2,-5.10403558800002));
#273561=CARTESIAN_POINT('Ctrl Pts',(-9.89993246800006,11.6,-5.10403558800002));
#273562=CARTESIAN_POINT('Ctrl Pts',(-9.90209452500006,15.2,-5.10653741200001));
#273563=CARTESIAN_POINT('Ctrl Pts',(-9.90209452500006,11.6,-5.10653741200001));
#273564=CARTESIAN_POINT('Ctrl Pts',(-9.90425784700006,15.2,-5.10904473100001));
#273565=CARTESIAN_POINT('Ctrl Pts',(-9.90425784700006,11.6,-5.10904473100001));
#273566=CARTESIAN_POINT('Ctrl Pts',(-9.90642242400006,15.2,-5.11155754400002));
#273567=CARTESIAN_POINT('Ctrl Pts',(-9.90642242400006,11.6,-5.11155754400002));
#273568=CARTESIAN_POINT('Ctrl Pts',(-9.90858824500006,15.2,-5.11407584900001));
#273569=CARTESIAN_POINT('Ctrl Pts',(-9.90858824500006,11.6,-5.11407584900001));
#273570=CARTESIAN_POINT('Ctrl Pts',(-9.91075529900005,15.2,-5.11659964200001));
#273571=CARTESIAN_POINT('Ctrl Pts',(-9.91075529900005,11.6,-5.11659964200001));
#273572=CARTESIAN_POINT('Ctrl Pts',(-9.91292357700006,15.2,-5.11912892300002));
#273573=CARTESIAN_POINT('Ctrl Pts',(-9.91292357700006,11.6,-5.11912892300002));
#273574=CARTESIAN_POINT('Ctrl Pts',(-9.91509306700006,15.2,-5.12166369100001));
#273575=CARTESIAN_POINT('Ctrl Pts',(-9.91509306700006,11.6,-5.12166369100001));
#273576=CARTESIAN_POINT('Ctrl Pts',(-9.91726376000006,15.2,-5.12420394000001));
#273577=CARTESIAN_POINT('Ctrl Pts',(-9.91726376000006,11.6,-5.12420394000001));
#273578=CARTESIAN_POINT('Ctrl Pts',(-9.91943564400006,15.2,-5.12674967200001));
#273579=CARTESIAN_POINT('Ctrl Pts',(-9.91943564400006,11.6,-5.12674967200001));
#273580=CARTESIAN_POINT('Ctrl Pts',(-9.92160871100005,15.2,-5.12930088300001));
#273581=CARTESIAN_POINT('Ctrl Pts',(-9.92160871100005,11.6,-5.12930088300001));
#273582=CARTESIAN_POINT('Ctrl Pts',(-9.92378294700006,15.2,-5.13185757200001));
#273583=CARTESIAN_POINT('Ctrl Pts',(-9.92378294700006,11.6,-5.13185757200001));
#273584=CARTESIAN_POINT('Ctrl Pts',(-9.92595834500005,15.2,-5.13441973500001));
#273585=CARTESIAN_POINT('Ctrl Pts',(-9.92595834500005,11.6,-5.13441973500001));
#273586=CARTESIAN_POINT('Ctrl Pts',(-9.92813489300006,15.2,-5.13698737200002));
#273587=CARTESIAN_POINT('Ctrl Pts',(-9.92813489300006,11.6,-5.13698737200002));
#273588=CARTESIAN_POINT('Ctrl Pts',(-9.93031258000006,15.2,-5.13956048000002));
#273589=CARTESIAN_POINT('Ctrl Pts',(-9.93031258000006,11.6,-5.13956048000002));
#273590=CARTESIAN_POINT('Ctrl Pts',(-9.93249139800006,15.2,-5.14213905700001));
#273591=CARTESIAN_POINT('Ctrl Pts',(-9.93249139800006,11.6,-5.14213905700001));
#273592=CARTESIAN_POINT('Ctrl Pts',(-9.93467133500006,15.2,-5.14472310100002));
#273593=CARTESIAN_POINT('Ctrl Pts',(-9.93467133500006,11.6,-5.14472310100002));
#273594=CARTESIAN_POINT('Ctrl Pts',(-9.93685238200005,15.2,-5.14731261100001));
#273595=CARTESIAN_POINT('Ctrl Pts',(-9.93685238200005,11.6,-5.14731261100001));
#273596=CARTESIAN_POINT('Ctrl Pts',(-9.93903452600006,15.2,-5.14990758300002));
#273597=CARTESIAN_POINT('Ctrl Pts',(-9.93903452600006,11.6,-5.14990758300002));
#273598=CARTESIAN_POINT('Ctrl Pts',(-9.94121776000006,15.2,-5.15250801600001));
#273599=CARTESIAN_POINT('Ctrl Pts',(-9.94121776000006,11.6,-5.15250801600001));
#273600=CARTESIAN_POINT('Ctrl Pts',(-9.94340207300005,15.2,-5.15511390800001));
#273601=CARTESIAN_POINT('Ctrl Pts',(-9.94340207300005,11.6,-5.15511390800001));
#273602=CARTESIAN_POINT('Ctrl Pts',(-9.94558745400006,15.2,-5.15772525700001));
#273603=CARTESIAN_POINT('Ctrl Pts',(-9.94558745400006,11.6,-5.15772525700001));
#273604=CARTESIAN_POINT('Ctrl Pts',(-9.94777389400006,15.2,-5.16034206000001));
#273605=CARTESIAN_POINT('Ctrl Pts',(-9.94777389400006,11.6,-5.16034206000001));
#273606=CARTESIAN_POINT('Ctrl Pts',(-9.94996138000005,15.2,-5.16296431600002));
#273607=CARTESIAN_POINT('Ctrl Pts',(-9.94996138000005,11.6,-5.16296431600002));
#273608=CARTESIAN_POINT('Ctrl Pts',(-9.95214990600006,15.2,-5.16559202200002));
#273609=CARTESIAN_POINT('Ctrl Pts',(-9.95214990600006,11.6,-5.16559202200002));
#273610=CARTESIAN_POINT('Ctrl Pts',(-9.95433945900006,15.2,-5.16822517700001));
#273611=CARTESIAN_POINT('Ctrl Pts',(-9.95433945900006,11.6,-5.16822517700001));
#273612=CARTESIAN_POINT('Ctrl Pts',(-9.95653003000006,15.2,-5.17086377700001));
#273613=CARTESIAN_POINT('Ctrl Pts',(-9.95653003000006,11.6,-5.17086377700001));
#273614=CARTESIAN_POINT('Ctrl Pts',(-9.95872160900005,15.2,-5.17350782200001));
#273615=CARTESIAN_POINT('Ctrl Pts',(-9.95872160900005,11.6,-5.17350782200001));
#273616=CARTESIAN_POINT('Ctrl Pts',(-9.96091418600006,15.2,-5.17615730900001));
#273617=CARTESIAN_POINT('Ctrl Pts',(-9.96091418600006,11.6,-5.17615730900001));
#273618=CARTESIAN_POINT('Ctrl Pts',(-9.96310775000006,15.2,-5.17881223600002));
#273619=CARTESIAN_POINT('Ctrl Pts',(-9.96310775000006,11.6,-5.17881223600002));
#273620=CARTESIAN_POINT('Ctrl Pts',(-9.96530229300006,15.2,-5.18147260100001));
#273621=CARTESIAN_POINT('Ctrl Pts',(-9.96530229300006,11.6,-5.18147260100001));
#273622=CARTESIAN_POINT('Ctrl Pts',(-9.96749780300006,15.2,-5.18413840100001));
#273623=CARTESIAN_POINT('Ctrl Pts',(-9.96749780300006,11.6,-5.18413840100001));
#273624=CARTESIAN_POINT('Ctrl Pts',(-9.96969427100005,15.2,-5.18680963500001));
#273625=CARTESIAN_POINT('Ctrl Pts',(-9.96969427100005,11.6,-5.18680963500001));
#273626=CARTESIAN_POINT('Ctrl Pts',(-9.97189168800006,15.2,-5.18948630000001));
#273627=CARTESIAN_POINT('Ctrl Pts',(-9.97189168800006,11.6,-5.18948630000001));
#273628=CARTESIAN_POINT('Ctrl Pts',(-9.97409004300006,15.2,-5.19216839600002));
#273629=CARTESIAN_POINT('Ctrl Pts',(-9.97409004300006,11.6,-5.19216839600002));
#273630=CARTESIAN_POINT('Ctrl Pts',(-9.97628932500006,15.2,-5.19485591700001));
#273631=CARTESIAN_POINT('Ctrl Pts',(-9.97628932500006,11.6,-5.19485591700001));
#273632=CARTESIAN_POINT('Ctrl Pts',(-9.97848952700006,15.2,-5.19754886400001));
#273633=CARTESIAN_POINT('Ctrl Pts',(-9.97848952700006,11.6,-5.19754886400001));
#273634=CARTESIAN_POINT('Ctrl Pts',(-9.98069063600006,15.2,-5.20024723400001));
#273635=CARTESIAN_POINT('Ctrl Pts',(-9.98069063600006,11.6,-5.20024723400001));
#273636=CARTESIAN_POINT('Ctrl Pts',(-9.98289264400006,15.2,-5.20295102400001));
#273637=CARTESIAN_POINT('Ctrl Pts',(-9.98289264400006,11.6,-5.20295102400001));
#273638=CARTESIAN_POINT('Ctrl Pts',(-9.98509554200006,15.2,-5.20566023400002));
#273639=CARTESIAN_POINT('Ctrl Pts',(-9.98509554200006,11.6,-5.20566023400002));
#273640=CARTESIAN_POINT('Ctrl Pts',(-9.98729931800005,15.2,-5.20837486000001));
#273641=CARTESIAN_POINT('Ctrl Pts',(-9.98729931800005,11.6,-5.20837486000001));
#273642=CARTESIAN_POINT('Ctrl Pts',(-9.98950396400006,15.2,-5.21109489900001));
#273643=CARTESIAN_POINT('Ctrl Pts',(-9.98950396400006,11.6,-5.21109489900001));
#273644=CARTESIAN_POINT('Ctrl Pts',(-9.99170947000006,15.2,-5.21382035100002));
#273645=CARTESIAN_POINT('Ctrl Pts',(-9.99170947000006,11.6,-5.21382035100002));
#273646=CARTESIAN_POINT('Ctrl Pts',(-9.99391582600006,15.2,-5.21655121300002));
#273647=CARTESIAN_POINT('Ctrl Pts',(-9.99391582600006,11.6,-5.21655121300002));
#273648=CARTESIAN_POINT('Ctrl Pts',(-9.99612302200006,15.2,-5.21928748300001));
#273649=CARTESIAN_POINT('Ctrl Pts',(-9.99612302200006,11.6,-5.21928748300001));
#273650=CARTESIAN_POINT('Ctrl Pts',(-9.99833104800006,15.2,-5.22202915700001));
#273651=CARTESIAN_POINT('Ctrl Pts',(-9.99833104800006,11.6,-5.22202915700001));
#273652=CARTESIAN_POINT('Ctrl Pts',(-10.0005398960001,15.2,-5.22477623700001));
#273653=CARTESIAN_POINT('Ctrl Pts',(-10.0005398960001,11.6,-5.22477623700001));
#273654=CARTESIAN_POINT('Ctrl Pts',(-10.0027495550001,15.2,-5.22752871700002));
#273655=CARTESIAN_POINT('Ctrl Pts',(-10.0027495550001,11.6,-5.22752871700002));
#273656=CARTESIAN_POINT('Ctrl Pts',(-10.0049600160001,15.2,-5.23028659500001));
#273657=CARTESIAN_POINT('Ctrl Pts',(-10.0049600160001,11.6,-5.23028659500001));
#273658=CARTESIAN_POINT('Ctrl Pts',(-10.0071712680001,15.2,-5.23304987100001));
#273659=CARTESIAN_POINT('Ctrl Pts',(-10.0071712680001,11.6,-5.23304987100001));
#273660=CARTESIAN_POINT('Ctrl Pts',(-10.0093833030001,15.2,-5.23581854200001));
#273661=CARTESIAN_POINT('Ctrl Pts',(-10.0093833030001,11.6,-5.23581854200001));
#273662=CARTESIAN_POINT('Ctrl Pts',(-10.0115961110001,15.2,-5.23859260400001));
#273663=CARTESIAN_POINT('Ctrl Pts',(-10.0115961110001,11.6,-5.23859260400001));
#273664=CARTESIAN_POINT('Ctrl Pts',(-10.0138096830001,15.2,-5.24137205800002));
#273665=CARTESIAN_POINT('Ctrl Pts',(-10.0138096830001,11.6,-5.24137205800002));
#273666=CARTESIAN_POINT('Ctrl Pts',(-10.0160240080001,15.2,-5.24415689900001));
#273667=CARTESIAN_POINT('Ctrl Pts',(-10.0160240080001,11.6,-5.24415689900001));
#273668=CARTESIAN_POINT('Ctrl Pts',(-10.0182390770001,15.2,-5.24694712600001));
#273669=CARTESIAN_POINT('Ctrl Pts',(-10.0182390770001,11.6,-5.24694712600001));
#273670=CARTESIAN_POINT('Ctrl Pts',(-10.0204548810001,15.2,-5.24974273600002));
#273671=CARTESIAN_POINT('Ctrl Pts',(-10.0204548810001,11.6,-5.24974273600002));
#273672=CARTESIAN_POINT('Ctrl Pts',(-10.0226714120001,15.2,-5.25254372800001));
#273673=CARTESIAN_POINT('Ctrl Pts',(-10.0226714120001,11.6,-5.25254372800001));
#273674=CARTESIAN_POINT('Ctrl Pts',(-10.0248886580001,15.2,-5.25535009900001));
#273675=CARTESIAN_POINT('Ctrl Pts',(-10.0248886580001,11.6,-5.25535009900001));
#273676=CARTESIAN_POINT('Ctrl Pts',(-10.0271066100001,15.2,-5.25816184700002));
#273677=CARTESIAN_POINT('Ctrl Pts',(-10.0271066100001,11.6,-5.25816184700002));
#273678=CARTESIAN_POINT('Ctrl Pts',(-10.0293252590001,15.2,-5.26097897000001));
#273679=CARTESIAN_POINT('Ctrl Pts',(-10.0293252590001,11.6,-5.26097897000001));
#273680=CARTESIAN_POINT('Ctrl Pts',(-10.0315445970001,15.2,-5.26380146500002));
#273681=CARTESIAN_POINT('Ctrl Pts',(-10.0315445970001,11.6,-5.26380146500002));
#273682=CARTESIAN_POINT('Ctrl Pts',(-10.0337646130001,15.2,-5.26662933100001));
#273683=CARTESIAN_POINT('Ctrl Pts',(-10.0337646130001,11.6,-5.26662933100001));
#273684=CARTESIAN_POINT('Ctrl Pts',(-10.0359852980001,15.2,-5.26946256500001));
#273685=CARTESIAN_POINT('Ctrl Pts',(-10.0359852980001,11.6,-5.26946256500001));
#273686=CARTESIAN_POINT('Ctrl Pts',(-10.0382066420001,15.2,-5.27230116500002));
#273687=CARTESIAN_POINT('Ctrl Pts',(-10.0382066420001,11.6,-5.27230116500002));
#273688=CARTESIAN_POINT('Ctrl Pts',(-10.0404286360001,15.2,-5.27514512700002));
#273689=CARTESIAN_POINT('Ctrl Pts',(-10.0404286360001,11.6,-5.27514512700002));
#273690=CARTESIAN_POINT('Ctrl Pts',(-10.0426512720001,15.2,-5.27799445100001));
#273691=CARTESIAN_POINT('Ctrl Pts',(-10.0426512720001,11.6,-5.27799445100001));
#273692=CARTESIAN_POINT('Ctrl Pts',(-10.0448745390001,15.2,-5.28084913400001));
#273693=CARTESIAN_POINT('Ctrl Pts',(-10.0448745390001,11.6,-5.28084913400001));
#273694=CARTESIAN_POINT('Ctrl Pts',(-10.0470984300001,15.2,-5.28370917400002));
#273695=CARTESIAN_POINT('Ctrl Pts',(-10.0470984300001,11.6,-5.28370917400002));
#273696=CARTESIAN_POINT('Ctrl Pts',(-10.0493229330001,15.2,-5.28657456900001));
#273697=CARTESIAN_POINT('Ctrl Pts',(-10.0493229330001,11.6,-5.28657456900001));
#273698=CARTESIAN_POINT('Ctrl Pts',(-10.0515480410001,15.2,-5.28944531500001));
#273699=CARTESIAN_POINT('Ctrl Pts',(-10.0515480410001,11.6,-5.28944531500001));
#273700=CARTESIAN_POINT('Ctrl Pts',(-10.0537737430001,15.2,-5.29232141200001));
#273701=CARTESIAN_POINT('Ctrl Pts',(-10.0537737430001,11.6,-5.29232141200001));
#273702=CARTESIAN_POINT('Ctrl Pts',(-10.0560000300001,15.2,-5.29520285700002));
#273703=CARTESIAN_POINT('Ctrl Pts',(-10.0560000300001,11.6,-5.29520285700002));
#273704=CARTESIAN_POINT('Ctrl Pts',(-10.0582268940001,15.2,-5.29808964700001));
#273705=CARTESIAN_POINT('Ctrl Pts',(-10.0582268940001,11.6,-5.29808964700001));
#273706=CARTESIAN_POINT('Ctrl Pts',(-10.0604543260001,15.2,-5.30098178000001));
#273707=CARTESIAN_POINT('Ctrl Pts',(-10.0604543260001,11.6,-5.30098178000001));
#273708=CARTESIAN_POINT('Ctrl Pts',(-10.0626823150001,15.2,-5.30387925400001));
#273709=CARTESIAN_POINT('Ctrl Pts',(-10.0626823150001,11.6,-5.30387925400001));
#273710=CARTESIAN_POINT('Ctrl Pts',(-10.0649108540001,15.2,-5.30678206600002));
#273711=CARTESIAN_POINT('Ctrl Pts',(-10.0649108540001,11.6,-5.30678206600002));
#273712=CARTESIAN_POINT('Ctrl Pts',(-10.0671399330001,15.2,-5.30969021500002));
#273713=CARTESIAN_POINT('Ctrl Pts',(-10.0671399330001,11.6,-5.30969021500002));
#273714=CARTESIAN_POINT('Ctrl Pts',(-10.0693695420001,15.2,-5.31260369700002));
#273715=CARTESIAN_POINT('Ctrl Pts',(-10.0693695420001,11.6,-5.31260369700002));
#273716=CARTESIAN_POINT('Ctrl Pts',(-10.0715996740001,15.2,-5.31552251300001));
#273717=CARTESIAN_POINT('Ctrl Pts',(-10.0715996740001,11.6,-5.31552251300001));
#273718=CARTESIAN_POINT('Ctrl Pts',(-10.0738303190001,15.2,-5.31844665600001));
#273719=CARTESIAN_POINT('Ctrl Pts',(-10.0738303190001,11.6,-5.31844665600001));
#273720=CARTESIAN_POINT('Ctrl Pts',(-10.0760614660001,15.2,-5.32137612700001));
#273721=CARTESIAN_POINT('Ctrl Pts',(-10.0760614660001,11.6,-5.32137612700001));
#273722=CARTESIAN_POINT('Ctrl Pts',(-10.0782931080001,15.2,-5.32431092300001));
#273723=CARTESIAN_POINT('Ctrl Pts',(-10.0782931080001,11.6,-5.32431092300001));
#273724=CARTESIAN_POINT('Ctrl Pts',(-10.0805252360001,15.2,-5.32725104100002));
#273725=CARTESIAN_POINT('Ctrl Pts',(-10.0805252360001,11.6,-5.32725104100002));
#273726=CARTESIAN_POINT('Ctrl Pts',(-10.0827578410001,15.2,-5.33019648000002));
#273727=CARTESIAN_POINT('Ctrl Pts',(-10.0827578410001,11.6,-5.33019648000002));
#273728=CARTESIAN_POINT('Ctrl Pts',(-10.0849909120001,15.2,-5.33314723600002));
#273729=CARTESIAN_POINT('Ctrl Pts',(-10.0849909120001,11.6,-5.33314723600002));
#273730=CARTESIAN_POINT('Ctrl Pts',(-10.0872244440001,15.2,-5.33610330700002));
#273731=CARTESIAN_POINT('Ctrl Pts',(-10.0872244440001,11.6,-5.33610330700002));
#273732=CARTESIAN_POINT('Ctrl Pts',(-10.0894584250001,15.2,-5.33906469200002));
#273733=CARTESIAN_POINT('Ctrl Pts',(-10.0894584250001,11.6,-5.33906469200002));
#273734=CARTESIAN_POINT('Ctrl Pts',(-10.0916928480001,15.2,-5.34203138700001));
#273735=CARTESIAN_POINT('Ctrl Pts',(-10.0916928480001,11.6,-5.34203138700001));
#273736=CARTESIAN_POINT('Ctrl Pts',(-10.0939277020001,15.2,-5.34500339300001));
#273737=CARTESIAN_POINT('Ctrl Pts',(-10.0939277020001,11.6,-5.34500339300001));
#273738=CARTESIAN_POINT('Ctrl Pts',(-10.0961629820001,15.2,-5.34798070300001));
#273739=CARTESIAN_POINT('Ctrl Pts',(-10.0961629820001,11.6,-5.34798070300001));
#273740=CARTESIAN_POINT('Ctrl Pts',(-10.0983986740001,15.2,-5.35096331800001));
#273741=CARTESIAN_POINT('Ctrl Pts',(-10.0983986740001,11.6,-5.35096331800001));
#273742=CARTESIAN_POINT('Ctrl Pts',(-10.1006347720001,15.2,-5.35395123400002));
#273743=CARTESIAN_POINT('Ctrl Pts',(-10.1006347720001,11.6,-5.35395123400002));
#273744=CARTESIAN_POINT('Ctrl Pts',(-10.1028712650001,15.2,-5.35694444900002));
#273745=CARTESIAN_POINT('Ctrl Pts',(-10.1028712650001,11.6,-5.35694444900002));
#273746=CARTESIAN_POINT('Ctrl Pts',(-10.1051081460001,15.2,-5.35994296100001));
#273747=CARTESIAN_POINT('Ctrl Pts',(-10.1051081460001,11.6,-5.35994296100001));
#273748=CARTESIAN_POINT('Ctrl Pts',(-10.1073454040001,15.2,-5.36294676700001));
#273749=CARTESIAN_POINT('Ctrl Pts',(-10.1073454040001,11.6,-5.36294676700001));
#273750=CARTESIAN_POINT('Ctrl Pts',(-10.1095830330001,15.2,-5.36595586500002));
#273751=CARTESIAN_POINT('Ctrl Pts',(-10.1095830330001,11.6,-5.36595586500002));
#273752=CARTESIAN_POINT('Ctrl Pts',(-10.1118210230001,15.2,-5.36897025200001));
#273753=CARTESIAN_POINT('Ctrl Pts',(-10.1118210230001,11.6,-5.36897025200001));
#273754=CARTESIAN_POINT('Ctrl Pts',(-10.1140593680001,15.2,-5.37198992800001));
#273755=CARTESIAN_POINT('Ctrl Pts',(-10.1140593680001,11.6,-5.37198992800001));
#273756=CARTESIAN_POINT('Ctrl Pts',(-10.1162980580001,15.2,-5.37501489000002));
#273757=CARTESIAN_POINT('Ctrl Pts',(-10.1162980580001,11.6,-5.37501489000002));
#273758=CARTESIAN_POINT('Ctrl Pts',(-10.1185370870001,15.2,-5.37804513400001));
#273759=CARTESIAN_POINT('Ctrl Pts',(-10.1185370870001,11.6,-5.37804513400001));
#273760=CARTESIAN_POINT('Ctrl Pts',(-10.1207764440001,15.2,-5.38108065900001));
#273761=CARTESIAN_POINT('Ctrl Pts',(-10.1207764440001,11.6,-5.38108065900001));
#273762=CARTESIAN_POINT('Ctrl Pts',(-10.1230161200001,15.2,-5.38412146200002));
#273763=CARTESIAN_POINT('Ctrl Pts',(-10.1230161200001,11.6,-5.38412146200002));
#273764=CARTESIAN_POINT('Ctrl Pts',(-10.1252561030001,15.2,-5.38716754100002));
#273765=CARTESIAN_POINT('Ctrl Pts',(-10.1252561030001,11.6,-5.38716754100002));
#273766=CARTESIAN_POINT('Ctrl Pts',(-10.1274963840001,15.2,-5.39021889200002));
#273767=CARTESIAN_POINT('Ctrl Pts',(-10.1274963840001,11.6,-5.39021889200002));
#273768=CARTESIAN_POINT('Ctrl Pts',(-10.1297369520001,15.2,-5.39327551300001));
#273769=CARTESIAN_POINT('Ctrl Pts',(-10.1297369520001,11.6,-5.39327551300001));
#273770=CARTESIAN_POINT('Ctrl Pts',(-10.1319777960001,15.2,-5.39633740000002));
#273771=CARTESIAN_POINT('Ctrl Pts',(-10.1319777960001,11.6,-5.39633740000002));
#273772=CARTESIAN_POINT('Ctrl Pts',(-10.1342189100001,15.2,-5.39940455200002));
#273773=CARTESIAN_POINT('Ctrl Pts',(-10.1342189100001,11.6,-5.39940455200002));
#273774=CARTESIAN_POINT('Ctrl Pts',(-10.1364602890001,15.2,-5.40247696800002));
#273775=CARTESIAN_POINT('Ctrl Pts',(-10.1364602890001,11.6,-5.40247696800002));
#273776=CARTESIAN_POINT('Ctrl Pts',(-10.1387019270001,15.2,-5.40555464300001));
#273777=CARTESIAN_POINT('Ctrl Pts',(-10.1387019270001,11.6,-5.40555464300001));
#273778=CARTESIAN_POINT('Ctrl Pts',(-10.1409438220001,15.2,-5.40863758200001));
#273779=CARTESIAN_POINT('Ctrl Pts',(-10.1409438220001,11.6,-5.40863758200001));
#273780=CARTESIAN_POINT('Ctrl Pts',(-10.1427375440001,15.2,-5.41110814000001));
#273781=CARTESIAN_POINT('Ctrl Pts',(-10.1427375440001,11.6,-5.41110814000001));
#273782=CARTESIAN_POINT('Ctrl Pts',(-10.1440829500001,15.2,-5.41296342600001));
#273783=CARTESIAN_POINT('Ctrl Pts',(-10.1440829500001,11.6,-5.41296342600001));
#273784=CARTESIAN_POINT('Ctrl Pts',(-10.1449799400001,15.2,-5.41420133600001));
#273785=CARTESIAN_POINT('Ctrl Pts',(-10.1449799400001,11.6,-5.41420133600001));
#273786=CARTESIAN_POINT('Ctrl Pts',(-10.1454284470001,15.2,-5.41482055400001));
#273787=CARTESIAN_POINT('Ctrl Pts',(-10.1454284470001,11.6,-5.41482055400001));
#273788=CARTESIAN_POINT('Ctrl Pts',(-9.31239140100006,15.2,-4.57383771200002));
#273789=CARTESIAN_POINT('Ctrl Pts',(-9.31392145135453,15.2,-4.5747602550189));
#273790=CARTESIAN_POINT('Ctrl Pts',(-9.31549767328181,15.2,-4.5757169317027));
#273791=CARTESIAN_POINT('Ctrl Pts',(-9.31711891458909,15.2,-4.57670776794144));
#273792=CARTESIAN_POINT('Ctrl Pts',(-9.31874797434146,15.2,-4.57770338249336));
#273793=CARTESIAN_POINT('Ctrl Pts',(-9.32042248440092,15.2,-4.57873349977316));
#273794=CARTESIAN_POINT('Ctrl Pts',(-9.32214130041636,15.2,-4.57979816338637));
#273795=CARTESIAN_POINT('Ctrl Pts',(-9.32386011627568,15.2,-4.58086282690287));
#273796=CARTESIAN_POINT('Ctrl Pts',(-9.32562323899895,15.2,-4.58196203944949));
#273797=CARTESIAN_POINT('Ctrl Pts',(-9.32742955676663,15.2,-4.58309584749161));
#273798=CARTESIAN_POINT('Ctrl Pts',(-9.32923587453431,15.2,-4.58422965553373));
#273799=CARTESIAN_POINT('Ctrl Pts',(-9.33108538730214,15.1999999999999,
-4.5853980568443));
#273800=CARTESIAN_POINT('Ctrl Pts',(-9.33297701357543,15.2,-4.58660109210866));
#273801=CARTESIAN_POINT('Ctrl Pts',(-9.33486864002055,15.2,-4.5878041274823));
#273802=CARTESIAN_POINT('Ctrl Pts',(-9.3368023827215,15.2,-4.58904179825028));
#273803=CARTESIAN_POINT('Ctrl Pts',(-9.33877718899858,15.2,-4.59031413865532));
#273804=CARTESIAN_POINT('Ctrl Pts',(-9.3407519950963,15.2,-4.59158647894478));
#273805=CARTESIAN_POINT('Ctrl Pts',(-9.34276786524956,15.2,-4.59289349118482));
#273806=CARTESIAN_POINT('Ctrl Pts',(-9.34482377851759,15.2,-4.59423520622557));
#273807=CARTESIAN_POINT('Ctrl Pts',(-9.34687969178564,15.2,-4.59557692126631));
#273808=CARTESIAN_POINT('Ctrl Pts',(-9.34897564777141,15.2,-4.59695334018431));
#273809=CARTESIAN_POINT('Ctrl Pts',(-9.3511106521088,15.2,-4.59836449038153));
#273810=CARTESIAN_POINT('Ctrl Pts',(-9.35324565664012,15.2,-4.59977564070692));
#273811=CARTESIAN_POINT('Ctrl Pts',(-9.35541970904296,15.2,-4.60122152401996));
#273812=CARTESIAN_POINT('Ctrl Pts',(-9.35763184074945,15.2,-4.60270216418635));
#273813=CARTESIAN_POINT('Ctrl Pts',(-9.35984397225501,15.2,-4.60418280421825));
#273814=CARTESIAN_POINT('Ctrl Pts',(-9.36209418289796,15.2,-4.60569820177273));
#273815=CARTESIAN_POINT('Ctrl Pts',(-9.36438152939981,15.2,-4.60724837688458));
#273816=CARTESIAN_POINT('Ctrl Pts',(-9.36666887590164,15.2,-4.60879855199643));
#273817=CARTESIAN_POINT('Ctrl Pts',(-9.36899335821715,15.2,-4.61038350755551));
#273818=CARTESIAN_POINT('Ctrl Pts',(-9.37135405587983,15.2,-4.61200325866183));
#273819=CARTESIAN_POINT('Ctrl Pts',(-9.3737147535425,15.2,-4.61362300976815));
#273820=CARTESIAN_POINT('Ctrl Pts',(-9.37611166665067,15.2,-4.61527755752124));
#273821=CARTESIAN_POINT('Ctrl Pts',(-9.37854389747655,15.2,-4.61696691654082));
#273822=CARTESIAN_POINT('Ctrl Pts',(-9.38097612852336,15.2,-4.61865627571385));
#273823=CARTESIAN_POINT('Ctrl Pts',(-9.38344367732367,15.2,-4.62038044747359));
#273824=CARTESIAN_POINT('Ctrl Pts',(-9.38594566837816,15.2,-4.6221394416543));
#273825=CARTESIAN_POINT('Ctrl Pts',(-9.38844765920541,15.2,-4.62389843567523));
#273826=CARTESIAN_POINT('Ctrl Pts',(-9.39098409293896,15.2,-4.62569225337402));
#273827=CARTESIAN_POINT('Ctrl Pts',(-9.3935541129405,15.2,-4.62752090148246));
#273828=CARTESIAN_POINT('Ctrl Pts',(-9.39612413294204,15.2,-4.62934954959089));
#273829=CARTESIAN_POINT('Ctrl Pts',(-9.39872774117737,15.2,-4.63121303114775));
#273830=CARTESIAN_POINT('Ctrl Pts',(-9.40136410124598,15.2,-4.63311134807638));
#273831=CARTESIAN_POINT('Ctrl Pts',(-9.40400046155406,15.2,-4.63500966517743));
#273832=CARTESIAN_POINT('Ctrl Pts',(-9.40666957427374,15.2,-4.63694281996525));
#273833=CARTESIAN_POINT('Ctrl Pts',(-9.40937062267234,15.2,-4.63891081407403));
#273834=CARTESIAN_POINT('Ctrl Pts',(-9.4120716708256,15.2,-4.64087880800404));
#273835=CARTESIAN_POINT('Ctrl Pts',(-9.4148046571617,15.2,-4.64288164279723));
#273836=CARTESIAN_POINT('Ctrl Pts',(-9.41756878149041,15.2,-4.64491931573237));
#273837=CARTESIAN_POINT('Ctrl Pts',(-9.42033290581914,15.2,-4.64695698866751));
#273838=CARTESIAN_POINT('Ctrl Pts',(-9.42312816853842,15.2,-4.64902950149088));
#273839=CARTESIAN_POINT('Ctrl Pts',(-9.42595379268368,15.2,-4.65113685049526));
#273840=CARTESIAN_POINT('Ctrl Pts',(-9.42877941708561,15.2,-4.65324419969107));
#273841=CARTESIAN_POINT('Ctrl Pts',(-9.4316353997261,15.2,-4.65538638539788));
#273842=CARTESIAN_POINT('Ctrl Pts',(-9.43452097952922,15.2,-4.65756340246064));
#273843=CARTESIAN_POINT('Ctrl Pts',(-9.43740655907024,15.2,-4.65974041932565));
#273844=CARTESIAN_POINT('Ctrl Pts',(-9.44032173581531,15.2,-4.66195226643992));
#273845=CARTESIAN_POINT('Ctrl Pts',(-9.44326576245833,15.2,-4.66419893644161));
#273846=CARTESIAN_POINT('Ctrl Pts',(-9.44620978910137,15.2,-4.66644560644331));
#273847=CARTESIAN_POINT('Ctrl Pts',(-9.4491826676622,15.2,-4.66872709947977));
#273848=CARTESIAN_POINT('Ctrl Pts',(-9.45218366545143,15.2,-4.6710434045093));
#273849=CARTESIAN_POINT('Ctrl Pts',(-9.45518466351327,15.2,-4.67335970974922));
#273850=CARTESIAN_POINT('Ctrl Pts',(-9.45821378240637,15.2,-4.67571082796929));
#273851=CARTESIAN_POINT('Ctrl Pts',(-9.46127030532485,15.2,-4.67809674501836));
#273852=CARTESIAN_POINT('Ctrl Pts',(-9.46432682796567,15.2,-4.68048266185072));
#273853=CARTESIAN_POINT('Ctrl Pts',(-9.46741075545025,15.2,-4.68290337572906));
#273854=CARTESIAN_POINT('Ctrl Pts',(-9.47052138718476,15.2,-4.68535887548441));
#273855=CARTESIAN_POINT('Ctrl Pts',(-9.47363201891927,15.2,-4.68781437523976));
#273856=CARTESIAN_POINT('Ctrl Pts',(-9.47676935546881,15.2,-4.69030465833076));
#273857=CARTESIAN_POINT('Ctrl Pts',(-9.47993270826938,15.2,-4.69282970715415));
#273858=CARTESIAN_POINT('Ctrl Pts',(-9.48256883569898,15.2,-4.69493391458343));
#273859=CARTESIAN_POINT('Ctrl Pts',(-9.48522303133183,15.2,-4.69706226520502));
#273860=CARTESIAN_POINT('Ctrl Pts',(-9.48789490535871,15.2,-4.69921474763433));
#273861=CARTESIAN_POINT('Ctrl Pts',(-9.49056677938559,15.2,-4.70136723006365));
#273862=CARTESIAN_POINT('Ctrl Pts',(-9.49325633158075,15.2,-4.70354384381107));
#273863=CARTESIAN_POINT('Ctrl Pts',(-9.49596317673188,15.2,-4.70574457701543));
#273864=CARTESIAN_POINT('Ctrl Pts',(-9.498670021883,15.2,-4.70794531021979));
#273865=CARTESIAN_POINT('Ctrl Pts',(-9.50139416162778,15.2,-4.71017016276661));
#273866=CARTESIAN_POINT('Ctrl Pts',(-9.50413521822501,15.2,-4.71241912026661));
#273867=CARTESIAN_POINT('Ctrl Pts',(-9.50687627482223,15.2,-4.71466807776662));
#273868=CARTESIAN_POINT('Ctrl Pts',(-9.50963424783888,15.2,-4.71694114255182));
#273869=CARTESIAN_POINT('Ctrl Pts',(-9.51240876618487,15.2,-4.71923829749288));
#273870=CARTESIAN_POINT('Ctrl Pts',(-9.51518328453086,15.2,-4.72153545243395));
#273871=CARTESIAN_POINT('Ctrl Pts',(-9.51797434851064,15.2,-4.72385669852445));
#273872=CARTESIAN_POINT('Ctrl Pts',(-9.52078159115037,15.2,-4.72620202088682));
#273873=CARTESIAN_POINT('Ctrl Pts',(-9.52358883379011,15.2,-4.72854734324919));
#273874=CARTESIAN_POINT('Ctrl Pts',(-9.52641225669053,15.2,-4.73091674053871));
#273875=CARTESIAN_POINT('Ctrl Pts',(-9.52925149842746,15.2,-4.73331019866496));
#273876=CARTESIAN_POINT('Ctrl Pts',(-9.53209074016441,15.2,-4.73570365679122));
#273877=CARTESIAN_POINT('Ctrl Pts',(-9.53494580164996,15.2,-4.7381211734154));
#273878=CARTESIAN_POINT('Ctrl Pts',(-9.53781632776663,15.2,-4.7405627325668));
#273879=CARTESIAN_POINT('Ctrl Pts',(-9.54068685388331,15.2,-4.7430042917182));
#273880=CARTESIAN_POINT('Ctrl Pts',(-9.54357284573936,15.2,-4.74546989288476));
#273881=CARTESIAN_POINT('Ctrl Pts',(-9.54647395337948,15.2,-4.74795951781727));
#273882=CARTESIAN_POINT('Ctrl Pts',(-9.54937506101962,15.2,-4.75044914274978));
#273883=CARTESIAN_POINT('Ctrl Pts',(-9.55229128489328,15.2,-4.7529627916299));
#273884=CARTESIAN_POINT('Ctrl Pts',(-9.55522228086673,15.2,-4.75550044559022));
#273885=CARTESIAN_POINT('Ctrl Pts',(-9.55815327652072,15.2,-4.75803809927393));
#273886=CARTESIAN_POINT('Ctrl Pts',(-9.56109904385334,15.2,-4.76059975770666));
#273887=CARTESIAN_POINT('Ctrl Pts',(-9.5640592454045,15.2,-4.76318540068676));
#273888=CARTESIAN_POINT('Ctrl Pts',(-9.56701944727832,15.2,-4.7657710439487));
#273889=CARTESIAN_POINT('Ctrl Pts',(-9.56999408261026,15.2,-4.76838067303523));
#273890=CARTESIAN_POINT('Ctrl Pts',(-9.57298281781743,15.2,-4.77101426463048));
#273891=CARTESIAN_POINT('Ctrl Pts',(-9.57597155302458,15.2,-4.77364785622573));
#273892=CARTESIAN_POINT('Ctrl Pts',(-9.57897438660657,15.2,-4.77630541294561));
#273893=CARTESIAN_POINT('Ctrl Pts',(-9.58199099264712,15.2,-4.77898691037422));
#273894=CARTESIAN_POINT('Ctrl Pts',(-9.58561092009308,15.2,-4.78220470746392));
#273895=CARTESIAN_POINT('Ctrl Pts',(-9.58925067816236,15.2,-4.78545698304766));
#273896=CARTESIAN_POINT('Ctrl Pts',(-9.59290970512903,15.2,-4.78874369530966));
#273897=CARTESIAN_POINT('Ctrl Pts',(-9.59595889410176,15.2,-4.79148262204539));
#273898=CARTESIAN_POINT('Ctrl Pts',(-9.59902146667348,15.2,-4.79424546467918));
#273899=CARTESIAN_POINT('Ctrl Pts',(-9.60209710216066,15.2,-4.79703219863947));
#273900=CARTESIAN_POINT('Ctrl Pts',(-9.60455761034924,15.2,-4.79926158562544));
#273901=CARTESIAN_POINT('Ctrl Pts',(-9.6070264804701,15.2,-4.80150626259555));
#273902=CARTESIAN_POINT('Ctrl Pts',(-9.6095035493226,15.2,-4.80376621829868));
#273903=CARTESIAN_POINT('Ctrl Pts',(-9.61198061851259,15.2,-4.80602617430972));
#273904=CARTESIAN_POINT('Ctrl Pts',(-9.61446588758684,15.2,-4.80830140910293));
#273905=CARTESIAN_POINT('Ctrl Pts',(-9.6169591975702,15.2,-4.81059190856574));
#273906=CARTESIAN_POINT('Ctrl Pts',(-9.61945250721385,15.2,-4.81288240771646));
#273907=CARTESIAN_POINT('Ctrl Pts',(-9.62195385795338,15.2,-4.8151881740372));
#273908=CARTESIAN_POINT('Ctrl Pts',(-9.62446309080331,15.2,-4.81750919056869));
#273909=CARTESIAN_POINT('Ctrl Pts',(-9.62697232399511,15.2,-4.81983020741642));
#273910=CARTESIAN_POINT('Ctrl Pts',(-9.62948943990175,15.2,-4.82216647831043));
#273911=CARTESIAN_POINT('Ctrl Pts',(-9.6320142837065,15.2,-4.82451798771733));
#273912=CARTESIAN_POINT('Ctrl Pts',(-9.63453912716724,15.2,-4.82686949680385));
#273913=CARTESIAN_POINT('Ctrl Pts',(-9.63707169781845,15.2,-4.82923624555923));
#273914=CARTESIAN_POINT('Ctrl Pts',(-9.63961184084815,15.2,-4.83161821937107));
#273915=CARTESIAN_POINT('Ctrl Pts',(-9.64215198422393,15.2,-4.83400019350745));
#273916=CARTESIAN_POINT('Ctrl Pts',(-9.6446997014748,15.2,-4.83639739330373));
#273917=CARTESIAN_POINT('Ctrl Pts',(-9.64725483872565,15.2,-4.83880980521398));
#273918=CARTESIAN_POINT('Ctrl Pts',(-9.64980997562837,15.2,-4.84122221679555));
#273919=CARTESIAN_POINT('Ctrl Pts',(-9.65237253334902,15.2,-4.84364983922404));
#273920=CARTESIAN_POINT('Ctrl Pts',(-9.65494236030487,15.2,-4.84609266013389));
#273921=CARTESIAN_POINT('Ctrl Pts',(-9.65751218761084,15.2,-4.84853548137659));
#273922=CARTESIAN_POINT('Ctrl Pts',(-9.66008928519087,15.2,-4.85099349973058));
#273923=CARTESIAN_POINT('Ctrl Pts',(-9.66267350251012,15.2,-4.85346670104331));
#273924=CARTESIAN_POINT('Ctrl Pts',(-9.66525771947728,15.2,-4.85593990201906));
#273925=CARTESIAN_POINT('Ctrl Pts',(-9.66784905781333,15.2,-4.85842828513574));
#273926=CARTESIAN_POINT('Ctrl Pts',(-9.67044736810021,15.2,-4.86093183737397));
#273927=CARTESIAN_POINT('Ctrl Pts',(-9.6730456787411,15.2,-4.8634353899533));
#273928=CARTESIAN_POINT('Ctrl Pts',(-9.67565096202709,15.2,-4.86595411054239));
#273929=CARTESIAN_POINT('Ctrl Pts',(-9.67826307255836,15.2,-4.86848798395828));
#273930=CARTESIAN_POINT('Ctrl Pts',(-9.68087518308964,15.2,-4.87102185737418));
#273931=CARTESIAN_POINT('Ctrl Pts',(-9.68349411927721,15.2,-4.87357088540569));
#273932=CARTESIAN_POINT('Ctrl Pts',(-9.68611973792099,15.2,-4.87613504943587));
#273933=CARTESIAN_POINT('Ctrl Pts',(-9.68874535620702,15.2,-4.87869921311667));
#273934=CARTESIAN_POINT('Ctrl Pts',(-9.69137765681035,15.2,-4.88127851637635));
#273935=CARTESIAN_POINT('Ctrl Pts',(-9.69401649577323,15.2,-4.88387294073152));
#273936=CARTESIAN_POINT('Ctrl Pts',(-9.69665533509566,15.2,-4.88646736544018));
#273937=CARTESIAN_POINT('Ctrl Pts',(-9.69930071320232,15.2,-4.88907691257618));
#273938=CARTESIAN_POINT('Ctrl Pts',(-9.70195248795859,15.2,-4.89170156588742));
#273939=CARTESIAN_POINT('Ctrl Pts',(-9.70460426235357,15.2,-4.89432621884106));
#273940=CARTESIAN_POINT('Ctrl Pts',(-9.70726243379217,15.2,-4.89696597790942));
#273941=CARTESIAN_POINT('Ctrl Pts',(-9.70992686274061,15.2,-4.89962082752473));
#273942=CARTESIAN_POINT('Ctrl Pts',(-9.71259129205207,15.2,-4.90227567750177));
#273943=CARTESIAN_POINT('Ctrl Pts',(-9.71526197812224,15.2,-4.90494561756343));
#273944=CARTESIAN_POINT('Ctrl Pts',(-9.71793878168015,15.2,-4.90763063162299));
#273945=CARTESIAN_POINT('Ctrl Pts',(-9.72128478594518,15.2,-4.91098689901451));
#273946=CARTESIAN_POINT('Ctrl Pts',(-9.7246403505394,15.2,-4.91436671868765));
#273947=CARTESIAN_POINT('Ctrl Pts',(-9.72800520470683,15.2,-4.91777005924512));
#273948=CARTESIAN_POINT('Ctrl Pts',(-9.73137005887425,15.2,-4.9211733998026));
#273949=CARTESIAN_POINT('Ctrl Pts',(-9.73474420335293,15.2,-4.92460025986046));
#273950=CARTESIAN_POINT('Ctrl Pts',(-9.73812737495089,15.2,-4.92805060791794));
#273951=CARTESIAN_POINT('Ctrl Pts',(-9.74083391200801,15.2,-4.93081088613827));
#273952=CARTESIAN_POINT('Ctrl Pts',(-9.74354622543582,15.2,-4.93358619639133));
#273953=CARTESIAN_POINT('Ctrl Pts',(-9.74626418178152,15.2,-4.93637652006472));
#273954=CARTESIAN_POINT('Ctrl Pts',(-9.74898213849753,15.2,-4.9391668441183));
#273955=CARTESIAN_POINT('Ctrl Pts',(-9.75170573663861,15.2,-4.94197218401417));
#273956=CARTESIAN_POINT('Ctrl Pts',(-9.75443484595458,15.2,-4.94479252000276));
#273957=CARTESIAN_POINT('Ctrl Pts',(-9.75716395489872,15.2,-4.94761285560708));
#273958=CARTESIAN_POINT('Ctrl Pts',(-9.75989857169488,15.2,-4.95044818819274));
#273959=CARTESIAN_POINT('Ctrl Pts',(-9.76263856802609,15.2,-4.95329849979209));
#273960=CARTESIAN_POINT('Ctrl Pts',(-9.76537856473063,15.2,-4.95614881177979));
#273961=CARTESIAN_POINT('Ctrl Pts',(-9.76812393932808,15.2,-4.95901410334082));
#273962=CARTESIAN_POINT('Ctrl Pts',(-9.77087456161587,15.2,-4.96189435614299));
#273963=CARTESIAN_POINT('Ctrl Pts',(-9.77362518352887,15.2,-4.96477460855272));
#273964=CARTESIAN_POINT('Ctrl Pts',(-9.77638105387264,15.2,-4.96766982170941));
#273965=CARTESIAN_POINT('Ctrl Pts',(-9.77914204175771,15.2,-4.97057997797052));
#273966=CARTESIAN_POINT('Ctrl Pts',(-9.78190303001894,15.2,-4.97349013462814));
#273967=CARTESIAN_POINT('Ctrl Pts',(-9.78466913800581,15.2,-4.9764152353709));
#273968=CARTESIAN_POINT('Ctrl Pts',(-9.78744023676829,15.2,-4.97935526003212));
#273969=CARTESIAN_POINT('Ctrl Pts',(-9.79021133515321,15.2,-4.98229528429275));
#273970=CARTESIAN_POINT('Ctrl Pts',(-9.79298742348709,15.2,-4.98525023270316));
#273971=CARTESIAN_POINT('Ctrl Pts',(-9.79576837653703,15.2,-4.9882200870144));
#273972=CARTESIAN_POINT('Ctrl Pts',(-9.79854932996587,15.2,-4.99118994173029));
#273973=CARTESIAN_POINT('Ctrl Pts',(-9.80133514680659,15.2,-4.9941747022415));
#273974=CARTESIAN_POINT('Ctrl Pts',(-9.80412570302694,15.2,-4.99717435075201));
#273975=CARTESIAN_POINT('Ctrl Pts',(-9.80691625886708,15.2,-5.00017399885381));
#273976=CARTESIAN_POINT('Ctrl Pts',(-9.80971155279107,15.2,-5.0031885337955));
#273977=CARTESIAN_POINT('Ctrl Pts',(-9.81251146128392,15.2,-5.00621793604632));
#273978=CARTESIAN_POINT('Ctrl Pts',(-9.81531137015826,15.2,-5.0092473387099));
#273979=CARTESIAN_POINT('Ctrl Pts',(-9.81811589324418,15.2,-5.01229160993879));
#273980=CARTESIAN_POINT('Ctrl Pts',(-9.82092490800837,15.2,-5.01535072921662));
#273981=CARTESIAN_POINT('Ctrl Pts',(-9.82373392277256,15.2,-5.01840984849443));
#273982=CARTESIAN_POINT('Ctrl Pts',(-9.82654742665396,15.2,-5.02148381624067));
#273983=CARTESIAN_POINT('Ctrl Pts',(-9.8293653014191,15.2,-5.02457261352165));
#273984=CARTESIAN_POINT('Ctrl Pts',(-9.8321831758003,15.2,-5.02766141038177));
#273985=CARTESIAN_POINT('Ctrl Pts',(-9.83500541940801,15.2,-5.0307650353942));
#273986=CARTESIAN_POINT('Ctrl Pts',(-9.83783191002311,15.2,-5.0338834702645));
#273987=CARTESIAN_POINT('Ctrl Pts',(-9.84065840102332,15.2,-5.03700190555969));
#273988=CARTESIAN_POINT('Ctrl Pts',(-9.84348913920863,15.2,-5.04013515023326));
#273989=CARTESIAN_POINT('Ctrl Pts',(-9.84632400669687,15.2,-5.04328318423967));
#273990=CARTESIAN_POINT('Ctrl Pts',(-9.84915887379886,15.2,-5.04643121781715));
#273991=CARTESIAN_POINT('Ctrl Pts',(-9.85199786805311,15.2,-5.04959404073994));
#273992=CARTESIAN_POINT('Ctrl Pts',(-9.85484087254266,15.2,-5.052771632257));
#273993=CARTESIAN_POINT('Ctrl Pts',(-9.85768387741957,15.2,-5.055949224207));
#273994=CARTESIAN_POINT('Ctrl Pts',(-9.86053089131561,15.2,-5.05914158624857));
#273995=CARTESIAN_POINT('Ctrl Pts',(-9.86338179694708,15.2,-5.06234869697374));
#273996=CARTESIAN_POINT('Ctrl Pts',(-9.86694542879219,15.2,-5.06635758516173));
#273997=CARTESIAN_POINT('Ctrl Pts',(-9.87051513947279,15.2,-5.07038951664512));
#273998=CARTESIAN_POINT('Ctrl Pts',(-9.8740907037094,15.2,-5.07444445456368));
#273999=CARTESIAN_POINT('Ctrl Pts',(-9.87695115486483,15.2,-5.07768840463335));
#274000=CARTESIAN_POINT('Ctrl Pts',(-9.87981535070587,15.2,-5.08094707675383));
#274001=CARTESIAN_POINT('Ctrl Pts',(-9.88268317724897,15.2,-5.0842204522075));
#274002=CARTESIAN_POINT('Ctrl Pts',(-9.88555100418281,15.2,-5.08749382810716));
#274003=CARTESIAN_POINT('Ctrl Pts',(-9.88842246196105,15.2,-5.09078190490244));
#274004=CARTESIAN_POINT('Ctrl Pts',(-9.89129743515057,15.2,-5.09408466430429));
#274005=CARTESIAN_POINT('Ctrl Pts',(-9.89417240794838,15.2,-5.09738742325614));
#274006=CARTESIAN_POINT('Ctrl Pts',(-9.89705089622251,15.2,-5.10070486193438));
#274007=CARTESIAN_POINT('Ctrl Pts',(-9.89993278676448,15.2,-5.10403696199437));
#274008=CARTESIAN_POINT('Ctrl Pts',(-9.90281467769911,15.2,-5.10736906250835));
#274009=CARTESIAN_POINT('Ctrl Pts',(-9.90569997112302,15.2,-5.11071582267962));
#274010=CARTESIAN_POINT('Ctrl Pts',(-9.90858855350288,15.2,-5.11407722130822));
#274011=CARTESIAN_POINT('Ctrl Pts',(-9.91147713548918,15.2,-5.11743861947884));
#274012=CARTESIAN_POINT('Ctrl Pts',(-9.91436900723339,15.2,-5.1208146564282));
#274013=CARTESIAN_POINT('Ctrl Pts',(-9.91726405736331,15.2,-5.12420531020803));
#274014=CARTESIAN_POINT('Ctrl Pts',(-9.91943534505935,15.2,-5.1267483006584));
#274015=CARTESIAN_POINT('Ctrl Pts',(-9.92160842085518,15.2,-5.12929951423611));
#274016=CARTESIAN_POINT('Ctrl Pts',(-9.92378323698427,15.2,-5.13185893997534));
#274017=CARTESIAN_POINT('Ctrl Pts',(-9.92595805350845,15.2,-5.13441836617954));
#274018=CARTESIAN_POINT('Ctrl Pts',(-9.9281346112081,15.2,-5.13698600510269));
#274019=CARTESIAN_POINT('Ctrl Pts',(-9.93031286319157,15.2,-5.1395618478115));
#274020=CARTESIAN_POINT('Ctrl Pts',(-9.93249111477933,15.2,-5.14213769005236));
#274021=CARTESIAN_POINT('Ctrl Pts',(-9.93467106195033,15.2,-5.14472173610946));
#274022=CARTESIAN_POINT('Ctrl Pts',(-9.93685265653787,15.2,-5.14731397680765));
#274023=CARTESIAN_POINT('Ctrl Pts',(-9.93903425112541,15.2,-5.14990621750584));
#274024=CARTESIAN_POINT('Ctrl Pts',(-9.94121749392148,15.2,-5.15250665203523));
#274025=CARTESIAN_POINT('Ctrl Pts',(-9.9434023400187,15.2,-5.155115272244));
#274026=CARTESIAN_POINT('Ctrl Pts',(-9.94558718611591,15.2,-5.15772389245277));
#274027=CARTESIAN_POINT('Ctrl Pts',(-9.94777363480096,15.2,-5.1603406977644));
#274028=CARTESIAN_POINT('Ctrl Pts',(-9.94996163993972,15.2,-5.16296567851424));
#274029=CARTESIAN_POINT('Ctrl Pts',(-9.95214964507848,15.2,-5.16559065926408));
#274030=CARTESIAN_POINT('Ctrl Pts',(-9.95433920767431,15.2,-5.16822381565886));
#274031=CARTESIAN_POINT('Ctrl Pts',(-9.95653028176125,15.2,-5.17086513793719));
#274032=CARTESIAN_POINT('Ctrl Pts',(-9.95872135584818,15.2,-5.17350646021553));
#274033=CARTESIAN_POINT('Ctrl Pts',(-9.96091394165166,15.2,-5.17615594921828));
#274034=CARTESIAN_POINT('Ctrl Pts',(-9.96310799423841,15.2,-5.17881359491226));
#274035=CARTESIAN_POINT('Ctrl Pts',(-9.96530204722373,15.2,-5.18147124108905));
#274036=CARTESIAN_POINT('Ctrl Pts',(-9.96749756672617,15.2,-5.18413704359317));
#274037=CARTESIAN_POINT('Ctrl Pts',(-9.96969450871231,15.2,-5.18681099335788));
#274038=CARTESIAN_POINT('Ctrl Pts',(-9.97189145029933,15.2,-5.18948494263682));
#274039=CARTESIAN_POINT('Ctrl Pts',(-9.97408981417886,15.2,-5.19216704003293));
#274040=CARTESIAN_POINT('Ctrl Pts',(-9.97628955537565,15.2,-5.1948572739872));
#274041=CARTESIAN_POINT('Ctrl Pts',(-9.97995579083685,15.2,-5.1993409974072));
#274042=CARTESIAN_POINT('Ctrl Pts',(-9.98362585221359,15.2,-5.20384732657383));
#274043=CARTESIAN_POINT('Ctrl Pts',(-9.9872995359639,15.2,-5.20837621386734));
#274044=CARTESIAN_POINT('Ctrl Pts',(-9.989503746134,15.2,-5.21109354614473));
#274045=CARTESIAN_POINT('Ctrl Pts',(-9.99170926115401,15.2,-5.21381899963));
#274046=CARTESIAN_POINT('Ctrl Pts',(-9.99391603624061,15.2,-5.21655256528139));
#274047=CARTESIAN_POINT('Ctrl Pts',(-9.9961228113272,15.2,-5.21928613093277));
#274048=CARTESIAN_POINT('Ctrl Pts',(-9.9983308461723,15.2,-5.22202780745652));
#274049=CARTESIAN_POINT('Ctrl Pts',(-10.0005400987687,15.2,-5.22477758703579));
#274050=CARTESIAN_POINT('Ctrl Pts',(-10.0027493513651,15.2,-5.22752736661506));
#274051=CARTESIAN_POINT('Ctrl Pts',(-10.0049598210517,15.2,-5.23028524661876));
#274052=CARTESIAN_POINT('Ctrl Pts',(-10.0071714637314,15.2,-5.23305121973911));
#274053=CARTESIAN_POINT('Ctrl Pts',(-10.0093831064111,15.2,-5.23581719285947));
#274054=CARTESIAN_POINT('Ctrl Pts',(-10.0115959234393,15.2,-5.23859125733195));
#274055=CARTESIAN_POINT('Ctrl Pts',(-10.0138098710254,15.2,-5.24137340448017));
#274056=CARTESIAN_POINT('Ctrl Pts',(-10.0160238186115,15.2,-5.24415555162838));
#274057=CARTESIAN_POINT('Ctrl Pts',(-10.0182388956476,15.2,-5.24694578014271));
#274058=CARTESIAN_POINT('Ctrl Pts',(-10.0204550622336,15.2,-5.24974408087327));
#274059=CARTESIAN_POINT('Ctrl Pts',(-10.0226712292222,15.2,-5.25254238211218));
#274060=CARTESIAN_POINT('Ctrl Pts',(-10.0248884846278,15.2,-5.25534875565338));
#274061=CARTESIAN_POINT('Ctrl Pts',(-10.027106784742,15.2,-5.25816319135518));
#274062=CARTESIAN_POINT('Ctrl Pts',(-10.0293250844532,15.2,-5.26097762654569));
#274063=CARTESIAN_POINT('Ctrl Pts',(-10.031544430856,15.2,-5.26380012362741));
#274064=CARTESIAN_POINT('Ctrl Pts',(-10.0337647804838,15.2,-5.26663067331696));
#274065=CARTESIAN_POINT('Ctrl Pts',(-10.0359851301115,15.2,-5.2694612230065));
#274066=CARTESIAN_POINT('Ctrl Pts',(-10.0382064823394,15.2,-5.27229982469302));
#274067=CARTESIAN_POINT('Ctrl Pts',(-10.0404287964771,15.2,-5.27514646747755));
#274068=CARTESIAN_POINT('Ctrl Pts',(-10.0426511106147,15.2,-5.27799311026207));
#274069=CARTESIAN_POINT('Ctrl Pts',(-10.0448743869021,15.2,-5.28084779557175));
#274070=CARTESIAN_POINT('Ctrl Pts',(-10.0470985830397,15.2,-5.28371051273069));
#274071=CARTESIAN_POINT('Ctrl Pts',(-10.0500641781592,15.2,-5.28752746928932));
#274072=CARTESIAN_POINT('Ctrl Pts',(-10.0530314081763,15.2,-5.29135870395377));
#274073=CARTESIAN_POINT('Ctrl Pts',(-10.0560001747271,15.2,-5.29520419388704));
#274074=CARTESIAN_POINT('Ctrl Pts',(-10.058226749438,15.2,-5.29808831107501));
#274075=CARTESIAN_POINT('Ctrl Pts',(-10.0604541895072,15.2,-5.30098044610422));
#274076=CARTESIAN_POINT('Ctrl Pts',(-10.0626824527179,15.2,-5.30388058883287));
#274077=CARTESIAN_POINT('Ctrl Pts',(-10.0649107159287,15.2,-5.30678073156153));
#274078=CARTESIAN_POINT('Ctrl Pts',(-10.0671398030063,15.2,-5.30968888177863));
#274079=CARTESIAN_POINT('Ctrl Pts',(-10.0693696727271,15.2,-5.31260503043594));
#274080=CARTESIAN_POINT('Ctrl Pts',(-10.0715995424479,15.2,-5.31552117909326));
#274081=CARTESIAN_POINT('Ctrl Pts',(-10.073830195969,15.2,-5.31844532509055));
#274082=CARTESIAN_POINT('Ctrl Pts',(-10.0760615897314,15.2,-5.3213774582473));
#274083=CARTESIAN_POINT('Ctrl Pts',(-10.0782929834937,15.2,-5.32430959140405));
#274084=CARTESIAN_POINT('Ctrl Pts',(-10.0805251200545,15.2,-5.32724971180322));
#274085=CARTESIAN_POINT('Ctrl Pts',(-10.0827579573067,15.2,-5.33019780894542));
#274086=CARTESIAN_POINT('Ctrl Pts',(-10.0849907945588,15.2,-5.33314590608762));
#274087=CARTESIAN_POINT('Ctrl Pts',(-10.0872243338109,15.2,-5.33610197912926));
#274088=CARTESIAN_POINT('Ctrl Pts',(-10.0894585349797,15.2,-5.33906601889547));
#274089=CARTESIAN_POINT('Ctrl Pts',(-10.0916927365543,15.2,-5.34203005920015));
#274090=CARTESIAN_POINT('Ctrl Pts',(-10.0939276000624,15.2,-5.34500206704876));
#274091=CARTESIAN_POINT('Ctrl Pts',(-10.0961630855541,15.2,-5.34798202985793));
#274092=CARTESIAN_POINT('Ctrl Pts',(-10.0991437321994,15.2,-5.35195531270122));
#274093=CARTESIAN_POINT('Ctrl Pts',(-10.1021254821311,15.2,-5.355942739759));
#274094=CARTESIAN_POINT('Ctrl Pts',(-10.1051082402897,15.2,-5.35994428450557));
#274095=CARTESIAN_POINT('Ctrl Pts',(-10.1073453090102,15.2,-5.3629454432018));
#274096=CARTESIAN_POINT('Ctrl Pts',(-10.1095829447208,15.2,-5.36595454263154));
#274097=CARTESIAN_POINT('Ctrl Pts',(-10.1118211114728,15.2,-5.36897157389624));
#274098=CARTESIAN_POINT('Ctrl Pts',(-10.1140592782247,15.2,-5.37198860516093));
#274099=CARTESIAN_POINT('Ctrl Pts',(-10.1162979764433,15.2,-5.37501356935007));
#274100=CARTESIAN_POINT('Ctrl Pts',(-10.1185371685286,15.2,-5.37804645357213));
#274101=CARTESIAN_POINT('Ctrl Pts',(-10.1207763610206,15.2,-5.38107933834516));
#274102=CARTESIAN_POINT('Ctrl Pts',(-10.1230160464794,15.2,-5.3841201444871));
#274103=CARTESIAN_POINT('Ctrl Pts',(-10.1252561779717,15.2,-5.38716885968126));
#274104=CARTESIAN_POINT('Ctrl Pts',(-10.1274963090571,15.2,-5.39021757432157));
#274105=CARTESIAN_POINT('Ctrl Pts',(-10.1297368853697,15.2,-5.3932741973836));
#274106=CARTESIAN_POINT('Ctrl Pts',(-10.131977863942,15.2,-5.39633871684295));
#274107=CARTESIAN_POINT('Ctrl Pts',(-10.1342188425142,15.2,-5.3994032363023));
#274108=CARTESIAN_POINT('Ctrl Pts',(-10.1364602251632,15.2,-5.40247565238601));
#274109=CARTESIAN_POINT('Ctrl Pts',(-10.1387019915142,15.2,-5.40555595924693));
#274110=CARTESIAN_POINT('Ctrl Pts',(-10.1409437578652,15.2,-5.40863626610785));
#274111=CARTESIAN_POINT('Ctrl Pts',(-10.1431859115927,15.2,-5.41172446343756));
#274112=CARTESIAN_POINT('Ctrl Pts',(-10.1454284470001,15.2,-5.41482055400001));
#274113=CARTESIAN_POINT('Ctrl Pts',(-9.31239140100006,12.2,-4.57383771200002));
#274114=CARTESIAN_POINT('Ctrl Pts',(-9.31392145135453,12.2,-4.5747602550189));
#274115=CARTESIAN_POINT('Ctrl Pts',(-9.31549767328181,12.2,-4.5757169317027));
#274116=CARTESIAN_POINT('Ctrl Pts',(-9.31711891458909,12.2,-4.57670776794144));
#274117=CARTESIAN_POINT('Ctrl Pts',(-9.31874797434146,12.2,-4.57770338249336));
#274118=CARTESIAN_POINT('Ctrl Pts',(-9.32042248440092,12.2,-4.57873349977316));
#274119=CARTESIAN_POINT('Ctrl Pts',(-9.32214130041636,12.2,-4.57979816338637));
#274120=CARTESIAN_POINT('Ctrl Pts',(-9.32386011627568,12.2,-4.58086282690287));
#274121=CARTESIAN_POINT('Ctrl Pts',(-9.32562323899895,12.2,-4.58196203944949));
#274122=CARTESIAN_POINT('Ctrl Pts',(-9.32742955676663,12.2,-4.58309584749161));
#274123=CARTESIAN_POINT('Ctrl Pts',(-9.32923587453431,12.2,-4.58422965553373));
#274124=CARTESIAN_POINT('Ctrl Pts',(-9.33108538730214,12.2,-4.5853980568443));
#274125=CARTESIAN_POINT('Ctrl Pts',(-9.33297701357543,12.2,-4.58660109210866));
#274126=CARTESIAN_POINT('Ctrl Pts',(-9.33486864002055,12.2,-4.5878041274823));
#274127=CARTESIAN_POINT('Ctrl Pts',(-9.3368023827215,12.2,-4.58904179825028));
#274128=CARTESIAN_POINT('Ctrl Pts',(-9.33877718899858,12.2,-4.59031413865532));
#274129=CARTESIAN_POINT('Ctrl Pts',(-9.3407519950963,12.2,-4.59158647894478));
#274130=CARTESIAN_POINT('Ctrl Pts',(-9.34276786524956,12.2,-4.59289349118482));
#274131=CARTESIAN_POINT('Ctrl Pts',(-9.34482377851759,12.2,-4.59423520622557));
#274132=CARTESIAN_POINT('Ctrl Pts',(-9.34687969178564,12.2,-4.59557692126631));
#274133=CARTESIAN_POINT('Ctrl Pts',(-9.34897564777141,12.2,-4.59695334018431));
#274134=CARTESIAN_POINT('Ctrl Pts',(-9.3511106521088,12.2,-4.59836449038153));
#274135=CARTESIAN_POINT('Ctrl Pts',(-9.35324565664012,12.2,-4.59977564070692));
#274136=CARTESIAN_POINT('Ctrl Pts',(-9.35541970904296,12.2,-4.60122152401996));
#274137=CARTESIAN_POINT('Ctrl Pts',(-9.35763184074945,12.2,-4.60270216418635));
#274138=CARTESIAN_POINT('Ctrl Pts',(-9.35984397225501,12.2,-4.60418280421825));
#274139=CARTESIAN_POINT('Ctrl Pts',(-9.36209418289797,12.2,-4.60569820177273));
#274140=CARTESIAN_POINT('Ctrl Pts',(-9.36438152939981,12.2,-4.60724837688458));
#274141=CARTESIAN_POINT('Ctrl Pts',(-9.36666887590164,12.2,-4.60879855199643));
#274142=CARTESIAN_POINT('Ctrl Pts',(-9.36899335821715,12.2,-4.61038350755551));
#274143=CARTESIAN_POINT('Ctrl Pts',(-9.37135405587982,12.2,-4.61200325866183));
#274144=CARTESIAN_POINT('Ctrl Pts',(-9.3737147535425,12.2,-4.61362300976815));
#274145=CARTESIAN_POINT('Ctrl Pts',(-9.37611166665068,12.2,-4.61527755752125));
#274146=CARTESIAN_POINT('Ctrl Pts',(-9.37854389747655,12.2,-4.61696691654082));
#274147=CARTESIAN_POINT('Ctrl Pts',(-9.38097612852336,12.2,-4.61865627571385));
#274148=CARTESIAN_POINT('Ctrl Pts',(-9.38344367732366,12.2,-4.62038044747359));
#274149=CARTESIAN_POINT('Ctrl Pts',(-9.38594566837816,12.2,-4.6221394416543));
#274150=CARTESIAN_POINT('Ctrl Pts',(-9.38844765920541,12.2,-4.62389843567522));
#274151=CARTESIAN_POINT('Ctrl Pts',(-9.39098409293896,12.2,-4.62569225337401));
#274152=CARTESIAN_POINT('Ctrl Pts',(-9.39355411294049,12.2,-4.62752090148245));
#274153=CARTESIAN_POINT('Ctrl Pts',(-9.39612413294203,12.2,-4.62934954959089));
#274154=CARTESIAN_POINT('Ctrl Pts',(-9.39872774117737,12.2,-4.63121303114775));
#274155=CARTESIAN_POINT('Ctrl Pts',(-9.40136410124598,12.2,-4.63311134807638));
#274156=CARTESIAN_POINT('Ctrl Pts',(-9.40400046155406,12.2,-4.63500966517744));
#274157=CARTESIAN_POINT('Ctrl Pts',(-9.40666957427374,12.2,-4.63694281996525));
#274158=CARTESIAN_POINT('Ctrl Pts',(-9.40937062267235,12.2,-4.63891081407403));
#274159=CARTESIAN_POINT('Ctrl Pts',(-9.4120716708256,12.2,-4.64087880800404));
#274160=CARTESIAN_POINT('Ctrl Pts',(-9.4148046571617,12.2,-4.64288164279723));
#274161=CARTESIAN_POINT('Ctrl Pts',(-9.41756878149041,12.2,-4.64491931573237));
#274162=CARTESIAN_POINT('Ctrl Pts',(-9.42033290581914,12.2,-4.64695698866751));
#274163=CARTESIAN_POINT('Ctrl Pts',(-9.42312816853842,12.2,-4.64902950149087));
#274164=CARTESIAN_POINT('Ctrl Pts',(-9.42595379268368,12.2,-4.65113685049526));
#274165=CARTESIAN_POINT('Ctrl Pts',(-9.42877941708561,12.2,-4.65324419969107));
#274166=CARTESIAN_POINT('Ctrl Pts',(-9.4316353997261,12.2,-4.65538638539789));
#274167=CARTESIAN_POINT('Ctrl Pts',(-9.43452097952923,12.2,-4.65756340246064));
#274168=CARTESIAN_POINT('Ctrl Pts',(-9.43740655907025,12.2,-4.65974041932565));
#274169=CARTESIAN_POINT('Ctrl Pts',(-9.44032173581533,12.2,-4.66195226643993));
#274170=CARTESIAN_POINT('Ctrl Pts',(-9.44326576245835,12.2,-4.66419893644163));
#274171=CARTESIAN_POINT('Ctrl Pts',(-9.44620978910138,12.2,-4.66644560644333));
#274172=CARTESIAN_POINT('Ctrl Pts',(-9.4491826676622,12.2,-4.66872709947977));
#274173=CARTESIAN_POINT('Ctrl Pts',(-9.45218366545143,12.2,-4.6710434045093));
#274174=CARTESIAN_POINT('Ctrl Pts',(-9.45518466351327,12.2,-4.67335970974922));
#274175=CARTESIAN_POINT('Ctrl Pts',(-9.45821378240637,12.2,-4.67571082796928));
#274176=CARTESIAN_POINT('Ctrl Pts',(-9.46127030532485,12.2,-4.67809674501836));
#274177=CARTESIAN_POINT('Ctrl Pts',(-9.46432682796567,12.2,-4.68048266185072));
#274178=CARTESIAN_POINT('Ctrl Pts',(-9.46741075545025,12.2,-4.68290337572907));
#274179=CARTESIAN_POINT('Ctrl Pts',(-9.47052138718476,12.2,-4.68535887548441));
#274180=CARTESIAN_POINT('Ctrl Pts',(-9.47363201891927,12.2,-4.68781437523976));
#274181=CARTESIAN_POINT('Ctrl Pts',(-9.4767693554688,12.2,-4.69030465833076));
#274182=CARTESIAN_POINT('Ctrl Pts',(-9.47993270826938,12.2,-4.69282970715415));
#274183=CARTESIAN_POINT('Ctrl Pts',(-9.48256883569897,12.2,-4.69493391458342));
#274184=CARTESIAN_POINT('Ctrl Pts',(-9.48522303133183,12.2,-4.69706226520502));
#274185=CARTESIAN_POINT('Ctrl Pts',(-9.48789490535872,12.2,-4.69921474763433));
#274186=CARTESIAN_POINT('Ctrl Pts',(-9.49056677938559,12.2,-4.70136723006365));
#274187=CARTESIAN_POINT('Ctrl Pts',(-9.49325633158075,12.2,-4.70354384381107));
#274188=CARTESIAN_POINT('Ctrl Pts',(-9.49596317673188,12.2,-4.70574457701543));
#274189=CARTESIAN_POINT('Ctrl Pts',(-9.498670021883,12.2,-4.70794531021979));
#274190=CARTESIAN_POINT('Ctrl Pts',(-9.50139416162778,12.2,-4.71017016276662));
#274191=CARTESIAN_POINT('Ctrl Pts',(-9.50413521822501,12.2,-4.71241912026662));
#274192=CARTESIAN_POINT('Ctrl Pts',(-9.50687627482223,12.2,-4.71466807776662));
#274193=CARTESIAN_POINT('Ctrl Pts',(-9.50963424783887,12.2,-4.71694114255181));
#274194=CARTESIAN_POINT('Ctrl Pts',(-9.51240876618487,12.2,-4.71923829749288));
#274195=CARTESIAN_POINT('Ctrl Pts',(-9.51518328453086,12.2,-4.72153545243394));
#274196=CARTESIAN_POINT('Ctrl Pts',(-9.51797434851064,12.2,-4.72385669852444));
#274197=CARTESIAN_POINT('Ctrl Pts',(-9.52078159115037,12.2,-4.72620202088682));
#274198=CARTESIAN_POINT('Ctrl Pts',(-9.52358883379011,12.2,-4.72854734324919));
#274199=CARTESIAN_POINT('Ctrl Pts',(-9.52641225669053,12.2,-4.73091674053871));
#274200=CARTESIAN_POINT('Ctrl Pts',(-9.52925149842746,12.2,-4.73331019866497));
#274201=CARTESIAN_POINT('Ctrl Pts',(-9.53209074016441,12.2,-4.73570365679122));
#274202=CARTESIAN_POINT('Ctrl Pts',(-9.53494580164996,12.2,-4.7381211734154));
#274203=CARTESIAN_POINT('Ctrl Pts',(-9.53781632776663,12.2,-4.7405627325668));
#274204=CARTESIAN_POINT('Ctrl Pts',(-9.54068685388331,12.2,-4.7430042917182));
#274205=CARTESIAN_POINT('Ctrl Pts',(-9.54357284573936,12.2,-4.74546989288476));
#274206=CARTESIAN_POINT('Ctrl Pts',(-9.54647395337949,12.2,-4.74795951781727));
#274207=CARTESIAN_POINT('Ctrl Pts',(-9.54937506101962,12.2,-4.75044914274978));
#274208=CARTESIAN_POINT('Ctrl Pts',(-9.55229128489328,12.2,-4.7529627916299));
#274209=CARTESIAN_POINT('Ctrl Pts',(-9.55522228086673,12.2,-4.75550044559022));
#274210=CARTESIAN_POINT('Ctrl Pts',(-9.55815327652072,12.2,-4.75803809927394));
#274211=CARTESIAN_POINT('Ctrl Pts',(-9.56109904385334,12.2,-4.76059975770666));
#274212=CARTESIAN_POINT('Ctrl Pts',(-9.5640592454045,12.2,-4.76318540068676));
#274213=CARTESIAN_POINT('Ctrl Pts',(-9.56701944727832,12.2,-4.7657710439487));
#274214=CARTESIAN_POINT('Ctrl Pts',(-9.56999408261026,12.2,-4.76838067303523));
#274215=CARTESIAN_POINT('Ctrl Pts',(-9.57298281781743,12.2,-4.77101426463048));
#274216=CARTESIAN_POINT('Ctrl Pts',(-9.57597155302458,12.2,-4.77364785622573));
#274217=CARTESIAN_POINT('Ctrl Pts',(-9.57897438660656,12.2,-4.7763054129456));
#274218=CARTESIAN_POINT('Ctrl Pts',(-9.58199099264712,12.2,-4.77898691037422));
#274219=CARTESIAN_POINT('Ctrl Pts',(-9.58500759868768,12.2,-4.78166840780283));
#274220=CARTESIAN_POINT('Ctrl Pts',(-9.58803797563447,12.2,-4.78437384870405));
#274221=CARTESIAN_POINT('Ctrl Pts',(-9.59108179939673,12.2,-4.78710320869987));
#274222=CARTESIAN_POINT('Ctrl Pts',(-9.59412562315899,12.2,-4.78983256869569));
#274223=CARTESIAN_POINT('Ctrl Pts',(-9.59718289253887,12.2,-4.79258584833639));
#274224=CARTESIAN_POINT('Ctrl Pts',(-9.60025329031597,12.2,-4.79536302479347));
#274225=CARTESIAN_POINT('Ctrl Pts',(-9.60332368809306,12.2,-4.79814020125056));
#274226=CARTESIAN_POINT('Ctrl Pts',(-9.60640721300385,12.2,-4.80094127343883));
#274227=CARTESIAN_POINT('Ctrl Pts',(-9.6095035493226,12.2,-4.80376621829868));
#274228=CARTESIAN_POINT('Ctrl Pts',(-9.6119806185126,12.2,-4.80602617430972));
#274229=CARTESIAN_POINT('Ctrl Pts',(-9.61446588758683,12.2,-4.80830140910293));
#274230=CARTESIAN_POINT('Ctrl Pts',(-9.61695919757019,12.2,-4.81059190856574));
#274231=CARTESIAN_POINT('Ctrl Pts',(-9.61945250721385,12.2,-4.81288240771646));
#274232=CARTESIAN_POINT('Ctrl Pts',(-9.62195385795338,12.2,-4.8151881740372));
#274233=CARTESIAN_POINT('Ctrl Pts',(-9.6244630908033,12.2,-4.81750919056869));
#274234=CARTESIAN_POINT('Ctrl Pts',(-9.62697232399511,12.2,-4.81983020741642));
#274235=CARTESIAN_POINT('Ctrl Pts',(-9.62948943990175,12.2,-4.82216647831043));
#274236=CARTESIAN_POINT('Ctrl Pts',(-9.6320142837065,12.2,-4.82451798771733));
#274237=CARTESIAN_POINT('Ctrl Pts',(-9.63453912716724,12.2,-4.82686949680385));
#274238=CARTESIAN_POINT('Ctrl Pts',(-9.63707169781845,12.2,-4.82923624555923));
#274239=CARTESIAN_POINT('Ctrl Pts',(-9.63961184084815,12.2,-4.83161821937107));
#274240=CARTESIAN_POINT('Ctrl Pts',(-9.64215198422393,12.2,-4.83400019350745));
#274241=CARTESIAN_POINT('Ctrl Pts',(-9.6446997014748,12.2,-4.83639739330373));
#274242=CARTESIAN_POINT('Ctrl Pts',(-9.64725483872565,12.2,-4.83880980521398));
#274243=CARTESIAN_POINT('Ctrl Pts',(-9.64980997562837,12.2,-4.84122221679555));
#274244=CARTESIAN_POINT('Ctrl Pts',(-9.65237253334902,12.2,-4.84364983922403));
#274245=CARTESIAN_POINT('Ctrl Pts',(-9.65494236030486,12.2,-4.84609266013389));
#274246=CARTESIAN_POINT('Ctrl Pts',(-9.65751218761083,12.2,-4.84853548137658));
#274247=CARTESIAN_POINT('Ctrl Pts',(-9.66008928519087,12.2,-4.85099349973058));
#274248=CARTESIAN_POINT('Ctrl Pts',(-9.66267350251012,12.2,-4.85346670104331));
#274249=CARTESIAN_POINT('Ctrl Pts',(-9.66525771947728,12.2,-4.85593990201906));
#274250=CARTESIAN_POINT('Ctrl Pts',(-9.66784905781333,12.2,-4.85842828513574));
#274251=CARTESIAN_POINT('Ctrl Pts',(-9.67044736810021,12.2,-4.86093183737397));
#274252=CARTESIAN_POINT('Ctrl Pts',(-9.6730456787411,12.2,-4.8634353899533));
#274253=CARTESIAN_POINT('Ctrl Pts',(-9.67565096202709,12.2,-4.86595411054239));
#274254=CARTESIAN_POINT('Ctrl Pts',(-9.67826307255836,12.2,-4.86848798395828));
#274255=CARTESIAN_POINT('Ctrl Pts',(-9.68087518308964,12.2,-4.87102185737418));
#274256=CARTESIAN_POINT('Ctrl Pts',(-9.68349411927721,12.2,-4.87357088540569));
#274257=CARTESIAN_POINT('Ctrl Pts',(-9.68611973792099,12.2,-4.87613504943587));
#274258=CARTESIAN_POINT('Ctrl Pts',(-9.68874535620702,12.2,-4.87869921311667));
#274259=CARTESIAN_POINT('Ctrl Pts',(-9.69137765681035,12.2,-4.88127851637635));
#274260=CARTESIAN_POINT('Ctrl Pts',(-9.69401649577323,12.2,-4.88387294073152));
#274261=CARTESIAN_POINT('Ctrl Pts',(-9.69665533509566,12.2,-4.88646736544018));
#274262=CARTESIAN_POINT('Ctrl Pts',(-9.69930071320232,12.2,-4.88907691257618));
#274263=CARTESIAN_POINT('Ctrl Pts',(-9.70195248795859,12.2,-4.89170156588742));
#274264=CARTESIAN_POINT('Ctrl Pts',(-9.70460426235357,12.2,-4.89432621884106));
#274265=CARTESIAN_POINT('Ctrl Pts',(-9.70726243379217,12.2,-4.89696597790942));
#274266=CARTESIAN_POINT('Ctrl Pts',(-9.70992686274061,12.2,-4.89962082752473));
#274267=CARTESIAN_POINT('Ctrl Pts',(-9.71259129205207,12.2,-4.90227567750177));
#274268=CARTESIAN_POINT('Ctrl Pts',(-9.71526197812224,12.2,-4.90494561756343));
#274269=CARTESIAN_POINT('Ctrl Pts',(-9.71793878168015,12.2,-4.90763063162299));
#274270=CARTESIAN_POINT('Ctrl Pts',(-9.72061558487334,12.2,-4.9103156453167));
#274271=CARTESIAN_POINT('Ctrl Pts',(-9.72329850607269,12.2,-4.91301573183997));
#274272=CARTESIAN_POINT('Ctrl Pts',(-9.72598740829694,12.2,-4.91573087672814));
#274273=CARTESIAN_POINT('Ctrl Pts',(-9.72867631088753,12.2,-4.91844602198624));
#274274=CARTESIAN_POINT('Ctrl Pts',(-9.73137119228999,12.2,-4.92117622362949));
#274275=CARTESIAN_POINT('Ctrl Pts',(-9.73407191843753,12.2,-4.92392146622452));
#274276=CARTESIAN_POINT('Ctrl Pts',(-9.73677264421712,12.2,-4.9266667084455));
#274277=CARTESIAN_POINT('Ctrl Pts',(-9.73947921572654,12.2,-4.92942699090073));
#274278=CARTESIAN_POINT('Ctrl Pts',(-9.74219149563983,12.2,-4.932202296089));
#274279=CARTESIAN_POINT('Ctrl Pts',(-9.74490377592268,12.2,-4.93497760165539));
#274280=CARTESIAN_POINT('Ctrl Pts',(-9.74762176627394,12.2,-4.93776792979501));
#274281=CARTESIAN_POINT('Ctrl Pts',(-9.75034533175607,12.2,-4.94057326500444));
#274282=CARTESIAN_POINT('Ctrl Pts',(-9.75306889686712,12.2,-4.94337859983163));
#274283=CARTESIAN_POINT('Ctrl Pts',(-9.75579803931316,12.2,-4.94619893957527));
#274284=CARTESIAN_POINT('Ctrl Pts',(-9.75853262381126,12.2,-4.94903426778638));
#274285=CARTESIAN_POINT('Ctrl Pts',(-9.76126720868195,12.2,-4.95186959638382));
#274286=CARTESIAN_POINT('Ctrl Pts',(-9.76400723812036,12.2,-4.95471991250215));
#274287=CARTESIAN_POINT('Ctrl Pts',(-9.7667525802269,12.2,-4.95758519972691));
#274288=CARTESIAN_POINT('Ctrl Pts',(-9.76949792195939,12.2,-4.96045048656128));
#274289=CARTESIAN_POINT('Ctrl Pts',(-9.77224857603917,12.2,-4.96333074362037));
#274290=CARTESIAN_POINT('Ctrl Pts',(-9.77500441375779,12.2,-4.96622595249326));
#274291=CARTESIAN_POINT('Ctrl Pts',(-9.77776025185188,12.2,-4.96912116176063));
#274292=CARTESIAN_POINT('Ctrl Pts',(-9.78052127223538,12.2,-4.97203132285163));
#274293=CARTESIAN_POINT('Ctrl Pts',(-9.78328734777504,12.2,-4.97495641823329));
#274294=CARTESIAN_POINT('Ctrl Pts',(-9.78743646070764,12.2,-4.97934406090722));
#274295=CARTESIAN_POINT('Ctrl Pts',(-9.79159694677267,12.2,-4.98376530534521));
#274296=CARTESIAN_POINT('Ctrl Pts',(-9.79576837653703,12.2,-4.9882200870144));
#274297=CARTESIAN_POINT('Ctrl Pts',(-9.79854932996587,12.2,-4.99118994173029));
#274298=CARTESIAN_POINT('Ctrl Pts',(-9.80133514680659,12.2,-4.9941747022415));
#274299=CARTESIAN_POINT('Ctrl Pts',(-9.80412570302694,12.2,-4.997174350752));
#274300=CARTESIAN_POINT('Ctrl Pts',(-9.80691625886708,12.2,-5.00017399885381));
#274301=CARTESIAN_POINT('Ctrl Pts',(-9.80971155279107,12.2,-5.0031885337955));
#274302=CARTESIAN_POINT('Ctrl Pts',(-9.81251146128392,12.2,-5.00621793604632));
#274303=CARTESIAN_POINT('Ctrl Pts',(-9.81531137015826,12.2,-5.0092473387099));
#274304=CARTESIAN_POINT('Ctrl Pts',(-9.81811589324418,12.2,-5.01229160993879));
#274305=CARTESIAN_POINT('Ctrl Pts',(-9.82092490800837,12.2,-5.01535072921662));
#274306=CARTESIAN_POINT('Ctrl Pts',(-9.82373392277256,12.2,-5.01840984849443));
#274307=CARTESIAN_POINT('Ctrl Pts',(-9.82654742665396,12.2,-5.02148381624067));
#274308=CARTESIAN_POINT('Ctrl Pts',(-9.8293653014191,12.2,-5.02457261352165));
#274309=CARTESIAN_POINT('Ctrl Pts',(-9.8321831758003,12.2,-5.02766141038177));
#274310=CARTESIAN_POINT('Ctrl Pts',(-9.83500541940801,12.2,-5.0307650353942));
#274311=CARTESIAN_POINT('Ctrl Pts',(-9.83783191002311,12.2,-5.0338834702645));
#274312=CARTESIAN_POINT('Ctrl Pts',(-9.84065840102332,12.2,-5.03700190555969));
#274313=CARTESIAN_POINT('Ctrl Pts',(-9.84348913920863,12.2,-5.04013515023326));
#274314=CARTESIAN_POINT('Ctrl Pts',(-9.84632400669687,12.2,-5.04328318423967));
#274315=CARTESIAN_POINT('Ctrl Pts',(-9.84915887379886,12.2,-5.04643121781715));
#274316=CARTESIAN_POINT('Ctrl Pts',(-9.85199786805311,12.2,-5.04959404073994));
#274317=CARTESIAN_POINT('Ctrl Pts',(-9.85484087254266,12.2,-5.052771632257));
#274318=CARTESIAN_POINT('Ctrl Pts',(-9.85839462844512,12.2,-5.05674362197803));
#274319=CARTESIAN_POINT('Ctrl Pts',(-9.86195464930968,12.2,-5.06073869074068));
#274320=CARTESIAN_POINT('Ctrl Pts',(-9.86552070300643,12.2,-5.06475679402278));
#274321=CARTESIAN_POINT('Ctrl Pts',(-9.86837354611931,12.2,-5.06797127682365));
#274322=CARTESIAN_POINT('Ctrl Pts',(-9.87123025216421,12.2,-5.07120050405204));
#274323=CARTESIAN_POINT('Ctrl Pts',(-9.8740907037094,12.2,-5.07444445456368));
#274324=CARTESIAN_POINT('Ctrl Pts',(-9.87695115486483,12.2,-5.07768840463335));
#274325=CARTESIAN_POINT('Ctrl Pts',(-9.87981535070587,12.2,-5.08094707675383));
#274326=CARTESIAN_POINT('Ctrl Pts',(-9.88268317724897,12.2,-5.0842204522075));
#274327=CARTESIAN_POINT('Ctrl Pts',(-9.88555100418281,12.2,-5.08749382810716));
#274328=CARTESIAN_POINT('Ctrl Pts',(-9.88842246196105,12.2,-5.09078190490244));
#274329=CARTESIAN_POINT('Ctrl Pts',(-9.89129743515057,12.2,-5.09408466430429));
#274330=CARTESIAN_POINT('Ctrl Pts',(-9.89417240794838,12.2,-5.09738742325614));
#274331=CARTESIAN_POINT('Ctrl Pts',(-9.89705089622251,12.2,-5.10070486193438));
#274332=CARTESIAN_POINT('Ctrl Pts',(-9.89993278676448,12.2,-5.10403696199437));
#274333=CARTESIAN_POINT('Ctrl Pts',(-9.90281467769911,12.2,-5.10736906250835));
#274334=CARTESIAN_POINT('Ctrl Pts',(-9.90569997112302,12.2,-5.11071582267963));
#274335=CARTESIAN_POINT('Ctrl Pts',(-9.90858855350289,12.2,-5.11407722130823));
#274336=CARTESIAN_POINT('Ctrl Pts',(-9.91147713548918,12.2,-5.11743861947885));
#274337=CARTESIAN_POINT('Ctrl Pts',(-9.91436900723339,12.2,-5.1208146564282));
#274338=CARTESIAN_POINT('Ctrl Pts',(-9.91726405736331,12.2,-5.12420531020803));
#274339=CARTESIAN_POINT('Ctrl Pts',(-9.91943534505935,12.2,-5.1267483006584));
#274340=CARTESIAN_POINT('Ctrl Pts',(-9.92160842085518,12.2,-5.12929951423611));
#274341=CARTESIAN_POINT('Ctrl Pts',(-9.92378323698427,12.2,-5.13185893997534));
#274342=CARTESIAN_POINT('Ctrl Pts',(-9.92595805350845,12.2,-5.13441836617954));
#274343=CARTESIAN_POINT('Ctrl Pts',(-9.9281346112081,12.2,-5.13698600510269));
#274344=CARTESIAN_POINT('Ctrl Pts',(-9.93031286319157,12.2,-5.1395618478115));
#274345=CARTESIAN_POINT('Ctrl Pts',(-9.93249111477933,12.2,-5.14213769005236));
#274346=CARTESIAN_POINT('Ctrl Pts',(-9.93467106195033,12.2,-5.14472173610946));
#274347=CARTESIAN_POINT('Ctrl Pts',(-9.93685265653787,12.2,-5.14731397680765));
#274348=CARTESIAN_POINT('Ctrl Pts',(-9.93903425112541,12.2,-5.14990621750584));
#274349=CARTESIAN_POINT('Ctrl Pts',(-9.94121749392148,12.2,-5.15250665203523));
#274350=CARTESIAN_POINT('Ctrl Pts',(-9.9434023400187,12.2,-5.155115272244));
#274351=CARTESIAN_POINT('Ctrl Pts',(-9.94558718611591,12.2,-5.15772389245277));
#274352=CARTESIAN_POINT('Ctrl Pts',(-9.94777363480096,12.2,-5.1603406977644));
#274353=CARTESIAN_POINT('Ctrl Pts',(-9.94996163993972,12.2,-5.16296567851424));
#274354=CARTESIAN_POINT('Ctrl Pts',(-9.95214964507848,12.2,-5.16559065926408));
#274355=CARTESIAN_POINT('Ctrl Pts',(-9.95433920767431,12.2,-5.16822381565886));
#274356=CARTESIAN_POINT('Ctrl Pts',(-9.95653028176125,12.2,-5.17086513793719));
#274357=CARTESIAN_POINT('Ctrl Pts',(-9.95872135584819,12.2,-5.17350646021553));
#274358=CARTESIAN_POINT('Ctrl Pts',(-9.96091394165166,12.2,-5.17615594921828));
#274359=CARTESIAN_POINT('Ctrl Pts',(-9.96310799423841,12.2,-5.17881359491226));
#274360=CARTESIAN_POINT('Ctrl Pts',(-9.96530204722373,12.2,-5.18147124108905));
#274361=CARTESIAN_POINT('Ctrl Pts',(-9.96749756672617,12.2,-5.18413704359317));
#274362=CARTESIAN_POINT('Ctrl Pts',(-9.96969450871231,12.2,-5.18681099335788));
#274363=CARTESIAN_POINT('Ctrl Pts',(-9.97189145029933,12.2,-5.18948494263682));
#274364=CARTESIAN_POINT('Ctrl Pts',(-9.97408981417886,12.2,-5.19216704003294));
#274365=CARTESIAN_POINT('Ctrl Pts',(-9.97628955537566,12.2,-5.1948572739872));
#274366=CARTESIAN_POINT('Ctrl Pts',(-9.97995579083685,12.2,-5.1993409974072));
#274367=CARTESIAN_POINT('Ctrl Pts',(-9.98362585221359,12.2,-5.20384732657383));
#274368=CARTESIAN_POINT('Ctrl Pts',(-9.9872995359639,12.2,-5.20837621386734));
#274369=CARTESIAN_POINT('Ctrl Pts',(-9.989503746134,12.2,-5.21109354614473));
#274370=CARTESIAN_POINT('Ctrl Pts',(-9.99170926115401,12.2,-5.21381899963));
#274371=CARTESIAN_POINT('Ctrl Pts',(-9.99391603624061,12.2,-5.21655256528139));
#274372=CARTESIAN_POINT('Ctrl Pts',(-9.9961228113272,12.2,-5.21928613093277));
#274373=CARTESIAN_POINT('Ctrl Pts',(-9.9983308461723,12.2,-5.22202780745652));
#274374=CARTESIAN_POINT('Ctrl Pts',(-10.0005400987687,12.2,-5.22477758703579));
#274375=CARTESIAN_POINT('Ctrl Pts',(-10.0027493513651,12.2,-5.22752736661506));
#274376=CARTESIAN_POINT('Ctrl Pts',(-10.0049598210517,12.2,-5.23028524661876));
#274377=CARTESIAN_POINT('Ctrl Pts',(-10.0071714637314,12.2,-5.23305121973911));
#274378=CARTESIAN_POINT('Ctrl Pts',(-10.0093831064111,12.2,-5.23581719285947));
#274379=CARTESIAN_POINT('Ctrl Pts',(-10.0115959234393,12.2,-5.23859125733195));
#274380=CARTESIAN_POINT('Ctrl Pts',(-10.0138098710254,12.2,-5.24137340448017));
